#45159 = CARTESIAN_POINT('Ctrl Pts',(-20.6099160380865,-21.5058009332471,
123.298380195676)) ;
#45160 = CARTESIAN_POINT('Ctrl Pts',(-20.9100801364126,-21.3258118528842,
123.270041130568)) ;
#45161 = CARTESIAN_POINT('Ctrl Pts',(-20.5720819647299,-21.5157699784016,
123.092270132128)) ;
#45162 = CARTESIAN_POINT('Ctrl Pts',(-20.8627908877047,-21.3357808980387,
123.01239695694)) ;
#45163 = CARTESIAN_POINT('Ctrl Pts',(-20.499885467458,-21.5256733690351,122.8969600671)) ;
#45164 = CARTESIAN_POINT('Ctrl Pts',(-20.7725483587208,-21.3456842886722,
122.768260657611)) ;
#45165 = CARTESIAN_POINT('Ctrl Pts',(-20.3931639686196,-21.5357311551478,
122.714452129114)) ;
#45166 = CARTESIAN_POINT('Ctrl Pts',(-20.6391462593297,-21.355742074785,122.540122041422)) ;
#45167 = CARTESIAN_POINT('Ctrl Pts',(-20.2592745444822,-21.5455831917976,
122.556386418772)) ;
#45168 = CARTESIAN_POINT('Ctrl Pts',(-20.471796281269,-21.3655941114347,122.342544854426)) ;
#45169 = CARTESIAN_POINT('Ctrl Pts',(-20.0435430288408,-21.5589483159408,
122.376446565359)) ;
#45170 = CARTESIAN_POINT('Ctrl Pts',(-20.202086568455,-21.3789592355779,122.117585029651)) ;
#45171 = CARTESIAN_POINT('Ctrl Pts',(-19.7882330766326,-21.5721743789038,
122.25842779773)) ;
#45172 = CARTESIAN_POINT('Ctrl Pts',(-19.8829746642869,-21.3921852985409,
121.970083356066)) ;
#45173 = CARTESIAN_POINT('Ctrl Pts',(-19.512730849252,-21.5854780271861,122.210256078633)) ;
#45174 = CARTESIAN_POINT('Ctrl Pts',(-19.5386166648269,-21.4054889468232,
121.909867161857)) ;
#45175 = CARTESIAN_POINT('Ctrl Pts',(-19.3026540676817,-21.5954695583491,
122.210450686566)) ;
#45176 = CARTESIAN_POINT('Ctrl Pts',(-19.2760167649195,-21.4154804779862,
121.910107183642)) ;
#45177 = CARTESIAN_POINT('Ctrl Pts',(-19.0948968921359,-21.6055090061484,
122.247567522211)) ;
#45178 = CARTESIAN_POINT('Ctrl Pts',(-19.0163207496462,-21.4255199257855,
121.956500605478)) ;
#45179 = CARTESIAN_POINT('Ctrl Pts',(-18.9004687004283,-21.6153527816622,
122.318496927726)) ;
#45180 = CARTESIAN_POINT('Ctrl Pts',(-18.7732843139319,-21.4353637012994,
122.045159677628)) ;
#45181 = CARTESIAN_POINT('Ctrl Pts',(-18.7185579083454,-21.6253384230499,
122.423213533386)) ;
#45182 = CARTESIAN_POINT('Ctrl Pts',(-18.5458944197202,-21.445349342687,122.176053036341)) ;
#45183 = CARTESIAN_POINT('Ctrl Pts',(-18.5582565476501,-21.6352752074117,
122.557220506057)) ;
#45184 = CARTESIAN_POINT('Ctrl Pts',(-18.3455158402902,-21.4552861270488,
122.343559635745)) ;
#45185 = CARTESIAN_POINT('Ctrl Pts',(-18.4222459587121,-21.645325041879,122.718871713832)) ;
#45186 = CARTESIAN_POINT('Ctrl Pts',(-18.1755004123989,-21.4653359615162,
122.545621877111)) ;
#45187 = CARTESIAN_POINT('Ctrl Pts',(-18.3183162605906,-21.6551754913822,
122.898008987532)) ;
#45188 = CARTESIAN_POINT('Ctrl Pts',(-18.0455857951863,-21.4751864110193,
122.769542152888)) ;
#45189 = CARTESIAN_POINT('Ctrl Pts',(-18.2456911500029,-21.6651475053643,
123.09464249712)) ;
#45190 = CARTESIAN_POINT('Ctrl Pts',(-17.9548017337126,-21.4851584250014,
123.015333175436)) ;
#45191 = CARTESIAN_POINT('Ctrl Pts',(-18.2082412582699,-21.6751426632114,
123.301442369805)) ;
#45192 = CARTESIAN_POINT('Ctrl Pts',(-17.9079865989931,-21.4951535828485,
123.273832595304)) ;
#45193 = CARTESIAN_POINT('Ctrl Pts',(-18.2075185297832,-21.6851765895751,
123.512368066183)) ;
#45194 = CARTESIAN_POINT('Ctrl Pts',(-17.9070803718407,-21.5051875092122,
123.537489745388)) ;
#45195 = CARTESIAN_POINT('Ctrl Pts',(-18.2424799085402,-21.6950322980075,
123.716614333339)) ;
#45196 = CARTESIAN_POINT('Ctrl Pts',(-17.9507793758627,-21.5150432176446,
123.792798278233)) ;
#45197 = CARTESIAN_POINT('Ctrl Pts',(-18.3130824839469,-21.7050304473461,
123.914559389374)) ;
#45198 = CARTESIAN_POINT('Ctrl Pts',(-18.0390300008137,-21.5250413669833,
124.040230621142)) ;
#45199 = CARTESIAN_POINT('Ctrl Pts',(-18.4158251214299,-21.7149298505197,
124.095582065844)) ;
#45200 = CARTESIAN_POINT('Ctrl Pts',(-18.1674560178269,-21.5349407701568,
124.266510551616)) ;
#45201 = CARTESIAN_POINT('Ctrl Pts',(-18.5504028728454,-21.7249810474082,
124.258463624392)) ;
#45202 = CARTESIAN_POINT('Ctrl Pts',(-18.3356760700349,-21.5449919670453,
124.470114254987)) ;
#45203 = CARTESIAN_POINT('Ctrl Pts',(-18.7085246366495,-21.734863371221,124.393249383885)) ;
#45204 = CARTESIAN_POINT('Ctrl Pts',(-18.5333267197165,-21.5548742908582,
124.63859875685)) ;
#45205 = CARTESIAN_POINT('Ctrl Pts',(-18.8894290935753,-21.7448582668776,
124.500128199222)) ;
#45206 = CARTESIAN_POINT('Ctrl Pts',(-18.7594560018533,-21.5648691865148,
124.772199667984)) ;
#45207 = CARTESIAN_POINT('Ctrl Pts',(-19.0867831919036,-21.7548793662602,
124.573882631177)) ;
#45208 = CARTESIAN_POINT('Ctrl Pts',(-19.0061476935566,-21.5748902858973,
124.864395292257)) ;
#45209 = CARTESIAN_POINT('Ctrl Pts',(-19.2915499840716,-21.7647866341222,
124.611973404616)) ;
#45210 = CARTESIAN_POINT('Ctrl Pts',(-19.2621059878606,-21.5847975537594,
124.912011501582)) ;
#45211 = CARTESIAN_POINT('Ctrl Pts',(-19.5004581738309,-21.7747249779475,
124.614356734753)) ;
#45212 = CARTESIAN_POINT('Ctrl Pts',(-19.523241461829,-21.5947358975846,124.914993347183)) ;
#45213 = CARTESIAN_POINT('Ctrl Pts',(-19.7080148034449,-21.784728397248,124.580333186118)) ;
#45214 = CARTESIAN_POINT('Ctrl Pts',(-19.7826877608653,-21.6047393168851,
124.872466522298)) ;
#45215 = CARTESIAN_POINT('Ctrl Pts',(-19.9069801683133,-21.7947629479551,
124.510252770105)) ;
#45216 = CARTESIAN_POINT('Ctrl Pts',(-20.0313953526163,-21.6147738675922,
124.784868563439)) ;
#45217 = CARTESIAN_POINT('Ctrl Pts',(-20.0874764819987,-21.8046078975607,
124.408942640164)) ;
#45218 = CARTESIAN_POINT('Ctrl Pts',(-20.2570175361055,-21.6246188171978,
124.658232944476)) ;
#45219 = CARTESIAN_POINT('Ctrl Pts',(-20.2501460126216,-21.8145937396736,
124.276289518342)) ;
#45220 = CARTESIAN_POINT('Ctrl Pts',(-20.4603562191612,-21.6346046593107,
124.492418457877)) ;
#45221 = CARTESIAN_POINT('Ctrl Pts',(-20.3867706955757,-21.8245285470427,
124.118261781283)) ;
#45222 = CARTESIAN_POINT('Ctrl Pts',(-20.6311392301702,-21.6445394666798,
124.294885221514)) ;
#45223 = CARTESIAN_POINT('Ctrl Pts',(-20.4950064678875,-21.834586088756,123.936658959793)) ;
#45224 = CARTESIAN_POINT('Ctrl Pts',(-20.7664361277187,-21.6545970083931,
124.067883129677)) ;
#45225 = CARTESIAN_POINT('Ctrl Pts',(-20.568620634059,-21.8444076862681,123.743721916865)) ;
#45226 = CARTESIAN_POINT('Ctrl Pts',(-20.8584564948569,-21.6644186059052,
123.826712005177)) ;
#45227 = CARTESIAN_POINT('Ctrl Pts',(-20.6089246273583,-21.8544639457486,
123.53620346997)) ;
#45228 = CARTESIAN_POINT('Ctrl Pts',(-20.9088388978743,-21.6744748653857,
123.567314526484)) ;
#45229 = CARTESIAN_POINT('Ctrl Pts',(-20.6121758192455,-21.864403882049,123.327248711453)) ;
#45230 = CARTESIAN_POINT('Ctrl Pts',(-20.912905442173,-21.6844148016861,123.306120784318)) ;
#45231 = CARTESIAN_POINT('Ctrl Pts',(-20.5798268668381,-21.8743110027934,
123.121499920529)) ;
#45232 = CARTESIAN_POINT('Ctrl Pts',(-20.8724715625939,-21.6943219224305,
123.048933898916)) ;
#45233 = CARTESIAN_POINT('Ctrl Pts',(-20.5112454372603,-21.8843539087187,
122.921820528397)) ;
#45234 = CARTESIAN_POINT('Ctrl Pts',(-20.7867471086995,-21.7043648283558,
122.799333949718)) ;
#45235 = CARTESIAN_POINT('Ctrl Pts',(-20.4104399306398,-21.8942616898179,
122.739536472857)) ;
#45236 = CARTESIAN_POINT('Ctrl Pts',(-20.6607421010669,-21.714272609455,122.571477249608)) ;
#45237 = CARTESIAN_POINT('Ctrl Pts',(-20.2784482766661,-21.9042720588203,
122.57561542797)) ;
#45238 = CARTESIAN_POINT('Ctrl Pts',(-20.4957543255686,-21.7242829784574,
122.366574426333)) ;
#45239 = CARTESIAN_POINT('Ctrl Pts',(-20.1193995034889,-21.9143028973891,
122.437148355259)) ;
#45240 = CARTESIAN_POINT('Ctrl Pts',(-20.2969450012254,-21.7343138170262,
122.19348877084)) ;
#45241 = CARTESIAN_POINT('Ctrl Pts',(-19.9421174960905,-21.9241557370288,
122.33000905002)) ;
#45242 = CARTESIAN_POINT('Ctrl Pts',(-20.0753430040453,-21.7441666566659,
122.059562188914)) ;
#45243 = CARTESIAN_POINT('Ctrl Pts',(-19.7464337621037,-21.9341437381937,
122.253902994198)) ;
#45244 = CARTESIAN_POINT('Ctrl Pts',(-19.8307389892015,-21.7541546578309,
121.964427436421)) ;
#45245 = CARTESIAN_POINT('Ctrl Pts',(-19.5417073868984,-21.9440725571729,
122.213164409012)) ;
#45246 = CARTESIAN_POINT('Ctrl Pts',(-19.5748309877734,-21.76408347681,121.913501885889)) ;
#45247 = CARTESIAN_POINT('Ctrl Pts',(-19.3317819851724,-21.9540602598952,
122.208211065697)) ;
#45248 = CARTESIAN_POINT('Ctrl Pts',(-19.3124241042443,-21.7740711795323,
121.907308024055)) ;
#45249 = CARTESIAN_POINT('Ctrl Pts',(-19.1232546991255,-21.9640962596979,
122.240283219505)) ;
#45250 = CARTESIAN_POINT('Ctrl Pts',(-19.0517647367421,-21.784107179335,121.947395958042)) ;
#45251 = CARTESIAN_POINT('Ctrl Pts',(-18.9269352967466,-21.9739511294993,
122.306534700964)) ;
#45252 = CARTESIAN_POINT('Ctrl Pts',(-18.8063639187183,-21.7939620491364,
122.030208537148)) ;
#45253 = CARTESIAN_POINT('Ctrl Pts',(-18.7423427052336,-21.9839505599228,
122.407048270959)) ;
#45254 = CARTESIAN_POINT('Ctrl Pts',(-18.5756220536227,-21.80396147956,122.155848712853)) ;
#45255 = CARTESIAN_POINT('Ctrl Pts',(-18.5795278154634,-21.9938456773881,
122.536588268655)) ;
#45256 = CARTESIAN_POINT('Ctrl Pts',(-18.3721015982493,-21.8138565970253,
122.317772569663)) ;
#45257 = CARTESIAN_POINT('Ctrl Pts',(-18.4394307306069,-22.0039061709051,
122.695002768727)) ;
#45258 = CARTESIAN_POINT('Ctrl Pts',(-18.1969788650756,-21.8239170905422,
122.515789157084)) ;
#45259 = CARTESIAN_POINT('Ctrl Pts',(-18.3311666833367,-22.0137556511063,
122.871529628342)) ;
#45260 = CARTESIAN_POINT('Ctrl Pts',(-18.0616465449145,-21.8337665707434,
122.736447563643)) ;
#45261 = CARTESIAN_POINT('Ctrl Pts',(-18.253333217475,-22.0237821013701,123.067418185129)) ;
#45262 = CARTESIAN_POINT('Ctrl Pts',(-17.9643529997641,-21.8437930210072,
122.981307539562)) ;
#45263 = CARTESIAN_POINT('Ctrl Pts',(-18.2112421000978,-22.0338133918482,
123.274069161545)) ;
#45264 = CARTESIAN_POINT('Ctrl Pts',(-17.911737129383,-21.8538243114853,123.239620782822)) ;
#45265 = CARTESIAN_POINT('Ctrl Pts',(-18.2053271335064,-22.0436547795,123.480882845049)) ;
#45266 = CARTESIAN_POINT('Ctrl Pts',(-17.9043414975955,-21.8636656991371,
123.498138969836)) ;
#45267 = CARTESIAN_POINT('Ctrl Pts',(-18.235499498762,-22.0536581803912,123.688988918486)) ;
#45268 = CARTESIAN_POINT('Ctrl Pts',(-17.9420552180239,-21.8736691000283,
123.758271923707)) ;
#45269 = CARTESIAN_POINT('Ctrl Pts',(-18.3013232908441,-22.0636425631824,
123.88834285791)) ;
#45270 = CARTESIAN_POINT('Ctrl Pts',(-18.0243333212748,-21.8836534828195,
124.007465107845)) ;
#45271 = CARTESIAN_POINT('Ctrl Pts',(-18.4014559554124,-22.0736816531958,
124.074106712805)) ;
#45272 = CARTESIAN_POINT('Ctrl Pts',(-18.1494974495607,-21.8936925728329,
124.239670692868)) ;
#45273 = CARTESIAN_POINT('Ctrl Pts',(-18.5295972273494,-22.0835274621049,
124.236682169581)) ;
#45274 = CARTESIAN_POINT('Ctrl Pts',(-18.3096733742783,-21.9035383817421,
124.442892027175)) ;
#45275 = CARTESIAN_POINT('Ctrl Pts',(-18.6858761362846,-22.0935118849239,
124.376767470781)) ;
#45276 = CARTESIAN_POINT('Ctrl Pts',(-18.5050211085327,-21.9135228045611,
124.618000034142)) ;
#45277 = CARTESIAN_POINT('Ctrl Pts',(-18.8633080302938,-22.1034515101651,
124.487199990123)) ;
#45278 = CARTESIAN_POINT('Ctrl Pts',(-18.7268105926817,-21.9234624298023,
124.756042327652)) ;
#45279 = CARTESIAN_POINT('Ctrl Pts',(-19.0591476044493,-22.1134911996838,
124.565868443362)) ;
#45280 = CARTESIAN_POINT('Ctrl Pts',(-18.9716093217471,-21.9335021193209,
124.854379340595)) ;
#45281 = CARTESIAN_POINT('Ctrl Pts',(-19.2625612087232,-22.1233793881024,
124.608789289149)) ;
#45282 = CARTESIAN_POINT('Ctrl Pts',(-19.2258769015638,-21.9433903077395,
124.908032136323)) ;
#45283 = CARTESIAN_POINT('Ctrl Pts',(-19.4724346347167,-22.1333689141044,
124.616203338408)) ;
#45284 = CARTESIAN_POINT('Ctrl Pts',(-19.4882188467763,-21.9533798337416,
124.917301153433)) ;
#45285 = CARTESIAN_POINT('Ctrl Pts',(-19.6797404481245,-22.1433274154596,
124.586994703036)) ;
#45286 = CARTESIAN_POINT('Ctrl Pts',(-19.7473517520323,-21.9633383350968,
124.88079179001)) ;
#45287 = CARTESIAN_POINT('Ctrl Pts',(-19.8778238010788,-22.1532270094633,
124.523101680733)) ;
#45288 = CARTESIAN_POINT('Ctrl Pts',(-19.9949571853173,-21.9732379291004,
124.800926502595)) ;
#45289 = CARTESIAN_POINT('Ctrl Pts',(-20.0644952954339,-22.1632748975846,
124.424277452298)) ;
#45290 = CARTESIAN_POINT('Ctrl Pts',(-20.2282969934944,-21.9832858172217,
124.67739751358)) ;
#45291 = CARTESIAN_POINT('Ctrl Pts',(-20.2287857483374,-22.1731703228301,
124.296606248266)) ;
#45292 = CARTESIAN_POINT('Ctrl Pts',(-20.4336615725465,-21.9931812424672,
124.51780896921)) ;
#45293 = CARTESIAN_POINT('Ctrl Pts',(-20.3707381562611,-22.1832317135307,
124.139823950091)) ;
#45294 = CARTESIAN_POINT('Ctrl Pts',(-20.6111028161255,-22.0032426331678,
124.321832200981)) ;
#45295 = CARTESIAN_POINT('Ctrl Pts',(-20.4809482851262,-22.1930772972174,
123.964606584726)) ;
#45296 = CARTESIAN_POINT('Ctrl Pts',(-20.7488672563639,-22.0130882168545,
124.102810049072)) ;
#45297 = CARTESIAN_POINT('Ctrl Pts',(-20.5606363459277,-22.2030402705266,
123.770920839856)) ;
#45298 = CARTESIAN_POINT('Ctrl Pts',(-20.8484784322108,-22.0230511901637,
123.860702848364)) ;
#45299 = CARTESIAN_POINT('Ctrl Pts',(-20.605498138732,-22.2130659373523,123.564965764745)) ;
#45300 = CARTESIAN_POINT('Ctrl Pts',(-20.9045567467684,-22.0330768569895,
123.603259320304)) ;
#45301 = CARTESIAN_POINT('Ctrl Pts',(-20.6139362962588,-22.2229804152186,
123.356710312389)) ;
#45302 = CARTESIAN_POINT('Ctrl Pts',(-20.9151055478435,-22.0429913348558,
123.342939247587)) ;
#45303 = CARTESIAN_POINT('Ctrl Pts',(-20.5862899774463,-22.2329689298936,
123.148530954525)) ;
#45304 = CARTESIAN_POINT('Ctrl Pts',(-20.8805485313156,-22.0529798495308,
123.082714706942)) ;
#45305 = CARTESIAN_POINT('Ctrl Pts',(-20.5221446354155,-22.2430130408091,
122.947370956092)) ;
#45306 = CARTESIAN_POINT('Ctrl Pts',(-20.8003679518013,-22.0630239604462,
122.831264561867)) ;
#45307 = CARTESIAN_POINT('Ctrl Pts',(-20.4265781092213,-22.2528411784036,
122.764149083107)) ;
#45308 = CARTESIAN_POINT('Ctrl Pts',(-20.6809098953037,-22.0728520980408,
122.602235481647)) ;
#45309 = CARTESIAN_POINT('Ctrl Pts',(-20.2975883675018,-22.2629177464626,
122.596160440805)) ;
#45310 = CARTESIAN_POINT('Ctrl Pts',(-20.5196736795458,-22.0829286660997,
122.392249516455)) ;
#45311 = CARTESIAN_POINT('Ctrl Pts',(-20.1448753794696,-22.2727699083667,
122.456169185964)) ;
#45312 = CARTESIAN_POINT('Ctrl Pts',(-20.328782028387,-22.0927808280039,122.217258955797)) ;
#45313 = CARTESIAN_POINT('Ctrl Pts',(-19.9664229552607,-22.2828428703236,
122.342221971823)) ;
#45314 = CARTESIAN_POINT('Ctrl Pts',(-20.1057172725599,-22.1028537899607,
122.074824536988)) ;
#45315 = CARTESIAN_POINT('Ctrl Pts',(-19.7753081970072,-22.2926854323265,
122.26285604015)) ;
#45316 = CARTESIAN_POINT('Ctrl Pts',(-19.8668228113398,-22.1126963519636,
121.975615871429)) ;
#45317 = CARTESIAN_POINT('Ctrl Pts',(-19.5706672880173,-22.3026658688203,
122.216568225967)) ;
#45318 = CARTESIAN_POINT('Ctrl Pts',(-19.6110214816132,-22.1226767884574,
121.917755554155)) ;
#45319 = CARTESIAN_POINT('Ctrl Pts',(-19.3602768856682,-22.3126841741447,
122.206883478724)) ;
#45320 = CARTESIAN_POINT('Ctrl Pts',(-19.3480335183811,-22.1326950937818,
121.905648968687)) ;
#45321 = CARTESIAN_POINT('Ctrl Pts',(-19.1541230507367,-22.3225681380641,
122.233089766057)) ;
#45322 = CARTESIAN_POINT('Ctrl Pts',(-19.090340079734,-22.1425790577013,121.938406487101)) ;
#45323 = CARTESIAN_POINT('Ctrl Pts',(-18.9520588230378,-22.3326340148027,
122.295865398734)) ;
#45324 = CARTESIAN_POINT('Ctrl Pts',(-18.8377600204759,-22.1526449344398,
122.016875429429)) ;
#45325 = CARTESIAN_POINT('Ctrl Pts',(-18.7681011669116,-22.3424731156636,
122.390486931831)) ;
#45326 = CARTESIAN_POINT('Ctrl Pts',(-18.6078114382176,-22.1624840353007,
122.135152615212)) ;
#45327 = CARTESIAN_POINT('Ctrl Pts',(-18.5998200970519,-22.3525061985293,
122.517638100478)) ;
#45328 = CARTESIAN_POINT('Ctrl Pts',(-18.3974600457705,-22.1725171181664,
122.294091316826)) ;
#45329 = CARTESIAN_POINT('Ctrl Pts',(-18.4567024912476,-22.3625278838048,
122.672277268552)) ;
#45330 = CARTESIAN_POINT('Ctrl Pts',(-18.2185627413665,-22.1825388034419,
122.487389938133)) ;
#45331 = CARTESIAN_POINT('Ctrl Pts',(-18.3441099722616,-22.3723945789033,
122.846470293017)) ;
#45332 = CARTESIAN_POINT('Ctrl Pts',(-18.0778211454052,-22.1924054985404,
122.70513209668)) ;
#45333 = CARTESIAN_POINT('Ctrl Pts',(-18.2621912773549,-22.3823544686378,
123.039178686657)) ;
#45334 = CARTESIAN_POINT('Ctrl Pts',(-17.9754225074273,-22.2023653882749,
122.946017980769)) ;
#45335 = CARTESIAN_POINT('Ctrl Pts',(-18.214942034536,-22.3923894564633,123.2447729843)) ;
#45336 = CARTESIAN_POINT('Ctrl Pts',(-17.9163607642041,-22.2124003761004,
123.203010659034)) ;
#45337 = CARTESIAN_POINT('Ctrl Pts',(-18.2039207070877,-22.4022761605376,
123.452359252462)) ;
#45338 = CARTESIAN_POINT('Ctrl Pts',(-17.9025839574836,-22.2222870801747,
123.462494584695)) ;
#45339 = CARTESIAN_POINT('Ctrl Pts',(-18.2296104639163,-22.4123413047705,
123.662360780197)) ;
#45340 = CARTESIAN_POINT('Ctrl Pts',(-17.9346959980839,-22.2323522244076,
123.724996117154)) ;
#45341 = CARTESIAN_POINT('Ctrl Pts',(-18.2898035554938,-22.422180595499,123.860294782693)) ;
#45342 = CARTESIAN_POINT('Ctrl Pts',(-18.0099377691919,-22.2421915151362,
123.972415043862)) ;
#45343 = CARTESIAN_POINT('Ctrl Pts',(-18.3852909858274,-22.4322431529375,
124.049037318576)) ;
#45344 = CARTESIAN_POINT('Ctrl Pts',(-18.1292969690806,-22.2522540725746,
124.208342841471)) ;
#45345 = CARTESIAN_POINT('Ctrl Pts',(-18.5102142780944,-22.4421402041896,
124.215443211625)) ;
#45346 = CARTESIAN_POINT('Ctrl Pts',(-18.2854516849338,-22.2621511238267,
124.416351010826)) ;
#45347 = CARTESIAN_POINT('Ctrl Pts',(-18.6621688535695,-22.4520714109378,
124.358617696287)) ;
#45348 = CARTESIAN_POINT('Ctrl Pts',(-18.4753956190122,-22.272082330575,124.595319409224)) ;
#45349 = CARTESIAN_POINT('Ctrl Pts',(-18.8387544421233,-22.4621135951567,
124.474321570263)) ;
#45350 = CARTESIAN_POINT('Ctrl Pts',(-18.6961275311406,-22.2821245147938,
124.739948983585)) ;
#45351 = CARTESIAN_POINT('Ctrl Pts',(-19.0296939400006,-22.4720002232676,
124.556460841573)) ;
#45352 = CARTESIAN_POINT('Ctrl Pts',(-18.9348029986765,-22.2920111429047,
124.842623278117)) ;
#45353 = CARTESIAN_POINT('Ctrl Pts',(-19.234076559489,-22.4819934958,124.605048925011)) ;
#45354 = CARTESIAN_POINT('Ctrl Pts',(-19.190281558459,-22.3020044154371,124.903358057767)) ;
#45355 = CARTESIAN_POINT('Ctrl Pts',(-19.4427962027987,-22.4919385713414,
124.617281907534)) ;
#45356 = CARTESIAN_POINT('Ctrl Pts',(-19.4511817330596,-22.3119494909786,
124.918648968524)) ;
#45357 = CARTESIAN_POINT('Ctrl Pts',(-19.6506180805942,-22.5018881220697,
124.593481317551)) ;
#45358 = CARTESIAN_POINT('Ctrl Pts',(-19.7109595708651,-22.3218990417068,
124.888897659172)) ;
#45359 = CARTESIAN_POINT('Ctrl Pts',(-19.8528843773795,-22.5119274569177,
124.5332335477)) ;
#45360 = CARTESIAN_POINT('Ctrl Pts',(-19.963792160214,-22.3319383765548,124.813587576149)) ;
#45361 = CARTESIAN_POINT('Ctrl Pts',(-20.0388462005348,-22.5218135958616,
124.440381350932)) ;
#45362 = CARTESIAN_POINT('Ctrl Pts',(-20.196245173065,-22.3418245154987,124.697521392829)) ;
#45363 = CARTESIAN_POINT('Ctrl Pts',(-20.2078788172091,-22.5318117088353,
124.315489125279)) ;
#45364 = CARTESIAN_POINT('Ctrl Pts',(-20.4075357060316,-22.3518226284724,
124.541405526169)) ;
#45365 = CARTESIAN_POINT('Ctrl Pts',(-20.3516487618174,-22.5417314711877,
124.164389810808)) ;
#45366 = CARTESIAN_POINT('Ctrl Pts',(-20.5872481934702,-22.3617423908249,
124.352530361773)) ;
#45367 = CARTESIAN_POINT('Ctrl Pts',(-20.4684258196986,-22.5517708668004,
123.98859191938)) ;
#45368 = CARTESIAN_POINT('Ctrl Pts',(-20.7332188476262,-22.3717817864375,
124.132782767646)) ;
#45369 = CARTESIAN_POINT('Ctrl Pts',(-20.5517552452748,-22.5616800525887,
123.797660250607)) ;
#45370 = CARTESIAN_POINT('Ctrl Pts',(-20.8373803848515,-22.3816909722258,
123.894117096644)) ;
#45371 = CARTESIAN_POINT('Ctrl Pts',(-20.6013649615286,-22.5716152367462,
123.594766848094)) ;
#45372 = CARTESIAN_POINT('Ctrl Pts',(-20.8993918232317,-22.3916261563833,
123.640499494821)) ;
#45373 = CARTESIAN_POINT('Ctrl Pts',(-20.6149297753148,-22.5816562941321,
123.384113634597)) ;
#45374 = CARTESIAN_POINT('Ctrl Pts',(-20.9163470243233,-22.4016672137692,
123.377183112359)) ;
#45375 = CARTESIAN_POINT('Ctrl Pts',(-20.5922146510685,-22.5915434521654,
123.177488411578)) ;
#45376 = CARTESIAN_POINT('Ctrl Pts',(-20.8879521472035,-22.4115543718025,
123.118900643946)) ;
#45377 = CARTESIAN_POINT('Ctrl Pts',(-20.5336910768669,-22.6015357318413,
122.975751109046)) ;
#45378 = CARTESIAN_POINT('Ctrl Pts',(-20.8147966666412,-22.4215466514784,
122.866729097642)) ;
#45379 = CARTESIAN_POINT('Ctrl Pts',(-20.4413703874593,-22.6114842488863,
122.788067427756)) ;
#45380 = CARTESIAN_POINT('Ctrl Pts',(-20.6993946933195,-22.4314951685235,
122.632124438289)) ;
#45381 = CARTESIAN_POINT('Ctrl Pts',(-20.3182652486574,-22.6214210264567,
122.619313417233)) ;
#45382 = CARTESIAN_POINT('Ctrl Pts',(-20.5455120187168,-22.4414319460939,
122.421182047729)) ;
#45383 = CARTESIAN_POINT('Ctrl Pts',(-20.1671801256002,-22.6314040626037,
122.473601909739)) ;
#45384 = CARTESIAN_POINT('Ctrl Pts',(-20.3566546113368,-22.4514149822408,
122.239043334206)) ;
#45385 = CARTESIAN_POINT('Ctrl Pts',(-19.991856607727,-22.6414478141974,122.355972854816)) ;
#45386 = CARTESIAN_POINT('Ctrl Pts',(-20.1374997937318,-22.4614587338345,
122.092007982459)) ;
#45387 = CARTESIAN_POINT('Ctrl Pts',(-19.8030570092897,-22.65127634341,122.271939115384)) ;
#45388 = CARTESIAN_POINT('Ctrl Pts',(-19.9014984819869,-22.4712872630471,
121.986966332369)) ;
#45389 = CARTESIAN_POINT('Ctrl Pts',(-19.5975962709593,-22.6613517043187,
122.220614922131)) ;
#45390 = CARTESIAN_POINT('Ctrl Pts',(-19.644672669795,-22.4813626239558,121.922812414429)) ;
#45391 = CARTESIAN_POINT('Ctrl Pts',(-19.3908522666017,-22.6712083032059,
122.205989042453)) ;
#45392 = CARTESIAN_POINT('Ctrl Pts',(-19.3862413607618,-22.491219222843,121.904531259593)) ;
#45393 = CARTESIAN_POINT('Ctrl Pts',(-19.1804545485629,-22.6812712972238,
122.227705733918)) ;
#45394 = CARTESIAN_POINT('Ctrl Pts',(-19.1232446773172,-22.5012822168609,
121.931678446646)) ;
#45395 = CARTESIAN_POINT('Ctrl Pts',(-18.9806951570671,-22.6911492315132,
122.284594628893)) ;
#45396 = CARTESIAN_POINT('Ctrl Pts',(-18.8735448281778,-22.5111601511503,
122.002791143889)) ;
#45397 = CARTESIAN_POINT('Ctrl Pts',(-18.7914526517928,-22.7011498790713,
122.376106438856)) ;
#45398 = CARTESIAN_POINT('Ctrl Pts',(-18.6369922199882,-22.5211607987084,
122.117182286071)) ;
#45399 = CARTESIAN_POINT('Ctrl Pts',(-18.6222332954635,-22.7110677255094,
122.497984639726)) ;
#45400 = CARTESIAN_POINT('Ctrl Pts',(-18.4254683343915,-22.5310786451465,
122.269531684477)) ;
#45401 = CARTESIAN_POINT('Ctrl Pts',(-18.474883672655,-22.721118842515,122.649391564558)) ;
#45402 = CARTESIAN_POINT('Ctrl Pts',(-18.2412825269459,-22.5411297621521,
122.45879123557)) ;
#45403 = CARTESIAN_POINT('Ctrl Pts',(-18.3579599908217,-22.7309895778256,
122.820875939281)) ;
#45404 = CARTESIAN_POINT('Ctrl Pts',(-18.0951286476762,-22.5510004974627,
122.673148447113)) ;
#45405 = CARTESIAN_POINT('Ctrl Pts',(-18.270849081835,-22.7410602850686,123.013805427642)) ;
#45406 = CARTESIAN_POINT('Ctrl Pts',(-17.986241610246,-22.5610712047057,122.914310640418)) ;
#45407 = CARTESIAN_POINT('Ctrl Pts',(-18.2196899669182,-22.7508932925205,
123.214115396645)) ;
#45408 = CARTESIAN_POINT('Ctrl Pts',(-17.9222939724761,-22.5709042121576,
123.164699747312)) ;
#45409 = CARTESIAN_POINT('Ctrl Pts',(-18.203176745519,-22.7609237848228,123.42433279345)) ;
#45410 = CARTESIAN_POINT('Ctrl Pts',(-17.9016542679233,-22.5809347044599,
123.427471548306)) ;
#45411 = CARTESIAN_POINT('Ctrl Pts',(-18.2240311555207,-22.7709553798962,
123.634206914964)) ;
#45412 = CARTESIAN_POINT('Ctrl Pts',(-17.927723884169,-22.5909662995333,123.689813957202)) ;
#45413 = CARTESIAN_POINT('Ctrl Pts',(-18.2794406669794,-22.7807850790344,
123.83327619676)) ;
#45414 = CARTESIAN_POINT('Ctrl Pts',(-17.9969878123147,-22.6007959986715,
123.93865131243)) ;
#45415 = CARTESIAN_POINT('Ctrl Pts',(-18.3694648397809,-22.790774528916,124.023019043572)) ;
#45416 = CARTESIAN_POINT('Ctrl Pts',(-18.1095198729244,-22.6107854485531,
124.175829191989)) ;
#45417 = CARTESIAN_POINT('Ctrl Pts',(-18.4921611930021,-22.8008183867317,
124.194863216364)) ;
#45418 = CARTESIAN_POINT('Ctrl Pts',(-18.2628916857644,-22.6208293063688,
124.390633246382)) ;
#45419 = CARTESIAN_POINT('Ctrl Pts',(-18.6391999982746,-22.8106400773219,
124.339828342554)) ;
#45420 = CARTESIAN_POINT('Ctrl Pts',(-18.446692434265,-22.630650996959,124.571839161793)) ;
#45421 = CARTESIAN_POINT('Ctrl Pts',(-18.8125751270944,-22.8206751678623,
124.460026469785)) ;
#45422 = CARTESIAN_POINT('Ctrl Pts',(-18.6634124377873,-22.6406860874994,
124.722085054435)) ;
#45423 = CARTESIAN_POINT('Ctrl Pts',(-19.0042354854205,-22.830699686845,124.547700241937)) ;
#45424 = CARTESIAN_POINT('Ctrl Pts',(-18.9029886662497,-22.6507106064821,
124.831675526016)) ;
#45425 = CARTESIAN_POINT('Ctrl Pts',(-19.2047392934395,-22.8405595322552,
124.600226995631)) ;
#45426 = CARTESIAN_POINT('Ctrl Pts',(-19.1536198777574,-22.6605704518923,
124.897332264122)) ;
#45427 = CARTESIAN_POINT('Ctrl Pts',(-19.4133825738018,-22.8505193085708,
124.617890170241)) ;
#45428 = CARTESIAN_POINT('Ctrl Pts',(-19.4144244913002,-22.670530228208,124.919409092967)) ;
#45429 = CARTESIAN_POINT('Ctrl Pts',(-19.6233229031397,-22.8605475058855,
124.598638239538)) ;
#45430 = CARTESIAN_POINT('Ctrl Pts',(-19.6768496651292,-22.6805584255226,
124.895342097645)) ;
#45431 = CARTESIAN_POINT('Ctrl Pts',(-19.8243679055007,-22.8704550481758,
124.544126078897)) ;
#45432 = CARTESIAN_POINT('Ctrl Pts',(-19.9281559636117,-22.6904659678129,
124.827199646983)) ;
#45433 = CARTESIAN_POINT('Ctrl Pts',(-20.0152757096399,-22.8804876987396,
124.454494142613)) ;
#45434 = CARTESIAN_POINT('Ctrl Pts',(-20.1667897461997,-22.7004986183768,
124.715157775083)) ;
#45435 = CARTESIAN_POINT('Ctrl Pts',(-20.1852178949266,-22.8903716551663,
124.33491330894)) ;
#45436 = CARTESIAN_POINT('Ctrl Pts',(-20.3792168210052,-22.7103825748034,
124.56567950925)) ;
#45437 = CARTESIAN_POINT('Ctrl Pts',(-20.3337523313298,-22.9003613565281,
124.186436934306)) ;
#45438 = CARTESIAN_POINT('Ctrl Pts',(-20.5648833309736,-22.7203722761653,
124.380082284069)) ;
#45439 = CARTESIAN_POINT('Ctrl Pts',(-20.4544985548872,-22.9104023518042,
124.013286908638)) ;
#45440 = CARTESIAN_POINT('Ctrl Pts',(-20.7158142403492,-22.7304132714413,
124.163643559951)) ;
#45441 = CARTESIAN_POINT('Ctrl Pts',(-20.5418120177757,-22.9202352410725,
123.825917664307)) ;
#45442 = CARTESIAN_POINT('Ctrl Pts',(-20.8249543879318,-22.7402461607097,
123.929430163563)) ;
#45443 = CARTESIAN_POINT('Ctrl Pts',(-20.5967197719903,-22.93022839944,123.623135595412)) ;
#45444 = CARTESIAN_POINT('Ctrl Pts',(-20.8935867559205,-22.7502393190771,
123.675951817842)) ;
#45445 = CARTESIAN_POINT('Ctrl Pts',(-20.6152207366922,-22.9402604417921,
123.413033506782)) ;
#45446 = CARTESIAN_POINT('Ctrl Pts',(-20.9167106283028,-22.7602713614292,
123.413324039136)) ;
#45447 = CARTESIAN_POINT('Ctrl Pts',(-20.5975204253957,-22.9501256857505,
123.2064025244)) ;
#45448 = CARTESIAN_POINT('Ctrl Pts',(-20.8945827853963,-22.7701366053876,
123.155034786092)) ;
#45449 = CARTESIAN_POINT('Ctrl Pts',(-20.5442580745083,-22.9600875769965,
123.003852214581)) ;
#45450 = CARTESIAN_POINT('Ctrl Pts',(-20.82800234089,-22.7800984966336,122.901847296241)) ;
#45451 = CARTESIAN_POINT('Ctrl Pts',(-20.4556884997879,-22.970122477015,122.812391064617)) ;
#45452 = CARTESIAN_POINT('Ctrl Pts',(-20.7172881603951,-22.7901333966521,
122.662521920387)) ;
#45453 = CARTESIAN_POINT('Ctrl Pts',(-20.3372800803288,-22.9800075574296,
122.641575983214)) ;
#45454 = CARTESIAN_POINT('Ctrl Pts',(-20.5692752424808,-22.8000184770667,
122.449004039222)) ;
#45455 = CARTESIAN_POINT('Ctrl Pts',(-20.1883694042385,-22.9900727295544,
122.491279319789)) ;
#45456 = CARTESIAN_POINT('Ctrl Pts',(-20.3831352080727,-22.8100836491915,
122.261135086256)) ;
#45457 = CARTESIAN_POINT('Ctrl Pts',(-20.0193951599007,-22.9999199642779,
122.37164075247)) ;
#45458 = CARTESIAN_POINT('Ctrl Pts',(-20.1719153765991,-22.819930883915,122.111588554488)) ;
#45459 = CARTESIAN_POINT('Ctrl Pts',(-19.8289685430891,-23.0099507755956,
122.281076764927)) ;
#45460 = CARTESIAN_POINT('Ctrl Pts',(-19.9338810019722,-22.8299616952328,
121.998385955222)) ;
#45461 = CARTESIAN_POINT('Ctrl Pts',(-19.6259877305142,-23.0199603915091,
122.225477205925)) ;
#45462 = CARTESIAN_POINT('Ctrl Pts',(-19.6801542546242,-22.8399713111463,
121.928888950712)) ;
#45463 = CARTESIAN_POINT('Ctrl Pts',(-19.4185677638405,-23.0298711709128,
122.205958909889)) ;
#45464 = CARTESIAN_POINT('Ctrl Pts',(-19.4208786354196,-22.84988209055,121.904493618432)) ;
#45465 = CARTESIAN_POINT('Ctrl Pts',(-19.2104507212989,-23.0398004367019,
122.222263809827)) ;
#45466 = CARTESIAN_POINT('Ctrl Pts',(-19.1607322268354,-22.859811356339,121.924877430898)) ;
#45467 = CARTESIAN_POINT('Ctrl Pts',(-19.0060800631454,-23.0498431300145,
122.275221685096)) ;
#45468 = CARTESIAN_POINT('Ctrl Pts',(-18.9052696006217,-22.8698540496516,
121.991077325652)) ;
#45469 = CARTESIAN_POINT('Ctrl Pts',(-18.816920652705,-23.0597296627092,122.361382751279)) ;
#45470 = CARTESIAN_POINT('Ctrl Pts',(-18.6688210508467,-22.8797405823464,
122.098781259546)) ;
#45471 = CARTESIAN_POINT('Ctrl Pts',(-18.6435653180198,-23.0697228078125,
122.480041622256)) ;
#45472 = CARTESIAN_POINT('Ctrl Pts',(-18.4521283292672,-22.8897337274496,
122.247107144986)) ;
#45473 = CARTESIAN_POINT('Ctrl Pts',(-18.4942067621472,-23.0796684884866,
122.626365687683)) ;
#45474 = CARTESIAN_POINT('Ctrl Pts',(-18.2654318576276,-22.8996794081237,
122.430014319229)) ;
#45475 = CARTESIAN_POINT('Ctrl Pts',(-18.3721507507593,-23.0896157461133,
122.796186530113)) ;
#45476 = CARTESIAN_POINT('Ctrl Pts',(-18.1128639588266,-22.9096266657504,
122.642292140986)) ;
#45477 = CARTESIAN_POINT('Ctrl Pts',(-18.280738860759,-23.0996636482348,122.986614485634)) ;
#45478 = CARTESIAN_POINT('Ctrl Pts',(-17.9986015572507,-22.9196745678719,
122.880328253833)) ;
#45479 = CARTESIAN_POINT('Ctrl Pts',(-18.2247452921894,-23.1095113538565,
123.185929489645)) ;
#45480 = CARTESIAN_POINT('Ctrl Pts',(-17.9286121291567,-22.9295222734936,
123.129473138919)) ;
#45481 = CARTESIAN_POINT('Ctrl Pts',(-18.203315371917,-23.1194728204906,123.394243964455)) ;
#45482 = CARTESIAN_POINT('Ctrl Pts',(-17.9018275042711,-22.9394837401277,
123.389866644002)) ;
#45483 = CARTESIAN_POINT('Ctrl Pts',(-18.2187690231212,-23.1295023737588,
123.604537566451)) ;
#45484 = CARTESIAN_POINT('Ctrl Pts',(-17.9211473399048,-22.9495132933959,
123.652733485376)) ;
#45485 = CARTESIAN_POINT('Ctrl Pts',(-18.2697520445231,-23.1394092657862,
123.806478018759)) ;
#45486 = CARTESIAN_POINT('Ctrl Pts',(-17.9848788717473,-22.9594201854233,
123.905158576402)) ;
#45487 = CARTESIAN_POINT('Ctrl Pts',(-18.3549970966278,-23.1493569098992,
123.997428173794)) ;
#45488 = CARTESIAN_POINT('Ctrl Pts',(-18.0914378078134,-22.9693678295363,
124.143845240036)) ;
#45489 = CARTESIAN_POINT('Ctrl Pts',(-18.4726356234465,-23.1593569529281,
124.171699257656)) ;
#45490 = CARTESIAN_POINT('Ctrl Pts',(-18.2384883382395,-22.9793678725652,
124.361682579422)) ;
#45491 = CARTESIAN_POINT('Ctrl Pts',(-18.6195515746322,-23.1693957189221,
124.323190189224)) ;
#45492 = CARTESIAN_POINT('Ctrl Pts',(-18.4221353271476,-22.9894066385592,
124.551044334108)) ;
#45493 = CARTESIAN_POINT('Ctrl Pts',(-18.7866669271075,-23.1792207809443,
124.444609990743)) ;
#45494 = CARTESIAN_POINT('Ctrl Pts',(-18.6310313255418,-22.9992317005814,
124.702816918751)) ;
#45495 = CARTESIAN_POINT('Ctrl Pts',(-18.9764845901678,-23.1892753282707,
124.537586105056)) ;
#45496 = CARTESIAN_POINT('Ctrl Pts',(-18.8683046803637,-23.0092862479078,
124.81903454041)) ;
#45497 = CARTESIAN_POINT('Ctrl Pts',(-19.1774335204479,-23.1992185717199,
124.595200515695)) ;
#45498 = CARTESIAN_POINT('Ctrl Pts',(-19.1194917233323,-23.019229491357,124.891049871198)) ;
#45499 = CARTESIAN_POINT('Ctrl Pts',(-19.3844025852747,-23.2091207433278,
124.617601381638)) ;
#45500 = CARTESIAN_POINT('Ctrl Pts',(-19.3782034066478,-23.0291316629649,
124.919048155738)) ;
#45501 = CARTESIAN_POINT('Ctrl Pts',(-19.5952575378545,-23.219173578938,124.603384824931)) ;
#45502 = CARTESIAN_POINT('Ctrl Pts',(-19.6417720055539,-23.0391844985751,
124.9012746228)) ;
#45503 = CARTESIAN_POINT('Ctrl Pts',(-19.796808082773,-23.2290466366235,124.553754633832)) ;
#45504 = CARTESIAN_POINT('Ctrl Pts',(-19.8937094829923,-23.0490575562606,
124.839234191459)) ;
#45505 = CARTESIAN_POINT('Ctrl Pts',(-19.9892291256445,-23.2390418981492,
124.469324547835)) ;
#45506 = CARTESIAN_POINT('Ctrl Pts',(-20.1342348698061,-23.0590528177863,
124.733693798384)) ;
#45507 = CARTESIAN_POINT('Ctrl Pts',(-20.1643902735447,-23.2490672675697,
124.352097383469)) ;
#45508 = CARTESIAN_POINT('Ctrl Pts',(-20.3531841875638,-23.0690781872068,
124.587158170132)) ;
#45509 = CARTESIAN_POINT('Ctrl Pts',(-20.3146713289308,-23.2589571000963,
124.208405044587)) ;
#45510 = CARTESIAN_POINT('Ctrl Pts',(-20.5410358788454,-23.0789680197334,
124.407538039965)) ;
#45511 = CARTESIAN_POINT('Ctrl Pts',(-20.4803738058375,-23.2722550709057,
123.98326749613)) ;
#45512 = CARTESIAN_POINT('Ctrl Pts',(-20.74814931711,-23.0922659905428,124.126127329763)) ;
#45513 = CARTESIAN_POINT('Ctrl Pts',(-20.5831671550575,-23.2854534660148,
123.722071678799)) ;
#45514 = CARTESIAN_POINT('Ctrl Pts',(-20.87663678955,-23.105464385652,123.799667857733)) ;
#45515 = CARTESIAN_POINT('Ctrl Pts',(-20.6148571245368,-23.2988489082943,
123.442305301246)) ;
#45516 = CARTESIAN_POINT('Ctrl Pts',(-20.9162580761209,-23.1188598279314,
123.449902418922)) ;
#45517 = CARTESIAN_POINT('Ctrl Pts',(-20.6022321518531,-23.3087247465333,
123.235027259948)) ;
#45518 = CARTESIAN_POINT('Ctrl Pts',(-20.9004717403109,-23.1287356661704,
123.190816756868)) ;
#45519 = CARTESIAN_POINT('Ctrl Pts',(-20.5530100746428,-23.318786149131,123.029348117295)) ;
#45520 = CARTESIAN_POINT('Ctrl Pts',(-20.8389416666321,-23.1387970687681,
122.933714939038)) ;
#45521 = CARTESIAN_POINT('Ctrl Pts',(-20.470495204662,-23.3286512060661,122.839039896976)) ;
#45522 = CARTESIAN_POINT('Ctrl Pts',(-20.7357971607144,-23.1486621257033,
122.69583283738)) ;
#45523 = CARTESIAN_POINT('Ctrl Pts',(-20.3548367842642,-23.3386633020149,
122.663215896037)) ;
#45524 = CARTESIAN_POINT('Ctrl Pts',(-20.5912157870178,-23.1586742216521,
122.476050346887)) ;
#45525 = CARTESIAN_POINT('Ctrl Pts',(-20.1631967914319,-23.3519406111604,
122.460187922931)) ;
#45526 = CARTESIAN_POINT('Ctrl Pts',(-20.3516936594044,-23.1719515307975,
122.222286259416)) ;
#45527 = CARTESIAN_POINT('Ctrl Pts',(-19.8630377268875,-23.3685396366677,
122.274632914981)) ;
#45528 = CARTESIAN_POINT('Ctrl Pts',(-19.9764398067608,-23.1885505563048,
121.990323874655)) ;
#45529 = CARTESIAN_POINT('Ctrl Pts',(-19.517487437228,-23.3851386847007,122.202591928007)) ;
#45530 = CARTESIAN_POINT('Ctrl Pts',(-19.5445846288261,-23.2051496043378,
121.900290049291)) ;
#45531 = CARTESIAN_POINT('Ctrl Pts',(-19.23951312528,-23.3983820967316,122.217815968059)) ;
#45532 = CARTESIAN_POINT('Ctrl Pts',(-19.197050432373,-23.2183930163688,121.919316506906)) ;
#45533 = CARTESIAN_POINT('Ctrl Pts',(-19.0339916765018,-23.4084195244201,
122.265667627133)) ;
#45534 = CARTESIAN_POINT('Ctrl Pts',(-18.9401631491161,-23.2284304440572,
121.979134289703)) ;
#45535 = CARTESIAN_POINT('Ctrl Pts',(-18.8424913044911,-23.4183238263757,
122.347410808801)) ;
#45536 = CARTESIAN_POINT('Ctrl Pts',(-18.7007825062615,-23.2383347460128,
122.08131781826)) ;
#45537 = CARTESIAN_POINT('Ctrl Pts',(-18.6084602838952,-23.4315906663508,
122.499189778994)) ;
#45538 = CARTESIAN_POINT('Ctrl Pts',(-18.4082618728628,-23.251601585988,122.271030307521)) ;
#45539 = CARTESIAN_POINT('Ctrl Pts',(-18.3717345959788,-23.4482168644408,
122.761707590166)) ;
#45540 = CARTESIAN_POINT('Ctrl Pts',(-18.1123399887699,-23.2682277840779,
122.599191193754)) ;
#45541 = CARTESIAN_POINT('Ctrl Pts',(-18.2123565640676,-23.4681359798242,
123.154114455554)) ;
#45542 = CARTESIAN_POINT('Ctrl Pts',(-17.9131297581632,-23.2881468994613,
123.089717711788)) ;
#45543 = CARTESIAN_POINT('Ctrl Pts',(-18.1988208253406,-23.4847424029584,
123.506996953541)) ;
#45544 = CARTESIAN_POINT('Ctrl Pts',(-17.8962057487813,-23.3047533225956,
123.530754190466)) ;
#45545 = CARTESIAN_POINT('Ctrl Pts',(-18.2607588524776,-23.4980386234541,
123.779530753442)) ;
#45546 = CARTESIAN_POINT('Ctrl Pts',(-17.9736383080703,-23.3180495430913,
123.871481315084)) ;
#45547 = CARTESIAN_POINT('Ctrl Pts',(-18.3683238744161,-23.5113074557956,
124.036997547401)) ;
#45548 = CARTESIAN_POINT('Ctrl Pts',(-18.1080876895051,-23.3313183754327,
124.193291225439)) ;
#45549 = CARTESIAN_POINT('Ctrl Pts',(-18.585515956159,-23.5279987038287,124.31755527357)) ;
#45550 = CARTESIAN_POINT('Ctrl Pts',(-18.3795904845808,-23.3480096234658,
124.544002089629)) ;
#45551 = CARTESIAN_POINT('Ctrl Pts',(-18.9413317824027,-23.5478084355015,
124.543077586913)) ;
#45552 = CARTESIAN_POINT('Ctrl Pts',(-18.8243580038784,-23.3678193551386,
124.825895671555)) ;
#45553 = CARTESIAN_POINT('Ctrl Pts',(-19.3559796542478,-23.56778604283,124.635208528437)) ;
#45554 = CARTESIAN_POINT('Ctrl Pts',(-19.3426692477421,-23.3877969624672,
124.941057197669)) ;
#45555 = CARTESIAN_POINT('Ctrl Pts',(-19.7759608022422,-23.5877123518879,
124.579685890579)) ;
#45556 = CARTESIAN_POINT('Ctrl Pts',(-19.8676443126626,-23.407723271525,124.871649885225)) ;
#45557 = CARTESIAN_POINT('Ctrl Pts',(-20.1505472402133,-23.6075292120526,
124.386491448277)) ;
#45558 = CARTESIAN_POINT('Ctrl Pts',(-20.3358743901566,-23.4275401316897,
124.630155280585)) ;
#45559 = CARTESIAN_POINT('Ctrl Pts',(-20.4401428515061,-23.6276290276466,
124.072390207339)) ;
#45560 = CARTESIAN_POINT('Ctrl Pts',(-20.6978674016167,-23.4476399472837,
124.237525821763)) ;
#45561 = CARTESIAN_POINT('Ctrl Pts',(-20.6026657871358,-23.6473859915291,
123.684825873049)) ;
#45562 = CARTESIAN_POINT('Ctrl Pts',(-20.9010174941863,-23.4673969111663,
123.753071870117)) ;
#45563 = CARTESIAN_POINT('Ctrl Pts',(-20.6242876059637,-23.6674229175986,
123.259481688023)) ;
#45564 = CARTESIAN_POINT('Ctrl Pts',(-20.9280426935608,-23.4874338372357,
123.221391133714)) ;
#45565 = CARTESIAN_POINT('Ctrl Pts',(-20.4997957023964,-23.6872924999801,
122.855645078802)) ;
#45566 = CARTESIAN_POINT('Ctrl Pts',(-20.772426096765,-23.5073034196172,122.716597558778)) ;
#45567 = CARTESIAN_POINT('Ctrl Pts',(-20.2454865673464,-23.7071970717333,
122.517448321673)) ;
#45568 = CARTESIAN_POINT('Ctrl Pts',(-20.4545393933605,-23.5272079913704,
122.293853597091)) ;
#45569 = CARTESIAN_POINT('Ctrl Pts',(-19.8900271158853,-23.7271496739318,
122.285727883188)) ;
#45570 = CARTESIAN_POINT('Ctrl Pts',(-20.0102149504557,-23.5471605935689,
122.004204373971)) ;
#45571 = CARTESIAN_POINT('Ctrl Pts',(-19.4778464728188,-23.747059164902,122.189596892363)) ;
#45572 = CARTESIAN_POINT('Ctrl Pts',(-19.4949902616942,-23.5670700845392,
121.884042017214)) ;
#45573 = CARTESIAN_POINT('Ctrl Pts',(-19.0585021845433,-23.7669105336015,
122.238587168872)) ;
#45574 = CARTESIAN_POINT('Ctrl Pts',(-18.9708122647659,-23.5869214532386,
121.94527950064)) ;
#45575 = CARTESIAN_POINT('Ctrl Pts',(-18.6771515985997,-23.7869907297375,
122.43039174872)) ;
#45576 = CARTESIAN_POINT('Ctrl Pts',(-18.4941229340544,-23.6070016493746,
122.185035924344)) ;
#45577 = CARTESIAN_POINT('Ctrl Pts',(-18.3880786328134,-23.8067916733129,
122.736642917923)) ;
#45578 = CARTESIAN_POINT('Ctrl Pts',(-18.1327837985555,-23.62680259295,122.567847534588)) ;
#45579 = CARTESIAN_POINT('Ctrl Pts',(-18.2185138748618,-23.8267756498224,
123.126183556028)) ;
#45580 = CARTESIAN_POINT('Ctrl Pts',(-17.9208269264055,-23.6467865694595,
123.054772698368)) ;
#45581 = CARTESIAN_POINT('Ctrl Pts',(-18.1928000702527,-23.846691612798,123.54886807584)) ;
#45582 = CARTESIAN_POINT('Ctrl Pts',(-17.8886839110732,-23.6667025324351,
123.583127051767)) ;
#45583 = CARTESIAN_POINT('Ctrl Pts',(-18.3114981929088,-23.8665620476199,
123.954437415859)) ;
#45584 = CARTESIAN_POINT('Ctrl Pts',(-18.0370543006657,-23.686572967257,124.090087584522)) ;
#45585 = CARTESIAN_POINT('Ctrl Pts',(-18.5641851710754,-23.886612332853,124.297650548748)) ;
#45586 = CARTESIAN_POINT('Ctrl Pts',(-18.3529120736301,-23.7066232524901,
124.519105466772)) ;
#45587 = CARTESIAN_POINT('Ctrl Pts',(-18.9138459519034,-23.9063863016123,
124.531438448419)) ;
#45588 = CARTESIAN_POINT('Ctrl Pts',(-18.789984541274,-23.7263972212494,124.811340607854)) ;
#45589 = CARTESIAN_POINT('Ctrl Pts',(-19.327728107229,-23.9264427597318,124.633511754983)) ;
#45590 = CARTESIAN_POINT('Ctrl Pts',(-19.3073372095614,-23.746453679369,124.93893490729)) ;
#45591 = CARTESIAN_POINT('Ctrl Pts',(-19.7463440551213,-23.9462376427228,
124.588636490226)) ;
#45592 = CARTESIAN_POINT('Ctrl Pts',(-19.8306051755044,-23.76624856236,124.882843707526)) ;
#45593 = CARTESIAN_POINT('Ctrl Pts',(-20.128134455108,-23.9662042980252,124.403168082798)) ;
#45594 = CARTESIAN_POINT('Ctrl Pts',(-20.3078444224997,-23.7862152176623,
124.651011447722)) ;
#45595 = CARTESIAN_POINT('Ctrl Pts',(-20.4232185491835,-23.9861632681017,
124.098054033906)) ;
#45596 = CARTESIAN_POINT('Ctrl Pts',(-20.6767016461882,-23.8061741877388,
124.269621393362)) ;
#45597 = CARTESIAN_POINT('Ctrl Pts',(-20.5961622014183,-24.0060593556918,
123.711998667547)) ;
#45598 = CARTESIAN_POINT('Ctrl Pts',(-20.892884068729,-23.8260702753289,123.787054530312)) ;
#45599 = CARTESIAN_POINT('Ctrl Pts',(-20.6274889819743,-24.0259575256034,
123.290106766545)) ;
#45600 = CARTESIAN_POINT('Ctrl Pts',(-20.9320464014087,-23.8459684452405,
123.259690813219)) ;
#45601 = CARTESIAN_POINT('Ctrl Pts',(-20.513337763902,-24.0458633609705,122.882506566483)) ;
#45602 = CARTESIAN_POINT('Ctrl Pts',(-20.7893616368976,-23.8658742806076,
122.750190072207)) ;
#45603 = CARTESIAN_POINT('Ctrl Pts',(-20.266431677999,-24.0658132859084,122.537627079781)) ;
#45604 = CARTESIAN_POINT('Ctrl Pts',(-20.4807327588592,-23.8858242055455,
122.319088447684)) ;
#45605 = CARTESIAN_POINT('Ctrl Pts',(-19.9180548383199,-24.0856924758188,
122.298181469176)) ;
#45606 = CARTESIAN_POINT('Ctrl Pts',(-20.0452649316201,-23.9057033954559,
122.019778092239)) ;
#45607 = CARTESIAN_POINT('Ctrl Pts',(-19.5069122512383,-24.1056738000994,
122.191249797151)) ;
#45608 = CARTESIAN_POINT('Ctrl Pts',(-19.5313379424967,-23.9256847197365,
121.886108846057)) ;
#45609 = CARTESIAN_POINT('Ctrl Pts',(-19.0849454561733,-24.1256035843077,
122.231166566416)) ;
#45610 = CARTESIAN_POINT('Ctrl Pts',(-19.0038793190178,-23.9456145039448,
121.936000230857)) ;
#45611 = CARTESIAN_POINT('Ctrl Pts',(-18.7022509031181,-24.1455235736985,
122.412432300618)) ;
#45612 = CARTESIAN_POINT('Ctrl Pts',(-18.5255093850671,-23.9655344933356,
122.162577000674)) ;
#45613 = CARTESIAN_POINT('Ctrl Pts',(-18.4045331289834,-24.1653787690525,
122.711900017558)) ;
#45614 = CARTESIAN_POINT('Ctrl Pts',(-18.1533588423712,-23.9853896886896,
122.536910497568)) ;
#45615 = CARTESIAN_POINT('Ctrl Pts',(-18.2256300026401,-24.1854247707119,
123.098661615411)) ;
#45616 = CARTESIAN_POINT('Ctrl Pts',(-17.9297252155865,-24.005435690349,123.020349675099)) ;
#45617 = CARTESIAN_POINT('Ctrl Pts',(-18.1956840876194,-24.2019245179217,
123.448290706154)) ;
#45618 = CARTESIAN_POINT('Ctrl Pts',(-17.8922881637436,-24.0219354375588,
123.457418896112)) ;
#45619 = CARTESIAN_POINT('Ctrl Pts',(-18.244751099481,-24.2153131223698,123.725437756677)) ;
#45620 = CARTESIAN_POINT('Ctrl Pts',(-17.9536182369137,-24.0353240420069,
123.803823185436)) ;
#45621 = CARTESIAN_POINT('Ctrl Pts',(-18.3158010212771,-24.2251749507047,
123.92021291796)) ;
#45622 = CARTESIAN_POINT('Ctrl Pts',(-18.0424306542549,-24.0451858703418,
124.047300970856)) ;
#45623 = CARTESIAN_POINT('Ctrl Pts',(-18.4201246805275,-24.2351410934622,
124.101932284297)) ;
#45624 = CARTESIAN_POINT('Ctrl Pts',(-18.1728224348044,-24.0551520130994,
124.274441107709)) ;
#45625 = CARTESIAN_POINT('Ctrl Pts',(-18.600479700421,-24.2485028395872,124.317163919076)) ;
#45626 = CARTESIAN_POINT('Ctrl Pts',(-18.398315477012,-24.0685137592243,124.543527593381)) ;
#45627 = CARTESIAN_POINT('Ctrl Pts',(-18.8864879871126,-24.2649571685423,
124.518993893139)) ;
#45628 = CARTESIAN_POINT('Ctrl Pts',(-18.7557534014151,-24.0849680881794,
124.795766078304)) ;
#45629 = CARTESIAN_POINT('Ctrl Pts',(-19.2302450355489,-24.2817244135906,
124.612794594497)) ;
#45630 = CARTESIAN_POINT('Ctrl Pts',(-19.1855079887731,-24.1017353332277,
124.913045707015)) ;
#45631 = CARTESIAN_POINT('Ctrl Pts',(-19.5076006939437,-24.2949109788646,
124.613694249436)) ;
#45632 = CARTESIAN_POINT('Ctrl Pts',(-19.5321625871901,-24.1149218985017,
124.914163508115)) ;
#45633 = CARTESIAN_POINT('Ctrl Pts',(-19.714585996907,-24.3049004376092,124.57853472076)) ;
#45634 = CARTESIAN_POINT('Ctrl Pts',(-19.7909027433267,-24.1249113572463,
124.870218955293)) ;
#45635 = CARTESIAN_POINT('Ctrl Pts',(-19.9117282679633,-24.3148542100903,
124.508226632481)) ;
#45636 = CARTESIAN_POINT('Ctrl Pts',(-20.0373293987813,-24.1348651297274,
124.782335916118)) ;
#45637 = CARTESIAN_POINT('Ctrl Pts',(-20.0952429868065,-24.324902026623,124.40366816945)) ;
#45638 = CARTESIAN_POINT('Ctrl Pts',(-20.2667248444726,-24.1449129462601,
124.651640371251)) ;
#45639 = CARTESIAN_POINT('Ctrl Pts',(-20.2546683283464,-24.3347435597455,
124.271759801232)) ;
#45640 = CARTESIAN_POINT('Ctrl Pts',(-20.4660081191832,-24.1547544793826,
124.486757064472)) ;
#45641 = CARTESIAN_POINT('Ctrl Pts',(-20.3910452829839,-24.3447298019652,
124.112189741865)) ;
#45642 = CARTESIAN_POINT('Ctrl Pts',(-20.6364815530708,-24.1647407216023,
124.287296273843)) ;
#45643 = CARTESIAN_POINT('Ctrl Pts',(-20.4972397987561,-24.3546664253901,
123.932255968931)) ;
#45644 = CARTESIAN_POINT('Ctrl Pts',(-20.7692271456916,-24.1746773450272,
124.062380424929)) ;
#45645 = CARTESIAN_POINT('Ctrl Pts',(-20.5712954604918,-24.3647163027731,
123.73440257886)) ;
#45646 = CARTESIAN_POINT('Ctrl Pts',(-20.8617993883025,-24.1847272224102,
123.815064619583)) ;
#45647 = CARTESIAN_POINT('Ctrl Pts',(-20.6092665986412,-24.3745667415506,
123.530810616257)) ;
#45648 = CARTESIAN_POINT('Ctrl Pts',(-20.9092661000716,-24.1945776611878,
123.560575071859)) ;
#45649 = CARTESIAN_POINT('Ctrl Pts',(-20.6118828892727,-24.3845387555194,
123.321210192378)) ;
#45650 = CARTESIAN_POINT('Ctrl Pts',(-20.9125392723098,-24.2045496751565,
123.298574461719)) ;
#45651 = CARTESIAN_POINT('Ctrl Pts',(-20.5779494879227,-24.3945339241455,
123.113804511949)) ;
#45652 = CARTESIAN_POINT('Ctrl Pts',(-20.8701252717379,-24.2145448437826,
123.039316830709)) ;
#45653 = CARTESIAN_POINT('Ctrl Pts',(-20.5080285322928,-24.4045678074067,
122.914803419106)) ;
#45654 = CARTESIAN_POINT('Ctrl Pts',(-20.7827267210347,-24.2245787270438,
122.790564493814)) ;
#45655 = CARTESIAN_POINT('Ctrl Pts',(-20.4067104297543,-24.41442367747,122.734046050817)) ;
#45656 = CARTESIAN_POINT('Ctrl Pts',(-20.6560814228119,-24.2344345971071,
122.564616215145)) ;
#45657 = CARTESIAN_POINT('Ctrl Pts',(-20.2739437816179,-24.4244212233872,
122.571137981273)) ;
#45658 = CARTESIAN_POINT('Ctrl Pts',(-20.4901252098502,-24.2444321430243,
122.3609792939)) ;
#45659 = CARTESIAN_POINT('Ctrl Pts',(-20.1163503321144,-24.4343293502864,
122.434915065284)) ;
#45660 = CARTESIAN_POINT('Ctrl Pts',(-20.293135035734,-24.2543402699236,122.190698398529)) ;
#45661 = CARTESIAN_POINT('Ctrl Pts',(-19.9358381554827,-24.4443397218086,
122.326707961461)) ;
#45662 = CARTESIAN_POINT('Ctrl Pts',(-20.0674961654377,-24.2643506414457,
122.055437128195)) ;
#45663 = CARTESIAN_POINT('Ctrl Pts',(-19.7387342050816,-24.454370164556,122.251783176735)) ;
#45664 = CARTESIAN_POINT('Ctrl Pts',(-19.8211172047256,-24.2743810841931,
121.961778537735)) ;
#45665 = CARTESIAN_POINT('Ctrl Pts',(-19.5354521664302,-24.4642181171093,
122.212461214448)) ;
#45666 = CARTESIAN_POINT('Ctrl Pts',(-19.5670147878812,-24.2842290367464,
121.912623318456)) ;
#45667 = CARTESIAN_POINT('Ctrl Pts',(-19.3239551652899,-24.4742807861303,
122.208794045191)) ;
#45668 = CARTESIAN_POINT('Ctrl Pts',(-19.3026436245788,-24.2942917057674,
121.908036631008)) ;
#45669 = CARTESIAN_POINT('Ctrl Pts',(-19.1185123192759,-24.4841751615942,
122.241504281932)) ;
#45670 = CARTESIAN_POINT('Ctrl Pts',(-19.0458393133714,-24.3041860812313,
121.948921771872)) ;
#45671 = CARTESIAN_POINT('Ctrl Pts',(-18.9207873898694,-24.4941169599123,
122.309170126325)) ;
#45672 = CARTESIAN_POINT('Ctrl Pts',(-18.7986820358757,-24.3141278795495,
122.033501629842)) ;
#45673 = CARTESIAN_POINT('Ctrl Pts',(-18.7366115575641,-24.5041194536396,
122.410711220208)) ;
#45674 = CARTESIAN_POINT('Ctrl Pts',(-18.5684608876012,-24.3241303732768,
122.160425707919)) ;
#45675 = CARTESIAN_POINT('Ctrl Pts',(-18.5725769314898,-24.5141542521466,
122.543347790697)) ;
#45676 = CARTESIAN_POINT('Ctrl Pts',(-18.3634159135229,-24.3341651717837,
122.326219304177)) ;
#45677 = CARTESIAN_POINT('Ctrl Pts',(-18.4364059179355,-24.5239991361259,
122.699231885075)) ;
#45678 = CARTESIAN_POINT('Ctrl Pts',(-18.1931997744196,-24.3440100557631,
122.521073096174)) ;
#45679 = CARTESIAN_POINT('Ctrl Pts',(-18.3275230682562,-24.533984992944,122.878683232876)) ;
#45680 = CARTESIAN_POINT('Ctrl Pts',(-18.0570939034257,-24.3539959125811,
122.745386068162)) ;
#45681 = CARTESIAN_POINT('Ctrl Pts',(-18.2516769257629,-24.5439198071187,
123.073327761756)) ;
#45682 = CARTESIAN_POINT('Ctrl Pts',(-17.9622837121039,-24.3639307267559,
122.988691099202)) ;
#45683 = CARTESIAN_POINT('Ctrl Pts',(-18.2104726947077,-24.5539773069041,
123.280683690247)) ;
#45684 = CARTESIAN_POINT('Ctrl Pts',(-17.9107758866694,-24.3739882265412,
123.247885388004)) ;
#45685 = CARTESIAN_POINT('Ctrl Pts',(-18.2056888743538,-24.5637990653224,
123.487134857633)) ;
#45686 = CARTESIAN_POINT('Ctrl Pts',(-17.904793545213,-24.3838099849595,123.505950068629)) ;
#45687 = CARTESIAN_POINT('Ctrl Pts',(-18.2371668828863,-24.5738547231064,
123.696162130977)) ;
#45688 = CARTESIAN_POINT('Ctrl Pts',(-17.9441385895894,-24.3938656427435,
123.767234420915)) ;
#45689 = CARTESIAN_POINT('Ctrl Pts',(-18.3040695591823,-24.5837969052864,
123.894192986261)) ;
#45690 = CARTESIAN_POINT('Ctrl Pts',(-18.0277646258523,-24.4038078249235,
124.014774122479)) ;
#45691 = CARTESIAN_POINT('Ctrl Pts',(-18.4034039808886,-24.5937021139811,
124.07720850749)) ;
#45692 = CARTESIAN_POINT('Ctrl Pts',(-18.1519307759585,-24.4137130336182,
124.243545142332)) ;
#45693 = CARTESIAN_POINT('Ctrl Pts',(-18.5348467278453,-24.6037439049435,
124.242401635363)) ;
#45694 = CARTESIAN_POINT('Ctrl Pts',(-18.3162322484998,-24.4237548245807,
124.450038000876)) ;
#45695 = CARTESIAN_POINT('Ctrl Pts',(-18.6908591823526,-24.6136516794158,
124.380420797567)) ;
#45696 = CARTESIAN_POINT('Ctrl Pts',(-18.5112465951366,-24.4336625990529,
124.622564118162)) ;
#45697 = CARTESIAN_POINT('Ctrl Pts',(-18.8701202015806,-24.6236631796434,
124.490724089556)) ;
#45698 = CARTESIAN_POINT('Ctrl Pts',(-18.7353216882572,-24.4436740992805,
124.760445262885)) ;
#45699 = CARTESIAN_POINT('Ctrl Pts',(-19.0663816760572,-24.6336959400361,
124.567979438688)) ;
#45700 = CARTESIAN_POINT('Ctrl Pts',(-18.9806475911732,-24.4537068596732,
124.857016709312)) ;
#45701 = CARTESIAN_POINT('Ctrl Pts',(-19.2692552137906,-24.643546509171,124.609578863151)) ;
#45702 = CARTESIAN_POINT('Ctrl Pts',(-19.2342398512447,-24.4635574288081,
124.909018469813)) ;
#45703 = CARTESIAN_POINT('Ctrl Pts',(-19.4791376987757,-24.6535351187009,
124.615797717259)) ;
#45704 = CARTESIAN_POINT('Ctrl Pts',(-19.496593073052,-24.473546038338,124.916794312844)) ;
#45705 = CARTESIAN_POINT('Ctrl Pts',(-19.6856874087961,-24.663463774725,124.585656540183)) ;
#45706 = CARTESIAN_POINT('Ctrl Pts',(-19.7547810174037,-24.4834746943621,
124.879120015881)) ;
#45707 = CARTESIAN_POINT('Ctrl Pts',(-19.8851618333618,-24.6734515209028,
124.520055763717)) ;
#45708 = CARTESIAN_POINT('Ctrl Pts',(-20.0041249025158,-24.4934624405399,
124.797121058112)) ;
#45709 = CARTESIAN_POINT('Ctrl Pts',(-20.0709240901513,-24.6834875098385,
124.420032910437)) ;
#45710 = CARTESIAN_POINT('Ctrl Pts',(-20.2363287243684,-24.5034984294756,
124.672094532501)) ;
#45711 = CARTESIAN_POINT('Ctrl Pts',(-20.2337420876468,-24.6933423796521,
124.291888982276)) ;
#45712 = CARTESIAN_POINT('Ctrl Pts',(-20.4398532893897,-24.5133532992892,
124.511915768883)) ;
#45713 = CARTESIAN_POINT('Ctrl Pts',(-20.3740410207416,-24.7033418208939,
124.135384425764)) ;
#45714 = CARTESIAN_POINT('Ctrl Pts',(-20.6152286146219,-24.523352740531,124.316286380148)) ;
#45715 = CARTESIAN_POINT('Ctrl Pts',(-20.4841026431737,-24.713236895074,123.958818728685)) ;
#45716 = CARTESIAN_POINT('Ctrl Pts',(-20.7528077611867,-24.5332478147111,
124.095579716367)) ;
#45717 = CARTESIAN_POINT('Ctrl Pts',(-20.5630911584333,-24.7232975509137,
123.762644267269)) ;
#45718 = CARTESIAN_POINT('Ctrl Pts',(-20.8515452176625,-24.5433084705508,
123.850362627596)) ;
#45719 = CARTESIAN_POINT('Ctrl Pts',(-20.6060224074376,-24.7331464251093,
123.560073880987)) ;
#45720 = CARTESIAN_POINT('Ctrl Pts',(-20.90521146566,-24.5531573447464,123.597149046186)) ;
#45721 = CARTESIAN_POINT('Ctrl Pts',(-20.6137892692649,-24.7431751370725,
123.349384846586)) ;
#45722 = CARTESIAN_POINT('Ctrl Pts',(-20.9149218984342,-24.5631860567097,
123.333787858284)) ;
#45723 = CARTESIAN_POINT('Ctrl Pts',(-20.5842846845228,-24.7532045376556,
123.140605694628)) ;
#45724 = CARTESIAN_POINT('Ctrl Pts',(-20.8780431867244,-24.5732154572928,
123.072813707619)) ;
#45725 = CARTESIAN_POINT('Ctrl Pts',(-20.5206480631986,-24.7630447312725,
122.943761957022)) ;
#45726 = CARTESIAN_POINT('Ctrl Pts',(-20.7984988600526,-24.5830556509096,
122.826757371458)) ;
#45727 = CARTESIAN_POINT('Ctrl Pts',(-20.4225485419105,-24.7730481538477,
122.757764156564)) ;
#45728 = CARTESIAN_POINT('Ctrl Pts',(-20.675875973219,-24.5930590734848,122.594259198633)) ;
#45729 = CARTESIAN_POINT('Ctrl Pts',(-20.2937856669965,-24.7830336909408,
122.591919417926)) ;
#45730 = CARTESIAN_POINT('Ctrl Pts',(-20.5149236678703,-24.6030446105779,
122.386952011327)) ;
#45731 = CARTESIAN_POINT('Ctrl Pts',(-20.1372175607481,-24.7930746954276,
122.450362162771)) ;
#45732 = CARTESIAN_POINT('Ctrl Pts',(-20.319214882974,-24.6130856150647,122.210004150072)) ;
#45733 = CARTESIAN_POINT('Ctrl Pts',(-19.9620847517272,-24.8029182343688,
122.340090117792)) ;
#45734 = CARTESIAN_POINT('Ctrl Pts',(-20.100298824301,-24.6229291540059,122.072161974285)) ;
#45735 = CARTESIAN_POINT('Ctrl Pts',(-19.7679204826026,-24.8129032653596,
122.260388804538)) ;
#45736 = CARTESIAN_POINT('Ctrl Pts',(-19.8575938757749,-24.6329141849967,
121.972533729906)) ;
#45737 = CARTESIAN_POINT('Ctrl Pts',(-19.5637613025099,-24.8228427278816,
122.215721170497)) ;
#45738 = CARTESIAN_POINT('Ctrl Pts',(-19.6023947114749,-24.6428536475187,
121.916697509575)) ;
#45739 = CARTESIAN_POINT('Ctrl Pts',(-19.3528855208101,-24.8328824601054,
122.207143938468)) ;
#45740 = CARTESIAN_POINT('Ctrl Pts',(-19.3388001962216,-24.6528933797425,
121.905974359338)) ;
#45741 = CARTESIAN_POINT('Ctrl Pts',(-19.1468393604488,-24.8427706404226,
122.234788301827)) ;
#45742 = CARTESIAN_POINT('Ctrl Pts',(-19.0812413725031,-24.6627815600597,
121.940528367606)) ;
#45743 = CARTESIAN_POINT('Ctrl Pts',(-18.9465910465543,-24.8527601561251,
122.298052941285)) ;
#45744 = CARTESIAN_POINT('Ctrl Pts',(-18.830930339593,-24.6727710757622,122.019607849904)) ;
#45745 = CARTESIAN_POINT('Ctrl Pts',(-18.7610210692701,-24.8627187067798,
122.394969542259)) ;
#45746 = CARTESIAN_POINT('Ctrl Pts',(-18.5989667873706,-24.6827296264169,
122.140752466296)) ;
#45747 = CARTESIAN_POINT('Ctrl Pts',(-18.5957514950734,-24.8726181138848,
122.521477714569)) ;
#45748 = CARTESIAN_POINT('Ctrl Pts',(-18.3923783177254,-24.6926290335219,
122.298887165231)) ;
#45749 = CARTESIAN_POINT('Ctrl Pts',(-18.4529280511965,-24.8826667003011,
122.677100505805)) ;
#45750 = CARTESIAN_POINT('Ctrl Pts',(-18.2138481637525,-24.7026776199382,
122.493414575767)) ;
#45751 = CARTESIAN_POINT('Ctrl Pts',(-18.3408505972411,-24.8925595192655,
122.85234593428)) ;
#45752 = CARTESIAN_POINT('Ctrl Pts',(-18.0737497675781,-24.7125704389027,
122.712471449112)) ;
#45753 = CARTESIAN_POINT('Ctrl Pts',(-18.2595668677293,-24.9026306367953,
123.047801925644)) ;
#45754 = CARTESIAN_POINT('Ctrl Pts',(-17.9721440404555,-24.7226415564325,
122.95679058556)) ;
#45755 = CARTESIAN_POINT('Ctrl Pts',(-18.2143360447103,-24.9124463307614,
123.249180345051)) ;
#45756 = CARTESIAN_POINT('Ctrl Pts',(-17.9156039987701,-24.7324572503985,
123.208514840523)) ;
#45757 = CARTESIAN_POINT('Ctrl Pts',(-18.2042126503118,-24.9225127082587,
123.460520176297)) ;
#45758 = CARTESIAN_POINT('Ctrl Pts',(-17.9029486725744,-24.7425236278958,
123.472689210429)) ;
#45759 = CARTESIAN_POINT('Ctrl Pts',(-18.2305681873623,-24.9324116943406,
123.667004534321)) ;
#45760 = CARTESIAN_POINT('Ctrl Pts',(-17.935892095498,-24.7524226139777,123.730795685717)) ;
#45761 = CARTESIAN_POINT('Ctrl Pts',(-18.2932377700678,-24.9424658743341,
123.868822725467)) ;
#45762 = CARTESIAN_POINT('Ctrl Pts',(-18.0142279454651,-24.7624767939712,
123.983068491379)) ;
#45763 = CARTESIAN_POINT('Ctrl Pts',(-18.3880943306794,-24.9523366872668,
124.053444339054)) ;
#45764 = CARTESIAN_POINT('Ctrl Pts',(-18.1327982653444,-24.7723476069039,
124.213846997016)) ;
#45765 = CARTESIAN_POINT('Ctrl Pts',(-18.5160928318226,-24.9624105881206,
124.222110708763)) ;
#45766 = CARTESIAN_POINT('Ctrl Pts',(-18.2927953165878,-24.7824215077577,
124.424680232047)) ;
#45767 = CARTESIAN_POINT('Ctrl Pts',(-18.6674180149936,-24.9722307435072,
124.362618007818)) ;
#45768 = CARTESIAN_POINT('Ctrl Pts',(-18.4819523062821,-24.7922416631444,
124.600316090913)) ;
#45769 = CARTESIAN_POINT('Ctrl Pts',(-18.8452136411496,-24.9823094504595,
124.477780776126)) ;
#45770 = CARTESIAN_POINT('Ctrl Pts',(-18.7041959809352,-24.8023203700966,
124.744270009316)) ;
#45771 = CARTESIAN_POINT('Ctrl Pts',(-19.0359724593799,-24.9921610389983,
124.558567319872)) ;
#45772 = CARTESIAN_POINT('Ctrl Pts',(-18.9426453970189,-24.8121719586354,
124.845254460228)) ;
#45773 = CARTESIAN_POINT('Ctrl Pts',(-19.2422734738344,-25.0022341555233,
124.606210580914)) ;
#45774 = CARTESIAN_POINT('Ctrl Pts',(-19.200521069137,-24.8222450751604,124.904809172551)) ;
#45775 = CARTESIAN_POINT('Ctrl Pts',(-19.4489294427733,-25.0120766726191,
124.617025230768)) ;
#45776 = CARTESIAN_POINT('Ctrl Pts',(-19.4588424041164,-24.8320875922562,
124.91832832477)) ;
#45777 = CARTESIAN_POINT('Ctrl Pts',(-19.6572595399181,-25.022057134173,124.592142989449)) ;
#45778 = CARTESIAN_POINT('Ctrl Pts',(-19.7192553917927,-24.8420680538102,
124.887225976131)) ;
#45779 = CARTESIAN_POINT('Ctrl Pts',(-19.858754508053,-25.0320753841638,124.530845580541)) ;
#45780 = CARTESIAN_POINT('Ctrl Pts',(-19.9711242826029,-24.8520863038009,
124.810604842072)) ;
#45781 = CARTESIAN_POINT('Ctrl Pts',(-20.0442458404208,-25.0419595443576,
124.437141256552)) ;
#45782 = CARTESIAN_POINT('Ctrl Pts',(-20.2029896410635,-24.8619704639947,
124.693474375189)) ;
#45783 = CARTESIAN_POINT('Ctrl Pts',(-20.2136336533158,-25.0520246913326,
124.310362839137)) ;
#45784 = CARTESIAN_POINT('Ctrl Pts',(-20.4147243951242,-24.8720356109697,
124.535001991824)) ;
#45785 = CARTESIAN_POINT('Ctrl Pts',(-20.3553327642867,-25.0618665149734,
124.159573795063)) ;
#45786 = CARTESIAN_POINT('Ctrl Pts',(-20.5918496186671,-24.8818774346105,
124.346514930548)) ;
#45787 = CARTESIAN_POINT('Ctrl Pts',(-20.4713227735349,-25.0718959874342,
123.98349792825)) ;
#45788 = CARTESIAN_POINT('Ctrl Pts',(-20.7368372685072,-24.8919069070713,
124.126420308641)) ;
#45789 = CARTESIAN_POINT('Ctrl Pts',(-20.5544183696664,-25.0819228426962,
123.789765828092)) ;
#45790 = CARTESIAN_POINT('Ctrl Pts',(-20.8407071584653,-24.9019337623334,
123.884255455993)) ;
#45791 = CARTESIAN_POINT('Ctrl Pts',(-20.6022129333517,-25.0917660928068,
123.58842207058)) ;
#45792 = CARTESIAN_POINT('Ctrl Pts',(-20.9004509562917,-24.9117770124439,
123.632574419147)) ;
#45793 = CARTESIAN_POINT('Ctrl Pts',(-20.6148605428865,-25.1018145323899,
123.377557024283)) ;
#45794 = CARTESIAN_POINT('Ctrl Pts',(-20.916260611242,-24.9218254520271,123.368993380643)) ;
#45795 = CARTESIAN_POINT('Ctrl Pts',(-20.590610957124,-25.1117640266378,123.16979691793)) ;
#45796 = CARTESIAN_POINT('Ctrl Pts',(-20.8859488523691,-24.931774946275,123.109292637768)) ;
#45797 = CARTESIAN_POINT('Ctrl Pts',(-20.5315027514083,-25.1216718823638,
122.970053451003)) ;
#45798 = CARTESIAN_POINT('Ctrl Pts',(-20.812063374515,-24.941682802001,122.85961242254)) ;
#45799 = CARTESIAN_POINT('Ctrl Pts',(-20.4370028959412,-25.1317313590138,
122.780884060618)) ;
#45800 = CARTESIAN_POINT('Ctrl Pts',(-20.6939388264685,-24.9517422786509,
122.623150935641)) ;
#45801 = CARTESIAN_POINT('Ctrl Pts',(-20.3140267459724,-25.1415721684225,
122.614484936629)) ;
#45802 = CARTESIAN_POINT('Ctrl Pts',(-20.5402177796958,-24.9615830880596,
122.415150839327)) ;
#45803 = CARTESIAN_POINT('Ctrl Pts',(-20.1608696779371,-25.1516343187233,
122.46860151475)) ;
#45804 = CARTESIAN_POINT('Ctrl Pts',(-20.3487716521003,-24.9716452383604,
122.232796879525)) ;
#45805 = CARTESIAN_POINT('Ctrl Pts',(-19.9874513742878,-25.1615314798458,
122.353608540262)) ;
#45806 = CARTESIAN_POINT('Ctrl Pts',(-20.1319979378848,-24.981542399483,122.089055106717)) ;
#45807 = CARTESIAN_POINT('Ctrl Pts',(-19.7963375421497,-25.1714626542499,
122.269557911198)) ;
#45808 = CARTESIAN_POINT('Ctrl Pts',(-19.8931048762682,-24.991473573887,121.983991783669)) ;
#45809 = CARTESIAN_POINT('Ctrl Pts',(-19.5912085972719,-25.1815048579749,
122.219637399699)) ;
#45810 = CARTESIAN_POINT('Ctrl Pts',(-19.6366938542377,-25.001515777612,121.921591372385)) ;
#45811 = CARTESIAN_POINT('Ctrl Pts',(-19.3837898601191,-25.1913914404053,
122.206149497569)) ;
#45812 = CARTESIAN_POINT('Ctrl Pts',(-19.3774193320319,-25.0114023600425,
121.904731667752)) ;
#45813 = CARTESIAN_POINT('Ctrl Pts',(-19.174930617181,-25.2013848761537,122.228779671047)) ;
#45814 = CARTESIAN_POINT('Ctrl Pts',(-19.116345118076,-25.0213957957908,121.933019786069)) ;
#45815 = CARTESIAN_POINT('Ctrl Pts',(-18.9741668937736,-25.2113293445118,
122.287109961351)) ;
#45816 = CARTESIAN_POINT('Ctrl Pts',(-18.8653899853733,-25.031340264149,122.0059331557)) ;
#45817 = CARTESIAN_POINT('Ctrl Pts',(-18.7862616744613,-25.2212811607574,
122.379130251146)) ;
#45818 = CARTESIAN_POINT('Ctrl Pts',(-18.6305081904514,-25.0412920803945,
122.120959221121)) ;
#45819 = CARTESIAN_POINT('Ctrl Pts',(-18.6158633692364,-25.2313185968719,
122.503584025425)) ;
#45820 = CARTESIAN_POINT('Ctrl Pts',(-18.4175106984375,-25.051329516509,122.276526693865)) ;
#45821 = CARTESIAN_POINT('Ctrl Pts',(-18.4717187038832,-25.2412035560482,
122.653303494758)) ;
#45822 = CARTESIAN_POINT('Ctrl Pts',(-18.2373294887089,-25.0612144756854,
122.463677159572)) ;
#45823 = CARTESIAN_POINT('Ctrl Pts',(-18.3542495988289,-25.2512016742602,
122.827576694392)) ;
#45824 = CARTESIAN_POINT('Ctrl Pts',(-18.0904935273236,-25.0712125938973,
122.681519130343)) ;
#45825 = CARTESIAN_POINT('Ctrl Pts',(-18.2693324752695,-25.2611226067721,
123.018101116052)) ;
#45826 = CARTESIAN_POINT('Ctrl Pts',(-17.9843474113932,-25.0811335264093,
122.919675638714)) ;
#45827 = CARTESIAN_POINT('Ctrl Pts',(-18.2181276836119,-25.2711639069942,
123.2228864421)) ;
#45828 = CARTESIAN_POINT('Ctrl Pts',(-17.9203421285094,-25.0911748266313,
123.175657289294)) ;
#45829 = CARTESIAN_POINT('Ctrl Pts',(-18.203527625728,-25.2810708253842,123.430650481538)) ;
#45830 = CARTESIAN_POINT('Ctrl Pts',(-17.9020926498255,-25.1010817450213,
123.435363279085)) ;
#45831 = CARTESIAN_POINT('Ctrl Pts',(-18.2246915361504,-25.2910066170932,
123.638458055856)) ;
#45832 = CARTESIAN_POINT('Ctrl Pts',(-17.9285484881312,-25.1110175367304,
123.69512331008)) ;
#45833 = CARTESIAN_POINT('Ctrl Pts',(-18.2824223938012,-25.3010475116711,
123.841496647617)) ;
#45834 = CARTESIAN_POINT('Ctrl Pts',(-18.0007127842541,-25.1210584313083,
123.948921149935)) ;
#45835 = CARTESIAN_POINT('Ctrl Pts',(-18.3729909834067,-25.310934713385,124.028599784085)) ;
#45836 = CARTESIAN_POINT('Ctrl Pts',(-18.1139247515408,-25.1309456330221,
124.18280063066)) ;
#45837 = CARTESIAN_POINT('Ctrl Pts',(-18.4956664931269,-25.3209269811466,
124.19910961797)) ;
#45838 = CARTESIAN_POINT('Ctrl Pts',(-18.2672700656794,-25.1409379007837,
124.395937506852)) ;
#45839 = CARTESIAN_POINT('Ctrl Pts',(-18.6454852083747,-25.3308755021684,
124.345063822644)) ;
#45840 = CARTESIAN_POINT('Ctrl Pts',(-18.4545445264848,-25.1508864218055,
124.578379945049)) ;
#45841 = CARTESIAN_POINT('Ctrl Pts',(-18.8179761803924,-25.3408122757461,
124.462875898515)) ;
#45842 = CARTESIAN_POINT('Ctrl Pts',(-18.6701593794825,-25.1608231953832,
124.72564450551)) ;
#45843 = CARTESIAN_POINT('Ctrl Pts',(-19.0091199998643,-25.3507953238871,
124.549608305468)) ;
#45844 = CARTESIAN_POINT('Ctrl Pts',(-18.9090898746252,-25.1708062435242,
124.834059046402)) ;
#45845 = CARTESIAN_POINT('Ctrl Pts',(-19.2137039022557,-25.3608390314972,
124.601767255972)) ;
#45846 = CARTESIAN_POINT('Ctrl Pts',(-19.1648198261409,-25.1808499511343,
124.899256681723)) ;
#45847 = CARTESIAN_POINT('Ctrl Pts',(-19.4197410435178,-25.3706677246505,
124.617749119944)) ;
#45848 = CARTESIAN_POINT('Ctrl Pts',(-19.4223677819913,-25.1906786442876,
124.919232914373)) ;
#45849 = CARTESIAN_POINT('Ctrl Pts',(-19.6305293861476,-25.3807424737799,
124.597364532467)) ;
#45850 = CARTESIAN_POINT('Ctrl Pts',(-19.6858526790546,-25.200753393417,124.893750955826)) ;
#45851 = CARTESIAN_POINT('Ctrl Pts',(-19.8303729849827,-25.3906077995755,
124.541808861825)) ;
#45852 = CARTESIAN_POINT('Ctrl Pts',(-19.9356579462158,-25.2106187192126,
124.824304856564)) ;
#45853 = CARTESIAN_POINT('Ctrl Pts',(-20.0207155288672,-25.4006299739324,
124.451476082817)) ;
#45854 = CARTESIAN_POINT('Ctrl Pts',(-20.173585469303,-25.2206408935695,124.711387601586)) ;
#45855 = CARTESIAN_POINT('Ctrl Pts',(-20.1922659082655,-25.4106560271393,
124.328983469291)) ;
#45856 = CARTESIAN_POINT('Ctrl Pts',(-20.3880226560733,-25.2306669467765,
124.558270853384)) ;
#45857 = CARTESIAN_POINT('Ctrl Pts',(-20.3376209909237,-25.4205097239856,
124.181407992117)) ;
#45858 = CARTESIAN_POINT('Ctrl Pts',(-20.5697163878782,-25.2405206436227,
124.373799671678)) ;
#45859 = CARTESIAN_POINT('Ctrl Pts',(-20.4569372871272,-25.4304691287386,
124.009344969333)) ;
#45860 = CARTESIAN_POINT('Ctrl Pts',(-20.7188606913848,-25.2504800483757,
124.15871963452)) ;
#45861 = CARTESIAN_POINT('Ctrl Pts',(-20.5449097818086,-25.4405073744435,
123.817532980503)) ;
#45862 = CARTESIAN_POINT('Ctrl Pts',(-20.8288249195141,-25.2605182940806,
123.91895416316)) ;
#45863 = CARTESIAN_POINT('Ctrl Pts',(-20.5977398559491,-25.4503815586055,
123.616753729714)) ;
#45864 = CARTESIAN_POINT('Ctrl Pts',(-20.8948612313139,-25.2703924782426,
123.667978712676)) ;
#45865 = CARTESIAN_POINT('Ctrl Pts',(-20.6152318947396,-25.4604513417434,
123.405808054371)) ;
#45866 = CARTESIAN_POINT('Ctrl Pts',(-20.9167246661195,-25.2804622613806,
123.404296836379)) ;
#45867 = CARTESIAN_POINT('Ctrl Pts',(-20.5963934662247,-25.4702845967642,
123.199925169976)) ;
#45868 = CARTESIAN_POINT('Ctrl Pts',(-20.8931748950452,-25.2902955164013,
123.146942101532)) ;
#45869 = CARTESIAN_POINT('Ctrl Pts',(-20.5415866211297,-25.4803150228959,
122.99630793319)) ;
#45870 = CARTESIAN_POINT('Ctrl Pts',(-20.824664603496,-25.300325942533,122.892421113422)) ;
#45871 = CARTESIAN_POINT('Ctrl Pts',(-20.4516839654255,-25.4903466350829,
122.805521136802)) ;
#45872 = CARTESIAN_POINT('Ctrl Pts',(-20.7122848539056,-25.31035755472,122.653938383803)) ;
#45873 = CARTESIAN_POINT('Ctrl Pts',(-20.3328358727724,-25.5001763319375,
122.636482789407)) ;
#45874 = CARTESIAN_POINT('Ctrl Pts',(-20.5637225648046,-25.3201872515746,
122.442640422475)) ;
#45875 = CARTESIAN_POINT('Ctrl Pts',(-20.1844921702679,-25.51016577384,122.487819824173)) ;
#45876 = CARTESIAN_POINT('Ctrl Pts',(-20.3782914259255,-25.3301766934771,
122.2568129731)) ;
#45877 = CARTESIAN_POINT('Ctrl Pts',(-20.0113511337868,-25.5202096658556,
122.366957918595)) ;
#45878 = CARTESIAN_POINT('Ctrl Pts',(-20.1618642262399,-25.3402205854928,
122.105737145019)) ;
#45879 = CARTESIAN_POINT('Ctrl Pts',(-19.8242733803076,-25.5300312276249,
122.279578448375)) ;
#45880 = CARTESIAN_POINT('Ctrl Pts',(-19.9280150892264,-25.350042147262,121.996514020556)) ;
#45881 = CARTESIAN_POINT('Ctrl Pts',(-19.6206530982633,-25.5400667992491,
122.2243313612)) ;
#45882 = CARTESIAN_POINT('Ctrl Pts',(-19.6734892886853,-25.3600777188862,
121.927457195706)) ;
#45883 = CARTESIAN_POINT('Ctrl Pts',(-19.4106109576734,-25.5500960735309,
122.205921274925)) ;
#45884 = CARTESIAN_POINT('Ctrl Pts',(-19.4109364974854,-25.370106993168,121.904446478748)) ;
#45885 = CARTESIAN_POINT('Ctrl Pts',(-19.2046030647571,-25.5599299106495,
122.22335172287)) ;
#45886 = CARTESIAN_POINT('Ctrl Pts',(-19.153425698316,-25.3799408302867,121.92623667871)) ;
#45887 = CARTESIAN_POINT('Ctrl Pts',(-19.000259823004,-25.5699823067377,122.277212320983)) ;
#45888 = CARTESIAN_POINT('Ctrl Pts',(-18.8979973838901,-25.3899932263748,
121.99356443242)) ;
#45889 = CARTESIAN_POINT('Ctrl Pts',(-18.8106744902198,-25.5799190736882,
122.364971233025)) ;
#45890 = CARTESIAN_POINT('Ctrl Pts',(-18.6610161340933,-25.3999299933253,
122.103265136597)) ;
#45891 = CARTESIAN_POINT('Ctrl Pts',(-18.6389522732557,-25.5898533086675,
122.483834336028)) ;
#45892 = CARTESIAN_POINT('Ctrl Pts',(-18.4463642084405,-25.4098642283046,
122.251846102408)) ;
#45893 = CARTESIAN_POINT('Ctrl Pts',(-18.4892297183612,-25.5998770719943,
122.632124416292)) ;
#45894 = CARTESIAN_POINT('Ctrl Pts',(-18.2592125481551,-25.4198879916314,
122.437210228712)) ;
#45895 = CARTESIAN_POINT('Ctrl Pts',(-18.3690729527359,-25.6097634133789,
122.801712077461)) ;
#45896 = CARTESIAN_POINT('Ctrl Pts',(-18.1090179641426,-25.429774333016,122.649196677396)) ;
#45897 = CARTESIAN_POINT('Ctrl Pts',(-18.2788188736161,-25.6197524621459,
122.991336888981)) ;
#45898 = CARTESIAN_POINT('Ctrl Pts',(-17.9962023976865,-25.439763381783,122.886228834323)) ;
#45899 = CARTESIAN_POINT('Ctrl Pts',(-18.2229938244163,-25.6297936828433,
123.194918820965)) ;
#45900 = CARTESIAN_POINT('Ctrl Pts',(-17.92642324804,-25.4498046024804,123.140706746069)) ;
#45901 = CARTESIAN_POINT('Ctrl Pts',(-18.2034358522084,-25.6396263230212,
123.400700722428)) ;
#45902 = CARTESIAN_POINT('Ctrl Pts',(-17.9019779830715,-25.4596372426583,
123.397935296118)) ;
#45903 = CARTESIAN_POINT('Ctrl Pts',(-18.2195753607672,-25.6496202523291,
123.610182629394)) ;
#45904 = CARTESIAN_POINT('Ctrl Pts',(-17.9221548130397,-25.4696311719663,
123.659787613403)) ;
#45905 = CARTESIAN_POINT('Ctrl Pts',(-18.2724604743426,-25.6596494600097,
123.814289690547)) ;
#45906 = CARTESIAN_POINT('Ctrl Pts',(-17.9882634627547,-25.4796603796468,
123.914920831953)) ;
#45907 = CARTESIAN_POINT('Ctrl Pts',(-18.358339643957,-25.6695252717138,124.003328990778)) ;
#45908 = CARTESIAN_POINT('Ctrl Pts',(-18.095614902813,-25.4895361913509,124.151219574805)) ;
#45909 = CARTESIAN_POINT('Ctrl Pts',(-18.4769919261622,-25.6795244986852,
124.176823257226)) ;
#45910 = CARTESIAN_POINT('Ctrl Pts',(-18.243932354423,-25.4995354183223,124.368086107195)) ;
#45911 = CARTESIAN_POINT('Ctrl Pts',(-18.6225453670208,-25.6894339798409,
124.325912667589)) ;
#45912 = CARTESIAN_POINT('Ctrl Pts',(-18.4258762775159,-25.509444899478,124.554446462771)) ;
#45913 = CARTESIAN_POINT('Ctrl Pts',(-18.7942023877807,-25.6994872101418,
124.449174674582)) ;
#45914 = CARTESIAN_POINT('Ctrl Pts',(-18.6404489287507,-25.5194981297789,
124.708521879958)) ;
#45915 = CARTESIAN_POINT('Ctrl Pts',(-18.9811834854639,-25.7093578266928,
124.539201485248)) ;
#45916 = CARTESIAN_POINT('Ctrl Pts',(-18.8741769469546,-25.52936874633,124.821053391255)) ;
#45917 = CARTESIAN_POINT('Ctrl Pts',(-19.1838697790237,-25.7193794884249,
124.596699644364)) ;
#45918 = CARTESIAN_POINT('Ctrl Pts',(-19.127535526737,-25.539390408062,124.892923586668)) ;
#45919 = CARTESIAN_POINT('Ctrl Pts',(-19.3935471693339,-25.729402301606,124.617654797258)) ;
#45920 = CARTESIAN_POINT('Ctrl Pts',(-19.3896325300281,-25.5494132212431,
124.919115026202)) ;
#45921 = CARTESIAN_POINT('Ctrl Pts',(-19.6004203943415,-25.7392694660659,
124.60247790701)) ;
#45922 = CARTESIAN_POINT('Ctrl Pts',(-19.6482244565105,-25.5592803857031,
124.900141299359)) ;
#45923 = CARTESIAN_POINT('Ctrl Pts',(-19.804222528808,-25.7492629082859,124.551424075459)) ;
#45924 = CARTESIAN_POINT('Ctrl Pts',(-19.902976585568,-25.569273827923,124.83632140457)) ;
#45925 = CARTESIAN_POINT('Ctrl Pts',(-19.9966241110481,-25.7592945818862,
124.465058729289)) ;
#45926 = CARTESIAN_POINT('Ctrl Pts',(-20.1434775002714,-25.5793055015233,
124.728362358273)) ;
#45927 = CARTESIAN_POINT('Ctrl Pts',(-20.1684200868147,-25.7691610169992,
124.348807750651)) ;
#45928 = CARTESIAN_POINT('Ctrl Pts',(-20.3582214202011,-25.5891719366363,
124.583046155646)) ;
#45929 = CARTESIAN_POINT('Ctrl Pts',(-20.3194620562051,-25.7791484675323,
124.202992595232)) ;
#45930 = CARTESIAN_POINT('Ctrl Pts',(-20.5470220993217,-25.5991593871694,
124.400775187836)) ;
#45931 = CARTESIAN_POINT('Ctrl Pts',(-20.4424893830337,-25.7890933973602,
124.033909844264)) ;
#45932 = CARTESIAN_POINT('Ctrl Pts',(-20.7008042109663,-25.6091043169973,
124.189419968421)) ;
#45933 = CARTESIAN_POINT('Ctrl Pts',(-20.5350834451132,-25.7991382924153,
123.844138661879)) ;
#45934 = CARTESIAN_POINT('Ctrl Pts',(-20.8165443609091,-25.6191492120525,
123.952204828847)) ;
#45935 = CARTESIAN_POINT('Ctrl Pts',(-20.5924455699357,-25.8090003541012,
123.64488433114)) ;
#45936 = CARTESIAN_POINT('Ctrl Pts',(-20.8882445301737,-25.6290112737383,
123.70313575114)) ;
#45937 = CARTESIAN_POINT('Ctrl Pts',(-20.6150418051958,-25.818992076888,123.436062409259)) ;
#45938 = CARTESIAN_POINT('Ctrl Pts',(-20.9164870894924,-25.6390029965252,
123.442107956851)) ;
#45939 = CARTESIAN_POINT('Ctrl Pts',(-20.6010425706833,-25.828924291128,123.22772327375)) ;
#45940 = CARTESIAN_POINT('Ctrl Pts',(-20.8989852870473,-25.6489352107651,
123.181683998695)) ;
#45941 = CARTESIAN_POINT('Ctrl Pts',(-20.5515128182878,-25.8388636096937,
123.024716518231)) ;
#45942 = CARTESIAN_POINT('Ctrl Pts',(-20.8370703423436,-25.6588745293309,
122.927926047669)) ;
#45943 = CARTESIAN_POINT('Ctrl Pts',(-20.4664264572267,-25.8489077844696,
122.831461041933)) ;
#45944 = CARTESIAN_POINT('Ctrl Pts',(-20.7307098426691,-25.6689187041067,
122.686357803622)) ;
#45945 = CARTESIAN_POINT('Ctrl Pts',(-20.3511977884892,-25.8587783385346,
122.658884676041)) ;
#45946 = CARTESIAN_POINT('Ctrl Pts',(-20.5866715410215,-25.6787892581717,
122.47063867262)) ;
#45947 = CARTESIAN_POINT('Ctrl Pts',(-20.2068205658345,-25.8687433208888,
122.507083215677)) ;
#45948 = CARTESIAN_POINT('Ctrl Pts',(-20.4061979028758,-25.6887542405259,
122.280888722177)) ;
#45949 = CARTESIAN_POINT('Ctrl Pts',(-20.0369803709032,-25.8787740237786,
122.382099598688)) ;
#45950 = CARTESIAN_POINT('Ctrl Pts',(-20.1938959519348,-25.6987849434157,
122.124661424676)) ;
#45951 = CARTESIAN_POINT('Ctrl Pts',(-19.8507320191725,-25.8886663638038,
122.289510710408)) ;
#45952 = CARTESIAN_POINT('Ctrl Pts',(-19.9610841220414,-25.7086772834409,
122.008927766554)) ;
#45953 = CARTESIAN_POINT('Ctrl Pts',(-19.6480507991876,-25.8987195969637,
122.229703855428)) ;
#45954 = CARTESIAN_POINT('Ctrl Pts',(-19.7077317559287,-25.7187305166009,
121.934171888619)) ;
#45955 = CARTESIAN_POINT('Ctrl Pts',(-19.4416056541742,-25.9086008414405,
122.206269923725)) ;
#45956 = CARTESIAN_POINT('Ctrl Pts',(-19.4496748815431,-25.7286117610776,
121.904882259363)) ;
#45957 = CARTESIAN_POINT('Ctrl Pts',(-19.2311053037005,-25.9186339623115,
122.219073769285)) ;
#45958 = CARTESIAN_POINT('Ctrl Pts',(-19.1865495494831,-25.7386448819486,
121.920889891667)) ;
#45959 = CARTESIAN_POINT('Ctrl Pts',(-19.0290124695695,-25.9285151725866,
122.267326061068)) ;
#45960 = CARTESIAN_POINT('Ctrl Pts',(-18.933934095788,-25.7485260922237,121.981208015015)) ;
#45961 = CARTESIAN_POINT('Ctrl Pts',(-18.8349223161673,-25.9385772483559,
122.351365482574)) ;
#45962 = CARTESIAN_POINT('Ctrl Pts',(-18.6913224502721,-25.758588167993,122.086259918764)) ;
#45963 = CARTESIAN_POINT('Ctrl Pts',(-18.6618773393018,-25.9484343067377,
122.465428901543)) ;
#45964 = CARTESIAN_POINT('Ctrl Pts',(-18.4750177696445,-25.7684452263748,
122.228841554689)) ;
#45965 = CARTESIAN_POINT('Ctrl Pts',(-18.508920686306,-25.9584288620267,122.609440179343)) ;
#45966 = CARTESIAN_POINT('Ctrl Pts',(-18.2838238477272,-25.7784397816638,
122.408857735709)) ;
#45967 = CARTESIAN_POINT('Ctrl Pts',(-18.3840592104564,-25.9683547495622,
122.776670958682)) ;
#45968 = CARTESIAN_POINT('Ctrl Pts',(-18.1277492566093,-25.7883656691993,
122.617897877619)) ;
#45969 = CARTESIAN_POINT('Ctrl Pts',(-18.2891587151755,-25.9783797695574,
122.964835760839)) ;
#45970 = CARTESIAN_POINT('Ctrl Pts',(-18.0091260993972,-25.7983906891946,
122.853105228335)) ;
#45971 = CARTESIAN_POINT('Ctrl Pts',(-18.2290682932492,-25.9882771466611,
123.164050381415)) ;
#45972 = CARTESIAN_POINT('Ctrl Pts',(-17.9340157762588,-25.8082880662982,
123.102124235181)) ;
#45973 = CARTESIAN_POINT('Ctrl Pts',(-18.2037946806714,-25.998267383742,123.3725562714)) ;
#45974 = CARTESIAN_POINT('Ctrl Pts',(-17.9024264992633,-25.8182783033791,
123.362756958186)) ;
#45975 = CARTESIAN_POINT('Ctrl Pts',(-18.2155658880432,-26.0083039965508,
123.583225928318)) ;
#45976 = CARTESIAN_POINT('Ctrl Pts',(-17.9171433202812,-25.8283149161879,
123.62609402293)) ;
#45977 = CARTESIAN_POINT('Ctrl Pts',(-18.2625157876823,-26.0181538799688,
123.784916905059)) ;
#45978 = CARTESIAN_POINT('Ctrl Pts',(-17.9758333009536,-25.8381647996059,
123.878206838358)) ;
#45979 = CARTESIAN_POINT('Ctrl Pts',(-18.3446404620089,-26.0281574968712,
123.978504100519)) ;
#45980 = CARTESIAN_POINT('Ctrl Pts',(-18.0784917995666,-25.8481684165084,
124.120189945079)) ;
#45981 = CARTESIAN_POINT('Ctrl Pts',(-18.4590946254507,-26.0381469086364,
124.154624318019)) ;
#45982 = CARTESIAN_POINT('Ctrl Pts',(-18.2215613397651,-25.8581578282735,
124.340338256903)) ;
#45983 = CARTESIAN_POINT('Ctrl Pts',(-18.6028685076964,-26.0481656699812,
124.308517074879)) ;
#45984 = CARTESIAN_POINT('Ctrl Pts',(-18.4012825635189,-25.8681765896183,
124.532704279284)) ;
#45985 = CARTESIAN_POINT('Ctrl Pts',(-18.8247544491437,-26.0613843453623,
124.475917456974)) ;
#45986 = CARTESIAN_POINT('Ctrl Pts',(-18.6786331146531,-25.8813952649994,
124.7419424)) ;
#45987 = CARTESIAN_POINT('Ctrl Pts',(-19.0869231326057,-26.074694652607,124.582399606467)) ;
#45988 = CARTESIAN_POINT('Ctrl Pts',(-19.0063037436624,-25.8947055722441,
124.875037990649)) ;
#45989 = CARTESIAN_POINT('Ctrl Pts',(-19.363072798974,-26.087932318833,124.616808325891)) ;
#45990 = CARTESIAN_POINT('Ctrl Pts',(-19.3515492793032,-25.9079432384701,
124.918059062423)) ;
#45991 = CARTESIAN_POINT('Ctrl Pts',(-19.5713918157783,-26.0978520142437,
124.606935546831)) ;
#45992 = CARTESIAN_POINT('Ctrl Pts',(-19.6119358669547,-25.9178629338808,
124.905712873478)) ;
#45993 = CARTESIAN_POINT('Ctrl Pts',(-19.7774861802108,-26.1079048812422,
124.560193148227)) ;
#45994 = CARTESIAN_POINT('Ctrl Pts',(-19.8695568706956,-25.9279158008794,
124.847282646854)) ;
#45995 = CARTESIAN_POINT('Ctrl Pts',(-19.9686281474796,-26.1177602895715,
124.480186051397)) ;
#45996 = CARTESIAN_POINT('Ctrl Pts',(-20.1084811470634,-25.9377712092086,
124.747272818571)) ;
#45997 = CARTESIAN_POINT('Ctrl Pts',(-20.14637377885,-26.1277989212481,124.366438520996)) ;
#45998 = CARTESIAN_POINT('Ctrl Pts',(-20.3306652047621,-25.9478098408852,
124.60508116567)) ;
#45999 = CARTESIAN_POINT('Ctrl Pts',(-20.3519626171017,-26.1411011035151,
124.176812384291)) ;
#46000 = CARTESIAN_POINT('Ctrl Pts',(-20.5876341488702,-25.9611120231522,
124.368071353018)) ;
#46001 = CARTESIAN_POINT('Ctrl Pts',(-20.5406207798638,-26.157646116598,123.879908726874)) ;
#46002 = CARTESIAN_POINT('Ctrl Pts',(-20.8234715239028,-25.9776570362351,
123.996893725382)) ;
#46003 = CARTESIAN_POINT('Ctrl Pts',(-20.6172088047157,-26.1742981326742,
123.534214772238)) ;
#46004 = CARTESIAN_POINT('Ctrl Pts',(-20.9191905979447,-25.9943090523113,
123.56485434143)) ;
#46005 = CARTESIAN_POINT('Ctrl Pts',(-20.6051217054238,-26.1875212235794,
123.256506578879)) ;
#46006 = CARTESIAN_POINT('Ctrl Pts',(-20.9040855806235,-26.0075321432166,
123.217655815596)) ;
#46007 = CARTESIAN_POINT('Ctrl Pts',(-20.5603924279369,-26.1974821831388,
123.05192147308)) ;
#46008 = CARTESIAN_POINT('Ctrl Pts',(-20.8481710288913,-26.0174931027759,
122.961938491828)) ;
#46009 = CARTESIAN_POINT('Ctrl Pts',(-20.4800725687243,-26.2075069798899,
122.857083849691)) ;
#46010 = CARTESIAN_POINT('Ctrl Pts',(-20.7477672743641,-26.027517899527,122.718386742879)) ;
#46011 = CARTESIAN_POINT('Ctrl Pts',(-20.3313987181556,-26.2207314272857,
122.62210740137)) ;
#46012 = CARTESIAN_POINT('Ctrl Pts',(-20.561933381812,-26.0407423469228,122.424679164752)) ;
#46013 = CARTESIAN_POINT('Ctrl Pts',(-20.0717140768469,-26.2373652119848,
122.382085717408)) ;
#46014 = CARTESIAN_POINT('Ctrl Pts',(-20.2373134506599,-26.0573761316219,
122.124643357412)) ;
#46015 = CARTESIAN_POINT('Ctrl Pts',(-19.6815099293272,-26.2572678787097,
122.218198924247)) ;
#46016 = CARTESIAN_POINT('Ctrl Pts',(-19.7495611853889,-26.0772787983468,
121.919792632271)) ;
#46017 = CARTESIAN_POINT('Ctrl Pts',(-19.2589510713564,-26.2771681064916,
122.196756051272)) ;
#46018 = CARTESIAN_POINT('Ctrl Pts',(-19.22136228124,-26.0971790261287,121.892991857284)) ;
#46019 = CARTESIAN_POINT('Ctrl Pts',(-18.8539777559444,-26.2970855940231,
122.320631928225)) ;
#46020 = CARTESIAN_POINT('Ctrl Pts',(-18.715147674176,-26.1170965136602,122.047840068895)) ;
#46021 = CARTESIAN_POINT('Ctrl Pts',(-18.5152044782925,-26.31701511984,122.575227475119)) ;
#46022 = CARTESIAN_POINT('Ctrl Pts',(-18.2916834899083,-26.1370260394771,
122.366086543322)) ;
#46023 = CARTESIAN_POINT('Ctrl Pts',(-18.2833320361407,-26.3369773877262,
122.930774152276)) ;
#46024 = CARTESIAN_POINT('Ctrl Pts',(-18.0018457091614,-26.1569883073634,
122.810521281011)) ;
#46025 = CARTESIAN_POINT('Ctrl Pts',(-18.187043146482,-26.3568675826784,123.342528444568)) ;
#46026 = CARTESIAN_POINT('Ctrl Pts',(-17.8814876928622,-26.1768785023156,
123.325213587121)) ;
#46027 = CARTESIAN_POINT('Ctrl Pts',(-18.2360005587426,-26.3767578274247,
123.762699469235)) ;
#46028 = CARTESIAN_POINT('Ctrl Pts',(-17.942686360803,-26.1967687470618,123.850425839036)) ;
#46029 = CARTESIAN_POINT('Ctrl Pts',(-18.4278756911333,-26.3968321999872,
124.143912754518)) ;
#46030 = CARTESIAN_POINT('Ctrl Pts',(-18.182532872639,-26.2168431196243,124.326942241085)) ;
#46031 = CARTESIAN_POINT('Ctrl Pts',(-18.7338400806782,-26.4166175773475,
124.432727082962)) ;
#46032 = CARTESIAN_POINT('Ctrl Pts',(-18.5649877790472,-26.2366284969846,
124.687956672163)) ;
#46033 = CARTESIAN_POINT('Ctrl Pts',(-19.1228257813227,-26.4365794514146,
124.602461953777)) ;
#46034 = CARTESIAN_POINT('Ctrl Pts',(-19.0512197803277,-26.2565903710517,
124.900124064153)) ;
#46035 = CARTESIAN_POINT('Ctrl Pts',(-19.5468805261724,-26.4565594269051,
124.628280549384)) ;
#46036 = CARTESIAN_POINT('Ctrl Pts',(-19.5812880978387,-26.2765703465422,
124.932395779744)) ;
#46037 = CARTESIAN_POINT('Ctrl Pts',(-19.9511224656437,-26.476371856783,124.509636259826)) ;
#46038 = CARTESIAN_POINT('Ctrl Pts',(-20.0865875254388,-26.2963827764202,
124.784090581285)) ;
#46039 = CARTESIAN_POINT('Ctrl Pts',(-20.2937255390238,-26.4963519648733,
124.258562719939)) ;
#46040 = CARTESIAN_POINT('Ctrl Pts',(-20.5148410357087,-26.3163628845105,
124.470248873448)) ;
#46041 = CARTESIAN_POINT('Ctrl Pts',(-20.5290130856317,-26.5162463484706,
123.906914863893)) ;
#46042 = CARTESIAN_POINT('Ctrl Pts',(-20.8089496480924,-26.3362572681077,
124.030690459046)) ;
#46043 = CARTESIAN_POINT('Ctrl Pts',(-20.6306703899268,-26.5361732764478,
123.495687774504)) ;
#46044 = CARTESIAN_POINT('Ctrl Pts',(-20.9360216455939,-26.3561841960849,
123.516657893152)) ;
#46045 = CARTESIAN_POINT('Ctrl Pts',(-20.58650883794,-26.556068133749,123.074882964739)) ;
#46046 = CARTESIAN_POINT('Ctrl Pts',(-20.8808211228342,-26.3760790533862,
122.990653193015)) ;
#46047 = CARTESIAN_POINT('Ctrl Pts',(-20.3997314232741,-26.5761073273527,
122.691961278104)) ;
#46048 = CARTESIAN_POINT('Ctrl Pts',(-20.647350202661,-26.3961182469898,122.512000068605)) ;
#46049 = CARTESIAN_POINT('Ctrl Pts',(-20.0964143874877,-26.5959472952634,
122.39871350997)) ;
#46050 = CARTESIAN_POINT('Ctrl Pts',(-20.2682064549475,-26.4159582149006,
122.145440895336)) ;
#46051 = CARTESIAN_POINT('Ctrl Pts',(-19.7103017728837,-26.6158621122275,
122.224956806707)) ;
#46052 = CARTESIAN_POINT('Ctrl Pts',(-19.7855675978371,-26.4358730318646,
121.928243360252)) ;
#46053 = CARTESIAN_POINT('Ctrl Pts',(-19.2874660199691,-26.6358043576238,
122.193640512695)) ;
#46054 = CARTESIAN_POINT('Ctrl Pts',(-19.2570238059739,-26.4558152772609,
121.889095738746)) ;
#46055 = CARTESIAN_POINT('Ctrl Pts',(-18.8804463278445,-26.6556764057383,
122.30743483587)) ;
#46056 = CARTESIAN_POINT('Ctrl Pts',(-18.748249738879,-26.4756873253754,122.031335489932)) ;
#46057 = CARTESIAN_POINT('Ctrl Pts',(-18.534656096257,-26.6756874706924,122.555130633679)) ;
#46058 = CARTESIAN_POINT('Ctrl Pts',(-18.3160101803626,-26.4956983903295,
122.340952921604)) ;
#46059 = CARTESIAN_POINT('Ctrl Pts',(-18.2958118938891,-26.695498994996,122.902353695436)) ;
#46060 = CARTESIAN_POINT('Ctrl Pts',(-18.0174531568864,-26.5155099146331,
122.774978345867)) ;
#46061 = CARTESIAN_POINT('Ctrl Pts',(-18.1886180442207,-26.7155942069594,
123.315793755655)) ;
#46062 = CARTESIAN_POINT('Ctrl Pts',(-17.883457283048,-26.5356051265965,123.29177843999)) ;
#46063 = CARTESIAN_POINT('Ctrl Pts',(-18.2284182206714,-26.7353749308792,
123.734667026007)) ;
#46064 = CARTESIAN_POINT('Ctrl Pts',(-17.9332038026506,-26.5553858505163,
123.815368387734)) ;
#46065 = CARTESIAN_POINT('Ctrl Pts',(-18.4096610154177,-26.755366006522,124.118979626269)) ;
#46066 = CARTESIAN_POINT('Ctrl Pts',(-18.1597535329976,-26.5753769261591,
124.295760856938)) ;
#46067 = CARTESIAN_POINT('Ctrl Pts',(-18.7099242034501,-26.775247945565,124.416730191879)) ;
#46068 = CARTESIAN_POINT('Ctrl Pts',(-18.5350790245251,-26.5952588652021,
124.667951356014)) ;
#46069 = CARTESIAN_POINT('Ctrl Pts',(-19.0947640893078,-26.7952005500682,
124.595125233846)) ;
#46070 = CARTESIAN_POINT('Ctrl Pts',(-19.0161267182173,-26.6152114697054,
124.89094908574)) ;
#46071 = CARTESIAN_POINT('Ctrl Pts',(-19.5163545803771,-26.8150994187989,
124.631394180349)) ;
#46072 = CARTESIAN_POINT('Ctrl Pts',(-19.5431138580635,-26.635110338436,124.936289536443)) ;
#46073 = CARTESIAN_POINT('Ctrl Pts',(-19.9249223900067,-26.8349928186085,
124.522185577163)) ;
#46074 = CARTESIAN_POINT('Ctrl Pts',(-20.0538241489415,-26.6550037382456,
124.799784245693)) ;
#46075 = CARTESIAN_POINT('Ctrl Pts',(-20.2724780813472,-26.8549019494485,
124.28036241543)) ;
#46076 = CARTESIAN_POINT('Ctrl Pts',(-20.4882718449817,-26.6749128690856,
124.497507103209)) ;
#46077 = CARTESIAN_POINT('Ctrl Pts',(-20.5176077328645,-26.8749340492121,
123.93208451665)) ;
#46078 = CARTESIAN_POINT('Ctrl Pts',(-20.7946862216762,-26.6949449688492,
124.062171882771)) ;
#46079 = CARTESIAN_POINT('Ctrl Pts',(-20.6098098899142,-26.8914661223815,
123.592826429201)) ;
#46080 = CARTESIAN_POINT('Ctrl Pts',(-20.9099487231253,-26.7114770420187,
123.638071483004)) ;
#46081 = CARTESIAN_POINT('Ctrl Pts',(-20.6110911401444,-26.9048014629875,
123.312495899499)) ;
#46082 = CARTESIAN_POINT('Ctrl Pts',(-20.9115489477632,-26.7248123826246,
123.287684923675)) ;
#46083 = CARTESIAN_POINT('Ctrl Pts',(-20.5764556782728,-26.9146440215272,
123.108474267684)) ;
#46084 = CARTESIAN_POINT('Ctrl Pts',(-20.8682561091955,-26.7346549411643,
123.032650001442)) ;
#46085 = CARTESIAN_POINT('Ctrl Pts',(-20.505658826445,-26.9246959283771,122.909381601415)) ;
#46086 = CARTESIAN_POINT('Ctrl Pts',(-20.77977083026,-26.7447068480142,122.78379500435)) ;
#46087 = CARTESIAN_POINT('Ctrl Pts',(-20.3681524800132,-26.937944442768,122.66718118586)) ;
#46088 = CARTESIAN_POINT('Ctrl Pts',(-20.6078481493321,-26.7579553624051,
122.480989791618)) ;
#46089 = CARTESIAN_POINT('Ctrl Pts',(-20.1207621070725,-26.9545436177157,
122.415419343604)) ;
#46090 = CARTESIAN_POINT('Ctrl Pts',(-20.2986718809481,-26.7745545373529,
122.166348506659)) ;
#46091 = CARTESIAN_POINT('Ctrl Pts',(-19.8026232747545,-26.9711324035108,
122.26320952748)) ;
#46092 = CARTESIAN_POINT('Ctrl Pts',(-19.9009478345017,-26.7911433231479,
121.976048097058)) ;
#46093 = CARTESIAN_POINT('Ctrl Pts',(-19.5282752383854,-26.9844082198528,
122.211739570841)) ;
#46094 = CARTESIAN_POINT('Ctrl Pts',(-19.5580496300445,-26.8044191394899,
121.911724128209)) ;
#46095 = CARTESIAN_POINT('Ctrl Pts',(-19.318603845964,-26.9943820706466,122.209154533502)) ;
#46096 = CARTESIAN_POINT('Ctrl Pts',(-19.2959531359205,-26.8143929902837,
121.908486613091)) ;
#46097 = CARTESIAN_POINT('Ctrl Pts',(-19.1105694524777,-27.004411102739,122.243420895193)) ;
#46098 = CARTESIAN_POINT('Ctrl Pts',(-19.0359115386452,-26.8244220223761,
121.951317775132)) ;
#46099 = CARTESIAN_POINT('Ctrl Pts',(-18.9143115037935,-27.0143012282409,
122.3121202507)) ;
#46100 = CARTESIAN_POINT('Ctrl Pts',(-18.7905877643252,-26.834312147878,122.037189062032)) ;
#46101 = CARTESIAN_POINT('Ctrl Pts',(-18.730980558228,-27.0242937065124,122.414640859144)) ;
#46102 = CARTESIAN_POINT('Ctrl Pts',(-18.5614228030226,-26.8443046261495,
122.165337470072)) ;
#46103 = CARTESIAN_POINT('Ctrl Pts',(-18.5687919015397,-27.0342449216098,
122.546836923164)) ;
#46104 = CARTESIAN_POINT('Ctrl Pts',(-18.3586851596353,-26.8542558412469,
122.330580371171)) ;
#46105 = CARTESIAN_POINT('Ctrl Pts',(-18.4308500276103,-27.0442934233648,
122.706804310669)) ;
#46106 = CARTESIAN_POINT('Ctrl Pts',(-18.1862556413636,-26.8643043430019,
122.530537857795)) ;
#46107 = CARTESIAN_POINT('Ctrl Pts',(-18.324778682574,-27.0541347729816,122.884464775646)) ;
#46108 = CARTESIAN_POINT('Ctrl Pts',(-18.0536640724743,-26.8741456926187,
122.752611956706)) ;
#46109 = CARTESIAN_POINT('Ctrl Pts',(-18.2496811215229,-27.0641210640018,
123.080480376407)) ;
#46110 = CARTESIAN_POINT('Ctrl Pts',(-17.9597894559771,-26.8841319836389,
122.997630523713)) ;
#46111 = CARTESIAN_POINT('Ctrl Pts',(-18.2098424384287,-27.0740576757304,
123.285580848838)) ;
#46112 = CARTESIAN_POINT('Ctrl Pts',(-17.9099883261813,-26.8940685953675,
123.254005646133)) ;
#46113 = CARTESIAN_POINT('Ctrl Pts',(-18.206286456587,-27.084107551098,123.496809557806)) ;
#46114 = CARTESIAN_POINT('Ctrl Pts',(-17.9055405282516,-26.9041184707351,
123.518041545854)) ;
#46115 = CARTESIAN_POINT('Ctrl Pts',(-18.2386548673565,-27.0939580096334,
123.701367310787)) ;
#46116 = CARTESIAN_POINT('Ctrl Pts',(-17.9459982769325,-26.9139689292705,
123.7737392886)) ;
#46117 = CARTESIAN_POINT('Ctrl Pts',(-18.3063479731576,-27.1039299465862,
123.899751686817)) ;
#46118 = CARTESIAN_POINT('Ctrl Pts',(-18.0306120394359,-26.9239408662233,
124.021720774531)) ;
#46119 = CARTESIAN_POINT('Ctrl Pts',(-18.4077546179831,-27.1139254035183,
124.083836779179)) ;
#46120 = CARTESIAN_POINT('Ctrl Pts',(-18.1573679303231,-26.9339363231554,
124.251828560722)) ;
#46121 = CARTESIAN_POINT('Ctrl Pts',(-18.5402337139463,-27.1239582105714,
124.247943977524)) ;
#46122 = CARTESIAN_POINT('Ctrl Pts',(-18.3229646348335,-26.9439691302085,
124.456964358552)) ;
#46123 = CARTESIAN_POINT('Ctrl Pts',(-18.696288367492,-27.1338180971613,124.384394875918)) ;
#46124 = CARTESIAN_POINT('Ctrl Pts',(-18.5180312778613,-26.9538290167985,
124.627530238962)) ;
#46125 = CARTESIAN_POINT('Ctrl Pts',(-18.8757602839204,-27.1438071777266,
124.493403942456)) ;
#46126 = CARTESIAN_POINT('Ctrl Pts',(-18.7423698226788,-26.9638180973637,
124.763794005457)) ;
#46127 = CARTESIAN_POINT('Ctrl Pts',(-19.0703285555277,-27.1537386569357,
124.569162296289)) ;
#46128 = CARTESIAN_POINT('Ctrl Pts',(-18.9855793301611,-26.9737495765729,
124.858494603905)) ;
#46129 = CARTESIAN_POINT('Ctrl Pts',(-19.2761569854026,-27.1637245163817,
124.610551053502)) ;
#46130 = CARTESIAN_POINT('Ctrl Pts',(-19.2428644372235,-26.9837354360188,
124.910233267454)) ;
#46131 = CARTESIAN_POINT('Ctrl Pts',(-19.4871247300181,-27.1737626670289,
124.61522608717)) ;
#46132 = CARTESIAN_POINT('Ctrl Pts',(-19.5065740592286,-26.993773586666,124.916079842677)) ;
#46133 = CARTESIAN_POINT('Ctrl Pts',(-19.6918470853474,-27.1836107575333,
124.584217748348)) ;
#46134 = CARTESIAN_POINT('Ctrl Pts',(-19.7624778086568,-27.0036216771704,
124.877322071397)) ;
#46135 = CARTESIAN_POINT('Ctrl Pts',(-19.8923339922519,-27.1936716660512,
124.516888561277)) ;
#46136 = CARTESIAN_POINT('Ctrl Pts',(-20.0130872707028,-27.0136825856884,
124.793163184846)) ;
#46137 = CARTESIAN_POINT('Ctrl Pts',(-20.0749863200746,-27.2035665132092,
124.417294329767)) ;
#46138 = CARTESIAN_POINT('Ctrl Pts',(-20.2414042796906,-27.0235774328464,
124.668672645301)) ;
#46139 = CARTESIAN_POINT('Ctrl Pts',(-20.2386525978464,-27.2135081852543,
124.287347778684)) ;
#46140 = CARTESIAN_POINT('Ctrl Pts',(-20.4459889974729,-27.0335191048914,
124.506241389245)) ;
#46141 = CARTESIAN_POINT('Ctrl Pts',(-20.3782156387396,-27.2235107123797,
124.130014539962)) ;
#46142 = CARTESIAN_POINT('Ctrl Pts',(-20.6204448444618,-27.0435216320169,
124.309576543544)) ;
#46143 = CARTESIAN_POINT('Ctrl Pts',(-20.4883897656227,-27.2335455035672,
123.950121732222)) ;
#46144 = CARTESIAN_POINT('Ctrl Pts',(-20.758164805552,-27.0535564232043,124.084711962413)) ;
#46145 = CARTESIAN_POINT('Ctrl Pts',(-20.5645263195821,-27.2433903834263,
123.757649358259)) ;
#46146 = CARTESIAN_POINT('Ctrl Pts',(-20.8533381771542,-27.0634013030634,
123.8441219504)) ;
#46147 = CARTESIAN_POINT('Ctrl Pts',(-20.6070596189447,-27.2533762640448,
123.552103054265)) ;
#46148 = CARTESIAN_POINT('Ctrl Pts',(-20.9065073830601,-27.0733871836819,
123.587189440378)) ;
#46149 = CARTESIAN_POINT('Ctrl Pts',(-20.6133781384881,-27.263310987138,123.343300034861)) ;
#46150 = CARTESIAN_POINT('Ctrl Pts',(-20.9144081114304,-27.0833219067751,
123.326185418482)) ;
#46151 = CARTESIAN_POINT('Ctrl Pts',(-20.5827915728053,-27.2733688274492,
123.134108713238)) ;
#46152 = CARTESIAN_POINT('Ctrl Pts',(-20.8761775034525,-27.0933797470863,
123.064696003703)) ;
#46153 = CARTESIAN_POINT('Ctrl Pts',(-20.5182131701365,-27.2831893148457,
122.937983170637)) ;
#46154 = CARTESIAN_POINT('Ctrl Pts',(-20.7954566740253,-27.1032002344828,
122.819537535272)) ;
#46155 = CARTESIAN_POINT('Ctrl Pts',(-20.4185100813219,-27.2932497161908,
122.751485493187)) ;
#46156 = CARTESIAN_POINT('Ctrl Pts',(-20.6708300595228,-27.1132606358279,
122.586414372848)) ;
#46157 = CARTESIAN_POINT('Ctrl Pts',(-20.2893670926231,-27.3031806817437,
122.587408843276)) ;
#46158 = CARTESIAN_POINT('Ctrl Pts',(-20.5094030853154,-27.1231916013808,
122.381316698631)) ;
#46159 = CARTESIAN_POINT('Ctrl Pts',(-20.1339171194866,-27.3131195440802,
122.447821260435)) ;
#46160 = CARTESIAN_POINT('Ctrl Pts',(-20.3150919759397,-27.1331304637173,
122.206830149708)) ;
#46161 = CARTESIAN_POINT('Ctrl Pts',(-19.9557909141703,-27.3231052750064,
122.336681000777)) ;
#46162 = CARTESIAN_POINT('Ctrl Pts',(-20.0924353593602,-27.1431161946435,
122.067902692524)) ;
#46163 = CARTESIAN_POINT('Ctrl Pts',(-19.7602720484493,-27.3331296604338,
122.258075382976)) ;
#46164 = CARTESIAN_POINT('Ctrl Pts',(-19.8480377025175,-27.1531405800709,
121.969643385179)) ;
#46165 = CARTESIAN_POINT('Ctrl Pts',(-19.5565899889511,-27.3430329447871,
122.214817299832)) ;
#46166 = CARTESIAN_POINT('Ctrl Pts',(-19.59343508194,-27.1630438644242,121.915568323419)) ;
#46167 = CARTESIAN_POINT('Ctrl Pts',(-19.3452475882926,-27.3530929493651,
122.207539583544)) ;
#46168 = CARTESIAN_POINT('Ctrl Pts',(-19.3292573389903,-27.1731038690022,
121.90646877428)) ;
#46169 = CARTESIAN_POINT('Ctrl Pts',(-19.1402979082901,-27.3629362184342,
122.236294727092)) ;
#46170 = CARTESIAN_POINT('Ctrl Pts',(-19.0730690560541,-27.1829471380713,
121.942410469089)) ;
#46171 = CARTESIAN_POINT('Ctrl Pts',(-18.9404022090521,-27.3729267840419,
122.300676483571)) ;
#46172 = CARTESIAN_POINT('Ctrl Pts',(-18.8231985706705,-27.192937703679,122.02288556215)) ;
#46173 = CARTESIAN_POINT('Ctrl Pts',(-18.7558672982378,-27.3828549158207,
122.398221029593)) ;
#46174 = CARTESIAN_POINT('Ctrl Pts',(-18.5925284415636,-27.2028658354578,
122.144814465017)) ;
#46175 = CARTESIAN_POINT('Ctrl Pts',(-18.5898557423788,-27.3928428029016,
122.526807079815)) ;
#46176 = CARTESIAN_POINT('Ctrl Pts',(-18.3850125185332,-27.2128537225387,
122.305545417301)) ;
#46177 = CARTESIAN_POINT('Ctrl Pts',(-18.4482910581977,-27.4028787524703,
122.68324070113)) ;
#46178 = CARTESIAN_POINT('Ctrl Pts',(-18.2080550368114,-27.2228896721074,
122.501085855653)) ;
#46179 = CARTESIAN_POINT('Ctrl Pts',(-18.3377591304148,-27.4127336388491,
122.858492901612)) ;
#46180 = CARTESIAN_POINT('Ctrl Pts',(-18.0698877945043,-27.2327445584862,
122.720150718132)) ;
#46181 = CARTESIAN_POINT('Ctrl Pts',(-18.2579406650141,-27.422733053197,123.052931220241)) ;
#46182 = CARTESIAN_POINT('Ctrl Pts',(-17.9701127120356,-27.2427439728341,
122.963197940076)) ;
#46183 = CARTESIAN_POINT('Ctrl Pts',(-18.2133303124607,-27.4326282183875,
123.256154680513)) ;
#46184 = CARTESIAN_POINT('Ctrl Pts',(-17.9143476221429,-27.2526391380246,
123.217227543753)) ;
#46185 = CARTESIAN_POINT('Ctrl Pts',(-18.204564058286,-27.4426885370794,123.467444615832)) ;
#46186 = CARTESIAN_POINT('Ctrl Pts',(-17.9033877648429,-27.2626994567166,
123.481339637183)) ;
#46187 = CARTESIAN_POINT('Ctrl Pts',(-18.2319167259409,-27.4525386688555,
123.672729223044)) ;
#46188 = CARTESIAN_POINT('Ctrl Pts',(-17.937576742963,-27.2725495884926,123.737946697359)) ;
#46189 = CARTESIAN_POINT('Ctrl Pts',(-18.2951613085268,-27.4625692393058,
123.87388597203)) ;
#46190 = CARTESIAN_POINT('Ctrl Pts',(-18.0166306722375,-27.2825801589429,
123.989393136718)) ;
#46191 = CARTESIAN_POINT('Ctrl Pts',(-18.392639370384,-27.4725833899786,124.060501742582)) ;
#46192 = CARTESIAN_POINT('Ctrl Pts',(-18.1384764760697,-27.2925943096157,
124.222663794495)) ;
#46193 = CARTESIAN_POINT('Ctrl Pts',(-18.5192133454885,-27.482476323524,124.225536129967)) ;
#46194 = CARTESIAN_POINT('Ctrl Pts',(-18.2966929164752,-27.3024872431611,
124.428958569241)) ;
#46195 = CARTESIAN_POINT('Ctrl Pts',(-18.6738373848897,-27.4924658375142,
124.367619074625)) ;
#46196 = CARTESIAN_POINT('Ctrl Pts',(-18.4899718704159,-27.3124767571514,
124.60656373873)) ;
#46197 = CARTESIAN_POINT('Ctrl Pts',(-18.8501175734663,-27.5024196081667,
124.480434768082)) ;
#46198 = CARTESIAN_POINT('Ctrl Pts',(-18.7103215045909,-27.3224305278038,
124.74758509881)) ;
#46199 = CARTESIAN_POINT('Ctrl Pts',(-19.0451588516024,-27.5124673768272,
124.561494657488)) ;
#46200 = CARTESIAN_POINT('Ctrl Pts',(-18.9541222140896,-27.3324782964644,
124.848911596832)) ;
#46201 = CARTESIAN_POINT('Ctrl Pts',(-19.2470679046849,-27.522309103267,124.606762346263)) ;
#46202 = CARTESIAN_POINT('Ctrl Pts',(-19.2065092981465,-27.3423200229042,
124.905498197986)) ;
#46203 = CARTESIAN_POINT('Ctrl Pts',(-19.4567187804264,-27.5322946200898,
124.616878516761)) ;
#46204 = CARTESIAN_POINT('Ctrl Pts',(-19.4685730601993,-27.3523055397269,
124.918145048951)) ;
#46205 = CARTESIAN_POINT('Ctrl Pts',(-19.6640500637913,-27.5422339517853,
124.590629381917)) ;
#46206 = CARTESIAN_POINT('Ctrl Pts',(-19.727737905255,-27.3622448714225,124.885335148688)) ;
#46207 = CARTESIAN_POINT('Ctrl Pts',(-19.8656328349993,-27.5522737214829,
124.52812532427)) ;
#46208 = CARTESIAN_POINT('Ctrl Pts',(-19.9797167083431,-27.37228464112,124.807206664709)) ;
#46209 = CARTESIAN_POINT('Ctrl Pts',(-20.050539305733,-27.5621618827317,124.433105551511)) ;
#46210 = CARTESIAN_POINT('Ctrl Pts',(-20.210851339288,-27.3821728023688,124.688432935281)) ;
#46211 = CARTESIAN_POINT('Ctrl Pts',(-20.2180592426687,-27.5721514372341,
124.306460221141)) ;
#46212 = CARTESIAN_POINT('Ctrl Pts',(-20.4202523049205,-27.3921623568712,
124.530127299133)) ;
#46213 = CARTESIAN_POINT('Ctrl Pts',(-20.3604835812191,-27.5821098517577,
124.153021019065)) ;
#46214 = CARTESIAN_POINT('Ctrl Pts',(-20.5982841261054,-27.4021207713948,
124.338329003495)) ;
#46215 = CARTESIAN_POINT('Ctrl Pts',(-20.473871725562,-27.5920097645871,123.978479224777)) ;
#46216 = CARTESIAN_POINT('Ctrl Pts',(-20.7400208952278,-27.4120206842242,
124.120151747141)) ;
#46217 = CARTESIAN_POINT('Ctrl Pts',(-20.5563690525815,-27.602056464237,123.784065248068)) ;
#46218 = CARTESIAN_POINT('Ctrl Pts',(-20.8431437130591,-27.4220673838741,
123.877134998684)) ;
#46219 = CARTESIAN_POINT('Ctrl Pts',(-20.6033030576586,-27.6119563245426,
123.581267591945)) ;
#46220 = CARTESIAN_POINT('Ctrl Pts',(-20.9018126855217,-27.4319672441797,
123.623637353348)) ;
#46221 = CARTESIAN_POINT('Ctrl Pts',(-20.6145464495285,-27.622007728748,123.370284273142)) ;
#46222 = CARTESIAN_POINT('Ctrl Pts',(-20.9158681861848,-27.4420186483852,
123.359908517845)) ;
#46223 = CARTESIAN_POINT('Ctrl Pts',(-20.5894865428159,-27.6318887656692,
123.164040601756)) ;
#46224 = CARTESIAN_POINT('Ctrl Pts',(-20.8845444215458,-27.4518996853063,
123.102102763115)) ;
#46225 = CARTESIAN_POINT('Ctrl Pts',(-20.5285619224102,-27.6418885978467,
122.96287053044)) ;
#46226 = CARTESIAN_POINT('Ctrl Pts',(-20.8083897017697,-27.4618995174838,
122.850639705419)) ;
#46227 = CARTESIAN_POINT('Ctrl Pts',(-20.4345314205031,-27.6518066008316,
122.776728506564)) ;
#46228 = CARTESIAN_POINT('Ctrl Pts',(-20.6908521995959,-27.4718175204687,
122.61796100732)) ;
#46229 = CARTESIAN_POINT('Ctrl Pts',(-20.307917816095,-27.6618579067061,122.607595735028)) ;
#46230 = CARTESIAN_POINT('Ctrl Pts',(-20.5325862276468,-27.4818688263432,
122.406544566139)) ;
#46231 = CARTESIAN_POINT('Ctrl Pts',(-20.1567577654715,-27.6717277300977,
122.465387827078)) ;
#46232 = CARTESIAN_POINT('Ctrl Pts',(-20.3436360267876,-27.4917386497348,
122.228783160696)) ;
#46233 = CARTESIAN_POINT('Ctrl Pts',(-19.979678811247,-27.681801896148,122.349293202809)) ;
#46234 = CARTESIAN_POINT('Ctrl Pts',(-20.1222882553386,-27.5018128157851,
122.083664260692)) ;
#46235 = CARTESIAN_POINT('Ctrl Pts',(-19.7900524651862,-27.6916219802896,
122.267545505754)) ;
#46236 = CARTESIAN_POINT('Ctrl Pts',(-19.8852542608473,-27.5116328999267,
121.981478176074)) ;
#46237 = CARTESIAN_POINT('Ctrl Pts',(-19.5839641602467,-27.7017007070255,
122.218539726718)) ;
#46238 = CARTESIAN_POINT('Ctrl Pts',(-19.6276445348726,-27.5217116266626,
121.920220233275)) ;
#46239 = CARTESIAN_POINT('Ctrl Pts',(-19.3771678744328,-27.711552287675,122.206266541028)) ;
#46240 = CARTESIAN_POINT('Ctrl Pts',(-19.3691479103184,-27.5315632073121,
121.904877852358)) ;
#46241 = CARTESIAN_POINT('Ctrl Pts',(-19.1668198410956,-27.7216254159734,
122.230427368706)) ;
#46242 = CARTESIAN_POINT('Ctrl Pts',(-19.1062132173581,-27.5416363356105,
121.935078088023)) ;
#46243 = CARTESIAN_POINT('Ctrl Pts',(-18.9684654062851,-27.7314678938648,
122.289410143151)) ;
#46244 = CARTESIAN_POINT('Ctrl Pts',(-18.8582685980059,-27.5514788135019,
122.008806224884)) ;
#46245 = CARTESIAN_POINT('Ctrl Pts',(-18.7804810737789,-27.7414485004629,
122.382594626151)) ;
#46246 = CARTESIAN_POINT('Ctrl Pts',(-18.6232876861483,-27.5614594201,122.125286522871)) ;
#46247 = CARTESIAN_POINT('Ctrl Pts',(-18.6111314469125,-27.7514662094817,
122.50779197817)) ;
#46248 = CARTESIAN_POINT('Ctrl Pts',(-18.4116002704639,-27.5714771291188,
122.281782687979)) ;
#46249 = CARTESIAN_POINT('Ctrl Pts',(-18.46769289707,-27.7613523885191,122.65822099697)) ;
#46250 = CARTESIAN_POINT('Ctrl Pts',(-18.2323009870814,-27.5813633081562,
122.469819398542)) ;
#46251 = CARTESIAN_POINT('Ctrl Pts',(-18.3505632690495,-27.7714100010914,
122.834235024386)) ;
#46252 = CARTESIAN_POINT('Ctrl Pts',(-18.0858887221731,-27.5914209207286,
122.689836404072)) ;
#46253 = CARTESIAN_POINT('Ctrl Pts',(-18.2672711578626,-27.7812863944636,
123.024442583232)) ;
#46254 = CARTESIAN_POINT('Ctrl Pts',(-17.981772680714,-27.6012973141007,122.927596725681)) ;
#46255 = CARTESIAN_POINT('Ctrl Pts',(-18.2171766731924,-27.791281422614,123.228504736778)) ;
#46256 = CARTESIAN_POINT('Ctrl Pts',(-17.9191542665853,-27.6112923422511,
123.182674524743)) ;
#46257 = CARTESIAN_POINT('Ctrl Pts',(-18.2035981744951,-27.80130216946,123.438743704045)) ;
#46258 = CARTESIAN_POINT('Ctrl Pts',(-17.9021807329972,-27.6213130890971,
123.445473162291)) ;
#46259 = CARTESIAN_POINT('Ctrl Pts',(-18.2262128560997,-27.8112042381264,
123.645681904527)) ;
#46260 = CARTESIAN_POINT('Ctrl Pts',(-17.930448869701,-27.6312151577635,123.704146901839)) ;
#46261 = CARTESIAN_POINT('Ctrl Pts',(-18.284639933744,-27.8211949779461,123.847429809037)) ;
#46262 = CARTESIAN_POINT('Ctrl Pts',(-18.0034825912362,-27.6412058975832,
123.956332064129)) ;
#46263 = CARTESIAN_POINT('Ctrl Pts',(-18.3770881160731,-27.8311581741564,
124.035370273374)) ;
#46264 = CARTESIAN_POINT('Ctrl Pts',(-18.1190427862629,-27.6511690937935,
124.191258163438)) ;
#46265 = CARTESIAN_POINT('Ctrl Pts',(-18.4996327245681,-27.8410623584565,
124.203730145458)) ;
#46266 = CARTESIAN_POINT('Ctrl Pts',(-18.2722240570765,-27.6610732780936,
124.401708795378)) ;
#46267 = CARTESIAN_POINT('Ctrl Pts',(-18.652006072211,-27.8511228188474,124.350375168077)) ;
#46268 = CARTESIAN_POINT('Ctrl Pts',(-18.4626904000373,-27.6711337384845,
124.585014918484)) ;
#46269 = CARTESIAN_POINT('Ctrl Pts',(-18.8235862046144,-27.8609633647182,
124.466005825925)) ;
#46270 = CARTESIAN_POINT('Ctrl Pts',(-18.6771667745688,-27.6809742843553,
124.729554078274)) ;
#46271 = CARTESIAN_POINT('Ctrl Pts',(-19.0167402747536,-27.8710255854299,
124.552208647531)) ;
#46272 = CARTESIAN_POINT('Ctrl Pts',(-18.9186090603338,-27.6910365050671,
124.83730737481)) ;
#46273 = CARTESIAN_POINT('Ctrl Pts',(-19.2186463887635,-27.8809227284465,
124.602519019844)) ;
#46274 = CARTESIAN_POINT('Ctrl Pts',(-19.1709926750529,-27.7009336480836,
124.900195583727)) ;
#46275 = CARTESIAN_POINT('Ctrl Pts',(-19.4268700305496,-27.8908539048637,
124.617749388412)) ;
#46276 = CARTESIAN_POINT('Ctrl Pts',(-19.4312729665485,-27.7108648245008,
124.919233320648)) ;
#46277 = CARTESIAN_POINT('Ctrl Pts',(-19.6368755079311,-27.9008961186423,
124.596126506695)) ;
#46278 = CARTESIAN_POINT('Ctrl Pts',(-19.6937795868889,-27.7209070382794,
124.892204557255)) ;
#46279 = CARTESIAN_POINT('Ctrl Pts',(-19.8368447731837,-27.910782658845,124.539408291931)) ;
#46280 = CARTESIAN_POINT('Ctrl Pts',(-19.9437421483585,-27.7307935784821,
124.821306255689)) ;
#46281 = CARTESIAN_POINT('Ctrl Pts',(-20.026076968928,-27.9207762534504,124.448165743483)) ;
#46282 = CARTESIAN_POINT('Ctrl Pts',(-20.180282407611,-27.7407871730876,124.707252644134)) ;
#46283 = CARTESIAN_POINT('Ctrl Pts',(-20.1957478692997,-27.930720128608,124.326020666064)) ;
#46284 = CARTESIAN_POINT('Ctrl Pts',(-20.3923713220577,-27.7507310482451,
124.554570637425)) ;
#46285 = CARTESIAN_POINT('Ctrl Pts',(-20.3420563337105,-27.9406806647228,
124.176229596615)) ;
#46286 = CARTESIAN_POINT('Ctrl Pts',(-20.5752568933734,-27.7606915843599,
124.367331130021)) ;
#46287 = CARTESIAN_POINT('Ctrl Pts',(-20.4606861174511,-27.9506772680455,
124.002726210929)) ;
#46288 = CARTESIAN_POINT('Ctrl Pts',(-20.7235437790341,-27.7706881876827,
124.150451479886)) ;
#46289 = CARTESIAN_POINT('Ctrl Pts',(-20.5474206151358,-27.960710351,123.810462365008)) ;
#46290 = CARTESIAN_POINT('Ctrl Pts',(-20.8319614750394,-27.7807212706372,
123.910121632712)) ;
#46291 = CARTESIAN_POINT('Ctrl Pts',(-20.5987649896307,-27.9705615197016,
123.609829364369)) ;
#46292 = CARTESIAN_POINT('Ctrl Pts',(-20.8961417940296,-27.7905724393387,
123.65932892789)) ;
#46293 = CARTESIAN_POINT('Ctrl Pts',(-20.6152871156439,-27.9805240104005,
123.401046818215)) ;
#46294 = CARTESIAN_POINT('Ctrl Pts',(-20.9167937428057,-27.8005349300376,
123.398350225034)) ;
#46295 = CARTESIAN_POINT('Ctrl Pts',(-20.5949125271602,-27.9905524388182,
123.191192264674)) ;
#46296 = CARTESIAN_POINT('Ctrl Pts',(-20.8913248727649,-27.8105633584554,
123.136032193867)) ;
#46297 = CARTESIAN_POINT('Ctrl Pts',(-20.53914584983,-28.0004628061828,122.990457378277)) ;
#46298 = CARTESIAN_POINT('Ctrl Pts',(-20.8216156440544,-27.8204737258199,
122.885112920422)) ;
#46299 = CARTESIAN_POINT('Ctrl Pts',(-20.4496374418431,-28.0103976737979,
122.801740219199)) ;
#46300 = CARTESIAN_POINT('Ctrl Pts',(-20.7097290522174,-27.830408593435,122.649216253135)) ;
#46301 = CARTESIAN_POINT('Ctrl Pts',(-20.3272748886815,-28.0204388157769,
122.629733634215)) ;
#46302 = CARTESIAN_POINT('Ctrl Pts',(-20.5567753117552,-27.840449735414,122.434208642636)) ;
#46303 = CARTESIAN_POINT('Ctrl Pts',(-20.1793010965195,-28.0303259519801,
122.483741362788)) ;
#46304 = CARTESIAN_POINT('Ctrl Pts',(-20.371806724897,-27.8503368716172,122.251718186914)) ;
#46305 = CARTESIAN_POINT('Ctrl Pts',(-20.0066274113567,-28.0403182343835,
122.364130675041)) ;
#46306 = CARTESIAN_POINT('Ctrl Pts',(-20.1559638841929,-27.8603291540206,
122.102205529793)) ;
#46307 = CARTESIAN_POINT('Ctrl Pts',(-19.8165954509597,-28.0502667623487,
122.276745364225)) ;
#46308 = CARTESIAN_POINT('Ctrl Pts',(-19.9184230348256,-27.8702776819858,
121.99297454764)) ;
#46309 = CARTESIAN_POINT('Ctrl Pts',(-19.6146202820985,-28.0602034935108,
122.223467272798)) ;
#46310 = CARTESIAN_POINT('Ctrl Pts',(-19.665953180287,-27.8802144131479,121.926377817828)) ;
#46311 = CARTESIAN_POINT('Ctrl Pts',(-19.4054676734705,-28.0701867043708,
122.205721541684)) ;
#46312 = CARTESIAN_POINT('Ctrl Pts',(-19.4045120642448,-27.8901976240079,
121.904196807196)) ;
#46313 = CARTESIAN_POINT('Ctrl Pts',(-19.1952379005433,-28.0802298035207,
122.225046803646)) ;
#46314 = CARTESIAN_POINT('Ctrl Pts',(-19.1417251311674,-27.9002407231578,
121.92835440127)) ;
#46315 = CARTESIAN_POINT('Ctrl Pts',(-18.9956932343111,-28.0900607677956,
122.278974247708)) ;
#46316 = CARTESIAN_POINT('Ctrl Pts',(-18.892293224786,-27.9100716874327,121.995765252508)) ;
#46317 = CARTESIAN_POINT('Ctrl Pts',(-18.8039248705908,-28.1001336201815,
122.368723820022)) ;
#46318 = CARTESIAN_POINT('Ctrl Pts',(-18.6525836805033,-27.9201445398186,
122.107953193368)) ;
#46319 = CARTESIAN_POINT('Ctrl Pts',(-18.6342195703199,-28.1099977478933,
122.487946903188)) ;
#46320 = CARTESIAN_POINT('Ctrl Pts',(-18.4404518362338,-27.9300086675304,
122.256983728471)) ;
#46321 = CARTESIAN_POINT('Ctrl Pts',(-18.4851003678343,-28.1200199500282,
122.636789063921)) ;
#46322 = CARTESIAN_POINT('Ctrl Pts',(-18.2540538810711,-27.9400308696653,
122.44303741669)) ;
#46323 = CARTESIAN_POINT('Ctrl Pts',(-18.3644270649533,-28.1300471429966,
122.809651509413)) ;
#46324 = CARTESIAN_POINT('Ctrl Pts',(-18.1032133230383,-27.9500580626337,
122.659116134907)) ;
#46325 = CARTESIAN_POINT('Ctrl Pts',(-18.2768385867952,-28.1399027369636,
122.997405819395)) ;
#46326 = CARTESIAN_POINT('Ctrl Pts',(-17.9937284543403,-27.9599136566007,
122.893810711294)) ;
#46327 = CARTESIAN_POINT('Ctrl Pts',(-18.2220200004676,-28.1498599088289,
123.199439317662)) ;
#46328 = CARTESIAN_POINT('Ctrl Pts',(-17.9252066477856,-27.969870828466,123.146353412769)) ;
#46329 = CARTESIAN_POINT('Ctrl Pts',(-18.2033226183059,-28.1598987528273,
123.409644983658)) ;
#46330 = CARTESIAN_POINT('Ctrl Pts',(-17.9018363926086,-27.9799096724644,
123.409110487333)) ;
#46331 = CARTESIAN_POINT('Ctrl Pts',(-18.2207487622362,-28.1697727767028,
123.616522805315)) ;
#46332 = CARTESIAN_POINT('Ctrl Pts',(-17.9236207437678,-27.98978369634,123.667708642615)) ;
#46333 = CARTESIAN_POINT('Ctrl Pts',(-18.2748756328717,-28.1798426026932,
123.821155710981)) ;
#46334 = CARTESIAN_POINT('Ctrl Pts',(-17.9912807797275,-27.9998535223304,
123.923499029241)) ;
#46335 = CARTESIAN_POINT('Ctrl Pts',(-18.3615430076775,-28.1896758465905,
124.008855877301)) ;
#46336 = CARTESIAN_POINT('Ctrl Pts',(-18.0996170115864,-28.0096867662276,
124.158124720439)) ;
#46337 = CARTESIAN_POINT('Ctrl Pts',(-18.4813453459947,-28.1997062743635,
124.18238158238)) ;
#46338 = CARTESIAN_POINT('Ctrl Pts',(-18.249371382821,-28.0197171940007,124.375030745284)) ;
#46339 = CARTESIAN_POINT('Ctrl Pts',(-18.6299243812976,-28.2097378911087,
124.332069289836)) ;
#46340 = CARTESIAN_POINT('Ctrl Pts',(-18.4350962680924,-28.0297488107458,
124.562139179243)) ;
#46341 = CARTESIAN_POINT('Ctrl Pts',(-18.7984985629321,-28.2195675680894,
124.451573981328)) ;
#46342 = CARTESIAN_POINT('Ctrl Pts',(-18.6458160519967,-28.0395784877265,
124.711519341739)) ;
#46343 = CARTESIAN_POINT('Ctrl Pts',(-18.9880488787878,-28.2295570849293,
124.542006375535)) ;
#46344 = CARTESIAN_POINT('Ctrl Pts',(-18.8827549500496,-28.0495680045665,
124.824558143869)) ;
#46345 = CARTESIAN_POINT('Ctrl Pts',(-19.1916515256229,-28.2396006970691,
124.597937925507)) ;
#46346 = CARTESIAN_POINT('Ctrl Pts',(-19.1372585887124,-28.0596116167062,
124.894470815532)) ;
#46347 = CARTESIAN_POINT('Ctrl Pts',(-19.3972114936263,-28.2494233034044,
124.617664945189)) ;
#46348 = CARTESIAN_POINT('Ctrl Pts',(-19.3942099817878,-28.0694342230415,
124.91912779169)) ;
#46349 = CARTESIAN_POINT('Ctrl Pts',(-19.6076212256826,-28.2594615333036,
124.601522484725)) ;
#46350 = CARTESIAN_POINT('Ctrl Pts',(-19.6572218646034,-28.0794724529408,
124.898947663021)) ;
#46351 = CARTESIAN_POINT('Ctrl Pts',(-19.8113776911949,-28.2694725680956,
124.548753711217)) ;
#46352 = CARTESIAN_POINT('Ctrl Pts',(-19.9119170104515,-28.0894834877327,
124.832984826371)) ;
#46353 = CARTESIAN_POINT('Ctrl Pts',(-20.0008298539462,-28.2793702990627,
124.462706665286)) ;
#46354 = CARTESIAN_POINT('Ctrl Pts',(-20.1487320477206,-28.0993812186998,
124.725423875281)) ;
#46355 = CARTESIAN_POINT('Ctrl Pts',(-20.1742139857442,-28.2893599269132,
124.344205140818)) ;
#46356 = CARTESIAN_POINT('Ctrl Pts',(-20.3654611748462,-28.1093708465503,
124.5772951408)) ;
#46357 = CARTESIAN_POINT('Ctrl Pts',(-20.3238283363393,-28.2993157173592,
124.19784376409)) ;
#46358 = CARTESIAN_POINT('Ctrl Pts',(-20.5524779416027,-28.1193266369963,
124.394341663434)) ;
#46359 = CARTESIAN_POINT('Ctrl Pts',(-20.4457396566452,-28.3092431159212,
124.028437006786)) ;
#46360 = CARTESIAN_POINT('Ctrl Pts',(-20.7048656204767,-28.1292540355584,
124.182581520283)) ;
#46361 = CARTESIAN_POINT('Ctrl Pts',(-20.5372193180134,-28.3192687110311,
123.838562812821)) ;
#46362 = CARTESIAN_POINT('Ctrl Pts',(-20.8192132351186,-28.1392796306682,
123.945237856592)) ;
#46363 = CARTESIAN_POINT('Ctrl Pts',(-20.5936698159923,-28.3291545617007,
123.638543561245)) ;
#46364 = CARTESIAN_POINT('Ctrl Pts',(-20.8897744387993,-28.1491654813378,
123.695212486568)) ;
#46365 = CARTESIAN_POINT('Ctrl Pts',(-20.6152462524492,-28.3391437415449,
123.429645094941)) ;
#46366 = CARTESIAN_POINT('Ctrl Pts',(-20.9167426862714,-28.159154661182,123.434089007642)) ;
#46367 = CARTESIAN_POINT('Ctrl Pts',(-20.5997049484337,-28.3491849286484,
123.219121094953)) ;
#46368 = CARTESIAN_POINT('Ctrl Pts',(-20.8973138529512,-28.1691958482856,
123.170934263122)) ;
#46369 = CARTESIAN_POINT('Ctrl Pts',(-20.5492532199071,-28.3590175721244,
123.018663279547)) ;
#46370 = CARTESIAN_POINT('Ctrl Pts',(-20.8342467261708,-28.1790284917615,
122.920361624849)) ;
#46371 = CARTESIAN_POINT('Ctrl Pts',(-20.4639239618416,-28.3690115218339,
122.826668029978)) ;
#46372 = CARTESIAN_POINT('Ctrl Pts',(-20.7275828726051,-28.189022441471,122.680368443651)) ;
#46373 = CARTESIAN_POINT('Ctrl Pts',(-20.3457702484628,-28.3790406446104,
122.652037807507)) ;
#46374 = CARTESIAN_POINT('Ctrl Pts',(-20.5798888066981,-28.1990515642475,
122.462081994114)) ;
#46375 = CARTESIAN_POINT('Ctrl Pts',(-20.2015610995993,-28.3889167755291,
122.502648999928)) ;
#46376 = CARTESIAN_POINT('Ctrl Pts',(-20.3996251641318,-28.2089276951662,
122.275347174546)) ;
#46377 = CARTESIAN_POINT('Ctrl Pts',(-20.0317039479304,-28.3989148105461,
122.37888357769)) ;
#46378 = CARTESIAN_POINT('Ctrl Pts',(-20.1873021799441,-28.2189257301832,
122.120642324747)) ;
#46379 = CARTESIAN_POINT('Ctrl Pts',(-19.8445504166726,-28.4088287403048,
122.287101606991)) ;
#46380 = CARTESIAN_POINT('Ctrl Pts',(-19.9533587455655,-28.2288396599419,
122.005916898594)) ;
#46381 = CARTESIAN_POINT('Ctrl Pts',(-19.6417453548372,-28.4188719280426,
122.228424618647)) ;
#46382 = CARTESIAN_POINT('Ctrl Pts',(-19.6998517913933,-28.2388828476797,
121.932573093305)) ;
#46383 = CARTESIAN_POINT('Ctrl Pts',(-19.4348032819945,-28.428771770183,122.206158950053)) ;
#46384 = CARTESIAN_POINT('Ctrl Pts',(-19.4411734358199,-28.2487826898201,
121.904743447238)) ;
#46385 = CARTESIAN_POINT('Ctrl Pts',(-19.225199951328,-28.438763036991,122.219845479332)) ;
#46386 = CARTESIAN_POINT('Ctrl Pts',(-19.1791693222562,-28.2587739566281,
121.921854204058)) ;
#46387 = CARTESIAN_POINT('Ctrl Pts',(-19.0204087974407,-28.4487951391229,
122.270276783567)) ;
#46388 = CARTESIAN_POINT('Ctrl Pts',(-18.923180998322,-28.2688060587601,121.984895781452)) ;
#46389 = CARTESIAN_POINT('Ctrl Pts',(-18.8305583447142,-28.4586620200777,
122.353843034253)) ;
#46390 = CARTESIAN_POINT('Ctrl Pts',(-18.6858684267657,-28.2786729397148,
122.08935619064)) ;
#46391 = CARTESIAN_POINT('Ctrl Pts',(-18.6556330787561,-28.4686538113658,
122.470151417965)) ;
#46392 = CARTESIAN_POINT('Ctrl Pts',(-18.4672132264588,-28.288664731003,122.234743944374)) ;
#46393 = CARTESIAN_POINT('Ctrl Pts',(-18.5032314430184,-28.4786859272774,
122.61594277691)) ;
#46394 = CARTESIAN_POINT('Ctrl Pts',(-18.276712974157,-28.2986968469145,122.416985014583)) ;
#46395 = CARTESIAN_POINT('Ctrl Pts',(-18.380260915545,-28.4885522440774,122.782991829368)) ;
#46396 = CARTESIAN_POINT('Ctrl Pts',(-18.1230016340979,-28.3085631637145,
122.625798315029)) ;
#46397 = CARTESIAN_POINT('Ctrl Pts',(-18.286740408124,-28.498539725551,122.970954331532)) ;
#46398 = CARTESIAN_POINT('Ctrl Pts',(-18.0061033569078,-28.3185506451881,
122.86075275285)) ;
#46399 = CARTESIAN_POINT('Ctrl Pts',(-18.2274077058308,-28.5084846499299,
123.171464369965)) ;
#46400 = CARTESIAN_POINT('Ctrl Pts',(-17.931940003922,-28.328495569567,123.111391293711)) ;
#46401 = CARTESIAN_POINT('Ctrl Pts',(-18.2036772806348,-28.5185295358406,
123.381282408305)) ;
#46402 = CARTESIAN_POINT('Ctrl Pts',(-17.902279648867,-28.3385404554777,123.373664123611)) ;
#46403 = CARTESIAN_POINT('Ctrl Pts',(-18.2163217636226,-28.5283916395532,
123.588243745579)) ;
#46404 = CARTESIAN_POINT('Ctrl Pts',(-17.9180879856087,-28.3484025591903,
123.632366059909)) ;
#46405 = CARTESIAN_POINT('Ctrl Pts',(-18.2649253863527,-28.5383832033776,
123.792581695052)) ;
#46406 = CARTESIAN_POINT('Ctrl Pts',(-17.978845222314,-28.3583941230148,123.887787950721)) ;
#46407 = CARTESIAN_POINT('Ctrl Pts',(-18.3478659471332,-28.5483160114405,
123.984221813374)) ;
#46408 = CARTESIAN_POINT('Ctrl Pts',(-18.0825235360191,-28.3683269310777,
124.127337211337)) ;
#46409 = CARTESIAN_POINT('Ctrl Pts',(-18.4624497179601,-28.5582531136769,
124.158918671784)) ;
#46410 = CARTESIAN_POINT('Ctrl Pts',(-18.2257556811439,-28.378264033314,124.345706898237)) ;
#46411 = CARTESIAN_POINT('Ctrl Pts',(-18.6074717807451,-28.5683055599473,
124.312619227432)) ;
#46412 = CARTESIAN_POINT('Ctrl Pts',(-18.4070352870554,-28.3883164795844,
124.537830699298)) ;
#46413 = CARTESIAN_POINT('Ctrl Pts',(-18.7733489453358,-28.5781516755289,
124.436472624767)) ;
#46414 = CARTESIAN_POINT('Ctrl Pts',(-18.6143836431893,-28.398162595166,124.692645379455)) ;
#46415 = CARTESIAN_POINT('Ctrl Pts',(-18.9618249797804,-28.5881996952438,
124.531831590146)) ;
#46416 = CARTESIAN_POINT('Ctrl Pts',(-18.8499799673712,-28.4082106148809,
124.811841582492)) ;
#46417 = CARTESIAN_POINT('Ctrl Pts',(-19.1619711895627,-28.5981416468727,
124.592099396301)) ;
#46418 = CARTESIAN_POINT('Ctrl Pts',(-19.1001636769322,-28.4181525665098,
124.887173703346)) ;
#46419 = CARTESIAN_POINT('Ctrl Pts',(-19.36940458292,-28.6080804278718,124.617204452178)) ;
#46420 = CARTESIAN_POINT('Ctrl Pts',(-19.3594558684256,-28.4280913475089,
124.91855224253)) ;
#46421 = CARTESIAN_POINT('Ctrl Pts',(-19.5798534901081,-28.6181064765979,
124.605652962537)) ;
#46422 = CARTESIAN_POINT('Ctrl Pts',(-19.6225169288426,-28.438117396235,124.904110048364)) ;
#46423 = CARTESIAN_POINT('Ctrl Pts',(-19.7823487906233,-28.6279933370061,
124.558649540917)) ;
#46424 = CARTESIAN_POINT('Ctrl Pts',(-19.8756354818284,-28.4480042566432,
124.845353062354)) ;
#46425 = CARTESIAN_POINT('Ctrl Pts',(-19.9763812601013,-28.6380246121379,
124.476122124052)) ;
#46426 = CARTESIAN_POINT('Ctrl Pts',(-20.1181752200281,-28.458035531775,124.742190925089)) ;
#46427 = CARTESIAN_POINT('Ctrl Pts',(-20.1507052106711,-28.6479075894383,
124.362992233123)) ;
#46428 = CARTESIAN_POINT('Ctrl Pts',(-20.3360779496977,-28.4679185090754,
124.600777052286)) ;
#46429 = CARTESIAN_POINT('Ctrl Pts',(-20.3053443200726,-28.6579644428455,
124.218890410107)) ;
#46430 = CARTESIAN_POINT('Ctrl Pts',(-20.5293776948737,-28.4779753624826,
124.420644314917)) ;
#46431 = CARTESIAN_POINT('Ctrl Pts',(-20.4724604666755,-28.6711326839214,
123.998058155589)) ;
#46432 = CARTESIAN_POINT('Ctrl Pts',(-20.7382563360483,-28.4911436035585,
124.144618303968)) ;
#46433 = CARTESIAN_POINT('Ctrl Pts',(-20.5799131365806,-28.6845337131479,
123.73425819107)) ;
#46434 = CARTESIAN_POINT('Ctrl Pts',(-20.8725696183407,-28.504544632785,123.814898572995)) ;
#46435 = CARTESIAN_POINT('Ctrl Pts',(-20.6142236375671,-28.6977466298788,
123.458567013862)) ;
#46436 = CARTESIAN_POINT('Ctrl Pts',(-20.9154664864313,-28.5177575495159,
123.470229804426)) ;
#46437 = CARTESIAN_POINT('Ctrl Pts',(-20.604352967794,-28.707675024332,123.250109379369)) ;
#46438 = CARTESIAN_POINT('Ctrl Pts',(-20.9031228604222,-28.5276859439691,
123.209668872578)) ;
#46439 = CARTESIAN_POINT('Ctrl Pts',(-20.5583282587321,-28.7176565244601,
123.045346923892)) ;
#46440 = CARTESIAN_POINT('Ctrl Pts',(-20.8455899283561,-28.5376674440972,
122.953713451803)) ;
#46441 = CARTESIAN_POINT('Ctrl Pts',(-20.4767166915395,-28.7276970677302,
122.850689815527)) ;
#46442 = CARTESIAN_POINT('Ctrl Pts',(-20.7435726949857,-28.5477079873673,
122.710393832338)) ;
#46443 = CARTESIAN_POINT('Ctrl Pts',(-20.3649428036905,-28.7375463995133,
122.676381992891)) ;
#46444 = CARTESIAN_POINT('Ctrl Pts',(-20.6038530329981,-28.5575573191504,
122.492510433972)) ;
#46445 = CARTESIAN_POINT('Ctrl Pts',(-20.2229203006753,-28.747541803985,122.521509294334)) ;
#46446 = CARTESIAN_POINT('Ctrl Pts',(-20.4263234254277,-28.5675527236221,
122.298921849287)) ;
#46447 = CARTESIAN_POINT('Ctrl Pts',(-20.0555849748291,-28.7575581314336,
122.393679057562)) ;
#46448 = CARTESIAN_POINT('Ctrl Pts',(-20.2171504397288,-28.5775690510707,
122.139134607576)) ;
#46449 = CARTESIAN_POINT('Ctrl Pts',(-19.8088912325934,-28.7707817886001,
122.265428926498)) ;
#46450 = CARTESIAN_POINT('Ctrl Pts',(-19.9087920777924,-28.5907927082372,
121.978832990271)) ;
#46451 = CARTESIAN_POINT('Ctrl Pts',(-19.5330216381452,-28.7840760799895,
122.203967929054)) ;
#46452 = CARTESIAN_POINT('Ctrl Pts',(-19.5639959876032,-28.6040869996266,
121.90200706357)) ;
#46453 = CARTESIAN_POINT('Ctrl Pts',(-19.2539859157199,-28.797360430921,122.215868648645)) ;
#46454 = CARTESIAN_POINT('Ctrl Pts',(-19.2151418343695,-28.6173713505581,
121.916882629654)) ;
#46455 = CARTESIAN_POINT('Ctrl Pts',(-19.0492445151565,-28.8073328119828,
122.260874137876)) ;
#46456 = CARTESIAN_POINT('Ctrl Pts',(-18.9592277477311,-28.6273437316199,
121.973142750752)) ;
#46457 = CARTESIAN_POINT('Ctrl Pts',(-18.8564919194603,-28.8172411916084,
122.339917001314)) ;
#46458 = CARTESIAN_POINT('Ctrl Pts',(-18.7182849243588,-28.6372521112455,
122.071948770313)) ;
#46459 = CARTESIAN_POINT('Ctrl Pts',(-18.6778931742279,-28.8272951903564,
122.452918665696)) ;
#46460 = CARTESIAN_POINT('Ctrl Pts',(-18.4950390577731,-28.6473061099936,
122.213201780035)) ;
#46461 = CARTESIAN_POINT('Ctrl Pts',(-18.524471696003,-28.8371573874727,122.592405825859)) ;
#46462 = CARTESIAN_POINT('Ctrl Pts',(-18.3032620688519,-28.6571683071099,
122.38756772639)) ;
#46463 = CARTESIAN_POINT('Ctrl Pts',(-18.3524307607685,-28.8505045138469,
122.814082154856)) ;
#46464 = CARTESIAN_POINT('Ctrl Pts',(-18.0882237967221,-28.670515433484,122.664637872146)) ;
#46465 = CARTESIAN_POINT('Ctrl Pts',(-18.2159876348167,-28.8670414794883,
123.138150036716)) ;
#46466 = CARTESIAN_POINT('Ctrl Pts',(-17.9176634712148,-28.6870523991254,
123.069772556873)) ;
#46467 = CARTESIAN_POINT('Ctrl Pts',(-18.1976653162901,-28.8836760836622,
123.491362438096)) ;
#46468 = CARTESIAN_POINT('Ctrl Pts',(-17.8947632869084,-28.7036870032994,
123.511208297081)) ;
#46469 = CARTESIAN_POINT('Ctrl Pts',(-18.2560525173173,-28.8969658769049,
123.764590199396)) ;
#46470 = CARTESIAN_POINT('Ctrl Pts',(-17.9677541226804,-28.716976796542,123.852806493769)) ;
#46471 = CARTESIAN_POINT('Ctrl Pts',(-18.3343741631932,-28.9069185081643,
123.958600107731)) ;
#46472 = CARTESIAN_POINT('Ctrl Pts',(-18.0656567609654,-28.7269294278014,
124.095304375433)) ;
#46473 = CARTESIAN_POINT('Ctrl Pts',(-18.4449965967694,-28.916870475469,124.136207394979)) ;
#46474 = CARTESIAN_POINT('Ctrl Pts',(-18.2039394803118,-28.7368813951061,
124.317317362258)) ;
#46475 = CARTESIAN_POINT('Ctrl Pts',(-18.6328431511708,-28.9302377339328,
124.345197379133)) ;
#46476 = CARTESIAN_POINT('Ctrl Pts',(-18.4387363200913,-28.7502486535699,
124.578542730155)) ;
#46477 = CARTESIAN_POINT('Ctrl Pts',(-18.9269841780433,-28.9467545458819,
124.537227554656)) ;
#46478 = CARTESIAN_POINT('Ctrl Pts',(-18.8064292376097,-28.7667654655191,
124.818587725884)) ;
#46479 = CARTESIAN_POINT('Ctrl Pts',(-19.3414615997305,-28.9667804408883,
124.634301072555)) ;
#46480 = CARTESIAN_POINT('Ctrl Pts',(-19.3245222155934,-28.7867913605254,
124.939922033055)) ;
#46481 = CARTESIAN_POINT('Ctrl Pts',(-19.759850235118,-28.9865911710184,124.584749330712)) ;
#46482 = CARTESIAN_POINT('Ctrl Pts',(-19.8475073460439,-28.8066020906556,
124.877979440127)) ;
#46483 = CARTESIAN_POINT('Ctrl Pts',(-20.1396804889429,-29.0065683871483,
124.394678367115)) ;
#46484 = CARTESIAN_POINT('Ctrl Pts',(-20.3222930272887,-28.8265793067854,
124.640387404646)) ;
#46485 = CARTESIAN_POINT('Ctrl Pts',(-20.4305598017003,-29.0264952625436,
124.086638339135)) ;
#46486 = CARTESIAN_POINT('Ctrl Pts',(-20.6858890813368,-28.8465061821807,
124.255335344324)) ;
#46487 = CARTESIAN_POINT('Ctrl Pts',(-20.5992504484349,-29.0463167240198,
123.700349376274)) ;
#46488 = CARTESIAN_POINT('Ctrl Pts',(-20.896748937638,-28.866327643657,123.772474684031)) ;
#46489 = CARTESIAN_POINT('Ctrl Pts',(-20.626046085885,-29.0663910418292,123.274422117827)) ;
#46490 = CARTESIAN_POINT('Ctrl Pts',(-20.930240651337,-28.8864019614663,123.240064582413)) ;
#46491 = CARTESIAN_POINT('Ctrl Pts',(-20.506795066352,-29.0862390108371,122.869477985307)) ;
#46492 = CARTESIAN_POINT('Ctrl Pts',(-20.7811745275789,-28.9062499304742,
122.733886817119)) ;
#46493 = CARTESIAN_POINT('Ctrl Pts',(-20.2560944539261,-29.1061860449003,
122.527490551716)) ;
#46494 = CARTESIAN_POINT('Ctrl Pts',(-20.4677973260097,-28.9261969645374,
122.306404432572)) ;
#46495 = CARTESIAN_POINT('Ctrl Pts',(-19.9044790885967,-29.1260819958724,
122.292205363375)) ;
#46496 = CARTESIAN_POINT('Ctrl Pts',(-20.0282780332881,-28.9460929155096,
122.012300463532)) ;
#46497 = CARTESIAN_POINT('Ctrl Pts',(-19.493912747964,-29.1459774754907,122.190368785616)) ;
#46498 = CARTESIAN_POINT('Ctrl Pts',(-19.5150711784553,-28.9659883951278,
121.885006525189)) ;
#46499 = CARTESIAN_POINT('Ctrl Pts',(-19.0718902420119,-29.1659335864555,
122.234795537404)) ;
#46500 = CARTESIAN_POINT('Ctrl Pts',(-18.987543756163,-28.9859445060926,121.940541079356)) ;
#46501 = CARTESIAN_POINT('Ctrl Pts',(-18.6914823643913,-29.1858381344955,
122.420160422829)) ;
#46502 = CARTESIAN_POINT('Ctrl Pts',(-18.5120357100849,-29.0058490541326,
122.172247469475)) ;
#46503 = CARTESIAN_POINT('Ctrl Pts',(-18.3967545767849,-29.2057122588146,
122.723103992137)) ;
#46504 = CARTESIAN_POINT('Ctrl Pts',(-18.1436273509991,-29.0257231784517,
122.550925494824)) ;
#46505 = CARTESIAN_POINT('Ctrl Pts',(-18.2221384336728,-29.2257667888136,
123.11205184558)) ;
#46506 = CARTESIAN_POINT('Ctrl Pts',(-17.9253569901024,-29.0457777084507,
123.037111210492)) ;
#46507 = CARTESIAN_POINT('Ctrl Pts',(-18.190981362348,-29.2455743025736,123.532149795036)) ;
#46508 = CARTESIAN_POINT('Ctrl Pts',(-17.8864107136343,-29.0655852222107,
123.562230606204)) ;
#46509 = CARTESIAN_POINT('Ctrl Pts',(-18.3051612613185,-29.2655576583413,
123.941359506721)) ;
#46510 = CARTESIAN_POINT('Ctrl Pts',(-18.0291344865639,-29.0855685779784,
124.073742812752)) ;
#46511 = CARTESIAN_POINT('Ctrl Pts',(-18.5518768276411,-29.2854759609252,
124.285589142629)) ;
#46512 = CARTESIAN_POINT('Ctrl Pts',(-18.3375275327191,-29.1054868805624,
124.504029337498)) ;
#46513 = CARTESIAN_POINT('Ctrl Pts',(-18.8998033234493,-29.305344176371,124.525350894694)) ;
#46514 = CARTESIAN_POINT('Ctrl Pts',(-18.7724331767996,-29.1253550960081,
124.803732067651)) ;
#46515 = CARTESIAN_POINT('Ctrl Pts',(-19.3123749934706,-29.3253944931673,
124.632263603809)) ;
#46516 = CARTESIAN_POINT('Ctrl Pts',(-19.2881479519155,-29.1454054128044,
124.937374691163)) ;
#46517 = CARTESIAN_POINT('Ctrl Pts',(-19.7312061051285,-29.3451705550497,
124.593056434788)) ;
#46518 = CARTESIAN_POINT('Ctrl Pts',(-19.8116842876558,-29.1651814746869,
124.888368150055)) ;
#46519 = CARTESIAN_POINT('Ctrl Pts',(-20.1166949902579,-29.3652251607422,
124.411179447447)) ;
#46520 = CARTESIAN_POINT('Ctrl Pts',(-20.2935470559368,-29.1852360803793,
124.661024000669)) ;
#46521 = CARTESIAN_POINT('Ctrl Pts',(-20.413193850282,-29.3850188498981,124.112306030586)) ;
#46522 = CARTESIAN_POINT('Ctrl Pts',(-20.6641709204212,-29.2050297695352,
124.287435707295)) ;
#46523 = CARTESIAN_POINT('Ctrl Pts',(-20.5924104104792,-29.4049855414925,
123.727541429383)) ;
#46524 = CARTESIAN_POINT('Ctrl Pts',(-20.8881946382118,-29.2249964611296,
123.806481690324)) ;
#46525 = CARTESIAN_POINT('Ctrl Pts',(-20.6289121024175,-29.4249455872434,
123.304630992729)) ;
#46526 = CARTESIAN_POINT('Ctrl Pts',(-20.9338249693073,-29.2449565068806,
123.277844260743)) ;
#46527 = CARTESIAN_POINT('Ctrl Pts',(-20.5195428798539,-29.4448438473937,
122.895946670909)) ;
#46528 = CARTESIAN_POINT('Ctrl Pts',(-20.7971171356574,-29.2648547670308,
122.766988876807)) ;
#46529 = CARTESIAN_POINT('Ctrl Pts',(-20.2777340208433,-29.4647387629429,
122.548875500711)) ;
#46530 = CARTESIAN_POINT('Ctrl Pts',(-20.4948597929885,-29.28474968258,122.33314837501)) ;
#46531 = CARTESIAN_POINT('Ctrl Pts',(-19.9319526108886,-29.4846489433565,
122.30463596634)) ;
#46532 = CARTESIAN_POINT('Ctrl Pts',(-20.0626359964947,-29.3046598629936,
122.027845909722)) ;
#46533 = CARTESIAN_POINT('Ctrl Pts',(-19.5230900240382,-29.5045847424707,
122.192721165908)) ;
#46534 = CARTESIAN_POINT('Ctrl Pts',(-19.5515593327172,-29.3245956621079,
121.887948224382)) ;
#46535 = CARTESIAN_POINT('Ctrl Pts',(-19.1005503152697,-29.5245226041249,
122.227022561574)) ;
#46536 = CARTESIAN_POINT('Ctrl Pts',(-19.0233846938744,-29.344533523762,121.930820617086)) ;
#46537 = CARTESIAN_POINT('Ctrl Pts',(-18.7153085805982,-29.5444416507625,
122.403062773862)) ;
#46538 = CARTESIAN_POINT('Ctrl Pts',(-18.5418309889796,-29.3644525703997,
122.150865733304)) ;
#46539 = CARTESIAN_POINT('Ctrl Pts',(-18.4127914875677,-29.5643905488167,
122.700380117268)) ;
#46540 = CARTESIAN_POINT('Ctrl Pts',(-18.1636813294162,-29.3844014684538,
122.522511403366)) ;
#46541 = CARTESIAN_POINT('Ctrl Pts',(-18.2301756318706,-29.5842963762597,
123.082237752554)) ;
#46542 = CARTESIAN_POINT('Ctrl Pts',(-17.9354075384507,-29.4043072958969,
122.999821271264)) ;
#46543 = CARTESIAN_POINT('Ctrl Pts',(-18.1953684956847,-29.600879071625,123.433028159498)) ;
#46544 = CARTESIAN_POINT('Ctrl Pts',(-17.8918934979895,-29.4208899912622,
123.438338526591)) ;
#46545 = CARTESIAN_POINT('Ctrl Pts',(-18.24027601235,-29.6141532853487,123.708522208439)) ;
#46546 = CARTESIAN_POINT('Ctrl Pts',(-17.9480247352152,-29.4341642049858,
123.782679410161)) ;
#46547 = CARTESIAN_POINT('Ctrl Pts',(-18.3100397706379,-29.624200004548,123.907851703837)) ;
#46548 = CARTESIAN_POINT('Ctrl Pts',(-18.0352295821613,-29.4442109241851,
124.031850013628)) ;
#46549 = CARTESIAN_POINT('Ctrl Pts',(-18.4110966673818,-29.6340440391937,
124.088481382499)) ;
#46550 = CARTESIAN_POINT('Ctrl Pts',(-18.1615379687603,-29.4540549588308,
124.257627504343)) ;
#46551 = CARTESIAN_POINT('Ctrl Pts',(-18.5878370635189,-29.6473784240982,
124.305998065082)) ;
#46552 = CARTESIAN_POINT('Ctrl Pts',(-18.3825117400926,-29.4673893437353,
124.529570908532)) ;
#46553 = CARTESIAN_POINT('Ctrl Pts',(-18.8736671997377,-29.663965641398,124.512799362027)) ;
#46554 = CARTESIAN_POINT('Ctrl Pts',(-18.7397290349317,-29.4839765610351,
124.788022651488)) ;
#46555 = CARTESIAN_POINT('Ctrl Pts',(-19.2135861785788,-29.6805988534359,
124.610126724355)) ;
#46556 = CARTESIAN_POINT('Ctrl Pts',(-19.1646822605817,-29.500609773073,124.90971077457)) ;
#46557 = CARTESIAN_POINT('Ctrl Pts',(-19.4928463617671,-29.6938812957081,
124.61484124617)) ;
#46558 = CARTESIAN_POINT('Ctrl Pts',(-19.5137203885275,-29.5138922153452,
124.915596996125)) ;
#46559 = CARTESIAN_POINT('Ctrl Pts',(-19.6985621110543,-29.7037871836223,
124.582563757789)) ;
#46560 = CARTESIAN_POINT('Ctrl Pts',(-19.7708729287446,-29.5237981032594,
124.875254844356)) ;
#46561 = CARTESIAN_POINT('Ctrl Pts',(-19.8973061665422,-29.7137756017274,
124.514736011145)) ;
#46562 = CARTESIAN_POINT('Ctrl Pts',(-20.0193014854552,-29.5337865213645,
124.790472867222)) ;
#46563 = CARTESIAN_POINT('Ctrl Pts',(-20.0817838352029,-29.7237990289661,
124.412880710944)) ;
#46564 = CARTESIAN_POINT('Ctrl Pts',(-20.2499022751864,-29.5438099486033,
124.663153811252)) ;
#46565 = CARTESIAN_POINT('Ctrl Pts',(-20.2438922250525,-29.7337034600831,
124.282207760991)) ;
#46566 = CARTESIAN_POINT('Ctrl Pts',(-20.4525327560064,-29.5537143797203,
124.499823981593)) ;
#46567 = CARTESIAN_POINT('Ctrl Pts',(-20.4278473297483,-29.7469666126936,
124.072677307792)) ;
#46568 = CARTESIAN_POINT('Ctrl Pts',(-20.6825120254526,-29.5669775323307,
124.237867726831)) ;
#46569 = CARTESIAN_POINT('Ctrl Pts',(-20.5532267657517,-29.7602915105975,
123.81863575924)) ;
#46570 = CARTESIAN_POINT('Ctrl Pts',(-20.8392151516731,-29.5803024302346,
123.9203381995)) ;
#46571 = CARTESIAN_POINT('Ctrl Pts',(-20.607805933461,-29.7735472542131,123.545295424663)) ;
#46572 = CARTESIAN_POINT('Ctrl Pts',(-20.9074394904579,-29.5935581738502,
123.578684401647)) ;
#46573 = CARTESIAN_POINT('Ctrl Pts',(-20.6128379852353,-29.7835066276604,
123.336009205538)) ;
#46574 = CARTESIAN_POINT('Ctrl Pts',(-20.9137330388378,-29.6035175472975,
123.317072430943)) ;
#46575 = CARTESIAN_POINT('Ctrl Pts',(-20.5817572009049,-29.7934504515873,
123.129255120168)) ;
#46576 = CARTESIAN_POINT('Ctrl Pts',(-20.8748846541773,-29.6134613712245,
123.058630457453)) ;
#46577 = CARTESIAN_POINT('Ctrl Pts',(-20.5143943920179,-29.8034983957346,
122.929061237664)) ;
#46578 = CARTESIAN_POINT('Ctrl Pts',(-20.7906838438031,-29.6235093153718,
122.808386846984)) ;
#46579 = CARTESIAN_POINT('Ctrl Pts',(-20.4154235821622,-29.8133493669528,
122.747128077914)) ;
#46580 = CARTESIAN_POINT('Ctrl Pts',(-20.666972739531,-29.6333602865899,122.580969032646)) ;
#46581 = CARTESIAN_POINT('Ctrl Pts',(-20.2852290763675,-29.8233211843949,
122.582848316609)) ;
#46582 = CARTESIAN_POINT('Ctrl Pts',(-20.504231739043,-29.643332104032,122.37561747521)) ;
#46583 = CARTESIAN_POINT('Ctrl Pts',(-20.128053971246,-29.833316606687,122.443331037292)) ;
#46584 = CARTESIAN_POINT('Ctrl Pts',(-20.3077646577954,-29.6533275263241,
122.20121873475)) ;
#46585 = CARTESIAN_POINT('Ctrl Pts',(-19.9482825221474,-29.8433496718107,
122.333015974272)) ;
#46586 = CARTESIAN_POINT('Ctrl Pts',(-20.0830517816903,-29.6633605914478,
122.063322483088)) ;
#46587 = CARTESIAN_POINT('Ctrl Pts',(-19.7554396738521,-29.8532150044759,
122.25669701737)) ;
#46588 = CARTESIAN_POINT('Ctrl Pts',(-19.8419990547799,-29.673225924113,121.967921099706)) ;
#46589 = CARTESIAN_POINT('Ctrl Pts',(-19.5504291193949,-29.8631755470735,
122.214013364722)) ;
#46590 = CARTESIAN_POINT('Ctrl Pts',(-19.5857362753535,-29.6831864667106,
121.914563791572)) ;
#46591 = CARTESIAN_POINT('Ctrl Pts',(-19.3395885460387,-29.8732092325752,
122.207884141582)) ;
#46592 = CARTESIAN_POINT('Ctrl Pts',(-19.3221856204255,-29.6932201522123,
121.906899471747)) ;
#46593 = CARTESIAN_POINT('Ctrl Pts',(-19.1338922316553,-29.8830940645654,
122.237651972592)) ;
#46594 = CARTESIAN_POINT('Ctrl Pts',(-19.0650645565921,-29.7031049842026,
121.944106565339)) ;
#46595 = CARTESIAN_POINT('Ctrl Pts',(-18.93291875455,-29.8931614913253,122.303910124113)) ;
#46596 = CARTESIAN_POINT('Ctrl Pts',(-18.8138468784926,-29.7131724109624,
122.026926609439)) ;
#46597 = CARTESIAN_POINT('Ctrl Pts',(-18.7505843551157,-29.9029999804841,
122.40163291113)) ;
#46598 = CARTESIAN_POINT('Ctrl Pts',(-18.5859272208204,-29.7230109001213,
122.149077864787)) ;
#46599 = CARTESIAN_POINT('Ctrl Pts',(-18.5841468216196,-29.9130634616742,
122.532193860216)) ;
#46600 = CARTESIAN_POINT('Ctrl Pts',(-18.3778786570836,-29.7330743813114,
122.312276880641)) ;
#46601 = CARTESIAN_POINT('Ctrl Pts',(-18.445382712112,-29.9229576194894,122.687180679488)) ;
#46602 = CARTESIAN_POINT('Ctrl Pts',(-18.2044212593036,-29.7429685391265,
122.506008820073)) ;
#46603 = CARTESIAN_POINT('Ctrl Pts',(-18.3346512088788,-29.9328994762337,
122.864415832755)) ;
#46604 = CARTESIAN_POINT('Ctrl Pts',(-18.0660044708574,-29.7529103958708,
122.727551566468)) ;
#46605 = CARTESIAN_POINT('Ctrl Pts',(-18.2558045501675,-29.9429019539051,
123.059389134583)) ;
#46606 = CARTESIAN_POINT('Ctrl Pts',(-17.9674436496093,-29.7629128735422,
122.971267274101)) ;
#46607 = CARTESIAN_POINT('Ctrl Pts',(-18.2122015809126,-29.9529367582094,
123.265783338575)) ;
#46608 = CARTESIAN_POINT('Ctrl Pts',(-17.9129372902024,-29.7729476778465,
123.229259453664)) ;
#46609 = CARTESIAN_POINT('Ctrl Pts',(-18.204883750954,-29.962781635055,123.472638058067)) ;
#46610 = CARTESIAN_POINT('Ctrl Pts',(-17.9037873257415,-29.7827925546922,
123.487828320676)) ;
#46611 = CARTESIAN_POINT('Ctrl Pts',(-18.2336070809338,-29.9727675146106,
123.680563989553)) ;
#46612 = CARTESIAN_POINT('Ctrl Pts',(-17.9396889314393,-29.7927784342477,
123.747736250522)) ;
#46613 = CARTESIAN_POINT('Ctrl Pts',(-18.2975455094374,-29.9827022449691,
123.879438238451)) ;
#46614 = CARTESIAN_POINT('Ctrl Pts',(-18.0196096204046,-29.8027131646062,
123.996330158484)) ;
#46615 = CARTESIAN_POINT('Ctrl Pts',(-18.3963927749203,-29.992760057282,124.066318685816)) ;
#46616 = CARTESIAN_POINT('Ctrl Pts',(-18.1431663387283,-29.8127709769191,
124.229931834435)) ;
#46617 = CARTESIAN_POINT('Ctrl Pts',(-18.5228873624992,-30.0025806494063,
124.229532798022)) ;
#46618 = CARTESIAN_POINT('Ctrl Pts',(-18.3012830487912,-29.8225915690435,
124.433951656902)) ;
#46619 = CARTESIAN_POINT('Ctrl Pts',(-18.6793976240298,-30.0126472350161,
124.371920994788)) ;
#46620 = CARTESIAN_POINT('Ctrl Pts',(-18.4969190824133,-29.8326581546532,
124.611938648179)) ;
#46621 = CARTESIAN_POINT('Ctrl Pts',(-18.8553834505121,-30.0225468155979,
124.483111642296)) ;
#46622 = CARTESIAN_POINT('Ctrl Pts',(-18.7169004533599,-29.8425577352351,
124.750929340355)) ;
#46623 = CARTESIAN_POINT('Ctrl Pts',(-19.0508479412311,-30.0325984152762,
124.563308795256)) ;
#46624 = CARTESIAN_POINT('Ctrl Pts',(-18.9612300162177,-29.8526093349133,
124.851178041536)) ;
#46625 = CARTESIAN_POINT('Ctrl Pts',(-19.2536676439756,-30.0424726016932,
124.607724013289)) ;
#46626 = CARTESIAN_POINT('Ctrl Pts',(-19.2147547487882,-29.8624835213303,
124.90669960071)) ;
#46627 = CARTESIAN_POINT('Ctrl Pts',(-19.4648637458808,-30.0525290775741,
124.616538418553)) ;
#46628 = CARTESIAN_POINT('Ctrl Pts',(-19.4787496446823,-29.8725399972112,
124.917720031893)) ;
#46629 = CARTESIAN_POINT('Ctrl Pts',(-19.6710664677573,-30.0624220088767,
124.589069886953)) ;
#46630 = CARTESIAN_POINT('Ctrl Pts',(-19.7365039466463,-29.8824329285138,
124.883386677831)) ;
#46631 = CARTESIAN_POINT('Ctrl Pts',(-19.8727094603673,-30.0724847875893,
124.525198764561)) ;
#46632 = CARTESIAN_POINT('Ctrl Pts',(-19.9885582400929,-29.8924957072264,
124.803550123632)) ;
#46633 = CARTESIAN_POINT('Ctrl Pts',(-20.0561959945725,-30.0823273131705,
124.429495466673)) ;
#46634 = CARTESIAN_POINT('Ctrl Pts',(-20.2179182729383,-29.9023382328076,
124.683922711731)) ;
#46635 = CARTESIAN_POINT('Ctrl Pts',(-20.2230137933602,-30.0923180785953,
124.301917210482)) ;
#46636 = CARTESIAN_POINT('Ctrl Pts',(-20.4264420362186,-29.9123289982325,
124.524451584241)) ;
#46637 = CARTESIAN_POINT('Ctrl Pts',(-20.364251196426,-30.1022461545934,124.148229737283)) ;
#46638 = CARTESIAN_POINT('Ctrl Pts',(-20.6029907905239,-29.9222570742305,
124.332343420825)) ;
#46639 = CARTESIAN_POINT('Ctrl Pts',(-20.4776444590878,-30.1122340649804,
123.971491927839)) ;
#46640 = CARTESIAN_POINT('Ctrl Pts',(-20.7447343008597,-29.9322449846175,
124.11142218186)) ;
#46641 = CARTESIAN_POINT('Ctrl Pts',(-20.5586797306925,-30.1222699771053,
123.776696813867)) ;
#46642 = CARTESIAN_POINT('Ctrl Pts',(-20.8460304545597,-29.9422808967425,
123.867929241378)) ;
#46643 = CARTESIAN_POINT('Ctrl Pts',(-20.6041716223551,-30.132124989953,123.57455346389)) ;
#46644 = CARTESIAN_POINT('Ctrl Pts',(-20.9028976475888,-29.9521359095901,
123.61524963978)) ;
#46645 = CARTESIAN_POINT('Ctrl Pts',(-20.6143059846248,-30.1421239358693,
123.364622415793)) ;
#46646 = CARTESIAN_POINT('Ctrl Pts',(-20.9155677101948,-29.9621348555064,
123.352835793816)) ;
#46647 = CARTESIAN_POINT('Ctrl Pts',(-20.5882986886202,-30.1520208483173,
123.158157718472)) ;
#46648 = CARTESIAN_POINT('Ctrl Pts',(-20.8830605294398,-29.9720317679544,
123.094753953415)) ;
#46649 = CARTESIAN_POINT('Ctrl Pts',(-20.5259041849406,-30.1620746464108,
122.956241447257)) ;
#46650 = CARTESIAN_POINT('Ctrl Pts',(-20.805069403928,-29.9820855660479,122.84235819033)) ;
#46651 = CARTESIAN_POINT('Ctrl Pts',(-20.4310894011429,-30.1719555672375,
122.771388410386)) ;
#46652 = CARTESIAN_POINT('Ctrl Pts',(-20.6865523391872,-29.9919664868746,
122.611290225832)) ;
#46653 = CARTESIAN_POINT('Ctrl Pts',(-20.3043799559765,-30.1819600932352,
122.603543945781)) ;
#46654 = CARTESIAN_POINT('Ctrl Pts',(-20.5281670015566,-30.0019710128723,
122.40148341337)) ;
#46655 = CARTESIAN_POINT('Ctrl Pts',(-20.1506815547945,-30.1919440568527,
122.460549966187)) ;
#46656 = CARTESIAN_POINT('Ctrl Pts',(-20.3360451640396,-30.0119549764898,
122.222739387201)) ;
#46657 = CARTESIAN_POINT('Ctrl Pts',(-19.9734411230241,-30.201983697404,122.345973899521)) ;
#46658 = CARTESIAN_POINT('Ctrl Pts',(-20.1144958155581,-30.0219946170411,
122.079517699187)) ;
#46659 = CARTESIAN_POINT('Ctrl Pts',(-19.782871813628,-30.2118277230187,122.26527172513)) ;
#46660 = CARTESIAN_POINT('Ctrl Pts',(-19.8762838854574,-30.0318386426558,
121.978637774701)) ;
#46661 = CARTESIAN_POINT('Ctrl Pts',(-19.5783094050863,-30.221818728836,122.217602614152)) ;
#46662 = CARTESIAN_POINT('Ctrl Pts',(-19.6205810796489,-30.0418296484732,
121.919049659348)) ;
#46663 = CARTESIAN_POINT('Ctrl Pts',(-19.3675704704491,-30.2318565203682,
122.206603916104)) ;
#46664 = CARTESIAN_POINT('Ctrl Pts',(-19.3571576412147,-30.0518674400053,
121.905299416152)) ;
#46665 = CARTESIAN_POINT('Ctrl Pts',(-19.1621069099491,-30.2417009201566,
122.231506538147)) ;
#46666 = CARTESIAN_POINT('Ctrl Pts',(-19.1003268169004,-30.0617118397937,
121.936426083733)) ;
#46667 = CARTESIAN_POINT('Ctrl Pts',(-18.9611771135097,-30.2516857207133,
122.292157840187)) ;
#46668 = CARTESIAN_POINT('Ctrl Pts',(-18.8491638611297,-30.0716966403505,
122.012238721689)) ;
#46669 = CARTESIAN_POINT('Ctrl Pts',(-18.7745889266096,-30.2616252441245,
122.386291238736)) ;
#46670 = CARTESIAN_POINT('Ctrl Pts',(-18.6159274223169,-30.0816361637616,
122.129904287764)) ;
#46671 = CARTESIAN_POINT('Ctrl Pts',(-18.6055578608464,-30.2716649632255,
122.512666339246)) ;
#46672 = CARTESIAN_POINT('Ctrl Pts',(-18.4046377386934,-30.0916758828626,
122.287871780247)) ;
#46673 = CARTESIAN_POINT('Ctrl Pts',(-18.4631237680064,-30.2815531351448,
122.664098676228)) ;
#46674 = CARTESIAN_POINT('Ctrl Pts',(-18.2265933390173,-30.1015640547819,
122.477161788335)) ;
#46675 = CARTESIAN_POINT('Ctrl Pts',(-18.3476602750316,-30.2915426975618,
122.839512639782)) ;
#46676 = CARTESIAN_POINT('Ctrl Pts',(-18.0822626446461,-30.1115536171989,
122.696428624441)) ;
#46677 = CARTESIAN_POINT('Ctrl Pts',(-18.264811021222,-30.3015010697565,123.031774138297)) ;
#46678 = CARTESIAN_POINT('Ctrl Pts',(-17.9786995241896,-30.1215119893936,
122.936755300708)) ;
#46679 = CARTESIAN_POINT('Ctrl Pts',(-18.2163954880168,-30.3114011439872,
123.234202863219)) ;
#46680 = CARTESIAN_POINT('Ctrl Pts',(-17.9181786121953,-30.1314120636243,
123.189791746356)) ;
#46681 = CARTESIAN_POINT('Ctrl Pts',(-18.2037078203567,-30.3214472403608,
123.445012427325)) ;
#46682 = CARTESIAN_POINT('Ctrl Pts',(-17.9023177046355,-30.1414581599979,
123.453303427384)) ;
#46683 = CARTESIAN_POINT('Ctrl Pts',(-18.2274762171961,-30.3313558243579,
123.651971116123)) ;
#46684 = CARTESIAN_POINT('Ctrl Pts',(-17.9320269697077,-30.151366743995,123.712002752069)) ;
#46685 = CARTESIAN_POINT('Ctrl Pts',(-18.2870541787712,-30.3413664029488,
123.853819127414)) ;
#46686 = CARTESIAN_POINT('Ctrl Pts',(-18.0064982865296,-30.1613773225859,
123.964313150607)) ;
#46687 = CARTESIAN_POINT('Ctrl Pts',(-18.3813325232713,-30.3513955610616,
124.042419862782)) ;
#46688 = CARTESIAN_POINT('Ctrl Pts',(-18.1243449648106,-30.1714064806987,
124.200064581345)) ;
#46689 = CARTESIAN_POINT('Ctrl Pts',(-18.5044666604839,-30.3612484428997,
124.20896945013)) ;
#46690 = CARTESIAN_POINT('Ctrl Pts',(-18.2782623863857,-30.1812593625368,
124.408253321648)) ;
#46691 = CARTESIAN_POINT('Ctrl Pts',(-18.6558439163059,-30.3712080040507,
124.353634907533)) ;
#46692 = CARTESIAN_POINT('Ctrl Pts',(-18.4674836005063,-30.1912189236878,
124.589086196399)) ;
#46693 = CARTESIAN_POINT('Ctrl Pts',(-18.8316171646393,-30.3812464386398,
124.470406891884)) ;
#46694 = CARTESIAN_POINT('Ctrl Pts',(-18.687199388826,-30.2012573582769,124.735052040734)) ;
#46695 = CARTESIAN_POINT('Ctrl Pts',(-19.0216991726386,-30.3911197108669,
124.553872844899)) ;
#46696 = CARTESIAN_POINT('Ctrl Pts',(-18.9248025261078,-30.211130630504,124.839385850343)) ;
#46697 = CARTESIAN_POINT('Ctrl Pts',(-19.2274128061745,-30.4011929528604,
124.603980425918)) ;
#46698 = CARTESIAN_POINT('Ctrl Pts',(-19.1819439103011,-30.2212038724976,
124.902021223868)) ;
#46699 = CARTESIAN_POINT('Ctrl Pts',(-19.4334667110816,-30.4110132843935,
124.617542684811)) ;
#46700 = CARTESIAN_POINT('Ctrl Pts',(-19.4395127810917,-30.2310242040306,
124.918975069592)) ;
#46701 = CARTESIAN_POINT('Ctrl Pts',(-19.64406951049,-30.4210919456203,124.594736003978)) ;
#46702 = CARTESIAN_POINT('Ctrl Pts',(-19.7027659038404,-30.2411028652574,
124.890467615748)) ;
#46703 = CARTESIAN_POINT('Ctrl Pts',(-19.8430448442677,-30.4309435409145,
124.537080259069)) ;
#46704 = CARTESIAN_POINT('Ctrl Pts',(-19.9514865660436,-30.2509544605516,
124.818398357271)) ;
#46705 = CARTESIAN_POINT('Ctrl Pts',(-20.0331712259711,-30.4410166761433,
124.443902678436)) ;
#46706 = CARTESIAN_POINT('Ctrl Pts',(-20.1891444820223,-30.2610275957804,
124.701927251076)) ;
#46707 = CARTESIAN_POINT('Ctrl Pts',(-20.200339647076,-30.4508591116683,124.32192778539)) ;
#46708 = CARTESIAN_POINT('Ctrl Pts',(-20.398106604193,-30.2708700313055,124.549458419366)) ;
#46709 = CARTESIAN_POINT('Ctrl Pts',(-20.3462888347876,-30.4608398808017,
124.171191115801)) ;
#46710 = CARTESIAN_POINT('Ctrl Pts',(-20.5805436587888,-30.2808508004389,
124.361037704408)) ;
#46711 = CARTESIAN_POINT('Ctrl Pts',(-20.4639585613339,-30.4708569820456,
123.996541687798)) ;
#46712 = CARTESIAN_POINT('Ctrl Pts',(-20.7276313527105,-30.2908679016827,
124.142726286126)) ;
#46713 = CARTESIAN_POINT('Ctrl Pts',(-20.5487810389583,-30.4807454296474,
123.806730562509)) ;
#46714 = CARTESIAN_POINT('Ctrl Pts',(-20.8336603363903,-30.3007563492846,
123.905461600815)) ;
#46715 = CARTESIAN_POINT('Ctrl Pts',(-20.6002259549947,-30.4908011438283,
123.601702375123)) ;
#46716 = CARTESIAN_POINT('Ctrl Pts',(-20.897966874934,-30.3108120634654,123.649176787978)) ;
#46717 = CARTESIAN_POINT('Ctrl Pts',(-20.615052892875,-30.5006763502421,123.394610916813)) ;
#46718 = CARTESIAN_POINT('Ctrl Pts',(-20.916501105489,-30.3206872698793,123.390311340077)) ;
#46719 = CARTESIAN_POINT('Ctrl Pts',(-20.5939426510148,-30.5106714027149,
123.185552599972)) ;
#46720 = CARTESIAN_POINT('Ctrl Pts',(-20.8901135577961,-30.330682322352,123.128988240062)) ;
#46721 = CARTESIAN_POINT('Ctrl Pts',(-20.536367759922,-30.520693286677,122.982872051517)) ;
#46722 = CARTESIAN_POINT('Ctrl Pts',(-20.8181453544106,-30.3407042063141,
122.87563748445)) ;
#46723 = CARTESIAN_POINT('Ctrl Pts',(-20.4457706611139,-30.5305972592063,
122.795404854875)) ;
#46724 = CARTESIAN_POINT('Ctrl Pts',(-20.7048988527743,-30.3506081788434,
122.641302484579)) ;
#46725 = CARTESIAN_POINT('Ctrl Pts',(-20.3232033140456,-30.5405857558672,
122.624895059131)) ;
#46726 = CARTESIAN_POINT('Ctrl Pts',(-20.5516896929561,-30.3605966755043,
122.428164932682)) ;
#46727 = CARTESIAN_POINT('Ctrl Pts',(-20.1731729387286,-30.5505495531152,
122.478730184432)) ;
#46728 = CARTESIAN_POINT('Ctrl Pts',(-20.3641515811051,-30.3705604727523,
122.245458339291)) ;
#46729 = CARTESIAN_POINT('Ctrl Pts',(-20.0013435844137,-30.5604535764232,
122.361105057577)) ;
#46730 = CARTESIAN_POINT('Ctrl Pts',(-20.1493641423966,-30.3804644960603,
122.098426355358)) ;
#46731 = CARTESIAN_POINT('Ctrl Pts',(-19.8086729775666,-30.5705140797448,
122.27392287476)) ;
#46732 = CARTESIAN_POINT('Ctrl Pts',(-19.9085262576648,-30.3905249993819,
121.989448658708)) ;
#46733 = CARTESIAN_POINT('Ctrl Pts',(-19.6082855481598,-30.5803546148847,
122.222396123201)) ;
#46734 = CARTESIAN_POINT('Ctrl Pts',(-19.6580405512922,-30.4003655345218,
121.925039834791)) ;
#46735 = CARTESIAN_POINT('Ctrl Pts',(-19.3974190538605,-30.5904168355893,
122.20582075455)) ;
#46736 = CARTESIAN_POINT('Ctrl Pts',(-19.3944577950573,-30.4104277552264,
121.904320740095)) ;
#46737 = CARTESIAN_POINT('Ctrl Pts',(-19.1903195961826,-30.6003139893655,
122.225997239462)) ;
#46738 = CARTESIAN_POINT('Ctrl Pts',(-19.1355824753204,-30.4203249090026,
121.929541442186)) ;
#46739 = CARTESIAN_POINT('Ctrl Pts',(-18.9890100939322,-30.610245122751,122.281343791059)) ;
#46740 = CARTESIAN_POINT('Ctrl Pts',(-18.8839449757999,-30.4302560423881,
121.998725090014)) ;
#46741 = CARTESIAN_POINT('Ctrl Pts',(-18.7983550338524,-30.6202874978967,
122.372017641209)) ;
#46742 = CARTESIAN_POINT('Ctrl Pts',(-18.6456264180008,-30.4402984175338,
122.112067478881)) ;
#46743 = CARTESIAN_POINT('Ctrl Pts',(-18.6289139729558,-30.6301734356628,
122.492389628347)) ;
#46744 = CARTESIAN_POINT('Ctrl Pts',(-18.4338243469554,-30.4501843553,122.26253329312)) ;
#46745 = CARTESIAN_POINT('Ctrl Pts',(-18.4811125942436,-30.6401692786477,
122.641749676501)) ;
#46746 = CARTESIAN_POINT('Ctrl Pts',(-18.2490727524169,-30.4601801982848,
122.449233759781)) ;
#46747 = CARTESIAN_POINT('Ctrl Pts',(-18.3621388083306,-30.6501112565263,
122.813609855738)) ;
#46748 = CARTESIAN_POINT('Ctrl Pts',(-18.1003554686225,-30.4701221761634,
122.664059702261)) ;
#46749 = CARTESIAN_POINT('Ctrl Pts',(-18.2744107318474,-30.6600706310073,
123.003708981063)) ;
#46750 = CARTESIAN_POINT('Ctrl Pts',(-17.9906956060769,-30.4800815506444,
122.901684237793)) ;
#46751 = CARTESIAN_POINT('Ctrl Pts',(-18.2207100016037,-30.6700672468411,
123.206915248933)) ;
#46752 = CARTESIAN_POINT('Ctrl Pts',(-17.9235701573867,-30.4900781664782,
123.15569235127)) ;
#46753 = CARTESIAN_POINT('Ctrl Pts',(-18.2033237827632,-30.6801014654146,
123.4171423923)) ;
#46754 = CARTESIAN_POINT('Ctrl Pts',(-17.9018377987369,-30.5001123850517,
123.418476175523)) ;
#46755 = CARTESIAN_POINT('Ctrl Pts',(-18.2221037500632,-30.6899545326252,
123.623428518409)) ;
#46756 = CARTESIAN_POINT('Ctrl Pts',(-17.9253133851979,-30.5099654522623,
123.676335153502)) ;
#46757 = CARTESIAN_POINT('Ctrl Pts',(-18.2764164848045,-30.6999147905028,
123.825650685452)) ;
#46758 = CARTESIAN_POINT('Ctrl Pts',(-17.9932051454583,-30.5199257101399,
123.929113114964)) ;
#46759 = CARTESIAN_POINT('Ctrl Pts',(-18.3658619188668,-30.7099438172084,
124.016591993771)) ;
#46760 = CARTESIAN_POINT('Ctrl Pts',(-18.1050124820995,-30.5299547368455,
124.167789386581)) ;
#46761 = CARTESIAN_POINT('Ctrl Pts',(-18.4856036512729,-30.7198540242428,
124.187076921124)) ;
#46762 = CARTESIAN_POINT('Ctrl Pts',(-18.2546907015098,-30.5398649438799,
124.380895877564)) ;
#46763 = CARTESIAN_POINT('Ctrl Pts',(-18.6331183540979,-30.7297889348904,
124.334947217682)) ;
#46764 = CARTESIAN_POINT('Ctrl Pts',(-18.4390851726062,-30.5497998545275,
124.565733591977)) ;
#46765 = CARTESIAN_POINT('Ctrl Pts',(-18.805998293057,-30.7398300650696,124.456072455855)) ;
#46766 = CARTESIAN_POINT('Ctrl Pts',(-18.6551854058701,-30.5598409847068,
124.71713937099)) ;
#46767 = CARTESIAN_POINT('Ctrl Pts',(-18.9943042437929,-30.7497172054396,
124.544111417618)) ;
#46768 = CARTESIAN_POINT('Ctrl Pts',(-18.8905691522215,-30.5697281250767,
124.827187732175)) ;
#46769 = CARTESIAN_POINT('Ctrl Pts',(-19.1970545158081,-30.7597094829755,
124.599022917554)) ;
#46770 = CARTESIAN_POINT('Ctrl Pts',(-19.1440074490238,-30.5797204026127,
124.895826199179)) ;
#46771 = CARTESIAN_POINT('Ctrl Pts',(-19.4053746987768,-30.7696580262439,
124.617756988556)) ;
#46772 = CARTESIAN_POINT('Ctrl Pts',(-19.4044083048242,-30.589668945881,124.919242868932)) ;
#46773 = CARTESIAN_POINT('Ctrl Pts',(-19.6135329763721,-30.7795947010611,
124.60035612135)) ;
#46774 = CARTESIAN_POINT('Ctrl Pts',(-19.6646066985077,-30.5996056206982,
124.897490650973)) ;
#46775 = CARTESIAN_POINT('Ctrl Pts',(-19.8165585167842,-30.7895781219974,
124.5470606735)) ;
#46776 = CARTESIAN_POINT('Ctrl Pts',(-19.9183885696594,-30.6095890416346,
124.830870140857)) ;
#46777 = CARTESIAN_POINT('Ctrl Pts',(-20.0081989085124,-30.7996204371867,
124.458507416817)) ;
#46778 = CARTESIAN_POINT('Ctrl Pts',(-20.1579384638186,-30.6196313568238,
124.720177686834)) ;
#46779 = CARTESIAN_POINT('Ctrl Pts',(-20.1782668651698,-30.8094607546259,
124.340716223305)) ;
#46780 = CARTESIAN_POINT('Ctrl Pts',(-20.3705238609549,-30.629471674263,124.572936951925)) ;
#46781 = CARTESIAN_POINT('Ctrl Pts',(-20.328476682033,-30.8194904586834,124.192735300873)) ;
#46782 = CARTESIAN_POINT('Ctrl Pts',(-20.5582851075911,-30.6395013783205,
124.387959911787)) ;
#46783 = CARTESIAN_POINT('Ctrl Pts',(-20.4501392005903,-30.8295114154059,
124.020744611247)) ;
#46784 = CARTESIAN_POINT('Ctrl Pts',(-20.7103623023063,-30.649522335043,124.172970910553)) ;
#46785 = CARTESIAN_POINT('Ctrl Pts',(-20.5391909200879,-30.8393779577095,
123.833391228608)) ;
#46786 = CARTESIAN_POINT('Ctrl Pts',(-20.8216762306296,-30.6593888773466,
123.938777584491)) ;
#46787 = CARTESIAN_POINT('Ctrl Pts',(-20.595495855653,-30.8494490576546,123.629308992589)) ;
#46788 = CARTESIAN_POINT('Ctrl Pts',(-20.8920560097773,-30.6694599772918,
123.683674797178)) ;
#46789 = CARTESIAN_POINT('Ctrl Pts',(-20.6150525003595,-30.8592911318322,
123.423316450362)) ;
#46790 = CARTESIAN_POINT('Ctrl Pts',(-20.9165006065021,-30.6793020514693,
123.426182698946)) ;
#46791 = CARTESIAN_POINT('Ctrl Pts',(-20.5991170580468,-30.8692519264192,
123.214521188728)) ;
#46792 = CARTESIAN_POINT('Ctrl Pts',(-20.8965796706122,-30.6892628460564,
123.165188338066)) ;
#46793 = CARTESIAN_POINT('Ctrl Pts',(-20.546363865341,-30.8792897993201,123.010200870518)) ;
#46794 = CARTESIAN_POINT('Ctrl Pts',(-20.8306367978976,-30.6993007189572,
122.909788435439)) ;
#46795 = CARTESIAN_POINT('Ctrl Pts',(-20.4606968836195,-30.8891640848642,
122.821085418058)) ;
#46796 = CARTESIAN_POINT('Ctrl Pts',(-20.7235512011237,-30.7091750045013,
122.673393853135)) ;
#46797 = CARTESIAN_POINT('Ctrl Pts',(-20.3411946934181,-30.8992338352781,
122.646376318982)) ;
#46798 = CARTESIAN_POINT('Ctrl Pts',(-20.5741723489282,-30.7192447549152,
122.45500866596)) ;
#46799 = CARTESIAN_POINT('Ctrl Pts',(-20.19669738145,-30.9090671198127,122.498514065535)) ;
#46800 = CARTESIAN_POINT('Ctrl Pts',(-20.3935486500737,-30.7290780394499,
122.270181067719)) ;
#46801 = CARTESIAN_POINT('Ctrl Pts',(-20.025723038719,-30.9190974606128,122.375099669013)) ;
#46802 = CARTESIAN_POINT('Ctrl Pts',(-20.1798297267143,-30.7391083802499,
122.115914599699)) ;
#46803 = CARTESIAN_POINT('Ctrl Pts',(-19.8356036746159,-30.9291293846124,
122.283783083488)) ;
#46804 = CARTESIAN_POINT('Ctrl Pts',(-19.9421798972545,-30.7491403042495,
122.001770363478)) ;
#46805 = CARTESIAN_POINT('Ctrl Pts',(-19.6367747487569,-30.9389579195483,
122.227591752257)) ;
#46806 = CARTESIAN_POINT('Ctrl Pts',(-19.6936420289257,-30.7589688391854,
121.931532551847)) ;
#46807 = CARTESIAN_POINT('Ctrl Pts',(-19.4278031799893,-30.948951697313,122.205853025162)) ;
#46808 = CARTESIAN_POINT('Ctrl Pts',(-19.4324272173847,-30.7689626169501,
121.904361062443)) ;
#46809 = CARTESIAN_POINT('Ctrl Pts',(-19.2175414225101,-30.9589794077985,
122.221194257031)) ;
#46810 = CARTESIAN_POINT('Ctrl Pts',(-19.1696001927807,-30.7789903274356,
121.923539411999)) ;
#46811 = CARTESIAN_POINT('Ctrl Pts',(-19.0159184250757,-30.9688678186325,
122.271841404524)) ;
#46812 = CARTESIAN_POINT('Ctrl Pts',(-18.9175710994844,-30.7888787382696,
121.986850390428)) ;
#46813 = CARTESIAN_POINT('Ctrl Pts',(-18.8243211742747,-30.978844669168,122.357145110244)) ;
#46814 = CARTESIAN_POINT('Ctrl Pts',(-18.6780751168425,-30.7988555888051,
122.09348195838)) ;
#46815 = CARTESIAN_POINT('Ctrl Pts',(-18.6501372622533,-30.9888364657185,
122.474607486696)) ;
#46816 = CARTESIAN_POINT('Ctrl Pts',(-18.4603462228554,-30.8088473853556,
122.240311680779)) ;
#46817 = CARTESIAN_POINT('Ctrl Pts',(-18.4985386548746,-30.9988724718122,
122.621327863081)) ;
#46818 = CARTESIAN_POINT('Ctrl Pts',(-18.2708493730239,-30.8188833914493,
122.42371347671)) ;
#46819 = CARTESIAN_POINT('Ctrl Pts',(-18.3767267027261,-31.008723206075,122.788826198165)) ;
#46820 = CARTESIAN_POINT('Ctrl Pts',(-18.1185854663055,-30.8287341257121,
122.633088418445)) ;
#46821 = CARTESIAN_POINT('Ctrl Pts',(-18.2842463817907,-31.0187144646032,
122.977386152329)) ;
#46822 = CARTESIAN_POINT('Ctrl Pts',(-18.0029869058182,-30.8387253842403,
122.868789450594)) ;
#46823 = CARTESIAN_POINT('Ctrl Pts',(-18.2262044455862,-31.0286323595064,
123.177677702795)) ;
#46824 = CARTESIAN_POINT('Ctrl Pts',(-17.9304364001845,-30.8486432791435,
123.119155041273)) ;
#46825 = CARTESIAN_POINT('Ctrl Pts',(-18.2035238002497,-31.0386605011694,
123.387260137324)) ;
#46826 = CARTESIAN_POINT('Ctrl Pts',(-17.9020877614499,-30.8586714208065,
123.3811332833)) ;
#46827 = CARTESIAN_POINT('Ctrl Pts',(-18.2172919464805,-31.0485456692853,
123.594625950143)) ;
#46828 = CARTESIAN_POINT('Ctrl Pts',(-17.9193001864898,-30.8685565889224,
123.640341140622)) ;
#46829 = CARTESIAN_POINT('Ctrl Pts',(-18.2668826506638,-31.0585350327913,
123.79869899324)) ;
#46830 = CARTESIAN_POINT('Ctrl Pts',(-17.9812908655851,-30.8785459524284,
123.895432047551)) ;
#46831 = CARTESIAN_POINT('Ctrl Pts',(-18.3519971283237,-31.0685761678013,
123.991875632271)) ;
#46832 = CARTESIAN_POINT('Ctrl Pts',(-18.0876859531419,-30.8885870874385,
124.136901868337)) ;
#46833 = CARTESIAN_POINT('Ctrl Pts',(-18.4666381472819,-31.0784088359894,
124.163882158032)) ;
#46834 = CARTESIAN_POINT('Ctrl Pts',(-18.2309896742768,-30.8984197556265,
124.35190954771)) ;
#46835 = CARTESIAN_POINT('Ctrl Pts',(-18.6113111204173,-31.0884027389439,
124.31623927594)) ;
#46836 = CARTESIAN_POINT('Ctrl Pts',(-18.4118327452605,-30.908413658581,124.542354351649)) ;
#46837 = CARTESIAN_POINT('Ctrl Pts',(-18.7811066172618,-31.0984320240284,
124.441246279883)) ;
#46838 = CARTESIAN_POINT('Ctrl Pts',(-18.6240784848063,-30.9184429436655,
124.698611210536)) ;
#46839 = CARTESIAN_POINT('Ctrl Pts',(-18.9669894085724,-31.1083075524703,
124.533744474352)) ;
#46840 = CARTESIAN_POINT('Ctrl Pts',(-18.856433654806,-30.9283184721074,124.814232093926)) ;
#46841 = CARTESIAN_POINT('Ctrl Pts',(-19.1685234135853,-31.1183078350863,
124.593519235339)) ;
#46842 = CARTESIAN_POINT('Ctrl Pts',(-19.1083519713591,-30.9383187547235,
124.888948210804)) ;
#46843 = CARTESIAN_POINT('Ctrl Pts',(-19.3755624886653,-31.1282198511434,
124.617355261767)) ;
#46844 = CARTESIAN_POINT('Ctrl Pts',(-19.3671515658204,-30.9482307707805,
124.918740815708)) ;
#46845 = CARTESIAN_POINT('Ctrl Pts',(-19.5862881147713,-31.1382619264824,
124.604773299215)) ;
#46846 = CARTESIAN_POINT('Ctrl Pts',(-19.6305583756846,-30.9582728461195,
124.903010863025)) ;
#46847 = CARTESIAN_POINT('Ctrl Pts',(-19.7887432035316,-31.1481617591385,
124.556475850266)) ;
#46848 = CARTESIAN_POINT('Ctrl Pts',(-19.8836271403426,-30.9681726787756,
124.842636496997)) ;
#46849 = CARTESIAN_POINT('Ctrl Pts',(-19.9816984118981,-31.1581541597165,
124.473418066137)) ;
#46850 = CARTESIAN_POINT('Ctrl Pts',(-20.1248202353029,-30.9781650793536,
124.738811837685)) ;
#46851 = CARTESIAN_POINT('Ctrl Pts',(-20.1578289058847,-31.1681881814759,
124.357322944161)) ;
#46852 = CARTESIAN_POINT('Ctrl Pts',(-20.3449819506173,-30.988199101113,124.593690835872)) ;
#46853 = CARTESIAN_POINT('Ctrl Pts',(-20.3087153180884,-31.1780527923171,
124.215054802295)) ;
#46854 = CARTESIAN_POINT('Ctrl Pts',(-20.5335886314549,-30.9980637119542,
124.415853378407)) ;
#46855 = CARTESIAN_POINT('Ctrl Pts',(-20.4346283251563,-31.1880451917782,
124.046895705598)) ;
#46856 = CARTESIAN_POINT('Ctrl Pts',(-20.6909778265813,-31.0080561114154,
124.205652827145)) ;
#46857 = CARTESIAN_POINT('Ctrl Pts',(-20.5294345452315,-31.1980771451111,
123.858502766262)) ;
#46858 = CARTESIAN_POINT('Ctrl Pts',(-20.8094832862645,-31.0180880647483,
123.970160489407)) ;
#46859 = CARTESIAN_POINT('Ctrl Pts',(-20.5893954841832,-31.2079435040528,
123.659927548445)) ;
#46860 = CARTESIAN_POINT('Ctrl Pts',(-20.8844320812118,-31.0279544236899,
123.721940205726)) ;
#46861 = CARTESIAN_POINT('Ctrl Pts',(-20.6146037556417,-31.2179309795386,
123.451503773627)) ;
#46862 = CARTESIAN_POINT('Ctrl Pts',(-20.9159397608911,-31.0379418991757,
123.461410041658)) ;
#46863 = CARTESIAN_POINT('Ctrl Pts',(-20.6033971471085,-31.2278758857271,
123.24270000188)) ;
#46864 = CARTESIAN_POINT('Ctrl Pts',(-20.9019287886433,-31.0478868053642,
123.200405236579)) ;
#46865 = CARTESIAN_POINT('Ctrl Pts',(-20.5555242405054,-31.2379208503873,
123.037041915201)) ;
#46866 = CARTESIAN_POINT('Ctrl Pts',(-20.8420850390457,-31.0579317700244,
122.943333258433)) ;
#46867 = CARTESIAN_POINT('Ctrl Pts',(-20.4743386324737,-31.2477826572922,
122.846253520561)) ;
#46868 = CARTESIAN_POINT('Ctrl Pts',(-20.7406003647243,-31.0677935769293,
122.704848430439)) ;
#46869 = CARTESIAN_POINT('Ctrl Pts',(-20.360117950421,-31.2577753295979,122.669966551316)) ;
#46870 = CARTESIAN_POINT('Ctrl Pts',(-20.597822144092,-31.0777862492351,122.484491140274)) ;
#46871 = CARTESIAN_POINT('Ctrl Pts',(-20.2178975470522,-31.2677040005433,
122.51716583229)) ;
#46872 = CARTESIAN_POINT('Ctrl Pts',(-20.4200444703197,-31.0877149201804,
122.293491951008)) ;
#46873 = CARTESIAN_POINT('Ctrl Pts',(-20.0511349253016,-31.2776565427686,
122.390821276081)) ;
#46874 = CARTESIAN_POINT('Ctrl Pts',(-20.2115893827837,-31.0976674624057,
122.135563380117)) ;
#46875 = CARTESIAN_POINT('Ctrl Pts',(-19.8640731557152,-31.2876578987645,
122.294767252677)) ;
#46876 = CARTESIAN_POINT('Ctrl Pts',(-19.9777608298293,-31.1076688184016,
122.015498299379)) ;
#46877 = CARTESIAN_POINT('Ctrl Pts',(-19.6625721454269,-31.2976865110392,
122.232767913839)) ;
#46878 = CARTESIAN_POINT('Ctrl Pts',(-19.7258837090503,-31.1176974306763,
121.93800176093)) ;
#46879 = CARTESIAN_POINT('Ctrl Pts',(-19.4568083883109,-31.3075508455887,
122.20682000382)) ;
#46880 = CARTESIAN_POINT('Ctrl Pts',(-19.468678402315,-31.1275617652258,121.905569609794)) ;
#46881 = CARTESIAN_POINT('Ctrl Pts',(-19.2470034323369,-31.3175431696653,
122.216797567056)) ;
#46882 = CARTESIAN_POINT('Ctrl Pts',(-19.2064222623212,-31.1375540893024,
121.918044378445)) ;
#46883 = CARTESIAN_POINT('Ctrl Pts',(-19.0433631987087,-31.3274706620311,
122.26264289437)) ;
#46884 = CARTESIAN_POINT('Ctrl Pts',(-18.9518724580088,-31.1474815816683,
121.975353810798)) ;
#46885 = CARTESIAN_POINT('Ctrl Pts',(-18.8488944828603,-31.337498020582,122.343946304587)) ;
#46886 = CARTESIAN_POINT('Ctrl Pts',(-18.7087875925179,-31.1575089402191,
122.076985697164)) ;
#46887 = CARTESIAN_POINT('Ctrl Pts',(-18.6738227975292,-31.3473844386331,
122.456025056537)) ;
#46888 = CARTESIAN_POINT('Ctrl Pts',(-18.4899494031481,-31.1673953582702,
122.217086576)) ;
#46889 = CARTESIAN_POINT('Ctrl Pts',(-18.5185992416469,-31.3574161733685,
122.598745584505)) ;
#46890 = CARTESIAN_POINT('Ctrl Pts',(-18.2959218218459,-31.1774270930056,
122.395489361766)) ;
#46891 = CARTESIAN_POINT('Ctrl Pts',(-18.3922256515261,-31.3672977546117,
122.76367605931)) ;
#46892 = CARTESIAN_POINT('Ctrl Pts',(-18.1379570317836,-31.1873086742489,
122.601654224087)) ;
#46893 = CARTESIAN_POINT('Ctrl Pts',(-18.2946472022262,-31.3773597326441,
122.951323265286)) ;
#46894 = CARTESIAN_POINT('Ctrl Pts',(-18.0159864387997,-31.1973706522812,
122.836214609579)) ;
#46895 = CARTESIAN_POINT('Ctrl Pts',(-18.2323356671991,-31.3872168110058,
123.148990652215)) ;
#46896 = CARTESIAN_POINT('Ctrl Pts',(-17.9380997062694,-31.2072277306429,
123.083299705092)) ;
#46897 = CARTESIAN_POINT('Ctrl Pts',(-18.2045044604485,-31.3972113841118,
123.357222538529)) ;
#46898 = CARTESIAN_POINT('Ctrl Pts',(-17.9033134792368,-31.2172223037489,
123.343589981846)) ;
#46899 = CARTESIAN_POINT('Ctrl Pts',(-18.2131184967394,-31.4071371803994,
123.565745265259)) ;
#46900 = CARTESIAN_POINT('Ctrl Pts',(-17.9140838363557,-31.2271481000365,
123.604243273479)) ;
#46901 = CARTESIAN_POINT('Ctrl Pts',(-18.2581923238068,-31.4171625475691,
123.771616644239)) ;
#46902 = CARTESIAN_POINT('Ctrl Pts',(-17.9704288396952,-31.2371734672062,
123.861581949243)) ;
#46903 = CARTESIAN_POINT('Ctrl Pts',(-18.3372215849961,-31.427058627223,123.964077719536)) ;
#46904 = CARTESIAN_POINT('Ctrl Pts',(-18.0692181290173,-31.2470695468601,
124.102157307068)) ;
#46905 = CARTESIAN_POINT('Ctrl Pts',(-18.4492191595014,-31.4370537069285,
124.141874347234)) ;
#46906 = CARTESIAN_POINT('Ctrl Pts',(-18.2092168773112,-31.2570646265657,
124.324401074987)) ;
#46907 = CARTESIAN_POINT('Ctrl Pts',(-18.5910734083571,-31.4470787947444,
124.297744881585)) ;
#46908 = CARTESIAN_POINT('Ctrl Pts',(-18.3865390046239,-31.2670897143815,
124.519239586884)) ;
#46909 = CARTESIAN_POINT('Ctrl Pts',(-18.8100884239902,-31.4602626171116,
124.467625344121)) ;
#46910 = CARTESIAN_POINT('Ctrl Pts',(-18.6602990640863,-31.2802735367488,
124.731576473087)) ;
#46911 = CARTESIAN_POINT('Ctrl Pts',(-19.0709153029651,-31.4735847352576,
124.578138378408)) ;
#46912 = CARTESIAN_POINT('Ctrl Pts',(-18.9862948594309,-31.2935956548947,
124.869711357312)) ;
#46913 = CARTESIAN_POINT('Ctrl Pts',(-19.3495941389619,-31.4869639448852,
124.6162385658)) ;
#46914 = CARTESIAN_POINT('Ctrl Pts',(-19.3347015527575,-31.3069748645223,
124.917347223178)) ;
#46915 = CARTESIAN_POINT('Ctrl Pts',(-19.5563094575702,-31.4968021821294,
124.608810856145)) ;
#46916 = CARTESIAN_POINT('Ctrl Pts',(-19.5930836021212,-31.3168131017665,
124.908057132309)) ;
#46917 = CARTESIAN_POINT('Ctrl Pts',(-19.763395166937,-31.5068751053881,124.564668379505)) ;
#46918 = CARTESIAN_POINT('Ctrl Pts',(-19.8519437779237,-31.3268860250252,
124.852876717695)) ;
#46919 = CARTESIAN_POINT('Ctrl Pts',(-19.9554908372654,-31.5167317468432,
124.486904342967)) ;
#46920 = CARTESIAN_POINT('Ctrl Pts',(-20.0920602272961,-31.3367426664803,
124.755670606679)) ;
#46921 = CARTESIAN_POINT('Ctrl Pts',(-20.1337307856986,-31.5267171223493,
124.376027908366)) ;
#46922 = CARTESIAN_POINT('Ctrl Pts',(-20.3148623984286,-31.3467280419864,
124.617067390045)) ;
#46923 = CARTESIAN_POINT('Ctrl Pts',(-20.3414635779869,-31.5400011538097,
124.189405170033)) ;
#46924 = CARTESIAN_POINT('Ctrl Pts',(-20.5745088879433,-31.3600120734468,
124.383813942974)) ;
#46925 = CARTESIAN_POINT('Ctrl Pts',(-20.5342357011611,-31.55651994568,123.895695798079)) ;
#46926 = CARTESIAN_POINT('Ctrl Pts',(-20.8154916492515,-31.3765308653172,
124.016626072661)) ;
#46927 = CARTESIAN_POINT('Ctrl Pts',(-20.615702601322,-31.5733056626867,123.5482462708)) ;
#46928 = CARTESIAN_POINT('Ctrl Pts',(-20.9173070492714,-31.3933165823238,
123.582394229583)) ;
#46929 = CARTESIAN_POINT('Ctrl Pts',(-20.607065235222,-31.5864188111957,123.272686183113)) ;
#46930 = CARTESIAN_POINT('Ctrl Pts',(-20.906515294897,-31.4064297308328,123.237879258058)) ;
#46931 = CARTESIAN_POINT('Ctrl Pts',(-20.5647775941507,-31.5964543602758,
123.066008473396)) ;
#46932 = CARTESIAN_POINT('Ctrl Pts',(-20.8536524123544,-31.416465279913,122.97954630541)) ;
#46933 = CARTESIAN_POINT('Ctrl Pts',(-20.4868139035535,-31.6064704164553,
122.870382663184)) ;
#46934 = CARTESIAN_POINT('Ctrl Pts',(-20.7561932613821,-31.4264813360924,
122.73500867879)) ;
#46935 = CARTESIAN_POINT('Ctrl Pts',(-20.3416392377526,-31.6196484523213,
122.634448176635)) ;
#46936 = CARTESIAN_POINT('Ctrl Pts',(-20.5747356330736,-31.4396593719584,
122.440107128178)) ;
#46937 = CARTESIAN_POINT('Ctrl Pts',(-20.0859156395753,-31.6362503295084,
122.3910420022)) ;
#46938 = CARTESIAN_POINT('Ctrl Pts',(-20.2550642401252,-31.4562612491455,
122.135837120638)) ;
#46939 = CARTESIAN_POINT('Ctrl Pts',(-19.6946086357507,-31.6563134741243,
122.221176683087)) ;
#46940 = CARTESIAN_POINT('Ctrl Pts',(-19.7659328719897,-31.4763243937614,
121.923514400748)) ;
#46941 = CARTESIAN_POINT('Ctrl Pts',(-19.2743459249407,-31.676114364208,122.195122229128)) ;
#46942 = CARTESIAN_POINT('Ctrl Pts',(-19.2406043647874,-31.4961252838451,
121.89094955361)) ;
#46943 = CARTESIAN_POINT('Ctrl Pts',(-18.8673343999719,-31.6960574894867,
122.313844662609)) ;
#46944 = CARTESIAN_POINT('Ctrl Pts',(-18.731841866447,-31.5160684091238,122.039356586224)) ;
#46945 = CARTESIAN_POINT('Ctrl Pts',(-18.5261587627728,-31.7159555346063,
122.564031122159)) ;
#46946 = CARTESIAN_POINT('Ctrl Pts',(-18.3053752399663,-31.5359664542434,
122.352092202936)) ;
#46947 = CARTESIAN_POINT('Ctrl Pts',(-18.2900690142787,-31.735841294233,122.914876518788)) ;
#46948 = CARTESIAN_POINT('Ctrl Pts',(-18.0102664114479,-31.5558522138702,
122.790649876929)) ;
#46949 = CARTESIAN_POINT('Ctrl Pts',(-18.1876243917938,-31.7559064694129,
123.328998046209)) ;
#46950 = CARTESIAN_POINT('Ctrl Pts',(-17.8822137797069,-31.57591738905,123.30830329177)) ;
#46951 = CARTESIAN_POINT('Ctrl Pts',(-18.2322702694616,-31.7757331125157,
123.748268184179)) ;
#46952 = CARTESIAN_POINT('Ctrl Pts',(-17.9380242803409,-31.5957440321528,
123.832388879101)) ;
#46953 = CARTESIAN_POINT('Ctrl Pts',(-18.4169480013837,-31.7956418219641,
124.129048330367)) ;
#46954 = CARTESIAN_POINT('Ctrl Pts',(-18.1688732800194,-31.6156527416012,
124.308361931682)) ;
#46955 = CARTESIAN_POINT('Ctrl Pts',(-18.7212311690732,-31.8155936589959,
124.424824302643)) ;
#46956 = CARTESIAN_POINT('Ctrl Pts',(-18.5492284834963,-31.635604578633,124.678079899656)) ;
#46957 = CARTESIAN_POINT('Ctrl Pts',(-19.109410695338,-31.835602133699,124.59881362796)) ;
#46958 = CARTESIAN_POINT('Ctrl Pts',(-19.0344540490019,-31.6556130533361,
124.895564294001)) ;
#46959 = CARTESIAN_POINT('Ctrl Pts',(-19.5292929940374,-31.8554035924605,
124.630074904832)) ;
#46960 = CARTESIAN_POINT('Ctrl Pts',(-19.5593044714881,-31.6754145120976,
124.934638681105)) ;
#46961 = CARTESIAN_POINT('Ctrl Pts',(-19.9381051953959,-31.8753604806964,
124.516346944635)) ;
#46962 = CARTESIAN_POINT('Ctrl Pts',(-20.0703188207212,-31.6953714003336,
124.792477849082)) ;
#46963 = CARTESIAN_POINT('Ctrl Pts',(-20.2834627517452,-31.8953443181105,
124.268832628097)) ;
#46964 = CARTESIAN_POINT('Ctrl Pts',(-20.502014723073,-31.7153552377477,124.483083841928)) ;
#46965 = CARTESIAN_POINT('Ctrl Pts',(-20.5222631166498,-31.9151527573315,
123.921823635472)) ;
#46966 = CARTESIAN_POINT('Ctrl Pts',(-20.8005129693209,-31.7351636769686,
124.049324638335)) ;
#46967 = CARTESIAN_POINT('Ctrl Pts',(-20.6296391609579,-31.9351384667117,
123.510794184968)) ;
#46968 = CARTESIAN_POINT('Ctrl Pts',(-20.9347328465596,-31.7551493863488,
123.535538119656)) ;
#46969 = CARTESIAN_POINT('Ctrl Pts',(-20.5906472244068,-31.955007989727,123.089943615466)) ;
#46970 = CARTESIAN_POINT('Ctrl Pts',(-20.8859933951321,-31.7750189093641,
123.009476827453)) ;
#46971 = CARTESIAN_POINT('Ctrl Pts',(-20.4089954990554,-31.9750287288442,
122.705129085206)) ;
#46972 = CARTESIAN_POINT('Ctrl Pts',(-20.6589290212962,-31.7950396484813,
122.528458277174)) ;
#46973 = CARTESIAN_POINT('Ctrl Pts',(-20.1103555337929,-31.9948327938211,
122.408035535206)) ;
#46974 = CARTESIAN_POINT('Ctrl Pts',(-20.2856318116993,-31.8148437134583,
122.157092625036)) ;
#46975 = CARTESIAN_POINT('Ctrl Pts',(-19.7236013982933,-32.0148947575519,
122.228362978264)) ;
#46976 = CARTESIAN_POINT('Ctrl Pts',(-19.8021889396994,-31.834905677189,121.932500294498)) ;
#46977 = CARTESIAN_POINT('Ctrl Pts',(-19.3033421555285,-32.0347279378404,
122.192269701717)) ;
#46978 = CARTESIAN_POINT('Ctrl Pts',(-19.2768672597706,-31.8547388574775,
121.88738259078)) ;
#46979 = CARTESIAN_POINT('Ctrl Pts',(-18.8940840487304,-32.0546471351664,
122.301037263848)) ;
#46980 = CARTESIAN_POINT('Ctrl Pts',(-18.7652950498868,-31.8746580548036,
122.02333953517)) ;
#46981 = CARTESIAN_POINT('Ctrl Pts',(-18.5462767706842,-32.0745851602798,
122.543427443625)) ;
#46982 = CARTESIAN_POINT('Ctrl Pts',(-18.3305352276764,-31.8945960799169,
122.32632493169)) ;
#46983 = CARTESIAN_POINT('Ctrl Pts',(-18.3022836708014,-32.0944632063358,
122.888601365163)) ;
#46984 = CARTESIAN_POINT('Ctrl Pts',(-18.0255423060835,-31.914474125973,122.757789608184)) ;
#46985 = CARTESIAN_POINT('Ctrl Pts',(-18.1901182041216,-32.1144479406239,
123.298403225457)) ;
#46986 = CARTESIAN_POINT('Ctrl Pts',(-17.8853325731395,-31.934458860261,123.270040998411)) ;
#46987 = CARTESIAN_POINT('Ctrl Pts',(-18.2243400099676,-32.1343587573024,
123.720498462101)) ;
#46988 = CARTESIAN_POINT('Ctrl Pts',(-17.928106557493,-31.9543696769395,123.797659471924)) ;
#46989 = CARTESIAN_POINT('Ctrl Pts',(-18.4014838664741,-32.1543577328211,
124.106965037813)) ;
#46990 = CARTESIAN_POINT('Ctrl Pts',(-18.1495333782431,-31.9743686524582,
124.280744001209)) ;
#46991 = CARTESIAN_POINT('Ctrl Pts',(-18.6967305235978,-32.1741626534663,
124.40735164037)) ;
#46992 = CARTESIAN_POINT('Ctrl Pts',(-18.5185878611027,-31.9941735731034,
124.656228575391)) ;
#46993 = CARTESIAN_POINT('Ctrl Pts',(-19.0797563575211,-32.1941466137575,
124.59108153163)) ;
#46994 = CARTESIAN_POINT('Ctrl Pts',(-18.9973682960231,-32.0141575333947,
124.885894562646)) ;
#46995 = CARTESIAN_POINT('Ctrl Pts',(-19.500620909332,-32.2140328174815,124.632705731497)) ;
#46996 = CARTESIAN_POINT('Ctrl Pts',(-19.5234477413584,-32.0340437371186,
124.937928873616)) ;
#46997 = CARTESIAN_POINT('Ctrl Pts',(-19.91172625123,-32.2339819958047,124.528376651481)) ;
#46998 = CARTESIAN_POINT('Ctrl Pts',(-20.0373301585634,-32.0539929154418,
124.807521706156)) ;
#46999 = CARTESIAN_POINT('Ctrl Pts',(-20.2616847114276,-32.2538837950442,
124.290492641391)) ;
#47000 = CARTESIAN_POINT('Ctrl Pts',(-20.4747803851015,-32.0738947146813,
124.510171457429)) ;
#47001 = CARTESIAN_POINT('Ctrl Pts',(-20.5099132977842,-32.2737624000966,
123.948363389314)) ;
#47002 = CARTESIAN_POINT('Ctrl Pts',(-20.7850691732621,-32.0937733197337,
124.082510674293)) ;
#47003 = CARTESIAN_POINT('Ctrl Pts',(-20.627203071623,-32.2937947598223,123.538857802633)) ;
#47004 = CARTESIAN_POINT('Ctrl Pts',(-20.9316880819048,-32.1138056794594,
123.570639458984)) ;
#47005 = CARTESIAN_POINT('Ctrl Pts',(-20.6022414190364,-32.3103764857783,
123.187181314506)) ;
#47006 = CARTESIAN_POINT('Ctrl Pts',(-20.9004840928426,-32.1303874054155,
123.13101387148)) ;
#47007 = CARTESIAN_POINT('Ctrl Pts',(-20.5124528604533,-32.3235706560763,
122.924720422985)) ;
#47008 = CARTESIAN_POINT('Ctrl Pts',(-20.7882628387208,-32.1435815757134,
122.802971043195)) ;
#47009 = CARTESIAN_POINT('Ctrl Pts',(-20.3776944343899,-32.3368828341695,
122.679500006612)) ;
#47010 = CARTESIAN_POINT('Ctrl Pts',(-20.6197762199004,-32.1568937538066,
122.496386987847)) ;
#47011 = CARTESIAN_POINT('Ctrl Pts',(-20.1339928139378,-32.3534490137628,
122.425047262597)) ;
#47012 = CARTESIAN_POINT('Ctrl Pts',(-20.3152084467147,-32.1734599333999,
122.178383590941)) ;
#47013 = CARTESIAN_POINT('Ctrl Pts',(-19.8172190621121,-32.370077208623,122.268225534679)) ;
#47014 = CARTESIAN_POINT('Ctrl Pts',(-19.9191951145893,-32.1900881282601,
121.982318684066)) ;
#47015 = CARTESIAN_POINT('Ctrl Pts',(-19.5432299461013,-32.3833657903327,
122.213296215293)) ;
#47016 = CARTESIAN_POINT('Ctrl Pts',(-19.5767420543761,-32.2033767099699,
121.913670003331)) ;
#47017 = CARTESIAN_POINT('Ctrl Pts',(-19.3337508719107,-32.3933340384363,
122.208232309393)) ;
#47018 = CARTESIAN_POINT('Ctrl Pts',(-19.3148866166845,-32.2133449580735,
121.907334290486)) ;
#47019 = CARTESIAN_POINT('Ctrl Pts',(-19.1276189549108,-32.4032487946925,
122.239193486121)) ;
#47020 = CARTESIAN_POINT('Ctrl Pts',(-19.0572238635977,-32.2232597143296,
121.946033185605)) ;
#47021 = CARTESIAN_POINT('Ctrl Pts',(-18.9279557063151,-32.4132619453437,
122.305913698926)) ;
#47022 = CARTESIAN_POINT('Ctrl Pts',(-18.8076409322538,-32.2332728649808,
122.029433371392)) ;
#47023 = CARTESIAN_POINT('Ctrl Pts',(-18.7430842089401,-32.4232746525457,
122.406578399065)) ;
#47024 = CARTESIAN_POINT('Ctrl Pts',(-18.5765593857256,-32.2432855721828,
122.155251712162)) ;
#47025 = CARTESIAN_POINT('Ctrl Pts',(-18.5254677572598,-32.436493941237,122.579410532713)) ;
#47026 = CARTESIAN_POINT('Ctrl Pts',(-18.3044914721772,-32.2565048608741,
122.371339808174)) ;
#47027 = CARTESIAN_POINT('Ctrl Pts',(-18.3148360496128,-32.453112622235,122.863088731423)) ;
#47028 = CARTESIAN_POINT('Ctrl Pts',(-18.0412520385267,-32.2731235418722,
122.725865756024)) ;
#47029 = CARTESIAN_POINT('Ctrl Pts',(-18.2135427727924,-32.4696775300085,
123.200444286709)) ;
#47030 = CARTESIAN_POINT('Ctrl Pts',(-17.9146049570504,-32.2896884496456,
123.147620680735)) ;
#47031 = CARTESIAN_POINT('Ctrl Pts',(-18.2053428109417,-32.4830760016193,
123.482028619465)) ;
#47032 = CARTESIAN_POINT('Ctrl Pts',(-17.904363104532,-32.3030869212564,123.499558748901)) ;
#47033 = CARTESIAN_POINT('Ctrl Pts',(-18.2351263930126,-32.4929172571063,
123.686778633759)) ;
#47034 = CARTESIAN_POINT('Ctrl Pts',(-17.9415874189062,-32.3129281767434,
123.755505137551)) ;
#47035 = CARTESIAN_POINT('Ctrl Pts',(-18.3005104295691,-32.5029035726945,
123.886247272274)) ;
#47036 = CARTESIAN_POINT('Ctrl Pts',(-18.0233154440135,-32.3229144923316,
124.004839610842)) ;
#47037 = CARTESIAN_POINT('Ctrl Pts',(-18.3989864711992,-32.5128401802809,
124.070517770327)) ;
#47038 = CARTESIAN_POINT('Ctrl Pts',(-18.1464078763225,-32.332851099918,124.2351797327)) ;
#47039 = CARTESIAN_POINT('Ctrl Pts',(-18.5294794836623,-32.5228900476492,
124.236655331214)) ;
#47040 = CARTESIAN_POINT('Ctrl Pts',(-18.3095220075479,-32.3429009672863,
124.44285330986)) ;
#47041 = CARTESIAN_POINT('Ctrl Pts',(-18.6836393496476,-32.532740542324,124.374955006091)) ;
#47042 = CARTESIAN_POINT('Ctrl Pts',(-18.5022200305885,-32.3527514619611,
124.615730119443)) ;
#47043 = CARTESIAN_POINT('Ctrl Pts',(-18.8613101056891,-32.5427123427185,
124.486175930194)) ;
#47044 = CARTESIAN_POINT('Ctrl Pts',(-18.7243070867326,-32.3627232623556,
124.754758703636)) ;
#47045 = CARTESIAN_POINT('Ctrl Pts',(-19.0561314475104,-32.5527083097443,
124.565050529732)) ;
#47046 = CARTESIAN_POINT('Ctrl Pts',(-18.9678327868554,-32.3727192293814,
124.853354582418)) ;
#47047 = CARTESIAN_POINT('Ctrl Pts',(-19.2625472172633,-32.5627457691255,
124.608788649609)) ;
#47048 = CARTESIAN_POINT('Ctrl Pts',(-19.225851948996,-32.3827566887626,124.90802999486)) ;
#47049 = CARTESIAN_POINT('Ctrl Pts',(-19.4693094256783,-32.5725864700262,
124.616272691469)) ;
#47050 = CARTESIAN_POINT('Ctrl Pts',(-19.4843048557896,-32.3925973896634,
124.917387851395)) ;
#47051 = CARTESIAN_POINT('Ctrl Pts',(-19.6785662287874,-32.5826344912936,
124.587453910695)) ;
#47052 = CARTESIAN_POINT('Ctrl Pts',(-19.7458762676805,-32.4026454109307,
124.881367125265)) ;
#47053 = CARTESIAN_POINT('Ctrl Pts',(-19.8775350367199,-32.5925818843763,
124.523064897387)) ;
#47054 = CARTESIAN_POINT('Ctrl Pts',(-19.9945882738061,-32.4125928040134,
124.800883482138)) ;
#47055 = CARTESIAN_POINT('Ctrl Pts',(-20.0619149648412,-32.6024920304227,
124.426032573854)) ;
#47056 = CARTESIAN_POINT('Ctrl Pts',(-20.2250646863654,-32.4225029500598,
124.679595400653)) ;
#47057 = CARTESIAN_POINT('Ctrl Pts',(-20.2289464125442,-32.6125509442723,
124.296375819046)) ;
#47058 = CARTESIAN_POINT('Ctrl Pts',(-20.4338556734805,-32.4325618639094,
124.517526668951)) ;
#47059 = CARTESIAN_POINT('Ctrl Pts',(-20.3680971425257,-32.6223917145616,
124.143243416164)) ;
#47060 = CARTESIAN_POINT('Ctrl Pts',(-20.6077963923764,-32.4424026341987,
124.326112710777)) ;
#47061 = CARTESIAN_POINT('Ctrl Pts',(-20.4812183694655,-32.6324545841402,
123.964505832737)) ;
#47062 = CARTESIAN_POINT('Ctrl Pts',(-20.749200205045,-32.4524655037773,124.102692225348)) ;
#47063 = CARTESIAN_POINT('Ctrl Pts',(-20.5601018658738,-32.6423489072707,
123.772009901321)) ;
#47064 = CARTESIAN_POINT('Ctrl Pts',(-20.8478072363101,-32.4623598269078,
123.862073047581)) ;
#47065 = CARTESIAN_POINT('Ctrl Pts',(-20.6051186285884,-32.6522907143652,
123.567933795961)) ;
#47066 = CARTESIAN_POINT('Ctrl Pts',(-20.9040808602051,-32.4723016340023,
123.606978235594)) ;
#47067 = CARTESIAN_POINT('Ctrl Pts',(-20.6141529517269,-32.6622932253205,
123.357815073032)) ;
#47068 = CARTESIAN_POINT('Ctrl Pts',(-20.9153764258059,-32.4823041449576,
123.34432986247)) ;
#47069 = CARTESIAN_POINT('Ctrl Pts',(-20.5861553370163,-32.6723279461389,
123.148732523265)) ;
#47070 = CARTESIAN_POINT('Ctrl Pts',(-20.8803820948059,-32.492338865776,123.082976331004)) ;
#47071 = CARTESIAN_POINT('Ctrl Pts',(-20.5238045844199,-32.6821731236446,
122.95135818224)) ;
#47072 = CARTESIAN_POINT('Ctrl Pts',(-20.8024460213099,-32.5021840432817,
122.836257068615)) ;
#47073 = CARTESIAN_POINT('Ctrl Pts',(-20.4271596502256,-32.6921578840457,
122.76505202383)) ;
#47074 = CARTESIAN_POINT('Ctrl Pts',(-20.6816420858177,-32.5121688036828,
122.603373026614)) ;
#47075 = CARTESIAN_POINT('Ctrl Pts',(-20.3002621335287,-32.7020967903621,
122.599012732577)) ;
#47076 = CARTESIAN_POINT('Ctrl Pts',(-20.523022050828,-32.5221077099992,122.395822102444)) ;
#47077 = CARTESIAN_POINT('Ctrl Pts',(-20.1448530384785,-32.7121390179978,
122.456148065448)) ;
#47078 = CARTESIAN_POINT('Ctrl Pts',(-20.3287624729339,-32.5321499376349,
122.217239391601)) ;
#47079 = CARTESIAN_POINT('Ctrl Pts',(-19.9698227420243,-32.7220242295822,
122.344065587158)) ;
#47080 = CARTESIAN_POINT('Ctrl Pts',(-20.1099755420916,-32.5420351492193,
122.077133850417)) ;
#47081 = CARTESIAN_POINT('Ctrl Pts',(-19.7759374579204,-32.7320231597841,
122.262927443023)) ;
#47082 = CARTESIAN_POINT('Ctrl Pts',(-19.8676198087422,-32.5520340794212,
121.975708802829)) ;
#47083 = CARTESIAN_POINT('Ctrl Pts',(-19.5725517032629,-32.7419405826945,
122.216894103156)) ;
#47084 = CARTESIAN_POINT('Ctrl Pts',(-19.6133877400118,-32.5619515023317,
121.918164610241)) ;
#47085 = CARTESIAN_POINT('Ctrl Pts',(-19.3615855045364,-32.7519885147733,
122.206786949472)) ;
#47086 = CARTESIAN_POINT('Ctrl Pts',(-19.3496802081964,-32.5719994344104,
121.905528177764)) ;
#47087 = CARTESIAN_POINT('Ctrl Pts',(-19.1555344402761,-32.7618658905827,
122.232817208028)) ;
#47088 = CARTESIAN_POINT('Ctrl Pts',(-19.0921154350541,-32.5818768102198,
121.938063647421)) ;
#47089 = CARTESIAN_POINT('Ctrl Pts',(-18.9536242961126,-32.7719197837506,
122.29520263043)) ;
#47090 = CARTESIAN_POINT('Ctrl Pts',(-18.8397271603765,-32.5919307033877,
122.016043063102)) ;
#47091 = CARTESIAN_POINT('Ctrl Pts',(-18.7684970290784,-32.7818134070039,
122.390109939971)) ;
#47092 = CARTESIAN_POINT('Ctrl Pts',(-18.6083164557563,-32.601824326641,122.134675324029)) ;
#47093 = CARTESIAN_POINT('Ctrl Pts',(-18.5998696574853,-32.7918760006269,
122.517792698711)) ;
#47094 = CARTESIAN_POINT('Ctrl Pts',(-18.3975309341739,-32.611886920264,122.29427674415)) ;
#47095 = CARTESIAN_POINT('Ctrl Pts',(-18.4590017312758,-32.8017185746159,
122.669394023076)) ;
#47096 = CARTESIAN_POINT('Ctrl Pts',(-18.221443696393,-32.6217294942531,122.483777412127)) ;
#47097 = CARTESIAN_POINT('Ctrl Pts',(-18.3445119360111,-32.8117093314989,
122.845452008546)) ;
#47098 = CARTESIAN_POINT('Ctrl Pts',(-18.0783294582589,-32.631720251136,122.703848805901)) ;
#47099 = CARTESIAN_POINT('Ctrl Pts',(-18.2628657738663,-32.8216373932568,
123.037550195113)) ;
#47100 = CARTESIAN_POINT('Ctrl Pts',(-17.9762694762357,-32.6416483128939,
122.943971098664)) ;
#47101 = CARTESIAN_POINT('Ctrl Pts',(-18.2151746216112,-32.831625369146,123.242049850644)) ;
#47102 = CARTESIAN_POINT('Ctrl Pts',(-17.9166533727178,-32.6516362887831,
123.19959535074)) ;
#47103 = CARTESIAN_POINT('Ctrl Pts',(-18.2040142138472,-32.8416610335024,
123.452729593888)) ;
#47104 = CARTESIAN_POINT('Ctrl Pts',(-17.9027006002209,-32.6616719531395,
123.462944824449)) ;
#47105 = CARTESIAN_POINT('Ctrl Pts',(-18.2288249971323,-32.8515169719221,
123.658452238389)) ;
#47106 = CARTESIAN_POINT('Ctrl Pts',(-17.9337120201421,-32.6715278915592,
123.720099296854)) ;
#47107 = CARTESIAN_POINT('Ctrl Pts',(-18.2894914318515,-32.861512463319,123.859618101424)) ;
#47108 = CARTESIAN_POINT('Ctrl Pts',(-18.0095431011939,-32.6815233829561,
123.971557376319)) ;
#47109 = CARTESIAN_POINT('Ctrl Pts',(-18.3833118947942,-32.8714222682724,
124.045643520541)) ;
#47110 = CARTESIAN_POINT('Ctrl Pts',(-18.1268171255641,-32.6914331879096,
124.20409067232)) ;
#47111 = CARTESIAN_POINT('Ctrl Pts',(-18.509018904418,-32.8814344905392,124.214478322823)) ;
#47112 = CARTESIAN_POINT('Ctrl Pts',(-18.2839493311189,-32.7014454101763,
124.41513539528)) ;
#47113 = CARTESIAN_POINT('Ctrl Pts',(-18.6626514296269,-32.891462371232,124.358845529882)) ;
#47114 = CARTESIAN_POINT('Ctrl Pts',(-18.4759885042275,-32.7114732908691,
124.595595889866)) ;
#47115 = CARTESIAN_POINT('Ctrl Pts',(-18.8358044204708,-32.9013187672146,
124.472662632877)) ;
#47116 = CARTESIAN_POINT('Ctrl Pts',(-18.6924294796709,-32.7213296868517,
124.737869480862)) ;
#47117 = CARTESIAN_POINT('Ctrl Pts',(-19.0291703242302,-32.9113435643946,
124.556493615886)) ;
#47118 = CARTESIAN_POINT('Ctrl Pts',(-18.9341360919731,-32.7313544840317,
124.842659911602)) ;
#47119 = CARTESIAN_POINT('Ctrl Pts',(-19.2344039020975,-32.9213744943784,
124.605003116564)) ;
#47120 = CARTESIAN_POINT('Ctrl Pts',(-19.1906775296738,-32.7413854140155,
124.903298738838)) ;
#47121 = CARTESIAN_POINT('Ctrl Pts',(-19.4409936637498,-32.931219096887,124.617286306071)) ;
#47122 = CARTESIAN_POINT('Ctrl Pts',(-19.4489157332629,-32.7512300165242,
124.918654695543)) ;
#47123 = CARTESIAN_POINT('Ctrl Pts',(-19.6497118954831,-32.9412099481111,
124.593725011282)) ;
#47124 = CARTESIAN_POINT('Ctrl Pts',(-19.7098139114528,-32.7612208677483,
124.889204775659)) ;
#47125 = CARTESIAN_POINT('Ctrl Pts',(-19.8519756476524,-32.9512477811224,
124.533550068226)) ;
#47126 = CARTESIAN_POINT('Ctrl Pts',(-19.962644010255,-32.7712587007595,124.813987935703)) ;
#47127 = CARTESIAN_POINT('Ctrl Pts',(-20.0372510161014,-32.9610921695878,
124.441308298038)) ;
#47128 = CARTESIAN_POINT('Ctrl Pts',(-20.1942400544308,-32.7811030892249,
124.698686780465)) ;
#47129 = CARTESIAN_POINT('Ctrl Pts',(-20.206287933549,-32.9710769739574,124.316898276306)) ;
#47130 = CARTESIAN_POINT('Ctrl Pts',(-20.4055373690367,-32.7910878935945,
124.543175419173)) ;
#47131 = CARTESIAN_POINT('Ctrl Pts',(-20.3506030576117,-32.9810164934402,
124.165738129342)) ;
#47132 = CARTESIAN_POINT('Ctrl Pts',(-20.5859328054878,-32.8010274130773,
124.354225945988)) ;
#47133 = CARTESIAN_POINT('Ctrl Pts',(-20.4675814605525,-32.9910562244416,
123.990072866531)) ;
#47134 = CARTESIAN_POINT('Ctrl Pts',(-20.7321570744506,-32.8110671440787,
124.134645385839)) ;
#47135 = CARTESIAN_POINT('Ctrl Pts',(-20.5511100440207,-33.0009443526879,
123.799699797302)) ;
#47136 = CARTESIAN_POINT('Ctrl Pts',(-20.8365696228075,-32.820955272325,123.896678841576)) ;
#47137 = CARTESIAN_POINT('Ctrl Pts',(-20.6011952592599,-33.0109340778964,
123.595752254043)) ;
#47138 = CARTESIAN_POINT('Ctrl Pts',(-20.8991776003898,-32.8309449975335,
123.641744550588)) ;
#47139 = CARTESIAN_POINT('Ctrl Pts',(-20.6149126949009,-33.0208918425979,
123.386861704438)) ;
#47140 = CARTESIAN_POINT('Ctrl Pts',(-20.9163259243604,-32.840902762235,123.380631029218)) ;
#47141 = CARTESIAN_POINT('Ctrl Pts',(-20.5927628252155,-33.0307941840099,
123.179858179155)) ;
#47142 = CARTESIAN_POINT('Ctrl Pts',(-20.8886398161754,-32.850805103647,123.121875613575)) ;
#47143 = CARTESIAN_POINT('Ctrl Pts',(-20.5341646522333,-33.0408383797163,
122.977001703688)) ;
#47144 = CARTESIAN_POINT('Ctrl Pts',(-20.8153934381563,-32.8608492993534,
122.868304834852)) ;
#47145 = CARTESIAN_POINT('Ctrl Pts',(-20.4425109806158,-33.0507457804755,
122.789954482795)) ;
#47146 = CARTESIAN_POINT('Ctrl Pts',(-20.7008271858602,-32.8707567001127,
122.634494488512)) ;
#47147 = CARTESIAN_POINT('Ctrl Pts',(-20.3187974646894,-33.0607563803499,
122.619697924543)) ;
#47148 = CARTESIAN_POINT('Ctrl Pts',(-20.5461862319884,-32.880767299987,122.421673048565)) ;
#47149 = CARTESIAN_POINT('Ctrl Pts',(-20.1668178861132,-33.0707866762621,
122.473511957559)) ;
#47150 = CARTESIAN_POINT('Ctrl Pts',(-20.356212767659,-32.8907975958992,122.238939688487)) ;
#47151 = CARTESIAN_POINT('Ctrl Pts',(-19.9950035419231,-33.0806414559118,
122.357764747843)) ;
#47152 = CARTESIAN_POINT('Ctrl Pts',(-20.1414444851523,-32.9006523755489,
122.094253937587)) ;
#47153 = CARTESIAN_POINT('Ctrl Pts',(-19.8039737443084,-33.0905987841293,
122.272141541311)) ;
#47154 = CARTESIAN_POINT('Ctrl Pts',(-19.9026572208542,-32.9106097037664,
121.987223818498)) ;
#47155 = CARTESIAN_POINT('Ctrl Pts',(-19.5992424579009,-33.1006378170362,
122.220935616222)) ;
#47156 = CARTESIAN_POINT('Ctrl Pts',(-19.6467435512146,-32.9206487366733,
121.923215339529)) ;
#47157 = CARTESIAN_POINT('Ctrl Pts',(-19.3921897280463,-33.1105109289255,
122.205912912299)) ;
#47158 = CARTESIAN_POINT('Ctrl Pts',(-19.3879265897767,-32.9305218485626,
121.90443588022)) ;
#47159 = CARTESIAN_POINT('Ctrl Pts',(-19.1815696557166,-33.1205842139526,
122.227554268862)) ;
#47160 = CARTESIAN_POINT('Ctrl Pts',(-19.1246518188088,-32.9405951335897,
121.93148651026)) ;
#47161 = CARTESIAN_POINT('Ctrl Pts',(-18.9828627675349,-33.1304045336893,
122.283747306268)) ;
#47162 = CARTESIAN_POINT('Ctrl Pts',(-18.8762664627294,-32.9504154533265,
122.001727342518)) ;
#47163 = CARTESIAN_POINT('Ctrl Pts',(-18.7920430269983,-33.1404831990678,
122.37573379343)) ;
#47164 = CARTESIAN_POINT('Ctrl Pts',(-18.6377418415184,-32.9604941187049,
122.116709479966)) ;
#47165 = CARTESIAN_POINT('Ctrl Pts',(-18.6238449944928,-33.1503347895516,
122.496666905546)) ;
#47166 = CARTESIAN_POINT('Ctrl Pts',(-18.4274927507125,-32.9703457091887,
122.267875972372)) ;
#47167 = CARTESIAN_POINT('Ctrl Pts',(-18.4758763515475,-33.1604079398705,
122.648110975471)) ;
#47168 = CARTESIAN_POINT('Ctrl Pts',(-18.2425317134073,-32.9804188595076,
122.457180219424)) ;
#47169 = CARTESIAN_POINT('Ctrl Pts',(-18.3591783280429,-33.1702503198455,
122.8190052862)) ;
#47170 = CARTESIAN_POINT('Ctrl Pts',(-18.0966577530102,-32.9902612394826,
122.670798846665)) ;
#47171 = CARTESIAN_POINT('Ctrl Pts',(-18.2721117533038,-33.1802312960886,
123.009903540524)) ;
#47172 = CARTESIAN_POINT('Ctrl Pts',(-17.987823954365,-33.0002422157257,122.90942173405)) ;
#47173 = CARTESIAN_POINT('Ctrl Pts',(-18.2196648188066,-33.1902476244439,
123.213853808958)) ;
#47174 = CARTESIAN_POINT('Ctrl Pts',(-17.9222646672302,-33.010258544081,123.164359426917)) ;
#47175 = CARTESIAN_POINT('Ctrl Pts',(-18.2033572918697,-33.200145421435,123.421288579882)) ;
#47176 = CARTESIAN_POINT('Ctrl Pts',(-17.9018796513175,-33.0201563410721,
123.423653833823)) ;
#47177 = CARTESIAN_POINT('Ctrl Pts',(-18.223190034098,-33.2101579781671,123.630863236516)) ;
#47178 = CARTESIAN_POINT('Ctrl Pts',(-17.9266701886612,-33.0301688978042,
123.685622214838)) ;
#47179 = CARTESIAN_POINT('Ctrl Pts',(-18.2796939241535,-33.2201900130135,
123.834047999503)) ;
#47180 = CARTESIAN_POINT('Ctrl Pts',(-17.9972994489001,-33.0402009326507,
123.939603199681)) ;
#47181 = CARTESIAN_POINT('Ctrl Pts',(-18.3684191094839,-33.230029413829,124.020926505679)) ;
#47182 = CARTESIAN_POINT('Ctrl Pts',(-18.1082062116321,-33.0500403334661,
124.173202825564)) ;
#47183 = CARTESIAN_POINT('Ctrl Pts',(-18.4908474188606,-33.2400951994806,
124.193500366468)) ;
#47184 = CARTESIAN_POINT('Ctrl Pts',(-18.2612411137015,-33.0601061191177,
124.388920029464)) ;
#47185 = CARTESIAN_POINT('Ctrl Pts',(-18.6388594412923,-33.2499856545952,
124.339567692069)) ;
#47186 = CARTESIAN_POINT('Ctrl Pts',(-18.4462566311347,-33.0699965742323,
124.571505176903)) ;
#47187 = CARTESIAN_POINT('Ctrl Pts',(-18.8114608537052,-33.2599777732309,
124.459283778179)) ;
#47188 = CARTESIAN_POINT('Ctrl Pts',(-18.6620084681289,-33.0799886928681,
124.721150558715)) ;
#47189 = CARTESIAN_POINT('Ctrl Pts',(-19.0017546265229,-33.269940599994,124.546778303222)) ;
#47190 = CARTESIAN_POINT('Ctrl Pts',(-18.8998759883332,-33.0899515196311,
124.830519144683)) ;
#47191 = CARTESIAN_POINT('Ctrl Pts',(-19.2030467259017,-33.2798448832669,
124.600106280176)) ;
#47192 = CARTESIAN_POINT('Ctrl Pts',(-19.1514920073142,-33.099855802904,124.897179406725)) ;
#47193 = CARTESIAN_POINT('Ctrl Pts',(-19.4137849185456,-33.289905317214,124.617764888055)) ;
#47194 = CARTESIAN_POINT('Ctrl Pts',(-19.4149143853563,-33.1099162368511,
124.919252762117)) ;
#47195 = CARTESIAN_POINT('Ctrl Pts',(-19.6198604520968,-33.2997458698872,
124.599243558957)) ;
#47196 = CARTESIAN_POINT('Ctrl Pts',(-19.6725102686655,-33.1197567895243,
124.896100987741)) ;
#47197 = CARTESIAN_POINT('Ctrl Pts',(-19.8241111476887,-33.3098080898329,
124.544278855776)) ;
#47198 = CARTESIAN_POINT('Ctrl Pts',(-19.9278232585217,-33.12981900947,124.827395120368)) ;
#47199 = CARTESIAN_POINT('Ctrl Pts',(-20.0125096552998,-33.3197052291114,
124.455943774085)) ;
#47200 = CARTESIAN_POINT('Ctrl Pts',(-20.1633223010035,-33.1397161487486,
124.716975844118)) ;
#47201 = CARTESIAN_POINT('Ctrl Pts',(-20.1836814999991,-33.3296364212465,
124.336404331942)) ;
#47202 = CARTESIAN_POINT('Ctrl Pts',(-20.377287539303,-33.1496473408836,124.567550900585)) ;
#47203 = CARTESIAN_POINT('Ctrl Pts',(-20.3329814659399,-33.3396785758916,
124.187146312258)) ;
#47204 = CARTESIAN_POINT('Ctrl Pts',(-20.5639122193513,-33.1596894955287,
124.380978396875)) ;
#47205 = CARTESIAN_POINT('Ctrl Pts',(-20.4523759830474,-33.3495653369109,
124.016987842125)) ;
#47206 = CARTESIAN_POINT('Ctrl Pts',(-20.7131557897439,-33.169576256548,124.168279265478)) ;
#47207 = CARTESIAN_POINT('Ctrl Pts',(-20.5416382969896,-33.3595646386281,
123.826694295305)) ;
#47208 = CARTESIAN_POINT('Ctrl Pts',(-20.8247334245669,-33.1795755582652,
123.930412036511)) ;
#47209 = CARTESIAN_POINT('Ctrl Pts',(-20.596223942968,-33.3694854367949,123.625368027277)) ;
#47210 = CARTESIAN_POINT('Ctrl Pts',(-20.8929652906654,-33.189496356432,123.678753341723)) ;
#47211 = CARTESIAN_POINT('Ctrl Pts',(-20.615255722677,-33.3795194903916,123.415304326235)) ;
#47212 = CARTESIAN_POINT('Ctrl Pts',(-20.9167545830113,-33.1995304100287,
123.416173818305)) ;
#47213 = CARTESIAN_POINT('Ctrl Pts',(-20.5978416091603,-33.389442607958,123.207385396435)) ;
#47214 = CARTESIAN_POINT('Ctrl Pts',(-20.894986412613,-33.2094535275951,123.156274431571)) ;
#47215 = CARTESIAN_POINT('Ctrl Pts',(-20.5438456870571,-33.3994987314571,
123.003007585044)) ;
#47216 = CARTESIAN_POINT('Ctrl Pts',(-20.8274911534907,-33.2195096510942,
122.900802570426)) ;
#47217 = CARTESIAN_POINT('Ctrl Pts',(-20.4571105200585,-33.4093441731119,
122.81506612472)) ;
#47218 = CARTESIAN_POINT('Ctrl Pts',(-20.7190711618733,-33.2293550927491,
122.665874666496)) ;
#47219 = CARTESIAN_POINT('Ctrl Pts',(-20.3382374891591,-33.4193064742361,
122.642647202006)) ;
#47220 = CARTESIAN_POINT('Ctrl Pts',(-20.5704789953411,-33.2393173938732,
122.450351068691)) ;
#47221 = CARTESIAN_POINT('Ctrl Pts',(-20.1900385777374,-33.4293349535112,
122.492672258745)) ;
#47222 = CARTESIAN_POINT('Ctrl Pts',(-20.3852299651721,-33.2493458731483,
122.262882911342)) ;
#47223 = CARTESIAN_POINT('Ctrl Pts',(-20.0201373732377,-33.4392453070209,
122.372100343306)) ;
#47224 = CARTESIAN_POINT('Ctrl Pts',(-20.172852355375,-33.259256226658,122.112168058019)) ;
#47225 = CARTESIAN_POINT('Ctrl Pts',(-19.8316354394708,-33.4491801791981,
122.282138877027)) ;
#47226 = CARTESIAN_POINT('Ctrl Pts',(-19.9372239609423,-33.2691910988352,
121.999716737927)) ;
#47227 = CARTESIAN_POINT('Ctrl Pts',(-19.628183907834,-33.4592213167838,122.225869096708)) ;
#47228 = CARTESIAN_POINT('Ctrl Pts',(-19.6829095119979,-33.2792322364209,
121.92938034057)) ;
#47229 = CARTESIAN_POINT('Ctrl Pts',(-19.4212710659109,-33.4691084659983,
122.205941031249)) ;
#47230 = CARTESIAN_POINT('Ctrl Pts',(-19.4242673412634,-33.2891193856355,
121.904471017884)) ;
#47231 = CARTESIAN_POINT('Ctrl Pts',(-19.2118367929156,-33.4791007007494,
122.222063506245)) ;
#47232 = CARTESIAN_POINT('Ctrl Pts',(-19.1624743734912,-33.2991116203865,
121.924625120071)) ;
#47233 = CARTESIAN_POINT('Ctrl Pts',(-19.0092605385172,-33.4890494063124,
122.274143933396)) ;
#47234 = CARTESIAN_POINT('Ctrl Pts',(-18.9092537722081,-33.3090603259495,
121.989726729914)) ;
#47235 = CARTESIAN_POINT('Ctrl Pts',(-18.8189440039273,-33.4989854747361,
122.360209294255)) ;
#47236 = CARTESIAN_POINT('Ctrl Pts',(-18.6713579683458,-33.3189963943732,
122.097309682469)) ;
#47237 = CARTESIAN_POINT('Ctrl Pts',(-18.6454357357952,-33.5089711589519,
122.478422695815)) ;
#47238 = CARTESIAN_POINT('Ctrl Pts',(-18.454473086345,-33.328982078589,122.245077547478)) ;
#47239 = CARTESIAN_POINT('Ctrl Pts',(-18.4945213063124,-33.5190115855205,
122.625987981149)) ;
#47240 = CARTESIAN_POINT('Ctrl Pts',(-18.2658309062383,-33.3390225051576,
122.429534786724)) ;
#47241 = CARTESIAN_POINT('Ctrl Pts',(-18.3736983247787,-33.5288506989843,
122.793886133219)) ;
#47242 = CARTESIAN_POINT('Ctrl Pts',(-18.1148023371037,-33.3488616186214,
122.639409270607)) ;
#47243 = CARTESIAN_POINT('Ctrl Pts',(-18.28169524401,-33.5388804331601,122.983614959474)) ;
#47244 = CARTESIAN_POINT('Ctrl Pts',(-17.9997997485683,-33.3588913527972,
122.876570796198)) ;
#47245 = CARTESIAN_POINT('Ctrl Pts',(-18.2246058172832,-33.548902532666,123.186427396069)) ;
#47246 = CARTESIAN_POINT('Ctrl Pts',(-17.9284390777351,-33.3689134523031,
123.130086625313)) ;
#47247 = CARTESIAN_POINT('Ctrl Pts',(-18.2034007562052,-33.5587709725594,
123.392821859869)) ;
#47248 = CARTESIAN_POINT('Ctrl Pts',(-17.9019339658882,-33.3787818921965,
123.388080969439)) ;
#47249 = CARTESIAN_POINT('Ctrl Pts',(-18.218661353348,-33.568839837245,123.603931402573)) ;
#47250 = CARTESIAN_POINT('Ctrl Pts',(-17.9210110195692,-33.3888507568821,
123.651967424913)) ;
#47251 = CARTESIAN_POINT('Ctrl Pts',(-18.2691838785988,-33.5786825103436,
123.804599750498)) ;
#47252 = CARTESIAN_POINT('Ctrl Pts',(-17.9841657910811,-33.3986934299808,
123.902803793652)) ;
#47253 = CARTESIAN_POINT('Ctrl Pts',(-18.3540908209291,-33.5886431445061,
123.996012857149)) ;
#47254 = CARTESIAN_POINT('Ctrl Pts',(-18.0903011027806,-33.4086540641432,
124.142069897794)) ;
#47255 = CARTESIAN_POINT('Ctrl Pts',(-18.472193287036,-33.5986810601842,124.170889366581)) ;
#47256 = CARTESIAN_POINT('Ctrl Pts',(-18.237930321801,-33.4186919798213,124.360664605472)) ;
#47257 = CARTESIAN_POINT('Ctrl Pts',(-18.6162214398664,-33.6085553350436,
124.320419679324)) ;
#47258 = CARTESIAN_POINT('Ctrl Pts',(-18.4179673638906,-33.4285662546808,
124.547577121921)) ;
#47259 = CARTESIAN_POINT('Ctrl Pts',(-18.787310591261,-33.6186250854188,124.445049310116)) ;
#47260 = CARTESIAN_POINT('Ctrl Pts',(-18.6318294560732,-33.4386360050559,
124.703362669157)) ;
#47261 = CARTESIAN_POINT('Ctrl Pts',(-18.9729667813463,-33.6284583807933,
124.536013927551)) ;
#47262 = CARTESIAN_POINT('Ctrl Pts',(-18.8639015606415,-33.4484693004304,
124.817067545813)) ;
#47263 = CARTESIAN_POINT('Ctrl Pts',(-19.1753880863516,-33.6384886782729,
124.595078783209)) ;
#47264 = CARTESIAN_POINT('Ctrl Pts',(-19.116928618104,-33.45849959791,124.890896842844)) ;
#47265 = CARTESIAN_POINT('Ctrl Pts',(-19.385109828368,-33.6485207647143,124.61748724909)) ;
#47266 = CARTESIAN_POINT('Ctrl Pts',(-19.3790808832761,-33.4685316843515,
124.918905806779)) ;
#47267 = CARTESIAN_POINT('Ctrl Pts',(-19.5912662914409,-33.6583486932033,
124.603887833734)) ;
#47268 = CARTESIAN_POINT('Ctrl Pts',(-19.6367776217658,-33.4783596128404,
124.901904690569)) ;
#47269 = CARTESIAN_POINT('Ctrl Pts',(-19.7955034306806,-33.668344734314,124.554404004129)) ;
#47270 = CARTESIAN_POINT('Ctrl Pts',(-19.8920737335198,-33.4883556539512,
124.840047977085)) ;
#47271 = CARTESIAN_POINT('Ctrl Pts',(-19.9884633521273,-33.6783705464153,
124.469582265232)) ;
#47272 = CARTESIAN_POINT('Ctrl Pts',(-20.133272867296,-33.4983814660524,124.734019156174)) ;
#47273 = CARTESIAN_POINT('Ctrl Pts',(-20.1614882739156,-33.6882577813101,
124.354388322665)) ;
#47274 = CARTESIAN_POINT('Ctrl Pts',(-20.3495536621585,-33.5082687009472,
124.590024685913)) ;
#47275 = CARTESIAN_POINT('Ctrl Pts',(-20.3134732484457,-33.6982346475211,
124.209865201567)) ;
#47276 = CARTESIAN_POINT('Ctrl Pts',(-20.5395336848334,-33.5182455671582,
124.409369154937)) ;
#47277 = CARTESIAN_POINT('Ctrl Pts',(-20.4383121739259,-33.7082275913929,
124.040861571576)) ;
#47278 = CARTESIAN_POINT('Ctrl Pts',(-20.6955808166486,-33.52823851103,124.198113299847)) ;
#47279 = CARTESIAN_POINT('Ctrl Pts',(-20.5320713712117,-33.7182655140643,
123.851823217952)) ;
#47280 = CARTESIAN_POINT('Ctrl Pts',(-20.8127780411408,-33.5382764337014,
123.961814580438)) ;
#47281 = CARTESIAN_POINT('Ctrl Pts',(-20.5907682106731,-33.728113978326,123.653255911294)) ;
#47282 = CARTESIAN_POINT('Ctrl Pts',(-20.8861474399005,-33.5481248979631,
123.713603887042)) ;
#47283 = CARTESIAN_POINT('Ctrl Pts',(-20.6148023086895,-33.73810584507,123.444605714219)) ;
#47284 = CARTESIAN_POINT('Ctrl Pts',(-20.9161879631416,-33.5581167647071,
123.452790730188)) ;
#47285 = CARTESIAN_POINT('Ctrl Pts',(-20.6024505201895,-33.7480235771112,
123.236442898067)) ;
#47286 = CARTESIAN_POINT('Ctrl Pts',(-20.9007460375611,-33.5680344967483,
123.192586764787)) ;
#47287 = CARTESIAN_POINT('Ctrl Pts',(-20.5536692961249,-33.7580517620064,
123.031357793843)) ;
#47288 = CARTESIAN_POINT('Ctrl Pts',(-20.8397673980302,-33.5780626816436,
122.936230922789)) ;
#47289 = CARTESIAN_POINT('Ctrl Pts',(-20.4712833025613,-33.7679369200553,
122.840563071159)) ;
#47290 = CARTESIAN_POINT('Ctrl Pts',(-20.7367825952507,-33.5879478396924,
122.697737712798)) ;
#47291 = CARTESIAN_POINT('Ctrl Pts',(-20.3562437198245,-33.777926280597,122.664861804041)) ;
#47292 = CARTESIAN_POINT('Ctrl Pts',(-20.5929810834346,-33.5979372002341,
122.478112272451)) ;
#47293 = CARTESIAN_POINT('Ctrl Pts',(-20.2113763674384,-33.7879674375313,
122.511319512586)) ;
#47294 = CARTESIAN_POINT('Ctrl Pts',(-20.4118953447041,-33.6079783571685,
122.28618599598)) ;
#47295 = CARTESIAN_POINT('Ctrl Pts',(-20.0457742353741,-33.7978000209865,
122.38760905629)) ;
#47296 = CARTESIAN_POINT('Ctrl Pts',(-20.2048905331621,-33.6178109406236,
122.131549195167)) ;
#47297 = CARTESIAN_POINT('Ctrl Pts',(-19.8584418259696,-33.8077942409485,
122.29246902554)) ;
#47298 = CARTESIAN_POINT('Ctrl Pts',(-19.9707238077735,-33.6278051605856,
122.012626278824)) ;
#47299 = CARTESIAN_POINT('Ctrl Pts',(-19.6566211003262,-33.8178223427358,
122.23150371137)) ;
#47300 = CARTESIAN_POINT('Ctrl Pts',(-19.718447243707,-33.6378332623729,121.936421881646)) ;
#47301 = CARTESIAN_POINT('Ctrl Pts',(-19.4504107987317,-33.8277022873588,
122.206582828826)) ;
#47302 = CARTESIAN_POINT('Ctrl Pts',(-19.4606834132683,-33.647713206996,121.905273090565)) ;
#47303 = CARTESIAN_POINT('Ctrl Pts',(-19.2406868639278,-33.8376926139159,
122.21764677824)) ;
#47304 = CARTESIAN_POINT('Ctrl Pts',(-19.1985284829144,-33.657703533553,121.919105510909)) ;
#47305 = CARTESIAN_POINT('Ctrl Pts',(-19.0370644043963,-33.8476335455702,
122.264726339862)) ;
#47306 = CARTESIAN_POINT('Ctrl Pts',(-18.9440006247662,-33.6676444652073,
121.977957452937)) ;
#47307 = CARTESIAN_POINT('Ctrl Pts',(-18.8436891463967,-33.8576206640731,
122.346553932478)) ;
#47308 = CARTESIAN_POINT('Ctrl Pts',(-18.7022824096691,-33.6776315837102,
122.080244334494)) ;
#47309 = CARTESIAN_POINT('Ctrl Pts',(-18.6668496652182,-33.8676539969703,
122.461506020677)) ;
#47310 = CARTESIAN_POINT('Ctrl Pts',(-18.481234424871,-33.6876649166074,122.223936502288)) ;
#47311 = CARTESIAN_POINT('Ctrl Pts',(-18.5149208707951,-33.877520101415,122.602747192623)) ;
#47312 = CARTESIAN_POINT('Ctrl Pts',(-18.2913247035046,-33.6975310210521,
122.400490262853)) ;
#47313 = CARTESIAN_POINT('Ctrl Pts',(-18.3872775083727,-33.8875862152953,
122.77150901783)) ;
#47314 = CARTESIAN_POINT('Ctrl Pts',(-18.1317726324715,-33.7075971349325,
122.611443969021)) ;
#47315 = CARTESIAN_POINT('Ctrl Pts',(-18.2928599718456,-33.8974422270637,
122.955967537504)) ;
#47316 = CARTESIAN_POINT('Ctrl Pts',(-18.0137527035476,-33.7174531467009,
122.84201884311)) ;
#47317 = CARTESIAN_POINT('Ctrl Pts',(-18.2304603251342,-33.9074369306951,
123.156602452202)) ;
#47318 = CARTESIAN_POINT('Ctrl Pts',(-17.9357556600526,-33.7274478503322,
123.0928133731)) ;
#47319 = CARTESIAN_POINT('Ctrl Pts',(-18.2041945369859,-33.9174682664199,
123.365854471469)) ;
#47320 = CARTESIAN_POINT('Ctrl Pts',(-17.9029259941155,-33.7374791860571,
123.354378720209)) ;
#47321 = CARTESIAN_POINT('Ctrl Pts',(-18.2141592542206,-33.9273347916236,
123.573047505969)) ;
#47322 = CARTESIAN_POINT('Ctrl Pts',(-17.9153845549704,-33.7473457112607,
123.613370405302)) ;
#47323 = CARTESIAN_POINT('Ctrl Pts',(-18.2601719129641,-33.9373222196694,
123.777885455416)) ;
#47324 = CARTESIAN_POINT('Ctrl Pts',(-17.9729030336068,-33.7573331393065,
123.869417371802)) ;
#47325 = CARTESIAN_POINT('Ctrl Pts',(-18.3406253597855,-33.9472671493558,
123.970893068674)) ;
#47326 = CARTESIAN_POINT('Ctrl Pts',(-18.0734724275908,-33.767278068993,124.110676065872)) ;
#47327 = CARTESIAN_POINT('Ctrl Pts',(-18.4545761365393,-33.9573120674643,
124.148662539094)) ;
#47328 = CARTESIAN_POINT('Ctrl Pts',(-18.2159131529908,-33.7773229871015,
124.332886434286)) ;
#47329 = CARTESIAN_POINT('Ctrl Pts',(-18.5949446142755,-33.9671740370782,
124.301270643735)) ;
#47330 = CARTESIAN_POINT('Ctrl Pts',(-18.3913760380472,-33.7871849567154,
124.523645046325)) ;
#47331 = CARTESIAN_POINT('Ctrl Pts',(-18.7615730312214,-33.9771661050995,
124.42915104515)) ;
#47332 = CARTESIAN_POINT('Ctrl Pts',(-18.5996633149286,-33.7971770247366,
124.683493416082)) ;
#47333 = CARTESIAN_POINT('Ctrl Pts',(-18.946781772386,-33.987097030474,124.525545967815)) ;
#47334 = CARTESIAN_POINT('Ctrl Pts',(-18.8311757134717,-33.8071079501112,
124.803984732102)) ;
#47335 = CARTESIAN_POINT('Ctrl Pts',(-19.1461772309718,-33.9970476586975,
124.588768735179)) ;
#47336 = CARTESIAN_POINT('Ctrl Pts',(-19.0804210325099,-33.8170585783346,
124.883010582507)) ;
#47337 = CARTESIAN_POINT('Ctrl Pts',(-19.3545768509614,-34.0070478977566,
124.616672563708)) ;
#47338 = CARTESIAN_POINT('Ctrl Pts',(-19.3409209971923,-33.8270588173937,
124.917887617961)) ;
#47339 = CARTESIAN_POINT('Ctrl Pts',(-19.5652047456883,-34.0170763531258,
124.607640135001)) ;
#47340 = CARTESIAN_POINT('Ctrl Pts',(-19.6042058083092,-33.8370872727629,
124.906594290871)) ;
#47341 = CARTESIAN_POINT('Ctrl Pts',(-19.7678153879952,-34.026942387709,124.563211304919)) ;
#47342 = CARTESIAN_POINT('Ctrl Pts',(-19.8574687091397,-33.8469533073462,
124.851055548244)) ;
#47343 = CARTESIAN_POINT('Ctrl Pts',(-19.9621929863248,-34.0369347094565,
124.483598324612)) ;
#47344 = CARTESIAN_POINT('Ctrl Pts',(-20.1004399415462,-33.8569456290936,
124.751536396934)) ;
#47345 = CARTESIAN_POINT('Ctrl Pts',(-20.1387770996676,-34.0468669991335,
124.372126827251)) ;
#47346 = CARTESIAN_POINT('Ctrl Pts',(-20.3211678423663,-33.8668779187706,
124.612195664073)) ;
#47347 = CARTESIAN_POINT('Ctrl Pts',(-20.2945220917022,-34.0568686441042,
124.230877087231)) ;
#47348 = CARTESIAN_POINT('Ctrl Pts',(-20.5158504184365,-33.8768795637414,
124.435627299884)) ;
#47349 = CARTESIAN_POINT('Ctrl Pts',(-20.4659642035819,-34.0701812775203,
124.009619570015)) ;
#47350 = CARTESIAN_POINT('Ctrl Pts',(-20.730134344151,-33.8901921971574,124.159073181011)) ;
#47351 = CARTESIAN_POINT('Ctrl Pts',(-20.575254365758,-34.0834130269018,123.750361749611)) ;
#47352 = CARTESIAN_POINT('Ctrl Pts',(-20.8667466130496,-33.903423946539,123.835025634149)) ;
#47353 = CARTESIAN_POINT('Ctrl Pts',(-20.6136526413231,-34.0967362917189,
123.472950552117)) ;
#47354 = CARTESIAN_POINT('Ctrl Pts',(-20.9147529608524,-33.916747211356,123.488209575824)) ;
#47355 = CARTESIAN_POINT('Ctrl Pts',(-20.6062950710004,-34.1066119979366,
123.265445897535)) ;
#47356 = CARTESIAN_POINT('Ctrl Pts',(-20.9055507233818,-33.9266229175737,
123.228839180932)) ;
#47357 = CARTESIAN_POINT('Ctrl Pts',(-20.5627942065194,-34.1166015890366,
123.060012974967)) ;
#47358 = CARTESIAN_POINT('Ctrl Pts',(-20.8511725357474,-33.9366125086737,
122.972045792766)) ;
#47359 = CARTESIAN_POINT('Ctrl Pts',(-20.4848858375353,-34.126528685492,122.866373888595)) ;
#47360 = CARTESIAN_POINT('Ctrl Pts',(-20.7537843023225,-33.9465396051291,
122.72999873487)) ;
#47361 = CARTESIAN_POINT('Ctrl Pts',(-20.3734933893588,-34.1365538339966,
122.687478257524)) ;
#47362 = CARTESIAN_POINT('Ctrl Pts',(-20.6145413556846,-33.9565647536337,
122.506380398598)) ;
#47363 = CARTESIAN_POINT('Ctrl Pts',(-20.2346205228606,-34.1464494881433,
122.532553580072)) ;
#47364 = CARTESIAN_POINT('Ctrl Pts',(-20.4409482369391,-33.9664604077804,
122.312726536766)) ;
#47365 = CARTESIAN_POINT('Ctrl Pts',(-20.0693873756585,-34.1564530225215,
122.402484078199)) ;
#47366 = CARTESIAN_POINT('Ctrl Pts',(-20.234405044289,-33.9764639421586,122.150141791109)) ;
#47367 = CARTESIAN_POINT('Ctrl Pts',(-19.8843645713023,-34.1664381609615,
122.303256991677)) ;
#47368 = CARTESIAN_POINT('Ctrl Pts',(-20.0031251936759,-33.9864490805987,
122.026110363717)) ;
#47369 = CARTESIAN_POINT('Ctrl Pts',(-19.6838837822579,-34.1764740855569,
122.237544345005)) ;
#47370 = CARTESIAN_POINT('Ctrl Pts',(-19.7525232072214,-33.996485005194,121.943972168262)) ;
#47371 = CARTESIAN_POINT('Ctrl Pts',(-19.4789063239412,-34.1863253609846,
122.207945323593)) ;
#47372 = CARTESIAN_POINT('Ctrl Pts',(-19.4963012262117,-34.0063362806217,
121.906976170342)) ;
#47373 = CARTESIAN_POINT('Ctrl Pts',(-19.2689143031909,-34.1963176221459,
122.213879430628)) ;
#47374 = CARTESIAN_POINT('Ctrl Pts',(-19.2338112579742,-34.0163285417831,
121.914396519971)) ;
#47375 = CARTESIAN_POINT('Ctrl Pts',(-19.0622877357805,-34.2063575061635,
122.256906073786)) ;
#47376 = CARTESIAN_POINT('Ctrl Pts',(-18.9755284714672,-34.0263684258007,
121.968182550343)) ;
#47377 = CARTESIAN_POINT('Ctrl Pts',(-18.8700474354873,-34.216192280666,122.33308360955)) ;
#47378 = CARTESIAN_POINT('Ctrl Pts',(-18.7352293588995,-34.0362032003031,
122.063406918151)) ;
#47379 = CARTESIAN_POINT('Ctrl Pts',(-18.6896382083871,-34.2262686616863,
122.444048971715)) ;
#47380 = CARTESIAN_POINT('Ctrl Pts',(-18.5097194264488,-34.0462795813234,
122.202115742426)) ;
#47381 = CARTESIAN_POINT('Ctrl Pts',(-18.5347718576947,-34.2361149348369,
122.581438980249)) ;
#47382 = CARTESIAN_POINT('Ctrl Pts',(-18.3161370097982,-34.056125854474,122.37385617066)) ;
#47383 = CARTESIAN_POINT('Ctrl Pts',(-18.3597451156534,-34.2494794561221,
122.801234068625)) ;
#47384 = CARTESIAN_POINT('Ctrl Pts',(-18.0973641720853,-34.0694903757593,
122.648596301571)) ;
#47385 = CARTESIAN_POINT('Ctrl Pts',(-18.2477846712695,-34.2626857005566,
123.058779918869)) ;
#47386 = CARTESIAN_POINT('Ctrl Pts',(-17.9574233667404,-34.0826966201937,
122.97048578706)) ;
#47387 = CARTESIAN_POINT('Ctrl Pts',(-18.205709003732,-34.2759506552338,123.334400391849)) ;
#47388 = CARTESIAN_POINT('Ctrl Pts',(-17.9048166903989,-34.0959615748709,
123.315069758424)) ;
#47389 = CARTESIAN_POINT('Ctrl Pts',(-18.2106566690873,-34.2859829357855,
123.545267006591)) ;
#47390 = CARTESIAN_POINT('Ctrl Pts',(-17.9110068532374,-34.1059938554226,
123.57864144408)) ;
#47391 = CARTESIAN_POINT('Ctrl Pts',(-18.2516149367393,-34.2958916693034,
123.749507046798)) ;
#47392 = CARTESIAN_POINT('Ctrl Pts',(-17.9622064695877,-34.1159025889405,
123.833943902984)) ;
#47393 = CARTESIAN_POINT('Ctrl Pts',(-18.3271317964583,-34.3058292201709,
123.944308961896)) ;
#47394 = CARTESIAN_POINT('Ctrl Pts',(-18.0566040745096,-34.125840139808,124.077443630493)) ;
#47395 = CARTESIAN_POINT('Ctrl Pts',(-18.4364641233543,-34.3158590677648,
124.124581975054)) ;
#47396 = CARTESIAN_POINT('Ctrl Pts',(-18.1932746081133,-34.1358699874019,
124.302786499422)) ;
#47397 = CARTESIAN_POINT('Ctrl Pts',(-18.6196354097619,-34.3290942076852,
124.334139196948)) ;
#47398 = CARTESIAN_POINT('Ctrl Pts',(-18.4222258929034,-34.1491051273224,
124.564718290271)) ;
#47399 = CARTESIAN_POINT('Ctrl Pts',(-18.9138855860305,-34.3457626720564,
124.531468794228)) ;
#47400 = CARTESIAN_POINT('Ctrl Pts',(-18.7900532730984,-34.1657735916935,
124.811391878838)) ;
#47401 = CARTESIAN_POINT('Ctrl Pts',(-19.3240781905893,-34.3656336839303,
124.633306467972)) ;
#47402 = CARTESIAN_POINT('Ctrl Pts',(-19.3028100031656,-34.1856446035674,
124.938674734945)) ;
#47403 = CARTESIAN_POINT('Ctrl Pts',(-19.6773043637108,-34.3823407683133,
124.596000454904)) ;
#47404 = CARTESIAN_POINT('Ctrl Pts',(-19.7442781237528,-34.2023516879504,
124.8920557054)) ;
#47405 = CARTESIAN_POINT('Ctrl Pts',(-19.9358882444672,-34.3955180496239,
124.496604146033)) ;
#47406 = CARTESIAN_POINT('Ctrl Pts',(-20.0675644892654,-34.215528969261,124.767792583565)) ;
#47407 = CARTESIAN_POINT('Ctrl Pts',(-20.1754272741693,-34.408785510138,124.353698894968)) ;
#47408 = CARTESIAN_POINT('Ctrl Pts',(-20.3669683527793,-34.2287964297751,
124.589169379259)) ;
#47409 = CARTESIAN_POINT('Ctrl Pts',(-20.4216795722527,-34.4253994008252,
124.10043464984)) ;
#47410 = CARTESIAN_POINT('Ctrl Pts',(-20.6747925423891,-34.2454103204623,
124.272577564532)) ;
#47411 = CARTESIAN_POINT('Ctrl Pts',(-20.5958914665089,-34.4453482002526,
123.713647161789)) ;
#47412 = CARTESIAN_POINT('Ctrl Pts',(-20.8925501699724,-34.2653591198897,
123.789095141607)) ;
#47413 = CARTESIAN_POINT('Ctrl Pts',(-20.6275282466341,-34.4652693117834,
123.291312891227)) ;
#47414 = CARTESIAN_POINT('Ctrl Pts',(-20.9320934628038,-34.2852802314206,
123.26117694893)) ;
#47415 = CARTESIAN_POINT('Ctrl Pts',(-20.5142733747202,-34.4851357599563,
122.884295294386)) ;
#47416 = CARTESIAN_POINT('Ctrl Pts',(-20.7905220573564,-34.3051466795934,
122.752407298956)) ;
#47417 = CARTESIAN_POINT('Ctrl Pts',(-20.2668055992271,-34.5051621065734,
122.537830920578)) ;
#47418 = CARTESIAN_POINT('Ctrl Pts',(-20.4811847888518,-34.3251730262106,
122.319328242786)) ;
#47419 = CARTESIAN_POINT('Ctrl Pts',(-19.9186956223332,-34.525024150963,122.298589670166)) ;
#47420 = CARTESIAN_POINT('Ctrl Pts',(-20.0460469289995,-34.3450350706001,
122.020279911706)) ;
#47421 = CARTESIAN_POINT('Ctrl Pts',(-19.5084246289227,-34.5449694536441,
122.191442824304)) ;
#47422 = CARTESIAN_POINT('Ctrl Pts',(-19.5332082975654,-34.3649803732812,
121.886348768634)) ;
#47423 = CARTESIAN_POINT('Ctrl Pts',(-19.0872125174688,-34.564864760703,122.230706330331)) ;
#47424 = CARTESIAN_POINT('Ctrl Pts',(-19.0066946739163,-34.3848756803401,
121.93543015809)) ;
#47425 = CARTESIAN_POINT('Ctrl Pts',(-18.7043989473763,-34.5847580308706,
122.410642685401)) ;
#47426 = CARTESIAN_POINT('Ctrl Pts',(-18.528179666335,-34.4047689505077,122.160351280735)) ;
#47427 = CARTESIAN_POINT('Ctrl Pts',(-18.4049696018283,-34.604723623551,122.711540803692)) ;
#47428 = CARTESIAN_POINT('Ctrl Pts',(-18.1538942485171,-34.4247345431882,
122.53647446393)) ;
#47429 = CARTESIAN_POINT('Ctrl Pts',(-18.2267125295678,-34.6245989472359,
123.094736417654)) ;
#47430 = CARTESIAN_POINT('Ctrl Pts',(-17.9310744457826,-34.444609866873,123.015467619857)) ;
#47431 = CARTESIAN_POINT('Ctrl Pts',(-18.1893069394518,-34.6445740098108,
123.517829036567)) ;
#47432 = CARTESIAN_POINT('Ctrl Pts',(-17.8843177630335,-34.464584929448,123.544333074597)) ;
#47433 = CARTESIAN_POINT('Ctrl Pts',(-18.299019392422,-34.6645264194419,123.927638801905)) ;
#47434 = CARTESIAN_POINT('Ctrl Pts',(-18.0214586110986,-34.4845373390791,
124.056594429955)) ;
#47435 = CARTESIAN_POINT('Ctrl Pts',(-18.5399052285237,-34.684362473678,124.273849716243)) ;
#47436 = CARTESIAN_POINT('Ctrl Pts',(-18.3225640751946,-34.5043733933152,
124.489356119812)) ;
#47437 = CARTESIAN_POINT('Ctrl Pts',(-18.8866675177332,-34.7043403850956,
124.51920099619)) ;
#47438 = CARTESIAN_POINT('Ctrl Pts',(-18.7560161142767,-34.5243513047327,
124.796045846229)) ;
#47439 = CARTESIAN_POINT('Ctrl Pts',(-19.2952182234732,-34.7242584345991,
124.630665769838)) ;
#47440 = CARTESIAN_POINT('Ctrl Pts',(-19.2667030759239,-34.5442693542362,
124.935377333597)) ;
#47441 = CARTESIAN_POINT('Ctrl Pts',(-19.7164297540769,-34.7441265783672,
124.597207733981)) ;
#47442 = CARTESIAN_POINT('Ctrl Pts',(-19.7932159078448,-34.5641374980043,
124.893556756045)) ;
#47443 = CARTESIAN_POINT('Ctrl Pts',(-20.1040277686893,-34.7641774349545,
124.419895888455)) ;
#47444 = CARTESIAN_POINT('Ctrl Pts',(-20.2777146690572,-34.5841883545916,
124.671918199537)) ;
#47445 = CARTESIAN_POINT('Ctrl Pts',(-20.404229106633,-34.7839578714104,124.125155942307)) ;
#47446 = CARTESIAN_POINT('Ctrl Pts',(-20.6529658815064,-34.6039687910475,
124.303496686845)) ;
#47447 = CARTESIAN_POINT('Ctrl Pts',(-20.5886433658768,-34.8039879270882,
123.741366661607)) ;
#47448 = CARTESIAN_POINT('Ctrl Pts',(-20.8834863290637,-34.6239988467253,
123.823760909331)) ;
#47449 = CARTESIAN_POINT('Ctrl Pts',(-20.630003600706,-34.823869032263,123.320595871531)) ;
#47450 = CARTESIAN_POINT('Ctrl Pts',(-20.9351889705778,-34.6438799519001,
123.297798988631)) ;
#47451 = CARTESIAN_POINT('Ctrl Pts',(-20.5264818869687,-34.8437494946307,
122.91079906104)) ;
#47452 = CARTESIAN_POINT('Ctrl Pts',(-20.805790334357,-34.6637604142679,122.785553366895)) ;
#47453 = CARTESIAN_POINT('Ctrl Pts',(-20.2879555038815,-34.8637346417751,
122.55910414027)) ;
#47454 = CARTESIAN_POINT('Ctrl Pts',(-20.5076352220214,-34.6837455614122,
122.345932910046)) ;
#47455 = CARTESIAN_POINT('Ctrl Pts',(-19.9453039790159,-34.8836252203115,
122.311181550038)) ;
#47456 = CARTESIAN_POINT('Ctrl Pts',(-20.0793236955457,-34.7036361399486,
122.036027427117)) ;
#47457 = CARTESIAN_POINT('Ctrl Pts',(-19.5387683050646,-34.9035192401859,
122.194334979435)) ;
#47458 = CARTESIAN_POINT('Ctrl Pts',(-19.5711560383436,-34.723530159823,121.889965636303)) ;
#47459 = CARTESIAN_POINT('Ctrl Pts',(-19.1162346707492,-34.9234406849123,
122.223156044862)) ;
#47460 = CARTESIAN_POINT('Ctrl Pts',(-19.0429893283783,-34.7434516045494,
121.925987779891)) ;
#47461 = CARTESIAN_POINT('Ctrl Pts',(-18.7288788831415,-34.9433388229677,
122.393621819122)) ;
#47462 = CARTESIAN_POINT('Ctrl Pts',(-18.5587933443279,-34.7633497426048,
122.139065599401)) ;
#47463 = CARTESIAN_POINT('Ctrl Pts',(-18.4209986101695,-34.9634095781838,
122.68903279055)) ;
#47464 = CARTESIAN_POINT('Ctrl Pts',(-18.1739396124289,-34.7834204978209,
122.508326536902)) ;
#47465 = CARTESIAN_POINT('Ctrl Pts',(-18.2348330469421,-34.983195128235,123.066398593346)) ;
#47466 = CARTESIAN_POINT('Ctrl Pts',(-17.9412291317738,-34.8032060478722,
122.980030562384)) ;
#47467 = CARTESIAN_POINT('Ctrl Pts',(-18.1871490528402,-35.0031782031124,
123.488530219856)) ;
#47468 = CARTESIAN_POINT('Ctrl Pts',(-17.8816194222905,-34.8231891227495,
123.507694573191)) ;
#47469 = CARTESIAN_POINT('Ctrl Pts',(-18.2866725644005,-35.0230872857583,
123.899991070555)) ;
#47470 = CARTESIAN_POINT('Ctrl Pts',(-18.0060182323476,-34.8430982053954,
124.022021160858)) ;
#47471 = CARTESIAN_POINT('Ctrl Pts',(-18.5190486689243,-35.0429458448811,
124.252608438494)) ;
#47472 = CARTESIAN_POINT('Ctrl Pts',(-18.2964865246401,-34.8629567645182,
124.462795926968)) ;
#47473 = CARTESIAN_POINT('Ctrl Pts',(-18.8611531383577,-35.0629892887198,
124.506625814478)) ;
#47474 = CARTESIAN_POINT('Ctrl Pts',(-18.7241036774144,-34.8830002083569,
124.780319588221)) ;
#47475 = CARTESIAN_POINT('Ctrl Pts',(-19.1973105599933,-35.079489353449,124.60730897235)) ;
#47476 = CARTESIAN_POINT('Ctrl Pts',(-19.1443314362236,-34.8995002730861,
124.906184977463)) ;
#47477 = CARTESIAN_POINT('Ctrl Pts',(-19.4786570547526,-35.0928790932979,
124.615810466112)) ;
#47478 = CARTESIAN_POINT('Ctrl Pts',(-19.4959856145689,-34.912890012935,124.916808895163)) ;
#47479 = CARTESIAN_POINT('Ctrl Pts',(-19.6837596141147,-35.1027359945063,
124.58607447705)) ;
#47480 = CARTESIAN_POINT('Ctrl Pts',(-19.7523697501484,-34.9227469141434,
124.879642738554)) ;
#47481 = CARTESIAN_POINT('Ctrl Pts',(-19.8833526181919,-35.1127275203528,
124.520719105362)) ;
#47482 = CARTESIAN_POINT('Ctrl Pts',(-20.0018598351797,-34.9327384399899,
124.79795143579)) ;
#47483 = CARTESIAN_POINT('Ctrl Pts',(-20.0674176518561,-35.1226522008037,
124.422401605199)) ;
#47484 = CARTESIAN_POINT('Ctrl Pts',(-20.2319445660988,-34.9426631204409,
124.675054574799)) ;
#47485 = CARTESIAN_POINT('Ctrl Pts',(-20.2330436349176,-35.1326627908481,
124.292596619006)) ;
#47486 = CARTESIAN_POINT('Ctrl Pts',(-20.438971803788,-34.9526737104853,124.512809926613)) ;
#47487 = CARTESIAN_POINT('Ctrl Pts',(-20.4195165261857,-35.1459220515518,
124.085363429725)) ;
#47488 = CARTESIAN_POINT('Ctrl Pts',(-20.6720998991134,-34.9659329711889,
124.253723717875)) ;
#47489 = CARTESIAN_POINT('Ctrl Pts',(-20.5482036535186,-35.1592731267021,
123.832398852526)) ;
#47490 = CARTESIAN_POINT('Ctrl Pts',(-20.8329350805989,-34.9792840463392,
123.937545082256)) ;
#47491 = CARTESIAN_POINT('Ctrl Pts',(-20.6059607274363,-35.1724794359369,
123.560762637728)) ;
#47492 = CARTESIAN_POINT('Ctrl Pts',(-20.9051329385635,-34.992490355574,123.598017654249)) ;
#47493 = CARTESIAN_POINT('Ctrl Pts',(-20.6137261119894,-35.1824662695272,
123.350990307265)) ;
#47494 = CARTESIAN_POINT('Ctrl Pts',(-20.914842890768,-35.0024771891643,123.335798885094)) ;
#47495 = CARTESIAN_POINT('Ctrl Pts',(-20.5851416406984,-35.1924189970233,
123.143676946331)) ;
#47496 = CARTESIAN_POINT('Ctrl Pts',(-20.8791149640092,-35.0124299166604,
123.076657694403)) ;
#47497 = CARTESIAN_POINT('Ctrl Pts',(-20.5202297895318,-35.2024670938648,
122.942679277039)) ;
#47498 = CARTESIAN_POINT('Ctrl Pts',(-20.7979778136165,-35.022478013502,122.825409407708)) ;
#47499 = CARTESIAN_POINT('Ctrl Pts',(-20.4236321858874,-35.2123085507367,
122.75969231486)) ;
#47500 = CARTESIAN_POINT('Ctrl Pts',(-20.6772333062096,-35.0323194703738,
122.596674503416)) ;
#47501 = CARTESIAN_POINT('Ctrl Pts',(-20.2952501726806,-35.2222948176502,
122.593621170823)) ;
#47502 = CARTESIAN_POINT('Ctrl Pts',(-20.5167579761239,-35.0423057372873,
122.389083764502)) ;
#47503 = CARTESIAN_POINT('Ctrl Pts',(-20.1407744583381,-35.2322314185506,
122.45294261696)) ;
#47504 = CARTESIAN_POINT('Ctrl Pts',(-20.3236651757576,-35.0522423381877,
122.213233449278)) ;
#47505 = CARTESIAN_POINT('Ctrl Pts',(-19.9621957115618,-35.2422813613376,
122.340068651411)) ;
#47506 = CARTESIAN_POINT('Ctrl Pts',(-20.1004431975683,-35.0622922809748,
122.072138574706)) ;
#47507 = CARTESIAN_POINT('Ctrl Pts',(-19.77064229135,-35.2521315610234,122.261352205955)) ;
#47508 = CARTESIAN_POINT('Ctrl Pts',(-19.861002389051,-35.0721424806605,121.973740369883)) ;
#47509 = CARTESIAN_POINT('Ctrl Pts',(-19.5659662743928,-35.2621044659555,
122.216007869496)) ;
#47510 = CARTESIAN_POINT('Ctrl Pts',(-19.6051578614204,-35.0821153855926,
121.917057183094)) ;
#47511 = CARTESIAN_POINT('Ctrl Pts',(-19.3559388586588,-35.2721028404351,
122.20693299255)) ;
#47512 = CARTESIAN_POINT('Ctrl Pts',(-19.3426236375317,-35.0921137600722,
121.905710783946)) ;
#47513 = CARTESIAN_POINT('Ctrl Pts',(-19.1471235458461,-35.2821230143051,
122.234669898377)) ;
#47514 = CARTESIAN_POINT('Ctrl Pts',(-19.0816040718578,-35.1021339339422,
121.940379135869)) ;
#47515 = CARTESIAN_POINT('Ctrl Pts',(-18.9486182041443,-35.2920240582471,
122.297318677213)) ;
#47516 = CARTESIAN_POINT('Ctrl Pts',(-18.8334713868321,-35.1120349778842,
122.018687487834)) ;
#47517 = CARTESIAN_POINT('Ctrl Pts',(-18.7622230203345,-35.3020128619714,
122.394038689284)) ;
#47518 = CARTESIAN_POINT('Ctrl Pts',(-18.600476033389,-35.1220237816085,122.139585076272)) ;
#47519 = CARTESIAN_POINT('Ctrl Pts',(-18.5959401033665,-35.3119783288032,
122.521468994438)) ;
#47520 = CARTESIAN_POINT('Ctrl Pts',(-18.3926205883172,-35.1319892484403,
122.298870811014)) ;
#47521 = CARTESIAN_POINT('Ctrl Pts',(-18.4547977142894,-35.3218818910762,
122.674558023421)) ;
#47522 = CARTESIAN_POINT('Ctrl Pts',(-18.2161904041538,-35.1418928107133,
122.490230413735)) ;
#47523 = CARTESIAN_POINT('Ctrl Pts',(-18.3407694318747,-35.3319425689542,
122.852663128969)) ;
#47524 = CARTESIAN_POINT('Ctrl Pts',(-18.0736527312663,-35.1519534885913,
122.712860272288)) ;
#47525 = CARTESIAN_POINT('Ctrl Pts',(-18.2609128534862,-35.3417828669036,
123.043535459525)) ;
#47526 = CARTESIAN_POINT('Ctrl Pts',(-17.9738293172813,-35.1617937865408,
122.951450001417)) ;
#47527 = CARTESIAN_POINT('Ctrl Pts',(-18.2141440011338,-35.3518458618131,
123.24982878148)) ;
#47528 = CARTESIAN_POINT('Ctrl Pts',(-17.9153656043643,-35.1718567814502,
123.209316008984)) ;
#47529 = CARTESIAN_POINT('Ctrl Pts',(-18.2042462712093,-35.3617401559602,
123.457624789983)) ;
#47530 = CARTESIAN_POINT('Ctrl Pts',(-17.9029906881241,-35.1817510755973,
123.469061216247)) ;
#47531 = CARTESIAN_POINT('Ctrl Pts',(-18.2301365974252,-35.3716819536571,
123.66499700929)) ;
#47532 = CARTESIAN_POINT('Ctrl Pts',(-17.9353509724904,-35.1916928732942,
123.728277083016)) ;
#47533 = CARTESIAN_POINT('Ctrl Pts',(-18.2919583226803,-35.3816845311862,
123.866019002124)) ;
#47534 = CARTESIAN_POINT('Ctrl Pts',(-18.0126256104855,-35.2016954508233,
123.979555436209)) ;
#47535 = CARTESIAN_POINT('Ctrl Pts',(-18.38832214789,-35.3917189951073,124.053667683726)) ;
#47536 = CARTESIAN_POINT('Ctrl Pts',(-18.1330779756745,-35.2117299147444,
124.214117512253)) ;
#47537 = CARTESIAN_POINT('Ctrl Pts',(-18.5131632869251,-35.4015651336283,
124.218788839764)) ;
#47538 = CARTESIAN_POINT('Ctrl Pts',(-18.2891276130123,-35.2215760532655,
124.420521008391)) ;
#47539 = CARTESIAN_POINT('Ctrl Pts',(-18.6665221671683,-35.4115463068653,
124.361984621255)) ;
#47540 = CARTESIAN_POINT('Ctrl Pts',(-18.4808245709193,-35.2315572265025,
124.59951775017)) ;
#47541 = CARTESIAN_POINT('Ctrl Pts',(-18.8419525073359,-35.4214986008226,
124.476017082833)) ;
#47542 = CARTESIAN_POINT('Ctrl Pts',(-18.7001113066703,-35.2415095204597,
124.742060651056)) ;
#47543 = CARTESIAN_POINT('Ctrl Pts',(-19.0353199148675,-35.4314973959572,
124.558494549662)) ;
#47544 = CARTESIAN_POINT('Ctrl Pts',(-18.9418196622479,-35.2515083155943,
124.845159871712)) ;
#47545 = CARTESIAN_POINT('Ctrl Pts',(-19.2409602408548,-35.441536504218,124.605934758552)) ;
#47546 = CARTESIAN_POINT('Ctrl Pts',(-19.1988694220206,-35.2615474238551,
124.904462676824)) ;
#47547 = CARTESIAN_POINT('Ctrl Pts',(-19.4472187958602,-35.4513614456571,
124.617157941758)) ;
#47548 = CARTESIAN_POINT('Ctrl Pts',(-19.4566932433114,-35.2713723652943,
124.918494235156)) ;
#47549 = CARTESIAN_POINT('Ctrl Pts',(-19.6571046505334,-35.4614161327315,
124.59216665789)) ;
#47550 = CARTESIAN_POINT('Ctrl Pts',(-19.7190507496054,-35.2814270523687,
124.887257605285)) ;
#47551 = CARTESIAN_POINT('Ctrl Pts',(-19.8571259179256,-35.4713589376717,
124.531443581548)) ;
#47552 = CARTESIAN_POINT('Ctrl Pts',(-19.9690783925131,-35.2913698573088,
124.811356103697)) ;
#47553 = CARTESIAN_POINT('Ctrl Pts',(-20.0431203480413,-35.4812627236682,
124.437854636446)) ;
#47554 = CARTESIAN_POINT('Ctrl Pts',(-20.2015729912878,-35.3012736433053,
124.694371844272)) ;
#47555 = CARTESIAN_POINT('Ctrl Pts',(-20.2123551288087,-35.491309540233,124.31150595345)) ;
#47556 = CARTESIAN_POINT('Ctrl Pts',(-20.4131178490129,-35.3113204598701,
124.536438012286)) ;
#47557 = CARTESIAN_POINT('Ctrl Pts',(-20.355073515676,-35.5012050597117,124.160099178899)) ;
#47558 = CARTESIAN_POINT('Ctrl Pts',(-20.5915179796175,-35.3212159793488,
124.347180770753)) ;
#47559 = CARTESIAN_POINT('Ctrl Pts',(-20.471223424041,-35.5112671450361,123.983338753384)) ;
#47560 = CARTESIAN_POINT('Ctrl Pts',(-20.7367072779153,-35.3312780646732,
124.126231712253)) ;
#47561 = CARTESIAN_POINT('Ctrl Pts',(-20.5532221554608,-35.521109855994,123.793329340615)) ;
#47562 = CARTESIAN_POINT('Ctrl Pts',(-20.8392082177454,-35.3411207756312,
123.888720096976)) ;
#47563 = CARTESIAN_POINT('Ctrl Pts',(-20.6021745079103,-35.5311005733001,
123.589104323875)) ;
#47564 = CARTESIAN_POINT('Ctrl Pts',(-20.9004009016988,-35.3511114929372,
123.633439183849)) ;
#47565 = CARTESIAN_POINT('Ctrl Pts',(-20.6148094254628,-35.5410286563966,
123.380757851225)) ;
#47566 = CARTESIAN_POINT('Ctrl Pts',(-20.9161968438839,-35.3610395760338,
123.373005745111)) ;
#47567 = CARTESIAN_POINT('Ctrl Pts',(-20.5912974926631,-35.5510165865084,
123.172091972982)) ;
#47568 = CARTESIAN_POINT('Ctrl Pts',(-20.8868090725257,-35.3710275061455,
123.112172972253)) ;
#47569 = CARTESIAN_POINT('Ctrl Pts',(-20.5312904374153,-35.5610524126357,
122.969827521401)) ;
#47570 = CARTESIAN_POINT('Ctrl Pts',(-20.8118024544747,-35.3810633322728,
122.859341843818)) ;
#47571 = CARTESIAN_POINT('Ctrl Pts',(-20.4390581243751,-35.5709077497493,
122.78428606231)) ;
#47572 = CARTESIAN_POINT('Ctrl Pts',(-20.6965136129544,-35.3909186693864,
122.627413231324)) ;
#47573 = CARTESIAN_POINT('Ctrl Pts',(-20.3145205708958,-35.5809054845995,
122.614998952204)) ;
#47574 = CARTESIAN_POINT('Ctrl Pts',(-20.5408432692029,-35.4009164042366,
122.415802979033)) ;
#47575 = CARTESIAN_POINT('Ctrl Pts',(-20.1638726572033,-35.5908133885839,
122.471137864884)) ;
#47576 = CARTESIAN_POINT('Ctrl Pts',(-20.3525343320192,-35.4108243082211,
122.235974665639)) ;
#47577 = CARTESIAN_POINT('Ctrl Pts',(-19.9889273945464,-35.6008244631324,
122.354124867634)) ;
#47578 = CARTESIAN_POINT('Ctrl Pts',(-20.1338538119606,-35.4208353827695,
122.089706748638)) ;
#47579 = CARTESIAN_POINT('Ctrl Pts',(-19.7958300056756,-35.610852318668,122.269519731036)) ;
#47580 = CARTESIAN_POINT('Ctrl Pts',(-19.8924829761476,-35.4308632383051,
121.983948431218)) ;
#47581 = CARTESIAN_POINT('Ctrl Pts',(-19.5945466869052,-35.6207099125732,
122.220212795873)) ;
#47582 = CARTESIAN_POINT('Ctrl Pts',(-19.6408783355081,-35.4407208322104,
121.922312589415)) ;
#47583 = CARTESIAN_POINT('Ctrl Pts',(-19.3842341645356,-35.6307365994113,
122.205941341897)) ;
#47584 = CARTESIAN_POINT('Ctrl Pts',(-19.3779878358377,-35.4507475190485,
121.904471410872)) ;
#47585 = CARTESIAN_POINT('Ctrl Pts',(-19.1746497432009,-35.6407652685651,
122.228931469731)) ;
#47586 = CARTESIAN_POINT('Ctrl Pts',(-19.116007159778,-35.4607761882022,121.933207053321)) ;
#47587 = CARTESIAN_POINT('Ctrl Pts',(-18.9758531060999,-35.6506104768465,
122.286508207348)) ;
#47588 = CARTESIAN_POINT('Ctrl Pts',(-18.8675097602884,-35.4706213964836,
122.005176454278)) ;
#47589 = CARTESIAN_POINT('Ctrl Pts',(-18.78706524933,-35.6606011658096,122.378575193346)) ;
#47590 = CARTESIAN_POINT('Ctrl Pts',(-18.6315240046396,-35.4806120854467,
122.120258716243)) ;
#47591 = CARTESIAN_POINT('Ctrl Pts',(-18.6166109529874,-35.6706390420919,
122.502982907208)) ;
#47592 = CARTESIAN_POINT('Ctrl Pts',(-18.4184551336644,-35.490649961729,122.275766762544)) ;
#47593 = CARTESIAN_POINT('Ctrl Pts',(-18.4728999980008,-35.6804834197341,
122.651921164381)) ;
#47594 = CARTESIAN_POINT('Ctrl Pts',(-18.2388143581137,-35.5004943393712,
122.461939201288)) ;
#47595 = CARTESIAN_POINT('Ctrl Pts',(-18.3552581448824,-35.6904682241255,
122.825736375078)) ;
#47596 = CARTESIAN_POINT('Ctrl Pts',(-18.0917605510307,-35.5104791437627,
122.679207506938)) ;
#47597 = CARTESIAN_POINT('Ctrl Pts',(-18.2698663052676,-35.7004077543441,
123.016483700906)) ;
#47598 = CARTESIAN_POINT('Ctrl Pts',(-17.9850190706446,-35.5204186739812,
122.917641507292)) ;
#47599 = CARTESIAN_POINT('Ctrl Pts',(-18.218436347525,-35.710447442381,123.221171010836)) ;
#47600 = CARTESIAN_POINT('Ctrl Pts',(-17.9207300902949,-35.5304583620181,
123.173500108613)) ;
#47601 = CARTESIAN_POINT('Ctrl Pts',(-18.2034516389984,-35.7203357317493,
123.428524856059)) ;
#47602 = CARTESIAN_POINT('Ctrl Pts',(-17.9019975600655,-35.5403466513864,
123.43269321979)) ;
#47603 = CARTESIAN_POINT('Ctrl Pts',(-18.2245179381264,-35.7303248554341,
123.637461026191)) ;
#47604 = CARTESIAN_POINT('Ctrl Pts',(-17.928329013415,-35.5503357750712,123.693863790479)) ;
#47605 = CARTESIAN_POINT('Ctrl Pts',(-18.281534545644,-35.7402848651087,123.838935805631)) ;
#47606 = CARTESIAN_POINT('Ctrl Pts',(-17.9995984433313,-35.5602957847458,
123.945708092075)) ;
#47607 = CARTESIAN_POINT('Ctrl Pts',(-18.3716800461657,-35.7501852948129,
124.026546743199)) ;
#47608 = CARTESIAN_POINT('Ctrl Pts',(-18.1122794989603,-35.57019621445,124.180223126085)) ;
#47609 = CARTESIAN_POINT('Ctrl Pts',(-18.4947794817171,-35.7602283762197,
124.198074355247)) ;
#47610 = CARTESIAN_POINT('Ctrl Pts',(-18.2661525939819,-35.5802392958568,
124.394633262475)) ;
#47611 = CARTESIAN_POINT('Ctrl Pts',(-18.6437627494517,-35.7701357701273,
124.343645611898)) ;
#47612 = CARTESIAN_POINT('Ctrl Pts',(-18.4523813317248,-35.5901466897644,
124.576598857662)) ;
#47613 = CARTESIAN_POINT('Ctrl Pts',(-18.8173428519059,-35.7801475011165,
124.462690565596)) ;
#47614 = CARTESIAN_POINT('Ctrl Pts',(-18.6693558214365,-35.6001584207536,
124.725406064343)) ;
#47615 = CARTESIAN_POINT('Ctrl Pts',(-19.0095259153143,-35.7901797188313,
124.549587699707)) ;
#47616 = CARTESIAN_POINT('Ctrl Pts',(-18.9095840015776,-35.6101906384684,
124.834028669225)) ;
#47617 = CARTESIAN_POINT('Ctrl Pts',(-19.2101294613733,-35.8000322280774,
124.601126477445)) ;
#47618 = CARTESIAN_POINT('Ctrl Pts',(-19.1603393482666,-35.6200431477146,
124.898453661677)) ;
#47619 = CARTESIAN_POINT('Ctrl Pts',(-19.4188119264436,-35.8099901646204,
124.617871878663)) ;
#47620 = CARTESIAN_POINT('Ctrl Pts',(-19.4211928177086,-35.6300010842576,
124.919386454323)) ;
#47621 = CARTESIAN_POINT('Ctrl Pts',(-19.6288700822666,-35.8200290346287,
124.59759241421)) ;
#47622 = CARTESIAN_POINT('Ctrl Pts',(-19.6837654584528,-35.6400399542659,
124.894038281209)) ;
#47623 = CARTESIAN_POINT('Ctrl Pts',(-19.8290080686716,-35.829902189787,124.542441752005)) ;
#47624 = CARTESIAN_POINT('Ctrl Pts',(-19.9339392913664,-35.6499131094241,
124.825100619419)) ;
#47625 = CARTESIAN_POINT('Ctrl Pts',(-20.0202339068438,-35.8399754646367,
124.45154743179)) ;
#47626 = CARTESIAN_POINT('Ctrl Pts',(-20.1729716447795,-35.6599863842738,
124.711483830272)) ;
#47627 = CARTESIAN_POINT('Ctrl Pts',(-20.1886685597443,-35.8497957818141,
124.332082596939)) ;
#47628 = CARTESIAN_POINT('Ctrl Pts',(-20.3835167615202,-35.6698067014512,
124.562152640001)) ;
#47629 = CARTESIAN_POINT('Ctrl Pts',(-20.3376896490082,-35.8598744676076,
124.181528608811)) ;
#47630 = CARTESIAN_POINT('Ctrl Pts',(-20.5697933970036,-35.6798853872447,
124.373961088606)) ;
#47631 = CARTESIAN_POINT('Ctrl Pts',(-20.455705088691,-35.8697259789907,124.011272096574)) ;
#47632 = CARTESIAN_POINT('Ctrl Pts',(-20.7173141230226,-35.6897368986278,
124.161139832778)) ;
#47633 = CARTESIAN_POINT('Ctrl Pts',(-20.5444435166218,-35.8797994252973,
123.81902845343)) ;
#47634 = CARTESIAN_POINT('Ctrl Pts',(-20.8282376597634,-35.6998103449344,
123.920835993557)) ;
#47635 = CARTESIAN_POINT('Ctrl Pts',(-20.5972105460148,-35.889640700422,123.618952464279)) ;
#47636 = CARTESIAN_POINT('Ctrl Pts',(-20.8941975462152,-35.7096516200591,
123.670739828049)) ;
#47637 = CARTESIAN_POINT('Ctrl Pts',(-20.6153373392273,-35.8996258000788,
123.409838328814)) ;
#47638 = CARTESIAN_POINT('Ctrl Pts',(-20.9168565666188,-35.7196367197159,
123.409346913405)) ;
#47639 = CARTESIAN_POINT('Ctrl Pts',(-20.5965431076934,-35.9096332762131,
123.200274922463)) ;
#47640 = CARTESIAN_POINT('Ctrl Pts',(-20.8933643885283,-35.7296441958502,
123.147392528966)) ;
#47641 = CARTESIAN_POINT('Ctrl Pts',(-20.5423042520483,-35.919555863922,122.998856521941)) ;
#47642 = CARTESIAN_POINT('Ctrl Pts',(-20.8255661487373,-35.7395667835592,
122.89561863727)) ;
#47643 = CARTESIAN_POINT('Ctrl Pts',(-20.453642398187,-35.9295424681954,122.808524797024)) ;
#47644 = CARTESIAN_POINT('Ctrl Pts',(-20.7147391058567,-35.7495533878325,
122.657703592569)) ;
#47645 = CARTESIAN_POINT('Ctrl Pts',(-20.3323311287311,-35.9395825965295,
122.635813523666)) ;
#47646 = CARTESIAN_POINT('Ctrl Pts',(-20.5631005957844,-35.7595935161666,
122.44181432373)) ;
#47647 = CARTESIAN_POINT('Ctrl Pts',(-20.1861543358301,-35.9494220310629,
122.48942292078)) ;
#47648 = CARTESIAN_POINT('Ctrl Pts',(-20.380378834698,-35.7694329507,122.258824742576)) ;
#47649 = CARTESIAN_POINT('Ctrl Pts',(-20.0130523083208,-35.9594860855539,
122.367808286558)) ;
#47650 = CARTESIAN_POINT('Ctrl Pts',(-20.1640017994239,-35.779497005191,122.106806406757)) ;
#47651 = CARTESIAN_POINT('Ctrl Pts',(-19.8246772259409,-35.969377004791,122.279705165194)) ;
#47652 = CARTESIAN_POINT('Ctrl Pts',(-19.9285321533398,-35.7893879244282,
121.996676734452)) ;
#47653 = CARTESIAN_POINT('Ctrl Pts',(-19.6219619525249,-35.9793689980971,
122.224671937856)) ;
#47654 = CARTESIAN_POINT('Ctrl Pts',(-19.67513790255,-35.7993799177342,121.927884966154)) ;
#47655 = CARTESIAN_POINT('Ctrl Pts',(-19.4133577856184,-35.9893318620564,
122.205921690186)) ;
#47656 = CARTESIAN_POINT('Ctrl Pts',(-19.4143822634357,-35.8093427816935,
121.904446853395)) ;
#47657 = CARTESIAN_POINT('Ctrl Pts',(-19.2058271684787,-35.9992361218741,
122.223048719964)) ;
#47658 = CARTESIAN_POINT('Ctrl Pts',(-19.1549680514992,-35.8192470415113,
121.925855666197)) ;
#47659 = CARTESIAN_POINT('Ctrl Pts',(-19.0013346182317,-36.0092966124456,
122.276950648324)) ;
#47660 = CARTESIAN_POINT('Ctrl Pts',(-18.8993526736226,-35.8293075320827,
121.993232864711)) ;
#47661 = CARTESIAN_POINT('Ctrl Pts',(-18.8133472495276,-36.0191369620766,
122.363379425987)) ;
#47662 = CARTESIAN_POINT('Ctrl Pts',(-18.6643671184913,-35.8391478817137,
122.101269435871)) ;
#47663 = CARTESIAN_POINT('Ctrl Pts',(-18.639274963066,-36.0291999375666,122.483558189516)) ;
#47664 = CARTESIAN_POINT('Ctrl Pts',(-18.4467771153745,-35.8492108572037,
122.251492745729)) ;
#47665 = CARTESIAN_POINT('Ctrl Pts',(-18.4913225975558,-36.03909425771,122.629802380059)) ;
#47666 = CARTESIAN_POINT('Ctrl Pts',(-18.2618359407232,-35.8591051773471,
122.434298711921)) ;
#47667 = CARTESIAN_POINT('Ctrl Pts',(-18.3700032350797,-36.0490359708416,
122.799959594122)) ;
#47668 = CARTESIAN_POINT('Ctrl Pts',(-18.1101865601334,-35.8690468904787,
122.646995887001)) ;
#47669 = CARTESIAN_POINT('Ctrl Pts',(-18.2794097534421,-36.0590388606357,
122.98977331008)) ;
#47670 = CARTESIAN_POINT('Ctrl Pts',(-17.9969449047293,-35.8790497802728,
122.884263259516)) ;
#47671 = CARTESIAN_POINT('Ctrl Pts',(-18.2233291545152,-36.0690787177962,
123.193235333935)) ;
#47672 = CARTESIAN_POINT('Ctrl Pts',(-17.9268443214871,-35.8890896374333,
123.138590645404)) ;
#47673 = CARTESIAN_POINT('Ctrl Pts',(-18.2033834024276,-36.0789028986338,
123.39882135021)) ;
#47674 = CARTESIAN_POINT('Ctrl Pts',(-17.9019122829128,-35.8989138182709,
123.395574782342)) ;
#47675 = CARTESIAN_POINT('Ctrl Pts',(-18.2195239600936,-36.088959872137,123.609616533739)) ;
#47676 = CARTESIAN_POINT('Ctrl Pts',(-17.9220883778628,-35.9089707917741,
123.659068393619)) ;
#47677 = CARTESIAN_POINT('Ctrl Pts',(-18.271611751821,-36.0988879963241,123.811744957845)) ;
#47678 = CARTESIAN_POINT('Ctrl Pts',(-17.9871986049093,-35.9188989159612,
123.911729558089)) ;
#47679 = CARTESIAN_POINT('Ctrl Pts',(-18.3577130799816,-36.1088416913975,
124.002470019801)) ;
#47680 = CARTESIAN_POINT('Ctrl Pts',(-18.0948259751119,-35.9288526110346,
124.150136156797)) ;
#47681 = CARTESIAN_POINT('Ctrl Pts',(-18.4769655018994,-36.1188878849728,
124.176781923495)) ;
#47682 = CARTESIAN_POINT('Ctrl Pts',(-18.2438917115577,-35.9388988046099,
124.368025599995)) ;
#47683 = CARTESIAN_POINT('Ctrl Pts',(-18.6216180385642,-36.1287359873327,
124.324902759185)) ;
#47684 = CARTESIAN_POINT('Ctrl Pts',(-18.4247087145349,-35.9487469069698,
124.553177298368)) ;
#47685 = CARTESIAN_POINT('Ctrl Pts',(-18.7913448950173,-36.1386975755603,
124.447570338406)) ;
#47686 = CARTESIAN_POINT('Ctrl Pts',(-18.6368680943373,-35.9587084951974,
124.706511430656)) ;
#47687 = CARTESIAN_POINT('Ctrl Pts',(-18.9811968842923,-36.1487262457165,
124.539290730649)) ;
#47688 = CARTESIAN_POINT('Ctrl Pts',(-18.8741832744797,-35.9687371653537,
124.821161297278)) ;
#47689 = CARTESIAN_POINT('Ctrl Pts',(-19.181656131435,-36.1586365485983,124.596034870755)) ;
#47690 = CARTESIAN_POINT('Ctrl Pts',(-19.1247583602108,-35.9786474682354,
124.892091064519)) ;
#47691 = CARTESIAN_POINT('Ctrl Pts',(-19.3893970231701,-36.1685714324062,
124.617709477038)) ;
#47692 = CARTESIAN_POINT('Ctrl Pts',(-19.3844352240823,-35.9885823520433,
124.919183512007)) ;
#47693 = CARTESIAN_POINT('Ctrl Pts',(-19.5999475350248,-36.1786125740968,
124.602631344921)) ;
#47694 = CARTESIAN_POINT('Ctrl Pts',(-19.6476231191508,-35.9986234937339,
124.900335055066)) ;
#47695 = CARTESIAN_POINT('Ctrl Pts',(-19.801594360988,-36.1884996952608,124.552149971975)) ;
#47696 = CARTESIAN_POINT('Ctrl Pts',(-19.8996824512963,-36.0085106148979,
124.837232249301)) ;
#47697 = CARTESIAN_POINT('Ctrl Pts',(-19.9935521891846,-36.1984920381093,
124.466851568675)) ;
#47698 = CARTESIAN_POINT('Ctrl Pts',(-20.1396295182809,-36.0185029577464,
124.730608252142)) ;
#47699 = CARTESIAN_POINT('Ctrl Pts',(-20.1670027855748,-36.2084403393333,
124.34997292154)) ;
#47700 = CARTESIAN_POINT('Ctrl Pts',(-20.3564426703236,-36.0284512589704,
124.584508836111)) ;
#47701 = CARTESIAN_POINT('Ctrl Pts',(-20.317556983034,-36.2183779170154,124.205144373366)) ;
#47702 = CARTESIAN_POINT('Ctrl Pts',(-20.5446351269655,-36.0383888366525,
124.403471920414)) ;
#47703 = CARTESIAN_POINT('Ctrl Pts',(-20.4414732897196,-36.228364491466,124.035646668692)) ;
#47704 = CARTESIAN_POINT('Ctrl Pts',(-20.6995297067376,-36.0483754111031,
124.191598913458)) ;
#47705 = CARTESIAN_POINT('Ctrl Pts',(-20.5342434755889,-36.2383933013744,
123.846317983117)) ;
#47706 = CARTESIAN_POINT('Ctrl Pts',(-20.8154914356218,-36.0584042210115,
123.954937669147)) ;
#47707 = CARTESIAN_POINT('Ctrl Pts',(-20.5920471788539,-36.2482716226812,
123.646853844354)) ;
#47708 = CARTESIAN_POINT('Ctrl Pts',(-20.887745257479,-36.0682825423183,123.705606150759)) ;
#47709 = CARTESIAN_POINT('Ctrl Pts',(-20.6150868311933,-36.2582632700286,
123.438058171806)) ;
#47710 = CARTESIAN_POINT('Ctrl Pts',(-20.9165435264159,-36.0782741896657,
123.444611225449)) ;
#47711 = CARTESIAN_POINT('Ctrl Pts',(-20.6010348993728,-36.2682977934664,
123.22757890962)) ;
#47712 = CARTESIAN_POINT('Ctrl Pts',(-20.8989774525734,-36.0883087131035,
123.181512331536)) ;
#47713 = CARTESIAN_POINT('Ctrl Pts',(-20.5519217356949,-36.278161150345,123.026098209884)) ;
#47714 = CARTESIAN_POINT('Ctrl Pts',(-20.8375844347476,-36.0981720699821,
122.929660650926)) ;
#47715 = CARTESIAN_POINT('Ctrl Pts',(-20.4668785726101,-36.2882313770253,
122.832246771308)) ;
#47716 = CARTESIAN_POINT('Ctrl Pts',(-20.7312794061574,-36.1082422966624,
122.687347241547)) ;
#47717 = CARTESIAN_POINT('Ctrl Pts',(-20.3520998438178,-36.2980736851599,
122.660073371831)) ;
#47718 = CARTESIAN_POINT('Ctrl Pts',(-20.5878041611143,-36.1180846047971,
122.472130151302)) ;
#47719 = CARTESIAN_POINT('Ctrl Pts',(-20.2080189864902,-36.3080344171834,
122.508121261806)) ;
#47720 = CARTESIAN_POINT('Ctrl Pts',(-20.4077016432791,-36.1280453368205,
122.282190824122)) ;
#47721 = CARTESIAN_POINT('Ctrl Pts',(-20.038192664759,-36.3180723063815,122.382865970972)) ;
#47722 = CARTESIAN_POINT('Ctrl Pts',(-20.1954179813049,-36.1380832260186,
122.125622966376)) ;
#47723 = CARTESIAN_POINT('Ctrl Pts',(-19.8524204650629,-36.3279465893003,
122.290172252973)) ;
#47724 = CARTESIAN_POINT('Ctrl Pts',(-19.9632011127719,-36.1479575089374,
122.009756791366)) ;
#47725 = CARTESIAN_POINT('Ctrl Pts',(-19.6494833161937,-36.3380163339178,
122.23000096421)) ;
#47726 = CARTESIAN_POINT('Ctrl Pts',(-19.7095295605332,-36.1580272535549,
121.93454430428)) ;
#47727 = CARTESIAN_POINT('Ctrl Pts',(-19.4440883718789,-36.3478496442634,
122.206429346095)) ;
#47728 = CARTESIAN_POINT('Ctrl Pts',(-19.4527844206973,-36.1678605639005,
121.90508124975)) ;
#47729 = CARTESIAN_POINT('Ctrl Pts',(-19.2335726861195,-36.3578798876161,
122.218526616125)) ;
#47730 = CARTESIAN_POINT('Ctrl Pts',(-19.1896400044963,-36.1778908072532,
121.920204651437)) ;
#47731 = CARTESIAN_POINT('Ctrl Pts',(-19.0284500534322,-36.3679121755945,
122.267618772406)) ;
#47732 = CARTESIAN_POINT('Ctrl Pts',(-18.9332371754208,-36.1879230952316,
121.981571396722)) ;
#47733 = CARTESIAN_POINT('Ctrl Pts',(-18.838731464373,-36.3777393520626,122.349413172309)) ;
#47734 = CARTESIAN_POINT('Ctrl Pts',(-18.6960884547325,-36.1977502716997,
122.083816541885)) ;
#47735 = CARTESIAN_POINT('Ctrl Pts',(-18.66275010468,-36.3877447349294,122.464585531392)) ;
#47736 = CARTESIAN_POINT('Ctrl Pts',(-18.4761127317123,-36.2077556545666,
122.22778364051)) ;
#47737 = CARTESIAN_POINT('Ctrl Pts',(-18.5097875290952,-36.3977273739222,
122.608332945589)) ;
#47738 = CARTESIAN_POINT('Ctrl Pts',(-18.2849106465945,-36.2177382935593,
122.407469430057)) ;
#47739 = CARTESIAN_POINT('Ctrl Pts',(-18.3835787051131,-36.4077714410588,
122.777596314135)) ;
#47740 = CARTESIAN_POINT('Ctrl Pts',(-18.127151161634,-36.2277823606959,122.619049599079)) ;
#47741 = CARTESIAN_POINT('Ctrl Pts',(-18.2904495023674,-36.4175926598628,
122.961880766302)) ;
#47742 = CARTESIAN_POINT('Ctrl Pts',(-18.0107408057579,-36.2376035794999,
122.849407145954)) ;
#47743 = CARTESIAN_POINT('Ctrl Pts',(-18.2289081179151,-36.4276294988008,
123.163709417083)) ;
#47744 = CARTESIAN_POINT('Ctrl Pts',(-17.9338160941293,-36.247640418438,123.101693464145)) ;
#47745 = CARTESIAN_POINT('Ctrl Pts',(-18.2039726595456,-36.4376539108986,
123.372981004564)) ;
#47746 = CARTESIAN_POINT('Ctrl Pts',(-17.902648663204,-36.2576648305357,123.363283148383)) ;
#47747 = CARTESIAN_POINT('Ctrl Pts',(-18.215091683057,-36.4475059953039,123.579807254946)) ;
#47748 = CARTESIAN_POINT('Ctrl Pts',(-17.9165495303506,-36.267516914941,123.621816862721)) ;
#47749 = CARTESIAN_POINT('Ctrl Pts',(-18.2622958006013,-36.457496892047,123.784448454171)) ;
#47750 = CARTESIAN_POINT('Ctrl Pts',(-17.9755567901383,-36.2775078116842,
123.877618050233)) ;
#47751 = CARTESIAN_POINT('Ctrl Pts',(-18.3436111264905,-36.467414883948,123.976473263927)) ;
#47752 = CARTESIAN_POINT('Ctrl Pts',(-18.0772031608818,-36.2874258035851,
124.117648747743)) ;
#47753 = CARTESIAN_POINT('Ctrl Pts',(-18.4582275633681,-36.477442999405,124.153397817123)) ;
#47754 = CARTESIAN_POINT('Ctrl Pts',(-18.2204755143682,-36.2974539190421,
124.338803226218)) ;
#47755 = CARTESIAN_POINT('Ctrl Pts',(-18.5997258463659,-36.4873281753471,
124.305609353233)) ;
#47756 = CARTESIAN_POINT('Ctrl Pts',(-18.3973504809565,-36.3073390949842,
124.529066690562)) ;
#47757 = CARTESIAN_POINT('Ctrl Pts',(-18.7669421447371,-36.497317533754,124.432667569944)) ;
#47758 = CARTESIAN_POINT('Ctrl Pts',(-18.6063723872479,-36.3173284533911,
124.687887703223)) ;
#47759 = CARTESIAN_POINT('Ctrl Pts',(-18.9548477278309,-36.5073586813343,
124.528860622711)) ;
#47760 = CARTESIAN_POINT('Ctrl Pts',(-18.8412552934419,-36.3273696009714,
124.808127004772)) ;
#47761 = CARTESIAN_POINT('Ctrl Pts',(-19.1523079783713,-36.5171913043407,
124.590003139352)) ;
#47762 = CARTESIAN_POINT('Ctrl Pts',(-19.088082204701,-36.3372022239778,124.884553235414)) ;
#47763 = CARTESIAN_POINT('Ctrl Pts',(-19.3606753506828,-36.5271853754515,
124.616945728491)) ;
#47764 = CARTESIAN_POINT('Ctrl Pts',(-19.3485418518654,-36.3471962950886,
124.918229067231)) ;
#47765 = CARTESIAN_POINT('Ctrl Pts',(-19.5712789350383,-36.5372140330923,
124.606849592832)) ;
#47766 = CARTESIAN_POINT('Ctrl Pts',(-19.6117962054243,-36.3572249527295,
124.905606556835)) ;
#47767 = CARTESIAN_POINT('Ctrl Pts',(-19.7740000727098,-36.5470983592851,
124.561235915968)) ;
#47768 = CARTESIAN_POINT('Ctrl Pts',(-19.8651977309864,-36.3671092789223,
124.848586979554)) ;
#47769 = CARTESIAN_POINT('Ctrl Pts',(-19.9675160561407,-36.5570641027758,
124.48092624152)) ;
#47770 = CARTESIAN_POINT('Ctrl Pts',(-20.1070919688669,-36.3770750224129,
124.748197481995)) ;
#47771 = CARTESIAN_POINT('Ctrl Pts',(-20.1450804636381,-36.567092481907,124.36727939808)) ;
#47772 = CARTESIAN_POINT('Ctrl Pts',(-20.3290461476334,-36.3871034015441,
124.606136879299)) ;
#47773 = CARTESIAN_POINT('Ctrl Pts',(-20.2984821281396,-36.5769933281139,
124.226551618622)) ;
#47774 = CARTESIAN_POINT('Ctrl Pts',(-20.5207969131445,-36.397004247751,124.430224963369)) ;
#47775 = CARTESIAN_POINT('Ctrl Pts',(-20.4270554223315,-36.587051985531,124.058705204649)) ;
#47776 = CARTESIAN_POINT('Ctrl Pts',(-20.6815114754316,-36.4070629051681,
124.220415524595)) ;
#47777 = CARTESIAN_POINT('Ctrl Pts',(-20.5228088976676,-36.5969095483129,
123.874874545121)) ;
#47778 = CARTESIAN_POINT('Ctrl Pts',(-20.8012013743605,-36.41692046795,123.990625446808)) ;
#47779 = CARTESIAN_POINT('Ctrl Pts',(-20.5866346710282,-36.6069779508661,
123.673090041248)) ;
#47780 = CARTESIAN_POINT('Ctrl Pts',(-20.8809810994181,-36.4269888705032,
123.738394192383)) ;
#47781 = CARTESIAN_POINT('Ctrl Pts',(-20.6138518765132,-36.6168333496057,
123.46767623189)) ;
#47782 = CARTESIAN_POINT('Ctrl Pts',(-20.9150001537344,-36.4368442692428,
123.481625971228)) ;
#47783 = CARTESIAN_POINT('Ctrl Pts',(-20.6054955842666,-36.6268282166796,
123.257725834414)) ;
#47784 = CARTESIAN_POINT('Ctrl Pts',(-20.9045521214138,-36.4468391363167,
123.219187981031)) ;
#47785 = CARTESIAN_POINT('Ctrl Pts',(-20.5602021180779,-36.636859511663,123.051753465069)) ;
#47786 = CARTESIAN_POINT('Ctrl Pts',(-20.8479327596291,-36.4568704313002,
122.961723074886)) ;
#47787 = CARTESIAN_POINT('Ctrl Pts',(-20.4814585623447,-36.6467260363896,
122.859848018416)) ;
#47788 = CARTESIAN_POINT('Ctrl Pts',(-20.7495006730971,-36.4667369560267,
122.721841789066)) ;
#47789 = CARTESIAN_POINT('Ctrl Pts',(-20.3695334272533,-36.6567135070853,
122.682228468216)) ;
#47790 = CARTESIAN_POINT('Ctrl Pts',(-20.609591909687,-36.4767244267224,122.499818683266)) ;
#47791 = CARTESIAN_POINT('Ctrl Pts',(-20.2291188401914,-36.6666582666492,
122.527284926112)) ;
#47792 = CARTESIAN_POINT('Ctrl Pts',(-20.4340715146542,-36.4866691862863,
122.306140896146)) ;
#47793 = CARTESIAN_POINT('Ctrl Pts',(-20.0622231051933,-36.676703822598,122.397914061097)) ;
#47794 = CARTESIAN_POINT('Ctrl Pts',(-20.2254502142119,-36.4967147422351,
122.144429454285)) ;
#47795 = CARTESIAN_POINT('Ctrl Pts',(-19.8789187763763,-36.6865634109731,
122.301092451122)) ;
#47796 = CARTESIAN_POINT('Ctrl Pts',(-19.9963181527322,-36.5065743306102,
122.023404639029)) ;
#47797 = CARTESIAN_POINT('Ctrl Pts',(-19.6789119610615,-36.6965643661092,
122.23637511333)) ;
#47798 = CARTESIAN_POINT('Ctrl Pts',(-19.7463087037596,-36.5165752857463,
121.942510562632)) ;
#47799 = CARTESIAN_POINT('Ctrl Pts',(-19.4726764661033,-36.7064685933867,
122.207479051172)) ;
#47800 = CARTESIAN_POINT('Ctrl Pts',(-19.4885136890261,-36.5264795130239,
121.906393185174)) ;
#47801 = CARTESIAN_POINT('Ctrl Pts',(-19.2617182497028,-36.7165106702819,
122.214872705184)) ;
#47802 = CARTESIAN_POINT('Ctrl Pts',(-19.2248160077214,-36.536521589919,121.915638023373)) ;
#47803 = CARTESIAN_POINT('Ctrl Pts',(-19.057927154021,-36.726418282968,122.2581086562)) ;
#47804 = CARTESIAN_POINT('Ctrl Pts',(-18.9700774883834,-36.5464292026052,
121.969685726458)) ;
#47805 = CARTESIAN_POINT('Ctrl Pts',(-18.8619321432003,-36.7364728135838,
122.337188886544)) ;
#47806 = CARTESIAN_POINT('Ctrl Pts',(-18.7250847627801,-36.5564837332209,
122.068538595468)) ;
#47807 = CARTESIAN_POINT('Ctrl Pts',(-18.6859875564324,-36.7463336001326,
122.446869658722)) ;
#47808 = CARTESIAN_POINT('Ctrl Pts',(-18.5051552713082,-36.5663445197698,
122.205642071035)) ;
#47809 = CARTESIAN_POINT('Ctrl Pts',(-18.5294655824155,-36.7563273552037,
122.586972488339)) ;
#47810 = CARTESIAN_POINT('Ctrl Pts',(-18.309504624998,-36.5763382748409,122.380772756738)) ;
#47811 = CARTESIAN_POINT('Ctrl Pts',(-18.4004150751371,-36.7662527154437,
122.750983302961)) ;
#47812 = CARTESIAN_POINT('Ctrl Pts',(-18.1481936177485,-36.5862636350808,
122.585788118924)) ;
#47813 = CARTESIAN_POINT('Ctrl Pts',(-18.3008055717462,-36.776280644839,122.936753966816)) ;
#47814 = CARTESIAN_POINT('Ctrl Pts',(-18.0236841922653,-36.5962915644761,
122.818002834881)) ;
#47815 = CARTESIAN_POINT('Ctrl Pts',(-18.2356726374387,-36.7861669116383,
123.134158053417)) ;
#47816 = CARTESIAN_POINT('Ctrl Pts',(-17.9422706636189,-36.6061778312754,
123.064758942346)) ;
#47817 = CARTESIAN_POINT('Ctrl Pts',(-18.2052669474954,-36.7961986805365,
123.342818627154)) ;
#47818 = CARTESIAN_POINT('Ctrl Pts',(-17.9042663342486,-36.6162096001737,
123.325585129761)) ;
#47819 = CARTESIAN_POINT('Ctrl Pts',(-18.2112586660847,-36.8060802763801,
123.550511838692)) ;
#47820 = CARTESIAN_POINT('Ctrl Pts',(-17.9117588182437,-36.6260911960173,
123.585201643652)) ;
#47821 = CARTESIAN_POINT('Ctrl Pts',(-18.2539211094933,-36.8161421618481,
123.757665242363)) ;
#47822 = CARTESIAN_POINT('Ctrl Pts',(-17.9650896020763,-36.6361530814852,
123.844142860244)) ;
#47823 = CARTESIAN_POINT('Ctrl Pts',(-18.3302768913769,-36.825999595867,123.950348541592)) ;
#47824 = CARTESIAN_POINT('Ctrl Pts',(-18.0605371633806,-36.6460105155041,
124.084996144572)) ;
#47825 = CARTESIAN_POINT('Ctrl Pts',(-18.4400202960657,-36.8359928389089,
124.129465514795)) ;
#47826 = CARTESIAN_POINT('Ctrl Pts',(-18.1977180729179,-36.6560037585461,
124.308890236601)) ;
#47827 = CARTESIAN_POINT('Ctrl Pts',(-18.5783392874067,-36.8459235997953,
124.285860530243)) ;
#47828 = CARTESIAN_POINT('Ctrl Pts',(-18.3706217888367,-36.6659345194324,
124.504384734692)) ;
#47829 = CARTESIAN_POINT('Ctrl Pts',(-18.7977945098984,-36.8592725919925,
124.460845444457)) ;
#47830 = CARTESIAN_POINT('Ctrl Pts',(-18.6449288885869,-36.6792835116296,
124.7231001116)) ;
#47831 = CARTESIAN_POINT('Ctrl Pts',(-19.0564575910086,-36.8725409648089,
124.573487171901)) ;
#47832 = CARTESIAN_POINT('Ctrl Pts',(-18.9682246085567,-36.692551884446,124.863897618014)) ;
#47833 = CARTESIAN_POINT('Ctrl Pts',(-19.332518152077,-36.8858239061933,124.615432948066)) ;
#47834 = CARTESIAN_POINT('Ctrl Pts',(-19.3133563776516,-36.7058348258304,
124.916340475203)) ;
#47835 = CARTESIAN_POINT('Ctrl Pts',(-19.5435804177348,-36.8958666920355,
124.610274690913)) ;
#47836 = CARTESIAN_POINT('Ctrl Pts',(-19.5771730601609,-36.7158776116726,
124.9098870958)) ;
#47837 = CARTESIAN_POINT('Ctrl Pts',(-19.7466220723449,-36.9057166345876,
124.569566521813)) ;
#47838 = CARTESIAN_POINT('Ctrl Pts',(-19.8309776235917,-36.7257275542247,
124.858999538569)) ;
#47839 = CARTESIAN_POINT('Ctrl Pts',(-19.9425753325179,-36.9157138675065,
124.493590570334)) ;
#47840 = CARTESIAN_POINT('Ctrl Pts',(-20.0759163398289,-36.7357247871437,
124.764028514352)) ;
#47841 = CARTESIAN_POINT('Ctrl Pts',(-20.1225212109622,-36.9257287628411,
124.384267908977)) ;
#47842 = CARTESIAN_POINT('Ctrl Pts',(-20.3008516831836,-36.7457396824782,
124.627366616209)) ;
#47843 = CARTESIAN_POINT('Ctrl Pts',(-20.3318880894533,-36.9389684394793,
124.200821795761)) ;
#47844 = CARTESIAN_POINT('Ctrl Pts',(-20.5625371625823,-36.7589793591164,
124.398087289449)) ;
#47845 = CARTESIAN_POINT('Ctrl Pts',(-20.528163224449,-36.9555156638846,123.9088995619)) ;
#47846 = CARTESIAN_POINT('Ctrl Pts',(-20.8079029753691,-36.7755265835217,
124.033128787356)) ;
#47847 = CARTESIAN_POINT('Ctrl Pts',(-20.6137528393046,-36.9721631010157,
123.56536786537)) ;
#47848 = CARTESIAN_POINT('Ctrl Pts',(-20.9148689308505,-36.7921740206528,
123.60379676647)) ;
#47849 = CARTESIAN_POINT('Ctrl Pts',(-20.6085683059766,-36.9854525984939,
123.286061986322)) ;
#47850 = CARTESIAN_POINT('Ctrl Pts',(-20.9083945687103,-36.805463518131,123.254597757722)) ;
#47851 = CARTESIAN_POINT('Ctrl Pts',(-20.5693560188396,-36.9953260063163,
123.082217819628)) ;
#47852 = CARTESIAN_POINT('Ctrl Pts',(-20.8593749513475,-36.8153369259534,
122.99980702422)) ;
#47853 = CARTESIAN_POINT('Ctrl Pts',(-20.4940428412356,-37.005378383909,122.884773388024)) ;
#47854 = CARTESIAN_POINT('Ctrl Pts',(-20.7652312032613,-36.8253893035461,
122.752998369539)) ;
#47855 = CARTESIAN_POINT('Ctrl Pts',(-20.3871047058436,-37.0152820374499,
122.706108282335)) ;
#47856 = CARTESIAN_POINT('Ctrl Pts',(-20.6315577727922,-36.835292957087,122.529670136184)) ;
#47857 = CARTESIAN_POINT('Ctrl Pts',(-20.2506236096731,-37.0252263064452,
122.547784485508)) ;
#47858 = CARTESIAN_POINT('Ctrl Pts',(-20.4609498467479,-36.8452372260823,
122.331765024518)) ;
#47859 = CARTESIAN_POINT('Ctrl Pts',(-20.0335787700198,-37.0385573147779,
122.37035520076)) ;
#47860 = CARTESIAN_POINT('Ctrl Pts',(-20.1896663855523,-36.858568234415,122.109990345323)) ;
#47861 = CARTESIAN_POINT('Ctrl Pts',(-19.7113303634737,-37.0551788953021,
122.225449965275)) ;
#47862 = CARTESIAN_POINT('Ctrl Pts',(-19.7868089891935,-36.8751898149393,
121.928852787723)) ;
#47863 = CARTESIAN_POINT('Ctrl Pts',(-19.3605381967804,-37.0717215660005,
122.198625173765)) ;
#47864 = CARTESIAN_POINT('Ctrl Pts',(-19.3483970122196,-36.8917324856377,
121.895325330693)) ;
#47865 = CARTESIAN_POINT('Ctrl Pts',(-19.084756283337,-37.0850707255635,122.250326858334)) ;
#47866 = CARTESIAN_POINT('Ctrl Pts',(-19.0036058959069,-36.9050816452006,
121.959959179237)) ;
#47867 = CARTESIAN_POINT('Ctrl Pts',(-18.8243006026364,-37.098298875723,122.34794994263)) ;
#47868 = CARTESIAN_POINT('Ctrl Pts',(-18.678061892058,-36.9183097953601,122.081981867065)) ;
#47869 = CARTESIAN_POINT('Ctrl Pts',(-18.5364100435384,-37.1149295528605,
122.553165444984)) ;
#47870 = CARTESIAN_POINT('Ctrl Pts',(-18.3181836591371,-36.9349404724976,
122.338513488551)) ;
#47871 = CARTESIAN_POINT('Ctrl Pts',(-18.2963005996991,-37.1348324921486,
122.901714167161)) ;
#47872 = CARTESIAN_POINT('Ctrl Pts',(-18.0180562107992,-36.9548434117857,
122.774198058464)) ;
#47873 = CARTESIAN_POINT('Ctrl Pts',(-18.1891582578052,-37.1547353587518,
123.311031502207)) ;
#47874 = CARTESIAN_POINT('Ctrl Pts',(-17.884130698863,-36.974746278389,123.285845641894)) ;
#47875 = CARTESIAN_POINT('Ctrl Pts',(-18.2275156867731,-37.1746485238567,
123.732793359214)) ;
#47876 = CARTESIAN_POINT('Ctrl Pts',(-17.9320811341198,-36.9946594434938,
123.813046654327)) ;
#47877 = CARTESIAN_POINT('Ctrl Pts',(-18.409140585469,-37.194684352998,124.118086353196)) ;
#47878 = CARTESIAN_POINT('Ctrl Pts',(-18.159115508631,-37.0146952726351,124.294661831118)) ;
#47879 = CARTESIAN_POINT('Ctrl Pts',(-18.7080016710259,-37.2145029278761,
124.41531311931)) ;
#47880 = CARTESIAN_POINT('Ctrl Pts',(-18.5326928560836,-37.0345138475132,
124.666191700449)) ;
#47881 = CARTESIAN_POINT('Ctrl Pts',(-19.0927718739483,-37.2344732289181,
124.594578380774)) ;
#47882 = CARTESIAN_POINT('Ctrl Pts',(-19.0136563927245,-37.0544841485552,
124.890270639901)) ;
#47883 = CARTESIAN_POINT('Ctrl Pts',(-19.5142339391822,-37.2543647612826,
124.631795562197)) ;
#47884 = CARTESIAN_POINT('Ctrl Pts',(-19.5404829664515,-37.0743756809197,
124.936789595179)) ;
#47885 = CARTESIAN_POINT('Ctrl Pts',(-19.9254766838517,-37.2743878590991,
124.521993821233)) ;
#47886 = CARTESIAN_POINT('Ctrl Pts',(-20.0545360586126,-37.0943987787363,
124.799534983068)) ;
#47887 = CARTESIAN_POINT('Ctrl Pts',(-20.2709110278147,-37.2941846120191,
124.281362408259)) ;
#47888 = CARTESIAN_POINT('Ctrl Pts',(-20.4863256454403,-37.1141955316562,
124.498745537816)) ;
#47889 = CARTESIAN_POINT('Ctrl Pts',(-20.5163858033962,-37.3141457005079,
123.935170853578)) ;
#47890 = CARTESIAN_POINT('Ctrl Pts',(-20.7931678599209,-37.134156620145,124.066005974626)) ;
#47891 = CARTESIAN_POINT('Ctrl Pts',(-20.6282493094601,-37.33412396944,123.52533621411)) ;
#47892 = CARTESIAN_POINT('Ctrl Pts',(-20.9329957734479,-37.1541348890772,
123.553712501942)) ;
#47893 = CARTESIAN_POINT('Ctrl Pts',(-20.5944348756213,-37.353943984231,123.105306555051)) ;
#47894 = CARTESIAN_POINT('Ctrl Pts',(-20.8907271345775,-37.1739549038682,
123.028678283237)) ;
#47895 = CARTESIAN_POINT('Ctrl Pts',(-20.419241626978,-37.3738823934829,122.719230553153)) ;
#47896 = CARTESIAN_POINT('Ctrl Pts',(-20.6717362479,-37.19389331312,122.546084069936)) ;
#47897 = CARTESIAN_POINT('Ctrl Pts',(-20.1204934119422,-37.3939295108753,
122.415110115247)) ;
#47898 = CARTESIAN_POINT('Ctrl Pts',(-20.298300215747,-37.2139404305124,122.165933042875)) ;
#47899 = CARTESIAN_POINT('Ctrl Pts',(-19.7397550775313,-37.4137757567091,
122.233254243053)) ;
#47900 = CARTESIAN_POINT('Ctrl Pts',(-19.8223796112928,-37.2337866763463,
121.938614397227)) ;
#47901 = CARTESIAN_POINT('Ctrl Pts',(-19.3198536517042,-37.4336247252212,
122.19057464082)) ;
#47902 = CARTESIAN_POINT('Ctrl Pts',(-19.2975051439848,-37.2536356448583,
121.885263707638)) ;
#47903 = CARTESIAN_POINT('Ctrl Pts',(-18.9066386247496,-37.4536750275325,
122.295305344993)) ;
#47904 = CARTESIAN_POINT('Ctrl Pts',(-18.7809853427193,-37.2736859471696,
122.01617607887)) ;
#47905 = CARTESIAN_POINT('Ctrl Pts',(-18.5576843444494,-37.4735099499637,
122.53234187102)) ;
#47906 = CARTESIAN_POINT('Ctrl Pts',(-18.3447935795883,-37.2935208696008,
122.312469305322)) ;
#47907 = CARTESIAN_POINT('Ctrl Pts',(-18.3088629623989,-37.4934403511896,
122.87517401801)) ;
#47908 = CARTESIAN_POINT('Ctrl Pts',(-18.0337656489116,-37.3134512708267,
122.741007439741)) ;
#47909 = CARTESIAN_POINT('Ctrl Pts',(-18.191627159294,-37.5133252965484,123.281572566289)) ;
#47910 = CARTESIAN_POINT('Ctrl Pts',(-17.8872187178112,-37.3333362161856,
123.249003693809)) ;
#47911 = CARTESIAN_POINT('Ctrl Pts',(-18.2210576117943,-37.5333979046998,
123.707273120117)) ;
#47912 = CARTESIAN_POINT('Ctrl Pts',(-17.9240043991043,-37.353408824337,123.781130410511)) ;
#47913 = CARTESIAN_POINT('Ctrl Pts',(-18.3915612941918,-37.5531892210279,
124.092070927854)) ;
#47914 = CARTESIAN_POINT('Ctrl Pts',(-18.1371306277917,-37.3732001406651,
124.262126611238)) ;
#47915 = CARTESIAN_POINT('Ctrl Pts',(-18.6846818237289,-37.5731540107952,
124.399080855856)) ;
#47916 = CARTESIAN_POINT('Ctrl Pts',(-18.5035285318798,-37.3931649304323,
124.645891221234)) ;
#47917 = CARTESIAN_POINT('Ctrl Pts',(-19.0658286606464,-37.5931369665455,
124.5868719561)) ;
#47918 = CARTESIAN_POINT('Ctrl Pts',(-18.979960539183,-37.4131478861826,124.8806328502)) ;
#47919 = CARTESIAN_POINT('Ctrl Pts',(-19.4844281526955,-37.6129454885216,
124.633785399383)) ;
#47920 = CARTESIAN_POINT('Ctrl Pts',(-19.5032077670167,-37.4329564081588,
124.93927814081)) ;
#47921 = CARTESIAN_POINT('Ctrl Pts',(-19.8975569980139,-37.6329310632575,
124.534652953361)) ;
#47922 = CARTESIAN_POINT('Ctrl Pts',(-20.0196196742879,-37.4529419828946,
124.815366561225)) ;
#47923 = CARTESIAN_POINT('Ctrl Pts',(-20.2503434108889,-37.6528137033259,
124.301519197252)) ;
#47924 = CARTESIAN_POINT('Ctrl Pts',(-20.4606042546842,-37.472824622963,124.523953283866)) ;
#47925 = CARTESIAN_POINT('Ctrl Pts',(-20.503477443757,-37.6727690154578,123.96110057976)) ;
#47926 = CARTESIAN_POINT('Ctrl Pts',(-20.7770251297192,-37.4927799350949,
124.098432867934)) ;
#47927 = CARTESIAN_POINT('Ctrl Pts',(-20.6250594607957,-37.6926433720656,
123.556310778876)) ;
#47928 = CARTESIAN_POINT('Ctrl Pts',(-20.9290068708027,-37.5126542917027,
123.592447664143)) ;
#47929 = CARTESIAN_POINT('Ctrl Pts',(-20.60136228044,-37.7126255789266,123.132144136794)) ;
#47930 = CARTESIAN_POINT('Ctrl Pts',(-20.8993899561854,-37.5326364985638,
123.062239130214)) ;
#47931 = CARTESIAN_POINT('Ctrl Pts',(-20.4345064783654,-37.7325566568766,
122.742488170039)) ;
#47932 = CARTESIAN_POINT('Ctrl Pts',(-20.690825481049,-37.5525675765137,122.575167631245)) ;
#47933 = CARTESIAN_POINT('Ctrl Pts',(-20.1449218342173,-37.7524836317316,
122.433312486334)) ;
#47934 = CARTESIAN_POINT('Ctrl Pts',(-20.3288457045334,-37.5724945513687,
122.188694790906)) ;
#47935 = CARTESIAN_POINT('Ctrl Pts',(-19.769249258697,-37.7723160906805,122.241620195832)) ;
#47936 = CARTESIAN_POINT('Ctrl Pts',(-19.8592684233419,-37.5923270103176,
121.94907564169)) ;
#47937 = CARTESIAN_POINT('Ctrl Pts',(-19.417912839103,-37.7889737748557,122.197692406398)) ;
#47938 = CARTESIAN_POINT('Ctrl Pts',(-19.4200658004663,-37.6089846944928,
121.894159881209)) ;
#47939 = CARTESIAN_POINT('Ctrl Pts',(-19.1419000183344,-37.8022229987628,
122.235811998342)) ;
#47940 = CARTESIAN_POINT('Ctrl Pts',(-19.0750788995633,-37.6222339183999,
121.941806794377)) ;
#47941 = CARTESIAN_POINT('Ctrl Pts',(-18.9408249504578,-37.812272020214,122.300516733024)) ;
#47942 = CARTESIAN_POINT('Ctrl Pts',(-18.8237258577179,-37.6322829398511,
122.022687580734)) ;
#47943 = CARTESIAN_POINT('Ctrl Pts',(-18.75748940626,-37.8221320284445,122.39727315745)) ;
#47944 = CARTESIAN_POINT('Ctrl Pts',(-18.5945663208798,-37.6421429480816,
122.143620577139)) ;
#47945 = CARTESIAN_POINT('Ctrl Pts',(-18.5363454819024,-37.8354155416691,
122.567770253279)) ;
#47946 = CARTESIAN_POINT('Ctrl Pts',(-18.318087679396,-37.6554264613062,122.356789242169)) ;
#47947 = CARTESIAN_POINT('Ctrl Pts',(-18.3218393831635,-37.8520614606699,
122.849331128677)) ;
#47948 = CARTESIAN_POINT('Ctrl Pts',(-18.0500066419728,-37.672072380307,122.708670183428)) ;
#47949 = CARTESIAN_POINT('Ctrl Pts',(-18.2164325706239,-37.868615438486,123.185138476082)) ;
#47950 = CARTESIAN_POINT('Ctrl Pts',(-17.9182173116251,-37.6886263581231,
123.1284860917)) ;
#47951 = CARTESIAN_POINT('Ctrl Pts',(-18.2044905733032,-37.8819751674576,
123.465776368873)) ;
#47952 = CARTESIAN_POINT('Ctrl Pts',(-17.9032980831102,-37.7019860870947,
123.479244069035)) ;
#47953 = CARTESIAN_POINT('Ctrl Pts',(-18.2317111895261,-37.8918682192543,
123.671978883509)) ;
#47954 = CARTESIAN_POINT('Ctrl Pts',(-17.9373186787806,-37.7118791388914,
123.737005381468)) ;
#47955 = CARTESIAN_POINT('Ctrl Pts',(-18.294652658177,-37.9018581845353,123.87232240774)) ;
#47956 = CARTESIAN_POINT('Ctrl Pts',(-18.0159935017335,-37.7218691041725,
123.987433562175)) ;
#47957 = CARTESIAN_POINT('Ctrl Pts',(-18.3909713233348,-37.9118100653962,
124.058088930702)) ;
#47958 = CARTESIAN_POINT('Ctrl Pts',(-18.1363891804887,-37.7318209850333,
124.219643590471)) ;
#47959 = CARTESIAN_POINT('Ctrl Pts',(-18.5194225453027,-37.921858417088,124.225768775159)) ;
#47960 = CARTESIAN_POINT('Ctrl Pts',(-18.2969510924967,-37.7418693367251,
124.42924502608)) ;
#47961 = CARTESIAN_POINT('Ctrl Pts',(-18.671696215703,-37.9316997011942,124.365864629888)) ;
#47962 = CARTESIAN_POINT('Ctrl Pts',(-18.4872912316246,-37.7517106208313,
124.60436691775)) ;
#47963 = CARTESIAN_POINT('Ctrl Pts',(-18.8482704727161,-37.9416864043198,
124.479380726251)) ;
#47964 = CARTESIAN_POINT('Ctrl Pts',(-18.7080075972399,-37.761697323957,124.746264446467)) ;
#47965 = CARTESIAN_POINT('Ctrl Pts',(-19.0408922738897,-37.9516214331373,
124.560242685434)) ;
#47966 = CARTESIAN_POINT('Ctrl Pts',(-18.9487838243805,-37.7716323527744,
124.847344520004)) ;
#47967 = CARTESIAN_POINT('Ctrl Pts',(-19.2470723983466,-37.9616772280442,
124.606804319472)) ;
#47968 = CARTESIAN_POINT('Ctrl Pts',(-19.2065084133453,-37.7816881476813,
124.905549326523)) ;
#47969 = CARTESIAN_POINT('Ctrl Pts',(-19.4534751390395,-37.9715055913335,
124.616954335681)) ;
#47970 = CARTESIAN_POINT('Ctrl Pts',(-19.4645118314012,-37.7915165109706,
124.918239663582)) ;
#47971 = CARTESIAN_POINT('Ctrl Pts',(-19.6633369830596,-37.9815665612314,
124.590805337205)) ;
#47972 = CARTESIAN_POINT('Ctrl Pts',(-19.7268395348764,-37.8015774808685,
124.885556198697)) ;
#47973 = CARTESIAN_POINT('Ctrl Pts',(-19.8625213753835,-37.9914808401212,
124.529341700821)) ;
#47974 = CARTESIAN_POINT('Ctrl Pts',(-19.975820977289,-37.8114917597583,124.808729302256)) ;
#47975 = CARTESIAN_POINT('Ctrl Pts',(-20.0499508132267,-38.0014898345894,
124.433695820454)) ;
#47976 = CARTESIAN_POINT('Ctrl Pts',(-20.2101091148539,-37.8215007542265,
124.689174409311)) ;
#47977 = CARTESIAN_POINT('Ctrl Pts',(-20.2180109913369,-38.0115196691532,
124.306354445413)) ;
#47978 = CARTESIAN_POINT('Ctrl Pts',(-20.4201860704738,-37.8315305887903,
124.529999912084)) ;
#47979 = CARTESIAN_POINT('Ctrl Pts',(-20.3592543198836,-38.0213778992254,
124.154667140303)) ;
#47980 = CARTESIAN_POINT('Ctrl Pts',(-20.596742436033,-37.8413888188625,124.340392518913)) ;
#47981 = CARTESIAN_POINT('Ctrl Pts',(-20.4738072405077,-38.0313766049678,
123.978459990424)) ;
#47982 = CARTESIAN_POINT('Ctrl Pts',(-20.7399359738029,-37.8513875246049,
124.120135025723)) ;
#47983 = CARTESIAN_POINT('Ctrl Pts',(-20.5554252299828,-38.0412712608866,
123.787082603069)) ;
#47984 = CARTESIAN_POINT('Ctrl Pts',(-20.8419611023496,-37.8612821805237,
123.880914135963)) ;
#47985 = CARTESIAN_POINT('Ctrl Pts',(-20.6032952967785,-38.0513343252705,
123.581049295425)) ;
#47986 = CARTESIAN_POINT('Ctrl Pts',(-20.9018013798977,-37.8713452449077,
123.62337316206)) ;
#47987 = CARTESIAN_POINT('Ctrl Pts',(-20.6146442268699,-38.0611739835504,
123.374466194036)) ;
#47988 = CARTESIAN_POINT('Ctrl Pts',(-20.9159903077687,-37.8811849031876,
123.365144028715)) ;
#47989 = CARTESIAN_POINT('Ctrl Pts',(-20.5896648476914,-38.0712371506323,
123.164415788226)) ;
#47990 = CARTESIAN_POINT('Ctrl Pts',(-20.8847687942713,-37.8912480702694,
123.102580743054)) ;
#47991 = CARTESIAN_POINT('Ctrl Pts',(-20.5294350178213,-38.0811313957594,
122.965294396189)) ;
#47992 = CARTESIAN_POINT('Ctrl Pts',(-20.809484036126,-37.9011423153965,122.853677895888)) ;
#47993 = CARTESIAN_POINT('Ctrl Pts',(-20.4356240821456,-38.091073217364,122.778550856413)) ;
#47994 = CARTESIAN_POINT('Ctrl Pts',(-20.6922226402162,-37.9110841370011,
122.620247034589)) ;
#47995 = CARTESIAN_POINT('Ctrl Pts',(-20.3100810134852,-38.1010757482821,
122.609819097008)) ;
#47996 = CARTESIAN_POINT('Ctrl Pts',(-20.5352958890887,-37.9210866679192,
122.40933067988)) ;
#47997 = CARTESIAN_POINT('Ctrl Pts',(-20.1564607952852,-38.1111103747396,
122.465250449914)) ;
#47998 = CARTESIAN_POINT('Ctrl Pts',(-20.3432724835516,-37.9311212943767,
122.228617908719)) ;
#47999 = CARTESIAN_POINT('Ctrl Pts',(-19.9835623722376,-38.120955909726,122.351445881566)) ;
#48000 = CARTESIAN_POINT('Ctrl Pts',(-20.1271504515569,-37.9409668293631,
122.086359667686)) ;
#48001 = CARTESIAN_POINT('Ctrl Pts',(-19.7910718790852,-38.130939334565,122.267833463766)) ;
#48002 = CARTESIAN_POINT('Ctrl Pts',(-19.8865382083941,-37.9509502542022,
121.981841696408)) ;
#48003 = CARTESIAN_POINT('Ctrl Pts',(-19.5876306579575,-38.1408897249301,
122.219111287809)) ;
#48004 = CARTESIAN_POINT('Ctrl Pts',(-19.6322370248592,-37.9609006445672,
121.920936388949)) ;
#48005 = CARTESIAN_POINT('Ctrl Pts',(-19.377833549305,-38.1508873652272,122.206109169437)) ;
#48006 = CARTESIAN_POINT('Ctrl Pts',(-19.3699906918077,-37.9708982848643,
121.904681189327)) ;
#48007 = CARTESIAN_POINT('Ctrl Pts',(-19.1681777198956,-38.1609264457904,
122.230248686122)) ;
#48008 = CARTESIAN_POINT('Ctrl Pts',(-19.1079206636273,-37.9809373654275,
121.934852971173)) ;
#48009 = CARTESIAN_POINT('Ctrl Pts',(-18.9700348987054,-38.1707525965595,
122.288711476729)) ;
#48010 = CARTESIAN_POINT('Ctrl Pts',(-18.860240682653,-37.9907635161966,122.007929238581)) ;
#48011 = CARTESIAN_POINT('Ctrl Pts',(-18.7805861370791,-38.1808091714886,
122.382535043644)) ;
#48012 = CARTESIAN_POINT('Ctrl Pts',(-18.6234287247367,-38.0008200911257,
122.125206427547)) ;
#48013 = CARTESIAN_POINT('Ctrl Pts',(-18.6124721251259,-38.1907497108689,
122.506687338433)) ;
#48014 = CARTESIAN_POINT('Ctrl Pts',(-18.4132844279037,-38.010760630506,122.280394942276)) ;
#48015 = CARTESIAN_POINT('Ctrl Pts',(-18.4685228176919,-38.2006541038453,
122.657141441856)) ;
#48016 = CARTESIAN_POINT('Ctrl Pts',(-18.2333456791287,-38.0206650234824,
122.468461282899)) ;
#48017 = CARTESIAN_POINT('Ctrl Pts',(-18.3513466171436,-38.2107007580502,
122.832848241972)) ;
#48018 = CARTESIAN_POINT('Ctrl Pts',(-18.0868734496572,-38.0307116776873,
122.68809334047)) ;
#48019 = CARTESIAN_POINT('Ctrl Pts',(-18.2675409912502,-38.2205963199886,
123.023293670157)) ;
#48020 = CARTESIAN_POINT('Ctrl Pts',(-17.9821139835232,-38.0406072396257,
122.926149688474)) ;
#48021 = CARTESIAN_POINT('Ctrl Pts',(-18.2172590198728,-38.2306583978341,
123.228736388666)) ;
#48022 = CARTESIAN_POINT('Ctrl Pts',(-17.9192592235961,-38.0506693174713,
123.182952338498)) ;
#48023 = CARTESIAN_POINT('Ctrl Pts',(-18.203592355486,-38.2405010962479,123.435232302293)) ;
#48024 = CARTESIAN_POINT('Ctrl Pts',(-17.9021734628791,-38.060512015885,123.441072933946)) ;
#48025 = CARTESIAN_POINT('Ctrl Pts',(-18.2258256609928,-38.2504918712094,
123.644062640654)) ;
#48026 = CARTESIAN_POINT('Ctrl Pts',(-17.9299628607559,-38.0705027908465,
123.702111270586)) ;
#48027 = CARTESIAN_POINT('Ctrl Pts',(-18.2836555871143,-38.2604197362285,
123.844617912795)) ;
#48028 = CARTESIAN_POINT('Ctrl Pts',(-18.0022482230094,-38.0804306558656,
123.952806457239)) ;
#48029 = CARTESIAN_POINT('Ctrl Pts',(-18.3756740561465,-38.2704084809947,
124.033382785649)) ;
#48030 = CARTESIAN_POINT('Ctrl Pts',(-18.1172694269985,-38.0904194006318,
124.188763665487)) ;
#48031 = CARTESIAN_POINT('Ctrl Pts',(-18.4998651142318,-38.2804412665816,
124.203869104548)) ;
#48032 = CARTESIAN_POINT('Ctrl Pts',(-18.2725063779841,-38.1004521862187,
124.401872836885)) ;
#48033 = CARTESIAN_POINT('Ctrl Pts',(-18.649102754769,-38.2903079512023,124.347923475099)) ;
#48034 = CARTESIAN_POINT('Ctrl Pts',(-18.4590525160662,-38.1103188708394,
124.581942987114)) ;
#48035 = CARTESIAN_POINT('Ctrl Pts',(-18.8224168744023,-38.3002698433654,
124.465501995061)) ;
#48036 = CARTESIAN_POINT('Ctrl Pts',(-18.6756943059788,-38.1202807630025,
124.728918023254)) ;
#48037 = CARTESIAN_POINT('Ctrl Pts',(-19.0150124373623,-38.310303320278,124.551507630539)) ;
#48038 = CARTESIAN_POINT('Ctrl Pts',(-18.9164378070942,-38.1303142399151,
124.836426983259)) ;
#48039 = CARTESIAN_POINT('Ctrl Pts',(-19.2165276853303,-38.3201876615263,
124.602331746933)) ;
#48040 = CARTESIAN_POINT('Ctrl Pts',(-19.1683321359747,-38.1401985811634,
124.899959302381)) ;
#48041 = CARTESIAN_POINT('Ctrl Pts',(-19.4274995678866,-38.3302506036474,
124.617665373522)) ;
#48042 = CARTESIAN_POINT('Ctrl Pts',(-19.4320465863447,-38.1502615232845,
124.919128358715)) ;
#48043 = CARTESIAN_POINT('Ctrl Pts',(-19.6335365424027,-38.340101005267,124.596684953135)) ;
#48044 = CARTESIAN_POINT('Ctrl Pts',(-19.6895940464433,-38.1601119249041,
124.892904733968)) ;
#48045 = CARTESIAN_POINT('Ctrl Pts',(-19.8364952866382,-38.3501278940566,
124.539756466439)) ;
#48046 = CARTESIAN_POINT('Ctrl Pts',(-19.9432929414163,-38.1701388136938,
124.821745925476)) ;
#48047 = CARTESIAN_POINT('Ctrl Pts',(-20.0262936192823,-38.3601565090128,
124.447932183891)) ;
#48048 = CARTESIAN_POINT('Ctrl Pts',(-20.1805416769707,-38.18016742865,124.706967424635)) ;
#48049 = CARTESIAN_POINT('Ctrl Pts',(-20.1943496803359,-38.3700017321329,
124.327134832878)) ;
#48050 = CARTESIAN_POINT('Ctrl Pts',(-20.3906137720793,-38.19001265177,124.555971632204)) ;
#48051 = CARTESIAN_POINT('Ctrl Pts',(-20.3414292534082,-38.3799924159389,
124.17718516851)) ;
#48052 = CARTESIAN_POINT('Ctrl Pts',(-20.574464611682,-38.200003335576,124.368535624673)) ;
#48053 = CARTESIAN_POINT('Ctrl Pts',(-20.4604073331127,-38.3900302980113,
124.002897673385)) ;
#48054 = CARTESIAN_POINT('Ctrl Pts',(-20.7231886883335,-38.2100412176484,
124.1506774248)) ;
#48055 = CARTESIAN_POINT('Ctrl Pts',(-20.5459739903831,-38.3998746576501,
123.814446734929)) ;
#48056 = CARTESIAN_POINT('Ctrl Pts',(-20.8301490996899,-38.2198855772873,
123.915113415464)) ;
#48057 = CARTESIAN_POINT('Ctrl Pts',(-20.5986469705977,-38.4098595282649,
123.611278948678)) ;
#48058 = CARTESIAN_POINT('Ctrl Pts',(-20.8959919668574,-38.229870447902,123.661153850813)) ;
#48059 = CARTESIAN_POINT('Ctrl Pts',(-20.6152674854277,-38.4197988115935,
123.402955218507)) ;
#48060 = CARTESIAN_POINT('Ctrl Pts',(-20.9167692456538,-38.2398097312307,
123.400748772405)) ;
#48061 = CARTESIAN_POINT('Ctrl Pts',(-20.5952009161257,-38.4298394209667,
123.192847662507)) ;
#48062 = CARTESIAN_POINT('Ctrl Pts',(-20.8916876625912,-38.2498503406038,
123.138114322854)) ;
#48063 = CARTESIAN_POINT('Ctrl Pts',(-20.5399668125986,-38.4397242718799,
122.992486933)) ;
#48064 = CARTESIAN_POINT('Ctrl Pts',(-20.8226462971584,-38.259735191517,122.887662089246)) ;
#48065 = CARTESIAN_POINT('Ctrl Pts',(-20.4499783459561,-38.4497262280487,
122.802478082637)) ;
#48066 = CARTESIAN_POINT('Ctrl Pts',(-20.710161993773,-38.2697371476858,122.650150261944)) ;
#48067 = CARTESIAN_POINT('Ctrl Pts',(-20.3294778320045,-38.4596448247692,
122.632260562364)) ;
#48068 = CARTESIAN_POINT('Ctrl Pts',(-20.5595370994859,-38.2796557444063,
122.437376954978)) ;
#48069 = CARTESIAN_POINT('Ctrl Pts',(-20.1793517400514,-38.469691646845,122.483728376265)) ;
#48070 = CARTESIAN_POINT('Ctrl Pts',(-20.3718806509748,-38.2897025664821,
122.251710845181)) ;
#48071 = CARTESIAN_POINT('Ctrl Pts',(-20.0087562410276,-38.4795659279577,
122.365386621562)) ;
#48072 = CARTESIAN_POINT('Ctrl Pts',(-20.1586361996875,-38.2995768475948,
122.103781930093)) ;
#48073 = CARTESIAN_POINT('Ctrl Pts',(-19.8168874460983,-38.4896201280023,
122.27679388918)) ;
#48074 = CARTESIAN_POINT('Ctrl Pts',(-19.9188009996355,-38.3096310476394,
121.993039914093)) ;
#48075 = CARTESIAN_POINT('Ctrl Pts',(-19.6157267682506,-38.4995155576375,
122.223611335087)) ;
#48076 = CARTESIAN_POINT('Ctrl Pts',(-19.6673495935004,-38.3195264772746,
121.926560229075)) ;
#48077 = CARTESIAN_POINT('Ctrl Pts',(-19.4049744065646,-38.5095771859549,
122.2058271605)) ;
#48078 = CARTESIAN_POINT('Ctrl Pts',(-19.403909575533,-38.329588105592,121.904328761475)) ;
#48079 = CARTESIAN_POINT('Ctrl Pts',(-19.198843636696,-38.5194218147848,122.224471407226)) ;
#48080 = CARTESIAN_POINT('Ctrl Pts',(-19.1462446840125,-38.3394327344219,
121.927632920062)) ;
#48081 = CARTESIAN_POINT('Ctrl Pts',(-18.9965533130945,-38.5293818623904,
122.278528162173)) ;
#48082 = CARTESIAN_POINT('Ctrl Pts',(-18.8933810810859,-38.3493927820275,
121.99520301882)) ;
#48083 = CARTESIAN_POINT('Ctrl Pts',(-18.8054118271966,-38.5394201685644,
122.367955384898)) ;
#48084 = CARTESIAN_POINT('Ctrl Pts',(-18.6544538829586,-38.3594310882016,
122.106985936773)) ;
#48085 = CARTESIAN_POINT('Ctrl Pts',(-18.63527681131,-38.5492934679971,122.48691582821)) ;
#48086 = CARTESIAN_POINT('Ctrl Pts',(-18.4417836193016,-38.3693043876342,
122.255686315727)) ;
#48087 = CARTESIAN_POINT('Ctrl Pts',(-18.4855083632064,-38.5593667295834,
122.636576989724)) ;
#48088 = CARTESIAN_POINT('Ctrl Pts',(-18.254572634365,-38.3793776492205,122.442761738888)) ;
#48089 = CARTESIAN_POINT('Ctrl Pts',(-18.3667777956026,-38.5691869555401,
122.805528697943)) ;
#48090 = CARTESIAN_POINT('Ctrl Pts',(-18.1061577776451,-38.3891978751772,
122.653952116024)) ;
#48091 = CARTESIAN_POINT('Ctrl Pts',(-18.2767515118799,-38.5792660194796,
122.997287213327)) ;
#48092 = CARTESIAN_POINT('Ctrl Pts',(-17.9936243510384,-38.3992769391167,
122.893649468812)) ;
#48093 = CARTESIAN_POINT('Ctrl Pts',(-18.2225229813274,-38.5891161094994,
123.197198324746)) ;
#48094 = CARTESIAN_POINT('Ctrl Pts',(-17.9258375544917,-38.4091270291365,
123.143539427592)) ;
#48095 = CARTESIAN_POINT('Ctrl Pts',(-18.2032956686347,-38.5991948631132,
123.408157950958)) ;
#48096 = CARTESIAN_POINT('Ctrl Pts',(-17.9018026838566,-38.4192057827503,
123.40723841002)) ;
#48097 = CARTESIAN_POINT('Ctrl Pts',(-18.2203875577578,-38.6090163303726,
123.613973329019)) ;
#48098 = CARTESIAN_POINT('Ctrl Pts',(-17.923166969544,-38.4290272500098,123.664509279081)) ;
#48099 = CARTESIAN_POINT('Ctrl Pts',(-18.2739238887591,-38.6190819287303,
123.818650277656)) ;
#48100 = CARTESIAN_POINT('Ctrl Pts',(-17.9900867207186,-38.4390928483674,
123.920355248471)) ;
#48101 = CARTESIAN_POINT('Ctrl Pts',(-18.3608489444241,-38.628984584505,124.007876019705)) ;
#48102 = CARTESIAN_POINT('Ctrl Pts',(-18.0987428644432,-38.4489955041421,
124.156888509072)) ;
#48103 = CARTESIAN_POINT('Ctrl Pts',(-18.4809742235416,-38.6390354103346,
124.181656276088)) ;
#48104 = CARTESIAN_POINT('Ctrl Pts',(-18.2488988281451,-38.4590463299717,
124.374113939604)) ;
#48105 = CARTESIAN_POINT('Ctrl Pts',(-18.6267574232004,-38.6489096146735,
124.329501799845)) ;
#48106 = CARTESIAN_POINT('Ctrl Pts',(-18.4311282813033,-38.4689205343106,
124.558922029202)) ;
#48107 = CARTESIAN_POINT('Ctrl Pts',(-18.7993133903288,-38.6589820647126,
124.452162400167)) ;
#48108 = CARTESIAN_POINT('Ctrl Pts',(-18.6468226000741,-38.4789929843497,
124.712247945028)) ;
#48109 = CARTESIAN_POINT('Ctrl Pts',(-18.9859137942603,-38.6688110814861,
124.541017706794)) ;
#48110 = CARTESIAN_POINT('Ctrl Pts',(-18.8800743167778,-38.4888220011232,
124.823318123614)) ;
#48111 = CARTESIAN_POINT('Ctrl Pts',(-19.1897774494704,-38.6788779274009,
124.597717051206)) ;
#48112 = CARTESIAN_POINT('Ctrl Pts',(-19.1349034186575,-38.498888847038,124.894192497804)) ;
#48113 = CARTESIAN_POINT('Ctrl Pts',(-19.3967662896624,-38.6887680987027,
124.617671141115)) ;
#48114 = CARTESIAN_POINT('Ctrl Pts',(-19.3936404772055,-38.5087790183398,
124.919135574597)) ;
#48115 = CARTESIAN_POINT('Ctrl Pts',(-19.6062117856198,-38.6987602923265,
124.601677520649)) ;
#48116 = CARTESIAN_POINT('Ctrl Pts',(-19.6554475745632,-38.5187712119636,
124.899143715405)) ;
#48117 = CARTESIAN_POINT('Ctrl Pts',(-19.8090578521169,-38.7087231029499,
124.549518835879)) ;
#48118 = CARTESIAN_POINT('Ctrl Pts',(-19.9090056650285,-38.5287340225871,
124.833945501294)) ;
#48119 = CARTESIAN_POINT('Ctrl Pts',(-19.9988839578665,-38.7186273757934,
124.463912950195)) ;
#48120 = CARTESIAN_POINT('Ctrl Pts',(-20.1462891748571,-38.5386382954305,
124.726937805208)) ;
#48121 = CARTESIAN_POINT('Ctrl Pts',(-20.1735373576463,-38.728687867598,124.344670095455)) ;
#48122 = CARTESIAN_POINT('Ctrl Pts',(-20.3646057034677,-38.5486987872351,
124.577884540204)) ;
#48123 = CARTESIAN_POINT('Ctrl Pts',(-20.3217496628908,-38.7385281992703,
124.200302181168)) ;
#48124 = CARTESIAN_POINT('Ctrl Pts',(-20.549872151261,-38.5585391189074,124.397423633048)) ;
#48125 = CARTESIAN_POINT('Ctrl Pts',(-20.4455536404309,-38.7485912453621,
124.028786981094)) ;
#48126 = CARTESIAN_POINT('Ctrl Pts',(-20.7046268368384,-38.5686021649992,
124.183029887266)) ;
#48127 = CARTESIAN_POINT('Ctrl Pts',(-20.5360148595755,-38.7584853010572,
123.841460701052)) ;
#48128 = CARTESIAN_POINT('Ctrl Pts',(-20.8177037943771,-38.5784962206943,
123.948871113631)) ;
#48129 = CARTESIAN_POINT('Ctrl Pts',(-20.5933924658413,-38.7684280013801,
123.640487605806)) ;
#48130 = CARTESIAN_POINT('Ctrl Pts',(-20.889425745872,-38.5884389210173,123.697654055537)) ;
#48131 = CARTESIAN_POINT('Ctrl Pts',(-20.6151860212168,-38.7784337423077,
123.431245299403)) ;
#48132 = CARTESIAN_POINT('Ctrl Pts',(-20.9166674415414,-38.5984446619449,
123.436101061356)) ;
#48133 = CARTESIAN_POINT('Ctrl Pts',(-20.6000592508299,-38.7884546528233,
123.221122882198)) ;
#48134 = CARTESIAN_POINT('Ctrl Pts',(-20.8977588227754,-38.6084655724604,
123.173448091062)) ;
#48135 = CARTESIAN_POINT('Ctrl Pts',(-20.5495758365941,-38.7983453882732,
123.0194036364)) ;
#48136 = CARTESIAN_POINT('Ctrl Pts',(-20.8346540510326,-38.6183563079104,
122.921298084122)) ;
#48137 = CARTESIAN_POINT('Ctrl Pts',(-20.4642602817029,-38.8083369290021,
122.827465431094)) ;
#48138 = CARTESIAN_POINT('Ctrl Pts',(-20.7280091756525,-38.6283478486392,
122.68137528438)) ;
#48139 = CARTESIAN_POINT('Ctrl Pts',(-20.3473737278901,-38.8182847894237,
122.654045824063)) ;
#48140 = CARTESIAN_POINT('Ctrl Pts',(-20.5819003598894,-38.6382957090609,
122.46460048107)) ;
#48141 = CARTESIAN_POINT('Ctrl Pts',(-20.202456742999,-38.8282314586101,122.503277801019)) ;
#48142 = CARTESIAN_POINT('Ctrl Pts',(-20.400753356158,-38.6482423782472,122.276140396852)) ;
#48143 = CARTESIAN_POINT('Ctrl Pts',(-20.0317199746376,-38.8382795347457,
122.378903058221)) ;
#48144 = CARTESIAN_POINT('Ctrl Pts',(-20.1873323482229,-38.6582904543828,
122.12067245961)) ;
#48145 = CARTESIAN_POINT('Ctrl Pts',(-19.8458354362141,-38.8481271327513,
122.287756233757)) ;
#48146 = CARTESIAN_POINT('Ctrl Pts',(-19.9549752001431,-38.6681380523884,
122.006738756206)) ;
#48147 = CARTESIAN_POINT('Ctrl Pts',(-19.6448376579705,-38.8580888558358,
122.228975330459)) ;
#48148 = CARTESIAN_POINT('Ctrl Pts',(-19.703727329421,-38.6780997754729,121.933263220706)) ;
#48149 = CARTESIAN_POINT('Ctrl Pts',(-19.4352361415482,-38.8681174909188,
122.206096194231)) ;
#48150 = CARTESIAN_POINT('Ctrl Pts',(-19.4417254602095,-38.6881284105559,
121.904664952716)) ;
#48151 = CARTESIAN_POINT('Ctrl Pts',(-19.2273465752442,-38.8780277992368,
122.219725256983)) ;
#48152 = CARTESIAN_POINT('Ctrl Pts',(-19.181862671313,-38.6980387188739,121.921702009282)) ;
#48153 = CARTESIAN_POINT('Ctrl Pts',(-19.0243342885466,-38.8879626963727,
122.26883883605)) ;
#48154 = CARTESIAN_POINT('Ctrl Pts',(-18.9280968782032,-38.7079736160098,
121.98309499747)) ;
#48155 = CARTESIAN_POINT('Ctrl Pts',(-18.8309772013695,-38.8980037793153,
122.353523961238)) ;
#48156 = CARTESIAN_POINT('Ctrl Pts',(-18.6864010149185,-38.7180146989524,
122.088952068271)) ;
#48157 = CARTESIAN_POINT('Ctrl Pts',(-18.6578590680997,-38.9078911221435,
122.468595150492)) ;
#48158 = CARTESIAN_POINT('Ctrl Pts',(-18.4700029594323,-38.7279020417806,
122.232792348805)) ;
#48159 = CARTESIAN_POINT('Ctrl Pts',(-18.5055317513843,-38.9178826370828,
122.613211351364)) ;
#48160 = CARTESIAN_POINT('Ctrl Pts',(-18.2795943518185,-38.73789355672,122.413563464237)) ;
#48161 = CARTESIAN_POINT('Ctrl Pts',(-18.3811911630624,-38.9278340282793,
122.781466926608)) ;
#48162 = CARTESIAN_POINT('Ctrl Pts',(-18.1241690742749,-38.7478449479164,
122.623883939098)) ;
#48163 = CARTESIAN_POINT('Ctrl Pts',(-18.2878097045155,-38.9377665616119,
122.968234846333)) ;
#48164 = CARTESIAN_POINT('Ctrl Pts',(-18.0074429397806,-38.7577774812491,
122.857344924824)) ;
#48165 = CARTESIAN_POINT('Ctrl Pts',(-18.2278106534503,-38.9477637195114,
123.1696520482)) ;
#48166 = CARTESIAN_POINT('Ctrl Pts',(-17.9324451631841,-38.7677746391485,
123.109116894518)) ;
#48167 = CARTESIAN_POINT('Ctrl Pts',(-18.2036416355779,-38.9577487296749,
123.378205341425)) ;
#48168 = CARTESIAN_POINT('Ctrl Pts',(-17.9022350151,-38.777759649312,123.369808873099)) ;
#48169 = CARTESIAN_POINT('Ctrl Pts',(-18.2164291819651,-38.9677915562447,
123.588920968376)) ;
#48170 = CARTESIAN_POINT('Ctrl Pts',(-17.918220476194,-38.7878024758818,123.633203162121)) ;
#48171 = CARTESIAN_POINT('Ctrl Pts',(-18.2641206916243,-38.9776217905496,
123.790038485593)) ;
#48172 = CARTESIAN_POINT('Ctrl Pts',(-17.9778363800637,-38.7976327101868,
123.884601181613)) ;
#48173 = CARTESIAN_POINT('Ctrl Pts',(-18.3479385843405,-38.9876978157843,
123.984532944223)) ;
#48174 = CARTESIAN_POINT('Ctrl Pts',(-18.0826097273411,-38.8077087354214,
124.127718361036)) ;
#48175 = CARTESIAN_POINT('Ctrl Pts',(-18.4616277736015,-38.9975500522752,
124.157720560445)) ;
#48176 = CARTESIAN_POINT('Ctrl Pts',(-18.22472296995,-38.8175609719123,124.344203206639)) ;
#48177 = CARTESIAN_POINT('Ctrl Pts',(-18.6066621317061,-39.0076232587093,
124.31198450881)) ;
#48178 = CARTESIAN_POINT('Ctrl Pts',(-18.4060166292549,-38.8276341783464,
124.537031920896)) ;
#48179 = CARTESIAN_POINT('Ctrl Pts',(-18.7724492303032,-39.0174647682165,
124.435789163625)) ;
#48180 = CARTESIAN_POINT('Ctrl Pts',(-18.6132523458117,-38.8374756878536,
124.691787453132)) ;
#48181 = CARTESIAN_POINT('Ctrl Pts',(-18.9590824114606,-39.0274257149963,
124.530751648875)) ;
#48182 = CARTESIAN_POINT('Ctrl Pts',(-18.8465449135048,-38.8474366346334,
124.810489310294)) ;
#48183 = CARTESIAN_POINT('Ctrl Pts',(-19.1610387527157,-39.0374635437963,
124.591933966622)) ;
#48184 = CARTESIAN_POINT('Ctrl Pts',(-19.0989906357663,-38.8574744634334,
124.886965770252)) ;
#48185 = CARTESIAN_POINT('Ctrl Pts',(-19.3671221533313,-39.0473378535508,
124.617096782991)) ;
#48186 = CARTESIAN_POINT('Ctrl Pts',(-19.3565960865171,-38.8673487731879,
124.918417832295)) ;
#48187 = CARTESIAN_POINT('Ctrl Pts',(-19.5784931233021,-39.0574075512239,
124.605867995762)) ;
#48188 = CARTESIAN_POINT('Ctrl Pts',(-19.620809364879,-38.8774184708611,124.90438027923)) ;
#48189 = CARTESIAN_POINT('Ctrl Pts',(-19.7799321898415,-39.0672410225113,
124.55932535313)) ;
#48190 = CARTESIAN_POINT('Ctrl Pts',(-19.8726090818737,-38.8872519421485,
124.846200103951)) ;
#48191 = CARTESIAN_POINT('Ctrl Pts',(-19.9742453524244,-39.0772706690413,
124.477468158144)) ;
#48192 = CARTESIAN_POINT('Ctrl Pts',(-20.1154997478902,-38.8972815886784,
124.743876964785)) ;
#48193 = CARTESIAN_POINT('Ctrl Pts',(-20.1511369807371,-39.0873051833686,
124.36251502401)) ;
#48194 = CARTESIAN_POINT('Ctrl Pts',(-20.336613329244,-38.9073161030058,124.600184240686)) ;
#48195 = CARTESIAN_POINT('Ctrl Pts',(-20.3025021754356,-39.0971304688395,
124.221961302064)) ;
#48196 = CARTESIAN_POINT('Ctrl Pts',(-20.525819561072,-38.9171413884767,124.424489904963)) ;
#48197 = CARTESIAN_POINT('Ctrl Pts',(-20.4297743163725,-39.1071347103881,
124.05455039433)) ;
#48198 = CARTESIAN_POINT('Ctrl Pts',(-20.684908264894,-38.9271456300252,124.215225042705)) ;
#48199 = CARTESIAN_POINT('Ctrl Pts',(-20.5257881932866,-39.1171173554672,
123.867889590297)) ;
#48200 = CARTESIAN_POINT('Ctrl Pts',(-20.8049240326916,-38.9371282751043,
123.981897983475)) ;
#48201 = CARTESIAN_POINT('Ctrl Pts',(-20.588074926157,-39.1271625525587,123.666125982417)) ;
#48202 = CARTESIAN_POINT('Ctrl Pts',(-20.8827806719574,-38.9471734721958,
123.729693087427)) ;
#48203 = CARTESIAN_POINT('Ctrl Pts',(-20.6141505417572,-39.1369856683188,
123.461258677549)) ;
#48204 = CARTESIAN_POINT('Ctrl Pts',(-20.915373446422,-38.9569965879559,123.473607472964)) ;
#48205 = CARTESIAN_POINT('Ctrl Pts',(-20.60457754197,-39.1470202801191,123.250519610856)) ;
#48206 = CARTESIAN_POINT('Ctrl Pts',(-20.9034051256726,-38.9670311997562,
123.210183840102)) ;
#48207 = CARTESIAN_POINT('Ctrl Pts',(-20.5580262468952,-39.1570452888922,
123.044960994217)) ;
#48208 = CARTESIAN_POINT('Ctrl Pts',(-20.8452141569218,-38.9770562085294,
122.953236014192)) ;
#48209 = CARTESIAN_POINT('Ctrl Pts',(-20.478316885892,-39.1668972137338,122.853791086259)) ;
#48210 = CARTESIAN_POINT('Ctrl Pts',(-20.7455751866615,-38.9869081333709,
122.714273478739)) ;
#48211 = CARTESIAN_POINT('Ctrl Pts',(-20.3653360181163,-39.1768881520565,
122.676754747224)) ;
#48212 = CARTESIAN_POINT('Ctrl Pts',(-20.6043472152323,-38.9968990716936,
122.492979055733)) ;
#48213 = CARTESIAN_POINT('Ctrl Pts',(-20.2244345622947,-39.186806137203,122.523026316099)) ;
#48214 = CARTESIAN_POINT('Ctrl Pts',(-20.4282184151075,-39.0068170568401,
122.300819554238)) ;
#48215 = CARTESIAN_POINT('Ctrl Pts',(-20.0572079878956,-39.1968342380985,
122.394673439318)) ;
#48216 = CARTESIAN_POINT('Ctrl Pts',(-20.2191838999621,-39.0168451577356,
122.140380206335)) ;
#48217 = CARTESIAN_POINT('Ctrl Pts',(-19.8729210552735,-39.2067194790411,
122.298607224345)) ;
#48218 = CARTESIAN_POINT('Ctrl Pts',(-19.988823563365,-39.0267303986782,122.020299045368)) ;
#48219 = CARTESIAN_POINT('Ctrl Pts',(-19.6728247514948,-39.2167085920077,
122.234848345753)) ;
#48220 = CARTESIAN_POINT('Ctrl Pts',(-19.7387023265392,-39.0367195116448,
121.940602617723)) ;
#48221 = CARTESIAN_POINT('Ctrl Pts',(-19.4635439074029,-39.2267506563485,
122.207112896328)) ;
#48222 = CARTESIAN_POINT('Ctrl Pts',(-19.477101074724,-39.0467615759856,121.905935512538)) ;
#48223 = CARTESIAN_POINT('Ctrl Pts',(-19.2570678726038,-39.236579857753,122.215554269047)) ;
#48224 = CARTESIAN_POINT('Ctrl Pts',(-19.2190051557775,-39.0565907773901,
121.91648957557)) ;
#48225 = CARTESIAN_POINT('Ctrl Pts',(-19.0514789396674,-39.2465866985112,
122.260060325551)) ;
#48226 = CARTESIAN_POINT('Ctrl Pts',(-18.96201942726,-39.0665976181483,121.972124528539)) ;
#48227 = CARTESIAN_POINT('Ctrl Pts',(-18.857109213024,-39.2565742227031,122.33957226792)) ;
#48228 = CARTESIAN_POINT('Ctrl Pts',(-18.7190580246925,-39.0765851423402,
122.071516726106)) ;
#48229 = CARTESIAN_POINT('Ctrl Pts',(-18.6788723961599,-39.2666038685117,
122.452193066981)) ;
#48230 = CARTESIAN_POINT('Ctrl Pts',(-18.4962632862226,-39.0866147881488,
122.21229469891)) ;
#48231 = CARTESIAN_POINT('Ctrl Pts',(-18.5251202819395,-39.2764778992504,
122.591691852542)) ;
#48232 = CARTESIAN_POINT('Ctrl Pts',(-18.3040742602747,-39.0964888188876,
122.386670421096)) ;
#48233 = CARTESIAN_POINT('Ctrl Pts',(-18.3961396998256,-39.2864772221145,
122.757647081456)) ;
#48234 = CARTESIAN_POINT('Ctrl Pts',(-18.142850412755,-39.1064881417517,122.594116058602)) ;
#48235 = CARTESIAN_POINT('Ctrl Pts',(-18.2985886975645,-39.2963880576901,
122.941797700532)) ;
#48236 = CARTESIAN_POINT('Ctrl Pts',(-18.0209136491181,-39.1163989773273,
122.824305926561)) ;
#48237 = CARTESIAN_POINT('Ctrl Pts',(-18.2336609868071,-39.3064423056642,
123.142915425112)) ;
#48238 = CARTESIAN_POINT('Ctrl Pts',(-17.939756418586,-39.1264532253013,123.075703741562)) ;
#48239 = CARTESIAN_POINT('Ctrl Pts',(-18.2049530968866,-39.3163010499269,
123.348215710506)) ;
#48240 = CARTESIAN_POINT('Ctrl Pts',(-17.9038739773889,-39.136311969564,123.332330097261)) ;
#48241 = CARTESIAN_POINT('Ctrl Pts',(-18.2123561541688,-39.3263691359999,
123.559718460866)) ;
#48242 = CARTESIAN_POINT('Ctrl Pts',(-17.9131303556298,-39.146380055637,123.596708290308)) ;
#48243 = CARTESIAN_POINT('Ctrl Pts',(-18.2554666856692,-39.3362246191794,
123.762394729141)) ;
#48244 = CARTESIAN_POINT('Ctrl Pts',(-17.9670211523186,-39.1562355388165,
123.850053708663)) ;
#48245 = CARTESIAN_POINT('Ctrl Pts',(-18.333618279946,-39.3462194649736,123.957436253623)) ;
#48246 = CARTESIAN_POINT('Ctrl Pts',(-18.0647131560755,-39.1662303846107,
124.093854715308)) ;
#48247 = CARTESIAN_POINT('Ctrl Pts',(-18.4452442598356,-39.3562507606361,
124.136365747188)) ;
#48248 = CARTESIAN_POINT('Ctrl Pts',(-18.2042478281487,-39.1762616802733,
124.31751521221)) ;
#48249 = CARTESIAN_POINT('Ctrl Pts',(-18.5836826690354,-39.366117303926,124.290842760862)) ;
#48250 = CARTESIAN_POINT('Ctrl Pts',(-18.3772981542013,-39.1861282235631,
124.510610102635)) ;
#48251 = CARTESIAN_POINT('Ctrl Pts',(-18.748604585584,-39.3761046996894,124.420751361441)) ;
#48252 = CARTESIAN_POINT('Ctrl Pts',(-18.5834523133935,-39.1961156193265,
124.672993813445)) ;
#48253 = CARTESIAN_POINT('Ctrl Pts',(-18.9327894876098,-39.3860497404194,
124.519754705833)) ;
#48254 = CARTESIAN_POINT('Ctrl Pts',(-18.8136849281219,-39.2060606600565,
124.796745724654)) ;
#48255 = CARTESIAN_POINT('Ctrl Pts',(-19.1333404381493,-39.3960942466361,
124.585800268565)) ;
#48256 = CARTESIAN_POINT('Ctrl Pts',(-19.0643744385041,-39.2161051662732,
124.879300115833)) ;
#48257 = CARTESIAN_POINT('Ctrl Pts',(-19.3385607919778,-39.4059577527734,
124.615667658985)) ;
#48258 = CARTESIAN_POINT('Ctrl Pts',(-19.3209006976939,-39.2259686724105,
124.916631731165)) ;
#48259 = CARTESIAN_POINT('Ctrl Pts',(-19.5485278972259,-39.4159506136095,
124.609740631774)) ;
#48260 = CARTESIAN_POINT('Ctrl Pts',(-19.5833595972504,-39.2359615332466,
124.909220187151)) ;
#48261 = CARTESIAN_POINT('Ctrl Pts',(-19.7529825851974,-39.4258768073284,
124.567812438431)) ;
#48262 = CARTESIAN_POINT('Ctrl Pts',(-19.838927622203,-39.2458877269655,124.856807196961)) ;
#48263 = CARTESIAN_POINT('Ctrl Pts',(-19.9488284655848,-39.435895733361,124.490360997072)) ;
#48264 = CARTESIAN_POINT('Ctrl Pts',(-20.0837340012441,-39.2559066529981,
124.759990302351)) ;
#48265 = CARTESIAN_POINT('Ctrl Pts',(-20.126540851108,-39.4458107327286,124.381363000925)) ;
#48266 = CARTESIAN_POINT('Ctrl Pts',(-20.3058732169499,-39.2658216523657,
124.623740322462)) ;
#48267 = CARTESIAN_POINT('Ctrl Pts',(-20.2847556242028,-39.4558655042859,
124.241221421377)) ;
#48268 = CARTESIAN_POINT('Ctrl Pts',(-20.5036398438425,-39.275876423923,124.448561261991)) ;
#48269 = CARTESIAN_POINT('Ctrl Pts',(-20.4138101110339,-39.4657244665834,
124.079002697982)) ;
#48270 = CARTESIAN_POINT('Ctrl Pts',(-20.6649559413948,-39.2857353862206,
124.245785908657)) ;
#48271 = CARTESIAN_POINT('Ctrl Pts',(-20.514413173183,-39.4757187104213,123.894581207319)) ;
#48272 = CARTESIAN_POINT('Ctrl Pts',(-20.7907073337683,-39.2957296300584,
124.015257630016)) ;
#48273 = CARTESIAN_POINT('Ctrl Pts',(-20.5811176261202,-39.4856439398455,
123.69683639536)) ;
#48274 = CARTESIAN_POINT('Ctrl Pts',(-20.8740852786362,-39.3056548594826,
123.76807558954)) ;
#48275 = CARTESIAN_POINT('Ctrl Pts',(-20.6127981685667,-39.495671903737,123.488439172828)) ;
#48276 = CARTESIAN_POINT('Ctrl Pts',(-20.9136831801555,-39.3156828233741,
123.507578576389)) ;
#48277 = CARTESIAN_POINT('Ctrl Pts',(-20.6080961840771,-39.5055581633674,
123.280620724186)) ;
#48278 = CARTESIAN_POINT('Ctrl Pts',(-20.9078028794062,-39.3255690830045,
123.247805458002)) ;
#48279 = CARTESIAN_POINT('Ctrl Pts',(-20.5669027528603,-39.5155899264452,
123.073819312021)) ;
#48280 = CARTESIAN_POINT('Ctrl Pts',(-20.8563083055305,-39.3356008460823,
122.989304179214)) ;
#48281 = CARTESIAN_POINT('Ctrl Pts',(-20.4917344516677,-39.5254715527393,
122.880112689592)) ;
#48282 = CARTESIAN_POINT('Ctrl Pts',(-20.7623452754649,-39.3454824723765,
122.747171858518)) ;
#48283 = CARTESIAN_POINT('Ctrl Pts',(-20.3821947597893,-39.5355333222255,
122.69919029706)) ;
#48284 = CARTESIAN_POINT('Ctrl Pts',(-20.6254181998426,-39.3555442418626,
122.521020260046)) ;
#48285 = CARTESIAN_POINT('Ctrl Pts',(-20.2457369593962,-39.545391189721,122.543178844289)) ;
#48286 = CARTESIAN_POINT('Ctrl Pts',(-20.4548438165245,-39.3654021093581,
122.326007790114)) ;
#48287 = CARTESIAN_POINT('Ctrl Pts',(-20.0824035138093,-39.5553828148383,
122.411136991431)) ;
#48288 = CARTESIAN_POINT('Ctrl Pts',(-20.2506752048756,-39.3753937344755,
122.160957633342)) ;
#48289 = CARTESIAN_POINT('Ctrl Pts',(-19.8995811867269,-39.5653196139466,
122.310034299086)) ;
#48290 = CARTESIAN_POINT('Ctrl Pts',(-20.0221459359135,-39.3853305335837,
122.034581725534)) ;
#48291 = CARTESIAN_POINT('Ctrl Pts',(-19.7010155069493,-39.5753104435039,
122.241558693215)) ;
#48292 = CARTESIAN_POINT('Ctrl Pts',(-19.7739378812529,-39.3953213631411,
121.948989845805)) ;
#48293 = CARTESIAN_POINT('Ctrl Pts',(-19.492862253122,-39.5853336792171,122.208735174446)) ;
#48294 = CARTESIAN_POINT('Ctrl Pts',(-19.5137457792809,-39.4053445988542,
121.90796320333)) ;
#48295 = CARTESIAN_POINT('Ctrl Pts',(-19.2848447608836,-39.5952300272463,
122.212328557573)) ;
#48296 = CARTESIAN_POINT('Ctrl Pts',(-19.2537240353539,-39.4152409468834,
121.912457737756)) ;
#48297 = CARTESIAN_POINT('Ctrl Pts',(-19.0785873856562,-39.6052195897488,
122.251922424187)) ;
#48298 = CARTESIAN_POINT('Ctrl Pts',(-18.9959028450578,-39.4252305093859,
121.961952758598)) ;
#48299 = CARTESIAN_POINT('Ctrl Pts',(-18.8815126411,-39.6152598974333,122.327498065648)) ;
#48300 = CARTESIAN_POINT('Ctrl Pts',(-18.7495601440801,-39.4352708170704,
122.056425100597)) ;
#48301 = CARTESIAN_POINT('Ctrl Pts',(-18.7038945149076,-39.6251022007805,
122.433676485987)) ;
#48302 = CARTESIAN_POINT('Ctrl Pts',(-18.5275396488835,-39.4451131204176,
122.189149904879)) ;
#48303 = CARTESIAN_POINT('Ctrl Pts',(-18.5443823308829,-39.6351259090596,
122.571330211097)) ;
#48304 = CARTESIAN_POINT('Ctrl Pts',(-18.3281491908963,-39.4551368286967,
122.361220908179)) ;
#48305 = CARTESIAN_POINT('Ctrl Pts',(-18.3685442000014,-39.6483480865273,
122.786691141863)) ;
#48306 = CARTESIAN_POINT('Ctrl Pts',(-18.1083641388758,-39.4683590061644,
122.630415698339)) ;
#48307 = CARTESIAN_POINT('Ctrl Pts',(-18.2520900531708,-39.6616406715866,
123.044166683935)) ;
#48308 = CARTESIAN_POINT('Ctrl Pts',(-17.9628051141578,-39.4816515912237,
122.952220149241)) ;
#48309 = CARTESIAN_POINT('Ctrl Pts',(-18.2067947635487,-39.6749255275082,
123.319772585123)) ;
#48310 = CARTESIAN_POINT('Ctrl Pts',(-17.9061735340481,-39.4949364471453,
123.296785705772)) ;
#48311 = CARTESIAN_POINT('Ctrl Pts',(-18.2090712913271,-39.684897754681,123.529386284599)) ;
#48312 = CARTESIAN_POINT('Ctrl Pts',(-17.9090249687646,-39.5049086743181,
123.558791097656)) ;
#48313 = CARTESIAN_POINT('Ctrl Pts',(-18.2471189349561,-39.69480637112,123.734216590928)) ;
#48314 = CARTESIAN_POINT('Ctrl Pts',(-17.956586488933,-39.5148172907571,123.814831513861)) ;
#48315 = CARTESIAN_POINT('Ctrl Pts',(-18.3212835409877,-39.7048595765037,
123.932106036806)) ;
#48316 = CARTESIAN_POINT('Ctrl Pts',(-18.0492936761947,-39.5248704961408,
124.062190998726)) ;
#48317 = CARTESIAN_POINT('Ctrl Pts',(-18.4265731448462,-39.714724710264,124.110805164923)) ;
#48318 = CARTESIAN_POINT('Ctrl Pts',(-18.1809125138042,-39.5347356299011,
124.285566478985)) ;
#48319 = CARTESIAN_POINT('Ctrl Pts',(-18.6083337458461,-39.7280637678903,
124.324363825404)) ;
#48320 = CARTESIAN_POINT('Ctrl Pts',(-18.4080910892468,-39.5480746875274,
124.552496993327)) ;
#48321 = CARTESIAN_POINT('Ctrl Pts',(-18.8983167375147,-39.7446329552234,
124.524458458027)) ;
#48322 = CARTESIAN_POINT('Ctrl Pts',(-18.7706176279161,-39.5646438748606,
124.802631868927)) ;
#48323 = CARTESIAN_POINT('Ctrl Pts',(-19.2406669716427,-39.7612780950745,
124.61423815662)) ;
#48324 = CARTESIAN_POINT('Ctrl Pts',(-19.1984775012585,-39.5812890147116,
124.914837427631)) ;
#48325 = CARTESIAN_POINT('Ctrl Pts',(-19.5196867167119,-39.7745503975479,
124.61271922313)) ;
#48326 = CARTESIAN_POINT('Ctrl Pts',(-19.5473160626107,-39.594561317185,124.912945050677)) ;
#48327 = CARTESIAN_POINT('Ctrl Pts',(-19.7261653450185,-39.7845313609955,
124.575425604287)) ;
#48328 = CARTESIAN_POINT('Ctrl Pts',(-19.8054003621908,-39.6045422806326,
124.866324423649)) ;
#48329 = CARTESIAN_POINT('Ctrl Pts',(-19.9223292162796,-39.7944731930648,
124.503237795506)) ;
#48330 = CARTESIAN_POINT('Ctrl Pts',(-20.0506098849888,-39.6144841127019,
124.776085831053)) ;
#48331 = CARTESIAN_POINT('Ctrl Pts',(-20.1643724086472,-39.8077927622802,
124.362474521717)) ;
#48332 = CARTESIAN_POINT('Ctrl Pts',(-20.3531494019142,-39.6278036819174,
124.600140541929)) ;
#48333 = CARTESIAN_POINT('Ctrl Pts',(-20.412637735221,-39.824322917213,124.113575614291)) ;
#48334 = CARTESIAN_POINT('Ctrl Pts',(-20.6634916788334,-39.6443338368501,
124.289002055755)) ;
#48335 = CARTESIAN_POINT('Ctrl Pts',(-20.5921614259415,-39.8443446427051,
123.727677934125)) ;
#48336 = CARTESIAN_POINT('Ctrl Pts',(-20.8878880488286,-39.6643555623422,
123.80663214029)) ;
#48337 = CARTESIAN_POINT('Ctrl Pts',(-20.62909002806,-39.8641560393119,123.307952932077)) ;
#48338 = CARTESIAN_POINT('Ctrl Pts',(-20.9340458411,-39.684166958949,123.281975948021)) ;
#48339 = CARTESIAN_POINT('Ctrl Pts',(-20.5203568846511,-39.8841412880207,
122.897261125277)) ;
#48340 = CARTESIAN_POINT('Ctrl Pts',(-20.7981256340549,-39.7041522076579,
122.768612564933)) ;
#48341 = CARTESIAN_POINT('Ctrl Pts',(-20.2787761694729,-39.9040353506567,
122.549947579521)) ;
#48342 = CARTESIAN_POINT('Ctrl Pts',(-20.4961474222789,-39.7240462702938,
122.334473379802)) ;
#48343 = CARTESIAN_POINT('Ctrl Pts',(-19.9329494436863,-39.9239670298303,
122.304988298998)) ;
#48344 = CARTESIAN_POINT('Ctrl Pts',(-20.0638627446628,-39.7439779494674,
122.028277249774)) ;
#48345 = CARTESIAN_POINT('Ctrl Pts',(-19.5235438881534,-39.9439310843023,
122.192828842814)) ;
#48346 = CARTESIAN_POINT('Ctrl Pts',(-19.552105313075,-39.7639420039394,121.888081012904)) ;
#48347 = CARTESIAN_POINT('Ctrl Pts',(-19.1021579397527,-39.9638119860652,
122.226651373111)) ;
#48348 = CARTESIAN_POINT('Ctrl Pts',(-19.0253744540023,-39.7838229057023,
121.930361827111)) ;
#48349 = CARTESIAN_POINT('Ctrl Pts',(-18.7163649280739,-39.9837506476736,
122.402373200005)) ;
#48350 = CARTESIAN_POINT('Ctrl Pts',(-18.5431348409718,-39.8037615673107,
122.150015941344)) ;
#48351 = CARTESIAN_POINT('Ctrl Pts',(-18.4142773535418,-40.0036471729289,
122.698534548937)) ;
#48352 = CARTESIAN_POINT('Ctrl Pts',(-18.1655278033416,-39.823658092566,122.520218221338)) ;
#48353 = CARTESIAN_POINT('Ctrl Pts',(-18.2307652703842,-40.0235422113832,
123.07969577924)) ;
#48354 = CARTESIAN_POINT('Ctrl Pts',(-17.9361396477719,-39.8435531310203,
122.99666905445)) ;
#48355 = CARTESIAN_POINT('Ctrl Pts',(-18.1882574040753,-40.0435060346893,
123.502015421763)) ;
#48356 = CARTESIAN_POINT('Ctrl Pts',(-17.883006132507,-39.8635169543264,123.524568225147)) ;
#48357 = CARTESIAN_POINT('Ctrl Pts',(-18.29165985598,-40.0633801588183,123.911779372075)) ;
#48358 = CARTESIAN_POINT('Ctrl Pts',(-18.0122595317287,-39.8833910784555,
124.036771136618)) ;
#48359 = CARTESIAN_POINT('Ctrl Pts',(-18.5295568784576,-40.0833552345456,
124.263648018593)) ;
#48360 = CARTESIAN_POINT('Ctrl Pts',(-18.3096308451413,-39.9033661541827,
124.476606505038)) ;
#48361 = CARTESIAN_POINT('Ctrl Pts',(-18.873213806286,-40.1033088039022,124.512438604021)) ;
#48362 = CARTESIAN_POINT('Ctrl Pts',(-18.7392016865621,-39.9233197235393,
124.787593898478)) ;
#48363 = CARTESIAN_POINT('Ctrl Pts',(-19.2785655362842,-40.12314671409,124.629117591118)) ;
#48364 = CARTESIAN_POINT('Ctrl Pts',(-19.245888696071,-39.9431576337272,124.933442271979)) ;
#48365 = CARTESIAN_POINT('Ctrl Pts',(-19.7023551259677,-40.143122542661,124.600718350869)) ;
#48366 = CARTESIAN_POINT('Ctrl Pts',(-19.7756254405552,-39.9631334622981,
124.897944226643)) ;
#48367 = CARTESIAN_POINT('Ctrl Pts',(-20.0896769698093,-40.1630405873712,
124.429488132005)) ;
#48368 = CARTESIAN_POINT('Ctrl Pts',(-20.259776971264,-39.9830515070084,124.68390775287)) ;
#48369 = CARTESIAN_POINT('Ctrl Pts',(-20.3954104326446,-40.1829108331589,
124.137764071626)) ;
#48370 = CARTESIAN_POINT('Ctrl Pts',(-20.6419438140887,-40.002921752796,124.319255201488)) ;
#48371 = CARTESIAN_POINT('Ctrl Pts',(-20.5842765338552,-40.2029598362585,
123.755710496064)) ;
#48372 = CARTESIAN_POINT('Ctrl Pts',(-20.8780281936789,-40.0229707558956,
123.841688417852)) ;
#48373 = CARTESIAN_POINT('Ctrl Pts',(-20.6312875915322,-40.2227390774993,
123.337660256565)) ;
#48374 = CARTESIAN_POINT('Ctrl Pts',(-20.9367938161444,-40.0427499971364,
123.319128562746)) ;
#48375 = CARTESIAN_POINT('Ctrl Pts',(-20.532247620092,-40.2427691412082,122.923541794563)) ;
#48376 = CARTESIAN_POINT('Ctrl Pts',(-20.8129964068986,-40.0627800608453,
122.801479468829)) ;
#48377 = CARTESIAN_POINT('Ctrl Pts',(-20.2989045718909,-40.2626514261102,
122.570943457578)) ;
#48378 = CARTESIAN_POINT('Ctrl Pts',(-20.5213204071413,-40.0826623457473,
122.360731282124)) ;
#48379 = CARTESIAN_POINT('Ctrl Pts',(-19.9600279754679,-40.2825337270031,
122.318257760773)) ;
#48380 = CARTESIAN_POINT('Ctrl Pts',(-20.0977276287473,-40.1025446466403,
122.044872252735)) ;
#48381 = CARTESIAN_POINT('Ctrl Pts',(-19.5531288014987,-40.3025168366215,
122.195882017085)) ;
#48382 = CARTESIAN_POINT('Ctrl Pts',(-19.5891047472004,-40.1225277562586,
121.891899364651)) ;
#48383 = CARTESIAN_POINT('Ctrl Pts',(-19.1308454732642,-40.3224072319994,
122.219647803408)) ;
#48384 = CARTESIAN_POINT('Ctrl Pts',(-19.0612514000338,-40.1424181516365,
121.921603035673)) ;
#48385 = CARTESIAN_POINT('Ctrl Pts',(-18.7417231158238,-40.3423040220336,
122.38552655651)) ;
#48386 = CARTESIAN_POINT('Ctrl Pts',(-18.5748477163413,-40.1623149416708,
122.128947492388)) ;
#48387 = CARTESIAN_POINT('Ctrl Pts',(-18.4318742792953,-40.3622210759752,
122.674244241734)) ;
#48388 = CARTESIAN_POINT('Ctrl Pts',(-18.1875342172556,-40.1822319956124,
122.489841093225)) ;
#48389 = CARTESIAN_POINT('Ctrl Pts',(-18.2384227273083,-40.3822246241788,
123.053097596815)) ;
#48390 = CARTESIAN_POINT('Ctrl Pts',(-17.9457158456868,-40.2022355438159,
122.963405930333)) ;
#48391 = CARTESIAN_POINT('Ctrl Pts',(-18.1866699600762,-40.4021629178314,
123.473848629645)) ;
#48392 = CARTESIAN_POINT('Ctrl Pts',(-17.8810209349113,-40.2221738374685,
123.489343815251)) ;
#48393 = CARTESIAN_POINT('Ctrl Pts',(-18.280049631561,-40.4219844052643,123.884838555175)) ;
#48394 = CARTESIAN_POINT('Ctrl Pts',(-17.9977400537545,-40.2419953249014,
124.003081008329)) ;
#48395 = CARTESIAN_POINT('Ctrl Pts',(-18.5094838644823,-40.4419627982552,
124.242285334387)) ;
#48396 = CARTESIAN_POINT('Ctrl Pts',(-18.2845312148424,-40.2619737178923,
124.449892679348)) ;
#48397 = CARTESIAN_POINT('Ctrl Pts',(-18.8460247213349,-40.4618611798689,
124.498817471921)) ;
#48398 = CARTESIAN_POINT('Ctrl Pts',(-18.7051945465058,-40.281872099506,124.770559205405)) ;
#48399 = CARTESIAN_POINT('Ctrl Pts',(-19.1823032913064,-40.4784441105988,
124.604500943763)) ;
#48400 = CARTESIAN_POINT('Ctrl Pts',(-19.1255703487818,-40.2984550302359,
124.902674539461)) ;
#48401 = CARTESIAN_POINT('Ctrl Pts',(-19.4611720898915,-40.4917183461876,
124.616752614585)) ;
#48402 = CARTESIAN_POINT('Ctrl Pts',(-19.4741295857763,-40.3117292658247,
124.917986772684)) ;
#48403 = CARTESIAN_POINT('Ctrl Pts',(-19.6705355947193,-40.5017647636438,
124.589137634991)) ;
#48404 = CARTESIAN_POINT('Ctrl Pts',(-19.7358425463294,-40.3217756832809,
124.883469686194)) ;
#48405 = CARTESIAN_POINT('Ctrl Pts',(-19.8680131387049,-40.5116099888631,
124.527058907304)) ;
#48406 = CARTESIAN_POINT('Ctrl Pts',(-19.9826774778135,-40.3316209085002,
124.805881778584)) ;
#48407 = CARTESIAN_POINT('Ctrl Pts',(-20.1170123821962,-40.5249449599025,
124.398409715662)) ;
#48408 = CARTESIAN_POINT('Ctrl Pts',(-20.293982933582,-40.3449558795396,124.645032731908)) ;
#48409 = CARTESIAN_POINT('Ctrl Pts',(-20.3777873292751,-40.5415278166951,
124.160882668887)) ;
#48410 = CARTESIAN_POINT('Ctrl Pts',(-20.6198884114383,-40.3615387363322,
124.348182656226)) ;
#48411 = CARTESIAN_POINT('Ctrl Pts',(-20.5424028350229,-40.5581708190445,
123.847768971427)) ;
#48412 = CARTESIAN_POINT('Ctrl Pts',(-20.8256972515988,-40.3781817386816,
123.956743051151)) ;
#48413 = CARTESIAN_POINT('Ctrl Pts',(-20.6040438140094,-40.5714145500762,
123.576158500164)) ;
#48414 = CARTESIAN_POINT('Ctrl Pts',(-20.9027340822747,-40.3914254697133,
123.617264907875)) ;
#48415 = CARTESIAN_POINT('Ctrl Pts',(-20.6143139077877,-40.5814689447508,
123.36507953087)) ;
#48416 = CARTESIAN_POINT('Ctrl Pts',(-20.9155780417739,-40.4014798643879,
123.353409333891)) ;
#48417 = CARTESIAN_POINT('Ctrl Pts',(-20.5885990189638,-40.5913100061393,
123.159754071886)) ;
#48418 = CARTESIAN_POINT('Ctrl Pts',(-20.8834362366564,-40.4113209257765,
123.096754250363)) ;
#48419 = CARTESIAN_POINT('Ctrl Pts',(-20.5264471958815,-40.6013762304958,
122.957500488943)) ;
#48420 = CARTESIAN_POINT('Ctrl Pts',(-20.805749324976,-40.421387150133,122.843935791926)) ;
#48421 = CARTESIAN_POINT('Ctrl Pts',(-20.4318111963384,-40.6112568434155,
122.772550933144)) ;
#48422 = CARTESIAN_POINT('Ctrl Pts',(-20.6874567828035,-40.4312677630526,
122.61274782886)) ;
#48423 = CARTESIAN_POINT('Ctrl Pts',(-20.3054294573994,-40.6212501365751,
122.604767036362)) ;
#48424 = CARTESIAN_POINT('Ctrl Pts',(-20.5294818312083,-40.4412610562122,
122.403016184153)) ;
#48425 = CARTESIAN_POINT('Ctrl Pts',(-20.1524873681173,-40.6312011447987,
122.461975515907)) ;
#48426 = CARTESIAN_POINT('Ctrl Pts',(-20.3383061144584,-40.4512120644359,
122.224524733115)) ;
#48427 = CARTESIAN_POINT('Ctrl Pts',(-19.9753190448652,-40.6412496591607,
122.346959912909)) ;
#48428 = CARTESIAN_POINT('Ctrl Pts',(-20.116847152072,-40.4612605787978,122.080752823443)) ;
#48429 = CARTESIAN_POINT('Ctrl Pts',(-19.7849296325353,-40.6510911652234,
122.265920115438)) ;
#48430 = CARTESIAN_POINT('Ctrl Pts',(-19.8788615309096,-40.4711020848605,
121.979450513905)) ;
#48431 = CARTESIAN_POINT('Ctrl Pts',(-19.5805644894003,-40.6610768178531,
122.218048516374)) ;
#48432 = CARTESIAN_POINT('Ctrl Pts',(-19.623405666514,-40.4810877374902,121.919608247054)) ;
#48433 = CARTESIAN_POINT('Ctrl Pts',(-19.3719102404823,-40.671015826698,122.206359844049)) ;
#48434 = CARTESIAN_POINT('Ctrl Pts',(-19.3625879444289,-40.4910267463351,
121.904994593026)) ;
#48435 = CARTESIAN_POINT('Ctrl Pts',(-19.1623259439942,-40.681056751991,122.231380193141)) ;
#48436 = CARTESIAN_POINT('Ctrl Pts',(-19.1006071741867,-40.5010676716281,
121.936267236992)) ;
#48437 = CARTESIAN_POINT('Ctrl Pts',(-18.9632287027856,-40.6909470737459,
122.291388692216)) ;
#48438 = CARTESIAN_POINT('Ctrl Pts',(-18.8517347176778,-40.510957993383,122.011275192603)) ;
#48439 = CARTESIAN_POINT('Ctrl Pts',(-18.7754842627344,-40.7009430470793,
122.385762996334)) ;
#48440 = CARTESIAN_POINT('Ctrl Pts',(-18.6170528304471,-40.5209539667164,
122.129240595666)) ;
#48441 = CARTESIAN_POINT('Ctrl Pts',(-18.6080361030909,-40.7108744466613,
122.51049410798)) ;
#48442 = CARTESIAN_POINT('Ctrl Pts',(-18.4077408551288,-40.5308853662985,
122.285152304524)) ;
#48443 = CARTESIAN_POINT('Ctrl Pts',(-18.4635012584254,-40.7208799871384,
122.663335115609)) ;
#48444 = CARTESIAN_POINT('Ctrl Pts',(-18.2270702114119,-40.5408909067755,
122.476201697503)) ;
#48445 = CARTESIAN_POINT('Ctrl Pts',(-18.3477150281808,-40.7309129710697,
122.839629729903)) ;
#48446 = CARTESIAN_POINT('Ctrl Pts',(-18.0823350470843,-40.5509238907068,
122.696568451517)) ;
#48447 = CARTESIAN_POINT('Ctrl Pts',(-18.2654267208358,-40.7407686018965,
123.029802709535)) ;
#48448 = CARTESIAN_POINT('Ctrl Pts',(-17.9794720037659,-40.5607795215337,
122.934283776559)) ;
#48449 = CARTESIAN_POINT('Ctrl Pts',(-18.2164553752564,-40.7507680040897,
123.234201010115)) ;
#48450 = CARTESIAN_POINT('Ctrl Pts',(-17.9182550889907,-40.5707789237268,
123.189781090327)) ;
#48451 = CARTESIAN_POINT('Ctrl Pts',(-18.2036080978333,-40.7606624734508,
123.441855570182)) ;
#48452 = CARTESIAN_POINT('Ctrl Pts',(-17.9021932202681,-40.5806733930879,
123.44934937898)) ;
#48453 = CARTESIAN_POINT('Ctrl Pts',(-18.2274647702079,-40.770725587615,123.652027977728)) ;
#48454 = CARTESIAN_POINT('Ctrl Pts',(-17.932011300945,-40.5907365072521,123.712065167649)) ;
#48455 = CARTESIAN_POINT('Ctrl Pts',(-18.2859206509781,-40.7805652333314,
123.85049263691)) ;
#48456 = CARTESIAN_POINT('Ctrl Pts',(-18.0050786320666,-40.6005761529685,
123.960147159055)) ;
#48457 = CARTESIAN_POINT('Ctrl Pts',(-18.3797695061755,-40.7906284008871,
124.040064614096)) ;
#48458 = CARTESIAN_POINT('Ctrl Pts',(-18.122387240134,-40.6106393205242,124.197113300157)) ;
#48459 = CARTESIAN_POINT('Ctrl Pts',(-18.5031774126307,-40.800522656682,124.207538533751)) ;
#48460 = CARTESIAN_POINT('Ctrl Pts',(-18.2766451104993,-40.6205335763191,
124.406457589584)) ;
#48461 = CARTESIAN_POINT('Ctrl Pts',(-18.654084810904,-40.8104644351417,124.352107908462)) ;
#48462 = CARTESIAN_POINT('Ctrl Pts',(-18.4652776966857,-40.6304753547788,
124.587171422744)) ;
#48463 = CARTESIAN_POINT('Ctrl Pts',(-18.828869034011,-40.8204671279719,124.469083088964)) ;
#48464 = CARTESIAN_POINT('Ctrl Pts',(-18.6837565652639,-40.640478047609,124.733392656185)) ;
#48465 = CARTESIAN_POINT('Ctrl Pts',(-19.0220064357381,-40.8305011499257,
124.553889575478)) ;
#48466 = CARTESIAN_POINT('Ctrl Pts',(-18.9251772147638,-40.6505120695628,
124.839403238279)) ;
#48467 = CARTESIAN_POINT('Ctrl Pts',(-19.223072436617,-40.8403489410147,124.603257935098)) ;
#48468 = CARTESIAN_POINT('Ctrl Pts',(-19.176509623626,-40.6603598606518,124.901116406676)) ;
#48469 = CARTESIAN_POINT('Ctrl Pts',(-19.4324060765276,-40.8503304655638,
124.617611036992)) ;
#48470 = CARTESIAN_POINT('Ctrl Pts',(-19.4381766703649,-40.6703413852009,
124.919060383607)) ;
#48471 = CARTESIAN_POINT('Ctrl Pts',(-19.6403984022838,-40.8602796890547,
124.595436731621)) ;
#48472 = CARTESIAN_POINT('Ctrl Pts',(-19.6981676204706,-40.6802906086918,
124.891345054652)) ;
#48473 = CARTESIAN_POINT('Ctrl Pts',(-19.842443083507,-40.8702773452713,124.537454340177)) ;
#48474 = CARTESIAN_POINT('Ctrl Pts',(-19.9507242764533,-40.6902882649084,
124.818869487459)) ;
#48475 = CARTESIAN_POINT('Ctrl Pts',(-20.0319489132289,-40.8803175583263,
124.444528163005)) ;
#48476 = CARTESIAN_POINT('Ctrl Pts',(-20.1876076661773,-40.7003284779634,
124.702714148648)) ;
#48477 = CARTESIAN_POINT('Ctrl Pts',(-20.1991246682804,-40.8901456056026,
124.323088911922)) ;
#48478 = CARTESIAN_POINT('Ctrl Pts',(-20.39657947432,-40.7101565252397,124.550916691026)) ;
#48479 = CARTESIAN_POINT('Ctrl Pts',(-20.346201088897,-40.9001999526349,124.171290921794)) ;
#48480 = CARTESIAN_POINT('Ctrl Pts',(-20.5804267072164,-40.7202108722721,
124.361171005036)) ;
#48481 = CARTESIAN_POINT('Ctrl Pts',(-20.4630696212735,-40.9101410889635,
123.998019997422)) ;
#48482 = CARTESIAN_POINT('Ctrl Pts',(-20.7265146724235,-40.7301520086006,
124.144583500037)) ;
#48483 = CARTESIAN_POINT('Ctrl Pts',(-20.5483504789561,-40.9200453220432,
123.808062649806)) ;
#48484 = CARTESIAN_POINT('Ctrl Pts',(-20.833118168353,-40.7400562416803,123.907137322024)) ;
#48485 = CARTESIAN_POINT('Ctrl Pts',(-20.5999532572044,-40.9300920188868,
123.60326863494)) ;
#48486 = CARTESIAN_POINT('Ctrl Pts',(-20.8976239886845,-40.7501029385239,
123.651145500443)) ;
#48487 = CARTESIAN_POINT('Ctrl Pts',(-20.6151760608575,-40.9399875701671,
123.395757075014)) ;
#48488 = CARTESIAN_POINT('Ctrl Pts',(-20.9166549329738,-40.7599984898042,
123.391755647878)) ;
#48489 = CARTESIAN_POINT('Ctrl Pts',(-20.5937893271631,-40.9500496480066,
123.185334655096)) ;
#48490 = CARTESIAN_POINT('Ctrl Pts',(-20.8899239295474,-40.7700605676437,
123.128727559493)) ;
#48491 = CARTESIAN_POINT('Ctrl Pts',(-20.5375466139094,-40.9598923571026,
122.986176025129)) ;
#48492 = CARTESIAN_POINT('Ctrl Pts',(-20.8196225925667,-40.7799032767398,
122.879777795718)) ;
#48493 = CARTESIAN_POINT('Ctrl Pts',(-20.4466945331734,-40.9698830893411,
122.796834964654)) ;
#48494 = CARTESIAN_POINT('Ctrl Pts',(-20.7060594583057,-40.7898940089782,
122.643100332516)) ;
#48495 = CARTESIAN_POINT('Ctrl Pts',(-20.32506530426,-40.9798111145698,122.627205149371)) ;
#48496 = CARTESIAN_POINT('Ctrl Pts',(-20.554024482547,-40.799822034207,122.43106134549)) ;
#48497 = CARTESIAN_POINT('Ctrl Pts',(-20.1751809243749,-40.9897992612204,
122.480136248305)) ;
#48498 = CARTESIAN_POINT('Ctrl Pts',(-20.3666704074435,-40.8098101808575,
122.247223536498)) ;
#48499 = CARTESIAN_POINT('Ctrl Pts',(-20.0010440003547,-40.9998342790604,
122.361035774299)) ;
#48500 = CARTESIAN_POINT('Ctrl Pts',(-20.1490005900659,-40.8198451986975,
122.098346117619)) ;
#48501 = CARTESIAN_POINT('Ctrl Pts',(-19.8122322682539,-41.0096990761655,
122.275263236687)) ;
#48502 = CARTESIAN_POINT('Ctrl Pts',(-19.9129860527782,-40.8297099958027,
121.991128079681)) ;
#48503 = CARTESIAN_POINT('Ctrl Pts',(-19.6095835568502,-41.0196598085217,
122.222477105135)) ;
#48504 = CARTESIAN_POINT('Ctrl Pts',(-19.6596753422036,-40.8396707281588,
121.925143350382)) ;
#48505 = CARTESIAN_POINT('Ctrl Pts',(-19.3993089283046,-41.0296932709187,
122.205909546878)) ;
#48506 = CARTESIAN_POINT('Ctrl Pts',(-19.3968323127543,-40.8497041905558,
121.904431778563)) ;
#48507 = CARTESIAN_POINT('Ctrl Pts',(-19.1923814571992,-41.0395788051301,
122.225463175371)) ;
#48508 = CARTESIAN_POINT('Ctrl Pts',(-19.1381719931737,-40.8595897247672,
121.928871855677)) ;
#48509 = CARTESIAN_POINT('Ctrl Pts',(-18.9884081997025,-41.0496436458101,
122.281644422525)) ;
#48510 = CARTESIAN_POINT('Ctrl Pts',(-18.8832051234913,-40.8696545654472,
121.999096373019)) ;
#48511 = CARTESIAN_POINT('Ctrl Pts',(-18.8013257411855,-41.0594917775389,
122.370368828685)) ;
#48512 = CARTESIAN_POINT('Ctrl Pts',(-18.6493502439054,-40.8795026971761,
122.110000505807)) ;
#48513 = CARTESIAN_POINT('Ctrl Pts',(-18.6291184084903,-41.0695192745291,
122.491953508965)) ;
#48514 = CARTESIAN_POINT('Ctrl Pts',(-18.4340900376583,-40.8895301941662,
122.261979815528)) ;
#48515 = CARTESIAN_POINT('Ctrl Pts',(-18.4810087173521,-41.0795477265741,
122.642011387807)) ;
#48516 = CARTESIAN_POINT('Ctrl Pts',(-18.2489515312442,-40.8995586462113,
122.449550693022)) ;
#48517 = CARTESIAN_POINT('Ctrl Pts',(-18.3630810655382,-41.0893929931382,
122.812094313911)) ;
#48518 = CARTESIAN_POINT('Ctrl Pts',(-18.1015397641077,-40.9094039127754,
122.662154181766)) ;
#48519 = CARTESIAN_POINT('Ctrl Pts',(-18.2746791888148,-41.0993836660792,
123.00262605961)) ;
#48520 = CARTESIAN_POINT('Ctrl Pts',(-17.9910357650172,-40.9193945857163,
122.900318312532)) ;
#48521 = CARTESIAN_POINT('Ctrl Pts',(-18.2209040134384,-41.1094215481676,
123.206685229747)) ;
#48522 = CARTESIAN_POINT('Ctrl Pts',(-17.9238150126673,-40.9294324678048,
123.155391668012)) ;
#48523 = CARTESIAN_POINT('Ctrl Pts',(-18.2033541254263,-41.1192659186073,
123.412907134102)) ;
#48524 = CARTESIAN_POINT('Ctrl Pts',(-17.9018757959936,-40.9392768382444,
123.413170064838)) ;
#48525 = CARTESIAN_POINT('Ctrl Pts',(-18.2217257491831,-41.1292507460027,
123.621985540264)) ;
#48526 = CARTESIAN_POINT('Ctrl Pts',(-17.9248387222201,-40.9492616656398,
123.674518463669)) ;
#48527 = CARTESIAN_POINT('Ctrl Pts',(-18.2757990112521,-41.139190191408,123.82385763404)) ;
#48528 = CARTESIAN_POINT('Ctrl Pts',(-17.9924288980122,-40.9592011110451,
123.926859519996)) ;
#48529 = CARTESIAN_POINT('Ctrl Pts',(-18.3650287174585,-41.1492301956939,
124.01511881118)) ;
#48530 = CARTESIAN_POINT('Ctrl Pts',(-18.1039644977268,-40.969241115331,124.165936540769)) ;
#48531 = CARTESIAN_POINT('Ctrl Pts',(-18.4841771963513,-41.1591173048795,
124.18546666406)) ;
#48532 = CARTESIAN_POINT('Ctrl Pts',(-18.2528993475112,-40.9791282245166,
124.378873025714)) ;
#48533 = CARTESIAN_POINT('Ctrl Pts',(-18.6325483512414,-41.169117364782,124.334363428523)) ;
#48534 = CARTESIAN_POINT('Ctrl Pts',(-18.4383623409919,-40.9891282844191,
124.564995129704)) ;
#48535 = CARTESIAN_POINT('Ctrl Pts',(-18.8030499054225,-41.1790347806967,
124.45442108235)) ;
#48536 = CARTESIAN_POINT('Ctrl Pts',(-18.6514890497464,-40.9990457003338,
124.715068772833)) ;
#48537 = CARTESIAN_POINT('Ctrl Pts',(-18.9942377867766,-41.1890815954375,
124.544124964319)) ;
#48538 = CARTESIAN_POINT('Ctrl Pts',(-18.8904730960395,-41.0090925150746,
124.827199842309)) ;
#48539 = CARTESIAN_POINT('Ctrl Pts',(-19.194625243992,-41.1989570726341,124.59855210773)) ;
#48540 = CARTESIAN_POINT('Ctrl Pts',(-19.1409580665125,-41.0189679922713,
124.895235368087)) ;
#48541 = CARTESIAN_POINT('Ctrl Pts',(-19.4051209957553,-41.2090131683554,
124.617812738333)) ;
#48542 = CARTESIAN_POINT('Ctrl Pts',(-19.4040773768789,-41.0290240879925,
124.919312459321)) ;
#48543 = CARTESIAN_POINT('Ctrl Pts',(-19.612431639119,-41.2189063303704,124.600588284095)) ;
#48544 = CARTESIAN_POINT('Ctrl Pts',(-19.6632167072632,-41.0389172500076,
124.897783110469)) ;
#48545 = CARTESIAN_POINT('Ctrl Pts',(-19.8169921171162,-41.228968566393,124.546802146257)) ;
#48546 = CARTESIAN_POINT('Ctrl Pts',(-19.918917313857,-41.0489794860302,124.830551760871)) ;
#48547 = CARTESIAN_POINT('Ctrl Pts',(-20.0049876675589,-41.238813032022,124.460234593198)) ;
#48548 = CARTESIAN_POINT('Ctrl Pts',(-20.1539134835327,-41.0588239516591,
124.722342924619)) ;
#48549 = CARTESIAN_POINT('Ctrl Pts',(-20.1775149384373,-41.2487731247261,
124.341583226709)) ;
#48550 = CARTESIAN_POINT('Ctrl Pts',(-20.3695735130956,-41.0687840443633,
124.574029278927)) ;
#48551 = CARTESIAN_POINT('Ctrl Pts',(-20.3276957983037,-41.2588114137072,
124.193333688779)) ;
#48552 = CARTESIAN_POINT('Ctrl Pts',(-20.5573002807056,-41.0788223333443,
124.388718288801)) ;
#48553 = CARTESIAN_POINT('Ctrl Pts',(-20.4481963084003,-41.2686847368134,
124.024285690543)) ;
#48554 = CARTESIAN_POINT('Ctrl Pts',(-20.7079273846869,-41.0886956564505,
124.177407956231)) ;
#48555 = CARTESIAN_POINT('Ctrl Pts',(-20.5392295552627,-41.2787579208985,
123.833127087447)) ;
#48556 = CARTESIAN_POINT('Ctrl Pts',(-20.8217196875643,-41.0987688405356,
123.938460528923)) ;
#48557 = CARTESIAN_POINT('Ctrl Pts',(-20.5945544507421,-41.2885784331864,
123.634173535179)) ;
#48558 = CARTESIAN_POINT('Ctrl Pts',(-20.8908771120928,-41.1085893528235,
123.689767340494)) ;
#48559 = CARTESIAN_POINT('Ctrl Pts',(-20.6152109322945,-41.2986564293022,
123.4233616068)) ;
#48560 = CARTESIAN_POINT('Ctrl Pts',(-20.9166985130199,-41.1186673489393,
123.426252975594)) ;
#48561 = CARTESIAN_POINT('Ctrl Pts',(-20.5993528249516,-41.3085105042855,
123.216758416183)) ;
#48562 = CARTESIAN_POINT('Ctrl Pts',(-20.8968766070843,-41.1285214239226,
123.167997632845)) ;
#48563 = CARTESIAN_POINT('Ctrl Pts',(-20.5470119355056,-41.3185743858692,
123.011801977239)) ;
#48564 = CARTESIAN_POINT('Ctrl Pts',(-20.8314512990001,-41.1385853055063,
122.911802236426)) ;
#48565 = CARTESIAN_POINT('Ctrl Pts',(-20.4613754347014,-41.3284578118429,
122.822450585418)) ;
#48566 = CARTESIAN_POINT('Ctrl Pts',(-20.7244059189189,-41.14846873148,122.675111707094)) ;
#48567 = CARTESIAN_POINT('Ctrl Pts',(-20.3430903346169,-41.338458415764,122.648681232655)) ;
#48568 = CARTESIAN_POINT('Ctrl Pts',(-20.5765499860383,-41.1584693354011,
122.457899543958)) ;
#48569 = CARTESIAN_POINT('Ctrl Pts',(-20.1976579653882,-41.3483782001018,
122.49916106268)) ;
#48570 = CARTESIAN_POINT('Ctrl Pts',(-20.3947593959915,-41.168389119739,122.270998373932)) ;
#48571 = CARTESIAN_POINT('Ctrl Pts',(-20.0263274877781,-41.3584255504587,
122.375678234952)) ;
#48572 = CARTESIAN_POINT('Ctrl Pts',(-20.1805968421938,-41.1784364700958,
122.116644490037)) ;
#48573 = CARTESIAN_POINT('Ctrl Pts',(-19.8394159318229,-41.368302892693,122.285119868391)) ;
#48574 = CARTESIAN_POINT('Ctrl Pts',(-19.9469565780985,-41.1883138123301,
122.003445575771)) ;
#48575 = CARTESIAN_POINT('Ctrl Pts',(-19.6358016808575,-41.3783727737676,
122.227321629888)) ;
#48576 = CARTESIAN_POINT('Ctrl Pts',(-19.6924393110652,-41.1983836934047,
121.931197405337)) ;
#48577 = CARTESIAN_POINT('Ctrl Pts',(-19.4302105986271,-41.3882024789693,
122.206046078144)) ;
#48578 = CARTESIAN_POINT('Ctrl Pts',(-19.4354489668085,-41.2082133986064,
121.904602386854)) ;
#48579 = CARTESIAN_POINT('Ctrl Pts',(-19.2191313622272,-41.3982691401357,
122.220859081126)) ;
#48580 = CARTESIAN_POINT('Ctrl Pts',(-19.1716002965813,-41.2182800597728,
121.923118301563)) ;
#48581 = CARTESIAN_POINT('Ctrl Pts',(-19.0174028500584,-41.408159362003,122.271341345919)) ;
#48582 = CARTESIAN_POINT('Ctrl Pts',(-18.9194385507973,-41.2281702816401,
121.986221032481)) ;
#48583 = CARTESIAN_POINT('Ctrl Pts',(-18.8253933440022,-41.4181515381132,
122.356520476582)) ;
#48584 = CARTESIAN_POINT('Ctrl Pts',(-18.6794263982386,-41.2381624577503,
122.092694865169)) ;
#48585 = CARTESIAN_POINT('Ctrl Pts',(-18.6517079385557,-41.4281143682258,
122.473569637497)) ;
#48586 = CARTESIAN_POINT('Ctrl Pts',(-18.462319115849,-41.2481252878629,122.239006352315)) ;
#48587 = CARTESIAN_POINT('Ctrl Pts',(-18.5014870756419,-41.4380185806261,
122.61777683837)) ;
#48588 = CARTESIAN_POINT('Ctrl Pts',(-18.2745423237503,-41.2580295002633,
122.419265967195)) ;
#48589 = CARTESIAN_POINT('Ctrl Pts',(-18.3768239906411,-41.448079294714,122.788607618059)) ;
#48590 = CARTESIAN_POINT('Ctrl Pts',(-18.1187135739592,-41.2680902143511,
122.632804079682)) ;
#48591 = CARTESIAN_POINT('Ctrl Pts',(-18.2854831726733,-41.4579187976968,
122.974241715456)) ;
#48592 = CARTESIAN_POINT('Ctrl Pts',(-18.0045368875343,-41.2779297173339,
122.864848022296)) ;
#48593 = CARTESIAN_POINT('Ctrl Pts',(-18.2262434983332,-41.4679849362632,
123.177367766874)) ;
#48594 = CARTESIAN_POINT('Ctrl Pts',(-17.9304874746578,-41.2879958559003,
123.11875522056)) ;
#48595 = CARTESIAN_POINT('Ctrl Pts',(-18.2036641637308,-41.4778674507492,
123.383929826508)) ;
#48596 = CARTESIAN_POINT('Ctrl Pts',(-17.902263224335,-41.2978783703863,123.376958924445)) ;
#48597 = CARTESIAN_POINT('Ctrl Pts',(-18.217028771755,-41.4878597501047,123.593541694944)) ;
#48598 = CARTESIAN_POINT('Ctrl Pts',(-17.9189692034043,-41.3078706697419,
123.638973965491)) ;
#48599 = CARTESIAN_POINT('Ctrl Pts',(-18.266354986361,-41.4978128170581,123.796921608966)) ;
#48600 = CARTESIAN_POINT('Ctrl Pts',(-17.9806273077311,-41.3178237366953,
123.893199304568)) ;
#48601 = CARTESIAN_POINT('Ctrl Pts',(-18.3509953062756,-41.5078475252634,
123.990141633652)) ;
#48602 = CARTESIAN_POINT('Ctrl Pts',(-18.0864278200169,-41.3278584449005,
124.134724121174)) ;
#48603 = CARTESIAN_POINT('Ctrl Pts',(-18.4660813786671,-41.5177357461675,
124.16327447273)) ;
#48604 = CARTESIAN_POINT('Ctrl Pts',(-18.2302862077972,-41.3377466658047,
124.351140926558)) ;
#48605 = CARTESIAN_POINT('Ctrl Pts',(-18.6107545882689,-41.527730169198,124.315632016027)) ;
#48606 = CARTESIAN_POINT('Ctrl Pts',(-18.411128140004,-41.3477410888351,124.541587743708)) ;
#48607 = CARTESIAN_POINT('Ctrl Pts',(-18.7789136987431,-41.5376755086441,
124.439882085286)) ;
#48608 = CARTESIAN_POINT('Ctrl Pts',(-18.6213277144287,-41.3576864282813,
124.696900401289)) ;
#48609 = CARTESIAN_POINT('Ctrl Pts',(-18.9659468148119,-41.5476228532555,
124.533455179256)) ;
#48610 = CARTESIAN_POINT('Ctrl Pts',(-18.8551198560532,-41.3676337728926,
124.813866561764)) ;
#48611 = CARTESIAN_POINT('Ctrl Pts',(-19.1684641307119,-41.5576707486665,
124.593501263556)) ;
#48612 = CARTESIAN_POINT('Ctrl Pts',(-19.1082663812488,-41.3776816683036,
124.888923688486)) ;
#48613 = CARTESIAN_POINT('Ctrl Pts',(-19.3741360186057,-41.5675183941458,
124.617169452633)) ;
#48614 = CARTESIAN_POINT('Ctrl Pts',(-19.3653576889217,-41.387529313783,124.918508593892)) ;
#48615 = CARTESIAN_POINT('Ctrl Pts',(-19.5832145971549,-41.5774801080598,
124.605278842965)) ;
#48616 = CARTESIAN_POINT('Ctrl Pts',(-19.6267063239456,-41.397491027697,124.903644555584)) ;
#48617 = CARTESIAN_POINT('Ctrl Pts',(-19.788383314369,-41.5875087323508,124.556678207782)) ;
#48618 = CARTESIAN_POINT('Ctrl Pts',(-19.8831669773239,-41.4075196519879,
124.842893155659)) ;
#48619 = CARTESIAN_POINT('Ctrl Pts',(-19.979718451431,-41.5974190930075,124.47424697805)) ;
#48620 = CARTESIAN_POINT('Ctrl Pts',(-20.1223364379903,-41.4174300126446,
124.739853154527)) ;
#48621 = CARTESIAN_POINT('Ctrl Pts',(-20.1545793968166,-41.6073537915808,
124.360016047797)) ;
#48622 = CARTESIAN_POINT('Ctrl Pts',(-20.3409126898904,-41.4273647112179,
124.597063389142)) ;
#48623 = CARTESIAN_POINT('Ctrl Pts',(-20.3084369890171,-41.617395616435,124.215477929178)) ;
#48624 = CARTESIAN_POINT('Ctrl Pts',(-20.5332339905114,-41.4374065360721,
124.416390285309)) ;
#48625 = CARTESIAN_POINT('Ctrl Pts',(-20.4330452256544,-41.6272801901794,
124.04915416565)) ;
#48626 = CARTESIAN_POINT('Ctrl Pts',(-20.6889942202741,-41.4472911098165,
124.208484214558)) ;
#48627 = CARTESIAN_POINT('Ctrl Pts',(-20.5281974762761,-41.6372820395426,
123.861676921121)) ;
#48628 = CARTESIAN_POINT('Ctrl Pts',(-20.8079337346372,-41.4572929591797,
123.974137087454)) ;
#48629 = CARTESIAN_POINT('Ctrl Pts',(-20.5890105169507,-41.6472013411166,
123.662177464747)) ;
#48630 = CARTESIAN_POINT('Ctrl Pts',(-20.8839492756787,-41.4672122607537,
123.724761737193)) ;
#48631 = CARTESIAN_POINT('Ctrl Pts',(-20.6145770333962,-41.6572454494619,
123.452589429869)) ;
#48632 = CARTESIAN_POINT('Ctrl Pts',(-20.9159063783837,-41.477256369099,123.462776779803)) ;
#48633 = CARTESIAN_POINT('Ctrl Pts',(-20.6036034057865,-41.6671298729041,
123.245068543956)) ;
#48634 = CARTESIAN_POINT('Ctrl Pts',(-20.9021882404978,-41.4871407925413,
123.203374700093)) ;
#48635 = CARTESIAN_POINT('Ctrl Pts',(-20.5565952979151,-41.6771462348136,
123.039799079144)) ;
#48636 = CARTESIAN_POINT('Ctrl Pts',(-20.8434269167983,-41.4971571544507,
122.946788139686)) ;
#48637 = CARTESIAN_POINT('Ctrl Pts',(-20.4739898693975,-41.687182890319,122.845651147378)) ;
#48638 = CARTESIAN_POINT('Ctrl Pts',(-20.740169246239,-41.5071938099561,122.704103736706)) ;
#48639 = CARTESIAN_POINT('Ctrl Pts',(-20.3617495143391,-41.6970130205083,
122.672097956593)) ;
#48640 = CARTESIAN_POINT('Ctrl Pts',(-20.5998669968465,-41.5170239401454,
122.487161714525)) ;
#48641 = CARTESIAN_POINT('Ctrl Pts',(-20.2176578236803,-41.7070890735982,
122.516880089597)) ;
#48642 = CARTESIAN_POINT('Ctrl Pts',(-20.4197517580595,-41.5270999932353,
122.293140547087)) ;
#48643 = CARTESIAN_POINT('Ctrl Pts',(-20.0525570282774,-41.716941302784,122.391738375316)) ;
#48644 = CARTESIAN_POINT('Ctrl Pts',(-20.2133740001492,-41.5369522224211,
122.136713686681)) ;
#48645 = CARTESIAN_POINT('Ctrl Pts',(-19.864251762106,-41.7270145105833,122.294921019345)) ;
#48646 = CARTESIAN_POINT('Ctrl Pts',(-19.9779921555952,-41.5470254302204,
122.015693380369)) ;
#48647 = CARTESIAN_POINT('Ctrl Pts',(-19.666587072999,-41.7368560219347,122.233752490588)) ;
#48648 = CARTESIAN_POINT('Ctrl Pts',(-19.7309096530658,-41.5568669415718,
121.939233606283)) ;
#48649 = CARTESIAN_POINT('Ctrl Pts',(-19.458933216277,-41.7468169599722,122.206739976442)) ;
#48650 = CARTESIAN_POINT('Ctrl Pts',(-19.4713417220652,-41.5668278796093,
121.905469506213)) ;
#48651 = CARTESIAN_POINT('Ctrl Pts',(-19.2481470392033,-41.7568548218972,
122.21668888155)) ;
#48652 = CARTESIAN_POINT('Ctrl Pts',(-19.2078592032353,-41.5768657415343,
121.917907090772)) ;
#48653 = CARTESIAN_POINT('Ctrl Pts',(-19.0455303660746,-41.7667290078943,
122.261958044375)) ;
#48654 = CARTESIAN_POINT('Ctrl Pts',(-18.9545877190135,-41.5867399275314,
121.974495320736)) ;
#48655 = CARTESIAN_POINT('Ctrl Pts',(-18.8501065214671,-41.7767991674721,
122.343300097971)) ;
#48656 = CARTESIAN_POINT('Ctrl Pts',(-18.7103088483806,-41.5968100871093,
122.076174219164)) ;
#48657 = CARTESIAN_POINT('Ctrl Pts',(-18.675884913286,-41.786630914898,122.454554501871)) ;
#48658 = CARTESIAN_POINT('Ctrl Pts',(-18.4925316287136,-41.6066418345351,
122.215244290512)) ;
#48659 = CARTESIAN_POINT('Ctrl Pts',(-18.5201147053539,-41.7966669949693,
122.596849719958)) ;
#48660 = CARTESIAN_POINT('Ctrl Pts',(-18.2978201733905,-41.6166779146064,
122.393114575387)) ;
#48661 = CARTESIAN_POINT('Ctrl Pts',(-18.3920704361308,-41.8066840418218,
122.764054383414)) ;
#48662 = CARTESIAN_POINT('Ctrl Pts',(-18.1377661291796,-41.6266949614589,
122.602121409424)) ;
#48663 = CARTESIAN_POINT('Ctrl Pts',(-18.2959657375201,-41.8165662999884,
122.948249336601)) ;
#48664 = CARTESIAN_POINT('Ctrl Pts',(-18.0176363964437,-41.6365772196255,
122.832366722384)) ;
#48665 = CARTESIAN_POINT('Ctrl Pts',(-18.2324121268901,-41.8265539827847,
123.148349956058)) ;
#48666 = CARTESIAN_POINT('Ctrl Pts',(-17.9381960769655,-41.6465649024218,
123.082493245792)) ;
#48667 = CARTESIAN_POINT('Ctrl Pts',(-18.2045073332423,-41.8365006395015,
123.355622216733)) ;
#48668 = CARTESIAN_POINT('Ctrl Pts',(-17.9033168942799,-41.6565115591386,
123.341584277109)) ;
#48669 = CARTESIAN_POINT('Ctrl Pts',(-18.2133253026657,-41.8465576975816,
123.566846105413)) ;
#48670 = CARTESIAN_POINT('Ctrl Pts',(-17.9143411683041,-41.6665686172188,
123.605613842751)) ;
#48671 = CARTESIAN_POINT('Ctrl Pts',(-18.2573346938639,-41.8563758771311,
123.768519750159)) ;
#48672 = CARTESIAN_POINT('Ctrl Pts',(-17.969355045573,-41.6763867967682,123.857706729659)) ;
#48673 = CARTESIAN_POINT('Ctrl Pts',(-18.3368951497359,-41.86641181157,123.963925455045)) ;
#48674 = CARTESIAN_POINT('Ctrl Pts',(-18.0688075005491,-41.6864227312072,
124.101962973962)) ;
#48675 = CARTESIAN_POINT('Ctrl Pts',(-18.449568449613,-41.876436465999,124.142036436665)) ;
#48676 = CARTESIAN_POINT('Ctrl Pts',(-18.2096507194806,-41.6964473856362,
124.324600663781)) ;
#48677 = CARTESIAN_POINT('Ctrl Pts',(-18.5886702041934,-41.8862884855786,
124.295499146271)) ;
#48678 = CARTESIAN_POINT('Ctrl Pts',(-18.3835301012507,-41.7062994052157,
124.51642843277)) ;
#48679 = CARTESIAN_POINT('Ctrl Pts',(-18.7543933359487,-41.8962793992935,
124.424504024787)) ;
#48680 = CARTESIAN_POINT('Ctrl Pts',(-18.5906854588075,-41.7162903189306,
124.677682956406)) ;
#48681 = CARTESIAN_POINT('Ctrl Pts',(-18.9386244083252,-41.9061973881331,
124.522200361594)) ;
#48682 = CARTESIAN_POINT('Ctrl Pts',(-18.8209758181354,-41.7262083077702,
124.799801736939)) ;
#48683 = CARTESIAN_POINT('Ctrl Pts',(-19.1391682617768,-41.9162254988639,
124.587172771734)) ;
#48684 = CARTESIAN_POINT('Ctrl Pts',(-19.0716562721303,-41.736236418501,124.88101516819)) ;
#48685 = CARTESIAN_POINT('Ctrl Pts',(-19.3449799514909,-41.9261106967723,
124.616011040742)) ;
#48686 = CARTESIAN_POINT('Ctrl Pts',(-19.3289219205496,-41.7461216164094,
124.917060930178)) ;
#48687 = CARTESIAN_POINT('Ctrl Pts',(-19.554878431118,-41.9360999720403,124.609111482474)) ;
#48688 = CARTESIAN_POINT('Ctrl Pts',(-19.5912951011556,-41.7561108916774,
124.908434150028)) ;
#48689 = CARTESIAN_POINT('Ctrl Pts',(-19.7613596240019,-41.9461414302098,
124.565200707997)) ;
#48690 = CARTESIAN_POINT('Ctrl Pts',(-19.8493960390687,-41.7661523498469,
124.853543536914)) ;
#48691 = CARTESIAN_POINT('Ctrl Pts',(-19.9531398235918,-41.9559728939981,
124.48810716658)) ;
#48692 = CARTESIAN_POINT('Ctrl Pts',(-20.089121327571,-41.7759838136352,124.757174104887)) ;
#48693 = CARTESIAN_POINT('Ctrl Pts',(-20.1319364909177,-41.965977826302,124.377372382878)) ;
#48694 = CARTESIAN_POINT('Ctrl Pts',(-20.3126159520966,-41.7859887459391,
124.618753527264)) ;
#48695 = CARTESIAN_POINT('Ctrl Pts',(-20.2884681065489,-41.9759641901967,
124.237408278261)) ;
#48696 = CARTESIAN_POINT('Ctrl Pts',(-20.5082790000552,-41.7959751098338,
124.44379651089)) ;
#48697 = CARTESIAN_POINT('Ctrl Pts',(-20.4187181316533,-41.9859938190826,
124.071617468983)) ;
#48698 = CARTESIAN_POINT('Ctrl Pts',(-20.6710896620277,-41.8060047387197,
124.236556568521)) ;
#48699 = CARTESIAN_POINT('Ctrl Pts',(-20.5169261211042,-41.995869041191,123.888684071241)) ;
#48700 = CARTESIAN_POINT('Ctrl Pts',(-20.7938478463196,-41.8158799608281,
124.007888084102)) ;
#48701 = CARTESIAN_POINT('Ctrl Pts',(-20.5829278692201,-42.0058702535881,
123.689089793923)) ;
#48702 = CARTESIAN_POINT('Ctrl Pts',(-20.8763477233689,-41.8258811732252,
123.758394357555)) ;
#48703 = CARTESIAN_POINT('Ctrl Pts',(-20.6131956145041,-42.0157788328236,
123.482954015089)) ;
#48704 = CARTESIAN_POINT('Ctrl Pts',(-20.9141799974451,-41.8357897524607,
123.500723797923)) ;
#48705 = CARTESIAN_POINT('Ctrl Pts',(-20.6070613238518,-42.0258336853796,
123.271692586383)) ;
#48706 = CARTESIAN_POINT('Ctrl Pts',(-20.9065096443018,-41.8458446050167,
123.236647196744)) ;
#48707 = CARTESIAN_POINT('Ctrl Pts',(-20.5653915462767,-42.0356922676544,
123.068629174948)) ;
#48708 = CARTESIAN_POINT('Ctrl Pts',(-20.8544198064542,-41.8557031872915,
122.982817801589)) ;
#48709 = CARTESIAN_POINT('Ctrl Pts',(-20.4876191246396,-42.0457603970971,
122.871804464288)) ;
#48710 = CARTESIAN_POINT('Ctrl Pts',(-20.7572019522211,-41.8657713167342,
122.736787999825)) ;
#48711 = CARTESIAN_POINT('Ctrl Pts',(-20.3791532075603,-42.0556158687862,
122.695250592433)) ;
#48712 = CARTESIAN_POINT('Ctrl Pts',(-20.6216170476226,-41.8756267884233,
122.516096462903)) ;
#48713 = CARTESIAN_POINT('Ctrl Pts',(-20.2402233414134,-42.0656107171724,
122.53762013048)) ;
#48714 = CARTESIAN_POINT('Ctrl Pts',(-20.4479526497867,-41.8856216368096,
122.319060073039)) ;
#48715 = CARTESIAN_POINT('Ctrl Pts',(-20.0751431990478,-42.0756420139569,
122.406377183477)) ;
#48716 = CARTESIAN_POINT('Ctrl Pts',(-20.2416008599543,-41.895652933594,122.155008415797)) ;
#48717 = CARTESIAN_POINT('Ctrl Pts',(-19.8929827389423,-42.085508550167,122.307151426831)) ;
#48718 = CARTESIAN_POINT('Ctrl Pts',(-20.0138985646584,-41.9055194698041,
122.030978291943)) ;
#48719 = CARTESIAN_POINT('Ctrl Pts',(-19.6940889865307,-42.0954959731278,
122.239940435497)) ;
#48720 = CARTESIAN_POINT('Ctrl Pts',(-19.7652803949844,-41.9155068927649,
121.946967065513)) ;
#48721 = CARTESIAN_POINT('Ctrl Pts',(-19.4873935007549,-42.1054409121476,
122.208304514953)) ;
#48722 = CARTESIAN_POINT('Ctrl Pts',(-19.5069103967345,-41.9254518317847,
121.907424800281)) ;
#48723 = CARTESIAN_POINT('Ctrl Pts',(-19.2762891943971,-42.1154857980076,
122.213185852874)) ;
#48724 = CARTESIAN_POINT('Ctrl Pts',(-19.2430300937842,-41.9354967176447,
121.913529165086)) ;
#48725 = CARTESIAN_POINT('Ctrl Pts',(-19.0728324499465,-42.1253543330938,
122.253813361827)) ;
#48726 = CARTESIAN_POINT('Ctrl Pts',(-18.9887092821943,-41.9453652527309,
121.964316287629)) ;
#48727 = CARTESIAN_POINT('Ctrl Pts',(-18.877416228865,-42.1353202011005,122.329344157201)) ;
#48728 = CARTESIAN_POINT('Ctrl Pts',(-18.7444398718667,-41.9553311207376,
122.058732418128)) ;
#48729 = CARTESIAN_POINT('Ctrl Pts',(-18.697163938135,-42.145342848553,122.438490697059)) ;
#48730 = CARTESIAN_POINT('Ctrl Pts',(-18.5191258960405,-41.9653537681901,
122.195167959833)) ;
#48731 = CARTESIAN_POINT('Ctrl Pts',(-18.5401483686295,-42.1552664875606,
122.575845813976)) ;
#48732 = CARTESIAN_POINT('Ctrl Pts',(-18.322858065799,-41.9752774071977,122.366864085304)) ;
#48733 = CARTESIAN_POINT('Ctrl Pts',(-18.408710854997,-42.1652092125663,122.738393134439)) ;
#48734 = CARTESIAN_POINT('Ctrl Pts',(-18.1585632397569,-41.9852201322034,
122.570050124167)) ;
#48735 = CARTESIAN_POINT('Ctrl Pts',(-18.3066794566052,-42.1752548186182,
122.92328748586)) ;
#48736 = CARTESIAN_POINT('Ctrl Pts',(-18.0310264117004,-41.9952657382553,
122.80116942064)) ;
#48737 = CARTESIAN_POINT('Ctrl Pts',(-18.2393302313391,-42.1851162411393,
123.119379879712)) ;
#48738 = CARTESIAN_POINT('Ctrl Pts',(-17.9468424318338,-42.0051271607764,
123.046286075553)) ;
#48739 = CARTESIAN_POINT('Ctrl Pts',(-18.2062726029867,-42.1951098095885,
123.32682877589)) ;
#48740 = CARTESIAN_POINT('Ctrl Pts',(-17.9055231594074,-42.0151207292256,
123.305597710692)) ;
#48741 = CARTESIAN_POINT('Ctrl Pts',(-18.2096058519718,-42.2050352803438,
123.53549760296)) ;
#48742 = CARTESIAN_POINT('Ctrl Pts',(-17.9096925519482,-42.0250461999809,
123.56643384868)) ;
#48743 = CARTESIAN_POINT('Ctrl Pts',(-18.2495067475796,-42.2150629542996,
123.742474063571)) ;
#48744 = CARTESIAN_POINT('Ctrl Pts',(-17.9595713839581,-42.0350738739368,
123.825153894762)) ;
#48745 = CARTESIAN_POINT('Ctrl Pts',(-18.3235158516873,-42.2249501323413,
123.936741246355)) ;
#48746 = CARTESIAN_POINT('Ctrl Pts',(-18.0520856877186,-42.0449610519785,
124.067987197481)) ;
#48747 = CARTESIAN_POINT('Ctrl Pts',(-18.4314996605536,-42.2349785117095,
124.117783872996)) ;
#48748 = CARTESIAN_POINT('Ctrl Pts',(-18.187066988808,-42.0549894313466,124.294288291678)) ;
#48749 = CARTESIAN_POINT('Ctrl Pts',(-18.5673819663472,-42.244872754431,124.27530549087)) ;
#48750 = CARTESIAN_POINT('Ctrl Pts',(-18.3569254897191,-42.0648836740681,
124.491191503969)) ;
#48751 = CARTESIAN_POINT('Ctrl Pts',(-18.784709731541,-42.2582256710819,124.452982254129)) ;
#48752 = CARTESIAN_POINT('Ctrl Pts',(-18.6285705558117,-42.078236590719,124.71326978042)) ;
#48753 = CARTESIAN_POINT('Ctrl Pts',(-19.0405785225545,-42.2714281888286,
124.568605528917)) ;
#48754 = CARTESIAN_POINT('Ctrl Pts',(-18.948377526286,-42.0914391084657,124.857795814166)) ;
#48755 = CARTESIAN_POINT('Ctrl Pts',(-19.3175485571435,-42.2847840941096,
124.614299554858)) ;
#48756 = CARTESIAN_POINT('Ctrl Pts',(-19.2946442505059,-42.1047950137467,
124.914924015773)) ;
#48757 = CARTESIAN_POINT('Ctrl Pts',(-19.5256323724528,-42.2946807427474,
124.612199384341)) ;
#48758 = CARTESIAN_POINT('Ctrl Pts',(-19.5547381910601,-42.1146916623845,
124.912293117139)) ;
#48759 = CARTESIAN_POINT('Ctrl Pts',(-19.7332792605488,-42.3047288807999,
124.573491321626)) ;
#48760 = CARTESIAN_POINT('Ctrl Pts',(-19.8142993016192,-42.124739800437,124.86390602345)) ;
#48761 = CARTESIAN_POINT('Ctrl Pts',(-19.9279820672216,-42.3146198409776,
124.500461827482)) ;
#48762 = CARTESIAN_POINT('Ctrl Pts',(-20.0576759368903,-42.1346307606148,
124.772616402038)) ;
#48763 = CARTESIAN_POINT('Ctrl Pts',(-20.1091567639837,-42.3246126768544,
124.394101946924)) ;
#48764 = CARTESIAN_POINT('Ctrl Pts',(-20.2841432703349,-42.1446235964915,
124.639664036342)) ;
#48765 = CARTESIAN_POINT('Ctrl Pts',(-20.2695244297562,-42.334651771856,124.256910080624)) ;
#48766 = CARTESIAN_POINT('Ctrl Pts',(-20.4846006078538,-42.1546626914931,
124.468172605259)) ;
#48767 = CARTESIAN_POINT('Ctrl Pts',(-20.4013315978798,-42.3444891277071,
124.097515807606)) ;
#48768 = CARTESIAN_POINT('Ctrl Pts',(-20.6493590677972,-42.1645000473443,
124.268925825602)) ;
#48769 = CARTESIAN_POINT('Ctrl Pts',(-20.5404892382136,-42.3578820756379,
123.852779647777)) ;
#48770 = CARTESIAN_POINT('Ctrl Pts',(-20.8232941424064,-42.177892995275,123.963015567167)) ;
#48771 = CARTESIAN_POINT('Ctrl Pts',(-20.6114090444013,-42.3710487520648,
123.581847669317)) ;
#48772 = CARTESIAN_POINT('Ctrl Pts',(-20.9119427186459,-42.1910596717019,
123.624389608226)) ;
#48773 = CARTESIAN_POINT('Ctrl Pts',(-20.6101088531211,-42.3844335334716,
123.300551825487)) ;
#48774 = CARTESIAN_POINT('Ctrl Pts',(-20.9103198254801,-42.2044444531087,
123.272710611957)) ;
#48775 = CARTESIAN_POINT('Ctrl Pts',(-20.5732425145346,-42.3942953161154,
123.096486655904)) ;
#48776 = CARTESIAN_POINT('Ctrl Pts',(-20.8642332429121,-42.2143062357526,
123.017641919768)) ;
#48777 = CARTESIAN_POINT('Ctrl Pts',(-20.5008532734841,-42.4042944640685,
122.899177214063)) ;
#48778 = CARTESIAN_POINT('Ctrl Pts',(-20.7737441303443,-42.2243053837056,
122.771002649473)) ;
#48779 = CARTESIAN_POINT('Ctrl Pts',(-20.3964434183661,-42.4141972566856,
122.719010769963)) ;
#48780 = CARTESIAN_POINT('Ctrl Pts',(-20.6432311626779,-42.2342081763227,
122.545797674276)) ;
#48781 = CARTESIAN_POINT('Ctrl Pts',(-20.2603721575889,-42.4242468365765,
122.5574632317)) ;
#48782 = CARTESIAN_POINT('Ctrl Pts',(-20.4731343577102,-42.2442577562136,
122.343862138749)) ;
#48783 = CARTESIAN_POINT('Ctrl Pts',(-20.0479239998599,-42.437433910386,122.379158143776)) ;
#48784 = CARTESIAN_POINT('Ctrl Pts',(-20.2076003346992,-42.2574448300231,
122.12099560958)) ;
#48785 = CARTESIAN_POINT('Ctrl Pts',(-19.7251865030468,-42.4541867003572,
122.228834167967)) ;
#48786 = CARTESIAN_POINT('Ctrl Pts',(-19.8041265873875,-42.2741976199943,
121.933081385993)) ;
#48787 = CARTESIAN_POINT('Ctrl Pts',(-19.3757249735959,-42.4706753524519,
122.198219597745)) ;
#48788 = CARTESIAN_POINT('Ctrl Pts',(-19.3673812946828,-42.290686272089,121.894819463525)) ;
#48789 = CARTESIAN_POINT('Ctrl Pts',(-19.0992014727295,-42.4840321786353,
122.246369143376)) ;
#48790 = CARTESIAN_POINT('Ctrl Pts',(-19.0216618585074,-42.3040430982724,
121.955010874022)) ;
#48791 = CARTESIAN_POINT('Ctrl Pts',(-18.9034559148771,-42.4939285635132,
122.317028660144)) ;
#48792 = CARTESIAN_POINT('Ctrl Pts',(-18.7769948829387,-42.3139394831503,
122.043336388622)) ;
#48793 = CARTESIAN_POINT('Ctrl Pts',(-18.7209921103284,-42.5039350780337,
122.42160568978)) ;
#48794 = CARTESIAN_POINT('Ctrl Pts',(-18.5489107993243,-42.3239459976708,
122.174062497428)) ;
#48795 = CARTESIAN_POINT('Ctrl Pts',(-18.5074778701341,-42.5171252015501,
122.598716946262)) ;
#48796 = CARTESIAN_POINT('Ctrl Pts',(-18.2820313956166,-42.3371361211872,
122.395439854909)) ;
#48797 = CARTESIAN_POINT('Ctrl Pts',(-18.3017330813565,-42.5338917626996,
122.889684627251)) ;
#48798 = CARTESIAN_POINT('Ctrl Pts',(-18.0248416307128,-42.3539026823368,
122.759167368776)) ;
#48799 = CARTESIAN_POINT('Ctrl Pts',(-18.1906918477385,-42.5536762514077,
123.295564658477)) ;
#48800 = CARTESIAN_POINT('Ctrl Pts',(-17.886048515107,-42.3736871710448,123.266512292216)) ;
#48801 = CARTESIAN_POINT('Ctrl Pts',(-18.2237744744841,-42.5736216990041,
123.718259239701)) ;
#48802 = CARTESIAN_POINT('Ctrl Pts',(-17.9274046621304,-42.3936326186413,
123.794881011967)) ;
#48803 = CARTESIAN_POINT('Ctrl Pts',(-18.3992319347338,-42.5935333611601,
124.103576998798)) ;
#48804 = CARTESIAN_POINT('Ctrl Pts',(-18.1467300052869,-42.4135442807972,
124.276525572974)) ;
#48805 = CARTESIAN_POINT('Ctrl Pts',(-18.6947270079494,-42.6134255531789,
124.406289323311)) ;
#48806 = CARTESIAN_POINT('Ctrl Pts',(-18.5161004763561,-42.4334364728161,
124.654913018434)) ;
#48807 = CARTESIAN_POINT('Ctrl Pts',(-19.078800891227,-42.6334666837336,124.590739441501)) ;
#48808 = CARTESIAN_POINT('Ctrl Pts',(-18.9961947812989,-42.4534776033707,
124.885472692553)) ;
#48809 = CARTESIAN_POINT('Ctrl Pts',(-19.4981893983463,-42.6532850183492,
124.632822667758)) ;
#48810 = CARTESIAN_POINT('Ctrl Pts',(-19.5204288936076,-42.4732959379863,
124.938073341943)) ;
#48811 = CARTESIAN_POINT('Ctrl Pts',(-19.9098714360872,-42.6732575835688,
124.529182144137)) ;
#48812 = CARTESIAN_POINT('Ctrl Pts',(-20.0350303911064,-42.4932685032059,
124.808520139639)) ;
#48813 = CARTESIAN_POINT('Ctrl Pts',(-20.2603190889311,-42.6931467997404,
124.292190471673)) ;
#48814 = CARTESIAN_POINT('Ctrl Pts',(-20.473087584271,-42.5131577193775,124.512279231662)) ;
#48815 = CARTESIAN_POINT('Ctrl Pts',(-20.5101445680897,-42.7131703740631,
123.947568704461)) ;
#48816 = CARTESIAN_POINT('Ctrl Pts',(-20.7853676285003,-42.5331812937002,
124.081500341418)) ;
#48817 = CARTESIAN_POINT('Ctrl Pts',(-20.6263908959112,-42.7329675371513,
123.542918161152)) ;
#48818 = CARTESIAN_POINT('Ctrl Pts',(-20.9306728526506,-42.5529784567885,
123.575689148436)) ;
#48819 = CARTESIAN_POINT('Ctrl Pts',(-20.5983617331869,-42.7529330309751,
123.119413546413)) ;
#48820 = CARTESIAN_POINT('Ctrl Pts',(-20.8956352696577,-42.5729439506122,
123.046309019479)) ;
#48821 = CARTESIAN_POINT('Ctrl Pts',(-20.4270355343715,-42.7728867387165,
122.731150195956)) ;
#48822 = CARTESIAN_POINT('Ctrl Pts',(-20.6814765719901,-42.5928976583536,
122.560980844406)) ;
#48823 = CARTESIAN_POINT('Ctrl Pts',(-20.1343395660946,-42.7927941154431,
122.425505425646)) ;
#48824 = CARTESIAN_POINT('Ctrl Pts',(-20.3156068294175,-42.6128050350802,
122.178926648595)) ;
#48825 = CARTESIAN_POINT('Ctrl Pts',(-19.7563159918193,-42.8126463269917,
122.237523332506)) ;
#48826 = CARTESIAN_POINT('Ctrl Pts',(-19.8430795028509,-42.6326572466288,
121.943950043858)) ;
#48827 = CARTESIAN_POINT('Ctrl Pts',(-19.3322246512801,-42.8327187139374,
122.189721479614)) ;
#48828 = CARTESIAN_POINT('Ctrl Pts',(-19.3129641321421,-42.6527296335745,
121.884197616228)) ;
#48829 = CARTESIAN_POINT('Ctrl Pts',(-18.9222367590498,-42.8525565835777,
122.288891061449)) ;
#48830 = CARTESIAN_POINT('Ctrl Pts',(-18.8004818960636,-42.6725675032148,
122.008159120081)) ;
#48831 = CARTESIAN_POINT('Ctrl Pts',(-18.5694696067115,-42.8724072381308,
122.520633431099)) ;
#48832 = CARTESIAN_POINT('Ctrl Pts',(-18.3595239816206,-42.6924181577679,
122.297834685126)) ;
#48833 = CARTESIAN_POINT('Ctrl Pts',(-18.314918147968,-42.8924591724712,122.862621733189)) ;
#48834 = CARTESIAN_POINT('Ctrl Pts',(-18.0413332378271,-42.7124700921084,
122.725319925752)) ;
#48835 = CARTESIAN_POINT('Ctrl Pts',(-18.1937042551041,-42.9122923600373,
123.266633949038)) ;
#48836 = CARTESIAN_POINT('Ctrl Pts',(-17.8898151802692,-42.7323032796744,
123.230332622468)) ;
#48837 = CARTESIAN_POINT('Ctrl Pts',(-18.2168953535135,-42.932221572268,123.689590915752)) ;
#48838 = CARTESIAN_POINT('Ctrl Pts',(-17.9188018275413,-42.7522324919051,
123.759028000003)) ;
#48839 = CARTESIAN_POINT('Ctrl Pts',(-18.382321733306,-42.9521065374824,124.078869953119)) ;
#48840 = CARTESIAN_POINT('Ctrl Pts',(-18.1255818945999,-42.7721174571195,
124.245626671825)) ;
#48841 = CARTESIAN_POINT('Ctrl Pts',(-18.6737062137308,-42.972180278627,124.390635608847)) ;
#48842 = CARTESIAN_POINT('Ctrl Pts',(-18.4898112910282,-42.7921911982641,
124.635336040243)) ;
#48843 = CARTESIAN_POINT('Ctrl Pts',(-19.0487871348763,-42.9919734604074,
124.581662444527)) ;
#48844 = CARTESIAN_POINT('Ctrl Pts',(-18.9586591560268,-42.8119843800445,
124.874120892103)) ;
#48845 = CARTESIAN_POINT('Ctrl Pts',(-19.4698565957341,-43.0119361684101,
124.634936091618)) ;
#48846 = CARTESIAN_POINT('Ctrl Pts',(-19.4849952307029,-42.8319470880472,
124.940716397595)) ;
#48847 = CARTESIAN_POINT('Ctrl Pts',(-19.88406254428,-43.0319191201525,124.540216705959)) ;
#48848 = CARTESIAN_POINT('Ctrl Pts',(-20.0027532085215,-42.8519300397896,
124.822320272742)) ;
#48849 = CARTESIAN_POINT('Ctrl Pts',(-20.2384793849242,-43.0517297399247,
124.312505833384)) ;
#48850 = CARTESIAN_POINT('Ctrl Pts',(-20.4457748038711,-42.8717406595618,
124.537685736192)) ;
#48851 = CARTESIAN_POINT('Ctrl Pts',(-20.4964670998854,-43.0717134559576,
123.975002267441)) ;
#48852 = CARTESIAN_POINT('Ctrl Pts',(-20.7682626054881,-42.8917243755947,
124.115808826861)) ;
#48853 = CARTESIAN_POINT('Ctrl Pts',(-20.6231390461281,-43.0915949198549,
123.571582193787)) ;
#48854 = CARTESIAN_POINT('Ctrl Pts',(-20.9266062652679,-42.911605839492,123.611535793601)) ;
#48855 = CARTESIAN_POINT('Ctrl Pts',(-20.6047789342682,-43.1115502496993,
123.147760811554)) ;
#48856 = CARTESIAN_POINT('Ctrl Pts',(-20.9036603572419,-42.9315611693364,
123.081759157368)) ;
#48857 = CARTESIAN_POINT('Ctrl Pts',(-20.4437676887391,-43.1314257105047,
122.756956257546)) ;
#48858 = CARTESIAN_POINT('Ctrl Pts',(-20.7024014511106,-42.9514366301419,
122.593252469761)) ;
#48859 = CARTESIAN_POINT('Ctrl Pts',(-20.1577658156796,-43.1514100305563,
122.442758918448)) ;
#48860 = CARTESIAN_POINT('Ctrl Pts',(-20.3449003201343,-42.9714209501934,
122.200502446689)) ;
#48861 = CARTESIAN_POINT('Ctrl Pts',(-19.7825309062967,-43.1713380633459,
122.245718411537)) ;
#48862 = CARTESIAN_POINT('Ctrl Pts',(-19.8758679528504,-42.991348982983,121.954198379585)) ;
#48863 = CARTESIAN_POINT('Ctrl Pts',(-19.4327161765644,-43.1879468252857,
122.19803250865)) ;
#48864 = CARTESIAN_POINT('Ctrl Pts',(-19.438573167792,-43.0079577449228,121.894584975642)) ;
#48865 = CARTESIAN_POINT('Ctrl Pts',(-19.1575751517247,-43.2011344639758,
122.232458878335)) ;
#48866 = CARTESIAN_POINT('Ctrl Pts',(-19.0946716817039,-43.0211453836129,
121.937615803098)) ;
#48867 = CARTESIAN_POINT('Ctrl Pts',(-18.9568164762122,-43.2111208983359,
122.29383159449)) ;
#48868 = CARTESIAN_POINT('Ctrl Pts',(-18.8437153066299,-43.031131817973,122.014331380066)) ;
#48869 = CARTESIAN_POINT('Ctrl Pts',(-18.7693989059073,-43.2211302722953,
122.389560213479)) ;
#48870 = CARTESIAN_POINT('Ctrl Pts',(-18.6094527009105,-43.0411411919324,
122.133980200505)) ;
#48871 = CARTESIAN_POINT('Ctrl Pts',(-18.5463444276645,-43.2344203058605,
122.557741103274)) ;
#48872 = CARTESIAN_POINT('Ctrl Pts',(-18.3305857336724,-43.0544312254977,
122.344252306569)) ;
#48873 = CARTESIAN_POINT('Ctrl Pts',(-18.3288675857434,-43.251014293523,122.835683924907)) ;
#48874 = CARTESIAN_POINT('Ctrl Pts',(-18.0587919012148,-43.0710252131601,
122.691613440136)) ;
#48875 = CARTESIAN_POINT('Ctrl Pts',(-18.2190954075611,-43.2676465487985,
123.171796668551)) ;
#48876 = CARTESIAN_POINT('Ctrl Pts',(-17.9215463024505,-43.0876574684357,
123.111805424013)) ;
#48877 = CARTESIAN_POINT('Ctrl Pts',(-18.2039836097742,-43.2808889324664,
123.449819348037)) ;
#48878 = CARTESIAN_POINT('Ctrl Pts',(-17.9026645543824,-43.1008998521035,
123.459298795023)) ;
#48879 = CARTESIAN_POINT('Ctrl Pts',(-18.2283482509571,-43.2908031406938,
123.656820558235)) ;
#48880 = CARTESIAN_POINT('Ctrl Pts',(-17.9331154384697,-43.1108140603309,
123.718057560274)) ;
#48881 = CARTESIAN_POINT('Ctrl Pts',(-18.289369033941,-43.3008597799655,123.85923089601)) ;
#48882 = CARTESIAN_POINT('Ctrl Pts',(-18.0093888248284,-43.1208706996026,
123.971069080689)) ;
#48883 = CARTESIAN_POINT('Ctrl Pts',(-18.382402147398,-43.3107055863856,124.044152684337)) ;
#48884 = CARTESIAN_POINT('Ctrl Pts',(-18.1256799001394,-43.1307165060227,
124.202224696424)) ;
#48885 = CARTESIAN_POINT('Ctrl Pts',(-18.5083351564249,-43.3207505860188,
124.213670912525)) ;
#48886 = CARTESIAN_POINT('Ctrl Pts',(-18.2830849970775,-43.1407615056559,
124.414117164475)) ;
#48887 = CARTESIAN_POINT('Ctrl Pts',(-18.7114677451612,-43.3340316083915,
124.405150502509)) ;
#48888 = CARTESIAN_POINT('Ctrl Pts',(-18.537043251934,-43.1540425280286,124.65350405423)) ;
#48889 = CARTESIAN_POINT('Ctrl Pts',(-18.9580635205512,-43.3472290549162,
124.539134994554)) ;
#48890 = CARTESIAN_POINT('Ctrl Pts',(-18.8452649773422,-43.1672399745533,
124.820961905211)) ;
#48891 = CARTESIAN_POINT('Ctrl Pts',(-19.232360254932,-43.3606433527231,124.60475396977)) ;
#48892 = CARTESIAN_POINT('Ctrl Pts',(-19.1881152200042,-43.1806542723603,
124.902985565981)) ;
#48893 = CARTESIAN_POINT('Ctrl Pts',(-19.4388332017117,-43.3704824181259,
124.617341847239)) ;
#48894 = CARTESIAN_POINT('Ctrl Pts',(-19.4462101896744,-43.190493337763,124.918723959337)) ;
#48895 = CARTESIAN_POINT('Ctrl Pts',(-19.6473989067929,-43.3804656244036,
124.594097451494)) ;
#48896 = CARTESIAN_POINT('Ctrl Pts',(-19.7069166424415,-43.2004765440407,
124.889671060815)) ;
#48897 = CARTESIAN_POINT('Ctrl Pts',(-19.8481271767385,-43.3904168593164,
124.535103924099)) ;
#48898 = CARTESIAN_POINT('Ctrl Pts',(-19.9578281238234,-43.2104277789535,
124.815931888651)) ;
#48899 = CARTESIAN_POINT('Ctrl Pts',(-20.0366117400743,-43.400417859018,124.441917217521)) ;
#48900 = CARTESIAN_POINT('Ctrl Pts',(-20.1934350689946,-43.2204287786551,
124.699450981921)) ;
#48901 = CARTESIAN_POINT('Ctrl Pts',(-20.2063611151425,-43.4104492048053,
124.316781602561)) ;
#48902 = CARTESIAN_POINT('Ctrl Pts',(-20.4056235278496,-43.2304601244425,
124.543033701341)) ;
#48903 = CARTESIAN_POINT('Ctrl Pts',(-20.3494415293354,-43.4203029695104,
124.166967548006)) ;
#48904 = CARTESIAN_POINT('Ctrl Pts',(-20.5844761556059,-43.2403138891475,
124.355767995576)) ;
#48905 = CARTESIAN_POINT('Ctrl Pts',(-20.4660990695742,-43.4302736231787,
123.992841247419)) ;
#48906 = CARTESIAN_POINT('Ctrl Pts',(-20.7303004788071,-43.2502845428158,
124.138111587072)) ;
#48907 = CARTESIAN_POINT('Ctrl Pts',(-20.550990914283,-43.4402708668359,123.800540309338)) ;
#48908 = CARTESIAN_POINT('Ctrl Pts',(-20.836417878929,-43.260281786473,123.897736472941)) ;
#48909 = CARTESIAN_POINT('Ctrl Pts',(-20.6011102529221,-43.4503043227801,
123.595664099876)) ;
#48910 = CARTESIAN_POINT('Ctrl Pts',(-20.8990697974022,-43.2703152424172,
123.641641842364)) ;
#48911 = CARTESIAN_POINT('Ctrl Pts',(-20.614988288072,-43.4601598270805,123.388915446738)) ;
#48912 = CARTESIAN_POINT('Ctrl Pts',(-20.9164201484356,-43.2801707467176,
123.383205983392)) ;
#48913 = CARTESIAN_POINT('Ctrl Pts',(-20.5927177301591,-43.4701592633666,
123.179916340754)) ;
#48914 = CARTESIAN_POINT('Ctrl Pts',(-20.8885847142338,-43.2901701830037,
123.121956715712)) ;
#48915 = CARTESIAN_POINT('Ctrl Pts',(-20.5353148533199,-43.4800537228825,
122.979940150803)) ;
#48916 = CARTESIAN_POINT('Ctrl Pts',(-20.8168337005953,-43.3000646425196,
122.871985466953)) ;
#48917 = CARTESIAN_POINT('Ctrl Pts',(-20.4424830563002,-43.4901168423341,
122.789877503651)) ;
#48918 = CARTESIAN_POINT('Ctrl Pts',(-20.7007964614407,-43.3101277619712,
122.634405971093)) ;
#48919 = CARTESIAN_POINT('Ctrl Pts',(-20.3209670354075,-43.4999564767461,
122.622428572666)) ;
#48920 = CARTESIAN_POINT('Ctrl Pts',(-20.5489034190072,-43.3199673963832,
122.425092863815)) ;
#48921 = CARTESIAN_POINT('Ctrl Pts',(-20.1690754221766,-43.5100196842319,
122.475206765639)) ;
#48922 = CARTESIAN_POINT('Ctrl Pts',(-20.3590408300149,-43.330030603869,122.2410636791)) ;
#48923 = CARTESIAN_POINT('Ctrl Pts',(-19.9967306491501,-43.5199137916111,
122.358701622462)) ;
#48924 = CARTESIAN_POINT('Ctrl Pts',(-20.1436111274021,-43.3399247112482,
122.095429795694)) ;
#48925 = CARTESIAN_POINT('Ctrl Pts',(-19.8061253691053,-43.5298561238035,
122.272988374327)) ;
#48926 = CARTESIAN_POINT('Ctrl Pts',(-19.9053553865041,-43.3498670434406,
121.988285686092)) ;
#48927 = CARTESIAN_POINT('Ctrl Pts',(-19.6023104751595,-43.5398567501185,
122.221256111772)) ;
#48928 = CARTESIAN_POINT('Ctrl Pts',(-19.6505873376339,-43.3598676697556,
121.923617759925)) ;
#48929 = CARTESIAN_POINT('Ctrl Pts',(-19.3917705372051,-43.5498984844004,
122.206031467105)) ;
#48930 = CARTESIAN_POINT('Ctrl Pts',(-19.3874126433953,-43.3699094040375,
121.904584247529)) ;
#48931 = CARTESIAN_POINT('Ctrl Pts',(-19.1862281430007,-43.5597239103495,
122.226676883472)) ;
#48932 = CARTESIAN_POINT('Ctrl Pts',(-19.1304837624484,-43.3797348299866,
121.930388446646)) ;
#48933 = CARTESIAN_POINT('Ctrl Pts',(-18.9826551708029,-43.5697807368771,
122.283706162221)) ;
#48934 = CARTESIAN_POINT('Ctrl Pts',(-18.876016923458,-43.3897916565143,122.001672516022)) ;
#48935 = CARTESIAN_POINT('Ctrl Pts',(-18.7946320656292,-43.5797081699987,
122.374314662117)) ;
#48936 = CARTESIAN_POINT('Ctrl Pts',(-18.6409865992809,-43.3997190896358,
122.114930897131)) ;
#48937 = CARTESIAN_POINT('Ctrl Pts',(-18.6244661109234,-43.5896581624049,
122.495982615423)) ;
#48938 = CARTESIAN_POINT('Ctrl Pts',(-18.428277440835,-43.4096690820421,122.267013929381)) ;
#48939 = CARTESIAN_POINT('Ctrl Pts',(-18.4767445700098,-43.5997133634789,
122.647173613548)) ;
#48940 = CARTESIAN_POINT('Ctrl Pts',(-18.2436237169547,-43.4197242831161,
122.456000772691)) ;
#48941 = CARTESIAN_POINT('Ctrl Pts',(-18.3599557995264,-43.6095356375312,
122.817488686517)) ;
#48942 = CARTESIAN_POINT('Ctrl Pts',(-18.0976352137637,-43.4295465571684,
122.668893815947)) ;
#48943 = CARTESIAN_POINT('Ctrl Pts',(-18.2721502560574,-43.6195915314905,
123.009781982913)) ;
#48944 = CARTESIAN_POINT('Ctrl Pts',(-17.987876075402,-43.4396024511276,122.909259308021)) ;
#48945 = CARTESIAN_POINT('Ctrl Pts',(-18.2200294874752,-43.6295322533356,
123.212171534823)) ;
#48946 = CARTESIAN_POINT('Ctrl Pts',(-17.9227225617815,-43.4495431729727,
123.162245934171)) ;
#48947 = CARTESIAN_POINT('Ctrl Pts',(-18.2032511636616,-43.6394365974222,
123.419718607872)) ;
#48948 = CARTESIAN_POINT('Ctrl Pts',(-17.9017472036595,-43.4594475170593,
123.421680109374)) ;
#48949 = CARTESIAN_POINT('Ctrl Pts',(-18.2231767398449,-43.6494832647217,
123.629971456285)) ;
#48950 = CARTESIAN_POINT('Ctrl Pts',(-17.926651728431,-43.4694941843588,123.684496298927)) ;
#48951 = CARTESIAN_POINT('Ctrl Pts',(-18.2782926714603,-43.6593788231716,
123.830608023793)) ;
#48952 = CARTESIAN_POINT('Ctrl Pts',(-17.9955444787495,-43.4793897428087,
123.935293204385)) ;
#48953 = CARTESIAN_POINT('Ctrl Pts',(-18.368880857869,-43.6694409018763,124.021733140042)) ;
#48954 = CARTESIAN_POINT('Ctrl Pts',(-18.1087774586024,-43.4894518215134,
124.174200467457)) ;
#48955 = CARTESIAN_POINT('Ctrl Pts',(-18.4885436290757,-43.6792836003421,
124.19057641474)) ;
#48956 = CARTESIAN_POINT('Ctrl Pts',(-18.258354480537,-43.4992945199792,124.38525663974)) ;
#48957 = CARTESIAN_POINT('Ctrl Pts',(-18.637534073092,-43.6892743742365,124.338585277532)) ;
#48958 = CARTESIAN_POINT('Ctrl Pts',(-18.4445910638163,-43.5092852938737,
124.570269448432)) ;
#48959 = CARTESIAN_POINT('Ctrl Pts',(-18.8089243606345,-43.6992022434715,
124.457711598807)) ;
#48960 = CARTESIAN_POINT('Ctrl Pts',(-18.6588280253988,-43.5192131631086,
124.719179491474)) ;
#48961 = CARTESIAN_POINT('Ctrl Pts',(-18.9994025238417,-43.7091909724413,
124.546144010481)) ;
#48962 = CARTESIAN_POINT('Ctrl Pts',(-18.8969249830435,-43.5292018920784,
124.829722059016)) ;
#48963 = CARTESIAN_POINT('Ctrl Pts',(-19.2034513375471,-43.7192303744251,
124.600051021114)) ;
#48964 = CARTESIAN_POINT('Ctrl Pts',(-19.1519853155007,-43.5392412940622,
124.897107996918)) ;
#48965 = CARTESIAN_POINT('Ctrl Pts',(-19.4095740593302,-43.7290705421618,
124.617767680818)) ;
#48966 = CARTESIAN_POINT('Ctrl Pts',(-19.4096395220042,-43.549081461799,124.91925607013)) ;
#48967 = CARTESIAN_POINT('Ctrl Pts',(-19.6200056310843,-43.7391187525363,
124.599348020896)) ;
#48968 = CARTESIAN_POINT('Ctrl Pts',(-19.6726790143965,-43.5591296721735,
124.896233588286)) ;
#48969 = CARTESIAN_POINT('Ctrl Pts',(-19.8219167217474,-43.7490659228241,
124.544896993531)) ;
#48970 = CARTESIAN_POINT('Ctrl Pts',(-19.9250688422305,-43.5690768424612,
124.828171804027)) ;
#48971 = CARTESIAN_POINT('Ctrl Pts',(-20.0108816230602,-43.7589767710792,
124.457103125973)) ;
#48972 = CARTESIAN_POINT('Ctrl Pts',(-20.1612764162791,-43.5789876907163,
124.718431010593)) ;
#48973 = CARTESIAN_POINT('Ctrl Pts',(-20.1841105037693,-43.7690330987569,
124.335929383685)) ;
#48974 = CARTESIAN_POINT('Ctrl Pts',(-20.3778135163567,-43.5890440183941,
124.566965650242)) ;
#48975 = CARTESIAN_POINT('Ctrl Pts',(-20.3307480730598,-43.7788835115255,
124.189689219311)) ;
#48976 = CARTESIAN_POINT('Ctrl Pts',(-20.561112631005,-43.5988944311626,124.384166137477)) ;
#48977 = CARTESIAN_POINT('Ctrl Pts',(-20.4523107242859,-43.7889103973592,
124.017478146335)) ;
#48978 = CARTESIAN_POINT('Ctrl Pts',(-20.7130674436225,-43.6089213169963,
124.168903399289)) ;
#48979 = CARTESIAN_POINT('Ctrl Pts',(-20.5416506384017,-43.79893901299,123.826498737951)) ;
#48980 = CARTESIAN_POINT('Ctrl Pts',(-20.8247441401648,-43.6189499326271,
123.930180059024)) ;
#48981 = CARTESIAN_POINT('Ctrl Pts',(-20.5958423754753,-43.8087842363675,
123.626753384018)) ;
#48982 = CARTESIAN_POINT('Ctrl Pts',(-20.8924859435401,-43.6287951560046,
123.680497788512)) ;
#48983 = CARTESIAN_POINT('Ctrl Pts',(-20.6153678869501,-43.8187749184691,
123.417621815396)) ;
#48984 = CARTESIAN_POINT('Ctrl Pts',(-20.9168945752152,-43.6387858381062,
123.419083293922)) ;
#48985 = CARTESIAN_POINT('Ctrl Pts',(-20.5977356287722,-43.8288128071015,
123.207333737344)) ;
#48986 = CARTESIAN_POINT('Ctrl Pts',(-20.8948561360059,-43.6488237267386,
123.156223171646)) ;
#48987 = CARTESIAN_POINT('Ctrl Pts',(-20.5452446975445,-43.8386571422047,
123.007134061094)) ;
#48988 = CARTESIAN_POINT('Ctrl Pts',(-20.8292438813552,-43.6586680618418,
122.905971997117)) ;
#48989 = CARTESIAN_POINT('Ctrl Pts',(-20.4579454357753,-43.8486421044022,
122.816264363838)) ;
#48990 = CARTESIAN_POINT('Ctrl Pts',(-20.7201211840109,-43.6686530240393,
122.667383970185)) ;
#48991 = CARTESIAN_POINT('Ctrl Pts',(-20.3394267685731,-43.8585810459356,
122.644144630097)) ;
#48992 = CARTESIAN_POINT('Ctrl Pts',(-20.5719738572654,-43.6785919655727,
122.452232949088)) ;
#48993 = CARTESIAN_POINT('Ctrl Pts',(-20.1912921885784,-43.868622930907,122.493758530072)) ;
#48994 = CARTESIAN_POINT('Ctrl Pts',(-20.3868068904669,-43.6886338505441,
122.264249292356)) ;
#48995 = CARTESIAN_POINT('Ctrl Pts',(-20.0220013238299,-43.8785094788153,
122.373139062939)) ;
#48996 = CARTESIAN_POINT('Ctrl Pts',(-20.1751934660884,-43.6985203984524,
122.113473137318)) ;
#48997 = CARTESIAN_POINT('Ctrl Pts',(-19.8324762444945,-43.8885034043153,
122.282516116147)) ;
#48998 = CARTESIAN_POINT('Ctrl Pts',(-19.9382875919748,-43.7085143239524,
122.000193047115)) ;
#48999 = CARTESIAN_POINT('Ctrl Pts',(-19.6312362520306,-43.8984394954417,
122.226393147008)) ;
#49000 = CARTESIAN_POINT('Ctrl Pts',(-19.6867374287566,-43.7184504150789,
121.930037797555)) ;
#49001 = CARTESIAN_POINT('Ctrl Pts',(-19.4214139020312,-43.9084687644217,
122.205920422731)) ;
#49002 = CARTESIAN_POINT('Ctrl Pts',(-19.4244597082895,-43.7284796840588,
121.904445450491)) ;
#49003 = CARTESIAN_POINT('Ctrl Pts',(-19.2142240963958,-43.918351146981,122.221693374748)) ;
#49004 = CARTESIAN_POINT('Ctrl Pts',(-19.1654713412245,-43.7383620666181,
121.924160359803)) ;
#49005 = CARTESIAN_POINT('Ctrl Pts',(-19.009498669417,-43.9284036640689,122.274004896839)) ;
#49006 = CARTESIAN_POINT('Ctrl Pts',(-18.909564469388,-43.748414583706,121.989548406113)) ;
#49007 = CARTESIAN_POINT('Ctrl Pts',(-18.819892626088,-43.9382977848928,122.359628820028)) ;
#49008 = CARTESIAN_POINT('Ctrl Pts',(-18.672555542748,-43.7583087045299,122.096577505371)) ;
#49009 = CARTESIAN_POINT('Ctrl Pts',(-18.6451418431221,-43.9483597643132,
122.478785235648)) ;
#49010 = CARTESIAN_POINT('Ctrl Pts',(-18.4541166120411,-43.7683706839503,
122.245521781435)) ;
#49011 = CARTESIAN_POINT('Ctrl Pts',(-18.4969665742692,-43.9582042975421,
122.623287056138)) ;
#49012 = CARTESIAN_POINT('Ctrl Pts',(-18.2688956918944,-43.7782152171792,
122.426149066543)) ;
#49013 = CARTESIAN_POINT('Ctrl Pts',(-18.3741086579576,-43.9681643764484,
122.792844278905)) ;
#49014 = CARTESIAN_POINT('Ctrl Pts',(-18.1153222214896,-43.7881752960855,
122.63809537997)) ;
#49015 = CARTESIAN_POINT('Ctrl Pts',(-18.2822146957173,-43.978202653021,122.982811873734)) ;
#49016 = CARTESIAN_POINT('Ctrl Pts',(-18.0004538039104,-43.7982135726581,
122.875554226971)) ;
#49017 = CARTESIAN_POINT('Ctrl Pts',(-18.2252522008148,-43.9880760395588,
123.182444364765)) ;
#49018 = CARTESIAN_POINT('Ctrl Pts',(-17.9292494152414,-43.8080869591959,
123.125095646778)) ;
#49019 = CARTESIAN_POINT('Ctrl Pts',(-18.2034535742499,-43.9981489823259,
123.393043925117)) ;
#49020 = CARTESIAN_POINT('Ctrl Pts',(-17.902000155212,-43.818159901963,123.388344568531)) ;
#49021 = CARTESIAN_POINT('Ctrl Pts',(-18.2179298683599,-44.0079703964542,
123.599052536948)) ;
#49022 = CARTESIAN_POINT('Ctrl Pts',(-17.9200947062017,-43.8279813160913,
123.645856942376)) ;
#49023 = CARTESIAN_POINT('Ctrl Pts',(-18.2689797272042,-44.0180450265265,
123.804569296683)) ;
#49024 = CARTESIAN_POINT('Ctrl Pts',(-17.9839061111706,-43.8380559461636,
123.902752660032)) ;
#49025 = CARTESIAN_POINT('Ctrl Pts',(-18.3532690236661,-44.0279116638434,
123.994127168066)) ;
#49026 = CARTESIAN_POINT('Ctrl Pts',(-18.0892674357171,-43.8479225834805,
124.139701464723)) ;
#49027 = CARTESIAN_POINT('Ctrl Pts',(-18.4705660574724,-44.0379352092152,
124.169178578053)) ;
#49028 = CARTESIAN_POINT('Ctrl Pts',(-18.2358881550822,-43.8579461288523,
124.358516056916)) ;
#49029 = CARTESIAN_POINT('Ctrl Pts',(-18.6168901850746,-44.0479609607324,
124.320901604425)) ;
#49030 = CARTESIAN_POINT('Ctrl Pts',(-18.4187926357899,-43.8679718803695,
124.54817037461)) ;
#49031 = CARTESIAN_POINT('Ctrl Pts',(-18.7841854234927,-44.0578145477417,
124.443049390508)) ;
#49032 = CARTESIAN_POINT('Ctrl Pts',(-18.6279123309116,-43.8778254673789,
124.700856473428)) ;
#49033 = CARTESIAN_POINT('Ctrl Pts',(-18.9722447032616,-44.0677915079697,
124.535943542531)) ;
#49034 = CARTESIAN_POINT('Ctrl Pts',(-18.8629865023443,-43.8878024276068,
124.816974766263)) ;
#49035 = CARTESIAN_POINT('Ctrl Pts',(-19.1745538584046,-44.0778126509981,
124.594687633836)) ;
#49036 = CARTESIAN_POINT('Ctrl Pts',(-19.1158727506149,-43.8978235706353,
124.890405499117)) ;
#49037 = CARTESIAN_POINT('Ctrl Pts',(-19.3810867415163,-44.0876952570181,
124.617517604128)) ;
#49038 = CARTESIAN_POINT('Ctrl Pts',(-19.3740398930884,-43.9077061766552,
124.918943559724)) ;
#49039 = CARTESIAN_POINT('Ctrl Pts',(-19.5922777528914,-44.0977637276508,
124.603809178215)) ;
#49040 = CARTESIAN_POINT('Ctrl Pts',(-19.6380282810842,-43.9177746472879,
124.901808568913)) ;
#49041 = CARTESIAN_POINT('Ctrl Pts',(-19.7931371162424,-44.1075938108345,
124.555043900469)) ;
#49042 = CARTESIAN_POINT('Ctrl Pts',(-19.889104080618,-43.9276047304716,124.840852015822)) ;
#49043 = CARTESIAN_POINT('Ctrl Pts',(-19.9870797834277,-44.1176603705148,
124.470429298828)) ;
#49044 = CARTESIAN_POINT('Ctrl Pts',(-20.1315321754818,-43.937671290152,124.735084209406)) ;
#49045 = CARTESIAN_POINT('Ctrl Pts',(-20.1602737104804,-44.1275506203441,
124.355334521144)) ;
#49046 = CARTESIAN_POINT('Ctrl Pts',(-20.3480256593167,-43.9475615399812,
124.591215461382)) ;
#49047 = CARTESIAN_POINT('Ctrl Pts',(-20.3126945664649,-44.1375427860929,
124.210797364723)) ;
#49048 = CARTESIAN_POINT('Ctrl Pts',(-20.5385520107773,-43.95755370573,124.41054400151)) ;
#49049 = CARTESIAN_POINT('Ctrl Pts',(-20.4371805511039,-44.147505629689,124.042362117162)) ;
#49050 = CARTESIAN_POINT('Ctrl Pts',(-20.6941599747678,-43.9675165493261,
124.199999732193)) ;
#49051 = CARTESIAN_POINT('Ctrl Pts',(-20.5304651406943,-44.1574097985167,
123.856190907026)) ;
#49052 = CARTESIAN_POINT('Ctrl Pts',(-20.8107661786076,-43.9774207181539,
123.967284902334)) ;
#49053 = CARTESIAN_POINT('Ctrl Pts',(-20.5907535668492,-44.1674706734111,
123.653482764697)) ;
#49054 = CARTESIAN_POINT('Ctrl Pts',(-20.8861267321908,-43.9874815930482,
123.713900101275)) ;
#49055 = CARTESIAN_POINT('Ctrl Pts',(-20.6146904777119,-44.1773095767404,
123.447994903833)) ;
#49056 = CARTESIAN_POINT('Ctrl Pts',(-20.9160480543138,-43.9973204963776,
123.457038808334)) ;
#49057 = CARTESIAN_POINT('Ctrl Pts',(-20.6025093175598,-44.1873779531143,
123.236711105022)) ;
#49058 = CARTESIAN_POINT('Ctrl Pts',(-20.9008215569112,-44.0073888727515,
123.192934464757)) ;
#49059 = CARTESIAN_POINT('Ctrl Pts',(-20.5546520539257,-44.197258569747,123.034546463508)) ;
#49060 = CARTESIAN_POINT('Ctrl Pts',(-20.8409996767229,-44.0172694893841,
122.940227571329)) ;
#49061 = CARTESIAN_POINT('Ctrl Pts',(-20.4719127587511,-44.207249729976,122.841516718461)) ;
#49062 = CARTESIAN_POINT('Ctrl Pts',(-20.7375752826336,-44.0272606496131,
122.698940269794)) ;
#49063 = CARTESIAN_POINT('Ctrl Pts',(-20.3573466961592,-44.2172028034081,
122.666384942682)) ;
#49064 = CARTESIAN_POINT('Ctrl Pts',(-20.5943672382838,-44.0372137230452,
122.480025241818)) ;
#49065 = CARTESIAN_POINT('Ctrl Pts',(-20.2129041498641,-44.2272386390207,
122.512619796291)) ;
#49066 = CARTESIAN_POINT('Ctrl Pts',(-20.413814021043,-44.0472495586578,122.28781904818)) ;
#49067 = CARTESIAN_POINT('Ctrl Pts',(-20.0464710387891,-44.2371287657509,
122.387973352536)) ;
#49068 = CARTESIAN_POINT('Ctrl Pts',(-20.2057716275745,-44.057139685388,122.132010547474)) ;
#49069 = CARTESIAN_POINT('Ctrl Pts',(-19.8591825427843,-44.2471209475202,
122.292859773078)) ;
#49070 = CARTESIAN_POINT('Ctrl Pts',(-19.9716606492844,-44.0671318671573,
122.013118819397)) ;
#49071 = CARTESIAN_POINT('Ctrl Pts',(-19.6591233355574,-44.2570668874946,
122.232057906524)) ;
#49072 = CARTESIAN_POINT('Ctrl Pts',(-19.721585969689,-44.0770778071318,121.93711664901)) ;
#49073 = CARTESIAN_POINT('Ctrl Pts',(-19.4515603480813,-44.2670140712541,
122.206490694919)) ;
#49074 = CARTESIAN_POINT('Ctrl Pts',(-19.4621316011703,-44.0870249908912,
121.905158079447)) ;
#49075 = CARTESIAN_POINT('Ctrl Pts',(-19.2406254966303,-44.2770620095444,
122.217696911722)) ;
#49076 = CARTESIAN_POINT('Ctrl Pts',(-19.1984633098486,-44.0970729291816,
121.91916626143)) ;
#49077 = CARTESIAN_POINT('Ctrl Pts',(-19.0388958129296,-44.286909644358,122.264239155619)) ;
#49078 = CARTESIAN_POINT('Ctrl Pts',(-18.9462999517132,-44.1069205639951,
121.977344862777)) ;
#49079 = CARTESIAN_POINT('Ctrl Pts',(-18.8458583821311,-44.296871358056,122.345428988857)) ;
#49080 = CARTESIAN_POINT('Ctrl Pts',(-18.7050030349617,-44.1168822776931,
122.078833023626)) ;
#49081 = CARTESIAN_POINT('Ctrl Pts',(-18.6687933154075,-44.3068999938771,
122.459902791905)) ;
#49082 = CARTESIAN_POINT('Ctrl Pts',(-18.4836721334991,-44.1269109135143,
122.221925767037)) ;
#49083 = CARTESIAN_POINT('Ctrl Pts',(-18.5160880962946,-44.3168103086289,
122.601623849684)) ;
#49084 = CARTESIAN_POINT('Ctrl Pts',(-18.2927904240574,-44.136821228266,122.39907817817)) ;
#49085 = CARTESIAN_POINT('Ctrl Pts',(-18.3895506603922,-44.3267451792916,
122.767800295044)) ;
#49086 = CARTESIAN_POINT('Ctrl Pts',(-18.1346189321038,-44.1467560989287,
122.60679979726)) ;
#49087 = CARTESIAN_POINT('Ctrl Pts',(-18.2929514113174,-44.3367863616933,
122.955488189601)) ;
#49088 = CARTESIAN_POINT('Ctrl Pts',(-18.0138706731733,-44.1567972813305,
122.841409864127)) ;
#49089 = CARTESIAN_POINT('Ctrl Pts',(-18.2312003577601,-44.3466733331581,
123.153977478668)) ;
#49090 = CARTESIAN_POINT('Ctrl Pts',(-17.9366823755265,-44.1666842527952,
123.089522740013)) ;
#49091 = CARTESIAN_POINT('Ctrl Pts',(-18.2042924362549,-44.3566727654207,
123.362440492209)) ;
#49092 = CARTESIAN_POINT('Ctrl Pts',(-17.903048419426,-44.1766836850578,123.350101781409)) ;
#49093 = CARTESIAN_POINT('Ctrl Pts',(-18.2137740339436,-44.3665928306773,
123.5708007757)) ;
#49094 = CARTESIAN_POINT('Ctrl Pts',(-17.9149014701427,-44.1866037503144,
123.610552838708)) ;
#49095 = CARTESIAN_POINT('Ctrl Pts',(-18.2597764971867,-44.3766296832615,
123.776719598034)) ;
#49096 = CARTESIAN_POINT('Ctrl Pts',(-17.9724055290717,-44.1966406028986,
123.867950986159)) ;
#49097 = CARTESIAN_POINT('Ctrl Pts',(-18.3398426561002,-44.3865423426014,
123.969124187214)) ;
#49098 = CARTESIAN_POINT('Ctrl Pts',(-18.072489495965,-44.2065532622386,124.10845708331)) ;
#49099 = CARTESIAN_POINT('Ctrl Pts',(-18.4526095787518,-44.3965335545164,
124.146348677994)) ;
#49100 = CARTESIAN_POINT('Ctrl Pts',(-18.2134492761814,-44.2165444741535,
124.329987229818)) ;
#49101 = CARTESIAN_POINT('Ctrl Pts',(-18.5954817229628,-44.4065751959195,
124.301740665686)) ;
#49102 = CARTESIAN_POINT('Ctrl Pts',(-18.3920400927921,-44.2265861155566,
124.524226386298)) ;
#49103 = CARTESIAN_POINT('Ctrl Pts',(-18.7593291885529,-44.4164039901265,
124.427686436395)) ;
#49104 = CARTESIAN_POINT('Ctrl Pts',(-18.5968513118657,-44.2364149097636,
124.681658511536)) ;
#49105 = CARTESIAN_POINT('Ctrl Pts',(-18.9470682784548,-44.4264804012478,
124.525725017682)) ;
#49106 = CARTESIAN_POINT('Ctrl Pts',(-18.8315253713429,-44.2464913208849,
124.804205426187)) ;
#49107 = CARTESIAN_POINT('Ctrl Pts',(-19.1445330347221,-44.4363325342902,
124.588381426749)) ;
#49108 = CARTESIAN_POINT('Ctrl Pts',(-19.0783578845555,-44.2563434539274,
124.882525081973)) ;
#49109 = CARTESIAN_POINT('Ctrl Pts',(-19.3543837050247,-44.4464057686315,
124.616582421442)) ;
#49110 = CARTESIAN_POINT('Ctrl Pts',(-19.3406710042076,-44.2664166882687,
124.917774928891)) ;
#49111 = CARTESIAN_POINT('Ctrl Pts',(-19.561120757118,-44.4562472699582,124.608057607434)) ;
#49112 = CARTESIAN_POINT('Ctrl Pts',(-19.5990935689742,-44.2762581895953,
124.907117526406)) ;
#49113 = CARTESIAN_POINT('Ctrl Pts',(-19.7658378555304,-44.466208221553,124.564003318983)) ;
#49114 = CARTESIAN_POINT('Ctrl Pts',(-19.8549900005199,-44.2862191411901,
124.852048007979)) ;
#49115 = CARTESIAN_POINT('Ctrl Pts',(-19.9611338445933,-44.4762460392736,
124.484072288273)) ;
#49116 = CARTESIAN_POINT('Ctrl Pts',(-20.0991093096047,-44.2962569589108,
124.752132918042)) ;
#49117 = CARTESIAN_POINT('Ctrl Pts',(-20.1369108495217,-44.4861203885307,
124.373589262142)) ;
#49118 = CARTESIAN_POINT('Ctrl Pts',(-20.3188305768388,-44.3061313081678,
124.61402724624)) ;
#49119 = CARTESIAN_POINT('Ctrl Pts',(-20.2938275249447,-44.4961899392729,
124.231536291723)) ;
#49120 = CARTESIAN_POINT('Ctrl Pts',(-20.5149750943613,-44.31620085891,124.436460091646)) ;
#49121 = CARTESIAN_POINT('Ctrl Pts',(-20.4207811078669,-44.5060239587815,
124.068339987398)) ;
#49122 = CARTESIAN_POINT('Ctrl Pts',(-20.6736665782886,-44.3260348784186,
124.232462693714)) ;
#49123 = CARTESIAN_POINT('Ctrl Pts',(-20.5199150721139,-44.516058113361,123.882148162082)) ;
#49124 = CARTESIAN_POINT('Ctrl Pts',(-20.7975823820433,-44.3360690329981,
123.999722159393)) ;
#49125 = CARTESIAN_POINT('Ctrl Pts',(-20.5846066652837,-44.5260740391835,
123.68175257298)) ;
#49126 = CARTESIAN_POINT('Ctrl Pts',(-20.8784453196383,-44.3460849588206,
123.749227159064)) ;
#49127 = CARTESIAN_POINT('Ctrl Pts',(-20.6135027473333,-44.5359562943777,
123.476012739199)) ;
#49128 = CARTESIAN_POINT('Ctrl Pts',(-20.914563804666,-44.3559672140149,123.492051220715)) ;
#49129 = CARTESIAN_POINT('Ctrl Pts',(-20.6064192234333,-44.5459451008887,
123.266159254011)) ;
#49130 = CARTESIAN_POINT('Ctrl Pts',(-20.9057075528016,-44.3659560205258,
123.229734225039)) ;
#49131 = CARTESIAN_POINT('Ctrl Pts',(-20.5633248096925,-44.5558936681514,
123.061463359673)) ;
#49132 = CARTESIAN_POINT('Ctrl Pts',(-20.8518375941005,-44.3759045877885,
122.973864298052)) ;
#49133 = CARTESIAN_POINT('Ctrl Pts',(-20.4843220668197,-44.5659484734534,
122.865422401674)) ;
#49134 = CARTESIAN_POINT('Ctrl Pts',(-20.7530825570645,-44.3859593930905,
122.728813985344)) ;
#49135 = CARTESIAN_POINT('Ctrl Pts',(-20.3753421768984,-44.575767256717,122.69010150794)) ;
#49136 = CARTESIAN_POINT('Ctrl Pts',(-20.616855401469,-44.3957781763541,122.509662800884)) ;
#49137 = CARTESIAN_POINT('Ctrl Pts',(-20.2349634944572,-44.5858030290775,
122.532602841201)) ;
#49138 = CARTESIAN_POINT('Ctrl Pts',(-20.4413805689007,-44.4058139487147,
122.312790934125)) ;
#49139 = CARTESIAN_POINT('Ctrl Pts',(-20.0691703030276,-44.5958277281062,
122.402480939027)) ;
#49140 = CARTESIAN_POINT('Ctrl Pts',(-20.2341379246685,-44.4158386477433,
122.150140067367)) ;
#49141 = CARTESIAN_POINT('Ctrl Pts',(-19.8867241174746,-44.6056797313652,
122.304432926397)) ;
#49142 = CARTESIAN_POINT('Ctrl Pts',(-20.0060783372853,-44.4256906510024,
122.027581366541)) ;
#49143 = CARTESIAN_POINT('Ctrl Pts',(-19.6873786654677,-44.6156706657625,
122.238342902669)) ;
#49144 = CARTESIAN_POINT('Ctrl Pts',(-19.7568956897588,-44.4356815853996,
121.944970803461)) ;
#49145 = CARTESIAN_POINT('Ctrl Pts',(-19.481074169139,-44.6255885881936,122.207949395056)) ;
#49146 = CARTESIAN_POINT('Ctrl Pts',(-19.4990141869541,-44.4455995078307,
121.906980973465)) ;
#49147 = CARTESIAN_POINT('Ctrl Pts',(-19.2703469798628,-44.6356169438759,
122.213857027712)) ;
#49148 = CARTESIAN_POINT('Ctrl Pts',(-19.2356052976764,-44.455627863513,121.914367687928)) ;
#49149 = CARTESIAN_POINT('Ctrl Pts',(-19.0667685393293,-44.6455012283865,
122.255560649441)) ;
#49150 = CARTESIAN_POINT('Ctrl Pts',(-18.9811319610234,-44.4655121480236,
121.966499520298)) ;
#49151 = CARTESIAN_POINT('Ctrl Pts',(-18.8712365177251,-44.6554939122944,
122.332371985697)) ;
#49152 = CARTESIAN_POINT('Ctrl Pts',(-18.7367176525546,-44.4755048319315,
122.06251590164)) ;
#49153 = CARTESIAN_POINT('Ctrl Pts',(-18.6915565635913,-44.6655226493021,
122.442678617086)) ;
#49154 = CARTESIAN_POINT('Ctrl Pts',(-18.5121188960608,-44.4855335689392,
122.20040107881)) ;
#49155 = CARTESIAN_POINT('Ctrl Pts',(-18.5358279806812,-44.675408045931,122.580307301666)) ;
#49156 = CARTESIAN_POINT('Ctrl Pts',(-18.3174591681186,-44.4954189655681,
122.372439116343)) ;
#49157 = CARTESIAN_POINT('Ctrl Pts',(-18.4048030817091,-44.6853959313449,
122.74436173368)) ;
#49158 = CARTESIAN_POINT('Ctrl Pts',(-18.1536797930773,-44.505406850982,122.577508760622)) ;
#49159 = CARTESIAN_POINT('Ctrl Pts',(-18.3045194431609,-44.6953466340055,
122.927987236834)) ;
#49160 = CARTESIAN_POINT('Ctrl Pts',(-18.0283271818904,-44.5153575536426,
122.807042074314)) ;
#49161 = CARTESIAN_POINT('Ctrl Pts',(-18.2371653977238,-44.7053869521029,
123.128009185341)) ;
#49162 = CARTESIAN_POINT('Ctrl Pts',(-17.9441368874462,-44.52539787174,123.057070192369)) ;
#49163 = CARTESIAN_POINT('Ctrl Pts',(-18.2058765293099,-44.7152615174361,
123.333255667552)) ;
#49164 = CARTESIAN_POINT('Ctrl Pts',(-17.9050280766287,-44.5352724370732,
123.313629339727)) ;
#49165 = CARTESIAN_POINT('Ctrl Pts',(-18.2104928246588,-44.7252611774972,
123.543394996734)) ;
#49166 = CARTESIAN_POINT('Ctrl Pts',(-17.9108009163294,-44.5452720971343,
123.576303554644)) ;
#49167 = CARTESIAN_POINT('Ctrl Pts',(-18.2509713151308,-44.7351701726649,
123.747780176754)) ;
#49168 = CARTESIAN_POINT('Ctrl Pts',(-17.9614015776546,-44.555181092302,123.831785012484)) ;
#49169 = CARTESIAN_POINT('Ctrl Pts',(-18.3274676749511,-44.7452249138281,
123.944798878115)) ;
#49170 = CARTESIAN_POINT('Ctrl Pts',(-18.0570243118767,-44.5652358334653,
124.078057381489)) ;
#49171 = CARTESIAN_POINT('Ctrl Pts',(-18.4347054519244,-44.7550835257419,
124.122200708846)) ;
#49172 = CARTESIAN_POINT('Ctrl Pts',(-18.1910740418543,-44.5750944453791,
124.299808917657)) ;
#49173 = CARTESIAN_POINT('Ctrl Pts',(-18.5738749657264,-44.7651516480213,
124.281638187706)) ;
#49174 = CARTESIAN_POINT('Ctrl Pts',(-18.3650377633451,-44.5851625676584,
124.499103963352)) ;
#49175 = CARTESIAN_POINT('Ctrl Pts',(-18.7351819980848,-44.7750071187245,
124.411700343814)) ;
#49176 = CARTESIAN_POINT('Ctrl Pts',(-18.5666736485935,-44.5950180383616,
124.661680062319)) ;
#49177 = CARTESIAN_POINT('Ctrl Pts',(-18.9188616429352,-44.7850019782178,
124.513733292732)) ;
#49178 = CARTESIAN_POINT('Ctrl Pts',(-18.7962745857909,-44.605012897855,124.789218966965)) ;
#49179 = CARTESIAN_POINT('Ctrl Pts',(-19.1183492113281,-44.7950332315598,
124.58214803004)) ;
#49180 = CARTESIAN_POINT('Ctrl Pts',(-19.0456348868395,-44.6150441511969,
124.874734939455)) ;
#49181 = CARTESIAN_POINT('Ctrl Pts',(-19.323218690417,-44.8048999304329,124.61467366931)) ;
#49182 = CARTESIAN_POINT('Ctrl Pts',(-19.3017226630708,-44.62491085007,124.915389460278)) ;
#49183 = CARTESIAN_POINT('Ctrl Pts',(-19.5331246188192,-44.8148867461841,
124.61143594484)) ;
#49184 = CARTESIAN_POINT('Ctrl Pts',(-19.5641051552104,-44.6348976658212,
124.911339609303)) ;
#49185 = CARTESIAN_POINT('Ctrl Pts',(-19.7385308241501,-44.8248339513795,
124.572042427275)) ;
#49186 = CARTESIAN_POINT('Ctrl Pts',(-19.8208626335505,-44.6448448710167,
124.862095013778)) ;
#49187 = CARTESIAN_POINT('Ctrl Pts',(-19.9357852330403,-44.8348769395058,
124.496793289442)) ;
#49188 = CARTESIAN_POINT('Ctrl Pts',(-20.0674296681808,-44.6548878591429,
124.76803108169)) ;
#49189 = CARTESIAN_POINT('Ctrl Pts',(-20.1138908734245,-44.8447442941273,
124.39042646345)) ;
#49190 = CARTESIAN_POINT('Ctrl Pts',(-20.2900606909374,-44.6647552137644,
124.635070010698)) ;
#49191 = CARTESIAN_POINT('Ctrl Pts',(-20.2727462782933,-44.8547101874254,
124.25383373658)) ;
#49192 = CARTESIAN_POINT('Ctrl Pts',(-20.4886282483647,-44.6747211070625,
124.464326907893)) ;
#49193 = CARTESIAN_POINT('Ctrl Pts',(-20.4060875110616,-44.8647339648015,
124.090636353554)) ;
#49194 = CARTESIAN_POINT('Ctrl Pts',(-20.6553026894128,-44.6847448844386,
124.260328412907)) ;
#49195 = CARTESIAN_POINT('Ctrl Pts',(-20.5080877736395,-44.8746595127332,
123.908610854612)) ;
#49196 = CARTESIAN_POINT('Ctrl Pts',(-20.7828007334005,-44.6946704323703,
124.032794984382)) ;
#49197 = CARTESIAN_POINT('Ctrl Pts',(-20.5775102693516,-44.8845999891542,
123.711485460031)) ;
#49198 = CARTESIAN_POINT('Ctrl Pts',(-20.8695762747895,-44.7046109087913,
123.786387153745)) ;
#49199 = CARTESIAN_POINT('Ctrl Pts',(-20.6117719571326,-44.8946461988171,
123.503092758623)) ;
#49200 = CARTESIAN_POINT('Ctrl Pts',(-20.912400649323,-44.7146571184542,123.525895807852)) ;
#49201 = CARTESIAN_POINT('Ctrl Pts',(-20.6095960962421,-44.9045074554789,
123.295771336016)) ;
#49202 = CARTESIAN_POINT('Ctrl Pts',(-20.9096780311405,-44.724518375116,123.26674378884)) ;
#49203 = CARTESIAN_POINT('Ctrl Pts',(-20.5713071076348,-44.9145010837542,
123.08922311595)) ;
#49204 = CARTESIAN_POINT('Ctrl Pts',(-20.8618140135343,-44.7345120033913,
123.008558951118)) ;
#49205 = CARTESIAN_POINT('Ctrl Pts',(-20.4983191373996,-44.9244264810644,
122.893708018613)) ;
#49206 = CARTESIAN_POINT('Ctrl Pts',(-20.7705763697433,-44.7444374007015,
122.764165937578)) ;
#49207 = CARTESIAN_POINT('Ctrl Pts',(-20.391433863342,-44.9344543889746,122.712025942917)) ;
#49208 = CARTESIAN_POINT('Ctrl Pts',(-20.6369673169243,-44.7544653086117,
122.537064718162)) ;
#49209 = CARTESIAN_POINT('Ctrl Pts',(-20.2566836205498,-44.9443407046438,
122.55374389634)) ;
#49210 = CARTESIAN_POINT('Ctrl Pts',(-20.4685272889073,-44.7643516242809,
122.33921389434)) ;
#49211 = CARTESIAN_POINT('Ctrl Pts',(-20.0942650307571,-44.9543722995476,
122.419270807689)) ;
#49212 = CARTESIAN_POINT('Ctrl Pts',(-20.2655021977993,-44.7743832191847,
122.171124667766)) ;
#49213 = CARTESIAN_POINT('Ctrl Pts',(-19.9137299172441,-44.9642545424993,
122.316394133528)) ;
#49214 = CARTESIAN_POINT('Ctrl Pts',(-20.0398318506451,-44.7842654621364,
122.042531241798)) ;
#49215 = CARTESIAN_POINT('Ctrl Pts',(-19.7146500331995,-44.9743140135291,
122.24510774136)) ;
#49216 = CARTESIAN_POINT('Ctrl Pts',(-19.790980965489,-44.7943249331663,121.953425884434)) ;
#49217 = CARTESIAN_POINT('Ctrl Pts',(-19.5101771870513,-44.9841804581923,
122.210176444507)) ;
#49218 = CARTESIAN_POINT('Ctrl Pts',(-19.5353894138272,-44.8041913778294,
121.909764540214)) ;
#49219 = CARTESIAN_POINT('Ctrl Pts',(-19.3006636334398,-44.994146582641,122.210628861832)) ;
#49220 = CARTESIAN_POINT('Ctrl Pts',(-19.2734974473692,-44.8141575022781,
121.910332881293)) ;
#49221 = CARTESIAN_POINT('Ctrl Pts',(-19.0931406754314,-45.0041768260321,
122.248023638702)) ;
#49222 = CARTESIAN_POINT('Ctrl Pts',(-19.0140941942044,-44.8241877456692,
121.957079096099)) ;
#49223 = CARTESIAN_POINT('Ctrl Pts',(-18.8978469326455,-45.0140698609852,
122.319615465346)) ;
#49224 = CARTESIAN_POINT('Ctrl Pts',(-18.7699778546539,-44.8340807806223,
122.04657166839)) ;
#49225 = CARTESIAN_POINT('Ctrl Pts',(-18.7150830259635,-45.024120775222,122.425627543441)) ;
#49226 = CARTESIAN_POINT('Ctrl Pts',(-18.5415249218624,-44.8441316948591,
122.179088598224)) ;
#49227 = CARTESIAN_POINT('Ctrl Pts',(-18.5560590605076,-45.0340106014466,
122.559577916951)) ;
#49228 = CARTESIAN_POINT('Ctrl Pts',(-18.3427444001931,-44.8540215210837,
122.346531093265)) ;
#49229 = CARTESIAN_POINT('Ctrl Pts',(-18.3758084791143,-45.0473454164935,
122.774344433157)) ;
#49230 = CARTESIAN_POINT('Ctrl Pts',(-18.1174461021876,-44.8673563361306,
122.614979487024)) ;
#49231 = CARTESIAN_POINT('Ctrl Pts',(-18.2567530669862,-45.060622507665,123.03030649385)) ;
#49232 = CARTESIAN_POINT('Ctrl Pts',(-17.9686335760902,-44.8806334273021,
122.934896659141)) ;
#49233 = CARTESIAN_POINT('Ctrl Pts',(-18.2079946984886,-45.0738707962633,
123.304511382558)) ;
#49234 = CARTESIAN_POINT('Ctrl Pts',(-17.9076731562678,-44.8938817159004,
123.277709414345)) ;
#49235 = CARTESIAN_POINT('Ctrl Pts',(-18.2078213156215,-45.0839256377574,
123.515872423413)) ;
#49236 = CARTESIAN_POINT('Ctrl Pts',(-17.9074623164892,-44.9039365573945,
123.541899571283)) ;
#49237 = CARTESIAN_POINT('Ctrl Pts',(-18.2432033461838,-45.0937566270649,
123.719534287493)) ;
#49238 = CARTESIAN_POINT('Ctrl Pts',(-17.9516919899064,-44.913767546702,123.796479325853)) ;
#49239 = CARTESIAN_POINT('Ctrl Pts',(-18.3149935437228,-45.1038331913881,
123.918803697903)) ;
#49240 = CARTESIAN_POINT('Ctrl Pts',(-18.0414310833544,-44.9238441110252,
124.045563596302)) ;
#49241 = CARTESIAN_POINT('Ctrl Pts',(-18.4179463690853,-45.1136825165221,
124.098479005577)) ;
#49242 = CARTESIAN_POINT('Ctrl Pts',(-18.1701298255741,-44.9336934361592,
124.270160085588)) ;
#49243 = CARTESIAN_POINT('Ctrl Pts',(-18.5971230912793,-45.1270305161593,
124.314496308919)) ;
#49244 = CARTESIAN_POINT('Ctrl Pts',(-18.3940753258795,-44.9470414357965,
124.540160290177)) ;
#49245 = CARTESIAN_POINT('Ctrl Pts',(-18.8849989168967,-45.1436152756959,
124.518050402463)) ;
#49246 = CARTESIAN_POINT('Ctrl Pts',(-18.7539725180923,-44.963626195333,124.794623795617)) ;
#49247 = CARTESIAN_POINT('Ctrl Pts',(-19.224601952066,-45.160183827044,124.611932790248)) ;
#49248 = CARTESIAN_POINT('Ctrl Pts',(-19.1783954643001,-44.9801947466811,
124.911954796591)) ;
#49249 = CARTESIAN_POINT('Ctrl Pts',(-19.5054327742707,-45.173543651863,124.613960046694)) ;
#49250 = CARTESIAN_POINT('Ctrl Pts',(-19.5295000394639,-44.9935545715001,
124.914496420765)) ;
#49251 = CARTESIAN_POINT('Ctrl Pts',(-19.7108114161679,-45.1834490606937,
124.579447586727)) ;
#49252 = CARTESIAN_POINT('Ctrl Pts',(-19.7862085515421,-45.0034599803308,
124.87135192276)) ;
#49253 = CARTESIAN_POINT('Ctrl Pts',(-19.9082218453753,-45.1934090872777,
124.509714834404)) ;
#49254 = CARTESIAN_POINT('Ctrl Pts',(-20.0329770475992,-45.0134200069148,
124.784181635824)) ;
#49255 = CARTESIAN_POINT('Ctrl Pts',(-20.1511287525541,-45.206666671463,124.372952742759)) ;
#49256 = CARTESIAN_POINT('Ctrl Pts',(-20.3365929403509,-45.0266775911001,
124.613239797289)) ;
#49257 = CARTESIAN_POINT('Ctrl Pts',(-20.4042739888879,-45.2233178829577,
124.12545280733)) ;
#49258 = CARTESIAN_POINT('Ctrl Pts',(-20.6530388478672,-45.0433288025948,
124.303846929761)) ;
#49259 = CARTESIAN_POINT('Ctrl Pts',(-20.5876289534092,-45.243236097068,123.743705041852)) ;
#49260 = CARTESIAN_POINT('Ctrl Pts',(-20.8822225928719,-45.0632470167051,
123.826665489803)) ;
#49261 = CARTESIAN_POINT('Ctrl Pts',(-20.630530145128,-45.2631138602888,123.323172796485)) ;
#49262 = CARTESIAN_POINT('Ctrl Pts',(-20.9358462100671,-45.0831247799259,
123.300999284693)) ;
#49263 = CARTESIAN_POINT('Ctrl Pts',(-20.5263138562725,-45.283126528076,122.910688719133)) ;
#49264 = CARTESIAN_POINT('Ctrl Pts',(-20.8055712371326,-45.1031374477131,
122.785395465323)) ;
#49265 = CARTESIAN_POINT('Ctrl Pts',(-20.2902208181443,-45.3029390507426,
122.561698389052)) ;
#49266 = CARTESIAN_POINT('Ctrl Pts',(-20.5104525719544,-45.1229499703797,
122.349160972193)) ;
#49267 = CARTESIAN_POINT('Ctrl Pts',(-19.9467946863038,-45.3229223507425,
122.31164395972)) ;
#49268 = CARTESIAN_POINT('Ctrl Pts',(-20.081167872577,-45.1429332703796,122.036595982268)) ;
#49269 = CARTESIAN_POINT('Ctrl Pts',(-19.5402451083145,-45.3428166278438,
122.194572866398)) ;
#49270 = CARTESIAN_POINT('Ctrl Pts',(-19.5729808270998,-45.1628275474809,
121.890260817414)) ;
#49271 = CARTESIAN_POINT('Ctrl Pts',(-19.1173631256665,-45.3627493896015,
122.222652545081)) ;
#49272 = CARTESIAN_POINT('Ctrl Pts',(-19.0443792388159,-45.1827603092387,
121.925363493254)) ;
#49273 = CARTESIAN_POINT('Ctrl Pts',(-18.7289083515365,-45.3827153953663,
122.393915397857)) ;
#49274 = CARTESIAN_POINT('Ctrl Pts',(-18.5588123388653,-45.2027263150034,
122.139444767471)) ;
#49275 = CARTESIAN_POINT('Ctrl Pts',(-18.4233281728612,-45.4025939275311,
122.685968903404)) ;
#49276 = CARTESIAN_POINT('Ctrl Pts',(-18.1768400075753,-45.2226048471683,
122.504512707876)) ;
#49277 = CARTESIAN_POINT('Ctrl Pts',(-18.2348448265652,-45.4225335941915,
123.065690568163)) ;
#49278 = CARTESIAN_POINT('Ctrl Pts',(-17.9412382746725,-45.2425445138286,
122.979165174917)) ;
#49279 = CARTESIAN_POINT('Ctrl Pts',(-18.1872285477888,-45.4424284688368,
123.486065831409)) ;
#49280 = CARTESIAN_POINT('Ctrl Pts',(-17.8817201357155,-45.262439388474,123.504633155352)) ;
#49281 = CARTESIAN_POINT('Ctrl Pts',(-18.2855438839301,-45.4623356081302,
123.897669851793)) ;
#49282 = CARTESIAN_POINT('Ctrl Pts',(-18.0046155637013,-45.2823465277673,
124.019136501102)) ;
#49283 = CARTESIAN_POINT('Ctrl Pts',(-18.5179787925655,-45.4822461562087,
124.251671884329)) ;
#49284 = CARTESIAN_POINT('Ctrl Pts',(-18.2951592685282,-45.3022570758458,
124.461637555377)) ;
#49285 = CARTESIAN_POINT('Ctrl Pts',(-18.8603532025877,-45.5023147415659,
124.506196821107)) ;
#49286 = CARTESIAN_POINT('Ctrl Pts',(-18.7231289192442,-45.322325661203,124.779793280886)) ;
#49287 = CARTESIAN_POINT('Ctrl Pts',(-19.2632916538043,-45.5220965388806,
124.627332831793)) ;
#49288 = CARTESIAN_POINT('Ctrl Pts',(-19.2267990765381,-45.3421074585177,
124.931211593154)) ;
#49289 = CARTESIAN_POINT('Ctrl Pts',(-19.6879024854321,-45.5421040858251,
124.604065554752)) ;
#49290 = CARTESIAN_POINT('Ctrl Pts',(-19.7575625515052,-45.3621150054623,
124.902127405188)) ;
#49291 = CARTESIAN_POINT('Ctrl Pts',(-20.0757175915424,-45.561925824128,124.438753736194)) ;
#49292 = CARTESIAN_POINT('Ctrl Pts',(-20.2423289587424,-45.3819367437651,
124.695488931146)) ;
#49293 = CARTESIAN_POINT('Ctrl Pts',(-20.3866991980944,-45.5819058440321,
124.149413523319)) ;
#49294 = CARTESIAN_POINT('Ctrl Pts',(-20.6310564599377,-45.4019167636693,
124.333814619466)) ;
#49295 = CARTESIAN_POINT('Ctrl Pts',(-20.579213898747,-45.6018232952944,123.772183038511)) ;
#49296 = CARTESIAN_POINT('Ctrl Pts',(-20.8717000555941,-45.4218342149315,
123.862278018821)) ;
#49297 = CARTESIAN_POINT('Ctrl Pts',(-20.6323140250136,-45.6216982164671,
123.35290988801)) ;
#49298 = CARTESIAN_POINT('Ctrl Pts',(-20.9380767680918,-45.4417091361042,
123.338188475184)) ;
#49299 = CARTESIAN_POINT('Ctrl Pts',(-20.5381944095279,-45.6417225850179,
122.937699622663)) ;
#49300 = CARTESIAN_POINT('Ctrl Pts',(-20.8204289201312,-45.461733504655,122.819174893006)) ;
#49301 = CARTESIAN_POINT('Ctrl Pts',(-20.3096913478822,-45.6615892693914,
122.582336964708)) ;
#49302 = CARTESIAN_POINT('Ctrl Pts',(-20.5348026192168,-45.4816001890285,
122.374971928378)) ;
#49303 = CARTESIAN_POINT('Ctrl Pts',(-19.9728378596493,-45.6815330912376,
122.324818392206)) ;
#49304 = CARTESIAN_POINT('Ctrl Pts',(-20.113737828752,-45.5015440108747,122.053072103722)) ;
#49305 = CARTESIAN_POINT('Ctrl Pts',(-19.5689770807575,-45.7014404604891,
122.198058930962)) ;
#49306 = CARTESIAN_POINT('Ctrl Pts',(-19.6089136734289,-45.5214513801262,
121.894620584429)) ;
#49307 = CARTESIAN_POINT('Ctrl Pts',(-19.1467685091688,-45.7213151582358,
122.215906390113)) ;
#49308 = CARTESIAN_POINT('Ctrl Pts',(-19.0811541092211,-45.5413260778729,
121.916926618997)) ;
#49309 = CARTESIAN_POINT('Ctrl Pts',(-18.7538192203983,-45.7412971007575,
122.377543259028)) ;
#49310 = CARTESIAN_POINT('Ctrl Pts',(-18.5899663032709,-45.5613080203947,
122.11896949238)) ;
#49311 = CARTESIAN_POINT('Ctrl Pts',(-18.4411535486972,-45.7611997676684,
122.662651717635)) ;
#49312 = CARTESIAN_POINT('Ctrl Pts',(-18.1991325996576,-45.5812106873055,
122.475351878754)) ;
#49313 = CARTESIAN_POINT('Ctrl Pts',(-18.2438603449424,-45.7810551252071,
123.035964325074)) ;
#49314 = CARTESIAN_POINT('Ctrl Pts',(-17.9525130136247,-45.6010660448442,
122.94198968938)) ;
#49315 = CARTESIAN_POINT('Ctrl Pts',(-18.1856815046609,-45.8011191639231,
123.458527247341)) ;
#49316 = CARTESIAN_POINT('Ctrl Pts',(-17.8797853306708,-45.6211300835602,
123.470193368152)) ;
#49317 = CARTESIAN_POINT('Ctrl Pts',(-18.2744755391468,-45.8209743436481,
123.871419259032)) ;
#49318 = CARTESIAN_POINT('Ctrl Pts',(-17.9907738386166,-45.6409852632853,
123.986308188026)) ;
#49319 = CARTESIAN_POINT('Ctrl Pts',(-18.4997930018078,-45.8409544483126,
124.231383616986)) ;
#49320 = CARTESIAN_POINT('Ctrl Pts',(-18.2724161799833,-45.6609653679497,
124.436265927067)) ;
#49321 = CARTESIAN_POINT('Ctrl Pts',(-18.8314673108359,-45.8607635534824,
124.49118909027)) ;
#49322 = CARTESIAN_POINT('Ctrl Pts',(-18.6870078952182,-45.6807744731195,
124.761025281335)) ;
#49323 = CARTESIAN_POINT('Ctrl Pts',(-19.2352299421936,-45.8807561738231,
124.623756846675)) ;
#49324 = CARTESIAN_POINT('Ctrl Pts',(-19.1916999501427,-45.7007670934602,
124.926741074859)) ;
#49325 = CARTESIAN_POINT('Ctrl Pts',(-19.586815630739,-45.8972956563272,124.612921446625)) ;
#49326 = CARTESIAN_POINT('Ctrl Pts',(-19.6312118173371,-45.7173065759643,
124.913196409966)) ;
#49327 = CARTESIAN_POINT('Ctrl Pts',(-19.8558718361537,-45.9106599743914,
124.532044526927)) ;
#49328 = CARTESIAN_POINT('Ctrl Pts',(-19.9674993568783,-45.7306708940285,
124.812112387644)) ;
#49329 = CARTESIAN_POINT('Ctrl Pts',(-20.1042094269978,-45.9238775768929,
124.407362624785)) ;
#49330 = CARTESIAN_POINT('Ctrl Pts',(-20.2779790594621,-45.74388849653,124.656227492421)) ;
#49331 = CARTESIAN_POINT('Ctrl Pts',(-20.368961477355,-45.9405351711707,124.172135837994)) ;
#49332 = CARTESIAN_POINT('Ctrl Pts',(-20.6088613725694,-45.7605460908078,
124.362235325753)) ;
#49333 = CARTESIAN_POINT('Ctrl Pts',(-20.5701552804557,-45.9604008732124,
123.800652640584)) ;
#49334 = CARTESIAN_POINT('Ctrl Pts',(-20.8603771681575,-45.7804117928495,
123.897882285973)) ;
#49335 = CARTESIAN_POINT('Ctrl Pts',(-20.6228240088762,-45.9770305999024,
123.451100482239)) ;
#49336 = CARTESIAN_POINT('Ctrl Pts',(-20.9262145451772,-45.7970415195396,
123.460911151536)) ;
#49337 = CARTESIAN_POINT('Ctrl Pts',(-20.5914361189551,-45.9903197150403,
123.173415800151)) ;
#49338 = CARTESIAN_POINT('Ctrl Pts',(-20.8869828199733,-45.8103306346774,
123.113835882224)) ;
#49339 = CARTESIAN_POINT('Ctrl Pts',(-20.5323594467668,-46.0002840620174,
122.972457040269)) ;
#49340 = CARTESIAN_POINT('Ctrl Pts',(-20.813137221631,-45.8202949816545,122.862628158048)) ;
#49341 = CARTESIAN_POINT('Ctrl Pts',(-20.4397374973719,-46.0102124300189,
122.785404683368)) ;
#49342 = CARTESIAN_POINT('Ctrl Pts',(-20.6973720958994,-45.830223349656,122.628822672111)) ;
#49343 = CARTESIAN_POINT('Ctrl Pts',(-20.2747057487913,-46.0234958631076,
122.560148912213)) ;
#49344 = CARTESIAN_POINT('Ctrl Pts',(-20.491036246019,-45.8435067827447,122.347203200446)) ;
#49345 = CARTESIAN_POINT('Ctrl Pts',(-19.9984819879349,-46.0401479408479,
122.338567938627)) ;
#49346 = CARTESIAN_POINT('Ctrl Pts',(-20.145826084982,-45.8601588604851,122.070280119537)) ;
#49347 = CARTESIAN_POINT('Ctrl Pts',(-19.6654083029669,-46.0566993101488,
122.225111293764)) ;
#49348 = CARTESIAN_POINT('Ctrl Pts',(-19.7294257177558,-45.8767102297859,
121.928426697341)) ;
#49349 = CARTESIAN_POINT('Ctrl Pts',(-19.3866709636188,-46.0699867382977,
122.205956450198)) ;
#49350 = CARTESIAN_POINT('Ctrl Pts',(-19.3810452958569,-45.8899976579349,
121.904492705596)) ;
#49351 = CARTESIAN_POINT('Ctrl Pts',(-19.1767289526485,-46.0800312779978,
122.228493274204)) ;
#49352 = CARTESIAN_POINT('Ctrl Pts',(-19.1186091401649,-45.900042197635,121.932658291026)) ;
#49353 = CARTESIAN_POINT('Ctrl Pts',(-18.9778591393557,-46.0898741198217,
122.285724273761)) ;
#49354 = CARTESIAN_POINT('Ctrl Pts',(-18.8700233535146,-45.9098850394588,
122.00419504513)) ;
#49355 = CARTESIAN_POINT('Ctrl Pts',(-18.7890949169887,-46.0998584040686,
122.37747258679)) ;
#49356 = CARTESIAN_POINT('Ctrl Pts',(-18.6340661750229,-45.9198693237057,
122.118877741184)) ;
#49357 = CARTESIAN_POINT('Ctrl Pts',(-18.6197187705816,-46.1098080494678,
122.500228764062)) ;
#49358 = CARTESIAN_POINT('Ctrl Pts',(-18.4223444457942,-45.9298189691049,
122.272320772615)) ;
#49359 = CARTESIAN_POINT('Ctrl Pts',(-18.4733104190095,-46.1198078111562,
122.651108437036)) ;
#49360 = CARTESIAN_POINT('Ctrl Pts',(-18.2393318883207,-45.9398187307933,
122.460918444187)) ;
#49361 = CARTESIAN_POINT('Ctrl Pts',(-18.3552472327061,-46.1298391571151,
122.825850445849)) ;
#49362 = CARTESIAN_POINT('Ctrl Pts',(-18.0917505487203,-45.9498500767522,
122.679344429148)) ;
#49363 = CARTESIAN_POINT('Ctrl Pts',(-18.2705494607926,-46.1396941115922,
123.014933391385)) ;
#49364 = CARTESIAN_POINT('Ctrl Pts',(-17.9858757132729,-45.9597050312293,
122.915697062005)) ;
#49365 = CARTESIAN_POINT('Ctrl Pts',(-18.2188977661992,-46.1496666495927,
123.218103084829)) ;
#49366 = CARTESIAN_POINT('Ctrl Pts',(-17.9213083460971,-45.9696775692299,
123.1696585988)) ;
#49367 = CARTESIAN_POINT('Ctrl Pts',(-18.2032838337834,-46.1596616433277,
123.427680803576)) ;
#49368 = CARTESIAN_POINT('Ctrl Pts',(-17.9017881316978,-45.9796725629648,
123.43163061832)) ;
#49369 = CARTESIAN_POINT('Ctrl Pts',(-18.2246312081846,-46.1696957021218,
123.637527281541)) ;
#49370 = CARTESIAN_POINT('Ctrl Pts',(-17.9284695515831,-45.9897066217589,
123.693939039804)) ;
#49371 = CARTESIAN_POINT('Ctrl Pts',(-18.2807599390842,-46.1795510449448,
123.836991427032)) ;
#49372 = CARTESIAN_POINT('Ctrl Pts',(-17.9986278342862,-45.9995619645819,
123.943270201395)) ;
#49373 = CARTESIAN_POINT('Ctrl Pts',(-18.3717042160913,-46.1895505242904,
124.026480311802)) ;
#49374 = CARTESIAN_POINT('Ctrl Pts',(-18.1123057056934,-46.0095614439275,
124.180132595263)) ;
#49375 = CARTESIAN_POINT('Ctrl Pts',(-18.4927341945723,-46.1994449730457,
124.195705746537)) ;
#49376 = CARTESIAN_POINT('Ctrl Pts',(-18.2635910838762,-46.0194558926828,
124.391666206078)) ;
#49377 = CARTESIAN_POINT('Ctrl Pts',(-18.6438307854289,-46.2095080924802,
124.343730651591)) ;
#49378 = CARTESIAN_POINT('Ctrl Pts',(-18.4524598572534,-46.0295190121173,
124.576699295059)) ;
#49379 = CARTESIAN_POINT('Ctrl Pts',(-18.8143876956358,-46.2193477377214,
124.460844662452)) ;
#49380 = CARTESIAN_POINT('Ctrl Pts',(-18.6656547763294,-46.0393586573585,
124.723094304069)) ;
#49381 = CARTESIAN_POINT('Ctrl Pts',(-19.0067961425218,-46.2294109019075,
124.548731031768)) ;
#49382 = CARTESIAN_POINT('Ctrl Pts',(-18.9061641632514,-46.0494218215446,
124.832954725746)) ;
#49383 = CARTESIAN_POINT('Ctrl Pts',(-19.2082002254343,-46.2393051716563,
124.60082520619)) ;
#49384 = CARTESIAN_POINT('Ctrl Pts',(-19.1579188977088,-46.0593160912934,
124.898075179652)) ;
#49385 = CARTESIAN_POINT('Ctrl Pts',(-19.4164887508991,-46.2492468976701,
124.617795648775)) ;
#49386 = CARTESIAN_POINT('Ctrl Pts',(-19.4182795982721,-46.0692578173072,
124.919290922679)) ;
#49387 = CARTESIAN_POINT('Ctrl Pts',(-19.625908760725,-46.2592497863295,124.598307790084)) ;
#49388 = CARTESIAN_POINT('Ctrl Pts',(-19.6800549445947,-46.0792607059666,
124.894933738321)) ;
#49389 = CARTESIAN_POINT('Ctrl Pts',(-19.8293605211461,-46.2692896351235,
124.542189850238)) ;
#49390 = CARTESIAN_POINT('Ctrl Pts',(-19.9343703358343,-46.0893005547606,
124.824788939864)) ;
#49391 = CARTESIAN_POINT('Ctrl Pts',(-20.0161177451334,-46.2791138505843,
124.453953136808)) ;
#49392 = CARTESIAN_POINT('Ctrl Pts',(-20.1678185633982,-46.0991247702215,
124.714495173511)) ;
#49393 = CARTESIAN_POINT('Ctrl Pts',(-20.1888529807882,-46.2891706940779,
124.332063949481)) ;
#49394 = CARTESIAN_POINT('Ctrl Pts',(-20.3837390423242,-46.109181613715,124.562135863679)) ;
#49395 = CARTESIAN_POINT('Ctrl Pts',(-20.3357237419567,-46.2990993034739,
124.183735609964)) ;
#49396 = CARTESIAN_POINT('Ctrl Pts',(-20.5673296043918,-46.119110223111,124.376727071012)) ;
#49397 = CARTESIAN_POINT('Ctrl Pts',(-20.4553698807106,-46.3090511875118,
124.012092768846)) ;
#49398 = CARTESIAN_POINT('Ctrl Pts',(-20.7168895335636,-46.1290621071489,
124.162174744986)) ;
#49399 = CARTESIAN_POINT('Ctrl Pts',(-20.5439344328811,-46.3191041403194,
123.820215375579)) ;
#49400 = CARTESIAN_POINT('Ctrl Pts',(-20.8275975547341,-46.1391150599565,
123.922329195858)) ;
#49401 = CARTESIAN_POINT('Ctrl Pts',(-20.5969834126444,-46.3289270167856,
123.620621819729)) ;
#49402 = CARTESIAN_POINT('Ctrl Pts',(-20.8939114402365,-46.1489379364227,
123.672837152796)) ;
#49403 = CARTESIAN_POINT('Ctrl Pts',(-20.6153551246027,-46.3389827493557,
123.41003275426)) ;
#49404 = CARTESIAN_POINT('Ctrl Pts',(-20.9168785394599,-46.1589936689928,
123.409601144836)) ;
#49405 = CARTESIAN_POINT('Ctrl Pts',(-20.5967235165246,-46.3489235143433,
123.201871132053)) ;
#49406 = CARTESIAN_POINT('Ctrl Pts',(-20.893591540016,-46.1689344339805,123.149398558187)) ;
#49407 = CARTESIAN_POINT('Ctrl Pts',(-20.5430611916777,-46.358827847249,123.000680696278)) ;
#49408 = CARTESIAN_POINT('Ctrl Pts',(-20.8265158340173,-46.1788387668861,
122.89790937762)) ;
#49409 = CARTESIAN_POINT('Ctrl Pts',(-20.4539067996073,-46.3688745161297,
122.809226303737)) ;
#49410 = CARTESIAN_POINT('Ctrl Pts',(-20.7150751051334,-46.1888854357668,
122.658590446776)) ;
#49411 = CARTESIAN_POINT('Ctrl Pts',(-20.3348107304018,-46.3787700794355,
122.638612779929)) ;
#49412 = CARTESIAN_POINT('Ctrl Pts',(-20.5662066575866,-46.1987809990726,
122.445321690522)) ;
#49413 = CARTESIAN_POINT('Ctrl Pts',(-20.1854730789962,-46.3888321371358,
122.48883600952)) ;
#49414 = CARTESIAN_POINT('Ctrl Pts',(-20.379536426161,-46.2088430567729,122.258099155572)) ;
#49415 = CARTESIAN_POINT('Ctrl Pts',(-20.0161942508695,-46.3986749147633,
122.369786755293)) ;
#49416 = CARTESIAN_POINT('Ctrl Pts',(-20.1679385535702,-46.2186858344004,
122.109285146216)) ;
#49417 = CARTESIAN_POINT('Ctrl Pts',(-19.8262618796166,-46.4086653930151,
122.28019126902)) ;
#49418 = CARTESIAN_POINT('Ctrl Pts',(-19.9305238988353,-46.2286763126523,
121.997288664891)) ;
#49419 = CARTESIAN_POINT('Ctrl Pts',(-19.6248584878059,-46.4185943656587,
122.225294019457)) ;
#49420 = CARTESIAN_POINT('Ctrl Pts',(-19.6787697821799,-46.2386052852958,
121.928664786175)) ;
#49421 = CARTESIAN_POINT('Ctrl Pts',(-19.4157226032529,-46.4285855025382,
122.205756739938)) ;
#49422 = CARTESIAN_POINT('Ctrl Pts',(-19.4173499655239,-46.2485964221754,
121.904240994676)) ;
#49423 = CARTESIAN_POINT('Ctrl Pts',(-19.2057405057304,-46.4386076200272,
122.223135749663)) ;
#49424 = CARTESIAN_POINT('Ctrl Pts',(-19.1548721753511,-46.2586185396643,
121.92596250925)) ;
#49425 = CARTESIAN_POINT('Ctrl Pts',(-19.0043894905299,-46.4485081304294,
122.275869896389)) ;
#49426 = CARTESIAN_POINT('Ctrl Pts',(-18.9031822162054,-46.2685190500665,
121.991878228814)) ;
#49427 = CARTESIAN_POINT('Ctrl Pts',(-18.813429020907,-46.4584971231755,122.363241063598)) ;
#49428 = CARTESIAN_POINT('Ctrl Pts',(-18.6644805817943,-46.2785080428126,
122.101090338779)) ;
#49429 = CARTESIAN_POINT('Ctrl Pts',(-18.6410397094411,-46.4684623672261,
122.482274292673)) ;
#49430 = CARTESIAN_POINT('Ctrl Pts',(-18.4489924497402,-46.2884732868632,
122.249880282488)) ;
#49431 = CARTESIAN_POINT('Ctrl Pts',(-18.4924874516743,-46.4783666317393,
122.62819862701)) ;
#49432 = CARTESIAN_POINT('Ctrl Pts',(-18.2633002251361,-46.2983775513764,
122.43228474134)) ;
#49433 = CARTESIAN_POINT('Ctrl Pts',(-18.3697789016585,-46.4884247234375,
122.800382922365)) ;
#49434 = CARTESIAN_POINT('Ctrl Pts',(-18.1099129937586,-46.3084356430746,
122.64751373004)) ;
#49435 = CARTESIAN_POINT('Ctrl Pts',(-18.2805605389299,-46.4982746638659,
122.987267125253)) ;
#49436 = CARTESIAN_POINT('Ctrl Pts',(-17.9983877780156,-46.318285583503,122.881119052211)) ;
#49437 = CARTESIAN_POINT('Ctrl Pts',(-18.2236525306218,-46.5083016750394,
123.190235923869)) ;
#49438 = CARTESIAN_POINT('Ctrl Pts',(-17.9272509867176,-46.3283125946766,
123.13482951254)) ;
#49439 = CARTESIAN_POINT('Ctrl Pts',(-18.2033939632025,-46.5183302616515,
123.400103024954)) ;
#49440 = CARTESIAN_POINT('Ctrl Pts',(-17.901925769436,-46.3383411812886,123.397163125626)) ;
#49441 = CARTESIAN_POINT('Ctrl Pts',(-18.2191889497681,-46.5281754757642,
123.606465447685)) ;
#49442 = CARTESIAN_POINT('Ctrl Pts',(-17.9216676872438,-46.3481863954013,
123.655117412453)) ;
#49443 = CARTESIAN_POINT('Ctrl Pts',(-18.2707942324504,-46.5381662239437,
123.810069040328)) ;
#49444 = CARTESIAN_POINT('Ctrl Pts',(-17.9861726596863,-46.3581771435809,
123.909622518266)) ;
#49445 = CARTESIAN_POINT('Ctrl Pts',(-18.357794261464,-46.5482038575292,124.002323055344)) ;
#49446 = CARTESIAN_POINT('Ctrl Pts',(-18.0949209308514,-46.3682147771664,
124.149940691054)) ;
#49447 = CARTESIAN_POINT('Ctrl Pts',(-18.4742897524447,-46.5580491467421,
124.173407953581)) ;
#49448 = CARTESIAN_POINT('Ctrl Pts',(-18.2405394895734,-46.3780600663792,
124.363798772761)) ;
#49449 = CARTESIAN_POINT('Ctrl Pts',(-18.620370895161,-46.568030547548,124.324028601828)) ;
#49450 = CARTESIAN_POINT('Ctrl Pts',(-18.4231399414147,-46.3880414671851,
124.552075901713)) ;
#49451 = CARTESIAN_POINT('Ctrl Pts',(-18.7899363735675,-46.5779827805379,
124.44660926478)) ;
#49452 = CARTESIAN_POINT('Ctrl Pts',(-18.6350962163679,-46.397993700175,124.705303329863)) ;
#49453 = CARTESIAN_POINT('Ctrl Pts',(-18.9789812034734,-46.5879815919945,
124.538563788364)) ;
#49454 = CARTESIAN_POINT('Ctrl Pts',(-18.8714017008727,-46.4079925116317,
124.820247929086)) ;
#49455 = CARTESIAN_POINT('Ctrl Pts',(-19.1820191632644,-46.5980206959252,
124.596131546056)) ;
#49456 = CARTESIAN_POINT('Ctrl Pts',(-19.1251985398827,-46.4180316155623,
124.892209201477)) ;
#49457 = CARTESIAN_POINT('Ctrl Pts',(-19.3874680290362,-46.6078456383445,
124.617557565118)) ;
#49458 = CARTESIAN_POINT('Ctrl Pts',(-19.3820108279109,-46.4278565579816,
124.918993385592)) ;
#49459 = CARTESIAN_POINT('Ctrl Pts',(-19.5983341246022,-46.6179003258204,
124.602993200605)) ;
#49460 = CARTESIAN_POINT('Ctrl Pts',(-19.64559328927,-46.4379112454576,124.900789356719)) ;
#49461 = CARTESIAN_POINT('Ctrl Pts',(-19.8011174374927,-46.6278431281773,
124.552252454525)) ;
#49462 = CARTESIAN_POINT('Ctrl Pts',(-19.8990733415374,-46.4478540478144,
124.837364781521)) ;
#49463 = CARTESIAN_POINT('Ctrl Pts',(-19.9915187465345,-46.637746924117,124.467991218211)) ;
#49464 = CARTESIAN_POINT('Ctrl Pts',(-20.1370762828401,-46.4577578437542,
124.732039090923)) ;
#49465 = CARTESIAN_POINT('Ctrl Pts',(-20.166805154378,-46.6477937034921,124.350181343917)) ;
#49466 = CARTESIAN_POINT('Ctrl Pts',(-20.3561848751386,-46.4678046231292,
124.584777991393)) ;
#49467 = CARTESIAN_POINT('Ctrl Pts',(-20.3168442450622,-46.6576893617867,
124.20602634747)) ;
#49468 = CARTESIAN_POINT('Ctrl Pts',(-20.5437352889847,-46.4777002814238,
124.40458454613)) ;
#49469 = CARTESIAN_POINT('Ctrl Pts',(-20.4416202810829,-46.6677509290373,
124.035249876144)) ;
#49470 = CARTESIAN_POINT('Ctrl Pts',(-20.6997061794261,-46.4877618486744,
124.191114977027)) ;
#49471 = CARTESIAN_POINT('Ctrl Pts',(-20.5328807367812,-46.6775955734746,
123.849484643393)) ;
#49472 = CARTESIAN_POINT('Ctrl Pts',(-20.8137834732747,-46.4976064931117,
123.958907813317)) ;
#49473 = CARTESIAN_POINT('Ctrl Pts',(-20.5918946295246,-46.6875556197173,
123.64858424823)) ;
#49474 = CARTESIAN_POINT('Ctrl Pts',(-20.8875519244176,-46.5075665393544,
123.707782162122)) ;
#49475 = CARTESIAN_POINT('Ctrl Pts',(-20.6148993357899,-46.6975939157357,
123.43881520395)) ;
#49476 = CARTESIAN_POINT('Ctrl Pts',(-20.9163089327259,-46.5176048353728,
123.445571143073)) ;
#49477 = CARTESIAN_POINT('Ctrl Pts',(-20.6017530846061,-46.707467257154,123.231632331)) ;
#49478 = CARTESIAN_POINT('Ctrl Pts',(-20.8998770457403,-46.5274781767911,
123.186591367245)) ;
#49479 = CARTESIAN_POINT('Ctrl Pts',(-20.5517975292825,-46.7175403609533,
123.025882379625)) ;
#49480 = CARTESIAN_POINT('Ctrl Pts',(-20.8374336990215,-46.5375512805904,
122.92940409922)) ;
#49481 = CARTESIAN_POINT('Ctrl Pts',(-20.4692073505912,-46.7273611760722,
122.836612568494)) ;
#49482 = CARTESIAN_POINT('Ctrl Pts',(-20.7341962066025,-46.5473720957093,
122.692815045796)) ;
#49483 = CARTESIAN_POINT('Ctrl Pts',(-20.3522770027166,-46.7374380411502,
122.660005076197)) ;
#49484 = CARTESIAN_POINT('Ctrl Pts',(-20.5880342149854,-46.5574489607873,
122.472055591262)) ;
#49485 = CARTESIAN_POINT('Ctrl Pts',(-20.2094265317654,-46.7473027808054,
122.509626266143)) ;
#49486 = CARTESIAN_POINT('Ctrl Pts',(-20.4094709146945,-46.5673137004426,
122.28408059887)) ;
#49487 = CARTESIAN_POINT('Ctrl Pts',(-20.0403249054971,-46.7573251840468,
122.383941295046)) ;
#49488 = CARTESIAN_POINT('Ctrl Pts',(-20.1980943113753,-46.5773361036839,
122.126973882739)) ;
#49489 = CARTESIAN_POINT('Ctrl Pts',(-19.8516517065092,-46.7673509083353,
122.28995820191)) ;
#49490 = CARTESIAN_POINT('Ctrl Pts',(-19.962253273062,-46.5873618279724,122.009494285123)) ;
#49491 = CARTESIAN_POINT('Ctrl Pts',(-19.6531005041751,-46.7772056913566,
122.23083936213)) ;
#49492 = CARTESIAN_POINT('Ctrl Pts',(-19.7140632034375,-46.5972166109937,
121.935594664619)) ;
#49493 = CARTESIAN_POINT('Ctrl Pts',(-19.4447550366577,-46.7871845350798,
122.206249292003)) ;
#49494 = CARTESIAN_POINT('Ctrl Pts',(-19.453631099447,-46.607195454717,121.904856532763)) ;
#49495 = CARTESIAN_POINT('Ctrl Pts',(-19.2345000747721,-46.7972034273165,
122.218618665142)) ;
#49496 = CARTESIAN_POINT('Ctrl Pts',(-19.1908123744642,-46.6172143469536,
121.920317600805)) ;
#49497 = CARTESIAN_POINT('Ctrl Pts',(-19.0322268033516,-46.8070866363575,
122.266237363921)) ;
#49498 = CARTESIAN_POINT('Ctrl Pts',(-18.9379696064049,-46.6270975559946,
121.979840758629)) ;
#49499 = CARTESIAN_POINT('Ctrl Pts',(-18.8378107169686,-46.8171549456977,
122.349847749281)) ;
#49500 = CARTESIAN_POINT('Ctrl Pts',(-18.6949496716682,-46.6371658653348,
122.084353104064)) ;
#49501 = CARTESIAN_POINT('Ctrl Pts',(-18.6648606133521,-46.8269850710304,
122.463033827998)) ;
#49502 = CARTESIAN_POINT('Ctrl Pts',(-18.4787605240765,-46.6469959906675,
122.225836194928)) ;
#49503 = CARTESIAN_POINT('Ctrl Pts',(-18.5104293304733,-46.8370516234074,
122.607686193805)) ;
#49504 = CARTESIAN_POINT('Ctrl Pts',(-18.2857214966169,-46.6570625430445,
122.406651152196)) ;
#49505 = CARTESIAN_POINT('Ctrl Pts',(-18.3857520045829,-46.8469418603011,
122.774114785356)) ;
#49506 = CARTESIAN_POINT('Ctrl Pts',(-18.1298739186722,-46.6669527799382,
122.614687511568)) ;
#49507 = CARTESIAN_POINT('Ctrl Pts',(-18.2905056904675,-46.8569340850951,
122.961335246674)) ;
#49508 = CARTESIAN_POINT('Ctrl Pts',(-18.0108157653476,-46.6769450047322,
122.848713195629)) ;
#49509 = CARTESIAN_POINT('Ctrl Pts',(-18.2295789136963,-46.866896705446,123.161719579238)) ;
#49510 = CARTESIAN_POINT('Ctrl Pts',(-17.9346569102099,-46.6869076250832,
123.099193972045)) ;
#49511 = CARTESIAN_POINT('Ctrl Pts',(-18.2040027326687,-46.8768017082092,
123.368391035254)) ;
#49512 = CARTESIAN_POINT('Ctrl Pts',(-17.9026865142012,-46.6968126278463,
123.35753421386)) ;
#49513 = CARTESIAN_POINT('Ctrl Pts',(-18.2150087934461,-46.8868594706073,
123.579531972586)) ;
#49514 = CARTESIAN_POINT('Ctrl Pts',(-17.9164439568202,-46.7068703902444,
123.621460054285)) ;
#49515 = CARTESIAN_POINT('Ctrl Pts',(-18.261371220002,-46.8967099899861,123.781380377064)) ;
#49516 = CARTESIAN_POINT('Ctrl Pts',(-17.9743972615009,-46.7167209096232,
123.873771940566)) ;
#49517 = CARTESIAN_POINT('Ctrl Pts',(-18.3431220571985,-46.9067415669843,
123.975771653837)) ;
#49518 = CARTESIAN_POINT('Ctrl Pts',(-18.076585890768,-46.7267524866214,124.116760874155)) ;
#49519 = CARTESIAN_POINT('Ctrl Pts',(-18.4574955443547,-46.9167513020892,
124.152440425366)) ;
#49520 = CARTESIAN_POINT('Ctrl Pts',(-18.2195527491891,-46.7367622217263,
124.337596888945)) ;
#49521 = CARTESIAN_POINT('Ctrl Pts',(-18.5992104285265,-46.9266608787155,
124.305119300968)) ;
#49522 = CARTESIAN_POINT('Ctrl Pts',(-18.3966970018907,-46.7466717983526,
124.528446109055)) ;
#49523 = CARTESIAN_POINT('Ctrl Pts',(-18.765279645767,-46.9365882645721,124.431541302977)) ;
#49524 = CARTESIAN_POINT('Ctrl Pts',(-18.6042842738298,-46.7565991842093,
124.686473857333)) ;
#49525 = CARTESIAN_POINT('Ctrl Pts',(-18.9530362774689,-46.9466331990624,
124.528179929632)) ;
#49526 = CARTESIAN_POINT('Ctrl Pts',(-18.8389799600762,-46.7666441186995,
124.807271873775)) ;
#49527 = CARTESIAN_POINT('Ctrl Pts',(-19.151511474355,-46.9565191312504,124.589883618221)) ;
#49528 = CARTESIAN_POINT('Ctrl Pts',(-19.0870750670697,-46.7765300508875,
124.884401576548)) ;
#49529 = CARTESIAN_POINT('Ctrl Pts',(-19.3598549427328,-46.9665124372034,
124.616830207834)) ;
#49530 = CARTESIAN_POINT('Ctrl Pts',(-19.3475046537344,-46.7865233568405,
124.918084459445)) ;
#49531 = CARTESIAN_POINT('Ctrl Pts',(-19.5687199932944,-46.9764580749853,
124.607155449397)) ;
#49532 = CARTESIAN_POINT('Ctrl Pts',(-19.6085865453895,-46.7964689946224,
124.905990634094)) ;
#49533 = CARTESIAN_POINT('Ctrl Pts',(-19.7728690713917,-46.9864053433312,
124.561770557663)) ;
#49534 = CARTESIAN_POINT('Ctrl Pts',(-19.8637733413823,-46.8064162629683,
124.84925888775)) ;
#49535 = CARTESIAN_POINT('Ctrl Pts',(-19.9678843674529,-46.9964532454683,
124.480604259967)) ;
#49536 = CARTESIAN_POINT('Ctrl Pts',(-20.1075420667063,-46.8164641651054,
124.747800719658)) ;
#49537 = CARTESIAN_POINT('Ctrl Pts',(-20.1423977281203,-47.0063009403085,
124.369220465197)) ;
#49538 = CARTESIAN_POINT('Ctrl Pts',(-20.3256846821778,-46.8263118599456,
124.608569806517)) ;
#49539 = CARTESIAN_POINT('Ctrl Pts',(-20.2971232610949,-47.0162624500529,
124.228102585513)) ;
#49540 = CARTESIAN_POINT('Ctrl Pts',(-20.5190914280319,-46.83627336969,124.432171593144)) ;
#49541 = CARTESIAN_POINT('Ctrl Pts',(-20.4256537019022,-47.0262918416617,
124.060947461949)) ;
#49542 = CARTESIAN_POINT('Ctrl Pts',(-20.6797539090321,-46.8463027612989,
124.223227378211)) ;
#49543 = CARTESIAN_POINT('Ctrl Pts',(-20.5221200134929,-47.0361993372165,
123.876344757324)) ;
#49544 = CARTESIAN_POINT('Ctrl Pts',(-20.8003366055072,-46.8562102568536,
123.992472885729)) ;
#49545 = CARTESIAN_POINT('Ctrl Pts',(-20.585700963853,-47.0461447288795,123.677180951145)) ;
#49546 = CARTESIAN_POINT('Ctrl Pts',(-20.8798121649612,-46.8661556485166,
123.743517315993)) ;
#49547 = CARTESIAN_POINT('Ctrl Pts',(-20.6140236281274,-47.0561466464769,
123.468796635054)) ;
#49548 = CARTESIAN_POINT('Ctrl Pts',(-20.915214625767,-46.876157566114,123.48303667498)) ;
#49549 = CARTESIAN_POINT('Ctrl Pts',(-20.6053144754768,-47.0661867140291,
123.257921725322)) ;
#49550 = CARTESIAN_POINT('Ctrl Pts',(-20.9043274469187,-46.8861976336662,
123.219443241607)) ;
#49551 = CARTESIAN_POINT('Ctrl Pts',(-20.5615451992037,-47.0760110254689,
123.056057517403)) ;
#49552 = CARTESIAN_POINT('Ctrl Pts',(-20.8496146260734,-46.896021945106,122.967111685229)) ;
#49553 = CARTESIAN_POINT('Ctrl Pts',(-20.48182941958,-47.086067266625,122.860270767228)) ;
#49554 = CARTESIAN_POINT('Ctrl Pts',(-20.7499690603553,-46.9060781862621,
122.722378928017)) ;
#49555 = CARTESIAN_POINT('Ctrl Pts',(-20.3705003700426,-47.0959981883606,
122.683623151021)) ;
#49556 = CARTESIAN_POINT('Ctrl Pts',(-20.6108065948018,-46.9160091079977,
122.501569334543)) ;
#49557 = CARTESIAN_POINT('Ctrl Pts',(-20.2303667268952,-47.1059414244368,
122.528548074826)) ;
#49558 = CARTESIAN_POINT('Ctrl Pts',(-20.4356383205666,-46.925952344074,122.307725777461)) ;
#49559 = CARTESIAN_POINT('Ctrl Pts',(-20.0648823735269,-47.1159227084493,
122.399473602791)) ;
#49560 = CARTESIAN_POINT('Ctrl Pts',(-20.2287819479061,-46.9359336280864,
122.146383450111)) ;
#49561 = CARTESIAN_POINT('Ctrl Pts',(-19.878210560702,-47.125967010075,122.300821311272)) ;
#49562 = CARTESIAN_POINT('Ctrl Pts',(-19.9954418662365,-46.9459779297121,
122.023069093696)) ;
#49563 = CARTESIAN_POINT('Ctrl Pts',(-19.6816640223288,-47.1357950912944,
122.236998796321)) ;
#49564 = CARTESIAN_POINT('Ctrl Pts',(-19.7497569427276,-46.9558060109315,
121.943291660823)) ;
#49565 = CARTESIAN_POINT('Ctrl Pts',(-19.4719363919362,-47.1458716941436,
122.207454533547)) ;
#49566 = CARTESIAN_POINT('Ctrl Pts',(-19.4875976586509,-46.9658826137807,
121.90636263565)) ;
#49567 = CARTESIAN_POINT('Ctrl Pts',(-19.2648901369236,-47.1557237732621,
122.214511172754)) ;
#49568 = CARTESIAN_POINT('Ctrl Pts',(-19.228788648694,-46.9757346928992,121.915184765414)) ;
#49569 = CARTESIAN_POINT('Ctrl Pts',(-19.0577050674081,-47.165797031571,122.258180662651)) ;
#49570 = CARTESIAN_POINT('Ctrl Pts',(-18.9698079849325,-46.9858079512082,
121.969772870616)) ;
#49571 = CARTESIAN_POINT('Ctrl Pts',(-18.8657477434276,-47.1756384909513,
122.335414466867)) ;
#49572 = CARTESIAN_POINT('Ctrl Pts',(-18.7298606158885,-46.9956494105884,
122.066316849577)) ;
#49573 = CARTESIAN_POINT('Ctrl Pts',(-18.6875856486329,-47.1855995863637,
122.445455661587)) ;
#49574 = CARTESIAN_POINT('Ctrl Pts',(-18.507158497528,-47.0056105060008,122.203869923558)) ;
#49575 = CARTESIAN_POINT('Ctrl Pts',(-18.5303140250955,-47.1956368707604,
122.586136597021)) ;
#49576 = CARTESIAN_POINT('Ctrl Pts',(-18.3105700406655,-47.0156477903975,
122.379722097263)) ;
#49577 = CARTESIAN_POINT('Ctrl Pts',(-18.4016481952308,-47.2055132094957,
122.749125228209)) ;
#49578 = CARTESIAN_POINT('Ctrl Pts',(-18.1497383800558,-47.0255241291328,
122.583459652795)) ;
#49579 = CARTESIAN_POINT('Ctrl Pts',(-18.3013741603539,-47.2155753356489,
122.935356273905)) ;
#49580 = CARTESIAN_POINT('Ctrl Pts',(-18.0243973839348,-47.0355862552861,
122.816248967698)) ;
#49581 = CARTESIAN_POINT('Ctrl Pts',(-18.2361754948208,-47.2254435096255,
123.132331116174)) ;
#49582 = CARTESIAN_POINT('Ctrl Pts',(-17.942900261197,-47.0454544292626,123.062469015826)) ;
#49583 = CARTESIAN_POINT('Ctrl Pts',(-18.205338043931,-47.2354490581293,123.340378376433)) ;
#49584 = CARTESIAN_POINT('Ctrl Pts',(-17.9043551712799,-47.0554599777664,
123.322528432364)) ;
#49585 = CARTESIAN_POINT('Ctrl Pts',(-18.2111535129992,-47.2454316900249,
123.550202526117)) ;
#49586 = CARTESIAN_POINT('Ctrl Pts',(-17.911626244223,-47.065442609662,123.58480879542)) ;
#49587 = CARTESIAN_POINT('Ctrl Pts',(-18.2537758997071,-47.2554756324466,
123.756993471745)) ;
#49588 = CARTESIAN_POINT('Ctrl Pts',(-17.964905818864,-47.0754865520838,123.843296984547)) ;
#49589 = CARTESIAN_POINT('Ctrl Pts',(-18.3297319147639,-47.2653037804738,
123.94914374406)) ;
#49590 = CARTESIAN_POINT('Ctrl Pts',(-18.0598529385593,-47.0853147001109,
124.083485382796)) ;
#49591 = CARTESIAN_POINT('Ctrl Pts',(-18.4391033103602,-47.2752936478482,
124.128436677712)) ;
#49592 = CARTESIAN_POINT('Ctrl Pts',(-18.1965689479448,-47.0953045674853,
124.307600675723)) ;
#49593 = CARTESIAN_POINT('Ctrl Pts',(-18.5791042370888,-47.2853373868037,
124.286501486607)) ;
#49594 = CARTESIAN_POINT('Ctrl Pts',(-18.3715713484641,-47.1053483064408,
124.505180389695)) ;
#49595 = CARTESIAN_POINT('Ctrl Pts',(-18.7405005083197,-47.2951591353416,
124.415289290748)) ;
#49596 = CARTESIAN_POINT('Ctrl Pts',(-18.5733188648744,-47.1151700549788,
124.666164420579)) ;
#49597 = CARTESIAN_POINT('Ctrl Pts',(-18.9254963348016,-47.3051941129514,
124.516697212118)) ;
#49598 = CARTESIAN_POINT('Ctrl Pts',(-18.8045645528301,-47.1252050325885,
124.792922450378)) ;
#49599 = CARTESIAN_POINT('Ctrl Pts',(-19.1252827024843,-47.3152190257091,
124.583820831396)) ;
#49600 = CARTESIAN_POINT('Ctrl Pts',(-19.0542980945525,-47.1352299453462,
124.876825162639)) ;
#49601 = CARTESIAN_POINT('Ctrl Pts',(-19.3300236054208,-47.3250709688029,
124.615141144271)) ;
#49602 = CARTESIAN_POINT('Ctrl Pts',(-19.3102255315884,-47.14508188844,124.915973693937)) ;
#49603 = CARTESIAN_POINT('Ctrl Pts',(-19.5399921824132,-47.335061930132,124.61069150491)) ;
#49604 = CARTESIAN_POINT('Ctrl Pts',(-19.5726863790115,-47.1550728497691,
124.910409512825)) ;
#49605 = CARTESIAN_POINT('Ctrl Pts',(-19.7445687503477,-47.3449798050004,
124.570275657887)) ;
#49606 = CARTESIAN_POINT('Ctrl Pts',(-19.8284072327233,-47.1649907246376,
124.859887472714)) ;
#49607 = CARTESIAN_POINT('Ctrl Pts',(-19.9411645038063,-47.3550083240017,
124.494169080804)) ;
#49608 = CARTESIAN_POINT('Ctrl Pts',(-20.074151105226,-47.1750192436388,124.764752235649)) ;
#49609 = CARTESIAN_POINT('Ctrl Pts',(-20.1190316044298,-47.3648920027995,
124.386736912704)) ;
#49610 = CARTESIAN_POINT('Ctrl Pts',(-20.2964844789698,-47.1849029224366,
124.630459757665)) ;
#49611 = CARTESIAN_POINT('Ctrl Pts',(-20.2776029483936,-47.3748869462393,
124.248868784575)) ;
#49612 = CARTESIAN_POINT('Ctrl Pts',(-20.4946972413566,-47.1948978658764,
124.458122754185)) ;
#49613 = CARTESIAN_POINT('Ctrl Pts',(-20.4099687757007,-47.3849138000617,
124.084811617486)) ;
#49614 = CARTESIAN_POINT('Ctrl Pts',(-20.6601527760735,-47.2049247196988,
124.253049913782)) ;
#49615 = CARTESIAN_POINT('Ctrl Pts',(-20.510642437193,-47.3947979644006,123.90302150782)) ;
#49616 = CARTESIAN_POINT('Ctrl Pts',(-20.7859931800233,-47.2148088840377,
124.025810555363)) ;
#49617 = CARTESIAN_POINT('Ctrl Pts',(-20.5791870198789,-47.404786062443,123.704564661141)) ;
#49618 = CARTESIAN_POINT('Ctrl Pts',(-20.8716717234267,-47.2247969820801,
123.777738571855)) ;
#49619 = CARTESIAN_POINT('Ctrl Pts',(-20.6122318337484,-47.4147371689001,
123.497960882242)) ;
#49620 = CARTESIAN_POINT('Ctrl Pts',(-20.912975435298,-47.2347480885372,123.519483140428)) ;
#49621 = CARTESIAN_POINT('Ctrl Pts',(-20.6087528151844,-47.4247822200682,
123.286823087064)) ;
#49622 = CARTESIAN_POINT('Ctrl Pts',(-20.908624300372,-47.2447931397053,123.255561025828)) ;
#49623 = CARTESIAN_POINT('Ctrl Pts',(-20.5695080656403,-47.4346439804265,
123.083245164977)) ;
#49624 = CARTESIAN_POINT('Ctrl Pts',(-20.8595658745191,-47.2546549000636,
123.001088343712)) ;
#49625 = CARTESIAN_POINT('Ctrl Pts',(-20.495357370561,-47.4446067972569,122.88735923458)) ;
#49626 = CARTESIAN_POINT('Ctrl Pts',(-20.7668750532524,-47.264617716894,122.756231591829)) ;
#49627 = CARTESIAN_POINT('Ctrl Pts',(-20.3872427945494,-47.4546414785377,
122.706219208448)) ;
#49628 = CARTESIAN_POINT('Ctrl Pts',(-20.6317297453688,-47.2746523981748,
122.529807845383)) ;
#49629 = CARTESIAN_POINT('Ctrl Pts',(-20.2516200642963,-47.4645265083184,
122.548722650758)) ;
#49630 = CARTESIAN_POINT('Ctrl Pts',(-20.4621990513068,-47.2845374279556,
122.332938364002)) ;
#49631 = CARTESIAN_POINT('Ctrl Pts',(-20.0877899814674,-47.4745921017164,
122.414841028809)) ;
#49632 = CARTESIAN_POINT('Ctrl Pts',(-20.2574099722437,-47.2946030213536,
122.16558837992)) ;
#49633 = CARTESIAN_POINT('Ctrl Pts',(-19.9073992267312,-47.4844312700779,
122.313551418133)) ;
#49634 = CARTESIAN_POINT('Ctrl Pts',(-20.0319196599626,-47.3044421897151,
122.038978242884)) ;
#49635 = CARTESIAN_POINT('Ctrl Pts',(-19.7078787306478,-47.4944938678194,
122.243312824082)) ;
#49636 = CARTESIAN_POINT('Ctrl Pts',(-19.7825183008089,-47.3145047874566,
121.95118250225)) ;
#49637 = CARTESIAN_POINT('Ctrl Pts',(-19.5025547915718,-47.5043908802264,
122.209566875106)) ;
#49638 = CARTESIAN_POINT('Ctrl Pts',(-19.5258624977633,-47.3244017998635,
121.909002521009)) ;
#49639 = CARTESIAN_POINT('Ctrl Pts',(-19.2937789957374,-47.514322202052,122.211297493397)) ;
#49640 = CARTESIAN_POINT('Ctrl Pts',(-19.2648924723534,-47.3343331216891,
121.911168475374)) ;
#49641 = CARTESIAN_POINT('Ctrl Pts',(-19.0862316655902,-47.5243639648065,
122.249899659143)) ;
#49642 = CARTESIAN_POINT('Ctrl Pts',(-19.0054588236434,-47.3443748844436,
121.959423773206)) ;
#49643 = CARTESIAN_POINT('Ctrl Pts',(-18.8914968548924,-47.5342521636972,
122.322686181889)) ;
#49644 = CARTESIAN_POINT('Ctrl Pts',(-18.7620408415515,-47.3542630833343,
122.050409572673)) ;
#49645 = CARTESIAN_POINT('Ctrl Pts',(-18.7102985265331,-47.544246102297,122.429005812639)) ;
#49646 = CARTESIAN_POINT('Ctrl Pts',(-18.5355442147587,-47.3642570219342,
122.18331150089)) ;
#49647 = CARTESIAN_POINT('Ctrl Pts',(-18.5511494828585,-47.5541869233339,
122.564478677246)) ;
#49648 = CARTESIAN_POINT('Ctrl Pts',(-18.3366094811848,-47.374197842971,122.352654796007)) ;
#49649 = CARTESIAN_POINT('Ctrl Pts',(-18.4175024086679,-47.5641463056221,
122.725638878256)) ;
#49650 = CARTESIAN_POINT('Ctrl Pts',(-18.1695526330089,-47.3841572252593,
122.554106932035)) ;
#49651 = CARTESIAN_POINT('Ctrl Pts',(-18.3133427089413,-47.5741440652745,
122.90822294444)) ;
#49652 = CARTESIAN_POINT('Ctrl Pts',(-18.0393553532008,-47.3941549849116,
122.782338451518)) ;
#49653 = CARTESIAN_POINT('Ctrl Pts',(-18.2424783139921,-47.5841802014768,
123.106952131826)) ;
#49654 = CARTESIAN_POINT('Ctrl Pts',(-17.9507774145601,-47.4041911211139,
123.03075086766)) ;
#49655 = CARTESIAN_POINT('Ctrl Pts',(-18.2076066802903,-47.5940309989677,
123.311088085714)) ;
#49656 = CARTESIAN_POINT('Ctrl Pts',(-17.9071905133116,-47.4140419186048,
123.285921661673)) ;
#49657 = CARTESIAN_POINT('Ctrl Pts',(-18.2080983621174,-47.603991864044,123.520488926134)) ;
#49658 = CARTESIAN_POINT('Ctrl Pts',(-17.9078079177087,-47.4240027836811,
123.547672833049)) ;
#49659 = CARTESIAN_POINT('Ctrl Pts',(-18.2454476002955,-47.6140207316744,
123.728004942344)) ;
#49660 = CARTESIAN_POINT('Ctrl Pts',(-17.9544972057267,-47.4340316513115,
123.807067402969)) ;
#49661 = CARTESIAN_POINT('Ctrl Pts',(-18.3173323666115,-47.6239309678108,
123.92354610878)) ;
#49662 = CARTESIAN_POINT('Ctrl Pts',(-18.0443558522348,-47.4439418874479,
124.051493099895)) ;
#49663 = CARTESIAN_POINT('Ctrl Pts',(-18.4218727530156,-47.6338659211253,
124.10437188864)) ;
#49664 = CARTESIAN_POINT('Ctrl Pts',(-18.1750338402729,-47.4538768407624,
124.27752403088)) ;
#49665 = CARTESIAN_POINT('Ctrl Pts',(-18.5577961313791,-47.6439068515349,
124.265872819916)) ;
#49666 = CARTESIAN_POINT('Ctrl Pts',(-18.3449402389459,-47.463917771172,124.479398422713)) ;
#49667 = CARTESIAN_POINT('Ctrl Pts',(-18.7171539318421,-47.6537947483165,
124.399365872321)) ;
#49668 = CARTESIAN_POINT('Ctrl Pts',(-18.5441394208993,-47.4738056679536,
124.646262687843)) ;
#49669 = CARTESIAN_POINT('Ctrl Pts',(-18.8989130954372,-47.6637841999752,
124.504559353168)) ;
#49670 = CARTESIAN_POINT('Ctrl Pts',(-18.7713398491585,-47.4837951196123,
124.777752129253)) ;
#49671 = CARTESIAN_POINT('Ctrl Pts',(-19.0956328686204,-47.6737432903405,
124.57621883154)) ;
#49672 = CARTESIAN_POINT('Ctrl Pts',(-19.0172406224052,-47.4937542099777,
124.867323859579)) ;
#49673 = CARTESIAN_POINT('Ctrl Pts',(-19.3004544560536,-47.6836406026468,
124.612933945687)) ;
#49674 = CARTESIAN_POINT('Ctrl Pts',(-19.2732681589925,-47.503651522284,124.913214982479)) ;
#49675 = CARTESIAN_POINT('Ctrl Pts',(-19.5118542835427,-47.6936970285471,
124.613436471454)) ;
#49676 = CARTESIAN_POINT('Ctrl Pts',(-19.5375180334294,-47.5137079481842,
124.913840318976)) ;
#49677 = CARTESIAN_POINT('Ctrl Pts',(-19.7163232652421,-47.7035670311368,
124.577994785846)) ;
#49678 = CARTESIAN_POINT('Ctrl Pts',(-19.7931038035126,-47.523577950774,124.86953541503)) ;
#49679 = CARTESIAN_POINT('Ctrl Pts',(-19.9142840722972,-47.7135709643141,
124.507042269719)) ;
#49680 = CARTESIAN_POINT('Ctrl Pts',(-20.0405538778607,-47.5335818839512,
124.780842159389)) ;
#49681 = CARTESIAN_POINT('Ctrl Pts',(-20.0966064940378,-47.723558224778,124.402844984413)) ;
#49682 = CARTESIAN_POINT('Ctrl Pts',(-20.2684557085201,-47.5435691444151,
124.650592871632)) ;
#49683 = CARTESIAN_POINT('Ctrl Pts',(-20.2585947292332,-47.7335852763637,
124.267974135904)) ;
#49684 = CARTESIAN_POINT('Ctrl Pts',(-20.470938720581,-47.5535961960008,124.482002870623)) ;
#49685 = CARTESIAN_POINT('Ctrl Pts',(-20.393034986563,-47.7434763661898,124.109317573844)) ;
#49686 = CARTESIAN_POINT('Ctrl Pts',(-20.6389889194383,-47.5634872858269,
124.283677447582)) ;
#49687 = CARTESIAN_POINT('Ctrl Pts',(-20.5342723905065,-47.7567741209708,
123.868088225556)) ;
#49688 = CARTESIAN_POINT('Ctrl Pts',(-20.8155222736475,-47.576785040608,123.982153459967)) ;
#49689 = CARTESIAN_POINT('Ctrl Pts',(-20.6091851589647,-47.769972180579,123.597577696433)) ;
#49690 = CARTESIAN_POINT('Ctrl Pts',(-20.9091627271371,-47.5899831002161,
123.644050843664)) ;
#49691 = CARTESIAN_POINT('Ctrl Pts',(-20.6114219199646,-47.7833689211482,
123.316008276815)) ;
#49692 = CARTESIAN_POINT('Ctrl Pts',(-20.911961468793,-47.6033798407853,123.29203099922)) ;
#49693 = CARTESIAN_POINT('Ctrl Pts',(-20.5772346324987,-47.7932398332216,
123.111276079564)) ;
#49694 = CARTESIAN_POINT('Ctrl Pts',(-20.8692234169841,-47.6132507528587,
123.036128094905)) ;
#49695 = CARTESIAN_POINT('Ctrl Pts',(-20.506620197884,-47.8033133949897,122.911669655053)) ;
#49696 = CARTESIAN_POINT('Ctrl Pts',(-20.7809529679,-47.6233243146269,122.78661751852)) ;
#49697 = CARTESIAN_POINT('Ctrl Pts',(-20.4051985250744,-47.8131348075781,
122.731761328968)) ;
#49698 = CARTESIAN_POINT('Ctrl Pts',(-20.6541739490141,-47.6331457272152,
122.561735103917)) ;
#49699 = CARTESIAN_POINT('Ctrl Pts',(-20.2709276734717,-47.8232088248091,
122.568046641826)) ;
#49700 = CARTESIAN_POINT('Ctrl Pts',(-20.4863320285724,-47.6432197444462,
122.357091382162)) ;
#49701 = CARTESIAN_POINT('Ctrl Pts',(-20.0611060975047,-47.8363676117737,
122.387657282842)) ;
#49702 = CARTESIAN_POINT('Ctrl Pts',(-20.2240587467137,-47.6563785314108,
122.131615915309)) ;
#49703 = CARTESIAN_POINT('Ctrl Pts',(-19.805342502725,-47.8497337148678,122.263873713802)) ;
#49704 = CARTESIAN_POINT('Ctrl Pts',(-19.904396611808,-47.669744634505,121.976897634996)) ;
#49705 = CARTESIAN_POINT('Ctrl Pts',(-19.5302562535324,-47.8630476497569,
122.211981763288)) ;
#49706 = CARTESIAN_POINT('Ctrl Pts',(-19.5604802159987,-47.683058569394,121.912018372431)) ;
#49707 = CARTESIAN_POINT('Ctrl Pts',(-19.3221676696211,-47.8729476892044,
122.209028722341)) ;
#49708 = CARTESIAN_POINT('Ctrl Pts',(-19.3003815270742,-47.6929586088415,
121.908333183184)) ;
#49709 = CARTESIAN_POINT('Ctrl Pts',(-19.115305104631,-47.8829120923389,122.242126287116)) ;
#49710 = CARTESIAN_POINT('Ctrl Pts',(-19.0418005240808,-47.702923011976,121.949706846036)) ;
#49711 = CARTESIAN_POINT('Ctrl Pts',(-18.9160968655024,-47.89294205946,122.311266661747)) ;
#49712 = CARTESIAN_POINT('Ctrl Pts',(-18.7927924422109,-47.7129529790972,
122.036134213176)) ;
#49713 = CARTESIAN_POINT('Ctrl Pts',(-18.7342345587612,-47.9028443360691,
122.412551802451)) ;
#49714 = CARTESIAN_POINT('Ctrl Pts',(-18.5654632174081,-47.7228552557062,
122.162745640329)) ;
#49715 = CARTESIAN_POINT('Ctrl Pts',(-18.5173604794192,-47.9161102652382,
122.58797464885)) ;
#49716 = CARTESIAN_POINT('Ctrl Pts',(-18.2943866086344,-47.7361211848754,
122.382011147429)) ;
#49717 = CARTESIAN_POINT('Ctrl Pts',(-18.309565842614,-47.9327317963447,122.873754193906)) ;
#49718 = CARTESIAN_POINT('Ctrl Pts',(-18.0346303797176,-47.7527427159818,
122.739250673809)) ;
#49719 = CARTESIAN_POINT('Ctrl Pts',(-18.1920101676508,-47.9526066249893,
123.279717316389)) ;
#49720 = CARTESIAN_POINT('Ctrl Pts',(-17.8876997701404,-47.7726175446265,
123.246720784385)) ;
#49721 = CARTESIAN_POINT('Ctrl Pts',(-18.2154597866439,-47.9692798330912,
123.633471891769)) ;
#49722 = CARTESIAN_POINT('Ctrl Pts',(-17.917000592734,-47.7892907527283,123.68884871812)) ;
#49723 = CARTESIAN_POINT('Ctrl Pts',(-18.3053614681726,-47.9825309580725,
123.897116716914)) ;
#49724 = CARTESIAN_POINT('Ctrl Pts',(-18.0293936752082,-47.8025418777096,
124.018462677686)) ;
#49725 = CARTESIAN_POINT('Ctrl Pts',(-18.4387378594094,-47.9957732768933,
124.141560057195)) ;
#49726 = CARTESIAN_POINT('Ctrl Pts',(-18.1961054880451,-47.8157841965304,
124.323995100748)) ;
#49727 = CARTESIAN_POINT('Ctrl Pts',(-18.6845127413368,-48.0125065172328,
124.39871352638)) ;
#49728 = CARTESIAN_POINT('Ctrl Pts',(-18.5033373266895,-47.8325174368699,
124.645448284564)) ;
#49729 = CARTESIAN_POINT('Ctrl Pts',(-19.0624327367419,-48.0323356654207,
124.585830606366)) ;
#49730 = CARTESIAN_POINT('Ctrl Pts',(-18.9757346113331,-47.8523465850579,
124.879336049279)) ;
#49731 = CARTESIAN_POINT('Ctrl Pts',(-19.4832475920745,-48.0522603605214,
124.633977070229)) ;
#49732 = CARTESIAN_POINT('Ctrl Pts',(-19.5017537468954,-47.8722712801585,
124.939516678205)) ;
#49733 = CARTESIAN_POINT('Ctrl Pts',(-19.8953466515693,-48.0721835891048,
124.53556105767)) ;
#49734 = CARTESIAN_POINT('Ctrl Pts',(-20.016875861944,-47.8921945087419,124.816493222092)) ;
#49735 = CARTESIAN_POINT('Ctrl Pts',(-20.2491680892978,-48.0921107282309,
124.302550900816)) ;
#49736 = CARTESIAN_POINT('Ctrl Pts',(-20.4591503180632,-47.912121647868,124.525228376918)) ;
#49737 = CARTESIAN_POINT('Ctrl Pts',(-20.5020771655509,-48.1119871908466,
123.963916176458)) ;
#49738 = CARTESIAN_POINT('Ctrl Pts',(-20.7752836476955,-47.9319981104837,
124.101934449769)) ;
#49739 = CARTESIAN_POINT('Ctrl Pts',(-20.6250718690425,-48.1319644194519,
123.557348462164)) ;
#49740 = CARTESIAN_POINT('Ctrl Pts',(-20.9290246638759,-47.951975339089,123.593724361099)) ;
#49741 = CARTESIAN_POINT('Ctrl Pts',(-20.6016537275589,-48.1518992774256,
123.134089906052)) ;
#49742 = CARTESIAN_POINT('Ctrl Pts',(-20.899749641412,-47.9719101970627,123.064652071563)) ;
#49743 = CARTESIAN_POINT('Ctrl Pts',(-20.4359503230159,-48.1717957263564,
122.744874511836)) ;
#49744 = CARTESIAN_POINT('Ctrl Pts',(-20.6926191392148,-47.9918066459935,
122.578134849579)) ;
#49745 = CARTESIAN_POINT('Ctrl Pts',(-20.1473267208655,-48.191717010423,122.434822386439)) ;
#49746 = CARTESIAN_POINT('Ctrl Pts',(-20.3318393279067,-48.0117279300601,
122.190571444876)) ;
#49747 = CARTESIAN_POINT('Ctrl Pts',(-19.7694900246731,-48.2116736600939,
122.241648838417)) ;
#49748 = CARTESIAN_POINT('Ctrl Pts',(-19.859543379667,-48.0316845797311,121.949105900427)) ;
#49749 = CARTESIAN_POINT('Ctrl Pts',(-19.3501801167776,-48.2315509532055,
122.189092571805)) ;
#49750 = CARTESIAN_POINT('Ctrl Pts',(-19.3354077539481,-48.0515618728427,
121.883411775971)) ;
#49751 = CARTESIAN_POINT('Ctrl Pts',(-18.9375691670233,-48.251437425434,122.281750555441)) ;
#49752 = CARTESIAN_POINT('Ctrl Pts',(-18.8196458602332,-48.0714483450711,
121.999233714919)) ;
#49753 = CARTESIAN_POINT('Ctrl Pts',(-18.5785832798502,-48.271498991358,122.512179757162)) ;
#49754 = CARTESIAN_POINT('Ctrl Pts',(-18.3709126385938,-48.0915099109951,
122.287270877205)) ;
#49755 = CARTESIAN_POINT('Ctrl Pts',(-18.3229725036018,-48.2913393988987,
122.847760478558)) ;
#49756 = CARTESIAN_POINT('Ctrl Pts',(-18.0514008754144,-48.1113503185359,
122.706744756814)) ;
#49757 = CARTESIAN_POINT('Ctrl Pts',(-18.1954566816947,-48.3111907228717,
123.250147542051)) ;
#49758 = CARTESIAN_POINT('Ctrl Pts',(-17.8920053839532,-48.1312016425088,
123.209726070964)) ;
#49759 = CARTESIAN_POINT('Ctrl Pts',(-18.2137292660296,-48.3312439928231,
123.676086435332)) ;
#49760 = CARTESIAN_POINT('Ctrl Pts',(-17.9148449517258,-48.1512549124602,
123.742150506195)) ;
#49761 = CARTESIAN_POINT('Ctrl Pts',(-18.3743522701606,-48.3510646502064,
124.065843827562)) ;
#49762 = CARTESIAN_POINT('Ctrl Pts',(-18.1156214422887,-48.1710755698436,
124.229345578872)) ;
#49763 = CARTESIAN_POINT('Ctrl Pts',(-18.6598163322656,-48.3710360715369,
124.380035479297)) ;
#49764 = CARTESIAN_POINT('Ctrl Pts',(-18.4724496628158,-48.1910469911741,
124.622086302263)) ;
#49765 = CARTESIAN_POINT('Ctrl Pts',(-19.0341051163834,-48.3909295639006,
124.577408934611)) ;
#49766 = CARTESIAN_POINT('Ctrl Pts',(-18.9403084788893,-48.2109404835378,
124.86880464151)) ;
#49767 = CARTESIAN_POINT('Ctrl Pts',(-19.4558297886332,-48.4109536501417,
124.635272002044)) ;
#49768 = CARTESIAN_POINT('Ctrl Pts',(-19.4674642242549,-48.2309645697788,
124.941135895711)) ;
#49769 = CARTESIAN_POINT('Ctrl Pts',(-19.8676091497869,-48.4307585292546,
124.54692460703)) ;
#49770 = CARTESIAN_POINT('Ctrl Pts',(-19.982186864098,-48.2507694488917,124.830704772301)) ;
#49771 = CARTESIAN_POINT('Ctrl Pts',(-20.2278594836264,-48.4507175449524,
124.322628489146)) ;
#49772 = CARTESIAN_POINT('Ctrl Pts',(-20.4325013285474,-48.2707284645896,
124.550337764469)) ;
#49773 = CARTESIAN_POINT('Ctrl Pts',(-20.4895249553124,-48.4707035685815,
123.987793204805)) ;
#49774 = CARTESIAN_POINT('Ctrl Pts',(-20.7595855617661,-48.2907144882186,
124.131795730191)) ;
#49775 = CARTESIAN_POINT('Ctrl Pts',(-20.620851700236,-48.490512064342,123.587567929602)) ;
#49776 = CARTESIAN_POINT('Ctrl Pts',(-20.9237469669242,-48.3105229839791,
123.631516939085)) ;
#49777 = CARTESIAN_POINT('Ctrl Pts',(-20.6081359744809,-48.5104947034476,
123.162963885691)) ;
#49778 = CARTESIAN_POINT('Ctrl Pts',(-20.9078563777569,-48.3305056230847,
123.100761863428)) ;
#49779 = CARTESIAN_POINT('Ctrl Pts',(-20.4519095426807,-48.5303761512416,
122.770042814153)) ;
#49780 = CARTESIAN_POINT('Ctrl Pts',(-20.7125774921877,-48.3503870708787,
122.609609792286)) ;
#49781 = CARTESIAN_POINT('Ctrl Pts',(-20.1703007545969,-48.5503326179791,
122.452751245619)) ;
#49782 = CARTESIAN_POINT('Ctrl Pts',(-20.3605699834758,-48.3703435376163,
122.212992650453)) ;
#49783 = CARTESIAN_POINT('Ctrl Pts',(-19.7987956805758,-48.5702100149347,
122.251075325285)) ;
#49784 = CARTESIAN_POINT('Ctrl Pts',(-19.8961915070511,-48.3902209345718,
121.960894036844)) ;
#49785 = CARTESIAN_POINT('Ctrl Pts',(-19.3787174367408,-48.59019196111,122.187732374788)) ;
#49786 = CARTESIAN_POINT('Ctrl Pts',(-19.3710944052881,-48.4102028807471,
121.881710834972)) ;
#49787 = CARTESIAN_POINT('Ctrl Pts',(-18.9632548947561,-48.6101210601467,
122.271556210172)) ;
#49788 = CARTESIAN_POINT('Ctrl Pts',(-18.8517658005324,-48.4301319797839,
121.986485155074)) ;
#49789 = CARTESIAN_POINT('Ctrl Pts',(-18.6014532782387,-48.6300496833594,
122.491970120177)) ;
#49790 = CARTESIAN_POINT('Ctrl Pts',(-18.3995108077568,-48.4500606029965,
122.262000851826)) ;
#49791 = CARTESIAN_POINT('Ctrl Pts',(-18.3371474305036,-48.6498840074658,
122.820662580448)) ;
#49792 = CARTESIAN_POINT('Ctrl Pts',(-18.0691275875861,-48.4698949271029,
122.672852581631)) ;
#49793 = CARTESIAN_POINT('Ctrl Pts',(-18.2224259879656,-48.6665362948492,
123.155533978461)) ;
#49794 = CARTESIAN_POINT('Ctrl Pts',(-17.9257131670204,-48.4865472144863,
123.091471777967)) ;
#49795 = CARTESIAN_POINT('Ctrl Pts',(-18.2035092636524,-48.6797967958714,
123.433741752069)) ;
#49796 = CARTESIAN_POINT('Ctrl Pts',(-17.9020712050957,-48.4998077155085,
123.439203218313)) ;
#49797 = CARTESIAN_POINT('Ctrl Pts',(-18.2254971301078,-48.6897982730727,
123.64284321915)) ;
#49798 = CARTESIAN_POINT('Ctrl Pts',(-17.9295520562288,-48.5098091927098,
123.700586123899)) ;
#49799 = CARTESIAN_POINT('Ctrl Pts',(-18.2839780007626,-48.6998302939322,
123.845485351349)) ;
#49800 = CARTESIAN_POINT('Ctrl Pts',(-18.002650404669,-48.5198412135693,123.953887639431)) ;
#49801 = CARTESIAN_POINT('Ctrl Pts',(-18.3749627895114,-48.7096938376577,
124.03181215673)) ;
#49802 = CARTESIAN_POINT('Ctrl Pts',(-18.116381192127,-48.5297047572949,124.186799307421)) ;
#49803 = CARTESIAN_POINT('Ctrl Pts',(-18.4977838557843,-48.7196625513279,
124.201640045108)) ;
#49804 = CARTESIAN_POINT('Ctrl Pts',(-18.2698960730485,-48.539673470965,124.399078392856)) ;
#49805 = CARTESIAN_POINT('Ctrl Pts',(-18.6994061492759,-48.7330082987316,
124.396656788491)) ;
#49806 = CARTESIAN_POINT('Ctrl Pts',(-18.5219675225796,-48.5530192183687,
124.642888173834)) ;
#49807 = CARTESIAN_POINT('Ctrl Pts',(-18.9435543299916,-48.7461588538042,
124.533062447628)) ;
#49808 = CARTESIAN_POINT('Ctrl Pts',(-18.8271260677206,-48.5661697734414,
124.813370160914)) ;
#49809 = CARTESIAN_POINT('Ctrl Pts',(-19.2163009315313,-48.7595442343541,
124.602291897744)) ;
#49810 = CARTESIAN_POINT('Ctrl Pts',(-19.1680417733709,-48.5795551539912,
124.899907926004)) ;
#49811 = CARTESIAN_POINT('Ctrl Pts',(-19.4236287954365,-48.7694321703469,
124.617669125966)) ;
#49812 = CARTESIAN_POINT('Ctrl Pts',(-19.4272046606678,-48.5894430899841,
124.919132760716)) ;
#49813 = CARTESIAN_POINT('Ctrl Pts',(-19.6326234694383,-48.7794233601596,
124.59695356156)) ;
#49814 = CARTESIAN_POINT('Ctrl Pts',(-19.6884474342547,-48.5994342797967,
124.893240945766)) ;
#49815 = CARTESIAN_POINT('Ctrl Pts',(-19.8341362224527,-48.7893754586979,
124.54055689342)) ;
#49816 = CARTESIAN_POINT('Ctrl Pts',(-19.9403393905158,-48.609386378335,124.822747843543)) ;
#49817 = CARTESIAN_POINT('Ctrl Pts',(-20.0244791000905,-48.7994217151483,
124.449067132527)) ;
#49818 = CARTESIAN_POINT('Ctrl Pts',(-20.1782692262088,-48.6194326347855,
124.708388111913)) ;
#49819 = CARTESIAN_POINT('Ctrl Pts',(-20.1927872751713,-48.8092711625425,
124.328441823876)) ;
#49820 = CARTESIAN_POINT('Ctrl Pts',(-20.3886560573569,-48.6292820821796,
124.557608789877)) ;
#49821 = CARTESIAN_POINT('Ctrl Pts',(-20.3397216534064,-48.8192338150376,
124.179192839321)) ;
#49822 = CARTESIAN_POINT('Ctrl Pts',(-20.572326095922,-48.6392447346748,124.371049479693)) ;
#49823 = CARTESIAN_POINT('Ctrl Pts',(-20.4590010872859,-48.8292569006798,
124.005486486065)) ;
#49824 = CARTESIAN_POINT('Ctrl Pts',(-20.7214277473186,-48.6492678203169,
124.153918077393)) ;
#49825 = CARTESIAN_POINT('Ctrl Pts',(-20.5456810010499,-48.8391820164367,
123.815659921871)) ;
#49826 = CARTESIAN_POINT('Ctrl Pts',(-20.8297802315917,-48.6591929360738,
123.916635975645)) ;
#49827 = CARTESIAN_POINT('Ctrl Pts',(-20.5986636057936,-48.8492344948365,
123.611094978186)) ;
#49828 = CARTESIAN_POINT('Ctrl Pts',(-20.8960112318138,-48.6692454144736,
123.660930444406)) ;
#49829 = CARTESIAN_POINT('Ctrl Pts',(-20.6151308206564,-48.8590859935392,
123.4046256451)) ;
#49830 = CARTESIAN_POINT('Ctrl Pts',(-20.9165980681484,-48.6790969131764,
123.402843889694)) ;
#49831 = CARTESIAN_POINT('Ctrl Pts',(-20.5958067267319,-48.8690577327418,
123.19590749213)) ;
#49832 = CARTESIAN_POINT('Ctrl Pts',(-20.8924457354999,-48.6890686523789,
123.141945824781)) ;
#49833 = CARTESIAN_POINT('Ctrl Pts',(-20.5403646088462,-48.8790529405074,
122.993187529069)) ;
#49834 = CARTESIAN_POINT('Ctrl Pts',(-20.8231457686488,-48.6990638601446,
122.888545055584)) ;
#49835 = CARTESIAN_POINT('Ctrl Pts',(-20.4500071936649,-48.8890869419765,
122.802593518848)) ;
#49836 = CARTESIAN_POINT('Ctrl Pts',(-20.71020152793,-48.7090978616136,122.650301300846)) ;
#49837 = CARTESIAN_POINT('Ctrl Pts',(-20.3303491214858,-48.8989423000689,
122.633423450339)) ;
#49838 = CARTESIAN_POINT('Ctrl Pts',(-20.5606310889083,-48.718953219706,122.438836911348)) ;
#49839 = CARTESIAN_POINT('Ctrl Pts',(-20.1812231910538,-48.9089417756622,
122.485307584382)) ;
#49840 = CARTESIAN_POINT('Ctrl Pts',(-20.3742255768515,-48.7289526952993,
122.253690036881)) ;
#49841 = CARTESIAN_POINT('Ctrl Pts',(-20.0105298951127,-48.9188362241573,
122.366356746529)) ;
#49842 = CARTESIAN_POINT('Ctrl Pts',(-20.1608603226581,-48.7388471437944,
122.104999075767)) ;
#49843 = CARTESIAN_POINT('Ctrl Pts',(-19.8186007680799,-48.928899348385,122.277447738823)) ;
#49844 = CARTESIAN_POINT('Ctrl Pts',(-19.9209501103882,-48.7489102680221,
121.993860313604)) ;
#49845 = CARTESIAN_POINT('Ctrl Pts',(-19.6186814141664,-48.9387389747136,
122.224180471466)) ;
#49846 = CARTESIAN_POINT('Ctrl Pts',(-19.6710512311322,-48.7587498943507,
121.927273469944)) ;
#49847 = CARTESIAN_POINT('Ctrl Pts',(-19.4079521083204,-48.9488022097566,
122.205769170469)) ;
#49848 = CARTESIAN_POINT('Ctrl Pts',(-19.4076398792598,-48.7688131293937,
121.904256633562)) ;
#49849 = CARTESIAN_POINT('Ctrl Pts',(-19.2007357621224,-48.9586962149906,
122.224096611744)) ;
#49850 = CARTESIAN_POINT('Ctrl Pts',(-19.1486188793919,-48.7787071346277,
121.927163232832)) ;
#49851 = CARTESIAN_POINT('Ctrl Pts',(-18.9987560013201,-48.9686389282064,
122.277825494424)) ;
#49852 = CARTESIAN_POINT('Ctrl Pts',(-18.8961432339119,-48.7886498478435,
121.99432181877)) ;
#49853 = CARTESIAN_POINT('Ctrl Pts',(-18.8079128243991,-48.9786446680046,
122.36634819626)) ;
#49854 = CARTESIAN_POINT('Ctrl Pts',(-18.6575880747036,-48.7986555876417,
122.104972809918)) ;
#49855 = CARTESIAN_POINT('Ctrl Pts',(-18.6352354087058,-48.988665570151,122.48702462515)) ;
#49856 = CARTESIAN_POINT('Ctrl Pts',(-18.4417397385889,-48.8086764897881,
122.255816146101)) ;
#49857 = CARTESIAN_POINT('Ctrl Pts',(-18.4878939976367,-48.9985563401998,
122.633756235366)) ;
#49858 = CARTESIAN_POINT('Ctrl Pts',(-18.2575608011542,-48.818567259837,122.439229061463)) ;
#49859 = CARTESIAN_POINT('Ctrl Pts',(-18.366802071252,-49.0085477509796,122.805381393975)) ;
#49860 = CARTESIAN_POINT('Ctrl Pts',(-18.106193675921,-48.8285586706167,122.653759103654)) ;
#49861 = CARTESIAN_POINT('Ctrl Pts',(-18.2777961208184,-49.0184960966441,
122.994637884771)) ;
#49862 = CARTESIAN_POINT('Ctrl Pts',(-17.9949337392161,-48.8385070162812,
122.890328842219)) ;
#49863 = CARTESIAN_POINT('Ctrl Pts',(-18.2225909158697,-49.0284409547052,
123.196309162691)) ;
#49864 = CARTESIAN_POINT('Ctrl Pts',(-17.9259246879504,-48.8484518743424,
123.142417551886)) ;
#49865 = CARTESIAN_POINT('Ctrl Pts',(-18.2033401476526,-49.0384957900982,
123.40679518885)) ;
#49866 = CARTESIAN_POINT('Ctrl Pts',(-17.9018586345267,-48.8585067097353,
123.405524737978)) ;
#49867 = CARTESIAN_POINT('Ctrl Pts',(-18.2201677805228,-49.0483181621996,
123.612623482533)) ;
#49868 = CARTESIAN_POINT('Ctrl Pts',(-17.9228907005279,-48.8683290818368,
123.662811089171)) ;
#49869 = CARTESIAN_POINT('Ctrl Pts',(-18.2733451038834,-49.0583740296434,
123.817216281984)) ;
#49870 = CARTESIAN_POINT('Ctrl Pts',(-17.9893599290882,-48.8783849492805,
123.918552606262)) ;
#49871 = CARTESIAN_POINT('Ctrl Pts',(-18.3605807016632,-49.0683147595013,
124.007132559612)) ;
#49872 = CARTESIAN_POINT('Ctrl Pts',(-18.0984022475195,-48.8883256791384,
124.155949320405)) ;
#49873 = CARTESIAN_POINT('Ctrl Pts',(-18.478492080276,-49.0782190980524,124.178754700712)) ;
#49874 = CARTESIAN_POINT('Ctrl Pts',(-18.2457897778608,-48.8982300176895,
124.370478803514)) ;
#49875 = CARTESIAN_POINT('Ctrl Pts',(-18.6265896771452,-49.0882657794809,
124.329321820747)) ;
#49876 = CARTESIAN_POINT('Ctrl Pts',(-18.4309099578703,-48.908276699118,124.558689346407)) ;
#49877 = CARTESIAN_POINT('Ctrl Pts',(-18.7959241485075,-49.0981612869501,
124.450228240295)) ;
#49878 = CARTESIAN_POINT('Ctrl Pts',(-18.6425771224679,-48.9181722065873,
124.709824664085)) ;
#49879 = CARTESIAN_POINT('Ctrl Pts',(-18.9867862815912,-49.1082235554488,
124.541375926304)) ;
#49880 = CARTESIAN_POINT('Ctrl Pts',(-18.8811535876977,-48.9282344750859,
124.823761366572)) ;
#49881 = CARTESIAN_POINT('Ctrl Pts',(-19.1861338900622,-49.1180655457194,
124.596897992535)) ;
#49882 = CARTESIAN_POINT('Ctrl Pts',(-19.1303382919628,-48.9380764653565,
124.893166471091)) ;
#49883 = CARTESIAN_POINT('Ctrl Pts',(-19.3951586958825,-49.1280589626003,
124.617736026602)) ;
#49884 = CARTESIAN_POINT('Ctrl Pts',(-19.3916192445913,-48.9480698822375,
124.919216288475)) ;
#49885 = CARTESIAN_POINT('Ctrl Pts',(-19.6032371853687,-49.1379834504525,
124.602087040925)) ;
#49886 = CARTESIAN_POINT('Ctrl Pts',(-19.6517180268275,-48.9579943700896,
124.899657271309)) ;
#49887 = CARTESIAN_POINT('Ctrl Pts',(-19.8069854701028,-49.147983084361,124.550380447897)) ;
#49888 = CARTESIAN_POINT('Ctrl Pts',(-19.9064040385048,-48.9679940039981,
124.835026142014)) ;
#49889 = CARTESIAN_POINT('Ctrl Pts',(-19.9984490408071,-49.1579691946177,
124.464185024781)) ;
#49890 = CARTESIAN_POINT('Ctrl Pts',(-20.145734566015,-48.9779801142549,124.72728379971)) ;
#49891 = CARTESIAN_POINT('Ctrl Pts',(-20.1727370286862,-49.1680051458049,
124.345311201538)) ;
#49892 = CARTESIAN_POINT('Ctrl Pts',(-20.363595758635,-48.988016065442,124.578693439179)) ;
#49893 = CARTESIAN_POINT('Ctrl Pts',(-20.3212855419175,-49.1778617841397,
124.200809116619)) ;
#49894 = CARTESIAN_POINT('Ctrl Pts',(-20.5492835774246,-48.9978727037768,
124.398066759077)) ;
#49895 = CARTESIAN_POINT('Ctrl Pts',(-20.4444358570333,-49.1878607442177,
124.030495135267)) ;
#49896 = CARTESIAN_POINT('Ctrl Pts',(-20.7032232576622,-49.0078716638548,
124.185175408038)) ;
#49897 = CARTESIAN_POINT('Ctrl Pts',(-20.5354258116152,-49.1977559745315,
123.843382253148)) ;
#49898 = CARTESIAN_POINT('Ctrl Pts',(-20.8169628556699,-49.0177668941686,
123.951284538968)) ;
#49899 = CARTESIAN_POINT('Ctrl Pts',(-20.5934596272314,-49.2078164870001,
123.640024401084)) ;
#49900 = CARTESIAN_POINT('Ctrl Pts',(-20.8895070310717,-49.0278274066372,
123.697088016909)) ;
#49901 = CARTESIAN_POINT('Ctrl Pts',(-20.614964621342,-49.2176657785463,123.434065207261)) ;
#49902 = CARTESIAN_POINT('Ctrl Pts',(-20.9163903855367,-49.0376766981834,
123.439638200355)) ;
#49903 = CARTESIAN_POINT('Ctrl Pts',(-20.6006524939482,-49.2276929644785,
123.223753772235)) ;
#49904 = CARTESIAN_POINT('Ctrl Pts',(-20.8985020837487,-49.0477038841156,
123.176748817994)) ;
#49905 = CARTESIAN_POINT('Ctrl Pts',(-20.5494925233518,-49.2377215009378,
123.019212625671)) ;
#49906 = CARTESIAN_POINT('Ctrl Pts',(-20.8345541010092,-49.0577324205749,
122.921071960557)) ;
#49907 = CARTESIAN_POINT('Ctrl Pts',(-20.4655325528851,-49.2475667409028,
122.830041408162)) ;
#49908 = CARTESIAN_POINT('Ctrl Pts',(-20.7296054273253,-49.0675776605399,
122.68460614522)) ;
#49909 = CARTESIAN_POINT('Ctrl Pts',(-20.3487525475356,-49.257557435826,122.655457201128)) ;
#49910 = CARTESIAN_POINT('Ctrl Pts',(-20.5836317515741,-49.0775683554631,
122.466374760989)) ;
#49911 = CARTESIAN_POINT('Ctrl Pts',(-20.2024139642059,-49.2675952565846,
122.503414527449)) ;
#49912 = CARTESIAN_POINT('Ctrl Pts',(-20.4007099669352,-49.0876061762217,
122.276320211683)) ;
#49913 = CARTESIAN_POINT('Ctrl Pts',(-20.0353851635832,-49.2774398503615,
122.381196686235)) ;
#49914 = CARTESIAN_POINT('Ctrl Pts',(-20.1919240683842,-49.0974507699987,
122.123545795109)) ;
#49915 = CARTESIAN_POINT('Ctrl Pts',(-19.8472610421014,-49.2874238457376,
122.288151641728)) ;
#49916 = CARTESIAN_POINT('Ctrl Pts',(-19.9567693977097,-49.1074347653747,
122.00723791885)) ;
#49917 = CARTESIAN_POINT('Ctrl Pts',(-19.6465098945046,-49.297372894299,122.229404619294)) ;
#49918 = CARTESIAN_POINT('Ctrl Pts',(-19.705830459049,-49.1173838139361,121.933802445044)) ;
#49919 = CARTESIAN_POINT('Ctrl Pts',(-19.4375191683223,-49.3073753332735,
122.206058321571)) ;
#49920 = CARTESIAN_POINT('Ctrl Pts',(-19.4445921214419,-49.1273862529106,
121.904618015651)) ;
#49921 = CARTESIAN_POINT('Ctrl Pts',(-19.2272793153479,-49.3173965745699,
122.219664475617)) ;
#49922 = CARTESIAN_POINT('Ctrl Pts',(-19.1817922313132,-49.137407494207,121.921624060379)) ;
#49923 = CARTESIAN_POINT('Ctrl Pts',(-19.0251633000382,-49.3272892530094,
122.268684611015)) ;
#49924 = CARTESIAN_POINT('Ctrl Pts',(-18.9291459751133,-49.1473001726465,
121.982897915693)) ;
#49925 = CARTESIAN_POINT('Ctrl Pts',(-18.8326207757844,-49.337279306957,122.352565184891)) ;
#49926 = CARTESIAN_POINT('Ctrl Pts',(-18.6884670363836,-49.1572902265941,
122.087747388181)) ;
#49927 = CARTESIAN_POINT('Ctrl Pts',(-18.65820968593,-49.3472376681055,122.468356623585)) ;
#49928 = CARTESIAN_POINT('Ctrl Pts',(-18.4704519830292,-49.1672485877426,
122.232485671817)) ;
#49929 = CARTESIAN_POINT('Ctrl Pts',(-18.5070800115735,-49.3571372949903,
122.611463780261)) ;
#49930 = CARTESIAN_POINT('Ctrl Pts',(-18.2815383415692,-49.1771482146274,
122.411369259889)) ;
#49931 = CARTESIAN_POINT('Ctrl Pts',(-18.3813177298446,-49.3671851917937,
122.781158712775)) ;
#49932 = CARTESIAN_POINT('Ctrl Pts',(-18.1243345330828,-49.1871961114308,
122.623486945981)) ;
#49933 = CARTESIAN_POINT('Ctrl Pts',(-18.2881930918701,-49.3770805494297,
122.96721883373)) ;
#49934 = CARTESIAN_POINT('Ctrl Pts',(-18.0079271717103,-49.1970914690668,
122.856062333984)) ;
#49935 = CARTESIAN_POINT('Ctrl Pts',(-18.2277777790016,-49.3871422018863,
123.169910866014)) ;
#49936 = CARTESIAN_POINT('Ctrl Pts',(-17.9324068931307,-49.2071531215235,
123.109426695893)) ;
#49937 = CARTESIAN_POINT('Ctrl Pts',(-18.2039634409259,-49.3969868061583,
123.375507420365)) ;
#49938 = CARTESIAN_POINT('Ctrl Pts',(-17.9026375541845,-49.2169977257954,
123.366423552934)) ;
#49939 = CARTESIAN_POINT('Ctrl Pts',(-18.21560282813,-49.4069469278563,123.584573029196)) ;
#49940 = CARTESIAN_POINT('Ctrl Pts',(-17.9171858178237,-49.2269578474934,
123.62775607521)) ;
#49941 = CARTESIAN_POINT('Ctrl Pts',(-18.2641366558949,-49.4169849622188,
123.789939361942)) ;
#49942 = CARTESIAN_POINT('Ctrl Pts',(-17.9778519477484,-49.2369958818559,
123.884464098742)) ;
#49943 = CARTESIAN_POINT('Ctrl Pts',(-18.3458936811806,-49.4268592748053,
123.980778500139)) ;
#49944 = CARTESIAN_POINT('Ctrl Pts',(-18.0800477463435,-49.2468701944424,
124.123014445666)) ;
#49945 = CARTESIAN_POINT('Ctrl Pts',(-18.4617697259283,-49.436928755588,124.1579063665)) ;
#49946 = CARTESIAN_POINT('Ctrl Pts',(-18.2248917333607,-49.2569396752251,
124.344424493672)) ;
#49947 = CARTESIAN_POINT('Ctrl Pts',(-18.6032069971224,-49.4467630916051,
124.308729317286)) ;
#49948 = CARTESIAN_POINT('Ctrl Pts',(-18.4016886197062,-49.2667740112422,
124.532954912051)) ;
#49949 = CARTESIAN_POINT('Ctrl Pts',(-18.7716598122527,-49.4567960493333,
124.435654755595)) ;
#49950 = CARTESIAN_POINT('Ctrl Pts',(-18.612254092902,-49.2768069689704,124.691612235755)) ;
#49951 = CARTESIAN_POINT('Ctrl Pts',(-18.9596285266735,-49.4668164479085,
124.530768810622)) ;
#49952 = CARTESIAN_POINT('Ctrl Pts',(-18.8472145112584,-49.2868273675456,
124.810505656813)) ;
#49953 = CARTESIAN_POINT('Ctrl Pts',(-19.1580012266402,-49.4766820216797,
124.591362825177)) ;
#49954 = CARTESIAN_POINT('Ctrl Pts',(-19.0951813191321,-49.2966929413168,
124.886249263445)) ;
#49955 = CARTESIAN_POINT('Ctrl Pts',(-19.3680870984409,-49.4867508963358,
124.617111323159)) ;
#49956 = CARTESIAN_POINT('Ctrl Pts',(-19.3577881565911,-49.3067618159729,
124.918435602837)) ;
#49957 = CARTESIAN_POINT('Ctrl Pts',(-19.5747954024805,-49.4965963272413,
124.606267618942)) ;
#49958 = CARTESIAN_POINT('Ctrl Pts',(-19.6161749842658,-49.3166072468784,
124.904881658473)) ;
#49959 = CARTESIAN_POINT('Ctrl Pts',(-19.7793647307938,-49.506575952112,124.559725510975)) ;
#49960 = CARTESIAN_POINT('Ctrl Pts',(-19.8718870581051,-49.3265868717491,
124.846704436863)) ;
#49961 = CARTESIAN_POINT('Ctrl Pts',(-19.9733472943274,-49.5165946350261,
124.477683630801)) ;
#49962 = CARTESIAN_POINT('Ctrl Pts',(-20.1143655069739,-49.3366055546632,
124.74415269252)) ;
#49963 = CARTESIAN_POINT('Ctrl Pts',(-20.1480134440682,-49.5264779002099,
124.365106465105)) ;
#49964 = CARTESIAN_POINT('Ctrl Pts',(-20.3326993754849,-49.346488819847,124.603431043373)) ;
#49965 = CARTESIAN_POINT('Ctrl Pts',(-20.3032270535751,-49.5365461943013,
124.221241519737)) ;
#49966 = CARTESIAN_POINT('Ctrl Pts',(-20.5267164375359,-49.3565571139384,
124.423600519391)) ;
#49967 = CARTESIAN_POINT('Ctrl Pts',(-20.4283133218922,-49.5463763244866,
124.056692970203)) ;
#49968 = CARTESIAN_POINT('Ctrl Pts',(-20.6830755384687,-49.3663872441237,
124.217913860219)) ;
#49969 = CARTESIAN_POINT('Ctrl Pts',(-20.5254162570907,-49.5564428727018,
123.868692053615)) ;
#49970 = CARTESIAN_POINT('Ctrl Pts',(-20.8044543031149,-49.3764537923389,
123.982913211132)) ;
#49971 = CARTESIAN_POINT('Ctrl Pts',(-20.5871922984484,-49.5663331213904,
123.67013049004)) ;
#49972 = CARTESIAN_POINT('Ctrl Pts',(-20.881675014768,-49.3863440410275,123.734710364339)) ;
#49973 = CARTESIAN_POINT('Ctrl Pts',(-20.6142760100577,-49.5763253031664,
123.461828924434)) ;
#49974 = CARTESIAN_POINT('Ctrl Pts',(-20.9155298639726,-49.3963362228035,
123.474333218862)) ;
#49975 = CARTESIAN_POINT('Ctrl Pts',(-20.6046113032203,-49.5862880837942,
123.252607087574)) ;
#49976 = CARTESIAN_POINT('Ctrl Pts',(-20.9034492216854,-49.4062990034313,
123.212805454271)) ;
#49977 = CARTESIAN_POINT('Ctrl Pts',(-20.5595393091731,-49.5961924884679,
123.049307305498)) ;
#49978 = CARTESIAN_POINT('Ctrl Pts',(-20.847109080545,-49.4162034081051,122.958679801309)) ;
#49979 = CARTESIAN_POINT('Ctrl Pts',(-20.478467374034,-49.606252482947,122.853990633004)) ;
#49980 = CARTESIAN_POINT('Ctrl Pts',(-20.7457693980106,-49.4262634025841,
122.714534227944)) ;
#49981 = CARTESIAN_POINT('Ctrl Pts',(-20.3672356635817,-49.6161011049168,
122.679339657836)) ;
#49982 = CARTESIAN_POINT('Ctrl Pts',(-20.6067290420419,-49.4361120245539,
122.496219298933)) ;
#49983 = CARTESIAN_POINT('Ctrl Pts',(-20.2251544951592,-49.6261315443286,
122.523536505665)) ;
#49984 = CARTESIAN_POINT('Ctrl Pts',(-20.4291275579387,-49.4461424639657,
122.301465539573)) ;
#49985 = CARTESIAN_POINT('Ctrl Pts',(-20.0582370192232,-49.6361412599634,
122.395350931652)) ;
#49986 = CARTESIAN_POINT('Ctrl Pts',(-20.2204806965298,-49.4561521796005,
122.141233524308)) ;
#49987 = CARTESIAN_POINT('Ctrl Pts',(-19.8735746846781,-49.646052012656,122.298896339654)) ;
#49988 = CARTESIAN_POINT('Ctrl Pts',(-19.9896519589518,-49.4660629322931,
122.020664911616)) ;
#49989 = CARTESIAN_POINT('Ctrl Pts',(-19.6747293616063,-49.6559812856024,
122.23534414131)) ;
#49990 = CARTESIAN_POINT('Ctrl Pts',(-19.7410945155268,-49.4759922052395,
121.941224683221)) ;
#49991 = CARTESIAN_POINT('Ctrl Pts',(-19.4655008779412,-49.666023976995,122.207142648671)) ;
#49992 = CARTESIAN_POINT('Ctrl Pts',(-19.4795590978915,-49.4860348966322,
121.90597303431)) ;
#49993 = CARTESIAN_POINT('Ctrl Pts',(-19.2578087514022,-49.6759105102126,
122.215430584698)) ;
#49994 = CARTESIAN_POINT('Ctrl Pts',(-19.219942862055,-49.4959214298497,121.916333239462)) ;
#49995 = CARTESIAN_POINT('Ctrl Pts',(-19.0524672632715,-49.6859036551446,
122.259778671092)) ;
#49996 = CARTESIAN_POINT('Ctrl Pts',(-18.9632658837388,-49.5059145747817,
121.971768765229)) ;
#49997 = CARTESIAN_POINT('Ctrl Pts',(-18.8588885046853,-49.6958493359811,
122.3388088344)) ;
#49998 = CARTESIAN_POINT('Ctrl Pts',(-18.7212920167133,-49.5158602556182,
122.070557018529)) ;
#49999 = CARTESIAN_POINT('Ctrl Pts',(-18.6817080873745,-49.7057965931296,
122.449910909112)) ;
#50000 = CARTESIAN_POINT('Ctrl Pts',(-18.499816284014,-49.5258075127667,122.209435357243)) ;
#50001 = CARTESIAN_POINT('Ctrl Pts',(-18.5251114478869,-49.7158444970016,
122.591672777569)) ;
#50002 = CARTESIAN_POINT('Ctrl Pts',(-18.3040709556974,-49.5358554166387,
122.386637839566)) ;
#50003 = CARTESIAN_POINT('Ctrl Pts',(-18.3979488536748,-49.7256921960996,
122.755046538999)) ;
#50004 = CARTESIAN_POINT('Ctrl Pts',(-18.1451172426182,-49.5457031157367,
122.590856449756)) ;
#50005 = CARTESIAN_POINT('Ctrl Pts',(-18.2993856740285,-49.7356536870782,
122.939814886333)) ;
#50006 = CARTESIAN_POINT('Ctrl Pts',(-18.0219137176075,-49.5556646067154,
122.821817640682)) ;
#50007 = CARTESIAN_POINT('Ctrl Pts',(-18.2342214042971,-49.7456831494922,
123.140352456418)) ;
#50008 = CARTESIAN_POINT('Ctrl Pts',(-17.940459021946,-49.5656940691293,123.072489705636)) ;
#50009 = CARTESIAN_POINT('Ctrl Pts',(-18.2051140091869,-49.7555903805921,
123.346589615801)) ;
#50010 = CARTESIAN_POINT('Ctrl Pts',(-17.9040753303837,-49.5756013002292,
123.330287135663)) ;
#50011 = CARTESIAN_POINT('Ctrl Pts',(-18.211860951267,-49.7655367592695,123.555572269236)) ;
#50012 = CARTESIAN_POINT('Ctrl Pts',(-17.9125098782815,-49.5855476789066,
123.591516015328)) ;
#50013 = CARTESIAN_POINT('Ctrl Pts',(-18.2549768342654,-49.7755415280784,
123.761455951672)) ;
#50014 = CARTESIAN_POINT('Ctrl Pts',(-17.9664056109614,-49.5955524477155,
123.848870528812)) ;
#50015 = CARTESIAN_POINT('Ctrl Pts',(-18.3335291933488,-49.7855626490986,
123.956934913202)) ;
#50016 = CARTESIAN_POINT('Ctrl Pts',(-18.0645967713653,-49.6055735687357,
124.09321890463)) ;
#50017 = CARTESIAN_POINT('Ctrl Pts',(-18.4431860931502,-49.7954535149512,
124.133615577516)) ;
#50018 = CARTESIAN_POINT('Ctrl Pts',(-18.201669169235,-49.6154644345883,124.314070124033)) ;
#50019 = CARTESIAN_POINT('Ctrl Pts',(-18.5830122161219,-49.8054443237105,
124.290330824793)) ;
#50020 = CARTESIAN_POINT('Ctrl Pts',(-18.3764527037186,-49.6254552433476,
124.509963682935)) ;
#50021 = CARTESIAN_POINT('Ctrl Pts',(-18.747304518671,-49.8153949818908,124.419846948591)) ;
#50022 = CARTESIAN_POINT('Ctrl Pts',(-18.5818191091062,-49.6354059015279,
124.671858407225)) ;
#50023 = CARTESIAN_POINT('Ctrl Pts',(-18.9311656323854,-49.8253311915329,
124.518959631838)) ;
#50024 = CARTESIAN_POINT('Ctrl Pts',(-18.8116465771157,-49.64534211117,124.795748611683)) ;
#50025 = CARTESIAN_POINT('Ctrl Pts',(-19.1303351595038,-49.8353143582578,
124.585224682126)) ;
#50026 = CARTESIAN_POINT('Ctrl Pts',(-19.0606091019556,-49.6553252778949,
124.878578886078)) ;
#50027 = CARTESIAN_POINT('Ctrl Pts',(-19.3392535954594,-49.8453581554681,
124.615693199531)) ;
#50028 = CARTESIAN_POINT('Ctrl Pts',(-19.3217571085356,-49.6653690751052,
124.916663479526)) ;
#50029 = CARTESIAN_POINT('Ctrl Pts',(-19.5458273359172,-49.8551863716364,
124.610045735336)) ;
#50030 = CARTESIAN_POINT('Ctrl Pts',(-19.5799756953038,-49.6751972912734,
124.909602892924)) ;
#50031 = CARTESIAN_POINT('Ctrl Pts',(-19.7533454043374,-49.8652629391056,
124.567682590718)) ;
#50032 = CARTESIAN_POINT('Ctrl Pts',(-19.8393726054235,-49.6852738587427,
124.85664781919)) ;
#50033 = CARTESIAN_POINT('Ctrl Pts',(-19.9460859117418,-49.875115024795,124.491728264813)) ;
#50034 = CARTESIAN_POINT('Ctrl Pts',(-20.0802989166778,-49.6951259444321,
124.761703259049)) ;
#50035 = CARTESIAN_POINT('Ctrl Pts',(-20.126701616753,-49.8851882922004,124.381226191815)) ;
#50036 = CARTESIAN_POINT('Ctrl Pts',(-20.3060674976311,-49.7051992118375,
124.623574721995)) ;
#50037 = CARTESIAN_POINT('Ctrl Pts',(-20.2817328321541,-49.895029708624,124.244194431429)) ;
#50038 = CARTESIAN_POINT('Ctrl Pts',(-20.4998566127892,-49.7150406282611,
124.452283158232)) ;
#50039 = CARTESIAN_POINT('Ctrl Pts',(-20.4127836030217,-49.9049909667667,
124.080861209861)) ;
#50040 = CARTESIAN_POINT('Ctrl Pts',(-20.6636690759953,-49.7250018864038,
124.248115309277)) ;
#50041 = CARTESIAN_POINT('Ctrl Pts',(-20.5138903858792,-49.9150276431986,
123.895664527938)) ;
#50042 = CARTESIAN_POINT('Ctrl Pts',(-20.7900512077694,-49.7350385628358,
124.016618869433)) ;
#50043 = CARTESIAN_POINT('Ctrl Pts',(-20.5805838627807,-49.9249062510625,
123.698962304801)) ;
#50044 = CARTESIAN_POINT('Ctrl Pts',(-20.8734168716423,-49.7449171706996,
123.770739635616)) ;
#50045 = CARTESIAN_POINT('Ctrl Pts',(-20.6127292545574,-49.9349664797013,
123.489949368876)) ;
#50046 = CARTESIAN_POINT('Ctrl Pts',(-20.9135969834897,-49.7549773993384,
123.509473505377)) ;
#50047 = CARTESIAN_POINT('Ctrl Pts',(-20.6082434967595,-49.9448334638621,
123.282536648227)) ;
#50048 = CARTESIAN_POINT('Ctrl Pts',(-20.9079881465136,-49.7648443834992,
123.250206599961)) ;
#50049 = CARTESIAN_POINT('Ctrl Pts',(-20.5676533220387,-49.9548390301148,
123.076169983753)) ;
#50050 = CARTESIAN_POINT('Ctrl Pts',(-20.8572486896229,-49.7748499497519,
122.992248525013)) ;
#50051 = CARTESIAN_POINT('Ctrl Pts',(-20.4919395617635,-49.9648228185294,
122.880371545976)) ;
#50052 = CARTESIAN_POINT('Ctrl Pts',(-20.762604793769,-49.7848337381665,122.747500893272)) ;
#50053 = CARTESIAN_POINT('Ctrl Pts',(-20.3825347856944,-49.974868675332,122.699741996269)) ;
#50054 = CARTESIAN_POINT('Ctrl Pts',(-20.6258474889343,-49.7948795949691,
122.521714953431)) ;
#50055 = CARTESIAN_POINT('Ctrl Pts',(-20.246666531369,-49.984694552548,122.544142027715)) ;
#50056 = CARTESIAN_POINT('Ctrl Pts',(-20.4560100049214,-49.8047054721851,
122.327215170071)) ;
#50057 = CARTESIAN_POINT('Ctrl Pts',(-20.0835826601991,-49.9946850283893,
122.411791016735)) ;
#50058 = CARTESIAN_POINT('Ctrl Pts',(-20.2521537953988,-49.8146959480264,
122.161777820883)) ;
#50059 = CARTESIAN_POINT('Ctrl Pts',(-19.8987503711464,-50.0047286042881,
122.309710132215)) ;
#50060 = CARTESIAN_POINT('Ctrl Pts',(-20.0211126978458,-49.8247395239252,
122.03417835331)) ;
#50061 = CARTESIAN_POINT('Ctrl Pts',(-19.7035546402409,-50.0145503965861,
122.242375343609)) ;
#50062 = CARTESIAN_POINT('Ctrl Pts',(-19.7771162248852,-49.8345613162232,
121.950011278901)) ;
#50063 = CARTESIAN_POINT('Ctrl Pts',(-19.495286249998,-50.024585362212,122.208741496858)) ;
#50064 = CARTESIAN_POINT('Ctrl Pts',(-19.5167805110166,-49.8445962818491,
121.907971037279)) ;
#50065 = CARTESIAN_POINT('Ctrl Pts',(-19.2845564519754,-50.034610279145,122.21236484356)) ;
#50066 = CARTESIAN_POINT('Ctrl Pts',(-19.25336832143,-49.8546211987822,121.912502122807)) ;
#50067 = CARTESIAN_POINT('Ctrl Pts',(-19.0811423574655,-50.0444622175212,
122.251384498715)) ;
#50068 = CARTESIAN_POINT('Ctrl Pts',(-18.9991000929311,-49.8644731371583,
121.961278882292)) ;
#50069 = CARTESIAN_POINT('Ctrl Pts',(-18.8847759421629,-50.0544531935459,
122.325861032936)) ;
#50070 = CARTESIAN_POINT('Ctrl Pts',(-18.7536426685323,-49.8744641131831,
122.054376600934)) ;
#50071 = CARTESIAN_POINT('Ctrl Pts',(-18.7055278261908,-50.0643710143496,
122.432422183055)) ;
#50072 = CARTESIAN_POINT('Ctrl Pts',(-18.5295831349131,-49.8843819339867,
122.187580190448)) ;
#50073 = CARTESIAN_POINT('Ctrl Pts',(-18.5457533128135,-50.0743997349142,
122.569951039098)) ;
#50074 = CARTESIAN_POINT('Ctrl Pts',(-18.3298664401693,-49.8944106545513,
122.359492881508)) ;
#50075 = CARTESIAN_POINT('Ctrl Pts',(-18.4140890328722,-50.0842826615234,
122.730702151589)) ;
#50076 = CARTESIAN_POINT('Ctrl Pts',(-18.1652873217021,-49.9042935811605,
122.56043375668)) ;
#50077 = CARTESIAN_POINT('Ctrl Pts',(-18.3108162869546,-50.0942869466428,
122.913895712092)) ;
#50078 = CARTESIAN_POINT('Ctrl Pts',(-18.0361983461571,-49.91429786628,122.789426912467)) ;
#50079 = CARTESIAN_POINT('Ctrl Pts',(-18.2410673724431,-50.1042706278507,
123.111893587272)) ;
#50080 = CARTESIAN_POINT('Ctrl Pts',(-17.949014297203,-49.9242815474878,123.036925185848)) ;
#50081 = CARTESIAN_POINT('Ctrl Pts',(-18.20680742649,-50.1143116265806,123.320172550146)) ;
#50082 = CARTESIAN_POINT('Ctrl Pts',(-17.9061915789435,-49.9343225462177,
123.297274155865)) ;
#50083 = CARTESIAN_POINT('Ctrl Pts',(-18.2088904962245,-50.1241440714477,
123.52687311072)) ;
#50084 = CARTESIAN_POINT('Ctrl Pts',(-17.9087977233851,-49.9441549910849,
123.555650792521)) ;
#50085 = CARTESIAN_POINT('Ctrl Pts',(-18.2468487955305,-50.1341390698781,
123.733536628154)) ;
#50086 = CARTESIAN_POINT('Ctrl Pts',(-17.9562480238635,-49.9541499895152,
123.81397987155)) ;
#50087 = CARTESIAN_POINT('Ctrl Pts',(-18.3208110885934,-50.1441706186277,
123.931048389592)) ;
#50088 = CARTESIAN_POINT('Ctrl Pts',(-18.0487030674048,-49.9641815382648,
124.060868717992)) ;
#50089 = CARTESIAN_POINT('Ctrl Pts',(-18.4259334331203,-50.1540359969332,
124.109821606205)) ;
#50090 = CARTESIAN_POINT('Ctrl Pts',(-18.1801084382992,-49.9740469165703,
124.284334653721)) ;
#50091 = CARTESIAN_POINT('Ctrl Pts',(-18.5613765662075,-50.1639978443934,
124.26956672375)) ;
#50092 = CARTESIAN_POINT('Ctrl Pts',(-18.3494144439518,-49.9840087640306,
124.484014610873)) ;
#50093 = CARTESIAN_POINT('Ctrl Pts',(-18.7238875342035,-50.1740327852077,
124.404073431431)) ;
#50094 = CARTESIAN_POINT('Ctrl Pts',(-18.5525546909306,-49.9940437048448,
124.652146083478)) ;
#50095 = CARTESIAN_POINT('Ctrl Pts',(-18.9044058295045,-50.1839177462248,
124.507085840432)) ;
#50096 = CARTESIAN_POINT('Ctrl Pts',(-18.7782043027359,-50.003928665862,124.780909685819)) ;
#50097 = CARTESIAN_POINT('Ctrl Pts',(-19.103599497382,-50.1939833551437,124.578405574943)) ;
#50098 = CARTESIAN_POINT('Ctrl Pts',(-19.0271970940224,-50.0139942747808,
124.870056934491)) ;
#50099 = CARTESIAN_POINT('Ctrl Pts',(-19.3074891707686,-50.2038225301854,
124.613469337633)) ;
#50100 = CARTESIAN_POINT('Ctrl Pts',(-19.2820603187455,-50.0238334498225,
124.913884244235)) ;
#50101 = CARTESIAN_POINT('Ctrl Pts',(-19.5190104294486,-50.2138850856853,
124.612870871899)) ;
#50102 = CARTESIAN_POINT('Ctrl Pts',(-19.5464617510403,-50.0338960053224,
124.913133557086)) ;
#50103 = CARTESIAN_POINT('Ctrl Pts',(-19.7237883029565,-50.2237822603782,
124.575939416995)) ;
#50104 = CARTESIAN_POINT('Ctrl Pts',(-19.8024340996347,-50.0437931800154,
124.866966630769)) ;
#50105 = CARTESIAN_POINT('Ctrl Pts',(-19.9199318195631,-50.2337129753016,
124.504433105692)) ;
#50106 = CARTESIAN_POINT('Ctrl Pts',(-20.0476128622874,-50.0537238949387,
124.777581121014)) ;
#50107 = CARTESIAN_POINT('Ctrl Pts',(-20.1026202548277,-50.2437570033792,
124.398553787405)) ;
#50108 = CARTESIAN_POINT('Ctrl Pts',(-20.2759720546877,-50.0637679230163,
124.645229703549)) ;
#50109 = CARTESIAN_POINT('Ctrl Pts',(-20.2617301651388,-50.2536432052325,
124.264811495273)) ;
#50110 = CARTESIAN_POINT('Ctrl Pts',(-20.4748580560086,-50.0736541248696,
124.478049522978)) ;
#50111 = CARTESIAN_POINT('Ctrl Pts',(-20.3968653014659,-50.2636363716993,
124.103982279919)) ;
#50112 = CARTESIAN_POINT('Ctrl Pts',(-20.6437749690615,-50.0836472913365,
124.277011182732)) ;
#50113 = CARTESIAN_POINT('Ctrl Pts',(-20.5015352977048,-50.2735758426865,
123.923098316065)) ;
#50114 = CARTESIAN_POINT('Ctrl Pts',(-20.7746102355523,-50.0935867623236,
124.050904663364)) ;
#50115 = CARTESIAN_POINT('Ctrl Pts',(-20.5737859343558,-50.2835923570407,
123.725325502378)) ;
#50116 = CARTESIAN_POINT('Ctrl Pts',(-20.8649209945911,-50.1036032766778,
123.803687664981)) ;
#50117 = CARTESIAN_POINT('Ctrl Pts',(-20.6104642438826,-50.2935223835175,
123.519782917965)) ;
#50118 = CARTESIAN_POINT('Ctrl Pts',(-20.9107662307901,-50.1135333031546,
123.546758707773)) ;
#50119 = CARTESIAN_POINT('Ctrl Pts',(-20.6108086522076,-50.303574919027,123.308465111307)) ;
#50120 = CARTESIAN_POINT('Ctrl Pts',(-20.9111940114087,-50.1235858386641,
123.282611468914)) ;
#50121 = CARTESIAN_POINT('Ctrl Pts',(-20.5753140283502,-50.3134213222466,
123.104521388382)) ;
#50122 = CARTESIAN_POINT('Ctrl Pts',(-20.8668229607071,-50.1334322418838,
123.02768188537)) ;
#50123 = CARTESIAN_POINT('Ctrl Pts',(-20.5047639569835,-50.3233833651007,
122.907340910753)) ;
#50124 = CARTESIAN_POINT('Ctrl Pts',(-20.7786326898469,-50.1433942847378,
122.781207115451)) ;
#50125 = CARTESIAN_POINT('Ctrl Pts',(-20.4001053609626,-50.3334119158914,
122.724304136021)) ;
#50126 = CARTESIAN_POINT('Ctrl Pts',(-20.6478070135381,-50.1534228355285,
122.552412487854)) ;
#50127 = CARTESIAN_POINT('Ctrl Pts',(-20.2669138933572,-50.343322241609,122.564103535408)) ;
#50128 = CARTESIAN_POINT('Ctrl Pts',(-20.4813154002532,-50.1633331612461,
122.352163354463)) ;
#50129 = CARTESIAN_POINT('Ctrl Pts',(-20.1078761445415,-50.3532571534386,
122.428702223204)) ;
#50130 = CARTESIAN_POINT('Ctrl Pts',(-20.2825162867384,-50.1732680730757,
122.182913771946)) ;
#50131 = CARTESIAN_POINT('Ctrl Pts',(-19.9257330097845,-50.3632981602067,
122.32201626754)) ;
#50132 = CARTESIAN_POINT('Ctrl Pts',(-20.0548359115821,-50.1833090798438,
122.049558725394)) ;
#50133 = CARTESIAN_POINT('Ctrl Pts',(-19.7308882493759,-50.3731857930389,
122.249563232581)) ;
#50134 = CARTESIAN_POINT('Ctrl Pts',(-19.8112788264307,-50.193196712676,121.958995011386)) ;
#50135 = CARTESIAN_POINT('Ctrl Pts',(-19.5243853029293,-50.3831762241369,
122.211289416377)) ;
#50136 = CARTESIAN_POINT('Ctrl Pts',(-19.5531495649687,-50.203187143774,121.911155500967)) ;
#50137 = CARTESIAN_POINT('Ctrl Pts',(-19.3150912519442,-50.3931316606941,
122.209571649096)) ;
#50138 = CARTESIAN_POINT('Ctrl Pts',(-19.2915318676096,-50.2131425803313,
121.909011127631)) ;
#50139 = CARTESIAN_POINT('Ctrl Pts',(-19.1095552736864,-50.4030426087935,
122.243685794913)) ;
#50140 = CARTESIAN_POINT('Ctrl Pts',(-19.0346123538421,-50.2230535284306,
121.951656547324)) ;
#50141 = CARTESIAN_POINT('Ctrl Pts',(-18.9109486179919,-50.4130546848912,
122.313456614259)) ;
#50142 = CARTESIAN_POINT('Ctrl Pts',(-18.7863546985664,-50.2330656045283,
122.038872975967)) ;
#50143 = CARTESIAN_POINT('Ctrl Pts',(-18.727435602444,-50.4230820069661,122.417161220471)) ;
#50144 = CARTESIAN_POINT('Ctrl Pts',(-18.5569655230889,-50.2430929266033,
122.168505406507)) ;
#50145 = CARTESIAN_POINT('Ctrl Pts',(-18.5670779315736,-50.4329407819203,
122.548532884562)) ;
#50146 = CARTESIAN_POINT('Ctrl Pts',(-18.3565173091822,-50.2529517015574,
122.332725267675)) ;
#50147 = CARTESIAN_POINT('Ctrl Pts',(-18.3833334191599,-50.4463669747327,
122.762717425023)) ;
#50148 = CARTESIAN_POINT('Ctrl Pts',(-18.126853897068,-50.2663778943698,122.600443072369)) ;
#50149 = CARTESIAN_POINT('Ctrl Pts',(-18.2623681721055,-50.4594509905141,
123.013391436687)) ;
#50150 = CARTESIAN_POINT('Ctrl Pts',(-17.975652168747,-50.2794619101513,122.913754436189)) ;
#50151 = CARTESIAN_POINT('Ctrl Pts',(-18.2092179613212,-50.4729244392694,
123.29151187479)) ;
#50152 = CARTESIAN_POINT('Ctrl Pts',(-17.909201931477,-50.2929353589065,123.261460162963)) ;
#50153 = CARTESIAN_POINT('Ctrl Pts',(-18.2065405992436,-50.4827573970752,
123.498250206426)) ;
#50154 = CARTESIAN_POINT('Ctrl Pts',(-17.9058612706939,-50.3027683167123,
123.519872041659)) ;
#50155 = CARTESIAN_POINT('Ctrl Pts',(-18.2393587707171,-50.4927206705259,
123.705106522157)) ;
#50156 = CARTESIAN_POINT('Ctrl Pts',(-17.9468858271895,-50.312731590163,123.778444889116)) ;
#50157 = CARTESIAN_POINT('Ctrl Pts',(-18.3085355723821,-50.5027577443438,
123.904453594488)) ;
#50158 = CARTESIAN_POINT('Ctrl Pts',(-18.0333597051189,-50.322768663981,124.027627149675)) ;
#50159 = CARTESIAN_POINT('Ctrl Pts',(-18.409286084184,-50.5126327473555,124.085999426355)) ;
#50160 = CARTESIAN_POINT('Ctrl Pts',(-18.1593001786209,-50.3326436669926,
124.254558222492)) ;
#50161 = CARTESIAN_POINT('Ctrl Pts',(-18.5425517962584,-50.5227004269817,
124.250393752023)) ;
#50162 = CARTESIAN_POINT('Ctrl Pts',(-18.3258841681713,-50.3427113466188,
124.460049111905)) ;
#50163 = CARTESIAN_POINT('Ctrl Pts',(-18.6986982462725,-50.5325412771994,
124.386149557232)) ;
#50164 = CARTESIAN_POINT('Ctrl Pts',(-18.5210703743217,-50.3525521968365,
124.629743114865)) ;
#50165 = CARTESIAN_POINT('Ctrl Pts',(-18.9386955742681,-50.5458774756753,
124.531065619422)) ;
#50166 = CARTESIAN_POINT('Ctrl Pts',(-18.8210606852671,-50.3658883953125,
124.810877501075)) ;
#50167 = CARTESIAN_POINT('Ctrl Pts',(-19.2087059356425,-50.5590949994898,
124.609228100724)) ;
#50168 = CARTESIAN_POINT('Ctrl Pts',(-19.1585310682997,-50.3791059191269,
124.908576997203)) ;
#50169 = CARTESIAN_POINT('Ctrl Pts',(-19.488920896454,-50.572429925981,124.615199991677)) ;
#50170 = CARTESIAN_POINT('Ctrl Pts',(-19.5088595130066,-50.3924408456182,
124.916046147867)) ;
#50171 = CARTESIAN_POINT('Ctrl Pts',(-19.6963926036681,-50.5824130265756,
124.583239687426)) ;
#50172 = CARTESIAN_POINT('Ctrl Pts',(-19.7681867122454,-50.4024239462128,
124.876091752188)) ;
#50173 = CARTESIAN_POINT('Ctrl Pts',(-19.8962274127877,-50.5924578024753,
124.515046658216)) ;
#50174 = CARTESIAN_POINT('Ctrl Pts',(-20.0179829922131,-50.4124687221124,
124.790847910221)) ;
#50175 = CARTESIAN_POINT('Ctrl Pts',(-20.0772393222898,-50.6022757256612,
124.415835187125)) ;
#50176 = CARTESIAN_POINT('Ctrl Pts',(-20.2442444733831,-50.4222866452983,
124.666833014598)) ;
#50177 = CARTESIAN_POINT('Ctrl Pts',(-20.2423226616433,-50.6123250396165,
124.284011355845)) ;
#50178 = CARTESIAN_POINT('Ctrl Pts',(-20.4505999318951,-50.4323359592536,
124.502045800867)) ;
#50179 = CARTESIAN_POINT('Ctrl Pts',(-20.4268261999454,-50.6256287802391,
124.073810716125)) ;
#50180 = CARTESIAN_POINT('Ctrl Pts',(-20.6812147142531,-50.4456396998762,
124.239319481561)) ;
#50181 = CARTESIAN_POINT('Ctrl Pts',(-20.5831565120962,-50.6421189757157,
123.759929328214)) ;
#50182 = CARTESIAN_POINT('Ctrl Pts',(-20.8766371020504,-50.4621298953529,
123.846918741757)) ;
#50183 = CARTESIAN_POINT('Ctrl Pts',(-20.6233943821416,-50.6588381406404,
123.40675844073)) ;
#50184 = CARTESIAN_POINT('Ctrl Pts',(-20.9269267933237,-50.4788490602775,
123.405534034858)) ;
#50185 = CARTESIAN_POINT('Ctrl Pts',(-20.5824794471599,-50.6719991343105,
123.133106842893)) ;
#50186 = CARTESIAN_POINT('Ctrl Pts',(-20.8757804021482,-50.4920100539476,
123.063406602128)) ;
#50187 = CARTESIAN_POINT('Ctrl Pts',(-20.516519250953,-50.6819953564158,122.933581400906)) ;
#50188 = CARTESIAN_POINT('Ctrl Pts',(-20.7933286314175,-50.5020062760529,
122.814013822185)) ;
#50189 = CARTESIAN_POINT('Ctrl Pts',(-20.4162173833348,-50.6920191959495,
122.748251975362)) ;
#50190 = CARTESIAN_POINT('Ctrl Pts',(-20.66794702487,-50.5120301155866,122.58234791319)) ;
#50191 = CARTESIAN_POINT('Ctrl Pts',(-20.2443086428061,-50.7052125179428,
122.530542353315)) ;
#50192 = CARTESIAN_POINT('Ctrl Pts',(-20.4530703195707,-50.5252234375799,
122.310222407941)) ;
#50193 = CARTESIAN_POINT('Ctrl Pts',(-19.9606322188696,-50.7218716897201,
122.318490004045)) ;
#50194 = CARTESIAN_POINT('Ctrl Pts',(-20.0984605249334,-50.5418826093572,
122.04515035663)) ;
#50195 = CARTESIAN_POINT('Ctrl Pts',(-19.5552783088555,-50.7417818652058,
122.196329453374)) ;
#50196 = CARTESIAN_POINT('Ctrl Pts',(-19.5917715291836,-50.5617927848429,
121.89245685484)) ;
#50197 = CARTESIAN_POINT('Ctrl Pts',(-19.1329219062142,-50.7616718530502,
122.218924903769)) ;
#50198 = CARTESIAN_POINT('Ctrl Pts',(-19.0638261203489,-50.5816827726873,
121.920703930916)) ;
#50199 = CARTESIAN_POINT('Ctrl Pts',(-18.7416302883475,-50.781677301065,122.385558421519)) ;
#50200 = CARTESIAN_POINT('Ctrl Pts',(-18.5747132438789,-50.6016882207021,
122.12899945876)) ;
#50201 = CARTESIAN_POINT('Ctrl Pts',(-18.4328824089552,-50.8015136950923,
122.673074672253)) ;
#50202 = CARTESIAN_POINT('Ctrl Pts',(-18.1887817456848,-50.6215246147294,
122.488396023025)) ;
#50203 = CARTESIAN_POINT('Ctrl Pts',(-18.2390777335758,-50.821521488989,123.051656272595)) ;
#50204 = CARTESIAN_POINT('Ctrl Pts',(-17.9465286197536,-50.6415324086261,
122.961624501261)) ;
#50205 = CARTESIAN_POINT('Ctrl Pts',(-18.1864063154851,-50.8413481252829,
123.469998542685)) ;
#50206 = CARTESIAN_POINT('Ctrl Pts',(-17.880692353325,-50.66135904492,123.484550765059)) ;
#50207 = CARTESIAN_POINT('Ctrl Pts',(-18.279598430072,-50.8613270682368,123.884440335655)) ;
#50208 = CARTESIAN_POINT('Ctrl Pts',(-17.9971845806245,-50.6813379878739,
124.002602226816)) ;
#50209 = CARTESIAN_POINT('Ctrl Pts',(-18.5086965529277,-50.8812588701058,
124.240917370752)) ;
#50210 = CARTESIAN_POINT('Ctrl Pts',(-18.2835587250181,-50.701269789743,124.448196582327)) ;
#50211 = CARTESIAN_POINT('Ctrl Pts',(-18.8431584214289,-50.9010831706034,
124.497674618011)) ;
#50212 = CARTESIAN_POINT('Ctrl Pts',(-18.7016353948024,-50.7210940902405,
124.769140330186)) ;
#50213 = CARTESIAN_POINT('Ctrl Pts',(-19.2506039421692,-50.9211791719433,
124.62581638792)) ;
#50214 = CARTESIAN_POINT('Ctrl Pts',(-19.2109425558882,-50.7411900915803,
124.929317666213)) ;
#50215 = CARTESIAN_POINT('Ctrl Pts',(-19.6705888408136,-50.9409375880472,
124.607973358778)) ;
#50216 = CARTESIAN_POINT('Ctrl Pts',(-19.7359254653028,-50.7609485076843,
124.90700825648)) ;
#50217 = CARTESIAN_POINT('Ctrl Pts',(-20.0654721859542,-50.9610312809313,
124.445475299511)) ;
#50218 = CARTESIAN_POINT('Ctrl Pts',(-20.2295077365795,-50.7810422005684,
124.703903011743)) ;
#50219 = CARTESIAN_POINT('Ctrl Pts',(-20.2716279154534,-50.9741422468379,
124.257625275152)) ;
#50220 = CARTESIAN_POINT('Ctrl Pts',(-20.4872438678407,-50.7941531664751,
124.469055541275)) ;
#50221 = CARTESIAN_POINT('Ctrl Pts',(-20.357892637621,-50.9808556216258,124.146615798218)) ;
#50222 = CARTESIAN_POINT('Ctrl Pts',(-20.5950497967257,-50.8008665412629,
124.330315451401)) ;
#50223 = CARTESIAN_POINT('',(-20.8451118641281,-12.0000000003486,123.237406291927)) ;
#50224 = CARTESIAN_POINT('Ctrl Pts',(-20.6521254138848,-12.1170415160268,
123.278341315447)) ;
#50225 = CARTESIAN_POINT('Ctrl Pts',(-20.6736893170551,-12.104042490247,123.276781066563)) ;
#50226 = CARTESIAN_POINT('Ctrl Pts',(-20.6956426458393,-12.0907896304746,
123.274049785805)) ;
#50227 = CARTESIAN_POINT('Ctrl Pts',(-20.7176046968127,-12.0775058642284,
123.270287525093)) ;
#50228 = CARTESIAN_POINT('Ctrl Pts',(-20.7393375909741,-12.0643607036855,
123.266564520626)) ;
#50229 = CARTESIAN_POINT('Ctrl Pts',(-20.7610782944406,-12.0511852792471,
123.261830892347)) ;
#50230 = CARTESIAN_POINT('Ctrl Pts',(-20.782453340365,-12.0381956240751,123.256276579118)) ;
#50231 = CARTESIAN_POINT('Ctrl Pts',(-20.8022914638292,-12.0261399595413,
123.251121635732)) ;
#50232 = CARTESIAN_POINT('Ctrl Pts',(-20.8218141748009,-12.0142443106129,
123.245260029577)) ;
#50233 = CARTESIAN_POINT('Ctrl Pts',(-20.8407272069771,-12.0026813802067,
123.238894624384)) ;
#50234 = CARTESIAN_POINT('Ctrl Pts',(-20.8421924596759,-12.0017855632469,
123.238401476217)) ;
#50235 = CARTESIAN_POINT('Ctrl Pts',(-20.8436540570881,-12.0008917432925,
123.237905329914)) ;
#50236 = CARTESIAN_POINT('Ctrl Pts',(-20.8451118646125,-12.0000000006492,
123.237406292805)) ;
#50237 = CARTESIAN_POINT('Ctrl Pts',(-20.8451118656667,-12.0000000000044,
123.237406292444)) ;
#50238 = CARTESIAN_POINT('Ctrl Pts',(-20.847700442803,-12.0000000000052,123.284550346716)) ;
#50239 = CARTESIAN_POINT('Ctrl Pts',(-20.8479707594182,-12.,123.331561909933)) ;
#50240 = CARTESIAN_POINT('Ctrl Pts',(-20.8459837280419,-12.,123.37822134492)) ;
#50241 = CARTESIAN_POINT('Ctrl Pts',(-20.8424452760623,-12.,123.461311210567)) ;
#50242 = CARTESIAN_POINT('Ctrl Pts',(-20.8317433199247,-12.,123.543372575294)) ;
#50243 = CARTESIAN_POINT('Ctrl Pts',(-20.8138854213481,-12.,123.624030867736)) ;
#50244 = CARTESIAN_POINT('Ctrl Pts',(-20.8018655450891,-12.,123.678320721061)) ;
#50245 = CARTESIAN_POINT('Ctrl Pts',(-20.7866123388131,-11.9999999780286,
123.73193986445)) ;
#50246 = CARTESIAN_POINT('Ctrl Pts',(-20.7684896206078,-11.9999999870879,
123.784085115621)) ;
#50247 = CARTESIAN_POINT('Ctrl Pts',(-20.759636032663,-11.9999999915136,123.809559912609)) ;
#50248 = CARTESIAN_POINT('Ctrl Pts',(-20.7500973712125,-12.,123.834683706848)) ;
#50249 = CARTESIAN_POINT('Ctrl Pts',(-20.7399146692478,-12.,123.859367148951)) ;
#50250 = CARTESIAN_POINT('Ctrl Pts',(-20.7147385522311,-12.,123.92039547217)) ;
#50251 = CARTESIAN_POINT('Ctrl Pts',(-20.6856174547214,-12.0000000184731,
123.97875125416)) ;
#50252 = CARTESIAN_POINT('Ctrl Pts',(-20.6525030990685,-12.0000000058446,
124.034758195809)) ;
#50253 = CARTESIAN_POINT('Ctrl Pts',(-20.644710021447,-12.0000000028726,124.047938776708)) ;
#50254 = CARTESIAN_POINT('Ctrl Pts',(-20.6366958712216,-12.,124.060989060861)) ;
#50255 = CARTESIAN_POINT('Ctrl Pts',(-20.6284602057521,-12.,124.073912891062)) ;
#50256 = CARTESIAN_POINT('Ctrl Pts',(-20.5990742768858,-12.,124.120026803335)) ;
#50257 = CARTESIAN_POINT('Ctrl Pts',(-20.5668676415575,-11.9999999840944,
124.164531604601)) ;
#50258 = CARTESIAN_POINT('Ctrl Pts',(-20.5324147688095,-11.9999999908829,
124.206739731105)) ;
#50259 = CARTESIAN_POINT('Ctrl Pts',(-20.5160790288264,-11.9999999941016,
124.226752604482)) ;
#50260 = CARTESIAN_POINT('Ctrl Pts',(-20.4992378958615,-12.,124.246249796365)) ;
#50261 = CARTESIAN_POINT('Ctrl Pts',(-20.4819503101481,-12.,124.26516140249)) ;
#50262 = CARTESIAN_POINT('Ctrl Pts',(-20.4318371386434,-12.,124.319982276665)) ;
#50263 = CARTESIAN_POINT('Ctrl Pts',(-20.3779831633315,-12.0000000080437,
124.369871658523)) ;
#50264 = CARTESIAN_POINT('Ctrl Pts',(-20.3205125767886,-12.000000000871,124.415059804215)) ;
#50265 = CARTESIAN_POINT('Ctrl Pts',(-20.3162101513788,-12.0000000003341,
124.418442728211)) ;
#50266 = CARTESIAN_POINT('Ctrl Pts',(-20.3118874716527,-12.,124.421799285237)) ;
#50267 = CARTESIAN_POINT('Ctrl Pts',(-20.3075445973449,-12.,124.425129563068)) ;
#50268 = CARTESIAN_POINT('Ctrl Pts',(-20.260709657936,-12.,124.461044339641)) ;
#50269 = CARTESIAN_POINT('Ctrl Pts',(-20.2115143902064,-11.9999999923458,
124.493911559955)) ;
#50270 = CARTESIAN_POINT('Ctrl Pts',(-20.1607019561465,-11.9999999967179,
124.523266658752)) ;
#50271 = CARTESIAN_POINT('Ctrl Pts',(-20.1437230877502,-11.9999999981788,
124.53307560352)) ;
#50272 = CARTESIAN_POINT('Ctrl Pts',(-20.1265633242237,-12.,124.542492681273)) ;
#50273 = CARTESIAN_POINT('Ctrl Pts',(-20.1092493826613,-12.,124.551501370856)) ;
#50274 = CARTESIAN_POINT('Ctrl Pts',(-20.0504925213261,-12.,124.582073399919)) ;
#50275 = CARTESIAN_POINT('Ctrl Pts',(-19.9900187394448,-11.9999999984792,
124.607913308289)) ;
#50276 = CARTESIAN_POINT('Ctrl Pts',(-19.9286682933254,-11.9999999996238,
124.62902433523)) ;
#50277 = CARTESIAN_POINT('Ctrl Pts',(-19.9176392817622,-11.9999999998296,
124.632819478949)) ;
#50278 = CARTESIAN_POINT('Ctrl Pts',(-19.9065818042026,-12.,124.636461817088)) ;
#50279 = CARTESIAN_POINT('Ctrl Pts',(-19.8955005664695,-12.,124.639951394143)) ;
#50280 = CARTESIAN_POINT('Ctrl Pts',(-19.8225767572884,-12.,124.66291572876)) ;
#50281 = CARTESIAN_POINT('Ctrl Pts',(-19.7485397875236,-12.,124.679290222045)) ;
#50282 = CARTESIAN_POINT('Ctrl Pts',(-19.6735413567767,-12.,124.68913473109)) ;
#50283 = CARTESIAN_POINT('Ctrl Pts',(-19.6163274050979,-12.,124.696644798423)) ;
#50284 = CARTESIAN_POINT('Ctrl Pts',(-19.5585508018213,-11.9999999945779,
124.70035487014)) ;
#50285 = CARTESIAN_POINT('Ctrl Pts',(-19.501082391029,-11.9999999978038,124.700220064632)) ;
#50286 = CARTESIAN_POINT('Ctrl Pts',(-19.4831056672055,-11.9999999988129,
124.70017789605)) ;
#50287 = CARTESIAN_POINT('Ctrl Pts',(-19.4651587236123,-12.,124.699759581626)) ;
#50288 = CARTESIAN_POINT('Ctrl Pts',(-19.4472671863275,-12.,124.698963935301)) ;
#50289 = CARTESIAN_POINT('Ctrl Pts',(-19.3889308676436,-12.,124.696369687707)) ;
#50290 = CARTESIAN_POINT('Ctrl Pts',(-19.3312538085245,-11.9999999905181,
124.689768246184)) ;
#50291 = CARTESIAN_POINT('Ctrl Pts',(-19.2749239756733,-11.9999999963922,
124.679509940194)) ;
#50292 = CARTESIAN_POINT('Ctrl Pts',(-19.2585509511539,-11.9999999980996,
124.676528225409)) ;
#50293 = CARTESIAN_POINT('Ctrl Pts',(-19.2422914255352,-12.,124.673237459633)) ;
#50294 = CARTESIAN_POINT('Ctrl Pts',(-19.226161509904,-12.,124.669645992527)) ;
#50295 = CARTESIAN_POINT('Ctrl Pts',(-19.1608299156492,-12.,124.655099340383)) ;
#50296 = CARTESIAN_POINT('Ctrl Pts',(-19.0975570030699,-12.0000000087182,
124.63560435259)) ;
#50297 = CARTESIAN_POINT('Ctrl Pts',(-19.0361906764906,-12.0000000012434,
124.611239898637)) ;
#50298 = CARTESIAN_POINT('Ctrl Pts',(-19.0300689734446,-12.0000000004977,
124.608809380789)) ;
#50299 = CARTESIAN_POINT('Ctrl Pts',(-19.0239662846671,-12.,124.606330417063)) ;
#50300 = CARTESIAN_POINT('Ctrl Pts',(-19.0178824861837,-12.,124.603803095076)) ;
#50301 = CARTESIAN_POINT('Ctrl Pts',(-18.9993535486714,-12.,124.596105833028)) ;
#50302 = CARTESIAN_POINT('Ctrl Pts',(-18.9809968021315,-11.9999999988781,
124.58795874914)) ;
#50303 = CARTESIAN_POINT('Ctrl Pts',(-18.9628485324419,-11.9999999980959,
124.579378422602)) ;
#50304 = CARTESIAN_POINT('Ctrl Pts',(-18.2740109056134,-10.1799890803629,
123.800437437226)) ;
#50305 = CARTESIAN_POINT('Ctrl Pts',(-17.9901976315307,-9.9999999998824,123.897592500224)) ;
#50306 = CARTESIAN_POINT('Ctrl Pts',(-18.3189528014318,-10.186615931181,123.93177221557)) ;
#50307 = CARTESIAN_POINT('Ctrl Pts',(-18.0463587733103,-10.0066268507005,
124.061733136893)) ;
#50308 = CARTESIAN_POINT('Ctrl Pts',(-18.4544999825326,-10.199846557662,124.178242251159)) ;
#50309 = CARTESIAN_POINT('Ctrl Pts',(-18.2158202081591,-10.0198574771815,
124.369865791322)) ;
#50310 = CARTESIAN_POINT('Ctrl Pts',(-18.7737258963307,-10.2198221789206,
124.458448669119)) ;
#50311 = CARTESIAN_POINT('Ctrl Pts',(-18.6148367044047,-10.0398330984402,
124.720100586921)) ;
#50312 = CARTESIAN_POINT('Ctrl Pts',(-19.1683517049307,-10.2397395138226,
124.612076715426)) ;
#50313 = CARTESIAN_POINT('Ctrl Pts',(-19.1081207669815,-10.0597504333421,
124.91214190006)) ;
#50314 = CARTESIAN_POINT('Ctrl Pts',(-19.5908221387894,-10.2596127905386,
124.622761896565)) ;
#50315 = CARTESIAN_POINT('Ctrl Pts',(-19.6362061149637,-10.0796237100581,
124.925498515678)) ;
#50316 = CARTESIAN_POINT('Ctrl Pts',(-19.9944586595383,-10.2796372807025,
124.487357143018)) ;
#50317 = CARTESIAN_POINT('Ctrl Pts',(-20.1407529321144,-10.0996482002221,
124.756244590511)) ;
#50318 = CARTESIAN_POINT('Ctrl Pts',(-20.3250726893908,-10.2995051218533,
124.224284503461)) ;
#50319 = CARTESIAN_POINT('Ctrl Pts',(-20.5540202997451,-10.1195160413728,
124.427406225565)) ;
#50320 = CARTESIAN_POINT('Ctrl Pts',(-20.5474404603406,-10.3194507727328,
123.863209826147)) ;
#50321 = CARTESIAN_POINT('Ctrl Pts',(-20.8319818409441,-10.1394616922523,
123.976064807505)) ;
#50322 = CARTESIAN_POINT('Ctrl Pts',(-20.6329204930996,-10.3393561733498,
123.448689022605)) ;
#50323 = CARTESIAN_POINT('Ctrl Pts',(-20.9388342402948,-10.1593670928693,
123.457915382841)) ;
#50324 = CARTESIAN_POINT('Ctrl Pts',(-20.5727382583942,-10.3592304011661,
123.030414178423)) ;
#50325 = CARTESIAN_POINT('Ctrl Pts',(-20.8636098404201,-10.1792413206857,
122.935072644665)) ;
#50326 = CARTESIAN_POINT('Ctrl Pts',(-20.3723372035374,-10.3792161920437,
122.655670923463)) ;
#50327 = CARTESIAN_POINT('Ctrl Pts',(-20.6131115835654,-10.1992271115633,
122.466642059104)) ;
#50328 = CARTESIAN_POINT('Ctrl Pts',(-20.0574028124706,-10.3991104347035,
122.373313004285)) ;
#50329 = CARTESIAN_POINT('Ctrl Pts',(-20.2194466572948,-10.219121354223,122.11369274918)) ;
#50330 = CARTESIAN_POINT('Ctrl Pts',(-19.6656681691958,-10.4189891507756,
122.214436559376)) ;
#50331 = CARTESIAN_POINT('Ctrl Pts',(-19.7297807740349,-10.2390000702951,
121.915093775182)) ;
#50332 = CARTESIAN_POINT('Ctrl Pts',(-19.2398981074651,-10.4390286006202,
122.199163423108)) ;
#50333 = CARTESIAN_POINT('Ctrl Pts',(-19.1975679684493,-10.2590395201397,
121.895998337618)) ;
#50334 = CARTESIAN_POINT('Ctrl Pts',(-18.8378689724914,-10.458891762158,122.328984896592)) ;
#50335 = CARTESIAN_POINT('Ctrl Pts',(-18.6950312338989,-10.2789026816776,
122.058270950061)) ;
#50336 = CARTESIAN_POINT('Ctrl Pts',(-18.5023795521869,-10.4788711301723,
122.589370841986)) ;
#50337 = CARTESIAN_POINT('Ctrl Pts',(-18.2756669290296,-10.2988820496918,
122.383749835429)) ;
#50338 = CARTESIAN_POINT('Ctrl Pts',(-18.2772917542457,-10.4986817106951,
122.945518138246)) ;
#50339 = CARTESIAN_POINT('Ctrl Pts',(-17.9943038603936,-10.3186926302146,
122.828930487485)) ;
#50340 = CARTESIAN_POINT('Ctrl Pts',(-18.1858955375249,-10.5186626389807,
123.360335745372)) ;
#50341 = CARTESIAN_POINT('Ctrl Pts',(-17.88005400599,-10.3386735585002,123.347451469635)) ;
#50342 = CARTESIAN_POINT('Ctrl Pts',(-18.2415877544767,-10.5385553108501,
123.779674054783)) ;
#50343 = CARTESIAN_POINT('Ctrl Pts',(-17.9496636134843,-10.3585662303696,
123.871624239583)) ;
#50344 = CARTESIAN_POINT('Ctrl Pts',(-18.4366892236376,-10.5584816411372,
124.155765874511)) ;
#50345 = CARTESIAN_POINT('Ctrl Pts',(-18.1935384903263,-10.3784925606567,
124.341742095362)) ;
#50346 = CARTESIAN_POINT('Ctrl Pts',(-18.7493758900079,-10.5784521952295,
124.443056780365)) ;
#50347 = CARTESIAN_POINT('Ctrl Pts',(-18.5843830564956,-10.398463114749,124.700856014448)) ;
#50348 = CARTESIAN_POINT('Ctrl Pts',(-19.0736750036282,-10.5949840343171,
124.578605622473)) ;
#50349 = CARTESIAN_POINT('Ctrl Pts',(-18.9897866675444,-10.4149949538366,
124.87030674853)) ;
#50350 = CARTESIAN_POINT('Ctrl Pts',(-19.3515822133367,-10.6083237731447,
124.616534422033)) ;
#50351 = CARTESIAN_POINT('Ctrl Pts',(-19.3371420473512,-10.4283346926642,
124.917711789974)) ;
#50352 = CARTESIAN_POINT('Ctrl Pts',(-19.5623087353055,-10.6183560153633,
124.608012512987)) ;
#50353 = CARTESIAN_POINT('Ctrl Pts',(-19.6005562667581,-10.4383669348828,
124.907063768978)) ;
#50354 = CARTESIAN_POINT('Ctrl Pts',(-19.7648570829155,-10.6282137160067,
124.564122231623)) ;
#50355 = CARTESIAN_POINT('Ctrl Pts',(-19.8537397871316,-10.4482246355263,
124.852203726934)) ;
#50356 = CARTESIAN_POINT('Ctrl Pts',(-19.9594412369529,-10.638205580646,124.485025335786)) ;
#50357 = CARTESIAN_POINT('Ctrl Pts',(-20.0969735540684,-10.4582165001655,
124.753332920259)) ;
#50358 = CARTESIAN_POINT('Ctrl Pts',(-20.1360906792147,-10.6481281304061,
124.374071893985)) ;
#50359 = CARTESIAN_POINT('Ctrl Pts',(-20.3177787347582,-10.4681390499256,
124.614652183523)) ;
#50360 = CARTESIAN_POINT('Ctrl Pts',(-20.3435921685771,-10.6614059038996,
124.187345412144)) ;
#50361 = CARTESIAN_POINT('Ctrl Pts',(-20.5771970982889,-10.4814168234191,
124.381203459018)) ;
#50362 = CARTESIAN_POINT('Ctrl Pts',(-20.4979359412099,-10.6747532428402,
123.949230531229)) ;
#50363 = CARTESIAN_POINT('Ctrl Pts',(-20.7701003709952,-10.4947641623597,
124.083584310545)) ;
#50364 = CARTESIAN_POINT('Ctrl Pts',(-20.5838202221108,-10.6879604746334,
123.685128933396)) ;
#50365 = CARTESIAN_POINT('Ctrl Pts',(-20.8774553695642,-10.5079713941529,
123.753475217099)) ;
#50366 = CARTESIAN_POINT('Ctrl Pts',(-20.6134756841563,-10.6979475907231,
123.477310674119)) ;
#50367 = CARTESIAN_POINT('Ctrl Pts',(-20.9145282393183,-10.5179585102426,
123.493699384286)) ;
#50368 = CARTESIAN_POINT('Ctrl Pts',(-20.6067552821165,-10.7078984963028,
123.26817900999)) ;
#50369 = CARTESIAN_POINT('Ctrl Pts',(-20.9061303771679,-10.5279094158224,
123.232285620244)) ;
#50370 = CARTESIAN_POINT('Ctrl Pts',(-20.5631517199141,-10.7179535983103,
123.061365279476)) ;
#50371 = CARTESIAN_POINT('Ctrl Pts',(-20.8516285274051,-10.5379645178298,
122.97376743029)) ;
#50372 = CARTESIAN_POINT('Ctrl Pts',(-20.4864480135789,-10.7277752716314,
122.869632358223)) ;
#50373 = CARTESIAN_POINT('Ctrl Pts',(-20.7557521456489,-10.5477861911509,
122.734100762243)) ;
#50374 = CARTESIAN_POINT('Ctrl Pts',(-20.3753148949047,-10.7378337427063,
122.689756073264)) ;
#50375 = CARTESIAN_POINT('Ctrl Pts',(-20.6168357132107,-10.5578446622258,
122.509252277596)) ;
#50376 = CARTESIAN_POINT('Ctrl Pts',(-20.2362698429268,-10.7477583538828,
122.534165638144)) ;
#50377 = CARTESIAN_POINT('Ctrl Pts',(-20.4430403515289,-10.5677692734023,
122.314768071312)) ;
#50378 = CARTESIAN_POINT('Ctrl Pts',(-20.0174236370264,-10.7610356927832,
122.360928612314)) ;
#50379 = CARTESIAN_POINT('Ctrl Pts',(-20.1694406713987,-10.5810466123027,
122.098190251733)) ;
#50380 = CARTESIAN_POINT('Ctrl Pts',(-19.7578453903065,-10.7743345720208,
122.248851511266)) ;
#50381 = CARTESIAN_POINT('Ctrl Pts',(-19.8449850135388,-10.5943454915403,
121.958111265145)) ;
#50382 = CARTESIAN_POINT('Ctrl Pts',(-19.4824813143237,-10.7875734441915,
122.208088439905)) ;
#50383 = CARTESIAN_POINT('Ctrl Pts',(-19.5008057716461,-10.607584363711,121.907157355451)) ;
#50384 = CARTESIAN_POINT('Ctrl Pts',(-19.2721785775522,-10.7975800623281,
122.213521358078)) ;
#50385 = CARTESIAN_POINT('Ctrl Pts',(-19.2379220825648,-10.6175909818476,
121.913944971208)) ;
#50386 = CARTESIAN_POINT('Ctrl Pts',(-19.0656000898289,-10.8076110073896,
122.255887753777)) ;
#50387 = CARTESIAN_POINT('Ctrl Pts',(-18.9796997396923,-10.6276219269091,
121.966900411235)) ;
#50388 = CARTESIAN_POINT('Ctrl Pts',(-18.8727746571245,-10.8174671807414,
122.33177975615)) ;
#50389 = CARTESIAN_POINT('Ctrl Pts',(-18.7386663422547,-10.6374781002609,
122.061762842425)) ;
#50390 = CARTESIAN_POINT('Ctrl Pts',(-18.6933942950045,-10.8274664517043,
122.441317819794)) ;
#50391 = CARTESIAN_POINT('Ctrl Pts',(-18.5144394577593,-10.6474773712238,
122.198683103259)) ;
#50392 = CARTESIAN_POINT('Ctrl Pts',(-18.5371942685893,-10.8373609034616,
122.578747643145)) ;
#50393 = CARTESIAN_POINT('Ctrl Pts',(-18.3191873795342,-10.6573718229811,
122.370468477296)) ;
#50394 = CARTESIAN_POINT('Ctrl Pts',(-18.4051122896899,-10.847424219271,122.743966469464)) ;
#50395 = CARTESIAN_POINT('Ctrl Pts',(-18.1540827675879,-10.6674351387905,
122.576990252157)) ;
#50396 = CARTESIAN_POINT('Ctrl Pts',(-18.3057391169289,-10.8572630760106,
122.925417587621)) ;
#50397 = CARTESIAN_POINT('Ctrl Pts',(-18.0298636945232,-10.6772739955301,
122.80380319054)) ;
#50398 = CARTESIAN_POINT('Ctrl Pts',(-18.2376490708675,-10.8673291978282,
123.125750203822)) ;
#50399 = CARTESIAN_POINT('Ctrl Pts',(-17.9447485716292,-10.6873401173477,
123.054218033055)) ;
#50400 = CARTESIAN_POINT('Ctrl Pts',(-18.2060503452321,-10.8772124255524,
123.331137906529)) ;
#50401 = CARTESIAN_POINT('Ctrl Pts',(-17.9052474069522,-10.697223345072,123.310952604454)) ;
#50402 = CARTESIAN_POINT('Ctrl Pts',(-18.2101816179164,-10.8872018868312,
123.541086163132)) ;
#50403 = CARTESIAN_POINT('Ctrl Pts',(-17.9104088181944,-10.7072128063507,
123.573388107833)) ;
#50404 = CARTESIAN_POINT('Ctrl Pts',(-18.2506800550467,-10.8971655972577,
123.746612755988)) ;
#50405 = CARTESIAN_POINT('Ctrl Pts',(-17.9610292608973,-10.7171765167772,
123.830297050036)) ;
#50406 = CARTESIAN_POINT('Ctrl Pts',(-18.3262823417106,-10.9071605999886,
123.942684202324)) ;
#50407 = CARTESIAN_POINT('Ctrl Pts',(-18.0555296750301,-10.7271715195081,
124.075387412866)) ;
#50408 = CARTESIAN_POINT('Ctrl Pts',(-18.4354992661144,-10.9171969309989,
124.123200848044)) ;
#50409 = CARTESIAN_POINT('Ctrl Pts',(-18.1920485021804,-10.7372078505184,
124.301034604056)) ;
#50410 = CARTESIAN_POINT('Ctrl Pts',(-18.5715282260324,-10.9270431603412,
124.279245467908)) ;
#50411 = CARTESIAN_POINT('Ctrl Pts',(-18.3620830672947,-10.7470540798607,
124.496092551368)) ;
#50412 = CARTESIAN_POINT('Ctrl Pts',(-18.734581283145,-10.9370286586164,124.411415680481)) ;
#50413 = CARTESIAN_POINT('Ctrl Pts',(-18.5658978744819,-10.7570395781359,
124.661307440099)) ;
#50414 = CARTESIAN_POINT('Ctrl Pts',(-18.9171658090595,-10.9469635615994,
124.512917995207)) ;
#50415 = CARTESIAN_POINT('Ctrl Pts',(-18.7941275673887,-10.7669744811189,
124.788187738408)) ;
#50416 = CARTESIAN_POINT('Ctrl Pts',(-19.1170341754858,-10.9570210646946,
124.581816159323)) ;
#50417 = CARTESIAN_POINT('Ctrl Pts',(-19.0439620659481,-10.7770319842141,
124.87431287259)) ;
#50418 = CARTESIAN_POINT('Ctrl Pts',(-19.3209344460454,-10.9668427210651,
124.614507954261)) ;
#50419 = CARTESIAN_POINT('Ctrl Pts',(-19.2988377714655,-10.7868536405847,
124.915180256384)) ;
#50420 = CARTESIAN_POINT('Ctrl Pts',(-19.5323077477126,-10.9768987837303,
124.611618015789)) ;
#50421 = CARTESIAN_POINT('Ctrl Pts',(-19.5630543230825,-10.7969097032498,
124.911570311967)) ;
#50422 = CARTESIAN_POINT('Ctrl Pts',(-19.7375399994228,-10.9868394484335,
124.572149859508)) ;
#50423 = CARTESIAN_POINT('Ctrl Pts',(-19.8195954463956,-10.806850367953,124.862237558484)) ;
#50424 = CARTESIAN_POINT('Ctrl Pts',(-19.932315810984,-10.996743852382,124.498530010297)) ;
#50425 = CARTESIAN_POINT('Ctrl Pts',(-20.0630665621227,-10.8167547719015,
124.770214821818)) ;
#50426 = CARTESIAN_POINT('Ctrl Pts',(-20.1138352643569,-11.0067903373756,
124.39058103883)) ;
#50427 = CARTESIAN_POINT('Ctrl Pts',(-20.2899670416995,-10.8268012568951,
124.635280761928)) ;
#50428 = CARTESIAN_POINT('Ctrl Pts',(-20.271611629066,-11.0166865651873,124.254920335698)) ;
#50429 = CARTESIAN_POINT('Ctrl Pts',(-20.4871895042753,-10.8366974847068,
124.465706330345)) ;
#50430 = CARTESIAN_POINT('Ctrl Pts',(-20.4056065237285,-11.0267461487508,
124.09133118011)) ;
#50431 = CARTESIAN_POINT('Ctrl Pts',(-20.6546848717609,-10.8467570682703,
124.261221540637)) ;
#50432 = CARTESIAN_POINT('Ctrl Pts',(-20.5070605056192,-11.0365981584196,
123.910749358251)) ;
#50433 = CARTESIAN_POINT('Ctrl Pts',(-20.7815048416838,-10.8566090779391,
124.035494716895)) ;
#50434 = CARTESIAN_POINT('Ctrl Pts',(-20.5770451368418,-11.0465606898592,
123.713354618847)) ;
#50435 = CARTESIAN_POINT('Ctrl Pts',(-20.8689878384845,-10.8665716093787,
123.788751735745)) ;
#50436 = CARTESIAN_POINT('Ctrl Pts',(-20.6116136924991,-11.0565922380985,
123.505305288482)) ;
#50437 = CARTESIAN_POINT('Ctrl Pts',(-20.9122007991014,-10.8766031576181,
123.528690516746)) ;
#50438 = CARTESIAN_POINT('Ctrl Pts',(-20.6097611314172,-11.0664836493116,
123.297365165469)) ;
#50439 = CARTESIAN_POINT('Ctrl Pts',(-20.9098873497408,-10.8864945688311,
123.268764662023)) ;
#50440 = CARTESIAN_POINT('Ctrl Pts',(-20.5717257520097,-11.0764999030196,
123.090247708174)) ;
#50441 = CARTESIAN_POINT('Ctrl Pts',(-20.862345248179,-10.8965108225391,123.009867420348)) ;
#50442 = CARTESIAN_POINT('Ctrl Pts',(-20.4977797269794,-11.0865300058643,
122.892777790247)) ;
#50443 = CARTESIAN_POINT('Ctrl Pts',(-20.7699148715379,-10.9065409253838,
122.763029266248)) ;
#50444 = CARTESIAN_POINT('Ctrl Pts',(-20.3928580773295,-11.096386454818,122.714076335493)) ;
#50445 = CARTESIAN_POINT('Ctrl Pts',(-20.6387642263058,-10.9163973743375,
122.53965056498)) ;
#50446 = CARTESIAN_POINT('Ctrl Pts',(-20.2567901765193,-11.1063854655903,
122.553889016232)) ;
#50447 = CARTESIAN_POINT('Ctrl Pts',(-20.4686808695235,-10.9263963851098,
122.339414946257)) ;
#50448 = CARTESIAN_POINT('Ctrl Pts',(-20.0967506938251,-11.1162806825083,
122.420933108959)) ;
#50449 = CARTESIAN_POINT('Ctrl Pts',(-20.2686322563454,-10.9362916020278,
122.173218025888)) ;
#50450 = CARTESIAN_POINT('Ctrl Pts',(-19.9130792390864,-11.1263411978656,
122.316112855486)) ;
#50451 = CARTESIAN_POINT('Ctrl Pts',(-20.0390441622467,-10.9463521173851,
122.042191046808)) ;
#50452 = CARTESIAN_POINT('Ctrl Pts',(-19.7181773873714,-11.1361904912527,
122.246149401792)) ;
#50453 = CARTESIAN_POINT('Ctrl Pts',(-19.7954165502643,-10.9562014107722,
121.954734482314)) ;
#50454 = CARTESIAN_POINT('Ctrl Pts',(-19.5105138121636,-11.1462176669327,
122.209933979005)) ;
#50455 = CARTESIAN_POINT('Ctrl Pts',(-19.5358374377871,-10.9662285864522,
121.9094633788)) ;
#50456 = CARTESIAN_POINT('Ctrl Pts',(-19.2996733625681,-11.1562462425598,
122.210880868471)) ;
#50457 = CARTESIAN_POINT('Ctrl Pts',(-19.2722869357614,-10.9762571620794,
121.910644965915)) ;
#50458 = CARTESIAN_POINT('Ctrl Pts',(-19.0959460919219,-11.1660913361057,
122.247342057068)) ;
#50459 = CARTESIAN_POINT('Ctrl Pts',(-19.017626412583,-10.9861022556252,121.956219772702)) ;
#50460 = CARTESIAN_POINT('Ctrl Pts',(-18.8985578247058,-11.1760825775375,
122.319166361709)) ;
#50461 = CARTESIAN_POINT('Ctrl Pts',(-18.7708903037758,-10.996093497057,122.045998590294)) ;
#50462 = CARTESIAN_POINT('Ctrl Pts',(-18.7160448813455,-11.1861183586808,
122.425022343304)) ;
#50463 = CARTESIAN_POINT('Ctrl Pts',(-18.5427482921645,-11.0061292782003,
122.178316885851)) ;
#50464 = CARTESIAN_POINT('Ctrl Pts',(-18.5574679836989,-11.1959705644105,
122.558254372856)) ;
#50465 = CARTESIAN_POINT('Ctrl Pts',(-18.344525155852,-11.01598148393,122.344856285485)) ;
#50466 = CARTESIAN_POINT('Ctrl Pts',(-18.4224794756724,-11.2059326585275,
122.718377576205)) ;
#50467 = CARTESIAN_POINT('Ctrl Pts',(-18.1757880511084,-11.025943578047,122.545009574719)) ;
#50468 = CARTESIAN_POINT('Ctrl Pts',(-18.3169268323872,-11.2159552193546,
122.900738727932)) ;
#50469 = CARTESIAN_POINT('Ctrl Pts',(-18.0438458204898,-11.0359661388741,
122.772960142216)) ;
#50470 = CARTESIAN_POINT('Ctrl Pts',(-18.2451248266948,-11.2258829910061,
123.096732722796)) ;
#50471 = CARTESIAN_POINT('Ctrl Pts',(-17.9540915964206,-11.0458939105257,
123.017952668875)) ;
#50472 = CARTESIAN_POINT('Ctrl Pts',(-18.2080492813558,-11.235925375131,123.304558510364)) ;
#50473 = CARTESIAN_POINT('Ctrl Pts',(-17.9077456058753,-11.0559362946505,
123.277734456011)) ;
#50474 = CARTESIAN_POINT('Ctrl Pts',(-18.2075431826477,-11.2458145992016,
123.512472427979)) ;
#50475 = CARTESIAN_POINT('Ctrl Pts',(-17.9071113954451,-11.0658255187211,
123.537627775353)) ;
#50476 = CARTESIAN_POINT('Ctrl Pts',(-18.2431137932323,-11.2558038473689,
123.719436413788)) ;
#50477 = CARTESIAN_POINT('Ctrl Pts',(-17.9515732676146,-11.0758147668884,
123.796333212602)) ;
#50478 = CARTESIAN_POINT('Ctrl Pts',(-18.3140127800185,-11.2657624244109,
123.916420734498)) ;
#50479 = CARTESIAN_POINT('Ctrl Pts',(-18.0401957305614,-11.0857733439304,
124.042564530928)) ;
#50480 = CARTESIAN_POINT('Ctrl Pts',(-18.4169840173117,-11.2756619935022,
124.097296523522)) ;
#50481 = CARTESIAN_POINT('Ctrl Pts',(-18.1689090610639,-11.0956729130217,
124.268660685229)) ;
#50482 = CARTESIAN_POINT('Ctrl Pts',(-18.5518230953768,-11.2857099055862,
124.259873078024)) ;
#50483 = CARTESIAN_POINT('Ctrl Pts',(-18.3374567293609,-11.1057208251057,
124.471882073921)) ;
#50484 = CARTESIAN_POINT('Ctrl Pts',(-18.7103328750192,-11.2956052598934,
124.394651304533)) ;
#50485 = CARTESIAN_POINT('Ctrl Pts',(-18.53559381129,-11.1156161794129,124.640356432315)) ;
#50486 = CARTESIAN_POINT('Ctrl Pts',(-18.8927897807584,-11.3056669103846,
124.50162581541)) ;
#50487 = CARTESIAN_POINT('Ctrl Pts',(-18.7636640135305,-11.1256778299041,
124.774075514003)) ;
#50488 = CARTESIAN_POINT('Ctrl Pts',(-19.0867894285585,-11.315511525847,124.573745609378)) ;
#50489 = CARTESIAN_POINT('Ctrl Pts',(-19.0061643663833,-11.1355224453666,
124.864226909417)) ;
#50490 = CARTESIAN_POINT('Ctrl Pts',(-19.2926054693123,-11.3254716047484,
124.612260164776)) ;
#50491 = CARTESIAN_POINT('Ctrl Pts',(-19.263434682634,-11.145482524268,124.912371167907)) ;
#50492 = CARTESIAN_POINT('Ctrl Pts',(-19.5036241030656,-11.3355097991068,
124.6140594671)) ;
#50493 = CARTESIAN_POINT('Ctrl Pts',(-19.5272078042134,-11.1555207186263,
124.914621442972)) ;
#50494 = CARTESIAN_POINT('Ctrl Pts',(-19.7084368116268,-11.3453835145064,
124.580138707835)) ;
#50495 = CARTESIAN_POINT('Ctrl Pts',(-19.7832249579071,-11.1653944340259,
124.872221302339)) ;
#50496 = CARTESIAN_POINT('Ctrl Pts',(-19.9081154986966,-11.3554552240407,
124.509785415039)) ;
#50497 = CARTESIAN_POINT('Ctrl Pts',(-20.0328232712861,-11.1754661435602,
124.784280775746)) ;
#50498 = CARTESIAN_POINT('Ctrl Pts',(-20.0882613339957,-11.3652876644932,
124.408381333972)) ;
#50499 = CARTESIAN_POINT('Ctrl Pts',(-20.2580073161576,-11.1852985840127,
124.657525797751)) ;
#50500 = CARTESIAN_POINT('Ctrl Pts',(-20.251660229155,-11.3753194854186,124.275048143701)) ;
#50501 = CARTESIAN_POINT('Ctrl Pts',(-20.4622563155218,-11.1953304049381,
124.490859965189)) ;
#50502 = CARTESIAN_POINT('Ctrl Pts',(-20.388818370831,-11.3853398553042,124.115153399644)) ;
#50503 = CARTESIAN_POINT('Ctrl Pts',(-20.6337047074071,-11.2053507748237,
124.290992198971)) ;
#50504 = CARTESIAN_POINT('Ctrl Pts',(-20.4949578126602,-11.3952066264379,
123.936918605361)) ;
#50505 = CARTESIAN_POINT('Ctrl Pts',(-20.7663802890228,-11.2152175459574,
124.068198059802)) ;
#50506 = CARTESIAN_POINT('Ctrl Pts',(-20.5700397801666,-11.4052773976273,
123.738981962488)) ;
#50507 = CARTESIAN_POINT('Ctrl Pts',(-20.8602333251997,-11.2252883171468,
123.820777914761)) ;
#50508 = CARTESIAN_POINT('Ctrl Pts',(-20.608748085118,-11.4151205581489,123.535688979496)) ;
#50509 = CARTESIAN_POINT('Ctrl Pts',(-20.9086197173424,-11.2351314776684,
123.566660443412)) ;
#50510 = CARTESIAN_POINT('Ctrl Pts',(-20.6122979783934,-11.4251007913353,
123.32590993056)) ;
#50511 = CARTESIAN_POINT('Ctrl Pts',(-20.9130575839416,-11.2451117108548,
123.304436329193)) ;
#50512 = CARTESIAN_POINT('Ctrl Pts',(-20.5788422571338,-11.4351193113705,
123.117968685033)) ;
#50513 = CARTESIAN_POINT('Ctrl Pts',(-20.8712385790231,-11.25513023089,123.044509679207)) ;
#50514 = CARTESIAN_POINT('Ctrl Pts',(-20.5111294875309,-11.4450026197542,
122.921507091262)) ;
#50515 = CARTESIAN_POINT('Ctrl Pts',(-20.7865977120134,-11.2650135392737,
122.798931493899)) ;
#50516 = CARTESIAN_POINT('Ctrl Pts',(-20.4083944122188,-11.455070903925,122.736483235784)) ;
#50517 = CARTESIAN_POINT('Ctrl Pts',(-20.6581795185986,-11.2750818234445,
122.567651782526)) ;
#50518 = CARTESIAN_POINT('Ctrl Pts',(-20.278392781555,-11.4649010305926,122.575789839308)) ;
#50519 = CARTESIAN_POINT('Ctrl Pts',(-20.4956768375376,-11.2849119501121,
122.366783576156)) ;
#50520 = CARTESIAN_POINT('Ctrl Pts',(-20.1189455476198,-11.4749676027992,
122.43668549405)) ;
#50521 = CARTESIAN_POINT('Ctrl Pts',(-20.2963683003265,-11.2949785223187,
122.19290316997)) ;
#50522 = CARTESIAN_POINT('Ctrl Pts',(-19.9408261904973,-11.4848577590399,
122.329373206102)) ;
#50523 = CARTESIAN_POINT('Ctrl Pts',(-20.07371839416,-11.3048686785594,122.058761956605)) ;
#50524 = CARTESIAN_POINT('Ctrl Pts',(-19.7449718071379,-11.4948502866163,
122.253435565076)) ;
#50525 = CARTESIAN_POINT('Ctrl Pts',(-19.8289002832583,-11.3148612061358,
121.963839656132)) ;
#50526 = CARTESIAN_POINT('Ctrl Pts',(-19.5394995838217,-11.5048117764906,
122.212958774971)) ;
#50527 = CARTESIAN_POINT('Ctrl Pts',(-19.572059601315,-11.3248226960101,121.913243324839)) ;
#50528 = CARTESIAN_POINT('Ctrl Pts',(-19.3312195995513,-11.5147209983778,
122.208316709471)) ;
#50529 = CARTESIAN_POINT('Ctrl Pts',(-19.3117087063637,-11.3347319178973,
121.907440658184)) ;
#50530 = CARTESIAN_POINT('Ctrl Pts',(-19.1224333832175,-11.5247695781881,
122.240425699493)) ;
#50531 = CARTESIAN_POINT('Ctrl Pts',(-19.0507261790371,-11.3447804977076,
121.947576761734)) ;
#50532 = CARTESIAN_POINT('Ctrl Pts',(-18.9256450998965,-11.5346525526582,
122.307117491957)) ;
#50533 = CARTESIAN_POINT('Ctrl Pts',(-18.8047397505395,-11.3546634721777,
122.030941792002)) ;
#50534 = CARTESIAN_POINT('Ctrl Pts',(-18.7411595782649,-11.5446474638009,
122.407688727702)) ;
#50535 = CARTESIAN_POINT('Ctrl Pts',(-18.5741327463721,-11.3646583833204,
122.156656021912)) ;
#50536 = CARTESIAN_POINT('Ctrl Pts',(-18.5766849466755,-11.5546678503745,
122.539338975724)) ;
#50537 = CARTESIAN_POINT('Ctrl Pts',(-18.3685394794627,-11.374678769894,122.321218804719)) ;
#50538 = CARTESIAN_POINT('Ctrl Pts',(-18.4390281447,-11.5645779542315,122.69570721258)) ;
#50539 = CARTESIAN_POINT('Ctrl Pts',(-18.1964679001567,-11.3845888737511,
122.51667981643)) ;
#50540 = CARTESIAN_POINT('Ctrl Pts',(-18.3299418694843,-11.5745056664414,
122.873650877876)) ;
#50541 = CARTESIAN_POINT('Ctrl Pts',(-18.0601098922916,-11.394516585961,122.739110167139)) ;
#50542 = CARTESIAN_POINT('Ctrl Pts',(-18.2526908814426,-11.5845487762087,
123.070140221989)) ;
#50543 = CARTESIAN_POINT('Ctrl Pts',(-17.9635464109793,-11.4045596957282,
122.984721718086)) ;
#50544 = CARTESIAN_POINT('Ctrl Pts',(-18.2112504293198,-11.5944351966642,
123.273822369061)) ;
#50545 = CARTESIAN_POINT('Ctrl Pts',(-17.9117458663191,-11.4144461161838,
123.239325516345)) ;
#50546 = CARTESIAN_POINT('Ctrl Pts',(-18.2053899399513,-11.6044283742699,
123.48381708741)) ;
#50547 = CARTESIAN_POINT('Ctrl Pts',(-17.9044206320669,-11.4244392937894,
123.501819128661)) ;
#50548 = CARTESIAN_POINT('Ctrl Pts',(-18.2360155974427,-11.6143740371738,
123.690651541286)) ;
#50549 = CARTESIAN_POINT('Ctrl Pts',(-17.9427031376008,-11.4343849566933,
123.760362733626)) ;
#50550 = CARTESIAN_POINT('Ctrl Pts',(-18.3016977196334,-11.624321333379,123.889202740392)) ;
#50551 = CARTESIAN_POINT('Ctrl Pts',(-18.0248064635829,-11.4443322528985,
124.00855211509)) ;
#50552 = CARTESIAN_POINT('Ctrl Pts',(-18.4020577550734,-11.6343690989569,
124.075068550386)) ;
#50553 = CARTESIAN_POINT('Ctrl Pts',(-18.1502567638643,-11.4543800184764,
124.240883955251)) ;
#50554 = CARTESIAN_POINT('Ctrl Pts',(-18.53043452236,-11.6442173121745,124.237499635771)) ;
#50555 = CARTESIAN_POINT('Ctrl Pts',(-18.3107289742964,-11.464228231694,124.443923603848)) ;
#50556 = CARTESIAN_POINT('Ctrl Pts',(-18.6863539195395,-11.6541768849686,
124.377247513015)) ;
#50557 = CARTESIAN_POINT('Ctrl Pts',(-18.50562907952,-11.4741878044881,124.618608196157)) ;
#50558 = CARTESIAN_POINT('Ctrl Pts',(-18.8657358234262,-11.6642135060011,
124.488337618152)) ;
#50559 = CARTESIAN_POINT('Ctrl Pts',(-18.7298566495651,-11.4842244255206,
124.757470221492)) ;
#50560 = CARTESIAN_POINT('Ctrl Pts',(-19.0585401018813,-11.6740940208114,
124.565687771704)) ;
#50561 = CARTESIAN_POINT('Ctrl Pts',(-18.9708633136044,-11.494104940331,124.85415763862)) ;
#50562 = CARTESIAN_POINT('Ctrl Pts',(-19.2653207495063,-11.6841466721185,
124.609197173488)) ;
#50563 = CARTESIAN_POINT('Ctrl Pts',(-19.2293390121218,-11.504157591638,124.908543575185)) ;
#50564 = CARTESIAN_POINT('Ctrl Pts',(-19.4732739400485,-11.6940420703985,
124.616120019601)) ;
#50565 = CARTESIAN_POINT('Ctrl Pts',(-19.4892814881059,-11.514052989918,124.917196362711)) ;
#50566 = CARTESIAN_POINT('Ctrl Pts',(-19.6824421140478,-11.7040921921046,
124.586475455409)) ;
#50567 = CARTESIAN_POINT('Ctrl Pts',(-19.7507413265629,-11.5241031116241,
124.88013986058)) ;
#50568 = CARTESIAN_POINT('Ctrl Pts',(-19.8800272774462,-11.7139764716465,
124.522061203542)) ;
#50569 = CARTESIAN_POINT('Ctrl Pts',(-19.9977235239475,-11.533987391166,124.799620909496)) ;
#50570 = CARTESIAN_POINT('Ctrl Pts',(-20.0656260604384,-11.7239712529384,
124.423592328542)) ;
#50571 = CARTESIAN_POINT('Ctrl Pts',(-20.2297217102498,-11.5439821724579,
124.6765338389)) ;
#50572 = CARTESIAN_POINT('Ctrl Pts',(-20.2305069833902,-11.7339190981252,
124.294916040327)) ;
#50573 = CARTESIAN_POINT('Ctrl Pts',(-20.4358226951657,-11.5539300176447,
124.515687379196)) ;
#50574 = CARTESIAN_POINT('Ctrl Pts',(-20.3705912261117,-11.7438560615126,
124.139963124901)) ;
#50575 = CARTESIAN_POINT('Ctrl Pts',(-20.6109276228693,-11.5638669810321,
124.321995035013)) ;
#50576 = CARTESIAN_POINT('Ctrl Pts',(-20.482403685854,-11.7538390262498,123.962322659801)) ;
#50577 = CARTESIAN_POINT('Ctrl Pts',(-20.7506923361084,-11.5738499457693,
124.099943608009)) ;
#50578 = CARTESIAN_POINT('Ctrl Pts',(-20.5617787036582,-11.7638828776654,
123.766682247549)) ;
#50579 = CARTESIAN_POINT('Ctrl Pts',(-20.8499100761848,-11.583893797185,123.855392878915)) ;
#50580 = CARTESIAN_POINT('Ctrl Pts',(-20.6055180822358,-11.7737110790002,
123.564713422646)) ;
#50581 = CARTESIAN_POINT('Ctrl Pts',(-20.9045834155349,-11.5937219985197,
123.602930177834)) ;
#50582 = CARTESIAN_POINT('Ctrl Pts',(-20.6138247387092,-11.7837876515982,
123.353078389392)) ;
#50583 = CARTESIAN_POINT('Ctrl Pts',(-20.9149654651719,-11.6037985711178,
123.338386769827)) ;
#50584 = CARTESIAN_POINT('Ctrl Pts',(-20.5859865681062,-11.7936397316058,
123.147790724545)) ;
#50585 = CARTESIAN_POINT('Ctrl Pts',(-20.880166307973,-11.6136506511253,123.081776137389)) ;
#50586 = CARTESIAN_POINT('Ctrl Pts',(-20.5217060175956,-11.8037130166099,
122.94604661898)) ;
#50587 = CARTESIAN_POINT('Ctrl Pts',(-20.7998144514066,-11.6237239361294,
122.82959680013)) ;
#50588 = CARTESIAN_POINT('Ctrl Pts',(-20.4255657745516,-11.8135543683204,
122.7628267317)) ;
#50589 = CARTESIAN_POINT('Ctrl Pts',(-20.6796373592565,-11.6335652878399,
122.600571403664)) ;
#50590 = CARTESIAN_POINT('Ctrl Pts',(-20.2981587765571,-11.8235158677169,
122.596634860964)) ;
#50591 = CARTESIAN_POINT('Ctrl Pts',(-20.5203770953298,-11.6435267872364,
122.392832222476)) ;
#50592 = CARTESIAN_POINT('Ctrl Pts',(-20.1424149976007,-11.8335516438469,
122.454293214028)) ;
#50593 = CARTESIAN_POINT('Ctrl Pts',(-20.3256964582165,-11.6535625633664,
122.214906329133)) ;
#50594 = CARTESIAN_POINT('Ctrl Pts',(-19.9670619376452,-11.8434400704844,
122.342638696447)) ;
#50595 = CARTESIAN_POINT('Ctrl Pts',(-20.1065035193812,-11.663450990004,122.075338994146)) ;
#50596 = CARTESIAN_POINT('Ctrl Pts',(-19.7726633460982,-11.8534553925594,
122.261733680716)) ;
#50597 = CARTESIAN_POINT('Ctrl Pts',(-19.8635046296482,-11.6734663120789,
121.974209274792)) ;
#50598 = CARTESIAN_POINT('Ctrl Pts',(-19.5667618955136,-11.8634857414596,
122.216223716099)) ;
#50599 = CARTESIAN_POINT('Ctrl Pts',(-19.6061275734969,-11.6834966609791,
121.917323321404)) ;
#50600 = CARTESIAN_POINT('Ctrl Pts',(-19.3600373542584,-11.8733291170662,
122.206909440911)) ;
#50601 = CARTESIAN_POINT('Ctrl Pts',(-19.347720607516,-11.6933400365858,121.905682077626)) ;
#50602 = CARTESIAN_POINT('Ctrl Pts',(-19.150888532225,-11.8833585539634,122.233670381781)) ;
#50603 = CARTESIAN_POINT('Ctrl Pts',(-19.0862848802304,-11.7033694734829,
121.93913503971)) ;
#50604 = CARTESIAN_POINT('Ctrl Pts',(-18.9496827788183,-11.8933904318963,
122.296907578933)) ;
#50605 = CARTESIAN_POINT('Ctrl Pts',(-18.8347782583479,-11.7134013514158,
122.018183058997)) ;
#50606 = CARTESIAN_POINT('Ctrl Pts',(-18.7661111079611,-11.9032200550018,
122.391777133203)) ;
#50607 = CARTESIAN_POINT('Ctrl Pts',(-18.6053133474058,-11.7232309745213,
122.13677215079)) ;
#50608 = CARTESIAN_POINT('Ctrl Pts',(-18.5987322084384,-11.9132095261549,
122.518627177409)) ;
#50609 = CARTESIAN_POINT('Ctrl Pts',(-18.3960907643913,-11.7332204456744,
122.295336373426)) ;
#50610 = CARTESIAN_POINT('Ctrl Pts',(-18.4555426602971,-11.9232533749173,
122.673809920536)) ;
#50611 = CARTESIAN_POINT('Ctrl Pts',(-18.2171052461789,-11.7432642944368,
122.489315907923)) ;
#50612 = CARTESIAN_POINT('Ctrl Pts',(-18.3436356389824,-11.933075080449,122.847337567212)) ;
#50613 = CARTESIAN_POINT('Ctrl Pts',(-18.0772224087066,-11.7530859999685,
122.70622755982)) ;
#50614 = CARTESIAN_POINT('Ctrl Pts',(-18.2613427697256,-11.9431101202768,
123.041592805838)) ;
#50615 = CARTESIAN_POINT('Ctrl Pts',(-17.9743582754355,-11.7631210397963,
122.949047319972)) ;
#50616 = CARTESIAN_POINT('Ctrl Pts',(-18.2146441937951,-11.9531348271682,
123.247112574505)) ;
#50617 = CARTESIAN_POINT('Ctrl Pts',(-17.9159869174325,-11.7731457466878,
123.205947428696)) ;
#50618 = CARTESIAN_POINT('Ctrl Pts',(-18.2040790572873,-11.962987531509,123.453976992299)) ;
#50619 = CARTESIAN_POINT('Ctrl Pts',(-17.9027824758796,-11.7829984510285,
123.464529062491)) ;
#50620 = CARTESIAN_POINT('Ctrl Pts',(-18.2295779813126,-11.9729756537167,
123.662389605254)) ;
#50621 = CARTESIAN_POINT('Ctrl Pts',(-17.9346582753254,-11.7929865732362,
123.725044751931)) ;
#50622 = CARTESIAN_POINT('Ctrl Pts',(-18.2905062794645,-11.982904123824,123.862032052655)) ;
#50623 = CARTESIAN_POINT('Ctrl Pts',(-18.0108208428839,-11.8029150433435,
123.974597685058)) ;
#50624 = CARTESIAN_POINT('Ctrl Pts',(-18.3854419619658,-11.9928931009912,
124.049358952293)) ;
#50625 = CARTESIAN_POINT('Ctrl Pts',(-18.1294925170237,-11.8129040205107,
124.208755459254)) ;
#50626 = CARTESIAN_POINT('Ctrl Pts',(-18.51235689706,-12.0029309082709,124.217948281748)) ;
#50627 = CARTESIAN_POINT('Ctrl Pts',(-18.288137840982,-11.8229418277904,124.419490767738)) ;
#50628 = CARTESIAN_POINT('Ctrl Pts',(-18.6634476701596,-12.0127772091342,
124.359445076949)) ;
#50629 = CARTESIAN_POINT('Ctrl Pts',(-18.4770035095754,-11.8327881286537,
124.596360779369)) ;
#50630 = CARTESIAN_POINT('Ctrl Pts',(-18.8397147754035,-12.0228029525135,
124.475014140463)) ;
#50631 = CARTESIAN_POINT('Ctrl Pts',(-18.6973386410408,-11.842813872033,124.740820127215)) ;
#50632 = CARTESIAN_POINT('Ctrl Pts',(-19.03368933323,-12.0328338189525,124.557760416671)) ;
#50633 = CARTESIAN_POINT('Ctrl Pts',(-18.9398076656581,-11.852844738472,124.844250930718)) ;
#50634 = CARTESIAN_POINT('Ctrl Pts',(-19.2350138531615,-12.0426711777513,
124.605047798355)) ;
#50635 = CARTESIAN_POINT('Ctrl Pts',(-19.191464763686,-11.8626820972708,124.903358127503)) ;
#50636 = CARTESIAN_POINT('Ctrl Pts',(-19.4447121805973,-12.052663138685,124.61740552715)) ;
#50637 = CARTESIAN_POINT('Ctrl Pts',(-19.4535879451902,-11.8726740582045,
124.918802860039)) ;
#50638 = CARTESIAN_POINT('Ctrl Pts',(-19.654174209039,-12.0626955012416,124.59264506007)) ;
#50639 = CARTESIAN_POINT('Ctrl Pts',(-19.7154151681685,-11.8827064207611,
124.887849956872)) ;
#50640 = CARTESIAN_POINT('Ctrl Pts',(-19.8528431822894,-12.072560661816,124.53314903407)) ;
#50641 = CARTESIAN_POINT('Ctrl Pts',(-19.9637513982511,-11.8925715813355,
124.813477415279)) ;
#50642 = CARTESIAN_POINT('Ctrl Pts',(-20.0402625333132,-12.0825225663937,
124.439673578487)) ;
#50643 = CARTESIAN_POINT('Ctrl Pts',(-20.1980246865614,-11.9025334859132,
124.696630723516)) ;
#50644 = CARTESIAN_POINT('Ctrl Pts',(-20.2096190237234,-12.0925574964694,
124.313895264945)) ;
#50645 = CARTESIAN_POINT('Ctrl Pts',(-20.4097188089495,-11.9125684159889,
124.539405883278)) ;
#50646 = CARTESIAN_POINT('Ctrl Pts',(-20.3526800116948,-12.102442443323,124.163124144137)) ;
#50647 = CARTESIAN_POINT('Ctrl Pts',(-20.5885436052506,-11.9224533628425,
124.350939834847)) ;
#50648 = CARTESIAN_POINT('Ctrl Pts',(-20.4694104296519,-12.1125081196345,
123.986661950019)) ;
#50649 = CARTESIAN_POINT('Ctrl Pts',(-20.7344544463685,-11.932519039154,124.13036082969)) ;
#50650 = CARTESIAN_POINT('Ctrl Pts',(-20.5520515995571,-12.1223470392694,
123.797005493285)) ;
#50651 = CARTESIAN_POINT('Ctrl Pts',(-20.8377538537587,-11.9423579587889,
123.893288587483)) ;
#50652 = CARTESIAN_POINT('Ctrl Pts',(-20.6018640316816,-12.1324105490038,
123.591417354039)) ;
#50653 = CARTESIAN_POINT('Ctrl Pts',(-20.9000168315464,-11.9524214685233,
123.636302931618)) ;
#50654 = CARTESIAN_POINT('Ctrl Pts',(-20.6148291614051,-12.1423041621656,
123.383802604213)) ;
#50655 = CARTESIAN_POINT('Ctrl Pts',(-20.9162207083321,-11.9623150816851,
123.376783859031)) ;
#50656 = CARTESIAN_POINT('Ctrl Pts',(-20.5919863900176,-12.152248168979,123.176028489943)) ;
#50657 = CARTESIAN_POINT('Ctrl Pts',(-20.8876645645134,-11.9722590884985,
123.117066234062)) ;
#50658 = CARTESIAN_POINT('Ctrl Pts',(-20.5331562624697,-12.1622491233333,
122.974141880329)) ;
#50659 = CARTESIAN_POINT('Ctrl Pts',(-20.8141243157822,-11.9822600428528,
122.864708641729)) ;
#50660 = CARTESIAN_POINT('Ctrl Pts',(-20.4394990832698,-12.1722878810256,
122.785036123018)) ;
#50661 = CARTESIAN_POINT('Ctrl Pts',(-20.6970504998674,-11.9922988005451,
122.628327620901)) ;
#50662 = CARTESIAN_POINT('Ctrl Pts',(-20.3174467550257,-12.1821120651956,
122.618401426981)) ;
#50663 = CARTESIAN_POINT('Ctrl Pts',(-20.5444825753375,-12.0021229847151,
122.420035360874)) ;
#50664 = CARTESIAN_POINT('Ctrl Pts',(-20.1650056351834,-12.192170130795,122.471888778406)) ;
#50665 = CARTESIAN_POINT('Ctrl Pts',(-20.353929339677,-12.0121810503145,122.236896566172)) ;
#50666 = CARTESIAN_POINT('Ctrl Pts',(-19.9914963261328,-12.2021001775697,
122.355781356402)) ;
#50667 = CARTESIAN_POINT('Ctrl Pts',(-20.1370409748098,-12.0221110970892,
122.09176436784)) ;
#50668 = CARTESIAN_POINT('Ctrl Pts',(-19.8002835579305,-12.2120516199068,
122.270882760811)) ;
#50669 = CARTESIAN_POINT('Ctrl Pts',(-19.8980237232306,-12.0320625394263,
121.985643564512)) ;
#50670 = CARTESIAN_POINT('Ctrl Pts',(-19.5952237413981,-12.2220984170861,
122.220273264171)) ;
#50671 = CARTESIAN_POINT('Ctrl Pts',(-19.641698308601,-12.0421093366056,121.922384338782)) ;
#50672 = CARTESIAN_POINT('Ctrl Pts',(-19.388673024252,-12.2319463577662,122.206126303153)) ;
#50673 = CARTESIAN_POINT('Ctrl Pts',(-19.3835093232641,-12.0519572772857,
121.904703348146)) ;
#50674 = CARTESIAN_POINT('Ctrl Pts',(-19.180367514707,-12.2419079891088,122.227663750523)) ;
#50675 = CARTESIAN_POINT('Ctrl Pts',(-19.1231275996939,-12.0619189086283,
121.931627958094)) ;
#50676 = CARTESIAN_POINT('Ctrl Pts',(-18.9776624918692,-12.2519366484847,
122.285690175812)) ;
#50677 = CARTESIAN_POINT('Ctrl Pts',(-18.869747044192,-12.0719475680042,122.004163670663)) ;
#50678 = CARTESIAN_POINT('Ctrl Pts',(-18.7903389023048,-12.2618469513729,
122.376871314838)) ;
#50679 = CARTESIAN_POINT('Ctrl Pts',(-18.6355935849324,-12.0818578708924,
122.118142692973)) ;
#50680 = CARTESIAN_POINT('Ctrl Pts',(-18.6209407245683,-12.2717818459351,
122.499062432989)) ;
#50681 = CARTESIAN_POINT('Ctrl Pts',(-18.4238474018539,-12.0917927654546,
122.270883952905)) ;
#50682 = CARTESIAN_POINT('Ctrl Pts',(-18.4739251947791,-12.281822944602,122.650538595866)) ;
#50683 = CARTESIAN_POINT('Ctrl Pts',(-18.2400799716367,-12.1018338641215,
122.460231143075)) ;
#50684 = CARTESIAN_POINT('Ctrl Pts',(-18.3571294374524,-12.2917102271064,
122.822498446866)) ;
#50685 = CARTESIAN_POINT('Ctrl Pts',(-18.094087509158,-12.1117211466259,122.67518267211)) ;
#50686 = CARTESIAN_POINT('Ctrl Pts',(-18.270751539422,-12.3017019676169,123.013960222828)) ;
#50687 = CARTESIAN_POINT('Ctrl Pts',(-17.9861176821352,-12.1217128871364,
122.914511116754)) ;
#50688 = CARTESIAN_POINT('Ctrl Pts',(-18.2192070084759,-12.3116525168523,
123.216713043698)) ;
#50689 = CARTESIAN_POINT('Ctrl Pts',(-17.9216897294066,-12.1316634363718,
123.167952928698)) ;
#50690 = CARTESIAN_POINT('Ctrl Pts',(-18.203364387181,-12.3215881944871,123.424977839185)) ;
#50691 = CARTESIAN_POINT('Ctrl Pts',(-17.9018892646537,-12.1415991140066,
123.42828420322)) ;
#50692 = CARTESIAN_POINT('Ctrl Pts',(-18.2238062767761,-12.3315736122799,
123.63392140019)) ;
#50693 = CARTESIAN_POINT('Ctrl Pts',(-17.9274444396139,-12.1515845317994,
123.689463440915)) ;
#50694 = CARTESIAN_POINT('Ctrl Pts',(-18.2807096673845,-12.3416024051504,
123.83693264531)) ;
#50695 = CARTESIAN_POINT('Ctrl Pts',(-17.9985764203864,-12.1616133246699,
123.943226816806)) ;
#50696 = CARTESIAN_POINT('Ctrl Pts',(-18.3704393887249,-12.3514819163783,
124.024245376824)) ;
#50697 = CARTESIAN_POINT('Ctrl Pts',(-18.1107411248912,-12.1714928358979,
124.177366527478)) ;
#50698 = CARTESIAN_POINT('Ctrl Pts',(-18.4923386110279,-12.3614754530513,
124.195371559684)) ;
#50699 = CARTESIAN_POINT('Ctrl Pts',(-18.2631174663862,-12.1814863725708,
124.391272663602)) ;
#50700 = CARTESIAN_POINT('Ctrl Pts',(-18.6429752247149,-12.3715077213151,
124.342978657029)) ;
#50701 = CARTESIAN_POINT('Ctrl Pts',(-18.4514152852325,-12.1915186408346,
124.575779592157)) ;
#50702 = CARTESIAN_POINT('Ctrl Pts',(-18.8138083567616,-12.381371683321,124.460571682728)) ;
#50703 = CARTESIAN_POINT('Ctrl Pts',(-18.6649582254015,-12.2013826028405,
124.722768521465)) ;
#50704 = CARTESIAN_POINT('Ctrl Pts',(-19.0063512318433,-12.3914417446659,
124.548529857693)) ;
#50705 = CARTESIAN_POINT('Ctrl Pts',(-18.905638121289,-12.2114526641854,124.832713751757)) ;
#50706 = CARTESIAN_POINT('Ctrl Pts',(-19.2066412567903,-12.4012841090146,
124.600516981642)) ;
#50707 = CARTESIAN_POINT('Ctrl Pts',(-19.1560012005411,-12.2212950285341,
124.897694900769)) ;
#50708 = CARTESIAN_POINT('Ctrl Pts',(-19.4153191948693,-12.4112447815171,
124.61790415066)) ;
#50709 = CARTESIAN_POINT('Ctrl Pts',(-19.4168488001027,-12.2312557010366,
124.919426126901)) ;
#50710 = CARTESIAN_POINT('Ctrl Pts',(-19.6254227673264,-12.4212828525849,
124.598226325567)) ;
#50711 = CARTESIAN_POINT('Ctrl Pts',(-19.6794781670687,-12.2412937721044,
124.894826056609)) ;
#50712 = CARTESIAN_POINT('Ctrl Pts',(-19.8257277780076,-12.4311564675453,
124.54365478677)) ;
#50713 = CARTESIAN_POINT('Ctrl Pts',(-19.9298584470985,-12.2511673870648,
124.826609084916)) ;
#50714 = CARTESIAN_POINT('Ctrl Pts',(-20.0172039066253,-12.4412287021266,
124.453332611574)) ;
#50715 = CARTESIAN_POINT('Ctrl Pts',(-20.1692027686534,-12.2612396216461,
124.713703675033)) ;
#50716 = CARTESIAN_POINT('Ctrl Pts',(-20.1860304534501,-12.4510527205754,
124.334292333234)) ;
#50717 = CARTESIAN_POINT('Ctrl Pts',(-20.3802336085828,-12.2710636400949,
124.56490174171)) ;
#50718 = CARTESIAN_POINT('Ctrl Pts',(-20.3353241205461,-12.4611176415514,
124.184411186943)) ;
#50719 = CARTESIAN_POINT('Ctrl Pts',(-20.5668505340547,-12.2811285610709,
124.377546847526)) ;
#50720 = CARTESIAN_POINT('Ctrl Pts',(-20.4942292788694,-12.4743279398461,
123.956554640027)) ;
#50721 = CARTESIAN_POINT('Ctrl Pts',(-20.7654710390159,-12.2943388593657,
124.092731380787)) ;
#50722 = CARTESIAN_POINT('Ctrl Pts',(-20.5910323234022,-12.4876433865781,
123.690569761034)) ;
#50723 = CARTESIAN_POINT('Ctrl Pts',(-20.8864681736876,-12.3076543060976,
123.760293059377)) ;
#50724 = CARTESIAN_POINT('Ctrl Pts',(-20.6153241142933,-12.5009336318454,
123.412181900129)) ;
#50725 = CARTESIAN_POINT('Ctrl Pts',(-20.9168412404455,-12.3209445513649,
123.412248798329)) ;
#50726 = CARTESIAN_POINT('Ctrl Pts',(-20.5967460044986,-12.5109843814525,
123.20173674764)) ;
#50727 = CARTESIAN_POINT('Ctrl Pts',(-20.8936136566243,-12.330995300972,123.149204261549)) ;
#50728 = CARTESIAN_POINT('Ctrl Pts',(-20.5435845802291,-12.5207969884347,
123.002381741764)) ;
#50729 = CARTESIAN_POINT('Ctrl Pts',(-20.8271599102325,-12.3408079079542,
122.900008574039)) ;
#50730 = CARTESIAN_POINT('Ctrl Pts',(-20.4546049045706,-12.530868086429,122.81028950204)) ;
#50731 = CARTESIAN_POINT('Ctrl Pts',(-20.71593398742,-12.3508790059485,122.659895486336)) ;
#50732 = CARTESIAN_POINT('Ctrl Pts',(-20.3356089336191,-12.5407576592038,
122.639785901111)) ;
#50733 = CARTESIAN_POINT('Ctrl Pts',(-20.5671825472654,-12.3607685787234,
122.446765213206)) ;
#50734 = CARTESIAN_POINT('Ctrl Pts',(-20.1392326312349,-12.5540277660071,
122.441591528531)) ;
#50735 = CARTESIAN_POINT('Ctrl Pts',(-20.3217335959038,-12.3740386855267,
122.199036770017)) ;
#50736 = CARTESIAN_POINT('Ctrl Pts',(-19.8341063016993,-12.5706444529296,
122.263562945351)) ;
#50737 = CARTESIAN_POINT('Ctrl Pts',(-19.9402799223981,-12.3906553724492,
121.976489962995)) ;
#50738 = CARTESIAN_POINT('Ctrl Pts',(-19.4873858216236,-12.5872184962459,
122.20023473755)) ;
#50739 = CARTESIAN_POINT('Ctrl Pts',(-19.5069560654211,-12.4072294157654,
121.897341845689)) ;
#50740 = CARTESIAN_POINT('Ctrl Pts',(-19.208770852032,-12.6005150636777,122.222555120843)) ;
#50741 = CARTESIAN_POINT('Ctrl Pts',(-19.1586250795814,-12.4205259831972,
121.925240968507)) ;
#50742 = CARTESIAN_POINT('Ctrl Pts',(-19.004699994285,-12.6105451272551,122.27569208682)) ;
#50743 = CARTESIAN_POINT('Ctrl Pts',(-18.9035497914933,-12.4305560467746,
121.99166480072)) ;
#50744 = CARTESIAN_POINT('Ctrl Pts',(-18.8155802354143,-12.6204390191043,
122.362230085653)) ;
#50745 = CARTESIAN_POINT('Ctrl Pts',(-18.6671468528082,-12.4404499386238,
122.099840645801)) ;
#50746 = CARTESIAN_POINT('Ctrl Pts',(-18.5855888789982,-12.6336917748899,
122.519603205496)) ;
#50747 = CARTESIAN_POINT('Ctrl Pts',(-18.3796682059846,-12.4537026944094,
122.29654963732)) ;
#50748 = CARTESIAN_POINT('Ctrl Pts',(-18.354522049861,-12.6504198798823,122.789922613237)) ;
#50749 = CARTESIAN_POINT('Ctrl Pts',(-18.0908280311932,-12.4704307994018,
122.634462100616)) ;
#50750 = CARTESIAN_POINT('Ctrl Pts',(-18.2063394457701,-12.6702507163608,
123.184767083892)) ;
#50751 = CARTESIAN_POINT('Ctrl Pts',(-17.9056069775823,-12.4902616358803,
123.128014485486)) ;
#50752 = CARTESIAN_POINT('Ctrl Pts',(-18.2007363155492,-12.690176108251,123.608303510177)) ;
#50753 = CARTESIAN_POINT('Ctrl Pts',(-17.8986058472055,-12.5101870277705,
123.657435239702)) ;
#50754 = CARTESIAN_POINT('Ctrl Pts',(-18.3400998829644,-12.710101321603,124.008460954811)) ;
#50755 = CARTESIAN_POINT('Ctrl Pts',(-18.072813481075,-12.5301122411225,124.157630024527)) ;
#50756 = CARTESIAN_POINT('Ctrl Pts',(-18.6074924622381,-12.7300263350881,
124.337014382701)) ;
#50757 = CARTESIAN_POINT('Ctrl Pts',(-18.4070561282593,-12.5500372546076,
124.568319257499)) ;
#50758 = CARTESIAN_POINT('Ctrl Pts',(-18.9698313696597,-12.7499028067881,
124.554607895198)) ;
#50759 = CARTESIAN_POINT('Ctrl Pts',(-18.8599799730538,-12.5699137263076,
124.840308097152)) ;
#50760 = CARTESIAN_POINT('Ctrl Pts',(-19.3867523160162,-12.7698821246969,
124.636089846791)) ;
#50761 = CARTESIAN_POINT('Ctrl Pts',(-19.3811313633257,-12.5898930442165,
124.942158139895)) ;
#50762 = CARTESIAN_POINT('Ctrl Pts',(-19.8054691433214,-12.7898151282729,
124.570240660478)) ;
#50763 = CARTESIAN_POINT('Ctrl Pts',(-19.904526260389,-12.6098260477925,124.859844414658)) ;
#50764 = CARTESIAN_POINT('Ctrl Pts',(-20.1760444374323,-12.8097103983006,
124.366269150013)) ;
#50765 = CARTESIAN_POINT('Ctrl Pts',(-20.3677432425444,-12.6297213178202,
124.604878989456)) ;
#50766 = CARTESIAN_POINT('Ctrl Pts',(-20.4554911510886,-12.8296317362065,
124.047921898696)) ;
#50767 = CARTESIAN_POINT('Ctrl Pts',(-20.7170498597673,-12.649642655726,124.206944794391)) ;
#50768 = CARTESIAN_POINT('Ctrl Pts',(-20.6097246596929,-12.8495893594727,
123.652566976865)) ;
#50769 = CARTESIAN_POINT('Ctrl Pts',(-20.9098403567553,-12.6696002789922,
123.712751204381)) ;
#50770 = CARTESIAN_POINT('Ctrl Pts',(-20.6198419912611,-12.8694691914299,
123.23005419397)) ;
#50771 = CARTESIAN_POINT('Ctrl Pts',(-20.9224859852008,-12.6894801109494,
123.18461209714)) ;
#50772 = CARTESIAN_POINT('Ctrl Pts',(-20.4862162340303,-12.8893510427268,
122.828900869269)) ;
#50773 = CARTESIAN_POINT('Ctrl Pts',(-20.755454544681,-12.7093619622463,122.683172172741)) ;
#50774 = CARTESIAN_POINT('Ctrl Pts',(-20.2206736454974,-12.9094220598306,
122.494883082429)) ;
#50775 = CARTESIAN_POINT('Ctrl Pts',(-20.4235254245616,-12.7294329793501,
122.265649140896)) ;
#50776 = CARTESIAN_POINT('Ctrl Pts',(-19.8617901510047,-12.9292292835837,
122.274337723655)) ;
#50777 = CARTESIAN_POINT('Ctrl Pts',(-19.974923765594,-12.7492402031032,121.989968961296)) ;
#50778 = CARTESIAN_POINT('Ctrl Pts',(-19.4458827143192,-12.9492104191524,
122.187802603992)) ;
#50779 = CARTESIAN_POINT('Ctrl Pts',(-19.4550399386843,-12.769221338672,121.881799009353)) ;
#50780 = CARTESIAN_POINT('Ctrl Pts',(-19.0266575984833,-12.9691379124917,
122.249044591949)) ;
#50781 = CARTESIAN_POINT('Ctrl Pts',(-18.9310095255051,-12.7891488320112,
121.958350587115)) ;
#50782 = CARTESIAN_POINT('Ctrl Pts',(-18.6546793341104,-12.9889585738495,
122.447395484881)) ;
#50783 = CARTESIAN_POINT('Ctrl Pts',(-18.466037843445,-12.808969493369,122.206286369056)) ;
#50784 = CARTESIAN_POINT('Ctrl Pts',(-18.3694697209431,-13.0090557630713,
122.765395487489)) ;
#50785 = CARTESIAN_POINT('Ctrl Pts',(-18.109523705677,-12.8290666825908,122.6037861273)) ;
#50786 = CARTESIAN_POINT('Ctrl Pts',(-18.2121462510153,-13.0288194420796,
123.155285689063)) ;
#50787 = CARTESIAN_POINT('Ctrl Pts',(-17.912868524015,-12.8488303615991,123.091145395835)) ;
#50788 = CARTESIAN_POINT('Ctrl Pts',(-18.1966161351743,-13.0488767207527,
123.581287391373)) ;
#50789 = CARTESIAN_POINT('Ctrl Pts',(-17.8934532248138,-12.8688876402722,
123.623648070262)) ;
#50790 = CARTESIAN_POINT('Ctrl Pts',(-18.3260055582142,-13.0686721445001,
123.981930815811)) ;
#50791 = CARTESIAN_POINT('Ctrl Pts',(-18.0551868056977,-12.8886830640196,
124.124451004314)) ;
#50792 = CARTESIAN_POINT('Ctrl Pts',(-18.585401546907,-13.0886357892277,124.317872249246)) ;
#50793 = CARTESIAN_POINT('Ctrl Pts',(-18.3794288062783,-12.9086467087472,
124.544379679974)) ;
#50794 = CARTESIAN_POINT('Ctrl Pts',(-18.9448204747835,-13.1086192805018,
124.544510743668)) ;
#50795 = CARTESIAN_POINT('Ctrl Pts',(-18.8287006510793,-12.9286302000213,
124.82768037988)) ;
#50796 = CARTESIAN_POINT('Ctrl Pts',(-19.3561968961379,-13.1284267756511,
124.634949141891)) ;
#50797 = CARTESIAN_POINT('Ctrl Pts',(-19.3429186866214,-12.9484376951706,
124.94073162018)) ;
#50798 = CARTESIAN_POINT('Ctrl Pts',(-19.7773691623945,-13.1484093663712,
124.579587344744)) ;
#50799 = CARTESIAN_POINT('Ctrl Pts',(-19.8693844497786,-12.9684202858907,
124.871533418585)) ;
#50800 = CARTESIAN_POINT('Ctrl Pts',(-20.1526165065807,-13.1682920203624,
124.384654627234)) ;
#50801 = CARTESIAN_POINT('Ctrl Pts',(-20.3384447755885,-12.988302939882,124.627871581508)) ;
#50802 = CARTESIAN_POINT('Ctrl Pts',(-20.4400164199857,-13.1882502652255,
124.072540016501)) ;
#50803 = CARTESIAN_POINT('Ctrl Pts',(-20.6976976849805,-13.008261184745,124.237731507752)) ;
#50804 = CARTESIAN_POINT('Ctrl Pts',(-20.6032765964651,-13.2081258522671,
123.682670644288)) ;
#50805 = CARTESIAN_POINT('Ctrl Pts',(-20.9017768871207,-13.0281367717866,
123.750397269488)) ;
#50806 = CARTESIAN_POINT('Ctrl Pts',(-20.6240984710499,-13.2281067404023,
123.258361807286)) ;
#50807 = CARTESIAN_POINT('Ctrl Pts',(-20.9278087945966,-13.0481176599219,
123.220011471901)) ;
#50808 = CARTESIAN_POINT('Ctrl Pts',(-20.498818644834,-13.2480418815133,122.853364041742)) ;
#50809 = CARTESIAN_POINT('Ctrl Pts',(-20.7712144055599,-13.0680528010329,
122.713763278136)) ;
#50810 = CARTESIAN_POINT('Ctrl Pts',(-20.2434545299471,-13.2679538995244,
122.515712779495)) ;
#50811 = CARTESIAN_POINT('Ctrl Pts',(-20.4520106817377,-13.0879648190439,
122.291696114126)) ;
#50812 = CARTESIAN_POINT('Ctrl Pts',(-19.8888180187742,-13.287842117768,122.285335601894)) ;
#50813 = CARTESIAN_POINT('Ctrl Pts',(-20.00872858781,-13.1078530372875,122.003722192525)) ;
#50814 = CARTESIAN_POINT('Ctrl Pts',(-19.5451472567373,-13.3044404216149,
122.205327702706)) ;
#50815 = CARTESIAN_POINT('Ctrl Pts',(-19.5791090604786,-13.1244513411344,
121.903703056024)) ;
#50816 = CARTESIAN_POINT('Ctrl Pts',(-19.2662111497509,-13.3177130115177,
122.214345970221)) ;
#50817 = CARTESIAN_POINT('Ctrl Pts',(-19.2304680801221,-13.1377239310372,
121.914976366428)) ;
#50818 = CARTESIAN_POINT('Ctrl Pts',(-19.0602727562378,-13.3277204264686,
122.257344197933)) ;
#50819 = CARTESIAN_POINT('Ctrl Pts',(-18.9730360738755,-13.1477313459881,
121.968723010214)) ;
#50820 = CARTESIAN_POINT('Ctrl Pts',(-18.8649743558658,-13.3377277732012,
122.335630979356)) ;
#50821 = CARTESIAN_POINT('Ctrl Pts',(-18.7289237746943,-13.1577386927207,
122.066570256141)) ;
#50822 = CARTESIAN_POINT('Ctrl Pts',(-18.6279877995192,-13.3509941330028,
122.482594738179)) ;
#50823 = CARTESIAN_POINT('Ctrl Pts',(-18.4326373530418,-13.1710050525223,
122.25031691369)) ;
#50824 = CARTESIAN_POINT('Ctrl Pts',(-18.38714068302,-13.3675087906257,122.738147005354)) ;
#50825 = CARTESIAN_POINT('Ctrl Pts',(-18.1316373286166,-13.1875197101453,
122.569692622174)) ;
#50826 = CARTESIAN_POINT('Ctrl Pts',(-18.2465546320846,-13.3841062238684,
123.06176278507)) ;
#50827 = CARTESIAN_POINT('Ctrl Pts',(-17.9558681005146,-13.2041171433879,
122.974265631434)) ;
#50828 = CARTESIAN_POINT('Ctrl Pts',(-18.2054801703779,-13.3974542210134,
123.339422999475)) ;
#50829 = CARTESIAN_POINT('Ctrl Pts',(-17.9045373894855,-13.2174651405329,
123.321302564881)) ;
#50830 = CARTESIAN_POINT('Ctrl Pts',(-18.2109540995371,-13.407349975365,123.547385217031)) ;
#50831 = CARTESIAN_POINT('Ctrl Pts',(-17.9113737955999,-13.2273608948845,
123.581262925404)) ;
#50832 = CARTESIAN_POINT('Ctrl Pts',(-18.2525836667426,-13.4173379292963,
123.753181102987)) ;
#50833 = CARTESIAN_POINT('Ctrl Pts',(-17.9634088819123,-13.2373488488159,
123.838506352594)) ;
#50834 = CARTESIAN_POINT('Ctrl Pts',(-18.3290068072186,-13.4272951530011,
123.948090648861)) ;
#50835 = CARTESIAN_POINT('Ctrl Pts',(-18.058934973792,-13.2473060725206,124.082144873738)) ;
#50836 = CARTESIAN_POINT('Ctrl Pts',(-18.4390335780382,-13.4373306995577,
124.128090732076)) ;
#50837 = CARTESIAN_POINT('Ctrl Pts',(-18.1964661584521,-13.2573416190773,
124.307146372582)) ;
#50838 = CARTESIAN_POINT('Ctrl Pts',(-18.576478403772,-13.4472178108339,124.284038519252)) ;
#50839 = CARTESIAN_POINT('Ctrl Pts',(-18.3682700532266,-13.2672287303534,
124.502082982848)) ;
#50840 = CARTESIAN_POINT('Ctrl Pts',(-18.7403986017361,-13.4572092159347,
124.415367414347)) ;
#50841 = CARTESIAN_POINT('Ctrl Pts',(-18.5731685999717,-13.2772201354542,
124.666246335996)) ;
#50842 = CARTESIAN_POINT('Ctrl Pts',(-18.9238269690954,-13.4671548371495,
124.515725679001)) ;
#50843 = CARTESIAN_POINT('Ctrl Pts',(-18.8024527486131,-13.287165756669,124.791696662309)) ;
#50844 = CARTESIAN_POINT('Ctrl Pts',(-19.1218420695638,-13.4771040854178,
124.583140773883)) ;
#50845 = CARTESIAN_POINT('Ctrl Pts',(-19.0499707908993,-13.2971150049373,
124.875968223362)) ;
#50846 = CARTESIAN_POINT('Ctrl Pts',(-19.3305917291493,-13.4871505805864,
124.615215322897)) ;
#50847 = CARTESIAN_POINT('Ctrl Pts',(-19.3109074952256,-13.3071615001059,
124.916064204666)) ;
#50848 = CARTESIAN_POINT('Ctrl Pts',(-19.5376622730773,-13.4970019233779,
124.610852955936)) ;
#50849 = CARTESIAN_POINT('Ctrl Pts',(-19.5697458477462,-13.3170128428975,
124.910614060324)) ;
#50850 = CARTESIAN_POINT('Ctrl Pts',(-19.7433819757979,-13.5069737035053,
124.570637442649)) ;
#50851 = CARTESIAN_POINT('Ctrl Pts',(-19.826896127891,-13.3269846230248,124.860347401869)) ;
#50852 = CARTESIAN_POINT('Ctrl Pts',(-19.9394995576033,-13.516968903483,124.495094530682)) ;
#50853 = CARTESIAN_POINT('Ctrl Pts',(-20.0720441859589,-13.3369798230025,
124.765921346822)) ;
#50854 = CARTESIAN_POINT('Ctrl Pts',(-20.1200428835865,-13.527002895179,124.386031569206)) ;
#50855 = CARTESIAN_POINT('Ctrl Pts',(-20.2977248333267,-13.3470138146985,
124.629595035507)) ;
#50856 = CARTESIAN_POINT('Ctrl Pts',(-20.2763242405218,-13.5368583001515,
124.249969630593)) ;
#50857 = CARTESIAN_POINT('Ctrl Pts',(-20.493078540568,-13.356869219671,124.459519571261)) ;
#50858 = CARTESIAN_POINT('Ctrl Pts',(-20.4086965221813,-13.5468575979973,
124.086710547082)) ;
#50859 = CARTESIAN_POINT('Ctrl Pts',(-20.6585461153618,-13.3668685175168,
124.255447402453)) ;
#50860 = CARTESIAN_POINT('Ctrl Pts',(-20.5098783796781,-13.5567527106025,
123.904908826794)) ;
#50861 = CARTESIAN_POINT('Ctrl Pts',(-20.7850259765466,-13.376763630122,124.028196369772)) ;
#50862 = CARTESIAN_POINT('Ctrl Pts',(-20.5790528982995,-13.5668133561375,
123.705062953625)) ;
#50863 = CARTESIAN_POINT('Ctrl Pts',(-20.8714967334466,-13.386824275657,123.778389961167)) ;
#50864 = CARTESIAN_POINT('Ctrl Pts',(-20.6118978850877,-13.5766622331267,
123.500614031643)) ;
#50865 = CARTESIAN_POINT('Ctrl Pts',(-20.9125557496579,-13.3966731526462,
123.522828864956)) ;
#50866 = CARTESIAN_POINT('Ctrl Pts',(-20.6092193159514,-13.5866909442203,
123.289798847138)) ;
#50867 = CARTESIAN_POINT('Ctrl Pts',(-20.9092102413502,-13.4067018637398,
123.259309807944)) ;
#50868 = CARTESIAN_POINT('Ctrl Pts',(-20.5694097322058,-13.5967203454764,
123.082737299415)) ;
#50869 = CARTESIAN_POINT('Ctrl Pts',(-20.8594509752274,-13.4167312649959,
123.000482346226)) ;
#50870 = CARTESIAN_POINT('Ctrl Pts',(-20.4961008853216,-13.6065605372724,
122.889286624956)) ;
#50871 = CARTESIAN_POINT('Ctrl Pts',(-20.7678172837384,-13.4265714567919,
122.758667592089)) ;
#50872 = CARTESIAN_POINT('Ctrl Pts',(-20.3889086577013,-13.6165639664654,
122.708376154055)) ;
#50873 = CARTESIAN_POINT('Ctrl Pts',(-20.6338292438647,-13.4365748859849,
122.532528062918)) ;
#50874 = CARTESIAN_POINT('Ctrl Pts',(-20.2520895253684,-13.6265494789316,
122.549112630056)) ;
#50875 = CARTESIAN_POINT('Ctrl Pts',(-20.4628072719018,-13.4465603984511,
122.333446821007)) ;
#50876 = CARTESIAN_POINT('Ctrl Pts',(-20.0887000777735,-13.6365905753156,
122.415484766701)) ;
#50877 = CARTESIAN_POINT('Ctrl Pts',(-20.258572195346,-13.4566014948351,122.166409914417)) ;
#50878 = CARTESIAN_POINT('Ctrl Pts',(-19.9083265613386,-13.6464337712666,
122.314020661915)) ;
#50879 = CARTESIAN_POINT('Ctrl Pts',(-20.0331061121941,-13.4664446907861,
122.03957718777)) ;
#50880 = CARTESIAN_POINT('Ctrl Pts',(-19.7104267761794,-13.656420082321,122.244041727144)) ;
#50881 = CARTESIAN_POINT('Ctrl Pts',(-19.7857320971964,-13.4764310018405,
121.952101012254)) ;
#50882 = CARTESIAN_POINT('Ctrl Pts',(-19.5044018483537,-13.6663547675787,
122.209514866081)) ;
#50883 = CARTESIAN_POINT('Ctrl Pts',(-19.5282010412024,-13.4863656870982,
121.90893984682)) ;
#50884 = CARTESIAN_POINT('Ctrl Pts',(-19.2929999960134,-13.6764123287957,
122.211492627575)) ;
#50885 = CARTESIAN_POINT('Ctrl Pts',(-19.2639488168424,-13.4964232483152,
121.91140943863)) ;
#50886 = CARTESIAN_POINT('Ctrl Pts',(-19.0899192604328,-13.6862339704043,
122.248938878938)) ;
#50887 = CARTESIAN_POINT('Ctrl Pts',(-19.0100966675006,-13.5062448899238,
121.958214887959)) ;
#50888 = CARTESIAN_POINT('Ctrl Pts',(-18.8917066678072,-13.6962900339953,
122.32241535315)) ;
#50889 = CARTESIAN_POINT('Ctrl Pts',(-18.7623301681439,-13.5163009535148,
122.050058119778)) ;
#50890 = CARTESIAN_POINT('Ctrl Pts',(-18.711524790799,-13.7062307097571,122.428304767284)) ;
#50891 = CARTESIAN_POINT('Ctrl Pts',(-18.5371012424823,-13.5262416292766,
122.182417857127)) ;
#50892 = CARTESIAN_POINT('Ctrl Pts',(-18.5526279674509,-13.7161350685454,
122.562874462865)) ;
#50893 = CARTESIAN_POINT('Ctrl Pts',(-18.338478245471,-13.5361459880649,122.350628473773)) ;
#50894 = CARTESIAN_POINT('Ctrl Pts',(-18.4177132106572,-13.7261817231212,
122.725360080974)) ;
#50895 = CARTESIAN_POINT('Ctrl Pts',(-18.1698329824766,-13.5461926426408,
122.553733855453)) ;
#50896 = CARTESIAN_POINT('Ctrl Pts',(-18.3144502475993,-13.7360773177641,
122.905994660676)) ;
#50897 = CARTESIAN_POINT('Ctrl Pts',(-18.0407519034869,-13.5560882372836,
122.779526388093)) ;
#50898 = CARTESIAN_POINT('Ctrl Pts',(-18.2429366007976,-13.7461392644209,
123.105048153552)) ;
#50899 = CARTESIAN_POINT('Ctrl Pts',(-17.9513576419596,-13.5661501839405,
123.028342279805)) ;
#50900 = CARTESIAN_POINT('Ctrl Pts',(-18.2077846553653,-13.7559888883531,
123.309123594396)) ;
#50901 = CARTESIAN_POINT('Ctrl Pts',(-17.9074152111613,-13.5759998078726,
123.283436990154)) ;
#50902 = CARTESIAN_POINT('Ctrl Pts',(-18.2079178316408,-13.7659521273829,
123.518569880535)) ;
#50903 = CARTESIAN_POINT('Ctrl Pts',(-17.9075794488089,-13.5859630469025,
123.545245160135)) ;
#50904 = CARTESIAN_POINT('Ctrl Pts',(-18.2449311630796,-13.7759767021588,
123.726054826624)) ;
#50905 = CARTESIAN_POINT('Ctrl Pts',(-17.9538438450152,-13.5959876216783,
123.804601716905)) ;
#50906 = CARTESIAN_POINT('Ctrl Pts',(-18.3165097926261,-13.7858952648465,
123.921897886242)) ;
#50907 = CARTESIAN_POINT('Ctrl Pts',(-18.0433151852417,-13.605906184366,124.049406829383)) ;
#50908 = CARTESIAN_POINT('Ctrl Pts',(-18.4214705157971,-13.7958874515705,
124.103877790771)) ;
#50909 = CARTESIAN_POINT('Ctrl Pts',(-18.1745142881597,-13.61589837109,124.276882942917)) ;
#50910 = CARTESIAN_POINT('Ctrl Pts',(-18.5572880042135,-13.8059222501547,
124.265295046581)) ;
#50911 = CARTESIAN_POINT('Ctrl Pts',(-18.3442843562415,-13.6259331696742,
124.478655912856)) ;
#50912 = CARTESIAN_POINT('Ctrl Pts',(-18.7159640539968,-13.8157774408283,
124.398542881549)) ;
#50913 = CARTESIAN_POINT('Ctrl Pts',(-18.5426287177336,-13.6357883603479,
124.645217964171)) ;
#50914 = CARTESIAN_POINT('Ctrl Pts',(-18.8978051688274,-13.8257767889813,
124.503949795873)) ;
#50915 = CARTESIAN_POINT('Ctrl Pts',(-18.7699291705139,-13.6457877085009,
124.776978498032)) ;
#50916 = CARTESIAN_POINT('Ctrl Pts',(-19.0931163675303,-13.8356719146565,
124.575663890585)) ;
#50917 = CARTESIAN_POINT('Ctrl Pts',(-19.0140681533063,-13.655682834176,124.86662328365)) ;
#50918 = CARTESIAN_POINT('Ctrl Pts',(-19.3012793398308,-13.8457324576046,
124.612957137398)) ;
#50919 = CARTESIAN_POINT('Ctrl Pts',(-19.2742712713046,-13.6657433771241,
124.913241818178)) ;
#50920 = CARTESIAN_POINT('Ctrl Pts',(-19.5083568286429,-13.8555817318715,
124.613644904383)) ;
#50921 = CARTESIAN_POINT('Ctrl Pts',(-19.533119164813,-13.675592651391,124.914103545098)) ;
#50922 = CARTESIAN_POINT('Ctrl Pts',(-19.7161637957389,-13.8656089564414,
124.578258675114)) ;
#50923 = CARTESIAN_POINT('Ctrl Pts',(-19.7928781485442,-13.6856198759609,
124.869872597829)) ;
#50924 = CARTESIAN_POINT('Ctrl Pts',(-19.9145234172926,-13.8756373556292,
124.506794850628)) ;
#50925 = CARTESIAN_POINT('Ctrl Pts',(-20.0408282969519,-13.6956482751487,
124.780544744332)) ;
#50926 = CARTESIAN_POINT('Ctrl Pts',(-20.0942981409798,-13.8854831060427,
124.404230045374)) ;
#50927 = CARTESIAN_POINT('Ctrl Pts',(-20.2655486147779,-13.7054940255622,
124.652339842869)) ;
#50928 = CARTESIAN_POINT('Ctrl Pts',(-20.2562410694359,-13.8954718964434,
124.27052516634)) ;
#50929 = CARTESIAN_POINT('Ctrl Pts',(-20.4679785319862,-13.715482815963,124.485209945461)) ;
#50930 = CARTESIAN_POINT('Ctrl Pts',(-20.3928548044161,-13.9055168248431,
124.109502618488)) ;
#50931 = CARTESIAN_POINT('Ctrl Pts',(-20.6387470356566,-13.7255277443626,
124.283933112368)) ;
#50932 = CARTESIAN_POINT('Ctrl Pts',(-20.4975212772136,-13.9153413096321,
123.931431530893)) ;
#50933 = CARTESIAN_POINT('Ctrl Pts',(-20.7695822852688,-13.7353522291516,
124.061344007663)) ;
#50934 = CARTESIAN_POINT('Ctrl Pts',(-20.5716663162285,-13.9253987071733,
123.733438159543)) ;
#50935 = CARTESIAN_POINT('Ctrl Pts',(-20.8622650303472,-13.7454096266928,
123.813853115612)) ;
#50936 = CARTESIAN_POINT('Ctrl Pts',(-20.6095387245746,-13.9353247987595,
123.528210702811)) ;
#50937 = CARTESIAN_POINT('Ctrl Pts',(-20.9096073546648,-13.755335718279,123.557318498523)) ;
#50938 = CARTESIAN_POINT('Ctrl Pts',(-20.6117482503137,-13.945279583904,123.318943735867)) ;
#50939 = CARTESIAN_POINT('Ctrl Pts',(-20.9123708212694,-13.7652905034236,
123.295734355708)) ;
#50940 = CARTESIAN_POINT('Ctrl Pts',(-20.5770731565774,-13.9553169535617,
123.110795951615)) ;
#50941 = CARTESIAN_POINT('Ctrl Pts',(-20.8690285858304,-13.7753278730812,
123.035549479052)) ;
#50942 = CARTESIAN_POINT('Ctrl Pts',(-20.5079730266207,-13.9652057636833,
122.914716225052)) ;
#50943 = CARTESIAN_POINT('Ctrl Pts',(-20.7826546063666,-13.7852166832028,
122.790448432854)) ;
#50944 = CARTESIAN_POINT('Ctrl Pts',(-20.4051720006662,-13.9751951227343,
122.731595284921)) ;
#50945 = CARTESIAN_POINT('Ctrl Pts',(-20.6541544834532,-13.7952060422539,
122.561546360004)) ;
#50946 = CARTESIAN_POINT('Ctrl Pts',(-20.2724273246368,-13.9851536701904,
122.569707167163)) ;
#50947 = CARTESIAN_POINT('Ctrl Pts',(-20.4882245282922,-13.80516458971,122.35918492389)) ;
#50948 = CARTESIAN_POINT('Ctrl Pts',(-20.1148509111908,-13.9950532467415,
122.433733040983)) ;
#50949 = CARTESIAN_POINT('Ctrl Pts',(-20.2912542117038,-13.815064166261,122.189215690004)) ;
#50950 = CARTESIAN_POINT('Ctrl Pts',(-19.9333707547642,-14.0051011585722,
122.32566998488)) ;
#50951 = CARTESIAN_POINT('Ctrl Pts',(-20.0644048945837,-13.8251120780917,
122.054135819747)) ;
#50952 = CARTESIAN_POINT('Ctrl Pts',(-19.738890370448,-14.0149965064327,122.251724804565)) ;
#50953 = CARTESIAN_POINT('Ctrl Pts',(-19.8213040212828,-13.8350074259523,
121.961702812235)) ;
#50954 = CARTESIAN_POINT('Ctrl Pts',(-19.5311506381738,-14.0250581829639,
122.211995828632)) ;
#50955 = CARTESIAN_POINT('Ctrl Pts',(-19.5616299166127,-13.8450691024834,
121.912040392263)) ;
#50956 = CARTESIAN_POINT('Ctrl Pts',(-19.3242027583877,-14.0349027007131,
122.208972747124)) ;
#50957 = CARTESIAN_POINT('Ctrl Pts',(-19.3029437659801,-13.8549136202326,
121.908260248604)) ;
#50958 = CARTESIAN_POINT('Ctrl Pts',(-19.1173623183453,-14.0448631444279,
122.241578718461)) ;
#50959 = CARTESIAN_POINT('Ctrl Pts',(-19.0443926106295,-13.8648740639474,
121.949016797417)) ;
#50960 = CARTESIAN_POINT('Ctrl Pts',(-18.917933653831,-14.0548999772461,122.310497086348)) ;
#50961 = CARTESIAN_POINT('Ctrl Pts',(-18.7951065532493,-13.8749108967656,
122.035163624094)) ;
#50962 = CARTESIAN_POINT('Ctrl Pts',(-18.7362181804366,-14.0647787739929,
122.41109597588)) ;
#50963 = CARTESIAN_POINT('Ctrl Pts',(-18.5679607591708,-13.8847896935124,
122.160911880305)) ;
#50964 = CARTESIAN_POINT('Ctrl Pts',(-18.5717693082948,-14.0748380901212,
122.544026993693)) ;
#50965 = CARTESIAN_POINT('Ctrl Pts',(-18.3623992979497,-13.8948490096408,
122.327074678563)) ;
#50966 = CARTESIAN_POINT('Ctrl Pts',(-18.4354824503582,-14.0847085368744,
122.700520863806)) ;
#50967 = CARTESIAN_POINT('Ctrl Pts',(-18.1920392189904,-13.904719456394,122.522692233356)) ;
#50968 = CARTESIAN_POINT('Ctrl Pts',(-18.3266320599271,-14.0947011751325,
122.880198948747)) ;
#50969 = CARTESIAN_POINT('Ctrl Pts',(-18.0559754685677,-13.914712094652,122.747289602209)) ;
#50970 = CARTESIAN_POINT('Ctrl Pts',(-18.2507605415013,-14.1047331906804,
123.076976227112)) ;
#50971 = CARTESIAN_POINT('Ctrl Pts',(-17.9611352241743,-13.9247441101999,
122.993260746161)) ;
#50972 = CARTESIAN_POINT('Ctrl Pts',(-18.2104322023642,-14.114599046987,123.280449832988)) ;
#50973 = CARTESIAN_POINT('Ctrl Pts',(-17.9107237976247,-13.9346099665065,
123.247603809007)) ;
#50974 = CARTESIAN_POINT('Ctrl Pts',(-18.2059368718994,-14.1246683364561,
123.492066961254)) ;
#50975 = CARTESIAN_POINT('Ctrl Pts',(-17.9051038743598,-13.9446792559756,
123.512124786781)) ;
#50976 = CARTESIAN_POINT('Ctrl Pts',(-18.2375102294898,-14.1345118940074,
123.696598560914)) ;
#50977 = CARTESIAN_POINT('Ctrl Pts',(-17.9445700336421,-13.9545228135269,
123.767790797039)) ;
#50978 = CARTESIAN_POINT('Ctrl Pts',(-18.3043848267997,-14.1444920207952,
123.895462028567)) ;
#50979 = CARTESIAN_POINT('Ctrl Pts',(-18.0281629108298,-13.9645029403147,
124.016370584177)) ;
#50980 = CARTESIAN_POINT('Ctrl Pts',(-18.4055151657071,-14.1545105693952,
124.080209802711)) ;
#50981 = CARTESIAN_POINT('Ctrl Pts',(-18.1545752561932,-13.9745214889147,
124.247305606121)) ;
#50982 = CARTESIAN_POINT('Ctrl Pts',(-18.5350837698109,-14.1643938699184,
124.242672415459)) ;
#50983 = CARTESIAN_POINT('Ctrl Pts',(-18.3165363212011,-13.9844047894379,
124.450385028089)) ;
#50984 = CARTESIAN_POINT('Ctrl Pts',(-18.6938257864244,-14.1744621569665,
124.382634186157)) ;
#50985 = CARTESIAN_POINT('Ctrl Pts',(-18.5149631926093,-13.994473076486,124.625337357564)) ;
#50986 = CARTESIAN_POINT('Ctrl Pts',(-18.8701172743958,-14.1842922799851,
124.490542166158)) ;
#50987 = CARTESIAN_POINT('Ctrl Pts',(-18.735328647287,-14.0043031995047,124.760223493844)) ;
#50988 = CARTESIAN_POINT('Ctrl Pts',(-19.0669291678649,-14.1943588639105,
124.568249490539)) ;
#50989 = CARTESIAN_POINT('Ctrl Pts',(-18.9813430292244,-14.01436978343,124.857357794822)) ;
#50990 = CARTESIAN_POINT('Ctrl Pts',(-19.2706943838824,-14.2042489769249,
124.609750952324)) ;
#50991 = CARTESIAN_POINT('Ctrl Pts',(-19.236050504993,-14.0242598964445,124.909235187497)) ;
#50992 = CARTESIAN_POINT('Ctrl Pts',(-19.4806689201278,-14.2142416656876,
124.615742309981)) ;
#50993 = CARTESIAN_POINT('Ctrl Pts',(-19.4985188781258,-14.0342525852071,
124.916724579679)) ;
#50994 = CARTESIAN_POINT('Ctrl Pts',(-19.6878386126546,-14.2242025540433,
124.585132160337)) ;
#50995 = CARTESIAN_POINT('Ctrl Pts',(-19.7574815058879,-14.0442134735629,
124.878462065285)) ;
#50996 = CARTESIAN_POINT('Ctrl Pts',(-19.8857808498602,-14.2341204989233,
124.519648220953)) ;
#50997 = CARTESIAN_POINT('Ctrl Pts',(-20.0049101278269,-14.0541314184429,
124.796606975694)) ;
#50998 = CARTESIAN_POINT('Ctrl Pts',(-20.0711543280967,-14.2441282520195,
124.42009338198)) ;
#50999 = CARTESIAN_POINT('Ctrl Pts',(-20.2366270329595,-14.0641391715391,
124.672163407257)) ;
#51000 = CARTESIAN_POINT('Ctrl Pts',(-20.2365214427845,-14.2541593459786,
124.289244206464)) ;
#51001 = CARTESIAN_POINT('Ctrl Pts',(-20.4433359396728,-14.0741702654981,
124.50860215391)) ;
#51002 = CARTESIAN_POINT('Ctrl Pts',(-20.3744629268658,-14.2640073140066,
124.134836918703)) ;
#51003 = CARTESIAN_POINT('Ctrl Pts',(-20.615763730972,-14.0840182335261,124.315591986996)) ;
#51004 = CARTESIAN_POINT('Ctrl Pts',(-20.4860083257482,-14.2740692701324,
123.95512196643)) ;
#51005 = CARTESIAN_POINT('Ctrl Pts',(-20.7551952258906,-14.094080189652,124.090948557051)) ;
#51006 = CARTESIAN_POINT('Ctrl Pts',(-20.5631955250995,-14.2839664817336,
123.761889219392)) ;
#51007 = CARTESIAN_POINT('Ctrl Pts',(-20.8516795938104,-14.1039774012531,
123.849406694929)) ;
#51008 = CARTESIAN_POINT('Ctrl Pts',(-20.6064757403202,-14.2938976483982,
123.557644080804)) ;
#51009 = CARTESIAN_POINT('Ctrl Pts',(-20.9057797424506,-14.1139085679177,
123.594099508441)) ;
#51010 = CARTESIAN_POINT('Ctrl Pts',(-20.6134856977865,-14.3039398326024,
123.346645043293)) ;
#51011 = CARTESIAN_POINT('Ctrl Pts',(-20.9145419980729,-14.1239507521219,
123.330350913857)) ;
#51012 = CARTESIAN_POINT('Ctrl Pts',(-20.5843602960543,-14.3138265008555,
123.140837465138)) ;
#51013 = CARTESIAN_POINT('Ctrl Pts',(-20.8781348523199,-14.1338374203751,
123.073090399062)) ;
#51014 = CARTESIAN_POINT('Ctrl Pts',(-20.5195898101172,-14.3238196128338,
122.940995926319)) ;
#51015 = CARTESIAN_POINT('Ctrl Pts',(-20.7971713177884,-14.1438305323533,
122.823288399559)) ;
#51016 = CARTESIAN_POINT('Ctrl Pts',(-20.4214970858592,-14.3337652904496,
122.756344163075)) ;
#51017 = CARTESIAN_POINT('Ctrl Pts',(-20.6745548237651,-14.1537762099691,
122.592473334144)) ;
#51018 = CARTESIAN_POINT('Ctrl Pts',(-20.2931422169085,-14.3437125934346,
122.591232662632)) ;
#51019 = CARTESIAN_POINT('Ctrl Pts',(-20.5141104751308,-14.1637235129541,
122.386083823413)) ;
#51020 = CARTESIAN_POINT('Ctrl Pts',(-20.1363573288779,-14.3537603171813,
122.449682535313)) ;
#51021 = CARTESIAN_POINT('Ctrl Pts',(-20.3181292652433,-14.1737712367009,
122.20914664792)) ;
#51022 = CARTESIAN_POINT('Ctrl Pts',(-19.9610119228354,-14.3636086909439,
122.339593196702)) ;
#51023 = CARTESIAN_POINT('Ctrl Pts',(-20.0989460634751,-14.1836196104634,
122.071534647339)) ;
#51024 = CARTESIAN_POINT('Ctrl Pts',(-19.7673215762674,-14.3735676633896,
122.260098624231)) ;
#51025 = CARTESIAN_POINT('Ctrl Pts',(-19.8568324062144,-14.1935785829091,
121.972166958739)) ;
#51026 = CARTESIAN_POINT('Ctrl Pts',(-19.5610549600458,-14.3836065252707,
122.215459746428)) ;
#51027 = CARTESIAN_POINT('Ctrl Pts',(-19.5989991593869,-14.2036174447902,
121.916368996424)) ;
#51028 = CARTESIAN_POINT('Ctrl Pts',(-19.3535221005735,-14.3934851294425,
122.207111470236)) ;
#51029 = CARTESIAN_POINT('Ctrl Pts',(-19.3395819370179,-14.2134960489621,
121.905934350524)) ;
#51030 = CARTESIAN_POINT('Ctrl Pts',(-19.1441263617507,-14.4035366706458,
122.235315239726)) ;
#51031 = CARTESIAN_POINT('Ctrl Pts',(-19.0778376414323,-14.2235475901654,
121.941189793679)) ;
#51032 = CARTESIAN_POINT('Ctrl Pts',(-18.9458547057129,-14.4134320686262,
122.298408849419)) ;
#51033 = CARTESIAN_POINT('Ctrl Pts',(-18.8299973983688,-14.2334429881457,
122.02005786211)) ;
#51034 = CARTESIAN_POINT('Ctrl Pts',(-18.7586516298394,-14.4234833011715,
122.396359934609)) ;
#51035 = CARTESIAN_POINT('Ctrl Pts',(-18.5959941771249,-14.243494220691,122.142497342869)) ;
#51036 = CARTESIAN_POINT('Ctrl Pts',(-18.5939939088903,-14.4333694917958,
122.523221653132)) ;
#51037 = CARTESIAN_POINT('Ctrl Pts',(-18.3901717061082,-14.2533804113153,
122.301075810648)) ;
#51038 = CARTESIAN_POINT('Ctrl Pts',(-18.4520997591911,-14.4433620311115,
122.678107054398)) ;
#51039 = CARTESIAN_POINT('Ctrl Pts',(-18.2128046215638,-14.2633729506311,
122.494683384561)) ;
#51040 = CARTESIAN_POINT('Ctrl Pts',(-18.3397922812975,-14.4533104770063,
122.854559106031)) ;
#51041 = CARTESIAN_POINT('Ctrl Pts',(-18.0724208012427,-14.2733213965258,
122.715249428695)) ;
#51042 = CARTESIAN_POINT('Ctrl Pts',(-18.2596593833855,-14.4632472795382,
123.047461897236)) ;
#51043 = CARTESIAN_POINT('Ctrl Pts',(-17.9722554345249,-14.2832581990577,
122.956378922606)) ;
#51044 = CARTESIAN_POINT('Ctrl Pts',(-18.2137581958001,-14.4732302869895,
123.252282638572)) ;
#51045 = CARTESIAN_POINT('Ctrl Pts',(-17.9148800448479,-14.293241206509,123.212405357777)) ;
#51046 = CARTESIAN_POINT('Ctrl Pts',(-18.2044493527583,-14.4832741284043,
123.463206431544)) ;
#51047 = CARTESIAN_POINT('Ctrl Pts',(-17.9032450352358,-14.3032850479238,
123.476059954935)) ;
#51048 = CARTESIAN_POINT('Ctrl Pts',(-18.2308383801991,-14.4931023270282,
123.668165335843)) ;
#51049 = CARTESIAN_POINT('Ctrl Pts',(-17.9362327114259,-14.3131132465477,
123.73225986307)) ;
#51050 = CARTESIAN_POINT('Ctrl Pts',(-18.2938523410951,-14.5031789204704,
123.870372485691)) ;
#51051 = CARTESIAN_POINT('Ctrl Pts',(-18.0150012317243,-14.3231898399899,
123.985018013504)) ;
#51052 = CARTESIAN_POINT('Ctrl Pts',(-18.3887993193818,-14.513030919812,124.0544990199)) ;
#51053 = CARTESIAN_POINT('Ctrl Pts',(-18.1336866674195,-14.3330418393315,
124.215176688704)) ;
#51054 = CARTESIAN_POINT('Ctrl Pts',(-18.516907971024,-14.5231045066358,124.223090197898)) ;
#51055 = CARTESIAN_POINT('Ctrl Pts',(-18.2938233160263,-14.3431154261554,
124.425914521078)) ;
#51056 = CARTESIAN_POINT('Ctrl Pts',(-18.6688091775145,-14.5329447317333,
124.363553032254)) ;
#51057 = CARTESIAN_POINT('Ctrl Pts',(-18.4837016927803,-14.3529556512529,
124.601492972364)) ;
#51058 = CARTESIAN_POINT('Ctrl Pts',(-18.8445804362272,-14.542910435762,124.477535027406)) ;
#51059 = CARTESIAN_POINT('Ctrl Pts',(-18.7034169617488,-14.3629213552815,
124.743969337186)) ;
#51060 = CARTESIAN_POINT('Ctrl Pts',(-19.0387987115393,-14.5529370690686,
124.559495745125)) ;
#51061 = CARTESIAN_POINT('Ctrl Pts',(-18.9461903268235,-14.3729479885881,
124.846418837784)) ;
#51062 = CARTESIAN_POINT('Ctrl Pts',(-19.2419467311579,-14.5628513647804,
124.606096057943)) ;
#51063 = CARTESIAN_POINT('Ctrl Pts',(-19.2001264119576,-14.3828622842999,
124.904667897302)) ;
#51064 = CARTESIAN_POINT('Ctrl Pts',(-19.4516521953088,-14.5728396534728,
124.61717510903)) ;
#51065 = CARTESIAN_POINT('Ctrl Pts',(-19.4622585244037,-14.3928505729924,
124.918515058981)) ;
#51066 = CARTESIAN_POINT('Ctrl Pts',(-19.6610834565671,-14.5828783866312,
124.591166378612)) ;
#51067 = CARTESIAN_POINT('Ctrl Pts',(-19.7240472766413,-14.4028893061507,
124.886002641623)) ;
#51068 = CARTESIAN_POINT('Ctrl Pts',(-19.858998903738,-14.5927217184587,124.530728055798)) ;
#51069 = CARTESIAN_POINT('Ctrl Pts',(-19.9714422785436,-14.4127326379783,
124.810452800166)) ;
#51070 = CARTESIAN_POINT('Ctrl Pts',(-20.0470907094626,-14.6027494443383,
124.43551748704)) ;
#51071 = CARTESIAN_POINT('Ctrl Pts',(-20.2065561511846,-14.4227603638579,
124.691438006676)) ;
#51072 = CARTESIAN_POINT('Ctrl Pts',(-20.215531250739,-14.6127817807269,124.308574127084)) ;
#51073 = CARTESIAN_POINT('Ctrl Pts',(-20.4171057820378,-14.4327927002464,
124.532757562509)) ;
#51074 = CARTESIAN_POINT('Ctrl Pts',(-20.3567549827595,-14.6226112810275,
124.157731091938)) ;
#51075 = CARTESIAN_POINT('Ctrl Pts',(-20.5936350312441,-14.442622200547,124.344201635672)) ;
#51076 = CARTESIAN_POINT('Ctrl Pts',(-20.4720182760222,-14.6326007849443,
123.982171250015)) ;
#51077 = CARTESIAN_POINT('Ctrl Pts',(-20.737712608456,-14.4526117044638,124.124750610664)) ;
#51078 = CARTESIAN_POINT('Ctrl Pts',(-20.5550029183584,-14.6426446254567,
123.788010434387)) ;
#51079 = CARTESIAN_POINT('Ctrl Pts',(-20.8414417060553,-14.4626555449762,
123.882049023621)) ;
#51080 = CARTESIAN_POINT('Ctrl Pts',(-20.6023692510491,-14.6524663312247,
123.587034176731)) ;
#51081 = CARTESIAN_POINT('Ctrl Pts',(-20.9006480361569,-14.4724772507443,
123.630827043139)) ;
#51082 = CARTESIAN_POINT('Ctrl Pts',(-20.614891393778,-14.6625013783571,123.376438673923)) ;
#51083 = CARTESIAN_POINT('Ctrl Pts',(-20.9162986356404,-14.4825122978766,
123.367582647653)) ;
#51084 = CARTESIAN_POINT('Ctrl Pts',(-20.5901024671484,-14.672526055794,123.167143676446)) ;
#51085 = CARTESIAN_POINT('Ctrl Pts',(-20.8853105897408,-14.4925369753135,
123.105964149127)) ;
#51086 = CARTESIAN_POINT('Ctrl Pts',(-20.5308125782497,-14.6823788706484,
122.968674050456)) ;
#51087 = CARTESIAN_POINT('Ctrl Pts',(-20.8111959913455,-14.502389790168,122.857876731608)) ;
#51088 = CARTESIAN_POINT('Ctrl Pts',(-20.4370276643577,-14.692366580256,122.780826892626)) ;
#51089 = CARTESIAN_POINT('Ctrl Pts',(-20.6939628550224,-14.5123774997755,
122.623068574683)) ;
#51090 = CARTESIAN_POINT('Ctrl Pts',(-20.3127672555841,-14.7022965902501,
122.613067626526)) ;
#51091 = CARTESIAN_POINT('Ctrl Pts',(-20.5386353140637,-14.5223075097696,
122.413370344733)) ;
#51092 = CARTESIAN_POINT('Ctrl Pts',(-20.1605796757999,-14.7122863454692,
122.468335495329)) ;
#51093 = CARTESIAN_POINT('Ctrl Pts',(-20.3483991861106,-14.5322972649888,
122.232456679477)) ;
#51094 = CARTESIAN_POINT('Ctrl Pts',(-19.9847778139171,-14.7223129541521,
122.352025348161)) ;
#51095 = CARTESIAN_POINT('Ctrl Pts',(-20.1286457022629,-14.5423238736717,
122.08707080773)) ;
#51096 = CARTESIAN_POINT('Ctrl Pts',(-19.7942886748206,-14.732196894174,122.269022419418)) ;
#51097 = CARTESIAN_POINT('Ctrl Pts',(-19.8905327192874,-14.5522078136935,
121.983318872729)) ;
#51098 = CARTESIAN_POINT('Ctrl Pts',(-19.5902331312652,-14.7421861217125,
122.219359207184)) ;
#51099 = CARTESIAN_POINT('Ctrl Pts',(-19.6354625878385,-14.562197041232,121.92124208015)) ;
#51100 = CARTESIAN_POINT('Ctrl Pts',(-19.3795093368715,-14.7522289922362,
122.206246194729)) ;
#51101 = CARTESIAN_POINT('Ctrl Pts',(-19.3720577988247,-14.5722399117557,
121.904853032833)) ;
#51102 = CARTESIAN_POINT('Ctrl Pts',(-19.1740714005142,-14.7620613789916,
122.229097308269)) ;
#51103 = CARTESIAN_POINT('Ctrl Pts',(-19.1152596799946,-14.5820722985111,
121.933419317654)) ;
#51104 = CARTESIAN_POINT('Ctrl Pts',(-18.9723061416938,-14.7720546721632,
122.287639558838)) ;
#51105 = CARTESIAN_POINT('Ctrl Pts',(-18.8630536664399,-14.5920655916827,
122.006599511698)) ;
#51106 = CARTESIAN_POINT('Ctrl Pts',(-18.7832226625352,-14.7820866778116,
122.381086795298)) ;
#51107 = CARTESIAN_POINT('Ctrl Pts',(-18.6267003874203,-14.6020975973311,
122.123410637807)) ;
#51108 = CARTESIAN_POINT('Ctrl Pts',(-18.6159274829548,-14.7919519337806,
122.503651125695)) ;
#51109 = CARTESIAN_POINT('Ctrl Pts',(-18.4175822403367,-14.6119628533001,
122.276618419778)) ;
#51110 = CARTESIAN_POINT('Ctrl Pts',(-18.4706094581403,-14.8019138136881,
122.654469653778)) ;
#51111 = CARTESIAN_POINT('Ctrl Pts',(-18.2359363518528,-14.6219247332076,
122.465143513875)) ;
#51112 = CARTESIAN_POINT('Ctrl Pts',(-18.3531243947538,-14.81194874705,122.829681165894)) ;
#51113 = CARTESIAN_POINT('Ctrl Pts',(-18.0890820794357,-14.6319596665695,
122.684159240986)) ;
#51114 = CARTESIAN_POINT('Ctrl Pts',(-18.2687841779479,-14.8218337054293,
123.019642132794)) ;
#51115 = CARTESIAN_POINT('Ctrl Pts',(-17.983658882904,-14.6418446249488,122.921611991584)) ;
#51116 = CARTESIAN_POINT('Ctrl Pts',(-18.2178545293784,-14.8318993323519,
123.224997323136)) ;
#51117 = CARTESIAN_POINT('Ctrl Pts',(-17.9199993002954,-14.6519102518714,
123.178306439045)) ;
#51118 = CARTESIAN_POINT('Ctrl Pts',(-18.2034666313483,-14.8417384380163,
123.431379104992)) ;
#51119 = CARTESIAN_POINT('Ctrl Pts',(-17.9020169236197,-14.6617493575358,
123.436284553323)) ;
#51120 = CARTESIAN_POINT('Ctrl Pts',(-18.2253374188485,-14.8518012530216,
123.641768968564)) ;
#51121 = CARTESIAN_POINT('Ctrl Pts',(-17.9293579838891,-14.6718121725412,
123.699271479275)) ;
#51122 = CARTESIAN_POINT('Ctrl Pts',(-18.2826422959049,-14.8616974590703,
123.841793280128)) ;
#51123 = CARTESIAN_POINT('Ctrl Pts',(-18.0009916817392,-14.6817083785898,
123.949301618053)) ;
#51124 = CARTESIAN_POINT('Ctrl Pts',(-18.3736753162085,-14.8716382820956,
124.029885460281)) ;
#51125 = CARTESIAN_POINT('Ctrl Pts',(-18.1147854786849,-14.6916492016151,
124.184415931346)) ;
#51126 = CARTESIAN_POINT('Ctrl Pts',(-18.4967554476146,-14.8816428650742,
124.200469969171)) ;
#51127 = CARTESIAN_POINT('Ctrl Pts',(-18.2686378472388,-14.7016537845938,
124.39764506361)) ;
#51128 = CARTESIAN_POINT('Ctrl Pts',(-18.6479893488011,-14.891663759519,124.347127592409)) ;
#51129 = CARTESIAN_POINT('Ctrl Pts',(-18.4576820791071,-14.7116746790385,
124.580965224335)) ;
#51130 = CARTESIAN_POINT('Ctrl Pts',(-18.8200089658471,-14.9015556801084,
124.463997418573)) ;
#51131 = CARTESIAN_POINT('Ctrl Pts',(-18.6727084409181,-14.7215665996279,
124.727050531161)) ;
#51132 = CARTESIAN_POINT('Ctrl Pts',(-19.0115199934511,-14.9115491124538,
124.550366690489)) ;
#51133 = CARTESIAN_POINT('Ctrl Pts',(-18.9120984380812,-14.7315600319733,
124.835009694432)) ;
#51134 = CARTESIAN_POINT('Ctrl Pts',(-19.2141671143431,-14.9214947173536,
124.601860043974)) ;
#51135 = CARTESIAN_POINT('Ctrl Pts',(-19.1654082296755,-14.7415056368732,
124.899373825416)) ;
#51136 = CARTESIAN_POINT('Ctrl Pts',(-19.422692143887,-14.9314419908352,124.617812488144)) ;
#51137 = CARTESIAN_POINT('Ctrl Pts',(-19.4260649276648,-14.7514529103547,
124.919311654215)) ;
#51138 = CARTESIAN_POINT('Ctrl Pts',(-19.6328836255055,-14.9414899053115,
124.596874131456)) ;
#51139 = CARTESIAN_POINT('Ctrl Pts',(-19.6888039980711,-14.7615008248311,
124.89313599866)) ;
#51140 = CARTESIAN_POINT('Ctrl Pts',(-19.8322491561593,-14.9513375456589,
124.541062785767)) ;
#51141 = CARTESIAN_POINT('Ctrl Pts',(-19.9380105597996,-14.7713484651784,
124.823369065598)) ;
#51142 = CARTESIAN_POINT('Ctrl Pts',(-20.0213303949895,-14.9612992610355,
124.451042034006)) ;
#51143 = CARTESIAN_POINT('Ctrl Pts',(-20.1743610166879,-14.781310180555,124.710840541292)) ;
#51144 = CARTESIAN_POINT('Ctrl Pts',(-20.1929184638276,-14.9713278846083,
124.328511186806)) ;
#51145 = CARTESIAN_POINT('Ctrl Pts',(-20.3888445240509,-14.7913388041278,
124.557674698041)) ;
#51146 = CARTESIAN_POINT('Ctrl Pts',(-20.3389145430226,-14.9812382466747,
124.179885799862)) ;
#51147 = CARTESIAN_POINT('Ctrl Pts',(-20.571337784828,-14.8012491661942,124.371890859746)) ;
#51148 = CARTESIAN_POINT('Ctrl Pts',(-20.4576406506801,-14.9911729403271,
124.008044457199)) ;
#51149 = CARTESIAN_POINT('Ctrl Pts',(-20.7197431783026,-14.8111838598466,
124.157087470562)) ;
#51150 = CARTESIAN_POINT('Ctrl Pts',(-20.5454669216902,-15.001214783455,123.816080842499)) ;
#51151 = CARTESIAN_POINT('Ctrl Pts',(-20.8295234846959,-14.8212257029745,
123.917131743908)) ;
#51152 = CARTESIAN_POINT('Ctrl Pts',(-20.5979816592684,-15.0110992890254,
123.615000802519)) ;
#51153 = CARTESIAN_POINT('Ctrl Pts',(-20.8951642261479,-14.8311102085449,
123.66578082451)) ;
#51154 = CARTESIAN_POINT('Ctrl Pts',(-20.6152250273524,-15.0211013928106,
123.405463995573)) ;
#51155 = CARTESIAN_POINT('Ctrl Pts',(-20.9167156316037,-14.8411123123301,
123.403859517349)) ;
#51156 = CARTESIAN_POINT('Ctrl Pts',(-20.5961521969141,-15.0310197442256,
123.197788238171)) ;
#51157 = CARTESIAN_POINT('Ctrl Pts',(-20.8928717592807,-14.8510306637451,
123.144264974563)) ;
#51158 = CARTESIAN_POINT('Ctrl Pts',(-20.5405596861251,-15.0410674002465,
122.994035665252)) ;
#51159 = CARTESIAN_POINT('Ctrl Pts',(-20.8233784418533,-14.861078319766,122.889574983687)) ;
#51160 = CARTESIAN_POINT('Ctrl Pts',(-20.4521948522776,-15.0509385932747,
122.806217337189)) ;
#51161 = CARTESIAN_POINT('Ctrl Pts',(-20.7129195793855,-14.8709495127942,
122.654803032881)) ;
#51162 = CARTESIAN_POINT('Ctrl Pts',(-20.330284242075,-15.0610043064182,122.633308943981)) ;
#51163 = CARTESIAN_POINT('Ctrl Pts',(-20.5605298605741,-14.8810152259377,
122.438669790485)) ;
#51164 = CARTESIAN_POINT('Ctrl Pts',(-20.1834794070481,-15.0708567669908,
122.487109307967)) ;
#51165 = CARTESIAN_POINT('Ctrl Pts',(-20.3770184512462,-14.8908676865104,
122.255919658866)) ;
#51166 = CARTESIAN_POINT('Ctrl Pts',(-19.9518872310143,-15.0842852297134,
122.325790591143)) ;
#51167 = CARTESIAN_POINT('Ctrl Pts',(-20.0875427688117,-14.9042961492329,
122.054287113997)) ;
#51168 = CARTESIAN_POINT('Ctrl Pts',(-19.6903665057396,-15.0973661772305,
122.230682396376)) ;
#51169 = CARTESIAN_POINT('Ctrl Pts',(-19.7606733442006,-14.91737709675,121.935403530336)) ;
#51170 = CARTESIAN_POINT('Ctrl Pts',(-19.4082962992305,-15.110840675465,122.205756665579)) ;
#51171 = CARTESIAN_POINT('Ctrl Pts',(-19.4080294143567,-14.9308515949846,
121.904239537887)) ;
#51172 = CARTESIAN_POINT('Ctrl Pts',(-19.2023473006596,-15.1206727790745,
122.223870629062)) ;
#51173 = CARTESIAN_POINT('Ctrl Pts',(-19.1506048229786,-14.940683698594,121.926886772447)) ;
#51174 = CARTESIAN_POINT('Ctrl Pts',(-18.9998068488561,-15.1306386822012,
122.277363273524)) ;
#51175 = CARTESIAN_POINT('Ctrl Pts',(-18.8974267386482,-14.9506496017207,
121.993755117813)) ;
#51176 = CARTESIAN_POINT('Ctrl Pts',(-18.8085430621808,-15.1406660915114,
122.366073015869)) ;
#51177 = CARTESIAN_POINT('Ctrl Pts',(-18.6583498544115,-14.9606770110309,
122.104643278196)) ;
#51178 = CARTESIAN_POINT('Ctrl Pts',(-18.6376088448104,-15.150577122878,122.48516450023)) ;
#51179 = CARTESIAN_POINT('Ctrl Pts',(-18.4446798400263,-14.9705880423975,
122.253516252839)) ;
#51180 = CARTESIAN_POINT('Ctrl Pts',(-18.4395743724625,-15.163821430499,122.681015377369)) ;
#51181 = CARTESIAN_POINT('Ctrl Pts',(-18.1971580266742,-14.9838323500186,
122.498300087625)) ;
#51182 = CARTESIAN_POINT('Ctrl Pts',(-18.2607335132502,-15.1805219131702,
122.987645959784)) ;
#51183 = CARTESIAN_POINT('Ctrl Pts',(-17.9735883958197,-15.0005328326897,
122.881645823186)) ;
#51184 = CARTESIAN_POINT('Ctrl Pts',(-18.1977869763505,-15.197028742326,123.333061812602)) ;
#51185 = CARTESIAN_POINT('Ctrl Pts',(-17.8949212633086,-15.0170396618455,
123.3133312933)) ;
#51186 = CARTESIAN_POINT('Ctrl Pts',(-18.2199642495241,-15.2103393705636,
123.611928517238)) ;
#51187 = CARTESIAN_POINT('Ctrl Pts',(-17.9226408361223,-15.0303502900831,
123.661981974287)) ;
#51188 = CARTESIAN_POINT('Ctrl Pts',(-18.2726848636332,-15.2203319341037,
123.815325721179)) ;
#51189 = CARTESIAN_POINT('Ctrl Pts',(-17.9885443790157,-15.0403428536232,
123.916213406542)) ;
#51190 = CARTESIAN_POINT('Ctrl Pts',(-18.3604503080189,-15.2303620171052,
124.007021668416)) ;
#51191 = CARTESIAN_POINT('Ctrl Pts',(-18.0982567043705,-15.0503729366247,
124.155839488653)) ;
#51192 = CARTESIAN_POINT('Ctrl Pts',(-18.5172815670806,-15.243535621103,124.235376320227)) ;
#51193 = CARTESIAN_POINT('Ctrl Pts',(-18.2942816286453,-15.0635465406225,
124.441261778011)) ;
#51194 = CARTESIAN_POINT('Ctrl Pts',(-18.785763220475,-15.2601733263344,124.465502936072)) ;
#51195 = CARTESIAN_POINT('Ctrl Pts',(-18.629900480376,-15.0801842458539,124.728937538322)) ;
#51196 = CARTESIAN_POINT('Ctrl Pts',(-19.1813810887829,-15.2800550889018,
124.614910728195)) ;
#51197 = CARTESIAN_POINT('Ctrl Pts',(-19.1244402676743,-15.1000660084213,
124.91568323805)) ;
#51198 = CARTESIAN_POINT('Ctrl Pts',(-19.536304822624,-15.2967514411183,124.619219755491)) ;
#51199 = CARTESIAN_POINT('Ctrl Pts',(-19.5680268437064,-15.1167623606378,
124.921075711026)) ;
#51200 = CARTESIAN_POINT('Ctrl Pts',(-19.8044165799873,-15.3099084689074,
124.551173766666)) ;
#51201 = CARTESIAN_POINT('Ctrl Pts',(-19.9032277012803,-15.1299193884269,
124.836006277141)) ;
#51202 = CARTESIAN_POINT('Ctrl Pts',(-20.0610790101127,-15.3232858235509,
124.436222758126)) ;
#51203 = CARTESIAN_POINT('Ctrl Pts',(-20.2240299228811,-15.1432967430705,
124.692326184218)) ;
#51204 = CARTESIAN_POINT('Ctrl Pts',(-20.3337494420324,-15.3398166578097,
124.214377221525)) ;
#51205 = CARTESIAN_POINT('Ctrl Pts',(-20.5648835409731,-15.1598275773293,
124.415004995592)) ;
#51206 = CARTESIAN_POINT('Ctrl Pts',(-20.552438862062,-15.3597813475528,123.850580679781)) ;
#51207 = CARTESIAN_POINT('Ctrl Pts',(-20.8382356612196,-15.1797922670724,
123.960261264847)) ;
#51208 = CARTESIAN_POINT('Ctrl Pts',(-20.6332747084739,-15.3796978409765,
123.434880640488)) ;
#51209 = CARTESIAN_POINT('Ctrl Pts',(-20.9392779041822,-15.199708760496,123.440635012871)) ;
#51210 = CARTESIAN_POINT('Ctrl Pts',(-20.5683199143235,-15.399587560326,123.016946237213)) ;
#51211 = CARTESIAN_POINT('Ctrl Pts',(-20.858080531106,-15.2195984798456,122.918218801379)) ;
#51212 = CARTESIAN_POINT('Ctrl Pts',(-20.3631949850862,-15.4195942899739,
122.644342249502)) ;
#51213 = CARTESIAN_POINT('Ctrl Pts',(-20.6016712397754,-15.2396052094934,
122.452465436855)) ;
#51214 = CARTESIAN_POINT('Ctrl Pts',(-20.0460283351885,-15.4394323436208,
122.366126910109)) ;
#51215 = CARTESIAN_POINT('Ctrl Pts',(-20.2052118911002,-15.2594432631403,
122.104699831963)) ;
#51216 = CARTESIAN_POINT('Ctrl Pts',(-19.6501954328286,-15.4594256818344,
122.211302972032)) ;
#51217 = CARTESIAN_POINT('Ctrl Pts',(-19.7104197648899,-15.2794366013539,
121.911172705937)) ;
#51218 = CARTESIAN_POINT('Ctrl Pts',(-19.22747548443,-15.479308481241,122.20116645109)) ;
#51219 = CARTESIAN_POINT('Ctrl Pts',(-19.1820210308517,-15.2993194007605,
121.898505003943)) ;
#51220 = CARTESIAN_POINT('Ctrl Pts',(-18.8264426794319,-15.4992006621597,
122.335208188009)) ;
#51221 = CARTESIAN_POINT('Ctrl Pts',(-18.6807320924974,-15.3192115816792,
122.066058969295)) ;
#51222 = CARTESIAN_POINT('Ctrl Pts',(-18.4944215574731,-15.5191028406548,
122.597782843408)) ;
#51223 = CARTESIAN_POINT('Ctrl Pts',(-18.2657076845191,-15.3391137601743,
122.394277865511)) ;
#51224 = CARTESIAN_POINT('Ctrl Pts',(-18.2711780684696,-15.5391401518585,
122.960525542868)) ;
#51225 = CARTESIAN_POINT('Ctrl Pts',(-17.9866547279515,-15.359151071378,122.847707709297)) ;
#51226 = CARTESIAN_POINT('Ctrl Pts',(-18.1854465994955,-15.5589525933994,
123.373166514348)) ;
#51227 = CARTESIAN_POINT('Ctrl Pts',(-17.879492215553,-15.3789635129189,123.363506708318)) ;
#51228 = CARTESIAN_POINT('Ctrl Pts',(-18.2465194115136,-15.5790178341343,
123.795207249882)) ;
#51229 = CARTESIAN_POINT('Ctrl Pts',(-17.9558345968631,-15.3990287536538,
123.891058298206)) ;
#51230 = CARTESIAN_POINT('Ctrl Pts',(-18.4447532133238,-15.5987750389901,
124.16581727744)) ;
#51231 = CARTESIAN_POINT('Ctrl Pts',(-18.2036257716139,-15.4187859585096,
124.354317293493)) ;
#51232 = CARTESIAN_POINT('Ctrl Pts',(-18.7611937431446,-15.6188083116358,
124.450642539288)) ;
#51233 = CARTESIAN_POINT('Ctrl Pts',(-18.5991767272437,-15.4388192311553,
124.710349085209)) ;
#51234 = CARTESIAN_POINT('Ctrl Pts',(-19.1518899017671,-15.6386212200896,
124.608729629548)) ;
#51235 = CARTESIAN_POINT('Ctrl Pts',(-19.0875441523598,-15.4586321396092,
124.907957059647)) ;
#51236 = CARTESIAN_POINT('Ctrl Pts',(-19.5765723952849,-15.6586173662171,
124.624694592537)) ;
#51237 = CARTESIAN_POINT('Ctrl Pts',(-19.6183970906581,-15.4786282857366,
124.927914166643)) ;
#51238 = CARTESIAN_POINT('Ctrl Pts',(-19.9789149548444,-15.6784791194396,
124.495740343834)) ;
#51239 = CARTESIAN_POINT('Ctrl Pts',(-20.1213238856596,-15.4984900389591,
124.766723103384)) ;
#51240 = CARTESIAN_POINT('Ctrl Pts',(-20.3161903072829,-15.6985476365677,
124.234500907358)) ;
#51241 = CARTESIAN_POINT('Ctrl Pts',(-20.5429196527663,-15.5185585560872,
124.440174246545)) ;
#51242 = CARTESIAN_POINT('Ctrl Pts',(-20.5412403283249,-15.7183785095645,
123.877812094549)) ;
#51243 = CARTESIAN_POINT('Ctrl Pts',(-20.8242320697883,-15.538389429084,123.994315885988)) ;
#51244 = CARTESIAN_POINT('Ctrl Pts',(-20.6325525181329,-15.7383004203812,
123.464277815718)) ;
#51245 = CARTESIAN_POINT('Ctrl Pts',(-20.938374323766,-15.5583113399007,123.477399544052)) ;
#51246 = CARTESIAN_POINT('Ctrl Pts',(-20.5770999387733,-15.7582298638165,
123.044097906908)) ;
#51247 = CARTESIAN_POINT('Ctrl Pts',(-20.8690610709312,-15.578240783336,122.952175131957)) ;
#51248 = CARTESIAN_POINT('Ctrl Pts',(-20.3819841700265,-15.7781395339329,
122.668482285981)) ;
#51249 = CARTESIAN_POINT('Ctrl Pts',(-20.6251692264673,-15.5981504534524,
122.482655310818)) ;
#51250 = CARTESIAN_POINT('Ctrl Pts',(-20.071398669403,-15.7980128911957,122.381885903197)) ;
#51251 = CARTESIAN_POINT('Ctrl Pts',(-20.2369405025118,-15.6180238107153,
122.124408326918)) ;
#51252 = CARTESIAN_POINT('Ctrl Pts',(-19.6794075493568,-15.8180044258137,
122.217622884656)) ;
#51253 = CARTESIAN_POINT('Ctrl Pts',(-19.7469529682798,-15.6380153453332,
121.919076471675)) ;
#51254 = CARTESIAN_POINT('Ctrl Pts',(-19.2574526738448,-15.8378700432244,
122.196935178988)) ;
#51255 = CARTESIAN_POINT('Ctrl Pts',(-19.2195107524635,-15.6578809627439,
121.893213319118)) ;
#51256 = CARTESIAN_POINT('Ctrl Pts',(-18.8513755370978,-15.8578509730526,
122.321775663419)) ;
#51257 = CARTESIAN_POINT('Ctrl Pts',(-18.7119132759403,-15.6778618925722,
122.049260143465)) ;
#51258 = CARTESIAN_POINT('Ctrl Pts',(-18.5132612033128,-15.8777894351358,
122.577542069427)) ;
#51259 = CARTESIAN_POINT('Ctrl Pts',(-18.289268421837,-15.6978003546553,122.368964780119)) ;
#51260 = CARTESIAN_POINT('Ctrl Pts',(-18.2826819587382,-15.8976816283575,
122.932185153396)) ;
#51261 = CARTESIAN_POINT('Ctrl Pts',(-18.0010412601392,-15.717692547877,122.812265657322)) ;
#51262 = CARTESIAN_POINT('Ctrl Pts',(-18.1868169762122,-15.9176523433929,
123.34575803658)) ;
#51263 = CARTESIAN_POINT('Ctrl Pts',(-17.8812058281196,-15.7376632629124,
123.329230583623)) ;
#51264 = CARTESIAN_POINT('Ctrl Pts',(-18.2367313458389,-15.937462015059,123.764098817235)) ;
#51265 = CARTESIAN_POINT('Ctrl Pts',(-17.9435942350171,-15.7574729345785,
123.852155946831)) ;
#51266 = CARTESIAN_POINT('Ctrl Pts',(-18.4277666040295,-15.9574552317502,
124.143691492752)) ;
#51267 = CARTESIAN_POINT('Ctrl Pts',(-18.1823832686069,-15.7774661512697,
124.326648974628)) ;
#51268 = CARTESIAN_POINT('Ctrl Pts',(-18.7346680099378,-15.9773061439465,
124.433713845188)) ;
#51269 = CARTESIAN_POINT('Ctrl Pts',(-18.5660086877581,-15.797317063466,124.689180060819)) ;
#51270 = CARTESIAN_POINT('Ctrl Pts',(-19.1263185071962,-15.9973807502655,
124.603150136167)) ;
#51271 = CARTESIAN_POINT('Ctrl Pts',(-19.0555605459573,-15.8173916697851,
124.900980308438)) ;
#51272 = CARTESIAN_POINT('Ctrl Pts',(-19.4769940370043,-16.0138973821489,
124.624006616587)) ;
#51273 = CARTESIAN_POINT('Ctrl Pts',(-19.493934124644,-15.8339083016684,124.927054797122)) ;
#51274 = CARTESIAN_POINT('Ctrl Pts',(-19.7517414985942,-16.027236089843,124.568093364996)) ;
#51275 = CARTESIAN_POINT('Ctrl Pts',(-19.8373421473109,-15.8472470093625,
124.857167360089)) ;
#51276 = CARTESIAN_POINT('Ctrl Pts',(-19.9444057679308,-16.0370784641513,
124.492551498524)) ;
#51277 = CARTESIAN_POINT('Ctrl Pts',(-20.0781804979996,-15.8570893836708,
124.762739876029)) ;
#51278 = CARTESIAN_POINT('Ctrl Pts',(-20.1249049321985,-16.047133484134,124.382567620846)) ;
#51279 = CARTESIAN_POINT('Ctrl Pts',(-20.3037960539398,-15.8671444036535,
124.625272793391)) ;
#51280 = CARTESIAN_POINT('Ctrl Pts',(-20.3337092884455,-16.0603656407916,
124.198785774196)) ;
#51281 = CARTESIAN_POINT('Ctrl Pts',(-20.5648469002763,-15.8803765603111,
124.395495442231)) ;
#51282 = CARTESIAN_POINT('Ctrl Pts',(-20.5299755382867,-16.0769806081367,
123.904990129354)) ;
#51283 = CARTESIAN_POINT('Ctrl Pts',(-20.8101326081078,-15.8969915276562,
124.02832371337)) ;
#51284 = CARTESIAN_POINT('Ctrl Pts',(-20.6139164154991,-16.0935751951479,
123.562338411869)) ;
#51285 = CARTESIAN_POINT('Ctrl Pts',(-20.9150857053266,-15.9135861146674,
123.599951810543)) ;
#51286 = CARTESIAN_POINT('Ctrl Pts',(-20.6085033819079,-16.1068087635033,
123.284128846805)) ;
#51287 = CARTESIAN_POINT('Ctrl Pts',(-20.9083137995466,-15.9268196830228,
123.252228775175)) ;
#51288 = CARTESIAN_POINT('Ctrl Pts',(-20.5678420997152,-16.1168523813119,
123.076956614971)) ;
#51289 = CARTESIAN_POINT('Ctrl Pts',(-20.8574915955287,-15.9368633008315,
122.993254896118)) ;
#51290 = CARTESIAN_POINT('Ctrl Pts',(-20.4930658285917,-16.1267393055468,
122.882997750619)) ;
#51291 = CARTESIAN_POINT('Ctrl Pts',(-20.7640240612381,-15.9467502250663,
122.750807958824)) ;
#51292 = CARTESIAN_POINT('Ctrl Pts',(-20.3849611897659,-16.1367299599936,
122.702938885806)) ;
#51293 = CARTESIAN_POINT('Ctrl Pts',(-20.6288932483085,-15.9567408795131,
122.525730668272)) ;
#51294 = CARTESIAN_POINT('Ctrl Pts',(-20.2475814117215,-16.1466917184475,
122.544854107054)) ;
#51295 = CARTESIAN_POINT('Ctrl Pts',(-20.4571800170958,-15.9667026379671,
122.328129169663)) ;
#51296 = CARTESIAN_POINT('Ctrl Pts',(-20.0298504240982,-16.1600315835148,
122.368082548189)) ;
#51297 = CARTESIAN_POINT('Ctrl Pts',(-20.1849716449942,-15.9800425030343,
122.107130949227)) ;
#51298 = CARTESIAN_POINT('Ctrl Pts',(-19.7713257253914,-16.1733403664281,
122.253045017901)) ;
#51299 = CARTESIAN_POINT('Ctrl Pts',(-19.8618390549998,-15.9933512859476,
121.963354375823)) ;
#51300 = CARTESIAN_POINT('Ctrl Pts',(-19.4973854044494,-16.1865361238721,
122.209149372698)) ;
#51301 = CARTESIAN_POINT('Ctrl Pts',(-19.519435246012,-16.0065470433916,121.908483591754)) ;
#51302 = CARTESIAN_POINT('Ctrl Pts',(-19.2879723974171,-16.1964980075486,
122.211840246962)) ;
#51303 = CARTESIAN_POINT('Ctrl Pts',(-19.257664641132,-16.0165089270682,121.911843867943)) ;
#51304 = CARTESIAN_POINT('Ctrl Pts',(-19.0805966754575,-16.2065411170633,
122.251508529244)) ;
#51305 = CARTESIAN_POINT('Ctrl Pts',(-18.9984455353408,-16.0265520365828,
121.961426597221)) ;
#51306 = CARTESIAN_POINT('Ctrl Pts',(-18.8869132560321,-16.2163933670625,
122.324927691343)) ;
#51307 = CARTESIAN_POINT('Ctrl Pts',(-18.756339852645,-16.036404286582,122.053197919674)) ;
#51308 = CARTESIAN_POINT('Ctrl Pts',(-18.7065271330224,-16.226364904013,122.431685493257)) ;
#51309 = CARTESIAN_POINT('Ctrl Pts',(-18.5308557512395,-16.0463758235325,
122.186642824369)) ;
#51310 = CARTESIAN_POINT('Ctrl Pts',(-18.5470082080786,-16.2363601694905,
122.56851706965)) ;
#51311 = CARTESIAN_POINT('Ctrl Pts',(-18.3314551895401,-16.05637108901,122.357680218266)) ;
#51312 = CARTESIAN_POINT('Ctrl Pts',(-18.413387011108,-16.2463941423641,122.731722217809)) ;
#51313 = CARTESIAN_POINT('Ctrl Pts',(-18.1644264950383,-16.0664050618836,
122.561684900237)) ;
#51314 = CARTESIAN_POINT('Ctrl Pts',(-18.3116651483155,-16.2562495571265,
122.91224766768)) ;
#51315 = CARTESIAN_POINT('Ctrl Pts',(-18.0372716141847,-16.076260476646,122.787340539563)) ;
#51316 = CARTESIAN_POINT('Ctrl Pts',(-18.2415770596379,-16.2662488346353,
123.110397616458)) ;
#51317 = CARTESIAN_POINT('Ctrl Pts',(-17.9496588450067,-16.0862597541548,
123.035027131205)) ;
#51318 = CARTESIAN_POINT('Ctrl Pts',(-18.2070866766184,-16.2761440187983,
123.315582482187)) ;
#51319 = CARTESIAN_POINT('Ctrl Pts',(-17.9065430992982,-16.0961549383178,
123.291508010325)) ;
#51320 = CARTESIAN_POINT('Ctrl Pts',(-18.2087980539472,-16.2862043984391,
123.527047846686)) ;
#51321 = CARTESIAN_POINT('Ctrl Pts',(-17.9086795501049,-16.1062153179586,
123.555839709405)) ;
#51322 = CARTESIAN_POINT('Ctrl Pts',(-18.2462808343881,-16.2960542674472,
123.730723195858)) ;
#51323 = CARTESIAN_POINT('Ctrl Pts',(-17.9555303864305,-16.1160651869667,
123.810434776904)) ;
#51324 = CARTESIAN_POINT('Ctrl Pts',(-18.3194286022039,-16.3060858286551,
123.928512270352)) ;
#51325 = CARTESIAN_POINT('Ctrl Pts',(-18.0469625661562,-16.1260967481746,
124.057672087781)) ;
#51326 = CARTESIAN_POINT('Ctrl Pts',(-18.425966779491,-16.3160962775374,124.110026603965)) ;
#51327 = CARTESIAN_POINT('Ctrl Pts',(-18.1801329407007,-16.1361071970569,
124.284566442548)) ;
#51328 = CARTESIAN_POINT('Ctrl Pts',(-18.560797825782,-16.3260030169544,124.268754201217)) ;
#51329 = CARTESIAN_POINT('Ctrl Pts',(-18.3486698657087,-16.1460139364739,
124.482977937669)) ;
#51330 = CARTESIAN_POINT('Ctrl Pts',(-18.7213836715412,-16.3359410330228,
124.402388892912)) ;
#51331 = CARTESIAN_POINT('Ctrl Pts',(-18.549400664377,-16.1559519525423,124.650023534822)) ;
#51332 = CARTESIAN_POINT('Ctrl Pts',(-18.9039216281586,-16.3459462794739,
124.506949932254)) ;
#51333 = CARTESIAN_POINT('Ctrl Pts',(-18.7775718600517,-16.1659571989935,
124.780727182853)) ;
#51334 = CARTESIAN_POINT('Ctrl Pts',(-19.1025026858816,-16.3559803405302,
124.578083634945)) ;
#51335 = CARTESIAN_POINT('Ctrl Pts',(-19.025797253829,-16.1759912600497,124.869646857172)) ;
#51336 = CARTESIAN_POINT('Ctrl Pts',(-19.3064644872942,-16.3658254215884,
124.613343041828)) ;
#51337 = CARTESIAN_POINT('Ctrl Pts',(-19.2807496064473,-16.1858363411079,
124.913723831407)) ;
#51338 = CARTESIAN_POINT('Ctrl Pts',(-19.5163642119704,-16.3758112275419,
124.61303502221)) ;
#51339 = CARTESIAN_POINT('Ctrl Pts',(-19.5431244270231,-16.1958221470614,
124.91334140973)) ;
#51340 = CARTESIAN_POINT('Ctrl Pts',(-19.7220636700193,-16.3857460480961,
124.576608850265)) ;
#51341 = CARTESIAN_POINT('Ctrl Pts',(-19.8002495182627,-16.2057569676156,
124.86781116913)) ;
#51342 = CARTESIAN_POINT('Ctrl Pts',(-19.9206078791978,-16.3958035732283,
124.503981755754)) ;
#51343 = CARTESIAN_POINT('Ctrl Pts',(-20.0484305676392,-16.2158144927478,
124.777029791005)) ;
#51344 = CARTESIAN_POINT('Ctrl Pts',(-20.0994392626122,-16.4056252238796,
124.400718208666)) ;
#51345 = CARTESIAN_POINT('Ctrl Pts',(-20.2719717474174,-16.2256361433992,
124.647952173923)) ;
#51346 = CARTESIAN_POINT('Ctrl Pts',(-20.2616227730663,-16.4156812873844,
124.265132165577)) ;
#51347 = CARTESIAN_POINT('Ctrl Pts',(-20.4747026405701,-16.2356922069039,
124.478471590854)) ;
#51348 = CARTESIAN_POINT('Ctrl Pts',(-20.3959657201901,-16.4256219544483,
124.105038813883)) ;
#51349 = CARTESIAN_POINT('Ctrl Pts',(-20.6426334924399,-16.2456328739678,
124.278356285914)) ;
#51350 = CARTESIAN_POINT('Ctrl Pts',(-20.5006527032414,-16.4355263481143,
123.925043149726)) ;
#51351 = CARTESIAN_POINT('Ctrl Pts',(-20.7734945783761,-16.2555372676338,
124.053362462571)) ;
#51352 = CARTESIAN_POINT('Ctrl Pts',(-20.5733913233739,-16.4455728718773,
123.726774248668)) ;
#51353 = CARTESIAN_POINT('Ctrl Pts',(-20.8644201158758,-16.2655837913968,
123.805527276541)) ;
#51354 = CARTESIAN_POINT('Ctrl Pts',(-20.6102491313444,-16.4554689548937,
123.521980484657)) ;
#51355 = CARTESIAN_POINT('Ctrl Pts',(-20.9104948423804,-16.2754798744132,
123.549534920319)) ;
#51356 = CARTESIAN_POINT('Ctrl Pts',(-20.6109490500216,-16.4655356541237,
123.310385747446)) ;
#51357 = CARTESIAN_POINT('Ctrl Pts',(-20.9113721564966,-16.2855465736432,
123.28504171042)) ;
#51358 = CARTESIAN_POINT('Ctrl Pts',(-20.5759933517223,-16.4753592645248,
123.106810422099)) ;
#51359 = CARTESIAN_POINT('Ctrl Pts',(-20.8676796984875,-16.2953701840443,
123.030571216628)) ;
#51360 = CARTESIAN_POINT('Ctrl Pts',(-20.504941661928,-16.4854151247023,122.907730675288)) ;
#51361 = CARTESIAN_POINT('Ctrl Pts',(-20.7788672824088,-16.3054260442218,
122.781720920148)) ;
#51362 = CARTESIAN_POINT('Ctrl Pts',(-20.4014184334642,-16.4953482710072,
122.726342025547)) ;
#51363 = CARTESIAN_POINT('Ctrl Pts',(-20.6494650622992,-16.3153591905267,
122.554983567569)) ;
#51364 = CARTESIAN_POINT('Ctrl Pts',(-20.2681709832991,-16.5052935267778,
122.565253208005)) ;
#51365 = CARTESIAN_POINT('Ctrl Pts',(-20.4829072058743,-16.3253044462973,
122.353620794786)) ;
#51366 = CARTESIAN_POINT('Ctrl Pts',(-20.1084390136851,-16.5152768252163,
122.429067661281)) ;
#51367 = CARTESIAN_POINT('Ctrl Pts',(-20.2832435138796,-16.3352877447358,
122.183387066426)) ;
#51368 = CARTESIAN_POINT('Ctrl Pts',(-19.9264011878482,-16.5253140053629,
122.322380814143)) ;
#51369 = CARTESIAN_POINT('Ctrl Pts',(-20.0556974558092,-16.3453249248824,
122.050026596241)) ;
#51370 = CARTESIAN_POINT('Ctrl Pts',(-19.7322826676452,-16.5351685580724,
122.24994521566)) ;
#51371 = CARTESIAN_POINT('Ctrl Pts',(-19.8130492091403,-16.3551794775919,
121.959479734029)) ;
#51372 = CARTESIAN_POINT('Ctrl Pts',(-19.5256465946988,-16.5451680765197,
122.211483731313)) ;
#51373 = CARTESIAN_POINT('Ctrl Pts',(-19.5547543717607,-16.3651789960392,
121.911400782408)) ;
#51374 = CARTESIAN_POINT('Ctrl Pts',(-19.3175976842918,-16.5550631589818,
122.209284349518)) ;
#51375 = CARTESIAN_POINT('Ctrl Pts',(-19.2946925229252,-16.3750740785013,
121.908649507568)) ;
#51376 = CARTESIAN_POINT('Ctrl Pts',(-19.1089595995031,-16.5651237044879,
122.243820775951)) ;
#51377 = CARTESIAN_POINT('Ctrl Pts',(-19.0338948184378,-16.3851346240074,
121.951817978714)) ;
#51378 = CARTESIAN_POINT('Ctrl Pts',(-18.9135973762475,-16.5749730117359,
122.312488918254)) ;
#51379 = CARTESIAN_POINT('Ctrl Pts',(-18.7896903908939,-16.3949839312554,
122.037651600256)) ;
#51380 = CARTESIAN_POINT('Ctrl Pts',(-18.7296234980827,-16.5850001018232,
122.415390660692)) ;
#51381 = CARTESIAN_POINT('Ctrl Pts',(-18.5597221684491,-16.4050110213428,
122.166277137721)) ;
#51382 = CARTESIAN_POINT('Ctrl Pts',(-18.5666258182799,-16.5950290059602,
122.549139612565)) ;
#51383 = CARTESIAN_POINT('Ctrl Pts',(-18.3559738382257,-16.4150399254797,
122.333461717316)) ;
#51384 = CARTESIAN_POINT('Ctrl Pts',(-18.4315607292266,-16.6048728710595,
122.705925530433)) ;
#51385 = CARTESIAN_POINT('Ctrl Pts',(-18.1871403033564,-16.424883790579,122.529443722396)) ;
#51386 = CARTESIAN_POINT('Ctrl Pts',(-18.3236876247588,-16.6148686977679,
122.886268946656)) ;
#51387 = CARTESIAN_POINT('Ctrl Pts',(-18.0522973394285,-16.4348796172874,
122.754872248822)) ;
#51388 = CARTESIAN_POINT('Ctrl Pts',(-18.2489074259559,-16.6248939144169,
123.083322704059)) ;
#51389 = CARTESIAN_POINT('Ctrl Pts',(-17.9588203684048,-16.4449048339364,
123.001188739164)) ;
#51390 = CARTESIAN_POINT('Ctrl Pts',(-18.2097358480084,-16.6347837465745,
123.287518104386)) ;
#51391 = CARTESIAN_POINT('Ctrl Pts',(-17.9098539907051,-16.454794666094,123.256433493442)) ;
#51392 = CARTESIAN_POINT('Ctrl Pts',(-18.2062951743029,-16.6447746026592,
123.497522176624)) ;
#51393 = CARTESIAN_POINT('Ctrl Pts',(-17.905551463918,-16.4647855221787,123.518938743189)) ;
#51394 = CARTESIAN_POINT('Ctrl Pts',(-18.2392588330395,-16.6547196972521,
123.70398395006)) ;
#51395 = CARTESIAN_POINT('Ctrl Pts',(-17.946754439527,-16.4747306167716,123.777016725502)) ;
#51396 = CARTESIAN_POINT('Ctrl Pts',(-18.3072491133093,-16.6646716010202,
123.901857207325)) ;
#51397 = CARTESIAN_POINT('Ctrl Pts',(-18.0317409620989,-16.4846825205397,
124.0243592607)) ;
#51398 = CARTESIAN_POINT('Ctrl Pts',(-18.4095792800101,-16.6747080004896,
124.086372613872)) ;
#51399 = CARTESIAN_POINT('Ctrl Pts',(-18.1596521830573,-16.4947189200091,
124.255004194096)) ;
#51400 = CARTESIAN_POINT('Ctrl Pts',(-18.5403323023959,-16.6845970705783,
124.24801603038)) ;
#51401 = CARTESIAN_POINT('Ctrl Pts',(-18.323092810584,-16.5046079900978,124.457060171017)) ;
#51402 = CARTESIAN_POINT('Ctrl Pts',(-18.6984981846878,-16.6945863599492,
124.386161267394)) ;
#51403 = CARTESIAN_POINT('Ctrl Pts',(-18.5207993713785,-16.5145972794687,
124.629742950679)) ;
#51404 = CARTESIAN_POINT('Ctrl Pts',(-18.8777747357484,-16.7045449261589,
124.494277089496)) ;
#51405 = CARTESIAN_POINT('Ctrl Pts',(-18.7448946530804,-16.5245558456784,
124.764889240913)) ;
#51406 = CARTESIAN_POINT('Ctrl Pts',(-19.071775886629,-16.7144444973757,124.569661405429)) ;
#51407 = CARTESIAN_POINT('Ctrl Pts',(-18.9873964306121,-16.5344554168952,
124.859121188033)) ;
#51408 = CARTESIAN_POINT('Ctrl Pts',(-19.2789592287976,-16.7244924117899,
124.6107434715)) ;
#51409 = CARTESIAN_POINT('Ctrl Pts',(-19.2463751320816,-16.5445033313095,
124.910475054248)) ;
#51410 = CARTESIAN_POINT('Ctrl Pts',(-19.4869725711741,-16.7343877546505,
124.615324364318)) ;
#51411 = CARTESIAN_POINT('Ctrl Pts',(-19.5063926931803,-16.55439867417,124.916202482364)) ;
#51412 = CARTESIAN_POINT('Ctrl Pts',(-19.6960268210127,-16.7444494485979,
124.583223874358)) ;
#51413 = CARTESIAN_POINT('Ctrl Pts',(-19.7677103787035,-16.5644603681175,
124.876078188876)) ;
#51414 = CARTESIAN_POINT('Ctrl Pts',(-19.8920494172545,-16.7542939016821,
124.51680250823)) ;
#51415 = CARTESIAN_POINT('Ctrl Pts',(-20.01274028279,-16.5743048212016,124.793052261306)) ;
#51416 = CARTESIAN_POINT('Ctrl Pts',(-20.0760402865908,-16.7642545866405,
124.416833948505)) ;
#51417 = CARTESIAN_POINT('Ctrl Pts',(-20.2427297442584,-16.5842655061601,
124.668092227986)) ;
#51418 = CARTESIAN_POINT('Ctrl Pts',(-20.2409080973794,-16.7742905191491,
124.285163854322)) ;
#51419 = CARTESIAN_POINT('Ctrl Pts',(-20.4488151081097,-16.5943014386686,
124.50350557831)) ;
#51420 = CARTESIAN_POINT('Ctrl Pts',(-20.3785099430271,-16.7841791348371,
124.129336922064)) ;
#51421 = CARTESIAN_POINT('Ctrl Pts',(-20.620818876143,-16.6041900543566,124.308721851052)) ;
#51422 = CARTESIAN_POINT('Ctrl Pts',(-20.4887120097041,-16.7941935439796,
123.949931511366)) ;
#51423 = CARTESIAN_POINT('Ctrl Pts',(-20.7585722336861,-16.6142044634991,
124.08446554872)) ;
#51424 = CARTESIAN_POINT('Ctrl Pts',(-20.5657191627696,-16.8042273529374,
123.753561423584)) ;
#51425 = CARTESIAN_POINT('Ctrl Pts',(-20.8548321534226,-16.6242382724569,
123.839003471693)) ;
#51426 = CARTESIAN_POINT('Ctrl Pts',(-20.6071867597122,-16.8140578071936,
123.551072730248)) ;
#51427 = CARTESIAN_POINT('Ctrl Pts',(-20.906667816104,-16.6340687267131,123.585891332069)) ;
#51428 = CARTESIAN_POINT('Ctrl Pts',(-20.6130753200358,-16.8241354747718,
123.339330931498)) ;
#51429 = CARTESIAN_POINT('Ctrl Pts',(-20.9140293674957,-16.6441463942913,
123.321214560571)) ;
#51430 = CARTESIAN_POINT('Ctrl Pts',(-20.582897122482,-16.833987342894,123.134379068764)) ;
#51431 = CARTESIAN_POINT('Ctrl Pts',(-20.8763072382661,-16.6539982624135,
123.06502331283)) ;
#51432 = CARTESIAN_POINT('Ctrl Pts',(-20.5163171737132,-16.8440603804594,
122.933388787276)) ;
#51433 = CARTESIAN_POINT('Ctrl Pts',(-20.7930831563984,-16.6640712999789,
122.813785637992)) ;
#51434 = CARTESIAN_POINT('Ctrl Pts',(-20.4180968317784,-16.8539029338102,
122.751244860052)) ;
#51435 = CARTESIAN_POINT('Ctrl Pts',(-20.6703077318771,-16.6739138533298,
122.58610411904)) ;
#51436 = CARTESIAN_POINT('Ctrl Pts',(-20.2885154375274,-16.8638833293037,
122.586232749684)) ;
#51437 = CARTESIAN_POINT('Ctrl Pts',(-20.5083311852049,-16.6838942488232,
122.379838432665)) ;
#51438 = CARTESIAN_POINT('Ctrl Pts',(-20.1313776052616,-16.8739018072815,
122.445995465439)) ;
#51439 = CARTESIAN_POINT('Ctrl Pts',(-20.3119093380775,-16.693912726801,122.204541346618)) ;
#51440 = CARTESIAN_POINT('Ctrl Pts',(-19.9549021525347,-16.8837851215876,
122.336275047287)) ;
#51441 = CARTESIAN_POINT('Ctrl Pts',(-20.0913143431546,-16.7037960411071,
122.067389838445)) ;
#51442 = CARTESIAN_POINT('Ctrl Pts',(-19.7584673745493,-16.8938534241263,
122.257523549518)) ;
#51443 = CARTESIAN_POINT('Ctrl Pts',(-19.8457714437735,-16.7138643436458,
121.968950139383)) ;
#51444 = CARTESIAN_POINT('Ctrl Pts',(-19.5562266361521,-16.9036834713997,
122.214849851963)) ;
#51445 = CARTESIAN_POINT('Ctrl Pts',(-19.5929691002895,-16.7236943909192,
121.915607289787)) ;
#51446 = CARTESIAN_POINT('Ctrl Pts',(-19.3447520721929,-16.9137503428152,
122.207507802747)) ;
#51447 = CARTESIAN_POINT('Ctrl Pts',(-19.3286263043278,-16.7337612623347,
121.906429428128)) ;
#51448 = CARTESIAN_POINT('Ctrl Pts',(-19.1388680110044,-16.9236393816143,
122.236594479174)) ;
#51449 = CARTESIAN_POINT('Ctrl Pts',(-19.0712701351057,-16.7436503011338,
121.942787563432)) ;
#51450 = CARTESIAN_POINT('Ctrl Pts',(-18.9389316545158,-16.9336360797484,
122.301281101622)) ;
#51451 = CARTESIAN_POINT('Ctrl Pts',(-18.8213494437003,-16.7536469992679,
122.023645715545)) ;
#51452 = CARTESIAN_POINT('Ctrl Pts',(-18.7540959744669,-16.9435885054603,
122.39935968639)) ;
#51453 = CARTESIAN_POINT('Ctrl Pts',(-18.5903042631905,-16.7635994249799,
122.146243992507)) ;
#51454 = CARTESIAN_POINT('Ctrl Pts',(-18.5891273339633,-16.9535298076933,
122.527650967993)) ;
#51455 = CARTESIAN_POINT('Ctrl Pts',(-18.3840928902973,-16.7735407272128,
122.306608387276)) ;
#51456 = CARTESIAN_POINT('Ctrl Pts',(-18.4481547796409,-16.9635130467772,
122.683169969797)) ;
#51457 = CARTESIAN_POINT('Ctrl Pts',(-18.2078769997332,-16.7835239662967,
122.501007316653)) ;
#51458 = CARTESIAN_POINT('Ctrl Pts',(-18.3360050079193,-16.9735518483458,
122.861931794176)) ;
#51459 = CARTESIAN_POINT('Ctrl Pts',(-18.067689740393,-16.7935627678653,122.724459360808)) ;
#51460 = CARTESIAN_POINT('Ctrl Pts',(-18.2577181334253,-16.9833999544674,
123.053617948428)) ;
#51461 = CARTESIAN_POINT('Ctrl Pts',(-17.9698306081202,-16.803410873987,122.964068373344)) ;
#51462 = CARTESIAN_POINT('Ctrl Pts',(-18.2127741605597,-16.9934601500428,
123.260266613058)) ;
#51463 = CARTESIAN_POINT('Ctrl Pts',(-17.9136507969245,-16.8134710695623,
123.2223788709)) ;
#51464 = CARTESIAN_POINT('Ctrl Pts',(-18.2047179854304,-17.0033578333542,
123.468199338141)) ;
#51465 = CARTESIAN_POINT('Ctrl Pts',(-17.9035805404894,-16.8233687528737,
123.48229577624)) ;
#51466 = CARTESIAN_POINT('Ctrl Pts',(-18.232302562789,-17.0132888737282,123.675146887286)) ;
#51467 = CARTESIAN_POINT('Ctrl Pts',(-17.9380616313287,-16.8332997932477,
123.740980891387)) ;
#51468 = CARTESIAN_POINT('Ctrl Pts',(-18.2963248753717,-17.0233310913848,
123.876321281435)) ;
#51469 = CARTESIAN_POINT('Ctrl Pts',(-18.0180896344632,-16.8433420109043,
123.992448629491)) ;
#51470 = CARTESIAN_POINT('Ctrl Pts',(-18.3926605695863,-17.0332177521188,
124.06050712681)) ;
#51471 = CARTESIAN_POINT('Ctrl Pts',(-18.1385099719493,-16.8532286716383,
124.222681786436)) ;
#51472 = CARTESIAN_POINT('Ctrl Pts',(-18.5205878645769,-17.0432108607212,
124.227139826993)) ;
#51473 = CARTESIAN_POINT('Ctrl Pts',(-18.2984195186076,-16.8632217802408,
124.43097259029)) ;
#51474 = CARTESIAN_POINT('Ctrl Pts',(-18.674831224359,-17.0531565593595,124.368304779055)) ;
#51475 = CARTESIAN_POINT('Ctrl Pts',(-18.4912243939608,-16.873167478879,124.607428923853)) ;
#51476 = CARTESIAN_POINT('Ctrl Pts',(-18.8510481817693,-17.0631037816305,
124.480927513138)) ;
#51477 = CARTESIAN_POINT('Ctrl Pts',(-18.7114963547142,-16.8831147011501,
124.74820721351)) ;
#51478 = CARTESIAN_POINT('Ctrl Pts',(-19.0461761282001,-17.0731518072107,
124.561829669415)) ;
#51479 = CARTESIAN_POINT('Ctrl Pts',(-18.9554062189033,-16.8931627267302,
124.849334420093)) ;
#51480 = CARTESIAN_POINT('Ctrl Pts',(-19.2482340808857,-17.0829990543536,
124.606880354677)) ;
#51481 = CARTESIAN_POINT('Ctrl Pts',(-19.2079801341209,-16.9030099738731,
124.905647600131)) ;
#51482 = CARTESIAN_POINT('Ctrl Pts',(-19.4574454956206,-17.0929622314443,
124.616933495659)) ;
#51483 = CARTESIAN_POINT('Ctrl Pts',(-19.4694948938914,-16.9129731509638,
124.918213293197)) ;
#51484 = CARTESIAN_POINT('Ctrl Pts',(-19.6665745901204,-17.1029919524777,
124.590015336654)) ;
#51485 = CARTESIAN_POINT('Ctrl Pts',(-19.7309060814968,-16.9230028719973,
124.88456498197)) ;
#51486 = CARTESIAN_POINT('Ctrl Pts',(-19.8654350785867,-17.1128964200106,
124.528216237133)) ;
#51487 = CARTESIAN_POINT('Ctrl Pts',(-19.979482337591,-16.9329073395301,124.807315147101)) ;
#51488 = CARTESIAN_POINT('Ctrl Pts',(-20.0527821290814,-17.1229209058404,
124.431754757046)) ;
#51489 = CARTESIAN_POINT('Ctrl Pts',(-20.2136657522635,-16.9429318253599,
124.686737651533)) ;
#51490 = CARTESIAN_POINT('Ctrl Pts',(-20.2186621175981,-17.1328247409643,
124.305869214479)) ;
#51491 = CARTESIAN_POINT('Ctrl Pts',(-20.4210159640352,-16.9528356604838,
124.529379524933)) ;
#51492 = CARTESIAN_POINT('Ctrl Pts',(-20.362268269371,-17.1428759316743,124.150890987089)) ;
#51493 = CARTESIAN_POINT('Ctrl Pts',(-20.60052287167,-16.9628868511938,124.335656355053)) ;
#51494 = CARTESIAN_POINT('Ctrl Pts',(-20.4749404633162,-17.1527603743326,
123.976262382427)) ;
#51495 = CARTESIAN_POINT('Ctrl Pts',(-20.7413629700132,-16.9727712938521,
124.117369250374)) ;
#51496 = CARTESIAN_POINT('Ctrl Pts',(-20.5568101272468,-17.1627533821844,
123.782806970068)) ;
#51497 = CARTESIAN_POINT('Ctrl Pts',(-20.8436992078529,-16.982764301704,123.875549411277)) ;
#51498 = CARTESIAN_POINT('Ctrl Pts',(-20.6035732599445,-17.1727017019007,
123.578943176126)) ;
#51499 = CARTESIAN_POINT('Ctrl Pts',(-20.9021522989073,-16.9927126214203,
123.620718922307)) ;
#51500 = CARTESIAN_POINT('Ctrl Pts',(-20.6145132332225,-17.1826385406102,
123.370344649638)) ;
#51501 = CARTESIAN_POINT('Ctrl Pts',(-20.9158262171433,-17.0026494601297,
123.35997007018)) ;
#51502 = CARTESIAN_POINT('Ctrl Pts',(-20.589206594443,-17.1926215295298,123.16197490794)) ;
#51503 = CARTESIAN_POINT('Ctrl Pts',(-20.8841917167147,-17.0126324490493,
123.099507780355)) ;
#51504 = CARTESIAN_POINT('Ctrl Pts',(-20.5273748243571,-17.2026654088939,
122.960102497268)) ;
#51505 = CARTESIAN_POINT('Ctrl Pts',(-20.8069010686547,-17.0226763284134,
122.847167752317)) ;
#51506 = CARTESIAN_POINT('Ctrl Pts',(-20.4339045567548,-17.2124934742523,
122.775800529378)) ;
#51507 = CARTESIAN_POINT('Ctrl Pts',(-20.6900614938181,-17.0325043937718,
122.616789554191)) ;
#51508 = CARTESIAN_POINT('Ctrl Pts',(-20.3068302236449,-17.2225705628072,
122.606349678098)) ;
#51509 = CARTESIAN_POINT('Ctrl Pts',(-20.5312178371621,-17.0425814823267,
122.404977089916)) ;
#51510 = CARTESIAN_POINT('Ctrl Pts',(-20.1557656867094,-17.2324207149635,
122.464630719431)) ;
#51511 = CARTESIAN_POINT('Ctrl Pts',(-20.3423853677775,-17.052431634483,122.227828485067)) ;
#51512 = CARTESIAN_POINT('Ctrl Pts',(-19.9784714409174,-17.2425011954158,
122.348631483285)) ;
#51513 = CARTESIAN_POINT('Ctrl Pts',(-20.1207672097145,-17.0625121149354,
122.082830799731)) ;
#51514 = CARTESIAN_POINT('Ctrl Pts',(-19.7888488448021,-17.2523156931847,
122.267175683269)) ;
#51515 = CARTESIAN_POINT('Ctrl Pts',(-19.883737034809,-17.0723266127042,121.98101173803)) ;
#51516 = CARTESIAN_POINT('Ctrl Pts',(-19.582938898268,-17.2623839892048,122.218356656156)) ;
#51517 = CARTESIAN_POINT('Ctrl Pts',(-19.6263495978875,-17.0823949087243,
121.919989507208)) ;
#51518 = CARTESIAN_POINT('Ctrl Pts',(-19.3751318674818,-17.2722828216876,
122.206291542029)) ;
#51519 = CARTESIAN_POINT('Ctrl Pts',(-19.3665898868727,-17.0922937412071,
121.904909547214)) ;
#51520 = CARTESIAN_POINT('Ctrl Pts',(-19.1652559904925,-17.2823357017021,
122.230785552897)) ;
#51521 = CARTESIAN_POINT('Ctrl Pts',(-19.1042454568957,-17.1023466212216,
121.93552853605)) ;
#51522 = CARTESIAN_POINT('Ctrl Pts',(-18.9663707089697,-17.2922055171983,
122.29008319877)) ;
#51523 = CARTESIAN_POINT('Ctrl Pts',(-18.8556383074436,-17.1122164367178,
122.009652399114)) ;
#51524 = CARTESIAN_POINT('Ctrl Pts',(-18.7770326931717,-17.3022781982811,
122.384835344758)) ;
#51525 = CARTESIAN_POINT('Ctrl Pts',(-18.6189668204918,-17.1222891178006,
122.128093849574)) ;
#51526 = CARTESIAN_POINT('Ctrl Pts',(-18.6109839358936,-17.312110676852,122.507981598294)) ;
#51527 = CARTESIAN_POINT('Ctrl Pts',(-18.4114058095582,-17.1321215963716,
122.28202873535)) ;
#51528 = CARTESIAN_POINT('Ctrl Pts',(-18.4655538333765,-17.3221413108381,
122.660674634817)) ;
#51529 = CARTESIAN_POINT('Ctrl Pts',(-18.2296195607227,-17.1421522303577,
122.472896223297)) ;
#51530 = CARTESIAN_POINT('Ctrl Pts',(-18.349337760532,-17.3321728680573,122.83667359108)) ;
#51531 = CARTESIAN_POINT('Ctrl Pts',(-18.0843508672524,-17.1521837875768,
122.692895741802)) ;
#51532 = CARTESIAN_POINT('Ctrl Pts',(-18.2667484940145,-17.342002576929,123.026088129245)) ;
#51533 = CARTESIAN_POINT('Ctrl Pts',(-17.9811153910442,-17.1620134964485,
122.929665784977)) ;
#51534 = CARTESIAN_POINT('Ctrl Pts',(-18.2169009601804,-17.3519920257311,
123.230102550982)) ;
#51535 = CARTESIAN_POINT('Ctrl Pts',(-17.9188078332525,-17.1720029452506,
123.184684449005)) ;
#51536 = CARTESIAN_POINT('Ctrl Pts',(-18.20369487068,-17.3620358781311,123.440840534949)) ;
#51537 = CARTESIAN_POINT('Ctrl Pts',(-17.9023020183694,-17.1820467976506,
123.448106892895)) ;
#51538 = CARTESIAN_POINT('Ctrl Pts',(-18.2263343781215,-17.3718575914632,
123.646078297448)) ;
#51539 = CARTESIAN_POINT('Ctrl Pts',(-17.9306034520585,-17.1918685109827,
123.70465512796)) ;
#51540 = CARTESIAN_POINT('Ctrl Pts',(-18.2850268408009,-17.3818925964519,
123.848716320605)) ;
#51541 = CARTESIAN_POINT('Ctrl Pts',(-18.0039709950905,-17.2019035159714,
123.957951977025)) ;
#51542 = CARTESIAN_POINT('Ctrl Pts',(-18.3784463059481,-17.3919174348995,
124.037642069545)) ;
#51543 = CARTESIAN_POINT('Ctrl Pts',(-18.1207470221514,-17.211928354419,124.194108297335)) ;
#51544 = CARTESIAN_POINT('Ctrl Pts',(-18.5007395484921,-17.4017696478547,
124.204809326343)) ;
#51545 = CARTESIAN_POINT('Ctrl Pts',(-18.2736158123272,-17.2217805673742,
124.40306698236)) ;
#51546 = CARTESIAN_POINT('Ctrl Pts',(-18.6520320192726,-17.4117596040485,
124.350454005425)) ;
#51547 = CARTESIAN_POINT('Ctrl Pts',(-18.4627330155444,-17.231770523568,124.58512141866)) ;
#51548 = CARTESIAN_POINT('Ctrl Pts',(-18.8252452575916,-17.4216877143317,
124.466918774105)) ;
#51549 = CARTESIAN_POINT('Ctrl Pts',(-18.6792511906033,-17.2416986338513,
124.730700896827)) ;
#51550 = CARTESIAN_POINT('Ctrl Pts',(-19.0170751012007,-17.4316763144113,
124.552359737803)) ;
#51551 = CARTESIAN_POINT('Ctrl Pts',(-18.9190395512915,-17.2516872339308,
124.837500136019)) ;
#51552 = CARTESIAN_POINT('Ctrl Pts',(-19.2216700740144,-17.4417029063388,
124.603105177326)) ;
#51553 = CARTESIAN_POINT('Ctrl Pts',(-19.1747837504834,-17.2617138258583,
124.90092984062)) ;
#51554 = CARTESIAN_POINT('Ctrl Pts',(-19.4289770875473,-17.451588034403,124.617568828443)) ;
#51555 = CARTESIAN_POINT('Ctrl Pts',(-19.4339184087877,-17.2715989539225,
124.91900725603)) ;
#51556 = CARTESIAN_POINT('Ctrl Pts',(-19.6379253432582,-17.4615791518765,
124.596058505797)) ;
#51557 = CARTESIAN_POINT('Ctrl Pts',(-19.6951036460035,-17.281590071396,124.89211702281)) ;
#51558 = CARTESIAN_POINT('Ctrl Pts',(-19.8408352338707,-17.4716197677283,
124.537884142129)) ;
#51559 = CARTESIAN_POINT('Ctrl Pts',(-19.948740310109,-17.2916306872478,124.819396963056)) ;
#51560 = CARTESIAN_POINT('Ctrl Pts',(-20.0267858411353,-17.481452758582,124.447583261545)) ;
#51561 = CARTESIAN_POINT('Ctrl Pts',(-20.1811784263094,-17.3014636781015,
124.706518373557)) ;
#51562 = CARTESIAN_POINT('Ctrl Pts',(-20.1973125975978,-17.4914458900323,
124.324881213278)) ;
#51563 = CARTESIAN_POINT('Ctrl Pts',(-20.3943355472786,-17.3114568095518,
124.55313875721)) ;
#51564 = CARTESIAN_POINT('Ctrl Pts',(-20.3442096502401,-17.5014779384677,
124.173532276575)) ;
#51565 = CARTESIAN_POINT('Ctrl Pts',(-20.5779551584514,-17.3214888579872,
124.363950983944)) ;
#51566 = CARTESIAN_POINT('Ctrl Pts',(-20.460827682046,-17.5113431850101,124.002039230905)) ;
#51567 = CARTESIAN_POINT('Ctrl Pts',(-20.7237261255781,-17.3313541045296,
124.1495827215)) ;
#51568 = CARTESIAN_POINT('Ctrl Pts',(-20.5472792275311,-17.5213050598369,
123.811278450178)) ;
#51569 = CARTESIAN_POINT('Ctrl Pts',(-20.8317883622719,-17.3413159793564,
123.911130472961)) ;
#51570 = CARTESIAN_POINT('Ctrl Pts',(-20.5993376398069,-17.5313400229482,
123.606847846578)) ;
#51571 = CARTESIAN_POINT('Ctrl Pts',(-20.8968589919692,-17.3513509424677,
123.655591647141)) ;
#51572 = CARTESIAN_POINT('Ctrl Pts',(-20.615228249655,-17.5412248674106,123.399615410114)) ;
#51573 = CARTESIAN_POINT('Ctrl Pts',(-20.9167197831636,-17.3612357869301,
123.396550342784)) ;
#51574 = CARTESIAN_POINT('Ctrl Pts',(-20.5944747720619,-17.5512909202513,
123.189052375223)) ;
#51575 = CARTESIAN_POINT('Ctrl Pts',(-20.8907754478071,-17.3713018397708,
123.133346946197)) ;
#51576 = CARTESIAN_POINT('Ctrl Pts',(-20.5389734302153,-17.5611284361603,
122.989783502597)) ;
#51577 = CARTESIAN_POINT('Ctrl Pts',(-20.8213961194626,-17.3811393556798,
122.884260853011)) ;
#51578 = CARTESIAN_POINT('Ctrl Pts',(-20.4478531306755,-17.5711971842692,
122.798763312751)) ;
#51579 = CARTESIAN_POINT('Ctrl Pts',(-20.7074934612371,-17.3912081037887,
122.645486865845)) ;
#51580 = CARTESIAN_POINT('Ctrl Pts',(-20.3271452161414,-17.5810777013002,
122.629676892913)) ;
#51581 = CARTESIAN_POINT('Ctrl Pts',(-20.556606167494,-17.4010886208197,122.434129920155)) ;
#51582 = CARTESIAN_POINT('Ctrl Pts',(-20.1775948897127,-17.5910688882346,
122.482227937037)) ;
#51583 = CARTESIAN_POINT('Ctrl Pts',(-20.3696663137793,-17.4110798077542,
122.2498205318)) ;
#51584 = CARTESIAN_POINT('Ctrl Pts',(-20.0053412492469,-17.6010219545096,
122.363377773261)) ;
#51585 = CARTESIAN_POINT('Ctrl Pts',(-20.1543475644743,-17.4210328740291,
122.101259878652)) ;
#51586 = CARTESIAN_POINT('Ctrl Pts',(-19.8135014291807,-17.6110577920422,
122.275600289609)) ;
#51587 = CARTESIAN_POINT('Ctrl Pts',(-19.9145466996496,-17.4310687115617,
121.991540433596)) ;
#51588 = CARTESIAN_POINT('Ctrl Pts',(-19.6123051874755,-17.6209479182536,
122.223092310276)) ;
#51589 = CARTESIAN_POINT('Ctrl Pts',(-19.6630503154373,-17.4409588377731,
121.925907930471)) ;
#51590 = CARTESIAN_POINT('Ctrl Pts',(-19.4029610311012,-17.6309401001616,
122.205808818066)) ;
#51591 = CARTESIAN_POINT('Ctrl Pts',(-19.4013697921705,-17.4509510196811,
121.904306259189)) ;
#51592 = CARTESIAN_POINT('Ctrl Pts',(-19.1947594778902,-17.6408860401002,
122.225118763395)) ;
#51593 = CARTESIAN_POINT('Ctrl Pts',(-19.1411178680451,-17.4608969596197,
121.928446401683)) ;
#51594 = CARTESIAN_POINT('Ctrl Pts',(-18.9929258923836,-17.6508332238642,
122.279886430677)) ;
#51595 = CARTESIAN_POINT('Ctrl Pts',(-18.888826411622,-17.4708441433838,121.99690869262)) ;
#51596 = CARTESIAN_POINT('Ctrl Pts',(-18.8018677982958,-17.6608811621717,
122.369974731862)) ;
#51597 = CARTESIAN_POINT('Ctrl Pts',(-18.6500049663537,-17.4808920816912,
122.109521528189)) ;
#51598 = CARTESIAN_POINT('Ctrl Pts',(-18.6326849760237,-17.670728796912,122.489300515306)) ;
#51599 = CARTESIAN_POINT('Ctrl Pts',(-18.4385276906649,-17.4907397164315,
122.258681232071)) ;
#51600 = CARTESIAN_POINT('Ctrl Pts',(-18.48464394166,-17.6806905108858,122.637419729703)) ;
#51601 = CARTESIAN_POINT('Ctrl Pts',(-18.2534782915333,-17.5007014304053,
122.443832320165)) ;
#51602 = CARTESIAN_POINT('Ctrl Pts',(-18.3639692527773,-17.6907191456766,
122.810318421013)) ;
#51603 = CARTESIAN_POINT('Ctrl Pts',(-18.1026371826534,-17.5107300651962,
122.659957308343)) ;
#51604 = CARTESIAN_POINT('Ctrl Pts',(-18.2761446006497,-17.7006294642738,
122.999238769557)) ;
#51605 = CARTESIAN_POINT('Ctrl Pts',(-17.9928588041681,-17.5206403837933,
122.896109111931)) ;
#51606 = CARTESIAN_POINT('Ctrl Pts',(-18.2217890454544,-17.7105643205853,
123.200911892758)) ;
#51607 = CARTESIAN_POINT('Ctrl Pts',(-17.9249170446057,-17.5305752401048,
123.148201377883)) ;
#51608 = CARTESIAN_POINT('Ctrl Pts',(-18.2032822313656,-17.720605556546,123.411187682898)) ;
#51609 = CARTESIAN_POINT('Ctrl Pts',(-17.9017863179622,-17.5406164760655,
123.411046406639)) ;
#51610 = CARTESIAN_POINT('Ctrl Pts',(-18.2211170108079,-17.730492328126,123.618292553974)) ;
#51611 = CARTESIAN_POINT('Ctrl Pts',(-17.9240826083119,-17.5505032476455,
123.66992741687)) ;
#51612 = CARTESIAN_POINT('Ctrl Pts',(-18.2749965572381,-17.7404925068322,
123.821474487423)) ;
#51613 = CARTESIAN_POINT('Ctrl Pts',(-17.9914347891507,-17.5605034263517,
123.923904178052)) ;
#51614 = CARTESIAN_POINT('Ctrl Pts',(-18.36246816189,-17.7504097850418,124.010768806246)) ;
#51615 = CARTESIAN_POINT('Ctrl Pts',(-18.1007768931829,-17.5704207045613,
124.16052097631)) ;
#51616 = CARTESIAN_POINT('Ctrl Pts',(-18.48305480673,-17.7604570314554,124.184154003306)) ;
#51617 = CARTESIAN_POINT('Ctrl Pts',(-18.2515125584344,-17.580467950975,124.377250917439)) ;
#51618 = CARTESIAN_POINT('Ctrl Pts',(-18.629232331941,-17.7703309204367,124.331582621373)) ;
#51619 = CARTESIAN_POINT('Ctrl Pts',(-18.4342365121,-17.5903418399563,124.561534748493)) ;
#51620 = CARTESIAN_POINT('Ctrl Pts',(-18.8019032378778,-17.7803929380173,
124.453733894309)) ;
#51621 = CARTESIAN_POINT('Ctrl Pts',(-18.650076844081,-17.6004038575368,124.714221581174)) ;
#51622 = CARTESIAN_POINT('Ctrl Pts',(-18.9895800757917,-17.7902639997516,
124.542325237439)) ;
#51623 = CARTESIAN_POINT('Ctrl Pts',(-18.8846741124634,-17.6102749192711,
124.824958215824)) ;
#51624 = CARTESIAN_POINT('Ctrl Pts',(-19.1921134940513,-17.8002580631119,
124.598226493753)) ;
#51625 = CARTESIAN_POINT('Ctrl Pts',(-19.1378416764375,-17.6202689826314,
124.894832090757)) ;
#51626 = CARTESIAN_POINT('Ctrl Pts',(-19.4021121856622,-17.8102902211453,
124.617721341239)) ;
#51627 = CARTESIAN_POINT('Ctrl Pts',(-19.4003404043866,-17.6303011406648,
124.919197850925)) ;
#51628 = CARTESIAN_POINT('Ctrl Pts',(-19.608844588004,-17.8201540973854,124.601197546684)) ;
#51629 = CARTESIAN_POINT('Ctrl Pts',(-19.6587556166783,-17.640165016905,124.898540309073)) ;
#51630 = CARTESIAN_POINT('Ctrl Pts',(-19.8137331839509,-17.8302246120237,
124.54797156307)) ;
#51631 = CARTESIAN_POINT('Ctrl Pts',(-19.9148657636733,-17.6502355315432,
124.832005118478)) ;
#51632 = CARTESIAN_POINT('Ctrl Pts',(-20.0019178911935,-17.8400652489647,
124.461988692631)) ;
#51633 = CARTESIAN_POINT('Ctrl Pts',(-20.1500954777308,-17.6600761684842,
124.72452389297)) ;
#51634 = CARTESIAN_POINT('Ctrl Pts',(-20.1748685848524,-17.8500323778049,
124.343718173055)) ;
#51635 = CARTESIAN_POINT('Ctrl Pts',(-20.3662817218057,-17.6700432973244,
124.576684082019)) ;
#51636 = CARTESIAN_POINT('Ctrl Pts',(-20.3252263227975,-17.8600463509294,
124.196347627969)) ;
#51637 = CARTESIAN_POINT('Ctrl Pts',(-20.5542290544657,-17.6800572704489,
124.392466662775)) ;
#51638 = CARTESIAN_POINT('Ctrl Pts',(-20.4877929513438,-17.8733310847927,
123.96921781494)) ;
#51639 = CARTESIAN_POINT('Ctrl Pts',(-20.7574242466932,-17.6933420043122,
124.108563216924)) ;
#51640 = CARTESIAN_POINT('Ctrl Pts',(-20.5871211093539,-17.8865563495074,
123.706157520284)) ;
#51641 = CARTESIAN_POINT('Ctrl Pts',(-20.8815792329842,-17.706567269027,123.779776387275)) ;
#51642 = CARTESIAN_POINT('Ctrl Pts',(-20.6152234023706,-17.8998668720623,
123.427758973367)) ;
#51643 = CARTESIAN_POINT('Ctrl Pts',(-20.9167156269414,-17.7198777915818,
123.431719811705)) ;
#51644 = CARTESIAN_POINT('Ctrl Pts',(-20.5994871791015,-17.9098955169645,
123.217511431126)) ;
#51645 = CARTESIAN_POINT('Ctrl Pts',(-20.8970403047877,-17.729906436484,123.168922156201)) ;
#51646 = CARTESIAN_POINT('Ctrl Pts',(-20.5484258087731,-17.9197765493184,
123.01615172322)) ;
#51647 = CARTESIAN_POINT('Ctrl Pts',(-20.8332113376201,-17.7397874688379,
122.917220164126)) ;
#51648 = CARTESIAN_POINT('Ctrl Pts',(-20.462715022261,-17.9297575219985,122.82462433537)) ;
#51649 = CARTESIAN_POINT('Ctrl Pts',(-20.7260717928648,-17.749768441518,122.677813694305)) ;
#51650 = CARTESIAN_POINT('Ctrl Pts',(-20.3449102482183,-17.9397386495845,
122.650999042694)) ;
#51651 = CARTESIAN_POINT('Ctrl Pts',(-20.5788081878734,-17.759749569104,122.460780264954)) ;
#51652 = CARTESIAN_POINT('Ctrl Pts',(-20.1513290480844,-17.9529818398459,
122.450788742147)) ;
#51653 = CARTESIAN_POINT('Ctrl Pts',(-20.3368568948601,-17.7729927593654,
122.210535455664)) ;
#51654 = CARTESIAN_POINT('Ctrl Pts',(-19.8474795977767,-17.9696498352067,
122.268601957147)) ;
#51655 = CARTESIAN_POINT('Ctrl Pts',(-19.9569936986042,-17.7896607547262,
121.982786748318)) ;
#51656 = CARTESIAN_POINT('Ctrl Pts',(-19.5025885485555,-17.9861703352187,
122.201337269194)) ;
#51657 = CARTESIAN_POINT('Ctrl Pts',(-19.5259606159794,-17.8061812547382,
121.898720901943)) ;
#51658 = CARTESIAN_POINT('Ctrl Pts',(-19.2234322226272,-17.9994833515347,
122.220261932405)) ;
#51659 = CARTESIAN_POINT('Ctrl Pts',(-19.1769501917379,-17.8194942710542,
121.922374301717)) ;
#51660 = CARTESIAN_POINT('Ctrl Pts',(-19.0209334833378,-18.0093999097677,
122.270017422137)) ;
#51661 = CARTESIAN_POINT('Ctrl Pts',(-18.9238414463317,-17.8294108292872,
121.98457134201)) ;
#51662 = CARTESIAN_POINT('Ctrl Pts',(-18.8281337131634,-18.0194275780706,
122.355152407899)) ;
#51663 = CARTESIAN_POINT('Ctrl Pts',(-18.682836795022,-17.8394384975901,122.090994480556)) ;
#51664 = CARTESIAN_POINT('Ctrl Pts',(-18.5974653025486,-18.0326081678152,
122.508905891752)) ;
#51665 = CARTESIAN_POINT('Ctrl Pts',(-18.3945158970904,-17.8526190873348,
122.283176068274)) ;
#51666 = CARTESIAN_POINT('Ctrl Pts',(-18.3626740824795,-18.0493563069346,
122.776403364024)) ;
#51667 = CARTESIAN_POINT('Ctrl Pts',(-18.1010163557202,-17.8693672264541,
122.617564692442)) ;
#51668 = CARTESIAN_POINT('Ctrl Pts',(-18.2093429381581,-18.0691510494452,
123.168585983566)) ;
#51669 = CARTESIAN_POINT('Ctrl Pts',(-17.909361184376,-17.8891619689647,123.107788785538)) ;
#51670 = CARTESIAN_POINT('Ctrl Pts',(-18.1984950373618,-18.089195442254,123.594497284543)) ;
#51671 = CARTESIAN_POINT('Ctrl Pts',(-17.8958042829193,-17.9092063617735,
123.640179567838)) ;
#51672 = CARTESIAN_POINT('Ctrl Pts',(-18.3326878160101,-18.1090346245527,
123.994538645704)) ;
#51673 = CARTESIAN_POINT('Ctrl Pts',(-18.0635490481216,-17.9290455440722,
124.140228438926)) ;
#51674 = CARTESIAN_POINT('Ctrl Pts',(-18.595526380158,-18.1289599482456,124.326686433183)) ;
#51675 = CARTESIAN_POINT('Ctrl Pts',(-18.3920994918679,-17.9489708677651,
124.555410464807)) ;
#51676 = CARTESIAN_POINT('Ctrl Pts',(-18.9560767803861,-18.1488835862971,
124.549228315396)) ;
#51677 = CARTESIAN_POINT('Ctrl Pts',(-18.842788696295,-17.9688945058166,124.833584548361)) ;
#51678 = CARTESIAN_POINT('Ctrl Pts',(-19.3708100254435,-18.1688084597626,
124.63548572576)) ;
#51679 = CARTESIAN_POINT('Ctrl Pts',(-19.361205130707,-17.9888193792821,124.941403037366)) ;
#51680 = CARTESIAN_POINT('Ctrl Pts',(-19.7892611661208,-18.1886870668415,
124.575714298968)) ;
#51681 = CARTESIAN_POINT('Ctrl Pts',(-19.8842672961857,-18.008697986361,124.866686275216)) ;
#51682 = CARTESIAN_POINT('Ctrl Pts',(-20.1641187112948,-18.2086645096735,
124.375945013966)) ;
#51683 = CARTESIAN_POINT('Ctrl Pts',(-20.3528378764047,-18.028675429193,124.616972672933)) ;
#51684 = CARTESIAN_POINT('Ctrl Pts',(-20.4474662277744,-18.2285963577582,
124.06073373373)) ;
#51685 = CARTESIAN_POINT('Ctrl Pts',(-20.7070199753462,-18.0486072772777,
124.222957551493)) ;
#51686 = CARTESIAN_POINT('Ctrl Pts',(-20.6063082660546,-18.2484916261008,
123.668688283209)) ;
#51687 = CARTESIAN_POINT('Ctrl Pts',(-20.905570212033,-18.0685025456203,123.7329012805)) ;
#51688 = CARTESIAN_POINT('Ctrl Pts',(-20.6223259515978,-18.2684141245129,
123.245374252905)) ;
#51689 = CARTESIAN_POINT('Ctrl Pts',(-20.9255908590547,-18.0884250440324,
123.203759760779)) ;
#51690 = CARTESIAN_POINT('Ctrl Pts',(-20.4925770960382,-18.2883736063889,
122.841276292266)) ;
#51691 = CARTESIAN_POINT('Ctrl Pts',(-20.7634037512627,-18.1083845259084,
122.698638234427)) ;
#51692 = CARTESIAN_POINT('Ctrl Pts',(-20.2338987435689,-18.3082513588482,
122.507109401429)) ;
#51693 = CARTESIAN_POINT('Ctrl Pts',(-20.4400561874545,-18.1282622783678,
122.280931726581)) ;
#51694 = CARTESIAN_POINT('Ctrl Pts',(-19.8771610118705,-18.3281331495828,
122.280132547987)) ;
#51695 = CARTESIAN_POINT('Ctrl Pts',(-19.9941357018043,-18.1481440691023,
121.997211525519)) ;
#51696 = CARTESIAN_POINT('Ctrl Pts',(-19.4603627437856,-18.3482064884338,
122.188495687106)) ;
#51697 = CARTESIAN_POINT('Ctrl Pts',(-19.4731366764473,-18.1682174079533,
121.882665391042)) ;
#51698 = CARTESIAN_POINT('Ctrl Pts',(-19.0428183765593,-18.3680109556696,
122.243747752997)) ;
#51699 = CARTESIAN_POINT('Ctrl Pts',(-18.9512092801426,-18.1880218751891,
121.951729931177)) ;
#51700 = CARTESIAN_POINT('Ctrl Pts',(-18.6655136826897,-18.3879942960774,
122.439019897287)) ;
#51701 = CARTESIAN_POINT('Ctrl Pts',(-18.4795781027084,-18.2080052155969,
122.195819043092)) ;
#51702 = CARTESIAN_POINT('Ctrl Pts',(-18.3789384655421,-18.4079092606754,
122.750760297529)) ;
#51703 = CARTESIAN_POINT('Ctrl Pts',(-18.1213593077318,-18.2279201801949,
122.585493056673)) ;
#51704 = CARTESIAN_POINT('Ctrl Pts',(-18.2152038691917,-18.4277777953917,
123.140286780608)) ;
#51705 = CARTESIAN_POINT('Ctrl Pts',(-17.9166900269877,-18.2477887149113,
123.072398846917)) ;
#51706 = CARTESIAN_POINT('Ctrl Pts',(-18.1947300807791,-18.4478301796035,
123.566037893384)) ;
#51707 = CARTESIAN_POINT('Ctrl Pts',(-17.8910961294277,-18.267841099123,123.60458827601)) ;
#51708 = CARTESIAN_POINT('Ctrl Pts',(-18.3185671471098,-18.4676041433927,
123.96801283456)) ;
#51709 = CARTESIAN_POINT('Ctrl Pts',(-18.0458895720213,-18.2876150629122,
124.10705494621)) ;
#51710 = CARTESIAN_POINT('Ctrl Pts',(-18.5752678737993,-18.487658522414,124.308284568343)) ;
#51711 = CARTESIAN_POINT('Ctrl Pts',(-18.3667637787216,-18.3076694419336,
124.532396665767)) ;
#51712 = CARTESIAN_POINT('Ctrl Pts',(-18.9284212326359,-18.5074552599873,
124.537569903936)) ;
#51713 = CARTESIAN_POINT('Ctrl Pts',(-18.8082021317787,-18.3274661795068,
124.819004328928)) ;
#51714 = CARTESIAN_POINT('Ctrl Pts',(-19.3416803678244,-18.5274230723387,
124.634498823647)) ;
#51715 = CARTESIAN_POINT('Ctrl Pts',(-19.3247749684636,-18.3474339918583,
124.940168786696)) ;
#51716 = CARTESIAN_POINT('Ctrl Pts',(-19.7631205986786,-18.5473820484038,
124.583927911147)) ;
#51717 = CARTESIAN_POINT('Ctrl Pts',(-19.8515753100361,-18.3673929679233,
124.876958419638)) ;
#51718 = CARTESIAN_POINT('Ctrl Pts',(-20.1408243512989,-18.5672769666812,
124.393475715096)) ;
#51719 = CARTESIAN_POINT('Ctrl Pts',(-20.3237057376105,-18.3872878862007,
124.638896796487)) ;
#51720 = CARTESIAN_POINT('Ctrl Pts',(-20.4312496937618,-18.5871732791315,
124.085918903188)) ;
#51721 = CARTESIAN_POINT('Ctrl Pts',(-20.6867396806704,-18.407184198651,124.254454113061)) ;
#51722 = CARTESIAN_POINT('Ctrl Pts',(-20.5998462621265,-18.6070812125056,
123.69761409053)) ;
#51723 = CARTESIAN_POINT('Ctrl Pts',(-20.8974889911539,-18.4270921320251,
123.769075405474)) ;
#51724 = CARTESIAN_POINT('Ctrl Pts',(-20.6258188714983,-18.6270311027941,
123.274258003805)) ;
#51725 = CARTESIAN_POINT('Ctrl Pts',(-20.9299591276609,-18.4470420223136,
123.239880881314)) ;
#51726 = CARTESIAN_POINT('Ctrl Pts',(-20.5065921902261,-18.6469083332954,
122.868736889825)) ;
#51727 = CARTESIAN_POINT('Ctrl Pts',(-20.7809301920066,-18.4669192528149,
122.732978965298)) ;
#51728 = CARTESIAN_POINT('Ctrl Pts',(-20.2550219026943,-18.6668910021664,
122.526359546569)) ;
#51729 = CARTESIAN_POINT('Ctrl Pts',(-20.4664719536268,-18.4869019216859,
122.305004321763)) ;
#51730 = CARTESIAN_POINT('Ctrl Pts',(-19.9023778798508,-18.6868238887468,
122.291166846904)) ;
#51731 = CARTESIAN_POINT('Ctrl Pts',(-20.0256670326926,-18.5068348082663,
122.011010323903)) ;
#51732 = CARTESIAN_POINT('Ctrl Pts',(-19.4912013862512,-18.7067366347647,
122.190280264544)) ;
#51733 = CARTESIAN_POINT('Ctrl Pts',(-19.5117084694542,-18.5267475542842,
121.884894904074)) ;
#51734 = CARTESIAN_POINT('Ctrl Pts',(-19.1409101901299,-18.7233063561065,
122.227714641459)) ;
#51735 = CARTESIAN_POINT('Ctrl Pts',(-19.0738118335659,-18.543317275626,121.931691304887)) ;
#51736 = CARTESIAN_POINT('Ctrl Pts',(-18.8799531775115,-18.7366063674115,
122.328226065219)) ;
#51737 = CARTESIAN_POINT('Ctrl Pts',(-18.7476501459494,-18.556617286931,122.057314468729)) ;
#51738 = CARTESIAN_POINT('Ctrl Pts',(-18.6408115625997,-18.7498765551614,
122.471815662188)) ;
#51739 = CARTESIAN_POINT('Ctrl Pts',(-18.448665698478,-18.5698874746809,122.236842368626)) ;
#51740 = CARTESIAN_POINT('Ctrl Pts',(-18.3949285657691,-18.7665039375268,
122.725952569314)) ;
#51741 = CARTESIAN_POINT('Ctrl Pts',(-18.141372227169,-18.5865148570463,122.554451894984)) ;
#51742 = CARTESIAN_POINT('Ctrl Pts',(-18.2507607995782,-18.783126227272,123.048601698657)) ;
#51743 = CARTESIAN_POINT('Ctrl Pts',(-17.9611265354326,-18.6031371467915,
122.957810899803)) ;
#51744 = CARTESIAN_POINT('Ctrl Pts',(-18.2066124842382,-18.7963714416665,
123.323560231487)) ;
#51745 = CARTESIAN_POINT('Ctrl Pts',(-17.9059528959397,-18.616382361186,123.301475150394)) ;
#51746 = CARTESIAN_POINT('Ctrl Pts',(-18.2091963113951,-18.8062834066272,
123.531933666297)) ;
#51747 = CARTESIAN_POINT('Ctrl Pts',(-17.9091768532067,-18.6262943261467,
123.561948497641)) ;
#51748 = CARTESIAN_POINT('Ctrl Pts',(-18.2487269856474,-18.8163420297916,
123.739647393853)) ;
#51749 = CARTESIAN_POINT('Ctrl Pts',(-17.9585883653442,-18.6363529493112,
123.821589557163)) ;
#51750 = CARTESIAN_POINT('Ctrl Pts',(-18.3218273859011,-18.8261821439075,
123.933204366604)) ;
#51751 = CARTESIAN_POINT('Ctrl Pts',(-18.0499609715988,-18.646193063427,124.063536985095)) ;
#51752 = CARTESIAN_POINT('Ctrl Pts',(-18.4296324438484,-18.8362479288651,
124.115263613763)) ;
#51753 = CARTESIAN_POINT('Ctrl Pts',(-18.1847150491307,-18.6562588483846,
124.291112489709)) ;
#51754 = CARTESIAN_POINT('Ctrl Pts',(-18.5650197569021,-18.846131246653,124.27291340767)) ;
#51755 = CARTESIAN_POINT('Ctrl Pts',(-18.3539469881779,-18.6661421661725,
124.488176476417)) ;
#51756 = CARTESIAN_POINT('Ctrl Pts',(-18.7271216090986,-18.8561206845115,
124.40639870705)) ;
#51757 = CARTESIAN_POINT('Ctrl Pts',(-18.5565725703095,-18.6761316040311,
124.65503529775)) ;
#51758 = CARTESIAN_POINT('Ctrl Pts',(-18.9095316281554,-18.8660843985643,
124.509393822221)) ;
#51759 = CARTESIAN_POINT('Ctrl Pts',(-18.7845837389449,-18.6860953180838,
124.783781642448)) ;
#51760 = CARTESIAN_POINT('Ctrl Pts',(-19.1076061689565,-18.8760794102235,
124.579581320828)) ;
#51761 = CARTESIAN_POINT('Ctrl Pts',(-19.0321760408192,-18.696090329743,124.871518685456)) ;
#51762 = CARTESIAN_POINT('Ctrl Pts',(-19.3157436958266,-18.8861157019177,
124.61412399333)) ;
#51763 = CARTESIAN_POINT('Ctrl Pts',(-19.2923475774005,-18.7061266214373,
124.91469979869)) ;
#51764 = CARTESIAN_POINT('Ctrl Pts',(-19.5227505678203,-18.8959620796112,
124.612380202904)) ;
#51765 = CARTESIAN_POINT('Ctrl Pts',(-19.5511061455556,-18.7159729991307,
124.912522869944)) ;
#51766 = CARTESIAN_POINT('Ctrl Pts',(-19.7292055330348,-18.9059470237619,
124.57459229136)) ;
#51767 = CARTESIAN_POINT('Ctrl Pts',(-19.8091754394727,-18.7259579432814,
124.865290742925)) ;
#51768 = CARTESIAN_POINT('Ctrl Pts',(-19.9251198106704,-18.9158839948918,
124.501974601842)) ;
#51769 = CARTESIAN_POINT('Ctrl Pts',(-20.0540693303344,-18.7358949144114,
124.774521245491)) ;
#51770 = CARTESIAN_POINT('Ctrl Pts',(-20.1073932158431,-18.9259337795236,
124.395175327921)) ;
#51771 = CARTESIAN_POINT('Ctrl Pts',(-20.2819125650072,-18.7459446990431,
124.64102455538)) ;
#51772 = CARTESIAN_POINT('Ctrl Pts',(-20.2652907922645,-18.9357842416011,
124.261160532584)) ;
#51773 = CARTESIAN_POINT('Ctrl Pts',(-20.4792864443041,-18.7557951611206,
124.473508135984)) ;
#51774 = CARTESIAN_POINT('Ctrl Pts',(-20.3995458132042,-18.9457562551215,
124.100179995345)) ;
#51775 = CARTESIAN_POINT('Ctrl Pts',(-20.6471074505212,-18.765767174641,124.272284173965)) ;
#51776 = CARTESIAN_POINT('Ctrl Pts',(-20.5040579564351,-18.9557514022409,
123.91784560784)) ;
#51777 = CARTESIAN_POINT('Ctrl Pts',(-20.7777500988216,-18.7757623217604,
124.044367513439)) ;
#51778 = CARTESIAN_POINT('Ctrl Pts',(-20.5753422248365,-18.965785371977,123.71932854599)) ;
#51779 = CARTESIAN_POINT('Ctrl Pts',(-20.8668580983504,-18.7857962914965,
123.796222100984)) ;
#51780 = CARTESIAN_POINT('Ctrl Pts',(-20.6107665468007,-18.9756409176476,
123.515165091888)) ;
#51781 = CARTESIAN_POINT('Ctrl Pts',(-20.9111412972564,-18.7956518371671,
123.541018035031)) ;
#51782 = CARTESIAN_POINT('Ctrl Pts',(-20.6104909571507,-18.9856396746608,
123.304993816628)) ;
#51783 = CARTESIAN_POINT('Ctrl Pts',(-20.9107995973893,-18.8056505941803,
123.278303845402)) ;
#51784 = CARTESIAN_POINT('Ctrl Pts',(-20.5742854817518,-18.995536809898,123.100067497722)) ;
#51785 = CARTESIAN_POINT('Ctrl Pts',(-20.8655454313835,-18.8155477294175,
123.022145216634)) ;
#51786 = CARTESIAN_POINT('Ctrl Pts',(-20.5019793355474,-19.0055899057376,
122.901496245715)) ;
#51787 = CARTESIAN_POINT('Ctrl Pts',(-20.7751653504057,-18.8256008252571,
122.773930212784)) ;
#51788 = CARTESIAN_POINT('Ctrl Pts',(-20.3980758274042,-19.0154734144682,
122.721542018855)) ;
#51789 = CARTESIAN_POINT('Ctrl Pts',(-20.6452882014999,-18.8354843339877,
122.548985779827)) ;
#51790 = CARTESIAN_POINT('Ctrl Pts',(-20.2633899531571,-19.0254682871143,
122.560268873648)) ;
#51791 = CARTESIAN_POINT('Ctrl Pts',(-20.4769328740491,-18.8454792066338,
122.347392525838)) ;
#51792 = CARTESIAN_POINT('Ctrl Pts',(-20.1021192146536,-19.03548824875,122.424730589061)) ;
#51793 = CARTESIAN_POINT('Ctrl Pts',(-20.2753461931857,-18.8554991682695,
122.177967546713)) ;
#51794 = CARTESIAN_POINT('Ctrl Pts',(-19.9219503779301,-19.0453936125498,
122.320315131971)) ;
#51795 = CARTESIAN_POINT('Ctrl Pts',(-20.0501362496351,-18.8654045320694,
122.047445707067)) ;
#51796 = CARTESIAN_POINT('Ctrl Pts',(-19.725850127901,-19.0553342001574,122.248117440437)) ;
#51797 = CARTESIAN_POINT('Ctrl Pts',(-19.8050116122728,-18.8753451196769,
121.957195984655)) ;
#51798 = CARTESIAN_POINT('Ctrl Pts',(-19.5188889597631,-19.065337018258,122.21070880174)) ;
#51799 = CARTESIAN_POINT('Ctrl Pts',(-19.5463105434704,-18.8853479377776,
121.910432554747)) ;
#51800 = CARTESIAN_POINT('Ctrl Pts',(-19.3079401318783,-19.0753717299822,
122.210144775601)) ;
#51801 = CARTESIAN_POINT('Ctrl Pts',(-19.2826245313251,-18.8953826495017,
121.909724812158)) ;
#51802 = CARTESIAN_POINT('Ctrl Pts',(-19.1039450954541,-19.0852166367195,
122.245193265837)) ;
#51803 = CARTESIAN_POINT('Ctrl Pts',(-19.0276297317247,-18.905227556239,121.953532899753)) ;
#51804 = CARTESIAN_POINT('Ctrl Pts',(-18.9062559735361,-19.0952024892885,
122.315743265558)) ;
#51805 = CARTESIAN_POINT('Ctrl Pts',(-18.7805173028512,-18.915213408808,122.041718001844)) ;
#51806 = CARTESIAN_POINT('Ctrl Pts',(-18.7246158514163,-19.1051372977015,
122.418922406294)) ;
#51807 = CARTESIAN_POINT('Ctrl Pts',(-18.5534655976268,-18.9251482172211,
122.170689853472)) ;
#51808 = CARTESIAN_POINT('Ctrl Pts',(-18.5618355249981,-19.1151948247826,
122.553818901335)) ;
#51809 = CARTESIAN_POINT('Ctrl Pts',(-18.3499886136617,-18.9352057443021,
122.339308389629)) ;
#51810 = CARTESIAN_POINT('Ctrl Pts',(-18.4278858922511,-19.1250164797797,
122.710986226802)) ;
#51811 = CARTESIAN_POINT('Ctrl Pts',(-18.1825491266174,-18.9450273992992,
122.535766487413)) ;
#51812 = CARTESIAN_POINT('Ctrl Pts',(-18.3204432885905,-19.1350725239527,
122.893038269463)) ;
#51813 = CARTESIAN_POINT('Ctrl Pts',(-18.048243794037,-18.9550834434722,122.763330187335)) ;
#51814 = CARTESIAN_POINT('Ctrl Pts',(-18.2474379776068,-19.1450132639979,
123.088867079134)) ;
#51815 = CARTESIAN_POINT('Ctrl Pts',(-17.9569846491174,-18.9650241835174,
123.008115620685)) ;
#51816 = CARTESIAN_POINT('Ctrl Pts',(-18.2090421542517,-19.1549173850707,
123.293514642458)) ;
#51817 = CARTESIAN_POINT('Ctrl Pts',(-17.9089873946553,-18.9749283045903,
123.26392514925)) ;
#51818 = CARTESIAN_POINT('Ctrl Pts',(-18.2068596104492,-19.164964926225,123.504719529866)) ;
#51819 = CARTESIAN_POINT('Ctrl Pts',(-17.9062567712307,-18.9849758457445,
123.527931134962)) ;
#51820 = CARTESIAN_POINT('Ctrl Pts',(-18.2407268057589,-19.1748636778254,
123.710075861997)) ;
#51821 = CARTESIAN_POINT('Ctrl Pts',(-17.9485884794036,-18.9948745973449,
123.784627499361)) ;
#51822 = CARTESIAN_POINT('Ctrl Pts',(-18.3106763440572,-19.1849121567912,
123.909385049677)) ;
#51823 = CARTESIAN_POINT('Ctrl Pts',(-18.0360231029504,-19.0049230763107,
124.033764662997)) ;
#51824 = CARTESIAN_POINT('Ctrl Pts',(-18.4125198148673,-19.1947996538749,
124.09061780245)) ;
#51825 = CARTESIAN_POINT('Ctrl Pts',(-18.1633256706012,-19.0148105733944,
124.26030732657)) ;
#51826 = CARTESIAN_POINT('Ctrl Pts',(-18.5453641416013,-19.204792744173,124.253347261805)) ;
#51827 = CARTESIAN_POINT('Ctrl Pts',(-18.3293793930391,-19.0248036636925,
124.463720725845)) ;
#51828 = CARTESIAN_POINT('Ctrl Pts',(-18.70386501416,-19.2147449142333,124.389942305651)) ;
#51829 = CARTESIAN_POINT('Ctrl Pts',(-18.527504240545,-19.0347558337528,124.634466520031)) ;
#51830 = CARTESIAN_POINT('Ctrl Pts',(-18.8832573055452,-19.2246833341478,
124.497026002691)) ;
#51831 = CARTESIAN_POINT('Ctrl Pts',(-18.7517438316603,-19.0446942536673,
124.768323297008)) ;
#51832 = CARTESIAN_POINT('Ctrl Pts',(-19.0793846745513,-19.2346684642334,
124.571917646202)) ;
#51833 = CARTESIAN_POINT('Ctrl Pts',(-18.996902443479,-19.0546793837529,124.861939963005)) ;
#51834 = CARTESIAN_POINT('Ctrl Pts',(-19.2866263766652,-19.2447051536475,
124.611508315712)) ;
#51835 = CARTESIAN_POINT('Ctrl Pts',(-19.2559540582178,-19.064716073167,124.911430512006)) ;
#51836 = CARTESIAN_POINT('Ctrl Pts',(-19.4937950988768,-19.25455983764,124.614789826941)) ;
#51837 = CARTESIAN_POINT('Ctrl Pts',(-19.5149158429262,-19.0745707571595,
124.915534596148)) ;
#51838 = CARTESIAN_POINT('Ctrl Pts',(-19.7013848668796,-19.2645593216878,
124.581864338488)) ;
#51839 = CARTESIAN_POINT('Ctrl Pts',(-19.7744035154957,-19.0845702412073,
124.874379795897)) ;
#51840 = CARTESIAN_POINT('Ctrl Pts',(-19.8981684622734,-19.2744544104647,
124.514296465217)) ;
#51841 = CARTESIAN_POINT('Ctrl Pts',(-20.0203843649361,-19.0944653299842,
124.789921645823)) ;
#51842 = CARTESIAN_POINT('Ctrl Pts',(-20.0832105036019,-19.2845149651109,
124.411914232186)) ;
#51843 = CARTESIAN_POINT('Ctrl Pts',(-20.2516876996053,-19.1045258846304,
124.661945764523)) ;
#51844 = CARTESIAN_POINT('Ctrl Pts',(-20.2443173608154,-19.2943642294838,
124.281814272574)) ;
#51845 = CARTESIAN_POINT('Ctrl Pts',(-20.453073345448,-19.1143751490033,124.499321729765)) ;
#51846 = CARTESIAN_POINT('Ctrl Pts',(-20.383234603429,-19.3043914819316,124.123263298254)) ;
#51847 = CARTESIAN_POINT('Ctrl Pts',(-20.6267212721774,-19.1244024014511,
124.301134265008)) ;
#51848 = CARTESIAN_POINT('Ctrl Pts',(-20.4920569293237,-19.3144197795018,
123.942681895053)) ;
#51849 = CARTESIAN_POINT('Ctrl Pts',(-20.7627508779272,-19.1344306990213,
124.07540861647)) ;
#51850 = CARTESIAN_POINT('Ctrl Pts',(-20.5668588209695,-19.3242659085078,
123.749683017547)) ;
#51851 = CARTESIAN_POINT('Ctrl Pts',(-20.856255422354,-19.1442768280273,123.83415966172)) ;
#51852 = CARTESIAN_POINT('Ctrl Pts',(-20.608133965986,-19.3342598138698,123.543674588756)) ;
#51853 = CARTESIAN_POINT('Ctrl Pts',(-20.9078510942606,-19.1542707333894,
123.576649296559)) ;
#51854 = CARTESIAN_POINT('Ctrl Pts',(-20.6126495317417,-19.3442839115529,
123.332979210101)) ;
#51855 = CARTESIAN_POINT('Ctrl Pts',(-20.913497410932,-19.1642948310724,123.313280162648)) ;
#51856 = CARTESIAN_POINT('Ctrl Pts',(-20.5812020044249,-19.3541737394069,
123.127452597675)) ;
#51857 = CARTESIAN_POINT('Ctrl Pts',(-20.8741896284399,-19.1741846589264,
123.056370784459)) ;
#51858 = CARTESIAN_POINT('Ctrl Pts',(-20.5141513741435,-19.3641657208373,
122.928386984327)) ;
#51859 = CARTESIAN_POINT('Ctrl Pts',(-20.7903778748862,-19.1841766403569,
122.807538053426)) ;
#51860 = CARTESIAN_POINT('Ctrl Pts',(-20.4139600151984,-19.3741127256032,
122.744833669231)) ;
#51861 = CARTESIAN_POINT('Ctrl Pts',(-20.6651399258501,-19.1941236451227,
122.578095153179)) ;
#51862 = CARTESIAN_POINT('Ctrl Pts',(-20.2836802509689,-19.384062376993,122.581175213375)) ;
#51863 = CARTESIAN_POINT('Ctrl Pts',(-20.5022911488961,-19.2040732965125,
122.373520731154)) ;
#51864 = CARTESIAN_POINT('Ctrl Pts',(-20.1254838491908,-19.3940993799704,
122.441545872889)) ;
#51865 = CARTESIAN_POINT('Ctrl Pts',(-20.3045468223484,-19.2141102994899,
122.198982921327)) ;
#51866 = CARTESIAN_POINT('Ctrl Pts',(-19.9481679622584,-19.4039882884054,
122.332997305238)) ;
#51867 = CARTESIAN_POINT('Ctrl Pts',(-20.0829020054468,-19.2239992079249,
122.063295386197)) ;
#51868 = CARTESIAN_POINT('Ctrl Pts',(-19.7528840797197,-19.4139776208829,
122.255763547514)) ;
#51869 = CARTESIAN_POINT('Ctrl Pts',(-19.8387974858014,-19.2339885404024,
121.966751761662)) ;
#51870 = CARTESIAN_POINT('Ctrl Pts',(-19.5477596783419,-19.42393617632,122.213894358969)) ;
#51871 = CARTESIAN_POINT('Ctrl Pts',(-19.5823918613981,-19.2439470958395,
121.914413714354)) ;
#51872 = CARTESIAN_POINT('Ctrl Pts',(-19.339716261487,-19.4338357475205,122.20779695739)) ;
#51873 = CARTESIAN_POINT('Ctrl Pts',(-19.3223367513791,-19.25384666704,121.90679061317)) ;
#51874 = CARTESIAN_POINT('Ctrl Pts',(-19.1307330189891,-19.4438836727725,
122.238435863334)) ;
#51875 = CARTESIAN_POINT('Ctrl Pts',(-19.0611077173533,-19.263894592292,121.945087876607)) ;
#51876 = CARTESIAN_POINT('Ctrl Pts',(-18.9331863686477,-19.4537789722985,
122.303747134582)) ;
#51877 = CARTESIAN_POINT('Ctrl Pts',(-18.8141731330482,-19.273789891818,122.026726024878)) ;
#51878 = CARTESIAN_POINT('Ctrl Pts',(-18.7469349813943,-19.4638408287464,
122.403975883156)) ;
#51879 = CARTESIAN_POINT('Ctrl Pts',(-18.5813585769284,-19.283851748266,122.152010675275)) ;
#51880 = CARTESIAN_POINT('Ctrl Pts',(-18.5844603918164,-19.4736846751631,
122.532169779838)) ;
#51881 = CARTESIAN_POINT('Ctrl Pts',(-18.3782635157995,-19.2936955946826,
122.31225286632)) ;
#51882 = CARTESIAN_POINT('Ctrl Pts',(-18.444520656928,-19.4836476242911,122.687999610544)) ;
#51883 = CARTESIAN_POINT('Ctrl Pts',(-18.2033377995914,-19.3036585438106,
122.507039819506)) ;
#51884 = CARTESIAN_POINT('Ctrl Pts',(-18.3332595420171,-19.4936816607191,
122.867226494345)) ;
#51885 = CARTESIAN_POINT('Ctrl Pts',(-18.0642605164211,-19.3136925802387,
122.731072712996)) ;
#51886 = CARTESIAN_POINT('Ctrl Pts',(-18.2557552508508,-19.5035690876772,
123.060098414967)) ;
#51887 = CARTESIAN_POINT('Ctrl Pts',(-17.9673787964987,-19.3235800071967,
122.972163161399)) ;
#51888 = CARTESIAN_POINT('Ctrl Pts',(-18.2119716822401,-19.5135835220135,
123.266045020976)) ;
#51889 = CARTESIAN_POINT('Ctrl Pts',(-17.91264845191,-19.3335944415331,123.229596243472)) ;
#51890 = CARTESIAN_POINT('Ctrl Pts',(-18.2051271781336,-19.5236184666485,
123.476886047581)) ;
#51891 = CARTESIAN_POINT('Ctrl Pts',(-17.9040917214434,-19.343629386168,123.493147352369)) ;
#51892 = CARTESIAN_POINT('Ctrl Pts',(-18.2338373099495,-19.5334508166795,
123.681614438135)) ;
#51893 = CARTESIAN_POINT('Ctrl Pts',(-17.9399787129284,-19.353461736199,123.749059430718)) ;
#51894 = CARTESIAN_POINT('Ctrl Pts',(-18.2991584830252,-19.5435262557967,
123.883066110455)) ;
#51895 = CARTESIAN_POINT('Ctrl Pts',(-18.0216292178934,-19.3635371753162,
124.00087385622)) ;
#51896 = CARTESIAN_POINT('Ctrl Pts',(-18.3962015107462,-19.5533787210313,
124.066105872207)) ;
#51897 = CARTESIAN_POINT('Ctrl Pts',(-18.1429328955144,-19.3733896405508,
124.229675102713)) ;
#51898 = CARTESIAN_POINT('Ctrl Pts',(-18.5262180602235,-19.5634515986082,
124.233211940351)) ;
#51899 = CARTESIAN_POINT('Ctrl Pts',(-18.3054527182946,-19.3834625181277,
124.43855780695)) ;
#51900 = CARTESIAN_POINT('Ctrl Pts',(-18.6797419077355,-19.5732941948007,
124.371972025685)) ;
#51901 = CARTESIAN_POINT('Ctrl Pts',(-18.4973580638429,-19.3933051143202,
124.612009431647)) ;
#51902 = CARTESIAN_POINT('Ctrl Pts',(-18.8570829768545,-19.583274578916,124.484089894838)) ;
#51903 = CARTESIAN_POINT('Ctrl Pts',(-18.7190343989905,-19.4032854984355,
124.752157350515)) ;
#51904 = CARTESIAN_POINT('Ctrl Pts',(-19.0520979345884,-19.5932930595648,
124.563638386236)) ;
#51905 = CARTESIAN_POINT('Ctrl Pts',(-18.9628028394282,-19.4133039790843,
124.851593566146)) ;
#51906 = CARTESIAN_POINT('Ctrl Pts',(-19.2551201360957,-19.6031763745651,
124.60795747562)) ;
#51907 = CARTESIAN_POINT('Ctrl Pts',(-19.2165815610686,-19.4231872940847,
124.906993129146)) ;
#51908 = CARTESIAN_POINT('Ctrl Pts',(-19.4665835366487,-19.6132446716556,
124.616412950505)) ;
#51909 = CARTESIAN_POINT('Ctrl Pts',(-19.4809103809794,-19.4332555911751,
124.917562972864)) ;
#51910 = CARTESIAN_POINT('Ctrl Pts',(-19.6714432989599,-19.6230747400279,
124.588929074882)) ;
#51911 = CARTESIAN_POINT('Ctrl Pts',(-19.7369866665315,-19.4430856595474,
124.883208337484)) ;
#51912 = CARTESIAN_POINT('Ctrl Pts',(-19.8731711829206,-19.6331415324963,
124.525058281319)) ;
#51913 = CARTESIAN_POINT('Ctrl Pts',(-19.9891462344997,-19.4531524520158,
124.803370269155)) ;
#51914 = CARTESIAN_POINT('Ctrl Pts',(-20.0574611220455,-19.6430308659848,
124.428741148867)) ;
#51915 = CARTESIAN_POINT('Ctrl Pts',(-20.2195097661445,-19.4630417855043,
124.682973671371)) ;
#51916 = CARTESIAN_POINT('Ctrl Pts',(-20.2242497094466,-19.6530329974009,
124.300749095355)) ;
#51917 = CARTESIAN_POINT('Ctrl Pts',(-20.4279957457152,-19.4730439169204,
124.522983695242)) ;
#51918 = CARTESIAN_POINT('Ctrl Pts',(-20.3653190292274,-19.6629568670219,
124.146990412121)) ;
#51919 = CARTESIAN_POINT('Ctrl Pts',(-20.6043330329384,-19.4829677865414,
124.330784900666)) ;
#51920 = CARTESIAN_POINT('Ctrl Pts',(-20.4788115638029,-19.6730003825391,
123.968976465865)) ;
#51921 = CARTESIAN_POINT('Ctrl Pts',(-20.746198747271,-19.4930113020586,124.108267757333)) ;
#51922 = CARTESIAN_POINT('Ctrl Pts',(-20.5586220167799,-19.6828825954274,
123.777121275203)) ;
#51923 = CARTESIAN_POINT('Ctrl Pts',(-20.8459623355023,-19.5028935149469,
123.868447779249)) ;
#51924 = CARTESIAN_POINT('Ctrl Pts',(-20.6047386809469,-19.6929506726468,
123.570583320886)) ;
#51925 = CARTESIAN_POINT('Ctrl Pts',(-20.9036081811708,-19.5129615921663,
123.61027574671)) ;
#51926 = CARTESIAN_POINT('Ctrl Pts',(-20.6142646304395,-19.702789177381,123.36393271165)) ;
#51927 = CARTESIAN_POINT('Ctrl Pts',(-20.9155157126523,-19.5228000969005,
123.35196100677)) ;
#51928 = CARTESIAN_POINT('Ctrl Pts',(-20.5874658464836,-19.7128519458104,
123.154111705371)) ;
#51929 = CARTESIAN_POINT('Ctrl Pts',(-20.8820171907135,-19.5328628653299,
123.089685129333)) ;
#51930 = CARTESIAN_POINT('Ctrl Pts',(-20.5254497535726,-19.7227489390931,
122.955490377615)) ;
#51931 = CARTESIAN_POINT('Ctrl Pts',(-20.8044967775685,-19.5427598586126,
122.841407511821)) ;
#51932 = CARTESIAN_POINT('Ctrl Pts',(-20.4301860161421,-19.7326801667279,
122.769710863237)) ;
#51933 = CARTESIAN_POINT('Ctrl Pts',(-20.6854165302219,-19.5526910862474,
122.609182603885)) ;
#51934 = CARTESIAN_POINT('Ctrl Pts',(-20.3025172159415,-19.74272232537,122.601572700884)) ;
#51935 = CARTESIAN_POINT('Ctrl Pts',(-20.5258305093351,-19.5627332448896,
122.39901017822)) ;
#51936 = CARTESIAN_POINT('Ctrl Pts',(-20.1500853642892,-19.7526090349011,
122.460258580595)) ;
#51937 = CARTESIAN_POINT('Ctrl Pts',(-20.3352897322211,-19.5726199544206,
122.22236696754)) ;
#51938 = CARTESIAN_POINT('Ctrl Pts',(-19.973762981087,-19.7626020073297,122.346058634074)) ;
#51939 = CARTESIAN_POINT('Ctrl Pts',(-20.1148863728096,-19.5826129268492,
122.079617245332)) ;
#51940 = CARTESIAN_POINT('Ctrl Pts',(-19.7811555655468,-19.7725482018663,
122.26467134964)) ;
#51941 = CARTESIAN_POINT('Ctrl Pts',(-19.8741264227168,-19.5925591213858,
121.977883228999)) ;
#51942 = CARTESIAN_POINT('Ctrl Pts',(-19.577440733495,-19.7824935767178,122.217515204757)) ;
#51943 = CARTESIAN_POINT('Ctrl Pts',(-19.6194821905745,-19.6025044962373,
121.918938430687)) ;
#51944 = CARTESIAN_POINT('Ctrl Pts',(-19.3663571883107,-19.7925484960777,
122.206654014904)) ;
#51945 = CARTESIAN_POINT('Ctrl Pts',(-19.3556280435111,-19.6125594155972,
121.905362356651)) ;
#51946 = CARTESIAN_POINT('Ctrl Pts',(-19.1613655130489,-19.8023700155212,
122.231619206292)) ;
#51947 = CARTESIAN_POINT('Ctrl Pts',(-19.0993869104664,-19.6223809350407,
121.936569596231)) ;
#51948 = CARTESIAN_POINT('Ctrl Pts',(-18.9588961884829,-19.8124357842881,
122.293030078192)) ;
#51949 = CARTESIAN_POINT('Ctrl Pts',(-18.8463008166021,-19.6324467038076,
122.013333704134)) ;
#51950 = CARTESIAN_POINT('Ctrl Pts',(-18.7732037589491,-19.8223377059431,
122.387203432726)) ;
#51951 = CARTESIAN_POINT('Ctrl Pts',(-18.6141847412785,-19.6423486254627,
122.131051370965)) ;
#51952 = CARTESIAN_POINT('Ctrl Pts',(-18.6042436666865,-19.8323807647642,
122.513786536381)) ;
#51953 = CARTESIAN_POINT('Ctrl Pts',(-18.4029852172294,-19.6523916842837,
122.289280682482)) ;
#51954 = CARTESIAN_POINT('Ctrl Pts',(-18.4618641617122,-19.8422867588069,
122.665775366195)) ;
#51955 = CARTESIAN_POINT('Ctrl Pts',(-18.2250106930519,-19.6622976783264,
122.479267826183)) ;
#51956 = CARTESIAN_POINT('Ctrl Pts',(-18.347162029579,-19.8522245318887,122.840394738477)) ;
#51957 = CARTESIAN_POINT('Ctrl Pts',(-18.0816334126947,-19.6722354514082,
122.69754307757)) ;
#51958 = CARTESIAN_POINT('Ctrl Pts',(-18.2638779267283,-19.862264895621,123.034345828099)) ;
#51959 = CARTESIAN_POINT('Ctrl Pts',(-17.9775290974317,-19.6822758151405,
122.939982086256)) ;
#51960 = CARTESIAN_POINT('Ctrl Pts',(-18.2161158206728,-19.8721522393445,
123.236657619917)) ;
#51961 = CARTESIAN_POINT('Ctrl Pts',(-17.9178270662773,-19.692163158864,123.192873036768)) ;
#51962 = CARTESIAN_POINT('Ctrl Pts',(-18.2037362405876,-19.8821444699132,
123.446346397897)) ;
#51963 = CARTESIAN_POINT('Ctrl Pts',(-17.9023535728988,-19.7021553894327,
123.454984271164)) ;
#51964 = CARTESIAN_POINT('Ctrl Pts',(-18.2279073020014,-19.8920929976968,
123.65410610834)) ;
#51965 = CARTESIAN_POINT('Ctrl Pts',(-17.9325684278091,-19.7121039172163,
123.714684335737)) ;
#51966 = CARTESIAN_POINT('Ctrl Pts',(-18.2874238407614,-19.9020297814201,
123.854332451644)) ;
#51967 = CARTESIAN_POINT('Ctrl Pts',(-18.0069653211823,-19.7220407009396,
123.964967568161)) ;
#51968 = CARTESIAN_POINT('Ctrl Pts',(-18.3810183276697,-19.912012782217,124.042211329903)) ;
#51969 = CARTESIAN_POINT('Ctrl Pts',(-18.1239596002325,-19.7320237017366,
124.199815869791)) ;
#51970 = CARTESIAN_POINT('Ctrl Pts',(-18.5068566623067,-19.9220566690578,
124.211741307508)) ;
#51971 = CARTESIAN_POINT('Ctrl Pts',(-18.2812582375545,-19.7420675885773,
124.411727571379)) ;
#51972 = CARTESIAN_POINT('Ctrl Pts',(-18.656625770795,-19.9318846926323,124.354124004755)) ;
#51973 = CARTESIAN_POINT('Ctrl Pts',(-18.4684715102243,-19.7518956121519,
124.58970605607)) ;
#51974 = CARTESIAN_POINT('Ctrl Pts',(-18.8330935902759,-19.941961940846,124.47126421145)) ;
#51975 = CARTESIAN_POINT('Ctrl Pts',(-18.6890566140146,-19.7619728603655,
124.736130030248)) ;
#51976 = CARTESIAN_POINT('Ctrl Pts',(-19.0228690100662,-19.9518114961513,
124.55424093318)) ;
#51977 = CARTESIAN_POINT('Ctrl Pts',(-18.9262775518615,-19.7718224156708,
124.839850242476)) ;
#51978 = CARTESIAN_POINT('Ctrl Pts',(-19.2288113073246,-19.961894204349,124.604205688793)) ;
#51979 = CARTESIAN_POINT('Ctrl Pts',(-19.1837052991387,-19.7819051238685,
124.902304787866)) ;
#51980 = CARTESIAN_POINT('Ctrl Pts',(-19.434720498365,-19.9717067972754,124.617486778315)) ;
#51981 = CARTESIAN_POINT('Ctrl Pts',(-19.4410933758835,-19.791717716795,124.918904855453)) ;
#51982 = CARTESIAN_POINT('Ctrl Pts',(-19.645072882955,-19.9817739895334,124.594577329218)) ;
#51983 = CARTESIAN_POINT('Ctrl Pts',(-19.704033340018,-19.8017849090529,124.890266579547)) ;
#51984 = CARTESIAN_POINT('Ctrl Pts',(-19.8449282407417,-19.991672818996,124.536378177571)) ;
#51985 = CARTESIAN_POINT('Ctrl Pts',(-19.9538529269763,-19.8116837385155,
124.81751598121)) ;
#51986 = CARTESIAN_POINT('Ctrl Pts',(-20.0345223013733,-20.0017268101862,
124.443044256288)) ;
#51987 = CARTESIAN_POINT('Ctrl Pts',(-20.1908446169872,-19.8217377297057,
124.700847328497)) ;
#51988 = CARTESIAN_POINT('Ctrl Pts',(-20.2021184222333,-20.0115985349694,
124.320569621367)) ;
#51989 = CARTESIAN_POINT('Ctrl Pts',(-20.4003396794263,-19.8316094544889,
124.547752149723)) ;
#51990 = CARTESIAN_POINT('Ctrl Pts',(-20.3487795362929,-20.0216689770996,
124.167933913824)) ;
#51991 = CARTESIAN_POINT('Ctrl Pts',(-20.583664674412,-19.8416798966191,124.35695666658)) ;
#51992 = CARTESIAN_POINT('Ctrl Pts',(-20.4640387398854,-20.0315020555299,
123.996302242053)) ;
#51993 = CARTESIAN_POINT('Ctrl Pts',(-20.7277380469989,-19.8515129750494,
124.142415105711)) ;
#51994 = CARTESIAN_POINT('Ctrl Pts',(-20.5499655152487,-20.0415325290313,
123.803739463889)) ;
#51995 = CARTESIAN_POINT('Ctrl Pts',(-20.835144817367,-19.8615434485508,123.901710971222)) ;
#51996 = CARTESIAN_POINT('Ctrl Pts',(-20.6005657766499,-20.0515641283299,
123.59899153)) ;
#51997 = CARTESIAN_POINT('Ctrl Pts',(-20.8983935516064,-19.8715750478495,
123.645775745979)) ;
#51998 = CARTESIAN_POINT('Ctrl Pts',(-20.6149874000634,-20.0613938293681,
123.392858537114)) ;
#51999 = CARTESIAN_POINT('Ctrl Pts',(-20.9164189117006,-19.8814047488876,
123.388108112835)) ;
#52000 = CARTESIAN_POINT('Ctrl Pts',(-20.593669608918,-20.0713832674246,123.183927476953)) ;
#52001 = CARTESIAN_POINT('Ctrl Pts',(-20.8897697073004,-19.8913941869441,
123.126944309938)) ;
#52002 = CARTESIAN_POINT('Ctrl Pts',(-20.5355721040913,-20.0814271706407,
122.980925519128)) ;
#52003 = CARTESIAN_POINT('Ctrl Pts',(-20.817146145232,-19.9014380901602,122.873192498194)) ;
#52004 = CARTESIAN_POINT('Ctrl Pts',(-20.445542899385,-20.0912486914542,122.795106271871)) ;
#52005 = CARTESIAN_POINT('Ctrl Pts',(-20.7046073619337,-19.9112596109737,
122.640918152562)) ;
#52006 = CARTESIAN_POINT('Ctrl Pts',(-20.3223921732371,-20.1012844157013,
122.623800659788)) ;
#52007 = CARTESIAN_POINT('Ctrl Pts',(-20.5506673335657,-19.9212953352208,
122.426787436303)) ;
#52008 = CARTESIAN_POINT('Ctrl Pts',(-20.1711768869751,-20.1113065696338,
122.477056253106)) ;
#52009 = CARTESIAN_POINT('Ctrl Pts',(-20.3616469062413,-19.9313174891533,
122.243358309421)) ;
#52010 = CARTESIAN_POINT('Ctrl Pts',(-19.9997783644996,-20.1211688013911,
122.360421499363)) ;
#52011 = CARTESIAN_POINT('Ctrl Pts',(-20.1473968173766,-19.9411797209106,
122.097565987301)) ;
#52012 = CARTESIAN_POINT('Ctrl Pts',(-19.8090973942944,-20.131127871849,122.273937081549)) ;
#52013 = CARTESIAN_POINT('Ctrl Pts',(-19.9090443946481,-19.9511387913685,
121.989462309613)) ;
#52014 = CARTESIAN_POINT('Ctrl Pts',(-19.6046796800119,-20.1411630442251,
122.221797594559)) ;
#52015 = CARTESIAN_POINT('Ctrl Pts',(-19.6535218175709,-19.9611739637447,
121.9242899919)) ;
#52016 = CARTESIAN_POINT('Ctrl Pts',(-19.3975520285983,-20.1510434293834,
122.205875090006)) ;
#52017 = CARTESIAN_POINT('Ctrl Pts',(-19.3946113132456,-19.9710543489029,
121.904388967312)) ;
#52018 = CARTESIAN_POINT('Ctrl Pts',(-19.1871508596279,-20.1611001439773,
122.226434671735)) ;
#52019 = CARTESIAN_POINT('Ctrl Pts',(-19.1316102592034,-19.9811110634969,
121.930090607087)) ;
#52020 = CARTESIAN_POINT('Ctrl Pts',(-18.9870826370418,-20.1709794125494,
122.28223552978)) ;
#52021 = CARTESIAN_POINT('Ctrl Pts',(-18.8815248169901,-19.9909903320689,
121.999843995858)) ;
#52022 = CARTESIAN_POINT('Ctrl Pts',(-18.7973905879869,-20.1809703700351,
122.372426720586)) ;
#52023 = CARTESIAN_POINT('Ctrl Pts',(-18.6444106248268,-20.0009812895546,
122.112585153675)) ;
#52024 = CARTESIAN_POINT('Ctrl Pts',(-18.6256580137942,-20.1910110286703,
122.495170942343)) ;
#52025 = CARTESIAN_POINT('Ctrl Pts',(-18.4297462674752,-20.0110219481898,
122.266017180196)) ;
#52026 = CARTESIAN_POINT('Ctrl Pts',(-18.4806610276397,-20.2008440083783,
122.642504839744)) ;
#52027 = CARTESIAN_POINT('Ctrl Pts',(-18.2485010033221,-20.0208549278978,
122.450186849421)) ;
#52028 = CARTESIAN_POINT('Ctrl Pts',(-18.3610435893545,-20.210837141628,122.81520973265)) ;
#52029 = CARTESIAN_POINT('Ctrl Pts',(-18.0989811416555,-20.0308480611475,
122.666069459548)) ;
#52030 = CARTESIAN_POINT('Ctrl Pts',(-18.2732819316886,-20.2208691940113,
123.00699894088)) ;
#52031 = CARTESIAN_POINT('Ctrl Pts',(-17.9892812122869,-20.0408801135309,
122.905806909193)) ;
#52032 = CARTESIAN_POINT('Ctrl Pts',(-18.2207950634058,-20.2307344229627,
123.207634736704)) ;
#52033 = CARTESIAN_POINT('Ctrl Pts',(-17.9236747633923,-20.0507453424822,
123.156602970146)) ;
#52034 = CARTESIAN_POINT('Ctrl Pts',(-18.2031854904533,-20.2406963642059,
123.416330007382)) ;
#52035 = CARTESIAN_POINT('Ctrl Pts',(-17.9016652915636,-20.0607072837254,
123.417472522823)) ;
#52036 = CARTESIAN_POINT('Ctrl Pts',(-18.2225552242185,-20.2507310792426,
123.626390528993)) ;
#52037 = CARTESIAN_POINT('Ctrl Pts',(-17.9258798986461,-20.0707419987622,
123.680047915011)) ;
#52038 = CARTESIAN_POINT('Ctrl Pts',(-18.2769648586683,-20.2606168495867,
123.826997944236)) ;
#52039 = CARTESIAN_POINT('Ctrl Pts',(-17.9938945219827,-20.0806277691062,
123.930807070549)) ;
#52040 = CARTESIAN_POINT('Ctrl Pts',(-18.3669425663381,-20.2706794469754,
124.018428595502)) ;
#52041 = CARTESIAN_POINT('Ctrl Pts',(-18.1063688769933,-20.090690366495,124.170094182649)) ;
#52042 = CARTESIAN_POINT('Ctrl Pts',(-18.4861705032572,-20.2805298588107,
124.187769337836)) ;
#52043 = CARTESIAN_POINT('Ctrl Pts',(-18.2554062653276,-20.1005407783302,
124.381769206499)) ;
#52044 = CARTESIAN_POINT('Ctrl Pts',(-18.6352264586599,-20.2905570280966,
124.336825287887)) ;
#52045 = CARTESIAN_POINT('Ctrl Pts',(-18.4417280627902,-20.1105679476161,
124.568087271063)) ;
#52046 = CARTESIAN_POINT('Ctrl Pts',(-18.8082335054071,-20.3005845088108,
124.457297088272)) ;
#52047 = CARTESIAN_POINT('Ctrl Pts',(-18.6579883239994,-20.1205954283303,
124.718674943261)) ;
#52048 = CARTESIAN_POINT('Ctrl Pts',(-18.9958279314293,-20.3104275613901,
124.544623627874)) ;
#52049 = CARTESIAN_POINT('Ctrl Pts',(-18.8924830332573,-20.1304384809096,
124.827831022369)) ;
#52050 = CARTESIAN_POINT('Ctrl Pts',(-19.19866746115,-20.3204214648287,124.599389527813)) ;
#52051 = CARTESIAN_POINT('Ctrl Pts',(-19.1460332395822,-20.1404323843482,
124.896285826052)) ;
#52052 = CARTESIAN_POINT('Ctrl Pts',(-19.4086704937467,-20.3304485876051,
124.617780480722)) ;
#52053 = CARTESIAN_POINT('Ctrl Pts',(-19.4085372828639,-20.1504595071246,
124.919271899914)) ;
#52054 = CARTESIAN_POINT('Ctrl Pts',(-19.6158404873169,-20.3403392924971,
124.599938377875)) ;
#52055 = CARTESIAN_POINT('Ctrl Pts',(-19.6674999586841,-20.1603502120167,
124.896966576289)) ;
#52056 = CARTESIAN_POINT('Ctrl Pts',(-19.8188925643533,-20.3503313193475,
124.546143797245)) ;
#52057 = CARTESIAN_POINT('Ctrl Pts',(-19.9213144644297,-20.170342238867,124.829720703372)) ;
#52058 = CARTESIAN_POINT('Ctrl Pts',(-20.0086203150577,-20.360277300836,124.458257930678)) ;
#52059 = CARTESIAN_POINT('Ctrl Pts',(-20.1584732284019,-20.1802882203555,
124.719860821216)) ;
#52060 = CARTESIAN_POINT('Ctrl Pts',(-20.1804782509526,-20.3702244734579,
124.339088999519)) ;
#52061 = CARTESIAN_POINT('Ctrl Pts',(-20.3732942472186,-20.1902353929774,
124.570897282549)) ;
#52062 = CARTESIAN_POINT('Ctrl Pts',(-20.3303594599015,-20.3802724147841,
124.190244480905)) ;
#52063 = CARTESIAN_POINT('Ctrl Pts',(-20.560643830539,-20.2002833343036,124.384839709469)) ;
#52064 = CARTESIAN_POINT('Ctrl Pts',(-20.4498405364493,-20.3901200485918,
124.021171300404)) ;
#52065 = CARTESIAN_POINT('Ctrl Pts',(-20.7099931678964,-20.2101309681114,
124.173496321079)) ;
#52066 = CARTESIAN_POINT('Ctrl Pts',(-20.5397614536319,-20.4000817632769,
123.832042454196)) ;
#52067 = CARTESIAN_POINT('Ctrl Pts',(-20.8223918372433,-20.2200926827964,
123.937083946843)) ;
#52068 = CARTESIAN_POINT('Ctrl Pts',(-20.5955998308358,-20.4101103961554,
123.628724338267)) ;
#52069 = CARTESIAN_POINT('Ctrl Pts',(-20.8921871414343,-20.2301213156749,
123.682935524413)) ;
#52070 = CARTESIAN_POINT('Ctrl Pts',(-20.6151216491279,-20.4200207216905,
123.421303306592)) ;
#52071 = CARTESIAN_POINT('Ctrl Pts',(-20.9165866655154,-20.2400316412101,
123.423658765386)) ;
#52072 = CARTESIAN_POINT('Ctrl Pts',(-20.5988309906371,-20.4299555521623,
123.213073747542)) ;
#52073 = CARTESIAN_POINT('Ctrl Pts',(-20.8962205048612,-20.2499664716818,
123.163371888236)) ;
#52074 = CARTESIAN_POINT('Ctrl Pts',(-20.5458999153234,-20.4399968845442,
123.008717300108)) ;
#52075 = CARTESIAN_POINT('Ctrl Pts',(-20.830054005879,-20.2600078040638,122.907927043648)) ;
#52076 = CARTESIAN_POINT('Ctrl Pts',(-20.4596544020495,-20.4498897579831,
122.819465298956)) ;
#52077 = CARTESIAN_POINT('Ctrl Pts',(-20.7222442143101,-20.2699006775026,
122.671362855036)) ;
#52078 = CARTESIAN_POINT('Ctrl Pts',(-20.3413828244053,-20.459858923801,122.646430648159)) ;
#52079 = CARTESIAN_POINT('Ctrl Pts',(-20.5744033926892,-20.2798698433205,
122.455071839325)) ;
#52080 = CARTESIAN_POINT('Ctrl Pts',(-20.1937587502541,-20.4698876575175,
122.49593053107)) ;
#52081 = CARTESIAN_POINT('Ctrl Pts',(-20.3898674158491,-20.289898577037,122.266945763513)) ;
#52082 = CARTESIAN_POINT('Ctrl Pts',(-19.9684033928012,-20.4830801762886,
122.334134273859)) ;
#52083 = CARTESIAN_POINT('Ctrl Pts',(-20.1081899356053,-20.3030910958082,
122.064717611177)) ;
#52084 = CARTESIAN_POINT('Ctrl Pts',(-19.7027899632007,-20.4964400443313,
122.233638145416)) ;
#52085 = CARTESIAN_POINT('Ctrl Pts',(-19.7762004294729,-20.3164509638508,
121.939098029861)) ;
#52086 = CARTESIAN_POINT('Ctrl Pts',(-19.4261080021341,-20.5096653814802,
122.206033322011)) ;
#52087 = CARTESIAN_POINT('Ctrl Pts',(-19.4302944299203,-20.3296763009997,
121.904585070662)) ;
#52088 = CARTESIAN_POINT('Ctrl Pts',(-19.2168158322053,-20.5196466073208,
122.221163224534)) ;
#52089 = CARTESIAN_POINT('Ctrl Pts',(-19.1686900557135,-20.3396575268403,
121.923502397254)) ;
#52090 = CARTESIAN_POINT('Ctrl Pts',(-19.0123335437991,-20.5296821743037,
122.273082359298)) ;
#52091 = CARTESIAN_POINT('Ctrl Pts',(-18.9130849261336,-20.3496930938232,
121.988403504141)) ;
#52092 = CARTESIAN_POINT('Ctrl Pts',(-18.8230767712462,-20.5395452522658,
122.357856292057)) ;
#52093 = CARTESIAN_POINT('Ctrl Pts',(-18.6765159439737,-20.3595561717853,
122.094373600116)) ;
#52094 = CARTESIAN_POINT('Ctrl Pts',(-18.6478204664462,-20.5496155510669,
122.476584772983)) ;
#52095 = CARTESIAN_POINT('Ctrl Pts',(-18.4574468060373,-20.3696264705864,
122.242786566347)) ;
#52096 = CARTESIAN_POINT('Ctrl Pts',(-18.4992676427898,-20.5594578496347,
122.620634851231)) ;
#52097 = CARTESIAN_POINT('Ctrl Pts',(-18.2717579004152,-20.3794687691542,
122.42285107559)) ;
#52098 = CARTESIAN_POINT('Ctrl Pts',(-18.3759064700005,-20.5694185478045,
122.789841274378)) ;
#52099 = CARTESIAN_POINT('Ctrl Pts',(-18.1175586645594,-20.389429467324,122.634360677971)) ;
#52100 = CARTESIAN_POINT('Ctrl Pts',(-18.283462315847,-20.579456581984,122.979538516165)) ;
#52101 = CARTESIAN_POINT('Ctrl Pts',(-18.0020059070318,-20.3994675015035,
122.871483585711)) ;
#52102 = CARTESIAN_POINT('Ctrl Pts',(-18.2259264092377,-20.5893303188304,
123.179010973159)) ;
#52103 = CARTESIAN_POINT('Ctrl Pts',(-17.9300887191848,-20.40934123835,123.120824683872)) ;
#52104 = CARTESIAN_POINT('Ctrl Pts',(-18.203489149074,-20.5994021027557,123.389529384903)) ;
#52105 = CARTESIAN_POINT('Ctrl Pts',(-17.9020448472088,-20.4194130222752,
123.383973224122)) ;
#52106 = CARTESIAN_POINT('Ctrl Pts',(-18.217479141793,-20.6092342239569,123.595777992507)) ;
#52107 = CARTESIAN_POINT('Ctrl Pts',(-17.9195350317834,-20.4292451434764,
123.641783391218)) ;
#52108 = CARTESIAN_POINT('Ctrl Pts',(-18.2675235725742,-20.6192672479823,
123.800670607276)) ;
#52109 = CARTESIAN_POINT('Ctrl Pts',(-17.9820931574861,-20.4392781675018,
123.897898640848)) ;
#52110 = CARTESIAN_POINT('Ctrl Pts',(-18.3527418081313,-20.629283128179,123.993235721321)) ;
#52111 = CARTESIAN_POINT('Ctrl Pts',(-18.0886185612783,-20.4492940476985,
124.138604141941)) ;
#52112 = CARTESIAN_POINT('Ctrl Pts',(-18.4682220622006,-20.6391666472732,
124.165972783851)) ;
#52113 = CARTESIAN_POINT('Ctrl Pts',(-18.2329706507137,-20.4591775667927,
124.354523332002)) ;
#52114 = CARTESIAN_POINT('Ctrl Pts',(-18.6132891948029,-20.6491570596368,
124.317833664429)) ;
#52115 = CARTESIAN_POINT('Ctrl Pts',(-18.4143074090082,-20.4691679791564,
124.544348991668)) ;
#52116 = CARTESIAN_POINT('Ctrl Pts',(-18.8379391592786,-20.6624202228403,
124.483045377824)) ;
#52117 = CARTESIAN_POINT('Ctrl Pts',(-18.6951170309133,-20.4824311423598,
124.750853866939)) ;
#52118 = CARTESIAN_POINT('Ctrl Pts',(-19.1007465541756,-20.6756977930915,
124.586193595685)) ;
#52119 = CARTESIAN_POINT('Ctrl Pts',(-19.0235816254098,-20.495708712611,124.879780338638)) ;
#52120 = CARTESIAN_POINT('Ctrl Pts',(-19.3792304841943,-20.6890280955981,
124.617392370144)) ;
#52121 = CARTESIAN_POINT('Ctrl Pts',(-19.3717460245729,-20.5090390151176,
124.918788838466)) ;
#52122 = CARTESIAN_POINT('Ctrl Pts',(-19.5869463660609,-20.6989267774145,
124.604614305006)) ;
#52123 = CARTESIAN_POINT('Ctrl Pts',(-19.631378352173,-20.518937696934,124.90281115376)) ;
#52124 = CARTESIAN_POINT('Ctrl Pts',(-19.7911870424571,-20.708916292462,124.555761796128)) ;
#52125 = CARTESIAN_POINT('Ctrl Pts',(-19.8866819314184,-20.5289272119815,
124.841743662689)) ;
#52126 = CARTESIAN_POINT('Ctrl Pts',(-19.9830582667155,-20.718864344237,124.472519591824)) ;
#52127 = CARTESIAN_POINT('Ctrl Pts',(-20.1265183760902,-20.5388752637566,
124.737689396251)) ;
#52128 = CARTESIAN_POINT('Ctrl Pts',(-20.1575675432332,-20.7288057475155,
124.357539674552)) ;
#52129 = CARTESIAN_POINT('Ctrl Pts',(-20.3446556458458,-20.5488166670351,
124.593959706132)) ;
#52130 = CARTESIAN_POINT('Ctrl Pts',(-20.3608485699155,-20.7420924122965,
124.165903707027)) ;
#52131 = CARTESIAN_POINT('Ctrl Pts',(-20.5987445477632,-20.562103331816,124.354427858085)) ;
#52132 = CARTESIAN_POINT('Ctrl Pts',(-20.5464483543658,-20.7587028339513,
123.865472903908)) ;
#52133 = CARTESIAN_POINT('Ctrl Pts',(-20.830752172196,-20.5787137534708,123.978870507254)) ;
#52134 = CARTESIAN_POINT('Ctrl Pts',(-20.6330141955444,-20.7786140962021,
123.451029395144)) ;
#52135 = CARTESIAN_POINT('Ctrl Pts',(-20.9389514262488,-20.5986250157216,
123.460821316343)) ;
#52136 = CARTESIAN_POINT('Ctrl Pts',(-20.5730157601791,-20.7985582253669,
123.03120703151)) ;
#52137 = CARTESIAN_POINT('Ctrl Pts',(-20.8639502683867,-20.6185691448865,
122.936042849548)) ;
#52138 = CARTESIAN_POINT('Ctrl Pts',(-20.3735473898492,-20.8184813879721,
122.657531564048)) ;
#52139 = CARTESIAN_POINT('Ctrl Pts',(-20.6146112120165,-20.6384923074917,
122.468951374425)) ;
#52140 = CARTESIAN_POINT('Ctrl Pts',(-20.0594536899428,-20.8383715103787,
122.374229560323)) ;
#52141 = CARTESIAN_POINT('Ctrl Pts',(-20.2219924332169,-20.6583824298982,
122.114827126758)) ;
#52142 = CARTESIAN_POINT('Ctrl Pts',(-19.6652757918242,-20.8583764639788,
122.21454943932)) ;
#52143 = CARTESIAN_POINT('Ctrl Pts',(-19.7292685933043,-20.6783873834983,
121.915230361373)) ;
#52144 = CARTESIAN_POINT('Ctrl Pts',(-19.2436756516205,-20.8782147209944,
122.198755207655)) ;
#52145 = CARTESIAN_POINT('Ctrl Pts',(-19.2022698837424,-20.6982256405139,
121.895490958005)) ;
#52146 = CARTESIAN_POINT('Ctrl Pts',(-18.8388276678669,-20.8982090217809,
122.328339296805)) ;
#52147 = CARTESIAN_POINT('Ctrl Pts',(-18.6962108823091,-20.7182199413004,
122.05747386277)) ;
#52148 = CARTESIAN_POINT('Ctrl Pts',(-18.5045195812377,-20.9180942638254,
122.587219380678)) ;
#52149 = CARTESIAN_POINT('Ctrl Pts',(-18.2783285951133,-20.7381051833449,
122.381075560739)) ;
#52150 = CARTESIAN_POINT('Ctrl Pts',(-18.2777383338491,-20.9379692103013,
122.943809989293)) ;
#52151 = CARTESIAN_POINT('Ctrl Pts',(-17.9948546691342,-20.7579801298208,
122.826813664057)) ;
#52152 = CARTESIAN_POINT('Ctrl Pts',(-18.1858465710656,-20.9580022802424,
123.359778806522)) ;
#52153 = CARTESIAN_POINT('Ctrl Pts',(-17.8799919146204,-20.7780131997619,
123.34677562979)) ;
#52154 = CARTESIAN_POINT('Ctrl Pts',(-18.2415322925881,-20.9778907871428,
123.778943620506)) ;
#52155 = CARTESIAN_POINT('Ctrl Pts',(-17.9496011376497,-20.7979017066623,
123.870729922747)) ;
#52156 = CARTESIAN_POINT('Ctrl Pts',(-18.4353283530407,-20.9977456469241,
124.154075261847)) ;
#52157 = CARTESIAN_POINT('Ctrl Pts',(-18.1918462217504,-20.8177565664436,
124.339642131921)) ;
#52158 = CARTESIAN_POINT('Ctrl Pts',(-18.7489158886705,-21.0177964807118,
124.442758777326)) ;
#52159 = CARTESIAN_POINT('Ctrl Pts',(-18.5838321067188,-20.8378074002313,
124.700496054301)) ;
#52160 = CARTESIAN_POINT('Ctrl Pts',(-19.136624015985,-21.037562422601,124.605282240514)) ;
#52161 = CARTESIAN_POINT('Ctrl Pts',(-19.0684642767864,-20.8575733421206,
124.903648312077)) ;
#52162 = CARTESIAN_POINT('Ctrl Pts',(-19.5614777516072,-21.0575751540604,
124.626836375853)) ;
#52163 = CARTESIAN_POINT('Ctrl Pts',(-19.5995315082897,-20.8775860735799,
124.930591112367)) ;
#52164 = CARTESIAN_POINT('Ctrl Pts',(-19.9658070655714,-21.0774679890039,
124.50224819763)) ;
#52165 = CARTESIAN_POINT('Ctrl Pts',(-20.1049415620224,-20.8974789085235,
124.77485635548)) ;
#52166 = CARTESIAN_POINT('Ctrl Pts',(-20.3038411949213,-21.0973750123435,
124.247672615778)) ;
#52167 = CARTESIAN_POINT('Ctrl Pts',(-20.5274834957616,-20.917385931863,124.45663837145)) ;
#52168 = CARTESIAN_POINT('Ctrl Pts',(-20.5353184672274,-21.1172902772442,
123.892968169314)) ;
#52169 = CARTESIAN_POINT('Ctrl Pts',(-20.8168305786149,-20.9373011967637,
124.013259477154)) ;
#52170 = CARTESIAN_POINT('Ctrl Pts',(-20.6318648780347,-21.1373219694039,
123.478162570319)) ;
#52171 = CARTESIAN_POINT('Ctrl Pts',(-20.9375148306312,-20.9573328889234,
123.494752291658)) ;
#52172 = CARTESIAN_POINT('Ctrl Pts',(-20.5815599947794,-21.1571650159769,
123.059210144883)) ;
#52173 = CARTESIAN_POINT('Ctrl Pts',(-20.874635385849,-20.9771759354964,122.971063764394)) ;
#52174 = CARTESIAN_POINT('Ctrl Pts',(-20.3915208487305,-21.1770815638767,
122.680835228278)) ;
#52175 = CARTESIAN_POINT('Ctrl Pts',(-20.6370889548768,-20.9970924833962,
122.498095047605)) ;
#52176 = CARTESIAN_POINT('Ctrl Pts',(-20.083403861949,-21.197013806868,122.389779528303)) ;
#52177 = CARTESIAN_POINT('Ctrl Pts',(-20.2519449230364,-21.0170247263875,
122.134274226548)) ;
#52178 = CARTESIAN_POINT('Ctrl Pts',(-19.69516019848,-21.2169176416773,122.221394595349)) ;
#52179 = CARTESIAN_POINT('Ctrl Pts',(-19.7666424549111,-21.0369285611968,
121.923791009996)) ;
#52180 = CARTESIAN_POINT('Ctrl Pts',(-19.2728466795046,-21.2368180418648,
122.195076901029)) ;
#52181 = CARTESIAN_POINT('Ctrl Pts',(-19.2387517746074,-21.0568289613843,
121.890890792198)) ;
#52182 = CARTESIAN_POINT('Ctrl Pts',(-18.8658292690085,-21.2567677182441,
122.314583734304)) ;
#52183 = CARTESIAN_POINT('Ctrl Pts',(-18.7299794805959,-21.0767786377636,
122.040270945646)) ;
#52184 = CARTESIAN_POINT('Ctrl Pts',(-18.5243803368553,-21.2767002424645,
122.565662246867)) ;
#52185 = CARTESIAN_POINT('Ctrl Pts',(-18.3031667101425,-21.096711161984,122.354115893551)) ;
#52186 = CARTESIAN_POINT('Ctrl Pts',(-18.288939857507,-21.2966202514507,122.917786612455)) ;
#52187 = CARTESIAN_POINT('Ctrl Pts',(-18.0088633207704,-21.1166311709702,
122.794268679454)) ;
#52188 = CARTESIAN_POINT('Ctrl Pts',(-18.1876872131217,-21.3165771576268,
123.329823315717)) ;
#52189 = CARTESIAN_POINT('Ctrl Pts',(-17.8822937306169,-21.1365880771464,
123.309313272752)) ;
#52190 = CARTESIAN_POINT('Ctrl Pts',(-18.2325869540117,-21.3364629971283,
123.750340197414)) ;
#52191 = CARTESIAN_POINT('Ctrl Pts',(-17.9384143244842,-21.1564739166479,
123.834958994866)) ;
#52192 = CARTESIAN_POINT('Ctrl Pts',(-18.4190587415346,-21.3564341692642,
124.131743478507)) ;
#52193 = CARTESIAN_POINT('Ctrl Pts',(-18.1714993858125,-21.1764450887837,
124.311714842778)) ;
#52194 = CARTESIAN_POINT('Ctrl Pts',(-18.721795903564,-21.3762483662486,124.42483382689)) ;
#52195 = CARTESIAN_POINT('Ctrl Pts',(-18.5499193846094,-21.1962592857681,
124.678080172102)) ;
#52196 = CARTESIAN_POINT('Ctrl Pts',(-19.109257994725,-21.3962295522168,124.59893775336)) ;
#52197 = CARTESIAN_POINT('Ctrl Pts',(-19.0342352621433,-21.2162404717363,
124.895714964124)) ;
#52198 = CARTESIAN_POINT('Ctrl Pts',(-19.460775786385,-21.4128050576061,124.624819419925)) ;
#52199 = CARTESIAN_POINT('Ctrl Pts',(-19.4736619237856,-21.2328159771256,
124.928069751386)) ;
#52200 = CARTESIAN_POINT('Ctrl Pts',(-19.7357438512233,-21.4261145054697,
124.572846707991)) ;
#52201 = CARTESIAN_POINT('Ctrl Pts',(-19.8173383619621,-21.2461254249892,
124.863112509831)) ;
#52202 = CARTESIAN_POINT('Ctrl Pts',(-19.9985231275647,-21.4394822032463,
124.473349278481)) ;
#52203 = CARTESIAN_POINT('Ctrl Pts',(-20.1458733463898,-21.2594931227658,
124.73871434383)) ;
#52204 = CARTESIAN_POINT('Ctrl Pts',(-20.2833722213967,-21.4559727749122,
124.268798347122)) ;
#52205 = CARTESIAN_POINT('Ctrl Pts',(-20.5018728443593,-21.2759836944317,
124.483060829802)) ;
#52206 = CARTESIAN_POINT('Ctrl Pts',(-20.5233223205152,-21.475893047245,123.919846821527)) ;
#52207 = CARTESIAN_POINT('Ctrl Pts',(-20.8018337603635,-21.2959039667645,
124.046874735423)) ;
#52208 = CARTESIAN_POINT('Ctrl Pts',(-20.6120012444767,-21.492510082966,123.577832825468)) ;
#52209 = CARTESIAN_POINT('Ctrl Pts',(-20.9126872839273,-21.3125210024855,
123.619326861739)) ;
#52210 = CARTESIAN_POINT('Ctrl Pts',(-20.6099160380865,-21.5058009332471,
123.298380195676)) ;
#52211 = CARTESIAN_POINT('Ctrl Pts',(-20.9100801366087,-21.3258118527666,
123.27004113055)) ;
#52212 = CARTESIAN_POINT('Ctrl Pts',(-20.5720819647299,-21.5157699784016,
123.092270132128)) ;
#52213 = CARTESIAN_POINT('Ctrl Pts',(-20.8627908878946,-21.3357808979211,
123.012396956888)) ;
#52214 = CARTESIAN_POINT('Ctrl Pts',(-20.499885467458,-21.5256733690351,122.8969600671)) ;
#52215 = CARTESIAN_POINT('Ctrl Pts',(-20.7725483588989,-21.3456842885546,
122.768260657527)) ;
#52216 = CARTESIAN_POINT('Ctrl Pts',(-20.3931639686196,-21.5357311551478,
122.714452129114)) ;
#52217 = CARTESIAN_POINT('Ctrl Pts',(-20.6391462594904,-21.3557420746674,
122.540122041308)) ;
#52218 = CARTESIAN_POINT('Ctrl Pts',(-20.2592745444822,-21.5455831917976,
122.556386418772)) ;
#52219 = CARTESIAN_POINT('Ctrl Pts',(-20.4717962814078,-21.3655941113171,
122.342544854286)) ;
#52220 = CARTESIAN_POINT('Ctrl Pts',(-20.0435430288408,-21.5589483159408,
122.376446565359)) ;
#52221 = CARTESIAN_POINT('Ctrl Pts',(-20.2020865685586,-21.3789592354603,
122.117585029482)) ;
#52222 = CARTESIAN_POINT('Ctrl Pts',(-19.7882330766326,-21.5721743789038,
122.25842779773)) ;
#52223 = CARTESIAN_POINT('Ctrl Pts',(-19.8829746643488,-21.3921852984233,
121.970083355878)) ;
#52224 = CARTESIAN_POINT('Ctrl Pts',(-19.512730849252,-21.5854780271861,122.210256078633)) ;
#52225 = CARTESIAN_POINT('Ctrl Pts',(-19.5386166648438,-21.4054889467056,
121.909867161661)) ;
#52226 = CARTESIAN_POINT('Ctrl Pts',(-19.3026540676817,-21.5954695583491,
122.210450686566)) ;
#52227 = CARTESIAN_POINT('Ctrl Pts',(-19.2760167649021,-21.4154804778686,
121.910107183446)) ;
#52228 = CARTESIAN_POINT('Ctrl Pts',(-19.0948968921359,-21.6055090061484,
122.247567522211)) ;
#52229 = CARTESIAN_POINT('Ctrl Pts',(-19.0163207495948,-21.4255199256679,
121.956500605288)) ;
#52230 = CARTESIAN_POINT('Ctrl Pts',(-18.9004687004283,-21.6153527816622,
122.318496927726)) ;
#52231 = CARTESIAN_POINT('Ctrl Pts',(-18.7732843138488,-21.4353637011818,
122.04515967745)) ;
#52232 = CARTESIAN_POINT('Ctrl Pts',(-18.7185579083454,-21.6253384230499,
122.423213533386)) ;
#52233 = CARTESIAN_POINT('Ctrl Pts',(-18.5458944196074,-21.4453493425694,
122.17605303618)) ;
#52234 = CARTESIAN_POINT('Ctrl Pts',(-18.5582565476501,-21.6352752074117,
122.557220506057)) ;
#52235 = CARTESIAN_POINT('Ctrl Pts',(-18.3455158401512,-21.4552861269312,
122.343559635606)) ;
#52236 = CARTESIAN_POINT('Ctrl Pts',(-18.4222459587121,-21.645325041879,122.718871713832)) ;
#52237 = CARTESIAN_POINT('Ctrl Pts',(-18.1755004122376,-21.4653359613986,
122.545621876998)) ;
#52238 = CARTESIAN_POINT('Ctrl Pts',(-18.3183162605906,-21.6551754913822,
122.898008987532)) ;
#52239 = CARTESIAN_POINT('Ctrl Pts',(-18.0455857950081,-21.4751864109017,
122.769542152805)) ;
#52240 = CARTESIAN_POINT('Ctrl Pts',(-18.2456911500029,-21.6651475053643,
123.09464249712)) ;
#52241 = CARTESIAN_POINT('Ctrl Pts',(-17.9548017335226,-21.4851584248838,
123.015333175384)) ;
#52242 = CARTESIAN_POINT('Ctrl Pts',(-18.2082412582699,-21.6751426632114,
123.301442369805)) ;
#52243 = CARTESIAN_POINT('Ctrl Pts',(-17.9079865987969,-21.4951535827309,
123.273832595286)) ;
#52244 = CARTESIAN_POINT('Ctrl Pts',(-18.2075185297832,-21.6851765895751,
123.512368066183)) ;
#52245 = CARTESIAN_POINT('Ctrl Pts',(-17.9070803716444,-21.5051875090946,
123.537489745404)) ;
#52246 = CARTESIAN_POINT('Ctrl Pts',(-18.2424799085402,-21.6950322980075,
123.716614333339)) ;
#52247 = CARTESIAN_POINT('Ctrl Pts',(-17.9507793756721,-21.515043217527,123.792798278283)) ;
#52248 = CARTESIAN_POINT('Ctrl Pts',(-18.3130824839469,-21.7050304473461,
123.914559389374)) ;
#52249 = CARTESIAN_POINT('Ctrl Pts',(-18.0390300006346,-21.5250413668657,
124.040230621224)) ;
#52250 = CARTESIAN_POINT('Ctrl Pts',(-18.4158251214299,-21.7149298505197,
124.095582065844)) ;
#52251 = CARTESIAN_POINT('Ctrl Pts',(-18.1674560176647,-21.5349407700392,
124.266510551727)) ;
#52252 = CARTESIAN_POINT('Ctrl Pts',(-18.5504028728454,-21.7249810474082,
124.258463624392)) ;
#52253 = CARTESIAN_POINT('Ctrl Pts',(-18.3356760698946,-21.5449919669277,
124.470114255126)) ;
#52254 = CARTESIAN_POINT('Ctrl Pts',(-18.7085246366495,-21.734863371221,124.393249383885)) ;
#52255 = CARTESIAN_POINT('Ctrl Pts',(-18.5333267196021,-21.5548742907406,
124.638598757011)) ;
#52256 = CARTESIAN_POINT('Ctrl Pts',(-18.8894290935753,-21.7448582668776,
124.500128199222)) ;
#52257 = CARTESIAN_POINT('Ctrl Pts',(-18.7594560017684,-21.5648691863972,
124.772199668162)) ;
#52258 = CARTESIAN_POINT('Ctrl Pts',(-19.0867831919036,-21.7548793662602,
124.573882631177)) ;
#52259 = CARTESIAN_POINT('Ctrl Pts',(-19.0061476935039,-21.5748902857797,
124.864395292446)) ;
#52260 = CARTESIAN_POINT('Ctrl Pts',(-19.2915499840716,-21.7647866341222,
124.611973404616)) ;
#52261 = CARTESIAN_POINT('Ctrl Pts',(-19.2621059878413,-21.5847975536418,
124.912011501778)) ;
#52262 = CARTESIAN_POINT('Ctrl Pts',(-19.5004581738309,-21.7747249779475,
124.614356734753)) ;
#52263 = CARTESIAN_POINT('Ctrl Pts',(-19.5232414618439,-21.594735897467,124.914993347379)) ;
#52264 = CARTESIAN_POINT('Ctrl Pts',(-19.7080148034449,-21.784728397248,124.580333186118)) ;
#52265 = CARTESIAN_POINT('Ctrl Pts',(-19.782687760914,-21.6047393167675,124.872466522489)) ;
#52266 = CARTESIAN_POINT('Ctrl Pts',(-19.9069801683133,-21.7947629479551,
124.510252770105)) ;
#52267 = CARTESIAN_POINT('Ctrl Pts',(-20.0313953526975,-21.6147738674746,
124.784868563619)) ;
#52268 = CARTESIAN_POINT('Ctrl Pts',(-20.0874764819987,-21.8046078975607,
124.408942640164)) ;
#52269 = CARTESIAN_POINT('Ctrl Pts',(-20.2570175362163,-21.6246188170802,
124.658232944639)) ;
#52270 = CARTESIAN_POINT('Ctrl Pts',(-20.2501460126216,-21.8145937396736,
124.276289518342)) ;
#52271 = CARTESIAN_POINT('Ctrl Pts',(-20.4603562192985,-21.6346046591931,
124.492418458019)) ;
#52272 = CARTESIAN_POINT('Ctrl Pts',(-20.3867706955757,-21.8245285470427,
124.118261781283)) ;
#52273 = CARTESIAN_POINT('Ctrl Pts',(-20.6311392303299,-21.6445394665622,
124.294885221629)) ;
#52274 = CARTESIAN_POINT('Ctrl Pts',(-20.4950064678875,-21.834586088756,123.936658959793)) ;
#52275 = CARTESIAN_POINT('Ctrl Pts',(-20.766436127896,-21.6545970082755,124.067883129763)) ;
#52276 = CARTESIAN_POINT('Ctrl Pts',(-20.568620634059,-21.8444076862681,123.743721916865)) ;
#52277 = CARTESIAN_POINT('Ctrl Pts',(-20.8584564950463,-21.6644186057876,
123.826712005231)) ;
#52278 = CARTESIAN_POINT('Ctrl Pts',(-20.6089246273583,-21.8544639457486,
123.53620346997)) ;
#52279 = CARTESIAN_POINT('Ctrl Pts',(-20.9088388980703,-21.6744748652681,
123.567314526505)) ;
#52280 = CARTESIAN_POINT('Ctrl Pts',(-20.6121758192455,-21.864403882049,123.327248711453)) ;
#52281 = CARTESIAN_POINT('Ctrl Pts',(-20.9129054423695,-21.6844148015685,
123.306120784304)) ;
#52282 = CARTESIAN_POINT('Ctrl Pts',(-20.5798268668381,-21.8743110027934,
123.121499920529)) ;
#52283 = CARTESIAN_POINT('Ctrl Pts',(-20.8724715627851,-21.6943219223129,
123.048933898869)) ;
#52284 = CARTESIAN_POINT('Ctrl Pts',(-20.5112454372603,-21.8843539087187,
122.921820528397)) ;
#52285 = CARTESIAN_POINT('Ctrl Pts',(-20.7867471088795,-21.7043648282382,
122.799333949638)) ;
#52286 = CARTESIAN_POINT('Ctrl Pts',(-20.4104399306398,-21.8942616898179,
122.739536472857)) ;
#52287 = CARTESIAN_POINT('Ctrl Pts',(-20.6607421012304,-21.7142726093374,
122.571477249499)) ;
#52288 = CARTESIAN_POINT('Ctrl Pts',(-20.2784482766661,-21.9042720588203,
122.57561542797)) ;
#52289 = CARTESIAN_POINT('Ctrl Pts',(-20.4957543257105,-21.7242829783398,
122.366574426196)) ;
#52290 = CARTESIAN_POINT('Ctrl Pts',(-20.1193995034889,-21.9143028973891,
122.437148355259)) ;
#52291 = CARTESIAN_POINT('Ctrl Pts',(-20.2969450013414,-21.7343138169086,
122.19348877068)) ;
#52292 = CARTESIAN_POINT('Ctrl Pts',(-19.9421174960905,-21.9241557370288,
122.33000905002)) ;
#52293 = CARTESIAN_POINT('Ctrl Pts',(-20.0753430041324,-21.7441666565483,
122.059562188737)) ;
#52294 = CARTESIAN_POINT('Ctrl Pts',(-19.7464337621037,-21.9341437381937,
122.253902994198)) ;
#52295 = CARTESIAN_POINT('Ctrl Pts',(-19.8307389892566,-21.7541546577133,
121.964427436232)) ;
#52296 = CARTESIAN_POINT('Ctrl Pts',(-19.5417073868984,-21.9440725571729,
122.213164409012)) ;
#52297 = CARTESIAN_POINT('Ctrl Pts',(-19.574830987795,-21.7640834766924,121.913501885693)) ;
#52298 = CARTESIAN_POINT('Ctrl Pts',(-19.3317819851724,-21.9540602598952,
122.208211065697)) ;
#52299 = CARTESIAN_POINT('Ctrl Pts',(-19.3124241042316,-21.7740711794147,
121.907308023859)) ;
#52300 = CARTESIAN_POINT('Ctrl Pts',(-19.1232546991255,-21.9640962596979,
122.240283219505)) ;
#52301 = CARTESIAN_POINT('Ctrl Pts',(-19.0517647366953,-21.7841071792174,
121.94739595785)) ;
#52302 = CARTESIAN_POINT('Ctrl Pts',(-18.9269352967466,-21.9739511294993,
122.306534700964)) ;
#52303 = CARTESIAN_POINT('Ctrl Pts',(-18.8063639186395,-21.7939620490188,
122.030208536967)) ;
#52304 = CARTESIAN_POINT('Ctrl Pts',(-18.7423427052336,-21.9839505599228,
122.407048270959)) ;
#52305 = CARTESIAN_POINT('Ctrl Pts',(-18.5756220535138,-21.8039614794424,
122.155848712689)) ;
#52306 = CARTESIAN_POINT('Ctrl Pts',(-18.5795278154634,-21.9938456773881,
122.536588268655)) ;
#52307 = CARTESIAN_POINT('Ctrl Pts',(-18.3721015981138,-21.8138565969077,
122.31777256952)) ;
#52308 = CARTESIAN_POINT('Ctrl Pts',(-18.4394307306069,-22.0039061709051,
122.695002768727)) ;
#52309 = CARTESIAN_POINT('Ctrl Pts',(-18.1969788649172,-21.8239170904246,
122.515789156967)) ;
#52310 = CARTESIAN_POINT('Ctrl Pts',(-18.3311666833367,-22.0137556511063,
122.871529628342)) ;
#52311 = CARTESIAN_POINT('Ctrl Pts',(-18.0616465447384,-21.8337665706258,
122.736447563555)) ;
#52312 = CARTESIAN_POINT('Ctrl Pts',(-18.253333217475,-22.0237821013701,123.067418185129)) ;
#52313 = CARTESIAN_POINT('Ctrl Pts',(-17.9643529995753,-21.8437930208896,
122.981307539506)) ;
#52314 = CARTESIAN_POINT('Ctrl Pts',(-18.2112421000978,-22.0338133918482,
123.274069161545)) ;
#52315 = CARTESIAN_POINT('Ctrl Pts',(-17.9117371291873,-21.8538243113677,
123.239620782799)) ;
#52316 = CARTESIAN_POINT('Ctrl Pts',(-18.2053271335064,-22.0436547795,123.480882845049)) ;
#52317 = CARTESIAN_POINT('Ctrl Pts',(-17.9043414973988,-21.8636656990195,
123.498138969847)) ;
#52318 = CARTESIAN_POINT('Ctrl Pts',(-18.235499498762,-22.0536581803912,123.688988918486)) ;
#52319 = CARTESIAN_POINT('Ctrl Pts',(-17.9420552178321,-21.8736690999107,
123.758271923752)) ;
#52320 = CARTESIAN_POINT('Ctrl Pts',(-18.3013232908441,-22.0636425631824,
123.88834285791)) ;
#52321 = CARTESIAN_POINT('Ctrl Pts',(-18.0243333210938,-21.8836534827019,
124.007465107923)) ;
#52322 = CARTESIAN_POINT('Ctrl Pts',(-18.4014559554124,-22.0736816531958,
124.074106712805)) ;
#52323 = CARTESIAN_POINT('Ctrl Pts',(-18.1494974493961,-21.8936925727153,
124.239670692976)) ;
#52324 = CARTESIAN_POINT('Ctrl Pts',(-18.5295972273494,-22.0835274621049,
124.236682169581)) ;
#52325 = CARTESIAN_POINT('Ctrl Pts',(-18.3096733741346,-21.9035383816245,
124.442892027309)) ;
#52326 = CARTESIAN_POINT('Ctrl Pts',(-18.6858761362846,-22.0935118849239,
124.376767470781)) ;
#52327 = CARTESIAN_POINT('Ctrl Pts',(-18.5050211084145,-21.9135228044435,
124.6180000343)) ;
#52328 = CARTESIAN_POINT('Ctrl Pts',(-18.8633080302938,-22.1034515101651,
124.487199990123)) ;
#52329 = CARTESIAN_POINT('Ctrl Pts',(-18.7268105925925,-21.9234624296847,
124.756042327827)) ;
#52330 = CARTESIAN_POINT('Ctrl Pts',(-19.0591476044493,-22.1134911996838,
124.565868443362)) ;
#52331 = CARTESIAN_POINT('Ctrl Pts',(-18.97160932169,-21.9335021192033,124.854379340784)) ;
#52332 = CARTESIAN_POINT('Ctrl Pts',(-19.2625612087232,-22.1233793881024,
124.608789289149)) ;
#52333 = CARTESIAN_POINT('Ctrl Pts',(-19.2258769015398,-21.9433903076219,
124.908032136519)) ;
#52334 = CARTESIAN_POINT('Ctrl Pts',(-19.4724346347167,-22.1333689141044,
124.616203338408)) ;
#52335 = CARTESIAN_POINT('Ctrl Pts',(-19.4882188467866,-21.953379833624,124.91730115363)) ;
#52336 = CARTESIAN_POINT('Ctrl Pts',(-19.6797404481245,-22.1433274154596,
124.586994703036)) ;
#52337 = CARTESIAN_POINT('Ctrl Pts',(-19.7473517520764,-21.9633383349792,
124.880791790202)) ;
#52338 = CARTESIAN_POINT('Ctrl Pts',(-19.8778238010788,-22.1532270094633,
124.523101680733)) ;
#52339 = CARTESIAN_POINT('Ctrl Pts',(-19.9949571853938,-21.9732379289828,
124.800926502776)) ;
#52340 = CARTESIAN_POINT('Ctrl Pts',(-20.0644952954339,-22.1632748975846,
124.424277452298)) ;
#52341 = CARTESIAN_POINT('Ctrl Pts',(-20.2282969936015,-21.9832858171041,
124.677397513745)) ;
#52342 = CARTESIAN_POINT('Ctrl Pts',(-20.2287857483374,-22.1731703228301,
124.296606248266)) ;
#52343 = CARTESIAN_POINT('Ctrl Pts',(-20.4336615726803,-21.9931812423496,
124.517808969355)) ;
#52344 = CARTESIAN_POINT('Ctrl Pts',(-20.3707381562611,-22.1832317135307,
124.139823950091)) ;
#52345 = CARTESIAN_POINT('Ctrl Pts',(-20.6111028162825,-22.0032426330502,
124.3218322011)) ;
#52346 = CARTESIAN_POINT('Ctrl Pts',(-20.4809482851262,-22.1930772972174,
123.964606584726)) ;
#52347 = CARTESIAN_POINT('Ctrl Pts',(-20.7488672565389,-22.0130882167369,
124.102810049163)) ;
#52348 = CARTESIAN_POINT('Ctrl Pts',(-20.5606363459277,-22.2030402705266,
123.770920839856)) ;
#52349 = CARTESIAN_POINT('Ctrl Pts',(-20.8484784323989,-22.0230511900461,
123.860702848423)) ;
#52350 = CARTESIAN_POINT('Ctrl Pts',(-20.605498138732,-22.2130659373523,123.564965764745)) ;
#52351 = CARTESIAN_POINT('Ctrl Pts',(-20.9045567469638,-22.0330768568719,
123.603259320329)) ;
#52352 = CARTESIAN_POINT('Ctrl Pts',(-20.6139362962588,-22.2229804152186,
123.356710312389)) ;
#52353 = CARTESIAN_POINT('Ctrl Pts',(-20.9151055480402,-22.0429913347382,
123.342939247578)) ;
#52354 = CARTESIAN_POINT('Ctrl Pts',(-20.5862899774463,-22.2329689298936,
123.148530954525)) ;
#52355 = CARTESIAN_POINT('Ctrl Pts',(-20.8805485315078,-22.0529798494131,
123.082714706899)) ;
#52356 = CARTESIAN_POINT('Ctrl Pts',(-20.5221446354155,-22.2430130408091,
122.947370956092)) ;
#52357 = CARTESIAN_POINT('Ctrl Pts',(-20.8003679519831,-22.0630239603286,
122.831264561791)) ;
#52358 = CARTESIAN_POINT('Ctrl Pts',(-20.4265781092213,-22.2528411784036,
122.764149083107)) ;
#52359 = CARTESIAN_POINT('Ctrl Pts',(-20.6809098954698,-22.0728520979232,
122.602235481541)) ;
#52360 = CARTESIAN_POINT('Ctrl Pts',(-20.2975883675018,-22.2629177464626,
122.596160440805)) ;
#52361 = CARTESIAN_POINT('Ctrl Pts',(-20.5196736796909,-22.0829286659821,
122.392249516322)) ;
#52362 = CARTESIAN_POINT('Ctrl Pts',(-20.1448753794696,-22.2727699083667,
122.456169185964)) ;
#52363 = CARTESIAN_POINT('Ctrl Pts',(-20.3287820285072,-22.0927808278863,
122.217258955641)) ;
#52364 = CARTESIAN_POINT('Ctrl Pts',(-19.9664229552607,-22.2828428703236,
122.342221971823)) ;
#52365 = CARTESIAN_POINT('Ctrl Pts',(-20.1057172726509,-22.1028537898431,
122.074824536813)) ;
#52366 = CARTESIAN_POINT('Ctrl Pts',(-19.7753081970072,-22.2926854323265,
122.26285604015)) ;
#52367 = CARTESIAN_POINT('Ctrl Pts',(-19.8668228113996,-22.112696351846,121.975615871241)) ;
#52368 = CARTESIAN_POINT('Ctrl Pts',(-19.5706672880173,-22.3026658688203,
122.216568225967)) ;
#52369 = CARTESIAN_POINT('Ctrl Pts',(-19.6110214816396,-22.1226767883398,
121.91775555396)) ;
#52370 = CARTESIAN_POINT('Ctrl Pts',(-19.3602768856682,-22.3126841741447,
122.206883478724)) ;
#52371 = CARTESIAN_POINT('Ctrl Pts',(-19.3480335183731,-22.1326950936642,
121.90564896849)) ;
#52372 = CARTESIAN_POINT('Ctrl Pts',(-19.1541230507367,-22.3225681380641,
122.233089766057)) ;
#52373 = CARTESIAN_POINT('Ctrl Pts',(-19.0903400796923,-22.1425790575837,
121.938406486908)) ;
#52374 = CARTESIAN_POINT('Ctrl Pts',(-18.9520588230378,-22.3326340148027,
122.295865398734)) ;
#52375 = CARTESIAN_POINT('Ctrl Pts',(-18.8377600204012,-22.1526449343222,
122.016875429247)) ;
#52376 = CARTESIAN_POINT('Ctrl Pts',(-18.7681011669116,-22.3424731156636,
122.390486931831)) ;
#52377 = CARTESIAN_POINT('Ctrl Pts',(-18.6078114381129,-22.1624840351831,
122.135152615045)) ;
#52378 = CARTESIAN_POINT('Ctrl Pts',(-18.5998200970519,-22.3525061985293,
122.517638100478)) ;
#52379 = CARTESIAN_POINT('Ctrl Pts',(-18.3974600456383,-22.1725171180488,
122.29409131668)) ;
#52380 = CARTESIAN_POINT('Ctrl Pts',(-18.4567024912476,-22.3625278838048,
122.672277268552)) ;
#52381 = CARTESIAN_POINT('Ctrl Pts',(-18.2185627412109,-22.1825388033243,
122.487389938012)) ;
#52382 = CARTESIAN_POINT('Ctrl Pts',(-18.3441099722616,-22.3723945789033,
122.846470293017)) ;
#52383 = CARTESIAN_POINT('Ctrl Pts',(-18.0778211452312,-22.1924054984228,
122.705132096587)) ;
#52384 = CARTESIAN_POINT('Ctrl Pts',(-18.2621912773549,-22.3823544686378,
123.039178686657)) ;
#52385 = CARTESIAN_POINT('Ctrl Pts',(-17.97542250724,-22.2023653881573,122.946017980709)) ;
#52386 = CARTESIAN_POINT('Ctrl Pts',(-18.214942034536,-22.3923894564633,123.2447729843)) ;
#52387 = CARTESIAN_POINT('Ctrl Pts',(-17.9163607640091,-22.2124003759828,
123.203010659007)) ;
#52388 = CARTESIAN_POINT('Ctrl Pts',(-18.2039207070877,-22.4022761605376,
123.452359252462)) ;
#52389 = CARTESIAN_POINT('Ctrl Pts',(-17.9025839572868,-22.2222870800571,
123.462494584702)) ;
#52390 = CARTESIAN_POINT('Ctrl Pts',(-18.2296104639163,-22.4123413047705,
123.662360780197)) ;
#52391 = CARTESIAN_POINT('Ctrl Pts',(-17.9346959978912,-22.23235222429,123.724996117195)) ;
#52392 = CARTESIAN_POINT('Ctrl Pts',(-18.2898035554938,-22.422180595499,123.860294782693)) ;
#52393 = CARTESIAN_POINT('Ctrl Pts',(-18.009937769009,-22.2421915150186,123.972415043935)) ;
#52394 = CARTESIAN_POINT('Ctrl Pts',(-18.3852909858274,-22.4322431529375,
124.049037318576)) ;
#52395 = CARTESIAN_POINT('Ctrl Pts',(-18.1292969689133,-22.252254072457,124.208342841575)) ;
#52396 = CARTESIAN_POINT('Ctrl Pts',(-18.5102142780944,-22.4421402041896,
124.215443211625)) ;
#52397 = CARTESIAN_POINT('Ctrl Pts',(-18.2854516847869,-22.2621511237091,
124.416351010957)) ;
#52398 = CARTESIAN_POINT('Ctrl Pts',(-18.6621688535695,-22.4520714109378,
124.358617696287)) ;
#52399 = CARTESIAN_POINT('Ctrl Pts',(-18.4753956188901,-22.2720823304574,
124.595319409378)) ;
#52400 = CARTESIAN_POINT('Ctrl Pts',(-18.8387544421233,-22.4621135951567,
124.474321570263)) ;
#52401 = CARTESIAN_POINT('Ctrl Pts',(-18.6961275310475,-22.2821245146762,
124.739948983759)) ;
#52402 = CARTESIAN_POINT('Ctrl Pts',(-19.0296939400006,-22.4720002232676,
124.556460841573)) ;
#52403 = CARTESIAN_POINT('Ctrl Pts',(-18.9348029986145,-22.2920111427871,
124.842623278303)) ;
#52404 = CARTESIAN_POINT('Ctrl Pts',(-19.234076559489,-22.4819934958,124.605048925011)) ;
#52405 = CARTESIAN_POINT('Ctrl Pts',(-19.1902815584304,-22.3020044153195,
124.903358057962)) ;
#52406 = CARTESIAN_POINT('Ctrl Pts',(-19.4427962027987,-22.4919385713414,
124.617281907534)) ;
#52407 = CARTESIAN_POINT('Ctrl Pts',(-19.4511817330651,-22.311949490861,124.918648968721)) ;
#52408 = CARTESIAN_POINT('Ctrl Pts',(-19.6506180805942,-22.5018881220697,
124.593481317551)) ;
#52409 = CARTESIAN_POINT('Ctrl Pts',(-19.7109595709045,-22.3218990415892,
124.888897659365)) ;
#52410 = CARTESIAN_POINT('Ctrl Pts',(-19.8528843773795,-22.5119274569177,
124.5332335477)) ;
#52411 = CARTESIAN_POINT('Ctrl Pts',(-19.9637921602865,-22.3319383764372,
124.813587576332)) ;
#52412 = CARTESIAN_POINT('Ctrl Pts',(-20.0388462005348,-22.5218135958616,
124.440381350932)) ;
#52413 = CARTESIAN_POINT('Ctrl Pts',(-20.1962451731678,-22.3418245153811,
124.697521392997)) ;
#52414 = CARTESIAN_POINT('Ctrl Pts',(-20.2078788172091,-22.5318117088353,
124.315489125279)) ;
#52415 = CARTESIAN_POINT('Ctrl Pts',(-20.407535706162,-22.3518226283548,124.541405526316)) ;
#52416 = CARTESIAN_POINT('Ctrl Pts',(-20.3516487618174,-22.5417314711877,
124.164389810808)) ;
#52417 = CARTESIAN_POINT('Ctrl Pts',(-20.5872481936241,-22.3617423907073,
124.352530361896)) ;
#52418 = CARTESIAN_POINT('Ctrl Pts',(-20.4684258196986,-22.5517708668004,
123.98859191938)) ;
#52419 = CARTESIAN_POINT('Ctrl Pts',(-20.7332188477992,-22.3717817863199,
124.13278276774)) ;
#52420 = CARTESIAN_POINT('Ctrl Pts',(-20.5517552452748,-22.5616800525887,
123.797660250607)) ;
#52421 = CARTESIAN_POINT('Ctrl Pts',(-20.8373803850382,-22.3816909721082,
123.894117096707)) ;
#52422 = CARTESIAN_POINT('Ctrl Pts',(-20.6013649615286,-22.5716152367462,
123.594766848094)) ;
#52423 = CARTESIAN_POINT('Ctrl Pts',(-20.8993918234264,-22.3916261562657,
123.640499494851)) ;
#52424 = CARTESIAN_POINT('Ctrl Pts',(-20.6149297753148,-22.5816562941321,
123.384113634597)) ;
#52425 = CARTESIAN_POINT('Ctrl Pts',(-20.9163470245203,-22.4016672136516,
123.377183112354)) ;
#52426 = CARTESIAN_POINT('Ctrl Pts',(-20.5922146510685,-22.5915434521654,
123.177488411578)) ;
#52427 = CARTESIAN_POINT('Ctrl Pts',(-20.8879521473968,-22.4115543716849,
123.118900643908)) ;
#52428 = CARTESIAN_POINT('Ctrl Pts',(-20.5336910768669,-22.6015357318413,
122.975751109046)) ;
#52429 = CARTESIAN_POINT('Ctrl Pts',(-20.8147966668249,-22.4215466513608,
122.866729097571)) ;
#52430 = CARTESIAN_POINT('Ctrl Pts',(-20.4413703874593,-22.6114842488863,
122.788067427756)) ;
#52431 = CARTESIAN_POINT('Ctrl Pts',(-20.6993946934881,-22.4314951684059,
122.632124438187)) ;
#52432 = CARTESIAN_POINT('Ctrl Pts',(-20.3182652486574,-22.6214210264567,
122.619313417233)) ;
#52433 = CARTESIAN_POINT('Ctrl Pts',(-20.5455120188652,-22.4414319459763,
122.4211820476)) ;
#52434 = CARTESIAN_POINT('Ctrl Pts',(-20.1671801256002,-22.6314040626037,
122.473601909739)) ;
#52435 = CARTESIAN_POINT('Ctrl Pts',(-20.3566546114606,-22.4514149821232,
122.239043334053)) ;
#52436 = CARTESIAN_POINT('Ctrl Pts',(-19.991856607727,-22.6414478141974,122.355972854816)) ;
#52437 = CARTESIAN_POINT('Ctrl Pts',(-20.137499793827,-22.4614587337169,122.092007982287)) ;
#52438 = CARTESIAN_POINT('Ctrl Pts',(-19.8030570092897,-22.65127634341,122.271939115384)) ;
#52439 = CARTESIAN_POINT('Ctrl Pts',(-19.9014984820513,-22.4712872629295,
121.986966332183)) ;
#52440 = CARTESIAN_POINT('Ctrl Pts',(-19.5975962709593,-22.6613517043187,
122.220614922131)) ;
#52441 = CARTESIAN_POINT('Ctrl Pts',(-19.6446726698257,-22.4813626238382,
121.922812414235)) ;
#52442 = CARTESIAN_POINT('Ctrl Pts',(-19.3908522666017,-22.6712083032059,
122.205989042453)) ;
#52443 = CARTESIAN_POINT('Ctrl Pts',(-19.3862413607588,-22.4912192227254,
121.904531259396)) ;
#52444 = CARTESIAN_POINT('Ctrl Pts',(-19.1804545485629,-22.6812712972238,
122.227705733918)) ;
#52445 = CARTESIAN_POINT('Ctrl Pts',(-19.1232446772798,-22.5012822167433,
121.931678446453)) ;
#52446 = CARTESIAN_POINT('Ctrl Pts',(-18.9806951570671,-22.6911492315132,
122.284594628893)) ;
#52447 = CARTESIAN_POINT('Ctrl Pts',(-18.8735448281078,-22.5111601510327,
122.002791143705)) ;
#52448 = CARTESIAN_POINT('Ctrl Pts',(-18.7914526517928,-22.7011498790713,
122.376106438856)) ;
#52449 = CARTESIAN_POINT('Ctrl Pts',(-18.6369922198873,-22.5211607985908,
122.117182285902)) ;
#52450 = CARTESIAN_POINT('Ctrl Pts',(-18.6222332954635,-22.7110677255094,
122.497984639726)) ;
#52451 = CARTESIAN_POINT('Ctrl Pts',(-18.425468334263,-22.5310786450289,122.269531684328)) ;
#52452 = CARTESIAN_POINT('Ctrl Pts',(-18.474883672655,-22.721118842515,122.649391564558)) ;
#52453 = CARTESIAN_POINT('Ctrl Pts',(-18.2412825267933,-22.5411297620345,
122.458791235445)) ;
#52454 = CARTESIAN_POINT('Ctrl Pts',(-18.3579599908217,-22.7309895778256,
122.820875939281)) ;
#52455 = CARTESIAN_POINT('Ctrl Pts',(-18.0951286475045,-22.5510004973451,
122.673148447016)) ;
#52456 = CARTESIAN_POINT('Ctrl Pts',(-18.270849081835,-22.7410602850686,123.013805427642)) ;
#52457 = CARTESIAN_POINT('Ctrl Pts',(-17.98624161006,-22.5610712045881,122.914310640353)) ;
#52458 = CARTESIAN_POINT('Ctrl Pts',(-18.2196899669182,-22.7508932925205,
123.214115396645)) ;
#52459 = CARTESIAN_POINT('Ctrl Pts',(-17.9222939722818,-22.57090421204,123.16469974728)) ;
#52460 = CARTESIAN_POINT('Ctrl Pts',(-18.203176745519,-22.7609237848228,123.42433279345)) ;
#52461 = CARTESIAN_POINT('Ctrl Pts',(-17.9016542677263,-22.5809347043423,
123.427471548308)) ;
#52462 = CARTESIAN_POINT('Ctrl Pts',(-18.2240311555207,-22.7709553798962,
123.634206914964)) ;
#52463 = CARTESIAN_POINT('Ctrl Pts',(-17.9277238839754,-22.5909662994157,
123.689813957238)) ;
#52464 = CARTESIAN_POINT('Ctrl Pts',(-18.2794406669794,-22.7807850790344,
123.83327619676)) ;
#52465 = CARTESIAN_POINT('Ctrl Pts',(-17.9969878121301,-22.6007959985539,
123.938651312499)) ;
#52466 = CARTESIAN_POINT('Ctrl Pts',(-18.3694648397809,-22.790774528916,124.023019043572)) ;
#52467 = CARTESIAN_POINT('Ctrl Pts',(-18.1095198727546,-22.6107854484355,
124.175829192089)) ;
#52468 = CARTESIAN_POINT('Ctrl Pts',(-18.4921611930021,-22.8008183867317,
124.194863216364)) ;
#52469 = CARTESIAN_POINT('Ctrl Pts',(-18.2628916856146,-22.6208293062512,
124.39063324651)) ;
#52470 = CARTESIAN_POINT('Ctrl Pts',(-18.6391999982746,-22.8106400773219,
124.339828342554)) ;
#52471 = CARTESIAN_POINT('Ctrl Pts',(-18.4466924341392,-22.6306509968414,
124.571839161944)) ;
#52472 = CARTESIAN_POINT('Ctrl Pts',(-18.8125751270944,-22.8206751678623,
124.460026469785)) ;
#52473 = CARTESIAN_POINT('Ctrl Pts',(-18.6634124376899,-22.6406860873818,
124.722085054606)) ;
#52474 = CARTESIAN_POINT('Ctrl Pts',(-19.0042354854205,-22.830699686845,124.547700241937)) ;
#52475 = CARTESIAN_POINT('Ctrl Pts',(-18.9029886661836,-22.6507106063645,
124.831675526202)) ;
#52476 = CARTESIAN_POINT('Ctrl Pts',(-19.2047392934395,-22.8405595322552,
124.600226995631)) ;
#52477 = CARTESIAN_POINT('Ctrl Pts',(-19.153619877724,-22.6605704517747,124.897332264316)) ;
#52478 = CARTESIAN_POINT('Ctrl Pts',(-19.4133825738018,-22.8505193085708,
124.617890170241)) ;
#52479 = CARTESIAN_POINT('Ctrl Pts',(-19.4144244913009,-22.6705302280904,
124.919409093164)) ;
#52480 = CARTESIAN_POINT('Ctrl Pts',(-19.6233229031397,-22.8605475058855,
124.598638239538)) ;
#52481 = CARTESIAN_POINT('Ctrl Pts',(-19.6768496651642,-22.680558425405,124.895342097839)) ;
#52482 = CARTESIAN_POINT('Ctrl Pts',(-19.8243679055007,-22.8704550481758,
124.544126078897)) ;
#52483 = CARTESIAN_POINT('Ctrl Pts',(-19.9281559636795,-22.6904659676953,
124.827199647168)) ;
#52484 = CARTESIAN_POINT('Ctrl Pts',(-20.0152757096399,-22.8804876987396,
124.454494142613)) ;
#52485 = CARTESIAN_POINT('Ctrl Pts',(-20.1667897462987,-22.7004986182592,
124.715157775253)) ;
#52486 = CARTESIAN_POINT('Ctrl Pts',(-20.1852178949266,-22.8903716551663,
124.33491330894)) ;
#52487 = CARTESIAN_POINT('Ctrl Pts',(-20.379216821132,-22.7103825746858,124.565679509401)) ;
#52488 = CARTESIAN_POINT('Ctrl Pts',(-20.3337523313298,-22.9003613565281,
124.186436934306)) ;
#52489 = CARTESIAN_POINT('Ctrl Pts',(-20.5648833311247,-22.7203722760477,
124.380082284195)) ;
#52490 = CARTESIAN_POINT('Ctrl Pts',(-20.4544985548872,-22.9104023518042,
124.013286908638)) ;
#52491 = CARTESIAN_POINT('Ctrl Pts',(-20.7158142405199,-22.7304132713237,
124.163643560049)) ;
#52492 = CARTESIAN_POINT('Ctrl Pts',(-20.5418120177757,-22.9202352410725,
123.825917664307)) ;
#52493 = CARTESIAN_POINT('Ctrl Pts',(-20.8249543881168,-22.7402461605921,
123.929430163631)) ;
#52494 = CARTESIAN_POINT('Ctrl Pts',(-20.5967197719903,-22.93022839944,123.623135595412)) ;
#52495 = CARTESIAN_POINT('Ctrl Pts',(-20.8935867561145,-22.7502393189595,
123.675951817877)) ;
#52496 = CARTESIAN_POINT('Ctrl Pts',(-20.6152207366922,-22.9402604417921,
123.413033506782)) ;
#52497 = CARTESIAN_POINT('Ctrl Pts',(-20.9167106284998,-22.7602713613116,
123.413324039136)) ;
#52498 = CARTESIAN_POINT('Ctrl Pts',(-20.5975204253957,-22.9501256857505,
123.2064025244)) ;
#52499 = CARTESIAN_POINT('Ctrl Pts',(-20.8945827855904,-22.77013660527,123.155034786058)) ;
#52500 = CARTESIAN_POINT('Ctrl Pts',(-20.5442580745083,-22.9600875769965,
123.003852214581)) ;
#52501 = CARTESIAN_POINT('Ctrl Pts',(-20.8280023410754,-22.780098496516,122.901847296174)) ;
#52502 = CARTESIAN_POINT('Ctrl Pts',(-20.4556884997879,-22.970122477015,122.812391064617)) ;
#52503 = CARTESIAN_POINT('Ctrl Pts',(-20.717288160566,-22.7901333965345,122.662521920289)) ;
#52504 = CARTESIAN_POINT('Ctrl Pts',(-20.3372800803288,-22.9800075574296,
122.641575983214)) ;
#52505 = CARTESIAN_POINT('Ctrl Pts',(-20.5692752426324,-22.8000184769491,
122.449004039096)) ;
#52506 = CARTESIAN_POINT('Ctrl Pts',(-20.1883694042385,-22.9900727295544,
122.491279319789)) ;
#52507 = CARTESIAN_POINT('Ctrl Pts',(-20.3831352082,-22.8100836490739,122.261135086105)) ;
#52508 = CARTESIAN_POINT('Ctrl Pts',(-20.0193951599007,-22.9999199642779,
122.37164075247)) ;
#52509 = CARTESIAN_POINT('Ctrl Pts',(-20.1719153766987,-22.8199308837974,
122.111588554318)) ;
#52510 = CARTESIAN_POINT('Ctrl Pts',(-19.8289685430891,-23.0099507755956,
122.281076764927)) ;
#52511 = CARTESIAN_POINT('Ctrl Pts',(-19.9338810020407,-22.8299616951152,
121.998385955038)) ;
#52512 = CARTESIAN_POINT('Ctrl Pts',(-19.6259877305142,-23.0199603915091,
122.225477205925)) ;
#52513 = CARTESIAN_POINT('Ctrl Pts',(-19.6801542546596,-22.8399713110287,
121.928888950518)) ;
#52514 = CARTESIAN_POINT('Ctrl Pts',(-19.4185677638405,-23.0298711709128,
122.205958909889)) ;
#52515 = CARTESIAN_POINT('Ctrl Pts',(-19.4208786354212,-22.8498820904324,
121.904493618235)) ;
#52516 = CARTESIAN_POINT('Ctrl Pts',(-19.2104507212989,-23.0398004367019,
122.222263809827)) ;
#52517 = CARTESIAN_POINT('Ctrl Pts',(-19.1607322268029,-22.8598113562214,
121.924877430704)) ;
#52518 = CARTESIAN_POINT('Ctrl Pts',(-19.0060800631454,-23.0498431300145,
122.275221685096)) ;
#52519 = CARTESIAN_POINT('Ctrl Pts',(-18.9052696005558,-22.869854049534,121.991077325466)) ;
#52520 = CARTESIAN_POINT('Ctrl Pts',(-18.816920652705,-23.0597296627092,122.361382751279)) ;
#52521 = CARTESIAN_POINT('Ctrl Pts',(-18.6688210507499,-22.8797405822288,
122.098781259374)) ;
#52522 = CARTESIAN_POINT('Ctrl Pts',(-18.6435653180198,-23.0697228078125,
122.480041622256)) ;
#52523 = CARTESIAN_POINT('Ctrl Pts',(-18.4521283291421,-22.889733727332,122.247107144834)) ;
#52524 = CARTESIAN_POINT('Ctrl Pts',(-18.4942067621472,-23.0796684884866,
122.626365687683)) ;
#52525 = CARTESIAN_POINT('Ctrl Pts',(-18.2654318574781,-22.8996794080061,
122.430014319101)) ;
#52526 = CARTESIAN_POINT('Ctrl Pts',(-18.3721507507593,-23.0896157461133,
122.796186530113)) ;
#52527 = CARTESIAN_POINT('Ctrl Pts',(-18.1128639586572,-22.9096266656328,
122.642292140885)) ;
#52528 = CARTESIAN_POINT('Ctrl Pts',(-18.280738860759,-23.0996636482348,122.986614485634)) ;
#52529 = CARTESIAN_POINT('Ctrl Pts',(-17.9986015570663,-22.9196745677543,
122.880328253764)) ;
#52530 = CARTESIAN_POINT('Ctrl Pts',(-18.2247452921894,-23.1095113538565,
123.185929489645)) ;
#52531 = CARTESIAN_POINT('Ctrl Pts',(-17.9286121289633,-22.929522273376,123.129473138882)) ;
#52532 = CARTESIAN_POINT('Ctrl Pts',(-18.203315371917,-23.1194728204906,123.394243964455)) ;
#52533 = CARTESIAN_POINT('Ctrl Pts',(-17.9018275040741,-22.9394837400101,
123.389866643999)) ;
#52534 = CARTESIAN_POINT('Ctrl Pts',(-18.2187690231212,-23.1295023737588,
123.604537566451)) ;
#52535 = CARTESIAN_POINT('Ctrl Pts',(-17.9211473397104,-22.9495132932783,
123.652733485407)) ;
#52536 = CARTESIAN_POINT('Ctrl Pts',(-18.2697520445231,-23.1394092657862,
123.806478018759)) ;
#52537 = CARTESIAN_POINT('Ctrl Pts',(-17.9848788715612,-22.9594201853057,
123.905158576466)) ;
#52538 = CARTESIAN_POINT('Ctrl Pts',(-18.3549970966278,-23.1493569098992,
123.997428173794)) ;
#52539 = CARTESIAN_POINT('Ctrl Pts',(-18.0914378076412,-22.9693678294187,
124.143845240132)) ;
#52540 = CARTESIAN_POINT('Ctrl Pts',(-18.4726356234465,-23.1593569529281,
124.171699257656)) ;
#52541 = CARTESIAN_POINT('Ctrl Pts',(-18.2384883380865,-22.9793678724476,
124.361682579546)) ;
#52542 = CARTESIAN_POINT('Ctrl Pts',(-18.6195515746322,-23.1693957189221,
124.323190189224)) ;
#52543 = CARTESIAN_POINT('Ctrl Pts',(-18.4221353270186,-22.9894066384416,
124.551044334256)) ;
#52544 = CARTESIAN_POINT('Ctrl Pts',(-18.7866669271075,-23.1792207809443,
124.444609990743)) ;
#52545 = CARTESIAN_POINT('Ctrl Pts',(-18.6310313254401,-22.9992317004638,
124.702816918919)) ;
#52546 = CARTESIAN_POINT('Ctrl Pts',(-18.9764845901678,-23.1892753282707,
124.537586105056)) ;
#52547 = CARTESIAN_POINT('Ctrl Pts',(-18.868304680293,-23.0092862477902,124.819034540594)) ;
#52548 = CARTESIAN_POINT('Ctrl Pts',(-19.1774335204479,-23.1992185717199,
124.595200515695)) ;
#52549 = CARTESIAN_POINT('Ctrl Pts',(-19.1194917232944,-23.0192294912394,
124.891049871391)) ;
#52550 = CARTESIAN_POINT('Ctrl Pts',(-19.3844025852747,-23.2091207433278,
124.617601381638)) ;
#52551 = CARTESIAN_POINT('Ctrl Pts',(-19.3782034066437,-23.0291316628473,
124.919048155935)) ;
#52552 = CARTESIAN_POINT('Ctrl Pts',(-19.5952575378545,-23.219173578938,124.603384824931)) ;
#52553 = CARTESIAN_POINT('Ctrl Pts',(-19.6417720055843,-23.0391844984575,
124.901274622995)) ;
#52554 = CARTESIAN_POINT('Ctrl Pts',(-19.796808082773,-23.2290466366235,124.553754633832)) ;
#52555 = CARTESIAN_POINT('Ctrl Pts',(-19.8937094830556,-23.049057556143,124.839234191646)) ;
#52556 = CARTESIAN_POINT('Ctrl Pts',(-19.9892291256445,-23.2390418981492,
124.469324547835)) ;
#52557 = CARTESIAN_POINT('Ctrl Pts',(-20.1342348699008,-23.0590528176687,
124.733693798557)) ;
#52558 = CARTESIAN_POINT('Ctrl Pts',(-20.1643902735447,-23.2490672675697,
124.352097383469)) ;
#52559 = CARTESIAN_POINT('Ctrl Pts',(-20.3531841876872,-23.0690781870892,
124.587158170286)) ;
#52560 = CARTESIAN_POINT('Ctrl Pts',(-20.3146713289308,-23.2589571000963,
124.208405044587)) ;
#52561 = CARTESIAN_POINT('Ctrl Pts',(-20.5410358789933,-23.0789680196158,
124.407538040095)) ;
#52562 = CARTESIAN_POINT('Ctrl Pts',(-20.4803738058375,-23.2722550709057,
123.98326749613)) ;
#52563 = CARTESIAN_POINT('Ctrl Pts',(-20.7481493172849,-23.0922659904252,
124.126127329856)) ;
#52564 = CARTESIAN_POINT('Ctrl Pts',(-20.5831671550575,-23.2854534660148,
123.722071678799)) ;
#52565 = CARTESIAN_POINT('Ctrl Pts',(-20.8766367897417,-23.1054643855344,
123.799667857784)) ;
#52566 = CARTESIAN_POINT('Ctrl Pts',(-20.6148571245368,-23.2988489082943,
123.442305301246)) ;
#52567 = CARTESIAN_POINT('Ctrl Pts',(-20.9162580763179,-23.1188598278138,
123.449902418927)) ;
#52568 = CARTESIAN_POINT('Ctrl Pts',(-20.6022321518531,-23.3087247465333,
123.235027259948)) ;
#52569 = CARTESIAN_POINT('Ctrl Pts',(-20.9004717405058,-23.1287356660528,
123.190816756839)) ;
#52570 = CARTESIAN_POINT('Ctrl Pts',(-20.5530100746428,-23.318786149131,123.029348117295)) ;
#52571 = CARTESIAN_POINT('Ctrl Pts',(-20.8389416668189,-23.1387970686505,
122.933714938976)) ;
#52572 = CARTESIAN_POINT('Ctrl Pts',(-20.470495204662,-23.3286512060661,122.839039896976)) ;
#52573 = CARTESIAN_POINT('Ctrl Pts',(-20.7357971608877,-23.1486621255857,
122.695832837286)) ;
#52574 = CARTESIAN_POINT('Ctrl Pts',(-20.3548367842642,-23.3386633020149,
122.663215896037)) ;
#52575 = CARTESIAN_POINT('Ctrl Pts',(-20.5912157871722,-23.1586742215345,
122.476050346765)) ;
#52576 = CARTESIAN_POINT('Ctrl Pts',(-20.1631967914319,-23.3519406111604,
122.460187922931)) ;
#52577 = CARTESIAN_POINT('Ctrl Pts',(-20.3516936595275,-23.1719515306799,
122.222286259261)) ;
#52578 = CARTESIAN_POINT('Ctrl Pts',(-19.8630377268875,-23.3685396366677,
122.274632914981)) ;
#52579 = CARTESIAN_POINT('Ctrl Pts',(-19.9764398068349,-23.1885505561872,
121.990323874469)) ;
#52580 = CARTESIAN_POINT('Ctrl Pts',(-19.517487437228,-23.3851386847007,122.202591928007)) ;
#52581 = CARTESIAN_POINT('Ctrl Pts',(-19.5445846288438,-23.2051496042202,
121.900290049093)) ;
#52582 = CARTESIAN_POINT('Ctrl Pts',(-19.23951312528,-23.3983820967316,122.217815968059)) ;
#52583 = CARTESIAN_POINT('Ctrl Pts',(-19.1970504323452,-23.2183930162512,
121.919316506711)) ;
#52584 = CARTESIAN_POINT('Ctrl Pts',(-19.0339916765018,-23.4084195244201,
122.265667627133)) ;
#52585 = CARTESIAN_POINT('Ctrl Pts',(-18.9401631490547,-23.2284304439396,
121.979134289516)) ;
#52586 = CARTESIAN_POINT('Ctrl Pts',(-18.8424913044911,-23.4183238263757,
122.347410808801)) ;
#52587 = CARTESIAN_POINT('Ctrl Pts',(-18.7007825061689,-23.2383347458952,
122.081317818087)) ;
#52588 = CARTESIAN_POINT('Ctrl Pts',(-18.6084602838952,-23.4315906663508,
122.499189778994)) ;
#52589 = CARTESIAN_POINT('Ctrl Pts',(-18.408261872732,-23.2516015858704,122.271030307372)) ;
#52590 = CARTESIAN_POINT('Ctrl Pts',(-18.3717345959788,-23.4482168644408,
122.761707590166)) ;
#52591 = CARTESIAN_POINT('Ctrl Pts',(-18.1123399886004,-23.2682277839603,
122.599191193648)) ;
#52592 = CARTESIAN_POINT('Ctrl Pts',(-18.2123565640676,-23.4681359798242,
123.154114455554)) ;
#52593 = CARTESIAN_POINT('Ctrl Pts',(-17.9131297579677,-23.2881468993437,
123.089717711746)) ;
#52594 = CARTESIAN_POINT('Ctrl Pts',(-18.1988208253406,-23.4847424029584,
123.506996953541)) ;
#52595 = CARTESIAN_POINT('Ctrl Pts',(-17.8962057485835,-23.3047533224779,
123.530754190481)) ;
#52596 = CARTESIAN_POINT('Ctrl Pts',(-18.2607588524776,-23.4980386234541,
123.779530753442)) ;
#52597 = CARTESIAN_POINT('Ctrl Pts',(-17.9736383078827,-23.3180495429737,
123.871481315145)) ;
#52598 = CARTESIAN_POINT('Ctrl Pts',(-18.3683238744161,-23.5113074557956,
124.036997547401)) ;
#52599 = CARTESIAN_POINT('Ctrl Pts',(-18.1080876893351,-23.3313183753151,
124.193291225541)) ;
#52600 = CARTESIAN_POINT('Ctrl Pts',(-18.585515956159,-23.5279987038287,124.31755527357)) ;
#52601 = CARTESIAN_POINT('Ctrl Pts',(-18.3795904844463,-23.3480096233482,
124.544002089777)) ;
#52602 = CARTESIAN_POINT('Ctrl Pts',(-18.9413317824027,-23.5478084355015,
124.543077586913)) ;
#52603 = CARTESIAN_POINT('Ctrl Pts',(-18.824358003802,-23.367819355021,124.825895671739)) ;
#52604 = CARTESIAN_POINT('Ctrl Pts',(-19.3559796542478,-23.56778604283,124.635208528437)) ;
#52605 = CARTESIAN_POINT('Ctrl Pts',(-19.3426692477334,-23.3877969623496,
124.941057197869)) ;
#52606 = CARTESIAN_POINT('Ctrl Pts',(-19.7759608022422,-23.5877123518879,
124.579685890579)) ;
#52607 = CARTESIAN_POINT('Ctrl Pts',(-19.8676443127225,-23.4077232714074,
124.871649885416)) ;
#52608 = CARTESIAN_POINT('Ctrl Pts',(-20.1505472402133,-23.6075292120526,
124.386491448277)) ;
#52609 = CARTESIAN_POINT('Ctrl Pts',(-20.3358743902777,-23.4275401315721,
124.630155280744)) ;
#52610 = CARTESIAN_POINT('Ctrl Pts',(-20.4401428515061,-23.6276290276466,
124.072390207339)) ;
#52611 = CARTESIAN_POINT('Ctrl Pts',(-20.6978674017851,-23.4476399471661,
124.237525821871)) ;
#52612 = CARTESIAN_POINT('Ctrl Pts',(-20.6026657871358,-23.6473859915291,
123.684825873049)) ;
#52613 = CARTESIAN_POINT('Ctrl Pts',(-20.9010174943812,-23.4673969110487,
123.753071870161)) ;
#52614 = CARTESIAN_POINT('Ctrl Pts',(-20.6242876059637,-23.6674229175986,
123.259481688023)) ;
#52615 = CARTESIAN_POINT('Ctrl Pts',(-20.9280426937593,-23.4874338371181,
123.221391133689)) ;
#52616 = CARTESIAN_POINT('Ctrl Pts',(-20.4997957023964,-23.6872924999801,
122.855645078802)) ;
#52617 = CARTESIAN_POINT('Ctrl Pts',(-20.7724260969431,-23.5073034194996,
122.716597558687)) ;
#52618 = CARTESIAN_POINT('Ctrl Pts',(-20.2454865673464,-23.7071970717333,
122.517448321673)) ;
#52619 = CARTESIAN_POINT('Ctrl Pts',(-20.4545393934971,-23.5272079912528,
122.293853596945)) ;
#52620 = CARTESIAN_POINT('Ctrl Pts',(-19.8900271158853,-23.7271496739318,
122.285727883188)) ;
#52621 = CARTESIAN_POINT('Ctrl Pts',(-20.0102149505342,-23.5471605934513,
122.004204373787)) ;
#52622 = CARTESIAN_POINT('Ctrl Pts',(-19.4778464728188,-23.747059164902,122.189596892363)) ;
#52623 = CARTESIAN_POINT('Ctrl Pts',(-19.4949902617054,-23.5670700844216,
121.884042017014)) ;
#52624 = CARTESIAN_POINT('Ctrl Pts',(-19.0585021845433,-23.7669105336015,
122.238587168872)) ;
#52625 = CARTESIAN_POINT('Ctrl Pts',(-18.9708122647086,-23.586921453121,121.945279500449)) ;
#52626 = CARTESIAN_POINT('Ctrl Pts',(-18.6771515985997,-23.7869907297375,
122.43039174872)) ;
#52627 = CARTESIAN_POINT('Ctrl Pts',(-18.4941229339348,-23.607001649257,122.185035924184)) ;
#52628 = CARTESIAN_POINT('Ctrl Pts',(-18.3880786328134,-23.8067916733129,
122.736642917923)) ;
#52629 = CARTESIAN_POINT('Ctrl Pts',(-18.1327837983887,-23.6268025928324,
122.567847534477)) ;
#52630 = CARTESIAN_POINT('Ctrl Pts',(-18.2185138748618,-23.8267756498224,
123.126183556028)) ;
#52631 = CARTESIAN_POINT('Ctrl Pts',(-17.920826926211,-23.6467865693419,123.054772698321)) ;
#52632 = CARTESIAN_POINT('Ctrl Pts',(-18.1928000702527,-23.846691612798,123.54886807584)) ;
#52633 = CARTESIAN_POINT('Ctrl Pts',(-17.8886839108745,-23.6667025323175,
123.583127051789)) ;
#52634 = CARTESIAN_POINT('Ctrl Pts',(-18.3114981929088,-23.8665620476199,
123.954437415859)) ;
#52635 = CARTESIAN_POINT('Ctrl Pts',(-18.0370543004863,-23.6865729671394,
124.090087584611)) ;
#52636 = CARTESIAN_POINT('Ctrl Pts',(-18.5641851710754,-23.886612332853,124.297650548748)) ;
#52637 = CARTESIAN_POINT('Ctrl Pts',(-18.352912073492,-23.7066232523725,124.519105466917)) ;
#52638 = CARTESIAN_POINT('Ctrl Pts',(-18.9138459519034,-23.9063863016123,
124.531438448419)) ;
#52639 = CARTESIAN_POINT('Ctrl Pts',(-18.789984541193,-23.7263972211318,124.811340608037)) ;
#52640 = CARTESIAN_POINT('Ctrl Pts',(-19.327728107229,-23.9264427597318,124.633511754983)) ;
#52641 = CARTESIAN_POINT('Ctrl Pts',(-19.3073372095481,-23.7464536792514,
124.938934907489)) ;
#52642 = CARTESIAN_POINT('Ctrl Pts',(-19.7463440551213,-23.9462376427228,
124.588636490226)) ;
#52643 = CARTESIAN_POINT('Ctrl Pts',(-19.8306051755594,-23.7662485622424,
124.882843707718)) ;
#52644 = CARTESIAN_POINT('Ctrl Pts',(-20.128134455108,-23.9662042980252,124.403168082798)) ;
#52645 = CARTESIAN_POINT('Ctrl Pts',(-20.3078444226172,-23.7862152175447,
124.651011447884)) ;
#52646 = CARTESIAN_POINT('Ctrl Pts',(-20.4232185491835,-23.9861632681017,
124.098054033906)) ;
#52647 = CARTESIAN_POINT('Ctrl Pts',(-20.6767016463538,-23.8061741876212,
124.269621393474)) ;
#52648 = CARTESIAN_POINT('Ctrl Pts',(-20.5961622014183,-24.0060593556918,
123.711998667547)) ;
#52649 = CARTESIAN_POINT('Ctrl Pts',(-20.8928840689229,-23.8260702752113,
123.787054530361)) ;
#52650 = CARTESIAN_POINT('Ctrl Pts',(-20.6274889819743,-24.0259575256034,
123.290106766545)) ;
#52651 = CARTESIAN_POINT('Ctrl Pts',(-20.9320464016076,-23.8459684451229,
123.2596908132)) ;
#52652 = CARTESIAN_POINT('Ctrl Pts',(-20.513337763902,-24.0458633609705,122.882506566483)) ;
#52653 = CARTESIAN_POINT('Ctrl Pts',(-20.7893616370779,-23.86587428049,122.75019007212)) ;
#52654 = CARTESIAN_POINT('Ctrl Pts',(-20.266431677999,-24.0658132859084,122.537627079781)) ;
#52655 = CARTESIAN_POINT('Ctrl Pts',(-20.4807327589992,-23.8858242054279,
122.319088447541)) ;
#52656 = CARTESIAN_POINT('Ctrl Pts',(-19.9180548383199,-24.0856924758188,
122.298181469176)) ;
#52657 = CARTESIAN_POINT('Ctrl Pts',(-20.0452649317032,-23.9057033953383,
122.019778092057)) ;
#52658 = CARTESIAN_POINT('Ctrl Pts',(-19.5069122512383,-24.1056738000994,
122.191249797151)) ;
#52659 = CARTESIAN_POINT('Ctrl Pts',(-19.5313379425127,-23.9256847196189,
121.886108845858)) ;
#52660 = CARTESIAN_POINT('Ctrl Pts',(-19.0849454561733,-24.1256035843077,
122.231166566416)) ;
#52661 = CARTESIAN_POINT('Ctrl Pts',(-19.0038793189648,-23.9456145038272,
121.936000230664)) ;
#52662 = CARTESIAN_POINT('Ctrl Pts',(-18.7022509031181,-24.1455235736985,
122.412432300618)) ;
#52663 = CARTESIAN_POINT('Ctrl Pts',(-18.5255093849516,-23.965534493218,122.162577000511)) ;
#52664 = CARTESIAN_POINT('Ctrl Pts',(-18.4045331289834,-24.1653787690525,
122.711900017558)) ;
#52665 = CARTESIAN_POINT('Ctrl Pts',(-18.1533588422071,-23.985389688572,122.536910497454)) ;
#52666 = CARTESIAN_POINT('Ctrl Pts',(-18.2256300026401,-24.1854247707119,
123.098661615411)) ;
#52667 = CARTESIAN_POINT('Ctrl Pts',(-17.9297252153932,-24.0054356902314,
123.020349675048)) ;
#52668 = CARTESIAN_POINT('Ctrl Pts',(-18.1956840876194,-24.2019245179217,
123.448290706154)) ;
#52669 = CARTESIAN_POINT('Ctrl Pts',(-17.8922881635453,-24.0219354374412,
123.457418896118)) ;
#52670 = CARTESIAN_POINT('Ctrl Pts',(-18.244751099481,-24.2153131223698,123.725437756677)) ;
#52671 = CARTESIAN_POINT('Ctrl Pts',(-17.9536182367235,-24.0353240418893,
123.803823185487)) ;
#52672 = CARTESIAN_POINT('Ctrl Pts',(-18.3158010212771,-24.2251749507047,
123.92021291796)) ;
#52673 = CARTESIAN_POINT('Ctrl Pts',(-18.0424306540763,-24.0451858702242,
124.047300970939)) ;
#52674 = CARTESIAN_POINT('Ctrl Pts',(-18.4201246805275,-24.2351410934622,
124.101932284297)) ;
#52675 = CARTESIAN_POINT('Ctrl Pts',(-18.1728224346428,-24.0551520129818,
124.274441107822)) ;
#52676 = CARTESIAN_POINT('Ctrl Pts',(-18.600479700421,-24.2485028395872,124.317163919076)) ;
#52677 = CARTESIAN_POINT('Ctrl Pts',(-18.3983154768799,-24.0685137591067,
124.543527593529)) ;
#52678 = CARTESIAN_POINT('Ctrl Pts',(-18.8864879871126,-24.2649571685423,
124.518993893139)) ;
#52679 = CARTESIAN_POINT('Ctrl Pts',(-18.7557534013296,-24.0849680880618,
124.795766078485)) ;
#52680 = CARTESIAN_POINT('Ctrl Pts',(-19.2302450355489,-24.2817244135906,
124.612794594497)) ;
#52681 = CARTESIAN_POINT('Ctrl Pts',(-19.1855079887439,-24.1017353331101,
124.913045707211)) ;
#52682 = CARTESIAN_POINT('Ctrl Pts',(-19.5076006939437,-24.2949109788646,
124.613694249436)) ;
#52683 = CARTESIAN_POINT('Ctrl Pts',(-19.5321625872062,-24.1149218983841,
124.914163508311)) ;
#52684 = CARTESIAN_POINT('Ctrl Pts',(-19.714585996907,-24.3049004376092,124.57853472076)) ;
#52685 = CARTESIAN_POINT('Ctrl Pts',(-19.7909027433766,-24.1249113571287,
124.870218955484)) ;
#52686 = CARTESIAN_POINT('Ctrl Pts',(-19.9117282679633,-24.3148542100903,
124.508226632481)) ;
#52687 = CARTESIAN_POINT('Ctrl Pts',(-20.0373293988633,-24.1348651296098,
124.782335916297)) ;
#52688 = CARTESIAN_POINT('Ctrl Pts',(-20.0952429868065,-24.324902026623,124.40366816945)) ;
#52689 = CARTESIAN_POINT('Ctrl Pts',(-20.2667248445847,-24.1449129461425,
124.651640371413)) ;
#52690 = CARTESIAN_POINT('Ctrl Pts',(-20.2546683283464,-24.3347435597455,
124.271759801232)) ;
#52691 = CARTESIAN_POINT('Ctrl Pts',(-20.4660081193213,-24.154754479265,124.486757064612)) ;
#52692 = CARTESIAN_POINT('Ctrl Pts',(-20.3910452829839,-24.3447298019652,
124.112189741865)) ;
#52693 = CARTESIAN_POINT('Ctrl Pts',(-20.6364815532312,-24.1647407214847,
124.287296273957)) ;
#52694 = CARTESIAN_POINT('Ctrl Pts',(-20.4972397987561,-24.3546664253901,
123.932255968931)) ;
#52695 = CARTESIAN_POINT('Ctrl Pts',(-20.7692271458693,-24.1746773449096,
124.062380425014)) ;
#52696 = CARTESIAN_POINT('Ctrl Pts',(-20.5712954604918,-24.3647163027731,
123.73440257886)) ;
#52697 = CARTESIAN_POINT('Ctrl Pts',(-20.8617993884923,-24.1847272222926,
123.815064619635)) ;
#52698 = CARTESIAN_POINT('Ctrl Pts',(-20.6092665986412,-24.3745667415506,
123.530810616257)) ;
#52699 = CARTESIAN_POINT('Ctrl Pts',(-20.9092661002677,-24.1945776610702,
123.560575071878)) ;
#52700 = CARTESIAN_POINT('Ctrl Pts',(-20.6118828892727,-24.3845387555194,
123.321210192378)) ;
#52701 = CARTESIAN_POINT('Ctrl Pts',(-20.9125392725062,-24.2045496750389,
123.298574461704)) ;
#52702 = CARTESIAN_POINT('Ctrl Pts',(-20.5779494879227,-24.3945339241455,
123.113804511949)) ;
#52703 = CARTESIAN_POINT('Ctrl Pts',(-20.8701252719288,-24.214544843665,123.03931683066)) ;
#52704 = CARTESIAN_POINT('Ctrl Pts',(-20.5080285322928,-24.4045678074067,
122.914803419106)) ;
#52705 = CARTESIAN_POINT('Ctrl Pts',(-20.7827267212142,-24.2245787269262,
122.790564493733)) ;
#52706 = CARTESIAN_POINT('Ctrl Pts',(-20.4067104297543,-24.41442367747,122.734046050817)) ;
#52707 = CARTESIAN_POINT('Ctrl Pts',(-20.6560814229748,-24.2344345969895,
122.564616215034)) ;
#52708 = CARTESIAN_POINT('Ctrl Pts',(-20.2739437816179,-24.4244212233872,
122.571137981273)) ;
#52709 = CARTESIAN_POINT('Ctrl Pts',(-20.4901252099915,-24.2444321429067,
122.360979293762)) ;
#52710 = CARTESIAN_POINT('Ctrl Pts',(-20.1163503321144,-24.4343293502864,
122.434915065284)) ;
#52711 = CARTESIAN_POINT('Ctrl Pts',(-20.2931350358495,-24.254340269806,122.190698398369)) ;
#52712 = CARTESIAN_POINT('Ctrl Pts',(-19.9358381554827,-24.4443397218086,
122.326707961461)) ;
#52713 = CARTESIAN_POINT('Ctrl Pts',(-20.0674961655237,-24.2643506413281,
122.055437128018)) ;
#52714 = CARTESIAN_POINT('Ctrl Pts',(-19.7387342050816,-24.454370164556,122.251783176735)) ;
#52715 = CARTESIAN_POINT('Ctrl Pts',(-19.8211172047794,-24.2743810840756,
121.961778537546)) ;
#52716 = CARTESIAN_POINT('Ctrl Pts',(-19.5354521664302,-24.4642181171093,
122.212461214448)) ;
#52717 = CARTESIAN_POINT('Ctrl Pts',(-19.5670147879019,-24.2842290366288,
121.91262331826)) ;
#52718 = CARTESIAN_POINT('Ctrl Pts',(-19.3239551652899,-24.4742807861303,
122.208794045191)) ;
#52719 = CARTESIAN_POINT('Ctrl Pts',(-19.3026436245649,-24.2942917056498,
121.908036630812)) ;
#52720 = CARTESIAN_POINT('Ctrl Pts',(-19.1185123192759,-24.4841751615942,
122.241504281932)) ;
#52721 = CARTESIAN_POINT('Ctrl Pts',(-19.045839313324,-24.3041860811137,121.948921771681)) ;
#52722 = CARTESIAN_POINT('Ctrl Pts',(-18.9207873898694,-24.4941169599123,
122.309170126325)) ;
#52723 = CARTESIAN_POINT('Ctrl Pts',(-18.7986820357959,-24.3141278794319,
122.033501629662)) ;
#52724 = CARTESIAN_POINT('Ctrl Pts',(-18.7366115575641,-24.5041194536396,
122.410711220208)) ;
#52725 = CARTESIAN_POINT('Ctrl Pts',(-18.5684608874913,-24.3241303731592,
122.160425707756)) ;
#52726 = CARTESIAN_POINT('Ctrl Pts',(-18.5725769314898,-24.5141542521466,
122.543347790697)) ;
#52727 = CARTESIAN_POINT('Ctrl Pts',(-18.3634159133862,-24.3341651716661,
122.326219304036)) ;
#52728 = CARTESIAN_POINT('Ctrl Pts',(-18.4364059179355,-24.5239991361259,
122.699231885075)) ;
#52729 = CARTESIAN_POINT('Ctrl Pts',(-18.1931997742607,-24.3440100556455,
122.521073096057)) ;
#52730 = CARTESIAN_POINT('Ctrl Pts',(-18.3275230682562,-24.533984992944,122.878683232876)) ;
#52731 = CARTESIAN_POINT('Ctrl Pts',(-18.057093903249,-24.3539959124635,122.745386068075)) ;
#52732 = CARTESIAN_POINT('Ctrl Pts',(-18.2516769257629,-24.5439198071187,
123.073327761756)) ;
#52733 = CARTESIAN_POINT('Ctrl Pts',(-17.9622837119148,-24.3639307266383,
122.988691099146)) ;
#52734 = CARTESIAN_POINT('Ctrl Pts',(-18.2104726947077,-24.5539773069041,
123.280683690247)) ;
#52735 = CARTESIAN_POINT('Ctrl Pts',(-17.9107758864736,-24.3739882264236,
123.247885387982)) ;
#52736 = CARTESIAN_POINT('Ctrl Pts',(-18.2056888743538,-24.5637990653224,
123.487134857633)) ;
#52737 = CARTESIAN_POINT('Ctrl Pts',(-17.9047935450164,-24.3838099848419,
123.505950068642)) ;
#52738 = CARTESIAN_POINT('Ctrl Pts',(-18.2371668828863,-24.5738547231064,
123.696162130977)) ;
#52739 = CARTESIAN_POINT('Ctrl Pts',(-17.9441385893979,-24.3938656426259,
123.767234420961)) ;
#52740 = CARTESIAN_POINT('Ctrl Pts',(-18.3040695591823,-24.5837969052864,
123.894192986261)) ;
#52741 = CARTESIAN_POINT('Ctrl Pts',(-18.0277646256718,-24.4038078248059,
124.014774122558)) ;
#52742 = CARTESIAN_POINT('Ctrl Pts',(-18.4034039808886,-24.5937021139811,
124.07720850749)) ;
#52743 = CARTESIAN_POINT('Ctrl Pts',(-18.1519307757942,-24.4137130335006,
124.243545142441)) ;
#52744 = CARTESIAN_POINT('Ctrl Pts',(-18.5348467278453,-24.6037439049435,
124.242401635363)) ;
#52745 = CARTESIAN_POINT('Ctrl Pts',(-18.316232248357,-24.4237548244631,124.450038001012)) ;
#52746 = CARTESIAN_POINT('Ctrl Pts',(-18.6908591823526,-24.6136516794158,
124.380420797567)) ;
#52747 = CARTESIAN_POINT('Ctrl Pts',(-18.5112465950193,-24.4336625989353,
124.622564118321)) ;
#52748 = CARTESIAN_POINT('Ctrl Pts',(-18.8701202015806,-24.6236631796434,
124.490724089556)) ;
#52749 = CARTESIAN_POINT('Ctrl Pts',(-18.7353216881692,-24.4436740991629,
124.760445263061)) ;
#52750 = CARTESIAN_POINT('Ctrl Pts',(-19.0663816760572,-24.6336959400361,
124.567979438688)) ;
#52751 = CARTESIAN_POINT('Ctrl Pts',(-18.9806475911172,-24.4537068595556,
124.8570167095)) ;
#52752 = CARTESIAN_POINT('Ctrl Pts',(-19.2692552137906,-24.643546509171,124.609578863151)) ;
#52753 = CARTESIAN_POINT('Ctrl Pts',(-19.2342398512218,-24.4635574286905,
124.909018470008)) ;
#52754 = CARTESIAN_POINT('Ctrl Pts',(-19.4791376987757,-24.6535351187009,
124.615797717259)) ;
#52755 = CARTESIAN_POINT('Ctrl Pts',(-19.4965930730634,-24.4735460382204,
124.916794313041)) ;
#52756 = CARTESIAN_POINT('Ctrl Pts',(-19.6856874087961,-24.663463774725,124.585656540183)) ;
#52757 = CARTESIAN_POINT('Ctrl Pts',(-19.7547810174489,-24.4834746942445,
124.879120016073)) ;
#52758 = CARTESIAN_POINT('Ctrl Pts',(-19.8851618333618,-24.6734515209028,
124.520055763717)) ;
#52759 = CARTESIAN_POINT('Ctrl Pts',(-20.0041249025935,-24.4934624404223,
124.797121058293)) ;
#52760 = CARTESIAN_POINT('Ctrl Pts',(-20.0709240901513,-24.6834875098385,
124.420032910437)) ;
#52761 = CARTESIAN_POINT('Ctrl Pts',(-20.2363287244765,-24.503498429358,124.672094532665)) ;
#52762 = CARTESIAN_POINT('Ctrl Pts',(-20.2337420876468,-24.6933423796521,
124.291888982276)) ;
#52763 = CARTESIAN_POINT('Ctrl Pts',(-20.4398532895244,-24.5133532991716,
124.511915769027)) ;
#52764 = CARTESIAN_POINT('Ctrl Pts',(-20.3740410207416,-24.7033418208939,
124.135384425764)) ;
#52765 = CARTESIAN_POINT('Ctrl Pts',(-20.6152286147795,-24.5233527404134,
124.316286380267)) ;
#52766 = CARTESIAN_POINT('Ctrl Pts',(-20.4841026431737,-24.713236895074,123.958818728685)) ;
#52767 = CARTESIAN_POINT('Ctrl Pts',(-20.7528077613622,-24.5332478145935,
124.095579716456)) ;
#52768 = CARTESIAN_POINT('Ctrl Pts',(-20.5630911584333,-24.7232975509137,
123.762644267269)) ;
#52769 = CARTESIAN_POINT('Ctrl Pts',(-20.851545217851,-24.5433084704332,123.850362627653)) ;
#52770 = CARTESIAN_POINT('Ctrl Pts',(-20.6060224074376,-24.7331464251093,
123.560073880987)) ;
#52771 = CARTESIAN_POINT('Ctrl Pts',(-20.9052114658555,-24.5531573446288,
123.59714904621)) ;
#52772 = CARTESIAN_POINT('Ctrl Pts',(-20.6137892692649,-24.7431751370725,
123.349384846586)) ;
#52773 = CARTESIAN_POINT('Ctrl Pts',(-20.9149218986309,-24.5631860565921,
123.333787858273)) ;
#52774 = CARTESIAN_POINT('Ctrl Pts',(-20.5842846845228,-24.7532045376556,
123.140605694628)) ;
#52775 = CARTESIAN_POINT('Ctrl Pts',(-20.8780431869163,-24.5732154571752,
123.072813707574)) ;
#52776 = CARTESIAN_POINT('Ctrl Pts',(-20.5206480631986,-24.7630447312725,
122.943761957022)) ;
#52777 = CARTESIAN_POINT('Ctrl Pts',(-20.7984988602342,-24.583055650792,122.826757371382)) ;
#52778 = CARTESIAN_POINT('Ctrl Pts',(-20.4225485419105,-24.7730481538477,
122.757764156564)) ;
#52779 = CARTESIAN_POINT('Ctrl Pts',(-20.6758759733845,-24.5930590733672,
122.594259198526)) ;
#52780 = CARTESIAN_POINT('Ctrl Pts',(-20.2937856669965,-24.7830336909408,
122.591919417926)) ;
#52781 = CARTESIAN_POINT('Ctrl Pts',(-20.5149236680147,-24.6030446104603,
122.386952011193)) ;
#52782 = CARTESIAN_POINT('Ctrl Pts',(-20.1372175607481,-24.7930746954276,
122.450362162771)) ;
#52783 = CARTESIAN_POINT('Ctrl Pts',(-20.3192148830929,-24.6130856149471,
122.210004149915)) ;
#52784 = CARTESIAN_POINT('Ctrl Pts',(-19.9620847517272,-24.8029182343688,
122.340090117792)) ;
#52785 = CARTESIAN_POINT('Ctrl Pts',(-20.1002988243913,-24.6229291538883,
122.07216197411)) ;
#52786 = CARTESIAN_POINT('Ctrl Pts',(-19.7679204826026,-24.8129032653596,
122.260388804538)) ;
#52787 = CARTESIAN_POINT('Ctrl Pts',(-19.8575938758335,-24.6329141848791,
121.972533729718)) ;
#52788 = CARTESIAN_POINT('Ctrl Pts',(-19.5637613025099,-24.8228427278816,
122.215721170497)) ;
#52789 = CARTESIAN_POINT('Ctrl Pts',(-19.6023947115002,-24.6428536474011,
121.916697509379)) ;
#52790 = CARTESIAN_POINT('Ctrl Pts',(-19.3528855208101,-24.8328824601054,
122.207143938468)) ;
#52791 = CARTESIAN_POINT('Ctrl Pts',(-19.3388001962124,-24.6528933796249,
121.905974359141)) ;
#52792 = CARTESIAN_POINT('Ctrl Pts',(-19.1468393604488,-24.8427706404226,
122.234788301827)) ;
#52793 = CARTESIAN_POINT('Ctrl Pts',(-19.0812413724602,-24.6627815599421,
121.940528367414)) ;
#52794 = CARTESIAN_POINT('Ctrl Pts',(-18.9465910465543,-24.8527601561251,
122.298052941285)) ;
#52795 = CARTESIAN_POINT('Ctrl Pts',(-18.8309303395174,-24.6727710756446,
122.019607849722)) ;
#52796 = CARTESIAN_POINT('Ctrl Pts',(-18.7610210692701,-24.8627187067798,
122.394969542259)) ;
#52797 = CARTESIAN_POINT('Ctrl Pts',(-18.5989667872647,-24.6827296262993,
122.140752466129)) ;
#52798 = CARTESIAN_POINT('Ctrl Pts',(-18.5957514950734,-24.8726181138848,
122.521477714569)) ;
#52799 = CARTESIAN_POINT('Ctrl Pts',(-18.3923783175925,-24.6926290334043,
122.298887165085)) ;
#52800 = CARTESIAN_POINT('Ctrl Pts',(-18.4529280511965,-24.8826667003011,
122.677100505805)) ;
#52801 = CARTESIAN_POINT('Ctrl Pts',(-18.2138481635963,-24.7026776198206,
122.493414575647)) ;
#52802 = CARTESIAN_POINT('Ctrl Pts',(-18.3408505972411,-24.8925595192655,
122.85234593428)) ;
#52803 = CARTESIAN_POINT('Ctrl Pts',(-18.0737497674036,-24.7125704387851,
122.712471449021)) ;
#52804 = CARTESIAN_POINT('Ctrl Pts',(-18.2595668677293,-24.9026306367953,
123.047801925644)) ;
#52805 = CARTESIAN_POINT('Ctrl Pts',(-17.9721440402677,-24.7226415563149,
122.9567905855)) ;
#52806 = CARTESIAN_POINT('Ctrl Pts',(-18.2143360447103,-24.9124463307614,
123.249180345051)) ;
#52807 = CARTESIAN_POINT('Ctrl Pts',(-17.9156039985749,-24.7324572502809,
123.208514840496)) ;
#52808 = CARTESIAN_POINT('Ctrl Pts',(-18.2042126503118,-24.9225127082587,
123.460520176297)) ;
#52809 = CARTESIAN_POINT('Ctrl Pts',(-17.9029486723776,-24.7425236277782,
123.472689210437)) ;
#52810 = CARTESIAN_POINT('Ctrl Pts',(-18.2305681873623,-24.9324116943406,
123.667004534321)) ;
#52811 = CARTESIAN_POINT('Ctrl Pts',(-17.9358920953055,-24.7524226138601,
123.730795685759)) ;
#52812 = CARTESIAN_POINT('Ctrl Pts',(-18.2932377700678,-24.9424658743341,
123.868822725467)) ;
#52813 = CARTESIAN_POINT('Ctrl Pts',(-18.0142279452828,-24.7624767938536,
123.983068491453)) ;
#52814 = CARTESIAN_POINT('Ctrl Pts',(-18.3880943306794,-24.9523366872668,
124.053444339054)) ;
#52815 = CARTESIAN_POINT('Ctrl Pts',(-18.1327982651776,-24.7723476067863,
124.21384699712)) ;
#52816 = CARTESIAN_POINT('Ctrl Pts',(-18.5160928318226,-24.9624105881206,
124.222110708763)) ;
#52817 = CARTESIAN_POINT('Ctrl Pts',(-18.2927953164419,-24.7824215076401,
124.424680232179)) ;
#52818 = CARTESIAN_POINT('Ctrl Pts',(-18.6674180149936,-24.9722307435072,
124.362618007818)) ;
#52819 = CARTESIAN_POINT('Ctrl Pts',(-18.4819523061609,-24.7922416630268,
124.600316091069)) ;
#52820 = CARTESIAN_POINT('Ctrl Pts',(-18.8452136411496,-24.9823094504595,
124.477780776126)) ;
#52821 = CARTESIAN_POINT('Ctrl Pts',(-18.7041959808431,-24.802320369979,124.74427000949)) ;
#52822 = CARTESIAN_POINT('Ctrl Pts',(-19.0359724593799,-24.9921610389983,
124.558567319872)) ;
#52823 = CARTESIAN_POINT('Ctrl Pts',(-18.9426453969579,-24.8121719585178,
124.845254460415)) ;
#52824 = CARTESIAN_POINT('Ctrl Pts',(-19.2422734738344,-25.0022341555233,
124.606210580914)) ;
#52825 = CARTESIAN_POINT('Ctrl Pts',(-19.2005210691097,-24.8222450750428,
124.904809172746)) ;
#52826 = CARTESIAN_POINT('Ctrl Pts',(-19.4489294427733,-25.0120766726191,
124.617025230768)) ;
#52827 = CARTESIAN_POINT('Ctrl Pts',(-19.4588424041229,-24.8320875921386,
124.918328324967)) ;
#52828 = CARTESIAN_POINT('Ctrl Pts',(-19.6572595399181,-25.022057134173,124.592142989449)) ;
#52829 = CARTESIAN_POINT('Ctrl Pts',(-19.7192553918332,-24.8420680536926,
124.887225976324)) ;
#52830 = CARTESIAN_POINT('Ctrl Pts',(-19.858754508053,-25.0320753841638,124.530845580541)) ;
#52831 = CARTESIAN_POINT('Ctrl Pts',(-19.9711242826763,-24.8520863036833,
124.810604842255)) ;
#52832 = CARTESIAN_POINT('Ctrl Pts',(-20.0442458404208,-25.0419595443576,
124.437141256552)) ;
#52833 = CARTESIAN_POINT('Ctrl Pts',(-20.2029896411673,-24.8619704638771,
124.693474375356)) ;
#52834 = CARTESIAN_POINT('Ctrl Pts',(-20.2136336533158,-25.0520246913326,
124.310362839137)) ;
#52835 = CARTESIAN_POINT('Ctrl Pts',(-20.4147243952556,-24.8720356108521,
124.53500199197)) ;
#52836 = CARTESIAN_POINT('Ctrl Pts',(-20.3553327642867,-25.0618665149734,
124.159573795063)) ;
#52837 = CARTESIAN_POINT('Ctrl Pts',(-20.5918496188217,-24.8818774344929,
124.34651493067)) ;
#52838 = CARTESIAN_POINT('Ctrl Pts',(-20.4713227735349,-25.0718959874342,
123.98349792825)) ;
#52839 = CARTESIAN_POINT('Ctrl Pts',(-20.7368372686807,-24.8919069069537,
124.126420308734)) ;
#52840 = CARTESIAN_POINT('Ctrl Pts',(-20.5544183696664,-25.0819228426962,
123.789765828092)) ;
#52841 = CARTESIAN_POINT('Ctrl Pts',(-20.8407071586523,-24.9019337622158,
123.884255456055)) ;
#52842 = CARTESIAN_POINT('Ctrl Pts',(-20.6022129333517,-25.0917660928068,
123.58842207058)) ;
#52843 = CARTESIAN_POINT('Ctrl Pts',(-20.9004509564866,-24.9117770123263,
123.632574419176)) ;
#52844 = CARTESIAN_POINT('Ctrl Pts',(-20.6148605428865,-25.1018145323899,
123.377557024283)) ;
#52845 = CARTESIAN_POINT('Ctrl Pts',(-20.9162606114389,-24.9218254519095,
123.368993380638)) ;
#52846 = CARTESIAN_POINT('Ctrl Pts',(-20.590610957124,-25.1117640266378,123.16979691793)) ;
#52847 = CARTESIAN_POINT('Ctrl Pts',(-20.8859488525621,-24.9317749461574,
123.109292637729)) ;
#52848 = CARTESIAN_POINT('Ctrl Pts',(-20.5315027514083,-25.1216718823638,
122.970053451003)) ;
#52849 = CARTESIAN_POINT('Ctrl Pts',(-20.8120633746983,-24.9416828018834,
122.859612422468)) ;
#52850 = CARTESIAN_POINT('Ctrl Pts',(-20.4370028959412,-25.1317313590138,
122.780884060618)) ;
#52851 = CARTESIAN_POINT('Ctrl Pts',(-20.6939388266364,-24.9517422785333,
122.623150935538)) ;
#52852 = CARTESIAN_POINT('Ctrl Pts',(-20.3140267459724,-25.1415721684225,
122.614484936629)) ;
#52853 = CARTESIAN_POINT('Ctrl Pts',(-20.5402177798436,-24.961583087942,122.415150839197)) ;
#52854 = CARTESIAN_POINT('Ctrl Pts',(-20.1608696779371,-25.1516343187233,
122.46860151475)) ;
#52855 = CARTESIAN_POINT('Ctrl Pts',(-20.348771652223,-24.9716452382428,122.232796879371)) ;
#52856 = CARTESIAN_POINT('Ctrl Pts',(-19.9874513742878,-25.1615314798458,
122.353608540262)) ;
#52857 = CARTESIAN_POINT('Ctrl Pts',(-20.1319979379793,-24.9815423993653,
122.089055106544)) ;
#52858 = CARTESIAN_POINT('Ctrl Pts',(-19.7963375421497,-25.1714626542499,
122.269557911198)) ;
#52859 = CARTESIAN_POINT('Ctrl Pts',(-19.8931048763315,-24.9914735737694,
121.983991783482)) ;
#52860 = CARTESIAN_POINT('Ctrl Pts',(-19.5912085972719,-25.1815048579749,
122.219637399699)) ;
#52861 = CARTESIAN_POINT('Ctrl Pts',(-19.6366938542674,-25.0015157774944,
121.921591372191)) ;
#52862 = CARTESIAN_POINT('Ctrl Pts',(-19.3837898601191,-25.1913914404053,
122.206149497569)) ;
#52863 = CARTESIAN_POINT('Ctrl Pts',(-19.3774193320278,-25.0114023599249,
121.904731667555)) ;
#52864 = CARTESIAN_POINT('Ctrl Pts',(-19.174930617181,-25.2013848761537,122.228779671047)) ;
#52865 = CARTESIAN_POINT('Ctrl Pts',(-19.1163451180377,-25.0213957956732,
121.933019785875)) ;
#52866 = CARTESIAN_POINT('Ctrl Pts',(-18.9741668937736,-25.2113293445118,
122.287109961351)) ;
#52867 = CARTESIAN_POINT('Ctrl Pts',(-18.8653899853022,-25.0313402640314,
122.005933155517)) ;
#52868 = CARTESIAN_POINT('Ctrl Pts',(-18.7862616744613,-25.2212811607574,
122.379130251146)) ;
#52869 = CARTESIAN_POINT('Ctrl Pts',(-18.6305081903496,-25.0412920802769,
122.120959220952)) ;
#52870 = CARTESIAN_POINT('Ctrl Pts',(-18.6158633692364,-25.2313185968719,
122.503584025425)) ;
#52871 = CARTESIAN_POINT('Ctrl Pts',(-18.4175106983079,-25.0513295163914,
122.276526693717)) ;
#52872 = CARTESIAN_POINT('Ctrl Pts',(-18.4717187038832,-25.2412035560482,
122.653303494758)) ;
#52873 = CARTESIAN_POINT('Ctrl Pts',(-18.2373294885558,-25.0612144755677,
122.463677159448)) ;
#52874 = CARTESIAN_POINT('Ctrl Pts',(-18.3542495988289,-25.2512016742602,
122.827576694392)) ;
#52875 = CARTESIAN_POINT('Ctrl Pts',(-18.0904935271512,-25.0712125937797,
122.681519130247)) ;
#52876 = CARTESIAN_POINT('Ctrl Pts',(-18.2693324752695,-25.2611226067721,
123.018101116052)) ;
#52877 = CARTESIAN_POINT('Ctrl Pts',(-17.984347411207,-25.0811335262917,122.91967563865)) ;
#52878 = CARTESIAN_POINT('Ctrl Pts',(-18.2181276836119,-25.2711639069942,
123.2228864421)) ;
#52879 = CARTESIAN_POINT('Ctrl Pts',(-17.9203421283148,-25.0911748265137,
123.175657289264)) ;
#52880 = CARTESIAN_POINT('Ctrl Pts',(-18.203527625728,-25.2810708253842,123.430650481538)) ;
#52881 = CARTESIAN_POINT('Ctrl Pts',(-17.9020926496286,-25.1010817449037,
123.435363279088)) ;
#52882 = CARTESIAN_POINT('Ctrl Pts',(-18.2246915361504,-25.2910066170932,
123.638458055856)) ;
#52883 = CARTESIAN_POINT('Ctrl Pts',(-17.9285484879378,-25.1110175366128,
123.695123310117)) ;
#52884 = CARTESIAN_POINT('Ctrl Pts',(-18.2824223938012,-25.3010475116711,
123.841496647617)) ;
#52885 = CARTESIAN_POINT('Ctrl Pts',(-18.0007127840701,-25.1210584311907,
123.948921150005)) ;
#52886 = CARTESIAN_POINT('Ctrl Pts',(-18.3729909834067,-25.310934713385,124.028599784085)) ;
#52887 = CARTESIAN_POINT('Ctrl Pts',(-18.1139247513715,-25.1309456329045,
124.182800630761)) ;
#52888 = CARTESIAN_POINT('Ctrl Pts',(-18.4956664931269,-25.3209269811466,
124.19910961797)) ;
#52889 = CARTESIAN_POINT('Ctrl Pts',(-18.2672700655301,-25.1409379006661,
124.395937506981)) ;
#52890 = CARTESIAN_POINT('Ctrl Pts',(-18.6454852083747,-25.3308755021684,
124.345063822644)) ;
#52891 = CARTESIAN_POINT('Ctrl Pts',(-18.45454452636,-25.1508864216879,124.578379945201)) ;
#52892 = CARTESIAN_POINT('Ctrl Pts',(-18.8179761803924,-25.3408122757461,
124.462875898515)) ;
#52893 = CARTESIAN_POINT('Ctrl Pts',(-18.6701593793859,-25.1608231952656,
124.725644505682)) ;
#52894 = CARTESIAN_POINT('Ctrl Pts',(-19.0091199998643,-25.3507953238871,
124.549608305468)) ;
#52895 = CARTESIAN_POINT('Ctrl Pts',(-18.9090898745599,-25.1708062434066,
124.834059046588)) ;
#52896 = CARTESIAN_POINT('Ctrl Pts',(-19.2137039022557,-25.3608390314972,
124.601767255972)) ;
#52897 = CARTESIAN_POINT('Ctrl Pts',(-19.164819826109,-25.1808499510167,124.899256681918)) ;
#52898 = CARTESIAN_POINT('Ctrl Pts',(-19.4197410435178,-25.3706677246505,
124.617749119944)) ;
#52899 = CARTESIAN_POINT('Ctrl Pts',(-19.422367781993,-25.19067864417,124.91923291457)) ;
#52900 = CARTESIAN_POINT('Ctrl Pts',(-19.6305293861476,-25.3807424737799,
124.597364532467)) ;
#52901 = CARTESIAN_POINT('Ctrl Pts',(-19.6858526790908,-25.2007533932995,
124.89375095602)) ;
#52902 = CARTESIAN_POINT('Ctrl Pts',(-19.8303729849827,-25.3906077995755,
124.541808861825)) ;
#52903 = CARTESIAN_POINT('Ctrl Pts',(-19.9356579462846,-25.210618719095,124.824304856749)) ;
#52904 = CARTESIAN_POINT('Ctrl Pts',(-20.0207155288672,-25.4006299739324,
124.451476082817)) ;
#52905 = CARTESIAN_POINT('Ctrl Pts',(-20.1735854694028,-25.2206408934519,
124.711387601756)) ;
#52906 = CARTESIAN_POINT('Ctrl Pts',(-20.1922659082655,-25.4106560271393,
124.328983469291)) ;
#52907 = CARTESIAN_POINT('Ctrl Pts',(-20.3880226562012,-25.2306669466589,
124.558270853534)) ;
#52908 = CARTESIAN_POINT('Ctrl Pts',(-20.3376209909237,-25.4205097239856,
124.181407992117)) ;
#52909 = CARTESIAN_POINT('Ctrl Pts',(-20.5697163880298,-25.2405206435051,
124.373799671804)) ;
#52910 = CARTESIAN_POINT('Ctrl Pts',(-20.4569372871272,-25.4304691287386,
124.009344969333)) ;
#52911 = CARTESIAN_POINT('Ctrl Pts',(-20.718860691556,-25.2504800482581,124.158719634618)) ;
#52912 = CARTESIAN_POINT('Ctrl Pts',(-20.5449097818086,-25.4405073744435,
123.817532980503)) ;
#52913 = CARTESIAN_POINT('Ctrl Pts',(-20.8288249196996,-25.260518293963,123.918954163227)) ;
#52914 = CARTESIAN_POINT('Ctrl Pts',(-20.5977398559491,-25.4503815586055,
123.616753729714)) ;
#52915 = CARTESIAN_POINT('Ctrl Pts',(-20.894861231508,-25.270392478125,123.667978712709)) ;
#52916 = CARTESIAN_POINT('Ctrl Pts',(-20.6152318947396,-25.4604513417434,
123.405808054371)) ;
#52917 = CARTESIAN_POINT('Ctrl Pts',(-20.9167246663165,-25.2804622612629,
123.404296836378)) ;
#52918 = CARTESIAN_POINT('Ctrl Pts',(-20.5963934662247,-25.4702845967642,
123.199925169976)) ;
#52919 = CARTESIAN_POINT('Ctrl Pts',(-20.8931748952391,-25.2902955162837,
123.146942101497)) ;
#52920 = CARTESIAN_POINT('Ctrl Pts',(-20.5415866211297,-25.4803150228959,
122.99630793319)) ;
#52921 = CARTESIAN_POINT('Ctrl Pts',(-20.824664603681,-25.3003259424154,122.892421113354)) ;
#52922 = CARTESIAN_POINT('Ctrl Pts',(-20.4516839654255,-25.4903466350829,
122.805521136802)) ;
#52923 = CARTESIAN_POINT('Ctrl Pts',(-20.7122848540759,-25.3103575546024,
122.653938383704)) ;
#52924 = CARTESIAN_POINT('Ctrl Pts',(-20.3328358727724,-25.5001763319375,
122.636482789407)) ;
#52925 = CARTESIAN_POINT('Ctrl Pts',(-20.5637225649554,-25.320187251457,122.442640422349)) ;
#52926 = CARTESIAN_POINT('Ctrl Pts',(-20.1844921702679,-25.51016577384,122.487819824173)) ;
#52927 = CARTESIAN_POINT('Ctrl Pts',(-20.3782914260521,-25.3301766933595,
122.256812972949)) ;
#52928 = CARTESIAN_POINT('Ctrl Pts',(-20.0113511337868,-25.5202096658556,
122.366957918595)) ;
#52929 = CARTESIAN_POINT('Ctrl Pts',(-20.1618642263382,-25.3402205853752,
122.105737144848)) ;
#52930 = CARTESIAN_POINT('Ctrl Pts',(-19.8242733803076,-25.5300312276249,
122.279578448375)) ;
#52931 = CARTESIAN_POINT('Ctrl Pts',(-19.9280150892942,-25.3500421471444,
121.996514020371)) ;
#52932 = CARTESIAN_POINT('Ctrl Pts',(-19.6206530982633,-25.5400667992491,
122.2243313612)) ;
#52933 = CARTESIAN_POINT('Ctrl Pts',(-19.6734892887198,-25.3600777187686,
121.927457195512)) ;
#52934 = CARTESIAN_POINT('Ctrl Pts',(-19.4106109576734,-25.5500960735309,
122.205921274925)) ;
#52935 = CARTESIAN_POINT('Ctrl Pts',(-19.4109364974857,-25.3701069930504,
121.904446478551)) ;
#52936 = CARTESIAN_POINT('Ctrl Pts',(-19.2046030647571,-25.5599299106495,
122.22335172287)) ;
#52937 = CARTESIAN_POINT('Ctrl Pts',(-19.1534256982825,-25.3799408301691,
121.926236678516)) ;
#52938 = CARTESIAN_POINT('Ctrl Pts',(-19.000259823004,-25.5699823067377,122.277212320983)) ;
#52939 = CARTESIAN_POINT('Ctrl Pts',(-18.8979973838233,-25.3899932262572,
121.993564432234)) ;
#52940 = CARTESIAN_POINT('Ctrl Pts',(-18.8106744902198,-25.5799190736882,
122.364971233025)) ;
#52941 = CARTESIAN_POINT('Ctrl Pts',(-18.6610161339955,-25.3999299932077,
122.103265136426)) ;
#52942 = CARTESIAN_POINT('Ctrl Pts',(-18.6389522732557,-25.5898533086675,
122.483834336028)) ;
#52943 = CARTESIAN_POINT('Ctrl Pts',(-18.4463642083147,-25.409864228187,122.251846102257)) ;
#52944 = CARTESIAN_POINT('Ctrl Pts',(-18.4892297183612,-25.5998770719943,
122.632124416292)) ;
#52945 = CARTESIAN_POINT('Ctrl Pts',(-18.2592125480049,-25.4198879915138,
122.437210228585)) ;
#52946 = CARTESIAN_POINT('Ctrl Pts',(-18.3690729527359,-25.6097634133789,
122.801712077461)) ;
#52947 = CARTESIAN_POINT('Ctrl Pts',(-18.1090179639727,-25.4297743328985,
122.649196677297)) ;
#52948 = CARTESIAN_POINT('Ctrl Pts',(-18.2788188736161,-25.6197524621459,
122.991336888981)) ;
#52949 = CARTESIAN_POINT('Ctrl Pts',(-17.9962023975018,-25.4397633816654,
122.886228834254)) ;
#52950 = CARTESIAN_POINT('Ctrl Pts',(-18.2229938244163,-25.6297936828433,
123.194918820965)) ;
#52951 = CARTESIAN_POINT('Ctrl Pts',(-17.9264232478463,-25.4498046023628,
123.140706746034)) ;
#52952 = CARTESIAN_POINT('Ctrl Pts',(-18.2034358522084,-25.6396263230212,
123.400700722428)) ;
#52953 = CARTESIAN_POINT('Ctrl Pts',(-17.9019779828745,-25.4596372425407,
123.397935296116)) ;
#52954 = CARTESIAN_POINT('Ctrl Pts',(-18.2195753607672,-25.6496202523291,
123.610182629394)) ;
#52955 = CARTESIAN_POINT('Ctrl Pts',(-17.9221548128454,-25.4696311718487,
123.659787613436)) ;
#52956 = CARTESIAN_POINT('Ctrl Pts',(-18.2724604743426,-25.6596494600097,
123.814289690547)) ;
#52957 = CARTESIAN_POINT('Ctrl Pts',(-17.988263462569,-25.4796603795292,123.914920832019)) ;
#52958 = CARTESIAN_POINT('Ctrl Pts',(-18.358339643957,-25.6695252717138,124.003328990778)) ;
#52959 = CARTESIAN_POINT('Ctrl Pts',(-18.0956149026414,-25.4895361912333,
124.151219574902)) ;
#52960 = CARTESIAN_POINT('Ctrl Pts',(-18.4769919261622,-25.6795244986852,
124.176823257226)) ;
#52961 = CARTESIAN_POINT('Ctrl Pts',(-18.2439323542707,-25.4995354182047,
124.368086107319)) ;
#52962 = CARTESIAN_POINT('Ctrl Pts',(-18.6225453670208,-25.6894339798409,
124.325912667589)) ;
#52963 = CARTESIAN_POINT('Ctrl Pts',(-18.4258762773874,-25.5094448993604,
124.554446462921)) ;
#52964 = CARTESIAN_POINT('Ctrl Pts',(-18.7942023877807,-25.6994872101418,
124.449174674582)) ;
#52965 = CARTESIAN_POINT('Ctrl Pts',(-18.6404489286503,-25.5194981296613,
124.708521880127)) ;
#52966 = CARTESIAN_POINT('Ctrl Pts',(-18.9811834854639,-25.7093578266928,
124.539201485248)) ;
#52967 = CARTESIAN_POINT('Ctrl Pts',(-18.8741769468847,-25.5293687462124,
124.821053391439)) ;
#52968 = CARTESIAN_POINT('Ctrl Pts',(-19.1838697790237,-25.7193794884249,
124.596699644364)) ;
#52969 = CARTESIAN_POINT('Ctrl Pts',(-19.1275355267002,-25.5393904079444,
124.892923586862)) ;
#52970 = CARTESIAN_POINT('Ctrl Pts',(-19.3935471693339,-25.729402301606,124.617654797258)) ;
#52971 = CARTESIAN_POINT('Ctrl Pts',(-19.3896325300255,-25.5494132211255,
124.919115026399)) ;
#52972 = CARTESIAN_POINT('Ctrl Pts',(-19.6004203943415,-25.7392694660659,
124.60247790701)) ;
#52973 = CARTESIAN_POINT('Ctrl Pts',(-19.6482244565418,-25.5592803855855,
124.900141299554)) ;
#52974 = CARTESIAN_POINT('Ctrl Pts',(-19.804222528808,-25.7492629082859,124.551424075459)) ;
#52975 = CARTESIAN_POINT('Ctrl Pts',(-19.9029765856325,-25.5692738278054,
124.836321404756)) ;
#52976 = CARTESIAN_POINT('Ctrl Pts',(-19.9966241110481,-25.7592945818862,
124.465058729289)) ;
#52977 = CARTESIAN_POINT('Ctrl Pts',(-20.1434775003674,-25.5793055014057,
124.728362358445)) ;
#52978 = CARTESIAN_POINT('Ctrl Pts',(-20.1684200868147,-25.7691610169992,
124.348807750651)) ;
#52979 = CARTESIAN_POINT('Ctrl Pts',(-20.3582214203252,-25.5891719365187,
124.583046155799)) ;
#52980 = CARTESIAN_POINT('Ctrl Pts',(-20.3194620562051,-25.7791484675323,
124.202992595232)) ;
#52981 = CARTESIAN_POINT('Ctrl Pts',(-20.5470220994703,-25.5991593870518,
124.400775187966)) ;
#52982 = CARTESIAN_POINT('Ctrl Pts',(-20.4424893830337,-25.7890933973602,
124.033909844264)) ;
#52983 = CARTESIAN_POINT('Ctrl Pts',(-20.7008042111351,-25.6091043168797,
124.189419968522)) ;
#52984 = CARTESIAN_POINT('Ctrl Pts',(-20.5350834451132,-25.7991382924153,
123.844138661879)) ;
#52985 = CARTESIAN_POINT('Ctrl Pts',(-20.816544361093,-25.6191492119349,123.952204828917)) ;
#52986 = CARTESIAN_POINT('Ctrl Pts',(-20.5924455699357,-25.8090003541012,
123.64488433114)) ;
#52987 = CARTESIAN_POINT('Ctrl Pts',(-20.888244530367,-25.6290112736207,123.703135751178)) ;
#52988 = CARTESIAN_POINT('Ctrl Pts',(-20.6150418051958,-25.818992076888,123.436062409259)) ;
#52989 = CARTESIAN_POINT('Ctrl Pts',(-20.9164870896894,-25.6390029964076,
123.442107956855)) ;
#52990 = CARTESIAN_POINT('Ctrl Pts',(-20.6010425706833,-25.828924291128,123.22772327375)) ;
#52991 = CARTESIAN_POINT('Ctrl Pts',(-20.898985287242,-25.6489352106475,123.181683998665)) ;
#52992 = CARTESIAN_POINT('Ctrl Pts',(-20.5515128182878,-25.8388636096937,
123.024716518231)) ;
#52993 = CARTESIAN_POINT('Ctrl Pts',(-20.8370703425302,-25.6588745292133,
122.927926047606)) ;
#52994 = CARTESIAN_POINT('Ctrl Pts',(-20.4664264572267,-25.8489077844696,
122.831461041933)) ;
#52995 = CARTESIAN_POINT('Ctrl Pts',(-20.7307098428418,-25.6689187039891,
122.686357803528)) ;
#52996 = CARTESIAN_POINT('Ctrl Pts',(-20.3511977884892,-25.8587783385346,
122.658884676041)) ;
#52997 = CARTESIAN_POINT('Ctrl Pts',(-20.5866715411754,-25.6787892580541,
122.470638672497)) ;
#52998 = CARTESIAN_POINT('Ctrl Pts',(-20.2068205658345,-25.8687433208888,
122.507083215677)) ;
#52999 = CARTESIAN_POINT('Ctrl Pts',(-20.406197903006,-25.6887542404083,122.280888722029)) ;
#53000 = CARTESIAN_POINT('Ctrl Pts',(-20.0369803709032,-25.8787740237786,
122.382099598688)) ;
#53001 = CARTESIAN_POINT('Ctrl Pts',(-20.1938959520374,-25.6987849432981,
122.124661424507)) ;
#53002 = CARTESIAN_POINT('Ctrl Pts',(-19.8507320191725,-25.8886663638038,
122.289510710408)) ;
#53003 = CARTESIAN_POINT('Ctrl Pts',(-19.9610841221135,-25.7086772833233,
122.008927766371)) ;
#53004 = CARTESIAN_POINT('Ctrl Pts',(-19.6480507991876,-25.8987195969637,
122.229703855428)) ;
#53005 = CARTESIAN_POINT('Ctrl Pts',(-19.7077317559677,-25.7187305164833,
121.934171888426)) ;
#53006 = CARTESIAN_POINT('Ctrl Pts',(-19.4416056541742,-25.9086008414405,
122.206269923725)) ;
#53007 = CARTESIAN_POINT('Ctrl Pts',(-19.4496748815484,-25.72861176096,121.904882259166)) ;
#53008 = CARTESIAN_POINT('Ctrl Pts',(-19.2311053037005,-25.9186339623115,
122.219073769285)) ;
#53009 = CARTESIAN_POINT('Ctrl Pts',(-19.186549549454,-25.738644881831,121.920889891472)) ;
#53010 = CARTESIAN_POINT('Ctrl Pts',(-19.0290124695695,-25.9285151725866,
122.267326061068)) ;
#53011 = CARTESIAN_POINT('Ctrl Pts',(-18.9339340957259,-25.7485260921061,
121.981208014828)) ;
#53012 = CARTESIAN_POINT('Ctrl Pts',(-18.8349223161673,-25.9385772483559,
122.351365482574)) ;
#53013 = CARTESIAN_POINT('Ctrl Pts',(-18.6913224501782,-25.7585881678754,
122.086259918591)) ;
#53014 = CARTESIAN_POINT('Ctrl Pts',(-18.6618773393018,-25.9484343067377,
122.465428901543)) ;
#53015 = CARTESIAN_POINT('Ctrl Pts',(-18.4750177695224,-25.7684452262572,
122.228841554535)) ;
#53016 = CARTESIAN_POINT('Ctrl Pts',(-18.508920686306,-25.9584288620267,122.609440179343)) ;
#53017 = CARTESIAN_POINT('Ctrl Pts',(-18.2838238475802,-25.7784397815462,
122.408857735578)) ;
#53018 = CARTESIAN_POINT('Ctrl Pts',(-18.3840592104564,-25.9683547495622,
122.776670958682)) ;
#53019 = CARTESIAN_POINT('Ctrl Pts',(-18.1277492564418,-25.7883656690817,
122.617897877515)) ;
#53020 = CARTESIAN_POINT('Ctrl Pts',(-18.2891587151755,-25.9783797695574,
122.964835760839)) ;
#53021 = CARTESIAN_POINT('Ctrl Pts',(-18.0091260992142,-25.798390689077,122.853105228262)) ;
#53022 = CARTESIAN_POINT('Ctrl Pts',(-18.2290682932492,-25.9882771466611,
123.164050381415)) ;
#53023 = CARTESIAN_POINT('Ctrl Pts',(-17.934015776066,-25.8082880661806,123.102124235141)) ;
#53024 = CARTESIAN_POINT('Ctrl Pts',(-18.2037946806714,-25.998267383742,123.3725562714)) ;
#53025 = CARTESIAN_POINT('Ctrl Pts',(-17.9024264990664,-25.8182783032615,
123.362756958179)) ;
#53026 = CARTESIAN_POINT('Ctrl Pts',(-18.2155658880432,-26.0083039965508,
123.583225928318)) ;
#53027 = CARTESIAN_POINT('Ctrl Pts',(-17.9171433200862,-25.8283149160703,
123.626094022958)) ;
#53028 = CARTESIAN_POINT('Ctrl Pts',(-18.2625157876823,-26.0181538799688,
123.784916905059)) ;
#53029 = CARTESIAN_POINT('Ctrl Pts',(-17.9758333007663,-25.8381647994883,
123.878206838419)) ;
#53030 = CARTESIAN_POINT('Ctrl Pts',(-18.3446404620089,-26.0281574968712,
123.978504100519)) ;
#53031 = CARTESIAN_POINT('Ctrl Pts',(-18.0784917993927,-25.8481684163907,
124.120189945172)) ;
#53032 = CARTESIAN_POINT('Ctrl Pts',(-18.4590946254507,-26.0381469086364,
124.154624318019)) ;
#53033 = CARTESIAN_POINT('Ctrl Pts',(-18.2215613396099,-25.8581578281559,
124.340338257024)) ;
#53034 = CARTESIAN_POINT('Ctrl Pts',(-18.6028685076964,-26.0481656699812,
124.308517074879)) ;
#53035 = CARTESIAN_POINT('Ctrl Pts',(-18.4012825633872,-25.8681765895007,
124.53270427943)) ;
#53036 = CARTESIAN_POINT('Ctrl Pts',(-18.8247544491437,-26.0613843453623,
124.475917456974)) ;
#53037 = CARTESIAN_POINT('Ctrl Pts',(-18.6786331145576,-25.8813952648818,
124.741942400174)) ;
#53038 = CARTESIAN_POINT('Ctrl Pts',(-19.0869231326057,-26.074694652607,124.582399606467)) ;
#53039 = CARTESIAN_POINT('Ctrl Pts',(-19.0063037436097,-25.8947055721265,
124.87503799084)) ;
#53040 = CARTESIAN_POINT('Ctrl Pts',(-19.363072798974,-26.087932318833,124.616808325891)) ;
#53041 = CARTESIAN_POINT('Ctrl Pts',(-19.3515492792957,-25.9079432383525,
124.91805906262)) ;
#53042 = CARTESIAN_POINT('Ctrl Pts',(-19.5713918157783,-26.0978520142437,
124.606935546831)) ;
#53043 = CARTESIAN_POINT('Ctrl Pts',(-19.6119358669811,-25.9178629337632,
124.905712873674)) ;
#53044 = CARTESIAN_POINT('Ctrl Pts',(-19.7774861802108,-26.1079048812422,
124.560193148227)) ;
#53045 = CARTESIAN_POINT('Ctrl Pts',(-19.8695568707557,-25.9279158007617,
124.847282647042)) ;
#53046 = CARTESIAN_POINT('Ctrl Pts',(-19.9686281474796,-26.1177602895715,
124.480186051397)) ;
#53047 = CARTESIAN_POINT('Ctrl Pts',(-20.1084811471548,-25.937771209091,124.747272818746)) ;
#53048 = CARTESIAN_POINT('Ctrl Pts',(-20.14637377885,-26.1277989212481,124.366438520996)) ;
#53049 = CARTESIAN_POINT('Ctrl Pts',(-20.3306652048825,-25.9478098407676,
124.605081165826)) ;
#53050 = CARTESIAN_POINT('Ctrl Pts',(-20.3519626171017,-26.1411011035151,
124.176812384291)) ;
#53051 = CARTESIAN_POINT('Ctrl Pts',(-20.5876341490242,-25.9611120230346,
124.368071353143)) ;
#53052 = CARTESIAN_POINT('Ctrl Pts',(-20.5406207798638,-26.157646116598,123.879908726874)) ;
#53053 = CARTESIAN_POINT('Ctrl Pts',(-20.8234715240876,-25.9776570361175,
123.996893725458)) ;
#53054 = CARTESIAN_POINT('Ctrl Pts',(-20.6172088047157,-26.1742981326742,
123.534214772238)) ;
#53055 = CARTESIAN_POINT('Ctrl Pts',(-20.919190598142,-25.9943090521937,123.56485434145)) ;
#53056 = CARTESIAN_POINT('Ctrl Pts',(-20.6051217054238,-26.1875212235794,
123.256506578879)) ;
#53057 = CARTESIAN_POINT('Ctrl Pts',(-20.9040855808188,-26.007532143099,123.21765581557)) ;
#53058 = CARTESIAN_POINT('Ctrl Pts',(-20.5603924279369,-26.1974821831388,
123.05192147308)) ;
#53059 = CARTESIAN_POINT('Ctrl Pts',(-20.8481710290793,-26.0174931026583,
122.961938491769)) ;
#53060 = CARTESIAN_POINT('Ctrl Pts',(-20.4800725687243,-26.2075069798899,
122.857083849691)) ;
#53061 = CARTESIAN_POINT('Ctrl Pts',(-20.747767274539,-26.0275178994094,122.718386742788)) ;
#53062 = CARTESIAN_POINT('Ctrl Pts',(-20.3313987181556,-26.2207314272857,
122.62210740137)) ;
#53063 = CARTESIAN_POINT('Ctrl Pts',(-20.5619333819627,-26.0407423468052,
122.424679164623)) ;
#53064 = CARTESIAN_POINT('Ctrl Pts',(-20.0717140768469,-26.2373652119848,
122.382085717408)) ;
#53065 = CARTESIAN_POINT('Ctrl Pts',(-20.2373134507681,-26.0573761315043,
122.124643357243)) ;
#53066 = CARTESIAN_POINT('Ctrl Pts',(-19.6815099293272,-26.2572678787097,
122.218198924247)) ;
#53067 = CARTESIAN_POINT('Ctrl Pts',(-19.7495611854334,-26.0772787982292,
121.919792632076)) ;
#53068 = CARTESIAN_POINT('Ctrl Pts',(-19.2589510713564,-26.2771681064916,
122.196756051272)) ;
#53069 = CARTESIAN_POINT('Ctrl Pts',(-19.2213622812154,-26.0971790260111,
121.892991857086)) ;
#53070 = CARTESIAN_POINT('Ctrl Pts',(-18.8539777559444,-26.2970855940231,
122.320631928225)) ;
#53071 = CARTESIAN_POINT('Ctrl Pts',(-18.7151476740853,-26.1170965135426,
122.047840068717)) ;
#53072 = CARTESIAN_POINT('Ctrl Pts',(-18.5152044782925,-26.31701511984,122.575227475119)) ;
#53073 = CARTESIAN_POINT('Ctrl Pts',(-18.2916834897623,-26.1370260393595,
122.366086543186)) ;
#53074 = CARTESIAN_POINT('Ctrl Pts',(-18.2833320361407,-26.3369773877262,
122.930774152276)) ;
#53075 = CARTESIAN_POINT('Ctrl Pts',(-18.0018457089775,-26.1569883072458,
122.810521280933)) ;
#53076 = CARTESIAN_POINT('Ctrl Pts',(-18.187043146482,-26.3568675826784,123.342528444568)) ;
#53077 = CARTESIAN_POINT('Ctrl Pts',(-17.8814876926625,-26.176878502198,123.32521358711)) ;
#53078 = CARTESIAN_POINT('Ctrl Pts',(-18.2360005587426,-26.3767578274247,
123.762699469235)) ;
#53079 = CARTESIAN_POINT('Ctrl Pts',(-17.9426863606114,-26.1967687469442,
123.850425839093)) ;
#53080 = CARTESIAN_POINT('Ctrl Pts',(-18.4278756911333,-26.3968321999872,
124.143912754518)) ;
#53081 = CARTESIAN_POINT('Ctrl Pts',(-18.1825328724787,-26.2168431195067,
124.326942241205)) ;
#53082 = CARTESIAN_POINT('Ctrl Pts',(-18.7338400806782,-26.4166175773475,
124.432727082962)) ;
#53083 = CARTESIAN_POINT('Ctrl Pts',(-18.5649877789369,-26.236628496867,124.68795667233)) ;
#53084 = CARTESIAN_POINT('Ctrl Pts',(-19.1228257813227,-26.4365794514146,
124.602461953777)) ;
#53085 = CARTESIAN_POINT('Ctrl Pts',(-19.0512197802809,-26.2565903709341,
124.900124064348)) ;
#53086 = CARTESIAN_POINT('Ctrl Pts',(-19.5468805261724,-26.4565594269051,
124.628280549384)) ;
#53087 = CARTESIAN_POINT('Ctrl Pts',(-19.5812880978611,-26.2765703464246,
124.932395779943)) ;
#53088 = CARTESIAN_POINT('Ctrl Pts',(-19.9511224656437,-26.476371856783,124.509636259826)) ;
#53089 = CARTESIAN_POINT('Ctrl Pts',(-20.0865875255273,-26.2963827763026,
124.784090581465)) ;
#53090 = CARTESIAN_POINT('Ctrl Pts',(-20.2937255390238,-26.4963519648733,
124.258562719939)) ;
#53091 = CARTESIAN_POINT('Ctrl Pts',(-20.5148410358532,-26.3163628843929,
124.470248873586)) ;
#53092 = CARTESIAN_POINT('Ctrl Pts',(-20.5290130856317,-26.5162463484706,
123.906914863893)) ;
#53093 = CARTESIAN_POINT('Ctrl Pts',(-20.8089496482753,-26.3362572679901,
124.030690459126)) ;
#53094 = CARTESIAN_POINT('Ctrl Pts',(-20.6306703899268,-26.5361732764478,
123.495687774504)) ;
#53095 = CARTESIAN_POINT('Ctrl Pts',(-20.9360216457934,-26.3561841959673,
123.516657893166)) ;
#53096 = CARTESIAN_POINT('Ctrl Pts',(-20.58650883794,-26.556068133749,123.074882964739)) ;
#53097 = CARTESIAN_POINT('Ctrl Pts',(-20.8808211230265,-26.3760790532686,
122.99065319296)) ;
#53098 = CARTESIAN_POINT('Ctrl Pts',(-20.3997314232741,-26.5761073273527,
122.691961278104)) ;
#53099 = CARTESIAN_POINT('Ctrl Pts',(-20.6473502028228,-26.3961182468722,
122.512000068487)) ;
#53100 = CARTESIAN_POINT('Ctrl Pts',(-20.0964143874877,-26.5959472952634,
122.39871350997)) ;
#53101 = CARTESIAN_POINT('Ctrl Pts',(-20.2682064550597,-26.415958214783,122.14544089517)) ;
#53102 = CARTESIAN_POINT('Ctrl Pts',(-19.7103017728837,-26.6158621122275,
122.224956806707)) ;
#53103 = CARTESIAN_POINT('Ctrl Pts',(-19.7855675978862,-26.435873031747,121.928243360059)) ;
#53104 = CARTESIAN_POINT('Ctrl Pts',(-19.2874660199691,-26.6358043576238,
122.193640512695)) ;
#53105 = CARTESIAN_POINT('Ctrl Pts',(-19.257023805954,-26.4558152771433,121.889095738547)) ;
#53106 = CARTESIAN_POINT('Ctrl Pts',(-18.8804463278445,-26.6556764057383,
122.30743483587)) ;
#53107 = CARTESIAN_POINT('Ctrl Pts',(-18.7482497387927,-26.4756873252578,
122.031335489751)) ;
#53108 = CARTESIAN_POINT('Ctrl Pts',(-18.534656096257,-26.6756874706924,122.555130633679)) ;
#53109 = CARTESIAN_POINT('Ctrl Pts',(-18.3160101802198,-26.4956983902119,
122.340952921464)) ;
#53110 = CARTESIAN_POINT('Ctrl Pts',(-18.2958118938891,-26.695498994996,122.902353695436)) ;
#53111 = CARTESIAN_POINT('Ctrl Pts',(-18.0174531567046,-26.5155099145155,
122.774978345783)) ;
#53112 = CARTESIAN_POINT('Ctrl Pts',(-18.1886180442207,-26.7155942069594,
123.315793755655)) ;
#53113 = CARTESIAN_POINT('Ctrl Pts',(-17.8834572828486,-26.5356051264789,
123.291778439974)) ;
#53114 = CARTESIAN_POINT('Ctrl Pts',(-18.2284182206714,-26.7353749308792,
123.734667026007)) ;
#53115 = CARTESIAN_POINT('Ctrl Pts',(-17.9332038024577,-26.5553858503987,
123.815368387787)) ;
#53116 = CARTESIAN_POINT('Ctrl Pts',(-18.4096610154177,-26.755366006522,124.118979626269)) ;
#53117 = CARTESIAN_POINT('Ctrl Pts',(-18.1597535328344,-26.5753769260415,
124.295760857053)) ;
#53118 = CARTESIAN_POINT('Ctrl Pts',(-18.7099242034501,-26.775247945565,124.416730191879)) ;
#53119 = CARTESIAN_POINT('Ctrl Pts',(-18.5350790244108,-26.5952588650845,
124.667951356178)) ;
#53120 = CARTESIAN_POINT('Ctrl Pts',(-19.0947640893078,-26.7952005500682,
124.595125233846)) ;
#53121 = CARTESIAN_POINT('Ctrl Pts',(-19.0161267181659,-26.6152114695878,
124.890949085933)) ;
#53122 = CARTESIAN_POINT('Ctrl Pts',(-19.5163545803771,-26.8150994187989,
124.631394180349)) ;
#53123 = CARTESIAN_POINT('Ctrl Pts',(-19.543113858081,-26.6351103383184,124.936289536642)) ;
#53124 = CARTESIAN_POINT('Ctrl Pts',(-19.9249223900067,-26.8349928186085,
124.522185577163)) ;
#53125 = CARTESIAN_POINT('Ctrl Pts',(-20.0538241490257,-26.655003738128,124.799784245875)) ;
#53126 = CARTESIAN_POINT('Ctrl Pts',(-20.2724780813472,-26.8549019494485,
124.28036241543)) ;
#53127 = CARTESIAN_POINT('Ctrl Pts',(-20.4882718451227,-26.674912868968,124.49750710335)) ;
#53128 = CARTESIAN_POINT('Ctrl Pts',(-20.5176077328645,-26.8749340492121,
123.93208451665)) ;
#53129 = CARTESIAN_POINT('Ctrl Pts',(-20.7946862218573,-26.6949449687316,
124.062171882856)) ;
#53130 = CARTESIAN_POINT('Ctrl Pts',(-20.6098098899142,-26.8914661223815,
123.592826429201)) ;
#53131 = CARTESIAN_POINT('Ctrl Pts',(-20.9099487233214,-26.711477041901,123.638071483034)) ;
#53132 = CARTESIAN_POINT('Ctrl Pts',(-20.6110911401444,-26.9048014629875,
123.312495899499)) ;
#53133 = CARTESIAN_POINT('Ctrl Pts',(-20.9115489479595,-26.724812382507,123.287684923659)) ;
#53134 = CARTESIAN_POINT('Ctrl Pts',(-20.5764556782728,-26.9146440215272,
123.108474267684)) ;
#53135 = CARTESIAN_POINT('Ctrl Pts',(-20.8682561093862,-26.7346549410467,
123.032650001393)) ;
#53136 = CARTESIAN_POINT('Ctrl Pts',(-20.505658826445,-26.9246959283771,122.909381601415)) ;
#53137 = CARTESIAN_POINT('Ctrl Pts',(-20.7797708304391,-26.7447068478966,
122.783795004268)) ;
#53138 = CARTESIAN_POINT('Ctrl Pts',(-20.3681524800132,-26.937944442768,122.66718118586)) ;
#53139 = CARTESIAN_POINT('Ctrl Pts',(-20.6078481494887,-26.7579553622875,
122.480989791496)) ;
#53140 = CARTESIAN_POINT('Ctrl Pts',(-20.1207621070725,-26.9545436177157,
122.415419343604)) ;
#53141 = CARTESIAN_POINT('Ctrl Pts',(-20.2986718810643,-26.7745545372353,
122.166348506496)) ;
#53142 = CARTESIAN_POINT('Ctrl Pts',(-19.8026232747545,-26.9711324035108,
122.26320952748)) ;
#53143 = CARTESIAN_POINT('Ctrl Pts',(-19.9009478345659,-26.7911433230303,
121.97604809687)) ;
#53144 = CARTESIAN_POINT('Ctrl Pts',(-19.5282752383854,-26.9844082198528,
122.211739570841)) ;
#53145 = CARTESIAN_POINT('Ctrl Pts',(-19.558049630064,-26.8044191393723,121.911724128013)) ;
#53146 = CARTESIAN_POINT('Ctrl Pts',(-19.318603845964,-26.9943820706466,122.209154533502)) ;
#53147 = CARTESIAN_POINT('Ctrl Pts',(-19.2959531359057,-26.8143929901661,
121.908486612894)) ;
#53148 = CARTESIAN_POINT('Ctrl Pts',(-19.1105694524777,-27.004411102739,122.243420895193)) ;
#53149 = CARTESIAN_POINT('Ctrl Pts',(-19.0359115385964,-26.8244220222585,
121.951317774941)) ;
#53150 = CARTESIAN_POINT('Ctrl Pts',(-18.9143115037935,-27.0143012282409,
122.3121202507)) ;
#53151 = CARTESIAN_POINT('Ctrl Pts',(-18.7905877642444,-26.8343121477604,
122.037189061852)) ;
#53152 = CARTESIAN_POINT('Ctrl Pts',(-18.730980558228,-27.0242937065124,122.414640859144)) ;
#53153 = CARTESIAN_POINT('Ctrl Pts',(-18.5614228029118,-26.8443046260319,
122.165337469909)) ;
#53154 = CARTESIAN_POINT('Ctrl Pts',(-18.5687919015397,-27.0342449216098,
122.546836923164)) ;
#53155 = CARTESIAN_POINT('Ctrl Pts',(-18.3586851594981,-26.8542558411293,
122.330580371029)) ;
#53156 = CARTESIAN_POINT('Ctrl Pts',(-18.4308500276103,-27.0442934233648,
122.706804310669)) ;
#53157 = CARTESIAN_POINT('Ctrl Pts',(-18.1862556412038,-26.8643043428843,
122.53053785768)) ;
#53158 = CARTESIAN_POINT('Ctrl Pts',(-18.324778682574,-27.0541347729816,122.884464775646)) ;
#53159 = CARTESIAN_POINT('Ctrl Pts',(-18.0536640722972,-26.8741456925011,
122.75261195662)) ;
#53160 = CARTESIAN_POINT('Ctrl Pts',(-18.2496811215229,-27.0641210640018,
123.080480376407)) ;
#53161 = CARTESIAN_POINT('Ctrl Pts',(-17.9597894557877,-26.8841319835213,
122.997630523659)) ;
#53162 = CARTESIAN_POINT('Ctrl Pts',(-18.2098424384287,-27.0740576757304,
123.285580848838)) ;
#53163 = CARTESIAN_POINT('Ctrl Pts',(-17.9099883259853,-26.8940685952499,
123.254005646112)) ;
#53164 = CARTESIAN_POINT('Ctrl Pts',(-18.206286456587,-27.084107551098,123.496809557806)) ;
#53165 = CARTESIAN_POINT('Ctrl Pts',(-17.9055405280551,-26.9041184706175,
123.518041545868)) ;
#53166 = CARTESIAN_POINT('Ctrl Pts',(-18.2386548673565,-27.0939580096334,
123.701367310787)) ;
#53167 = CARTESIAN_POINT('Ctrl Pts',(-17.9459982767413,-26.9139689291529,
123.773739288648)) ;
#53168 = CARTESIAN_POINT('Ctrl Pts',(-18.3063479731576,-27.1039299465862,
123.899751686817)) ;
#53169 = CARTESIAN_POINT('Ctrl Pts',(-18.0306120392557,-26.9239408661057,
124.021720774611)) ;
#53170 = CARTESIAN_POINT('Ctrl Pts',(-18.4077546179831,-27.1139254035183,
124.083836779179)) ;
#53171 = CARTESIAN_POINT('Ctrl Pts',(-18.1573679301595,-26.9339363230378,
124.251828560832)) ;
#53172 = CARTESIAN_POINT('Ctrl Pts',(-18.5402337139463,-27.1239582105714,
124.247943977524)) ;
#53173 = CARTESIAN_POINT('Ctrl Pts',(-18.3229646346915,-26.9439691300909,
124.456964358689)) ;
#53174 = CARTESIAN_POINT('Ctrl Pts',(-18.696288367492,-27.1338180971613,124.384394875918)) ;
#53175 = CARTESIAN_POINT('Ctrl Pts',(-18.5180312777449,-26.9538290166809,
124.627530239121)) ;
#53176 = CARTESIAN_POINT('Ctrl Pts',(-18.8757602839204,-27.1438071777266,
124.493403942456)) ;
#53177 = CARTESIAN_POINT('Ctrl Pts',(-18.7423698225916,-26.9638180972461,
124.763794005634)) ;
#53178 = CARTESIAN_POINT('Ctrl Pts',(-19.0703285555277,-27.1537386569357,
124.569162296289)) ;
#53179 = CARTESIAN_POINT('Ctrl Pts',(-18.9855793301058,-26.9737495764553,
124.858494604094)) ;
#53180 = CARTESIAN_POINT('Ctrl Pts',(-19.2761569854026,-27.1637245163817,
124.610551053502)) ;
#53181 = CARTESIAN_POINT('Ctrl Pts',(-19.2428644372017,-26.9837354359012,
124.91023326765)) ;
#53182 = CARTESIAN_POINT('Ctrl Pts',(-19.4871247300181,-27.1737626670289,
124.61522608717)) ;
#53183 = CARTESIAN_POINT('Ctrl Pts',(-19.5065740592413,-26.9937735865484,
124.916079842873)) ;
#53184 = CARTESIAN_POINT('Ctrl Pts',(-19.6918470853474,-27.1836107575333,
124.584217748348)) ;
#53185 = CARTESIAN_POINT('Ctrl Pts',(-19.762477808703,-27.0036216770528,124.877322071589)) ;
#53186 = CARTESIAN_POINT('Ctrl Pts',(-19.8923339922519,-27.1936716660512,
124.516888561277)) ;
#53187 = CARTESIAN_POINT('Ctrl Pts',(-20.0130872707817,-27.0136825855708,
124.793163185026)) ;
#53188 = CARTESIAN_POINT('Ctrl Pts',(-20.0749863200746,-27.2035665132092,
124.417294329767)) ;
#53189 = CARTESIAN_POINT('Ctrl Pts',(-20.2414042797993,-27.0235774327288,
124.668672645465)) ;
#53190 = CARTESIAN_POINT('Ctrl Pts',(-20.2386525978464,-27.2135081852543,
124.287347778684)) ;
#53191 = CARTESIAN_POINT('Ctrl Pts',(-20.4459889976083,-27.0335191047738,
124.506241389388)) ;
#53192 = CARTESIAN_POINT('Ctrl Pts',(-20.3782156387396,-27.2235107123797,
124.130014539962)) ;
#53193 = CARTESIAN_POINT('Ctrl Pts',(-20.62044484462,-27.0435216318993,124.309576543661)) ;
#53194 = CARTESIAN_POINT('Ctrl Pts',(-20.4883897656227,-27.2335455035672,
123.950121732222)) ;
#53195 = CARTESIAN_POINT('Ctrl Pts',(-20.7581648057283,-27.0535564230867,
124.084711962501)) ;
#53196 = CARTESIAN_POINT('Ctrl Pts',(-20.5645263195821,-27.2433903834263,
123.757649358259)) ;
#53197 = CARTESIAN_POINT('Ctrl Pts',(-20.8533381773429,-27.0634013029458,
123.844121950457)) ;
#53198 = CARTESIAN_POINT('Ctrl Pts',(-20.6070596189447,-27.2533762640448,
123.552103054265)) ;
#53199 = CARTESIAN_POINT('Ctrl Pts',(-20.9065073832557,-27.0733871835643,
123.587189440401)) ;
#53200 = CARTESIAN_POINT('Ctrl Pts',(-20.6133781384881,-27.263310987138,123.343300034861)) ;
#53201 = CARTESIAN_POINT('Ctrl Pts',(-20.9144081116271,-27.0833219066575,
123.326185418471)) ;
#53202 = CARTESIAN_POINT('Ctrl Pts',(-20.5827915728053,-27.2733688274492,
123.134108713238)) ;
#53203 = CARTESIAN_POINT('Ctrl Pts',(-20.8761775036442,-27.0933797469687,
123.064696003657)) ;
#53204 = CARTESIAN_POINT('Ctrl Pts',(-20.5182131701365,-27.2831893148457,
122.937983170637)) ;
#53205 = CARTESIAN_POINT('Ctrl Pts',(-20.7954566742065,-27.1032002343652,
122.819537535194)) ;
#53206 = CARTESIAN_POINT('Ctrl Pts',(-20.4185100813219,-27.2932497161908,
122.751485493187)) ;
#53207 = CARTESIAN_POINT('Ctrl Pts',(-20.6708300596876,-27.1132606357103,
122.586414372741)) ;
#53208 = CARTESIAN_POINT('Ctrl Pts',(-20.2893670926231,-27.3031806817437,
122.587408843276)) ;
#53209 = CARTESIAN_POINT('Ctrl Pts',(-20.5094030854592,-27.1231916012632,
122.381316698496)) ;
#53210 = CARTESIAN_POINT('Ctrl Pts',(-20.1339171194866,-27.3131195440802,
122.447821260435)) ;
#53211 = CARTESIAN_POINT('Ctrl Pts',(-20.3150919760581,-27.1331304635997,
122.206830149551)) ;
#53212 = CARTESIAN_POINT('Ctrl Pts',(-19.9557909141703,-27.3231052750064,
122.336681000777)) ;
#53213 = CARTESIAN_POINT('Ctrl Pts',(-20.0924353594494,-27.1431161945259,
122.067902692348)) ;
#53214 = CARTESIAN_POINT('Ctrl Pts',(-19.7602720484493,-27.3331296604338,
122.258075382976)) ;
#53215 = CARTESIAN_POINT('Ctrl Pts',(-19.8480377025749,-27.1531405799533,
121.969643384991)) ;
#53216 = CARTESIAN_POINT('Ctrl Pts',(-19.5565899889511,-27.3430329447871,
122.214817299832)) ;
#53217 = CARTESIAN_POINT('Ctrl Pts',(-19.5934350819641,-27.1630438643066,
121.915568323224)) ;
#53218 = CARTESIAN_POINT('Ctrl Pts',(-19.3452475882926,-27.3530929493651,
122.207539583544)) ;
#53219 = CARTESIAN_POINT('Ctrl Pts',(-19.3292573389798,-27.1731038688846,
121.906468774083)) ;
#53220 = CARTESIAN_POINT('Ctrl Pts',(-19.1402979082901,-27.3629362184342,
122.236294727092)) ;
#53221 = CARTESIAN_POINT('Ctrl Pts',(-19.0730690560102,-27.1829471379537,
121.942410468897)) ;
#53222 = CARTESIAN_POINT('Ctrl Pts',(-18.9404022090521,-27.3729267840419,
122.300676483571)) ;
#53223 = CARTESIAN_POINT('Ctrl Pts',(-18.8231985705939,-27.1929377035614,
122.022885561969)) ;
#53224 = CARTESIAN_POINT('Ctrl Pts',(-18.7558672982378,-27.3828549158207,
122.398221029593)) ;
#53225 = CARTESIAN_POINT('Ctrl Pts',(-18.5925284414569,-27.2028658353402,
122.144814464852)) ;
#53226 = CARTESIAN_POINT('Ctrl Pts',(-18.5898557423788,-27.3928428029016,
122.526807079815)) ;
#53227 = CARTESIAN_POINT('Ctrl Pts',(-18.3850125183994,-27.2128537224211,
122.305545417157)) ;
#53228 = CARTESIAN_POINT('Ctrl Pts',(-18.4482910581977,-27.4028787524703,
122.68324070113)) ;
#53229 = CARTESIAN_POINT('Ctrl Pts',(-18.2080550366544,-27.2228896719898,
122.501085855534)) ;
#53230 = CARTESIAN_POINT('Ctrl Pts',(-18.3377591304148,-27.4127336388491,
122.858492901612)) ;
#53231 = CARTESIAN_POINT('Ctrl Pts',(-18.0698877943292,-27.2327445583686,
122.720150718042)) ;
#53232 = CARTESIAN_POINT('Ctrl Pts',(-18.2579406650141,-27.422733053197,123.052931220241)) ;
#53233 = CARTESIAN_POINT('Ctrl Pts',(-17.9701127118475,-27.2427439727165,
122.963197940017)) ;
#53234 = CARTESIAN_POINT('Ctrl Pts',(-18.2133303124607,-27.4326282183875,
123.256154680513)) ;
#53235 = CARTESIAN_POINT('Ctrl Pts',(-17.9143476219476,-27.252639137907,123.217227543727)) ;
#53236 = CARTESIAN_POINT('Ctrl Pts',(-18.204564058286,-27.4426885370794,123.467444615832)) ;
#53237 = CARTESIAN_POINT('Ctrl Pts',(-17.9033877646461,-27.262699456599,123.481339637192)) ;
#53238 = CARTESIAN_POINT('Ctrl Pts',(-18.2319167259409,-27.4525386688555,
123.672729223044)) ;
#53239 = CARTESIAN_POINT('Ctrl Pts',(-17.9375767427707,-27.272549588375,123.737946697401)) ;
#53240 = CARTESIAN_POINT('Ctrl Pts',(-18.2951613085268,-27.4625692393058,
123.87388597203)) ;
#53241 = CARTESIAN_POINT('Ctrl Pts',(-18.0166306720555,-27.2825801588253,
123.989393136794)) ;
#53242 = CARTESIAN_POINT('Ctrl Pts',(-18.392639370384,-27.4725833899786,124.060501742582)) ;
#53243 = CARTESIAN_POINT('Ctrl Pts',(-18.1384764759036,-27.2925943094981,
124.222663794601)) ;
#53244 = CARTESIAN_POINT('Ctrl Pts',(-18.5192133454885,-27.482476323524,124.225536129967)) ;
#53245 = CARTESIAN_POINT('Ctrl Pts',(-18.2966929163298,-27.3024872430435,
124.428958569374)) ;
#53246 = CARTESIAN_POINT('Ctrl Pts',(-18.6738373848897,-27.4924658375142,
124.367619074625)) ;
#53247 = CARTESIAN_POINT('Ctrl Pts',(-18.4899718702957,-27.3124767570338,
124.606563738886)) ;
#53248 = CARTESIAN_POINT('Ctrl Pts',(-18.8501175734663,-27.5024196081667,
124.480434768082)) ;
#53249 = CARTESIAN_POINT('Ctrl Pts',(-18.7103215044996,-27.3224305276862,
124.747585098985)) ;
#53250 = CARTESIAN_POINT('Ctrl Pts',(-19.0451588516024,-27.5124673768272,
124.561494657488)) ;
#53251 = CARTESIAN_POINT('Ctrl Pts',(-18.9541222140301,-27.3324782963468,
124.84891159702)) ;
#53252 = CARTESIAN_POINT('Ctrl Pts',(-19.2470679046849,-27.522309103267,124.606762346263)) ;
#53253 = CARTESIAN_POINT('Ctrl Pts',(-19.20650929812,-27.3423200227866,124.905498198181)) ;
#53254 = CARTESIAN_POINT('Ctrl Pts',(-19.4567187804264,-27.5322946200898,
124.616878516761)) ;
#53255 = CARTESIAN_POINT('Ctrl Pts',(-19.468573060207,-27.3523055396093,124.918145049147)) ;
#53256 = CARTESIAN_POINT('Ctrl Pts',(-19.6640500637913,-27.5422339517853,
124.590629381917)) ;
#53257 = CARTESIAN_POINT('Ctrl Pts',(-19.7277379052966,-27.3622448713049,
124.885335148881)) ;
#53258 = CARTESIAN_POINT('Ctrl Pts',(-19.8656328349993,-27.5522737214829,
124.52812532427)) ;
#53259 = CARTESIAN_POINT('Ctrl Pts',(-19.9797167084176,-27.3722846410024,
124.807206664891)) ;
#53260 = CARTESIAN_POINT('Ctrl Pts',(-20.050539305733,-27.5621618827317,124.433105551511)) ;
#53261 = CARTESIAN_POINT('Ctrl Pts',(-20.2108513393927,-27.3821728022512,
124.688432935448)) ;
#53262 = CARTESIAN_POINT('Ctrl Pts',(-20.2180592426687,-27.5721514372341,
124.306460221141)) ;
#53263 = CARTESIAN_POINT('Ctrl Pts',(-20.4202523050526,-27.3921623567536,
124.530127299279)) ;
#53264 = CARTESIAN_POINT('Ctrl Pts',(-20.3604835812191,-27.5821098517577,
124.153021019065)) ;
#53265 = CARTESIAN_POINT('Ctrl Pts',(-20.5982841262608,-27.4021207712772,
124.338329003616)) ;
#53266 = CARTESIAN_POINT('Ctrl Pts',(-20.473871725562,-27.5920097645871,123.978479224777)) ;
#53267 = CARTESIAN_POINT('Ctrl Pts',(-20.7400208954016,-27.4120206841066,
124.120151747233)) ;
#53268 = CARTESIAN_POINT('Ctrl Pts',(-20.5563690525815,-27.602056464237,123.784065248068)) ;
#53269 = CARTESIAN_POINT('Ctrl Pts',(-20.8431437132464,-27.4220673837565,
123.877134998745)) ;
#53270 = CARTESIAN_POINT('Ctrl Pts',(-20.6033030576586,-27.6119563245426,
123.581267591945)) ;
#53271 = CARTESIAN_POINT('Ctrl Pts',(-20.9018126857167,-27.4319672440621,
123.623637353375)) ;
#53272 = CARTESIAN_POINT('Ctrl Pts',(-20.6145464495285,-27.622007728748,123.370284273142)) ;
#53273 = CARTESIAN_POINT('Ctrl Pts',(-20.9158681863817,-27.4420186482676,
123.359908517839)) ;
#53274 = CARTESIAN_POINT('Ctrl Pts',(-20.5894865428159,-27.6318887656692,
123.164040601756)) ;
#53275 = CARTESIAN_POINT('Ctrl Pts',(-20.8845444217385,-27.4518996851887,
123.102102763074)) ;
#53276 = CARTESIAN_POINT('Ctrl Pts',(-20.5285619224102,-27.6418885978467,
122.96287053044)) ;
#53277 = CARTESIAN_POINT('Ctrl Pts',(-20.8083897019526,-27.4618995173662,
122.850639705346)) ;
#53278 = CARTESIAN_POINT('Ctrl Pts',(-20.4345314205031,-27.6518066008316,
122.776728506564)) ;
#53279 = CARTESIAN_POINT('Ctrl Pts',(-20.6908521997633,-27.4718175203511,
122.617961007216)) ;
#53280 = CARTESIAN_POINT('Ctrl Pts',(-20.307917816095,-27.6618579067061,122.607595735028)) ;
#53281 = CARTESIAN_POINT('Ctrl Pts',(-20.5325862277936,-27.4818688262257,
122.406544566008)) ;
#53282 = CARTESIAN_POINT('Ctrl Pts',(-20.1567577654715,-27.6717277300977,
122.465387827078)) ;
#53283 = CARTESIAN_POINT('Ctrl Pts',(-20.3436360269097,-27.4917386496172,
122.228783160542)) ;
#53284 = CARTESIAN_POINT('Ctrl Pts',(-19.979678811247,-27.681801896148,122.349293202809)) ;
#53285 = CARTESIAN_POINT('Ctrl Pts',(-20.1222882554318,-27.5018128156675,
122.083664260518)) ;
#53286 = CARTESIAN_POINT('Ctrl Pts',(-19.7900524651862,-27.6916219802896,
122.267545505754)) ;
#53287 = CARTESIAN_POINT('Ctrl Pts',(-19.8852542609095,-27.5116328998091,
121.981478175887)) ;
#53288 = CARTESIAN_POINT('Ctrl Pts',(-19.5839641602467,-27.7017007070255,
122.218539726718)) ;
#53289 = CARTESIAN_POINT('Ctrl Pts',(-19.6276445349011,-27.521711626545,121.92022023308)) ;
#53290 = CARTESIAN_POINT('Ctrl Pts',(-19.3771678744328,-27.711552287675,122.206266541028)) ;
#53291 = CARTESIAN_POINT('Ctrl Pts',(-19.3691479103132,-27.5315632071945,
121.904877852162)) ;
#53292 = CARTESIAN_POINT('Ctrl Pts',(-19.1668198410956,-27.7216254159734,
122.230427368706)) ;
#53293 = CARTESIAN_POINT('Ctrl Pts',(-19.1062132173185,-27.5416363354929,
121.93507808783)) ;
#53294 = CARTESIAN_POINT('Ctrl Pts',(-18.9684654062851,-27.7314678938648,
122.289410143151)) ;
#53295 = CARTESIAN_POINT('Ctrl Pts',(-18.8582685979339,-27.5514788133843,
122.008806224701)) ;
#53296 = CARTESIAN_POINT('Ctrl Pts',(-18.7804810737789,-27.7414485004629,
122.382594626151)) ;
#53297 = CARTESIAN_POINT('Ctrl Pts',(-18.6232876860456,-27.5614594199824,
122.125286522703)) ;
#53298 = CARTESIAN_POINT('Ctrl Pts',(-18.6111314469125,-27.7514662094817,
122.50779197817)) ;
#53299 = CARTESIAN_POINT('Ctrl Pts',(-18.4116002703336,-27.5714771290012,
122.281782687831)) ;
#53300 = CARTESIAN_POINT('Ctrl Pts',(-18.46769289707,-27.7613523885191,122.65822099697)) ;
#53301 = CARTESIAN_POINT('Ctrl Pts',(-18.2323009869276,-27.5813633080386,
122.469819398419)) ;
#53302 = CARTESIAN_POINT('Ctrl Pts',(-18.3505632690495,-27.7714100010914,
122.834235024386)) ;
#53303 = CARTESIAN_POINT('Ctrl Pts',(-18.0858887220002,-27.591420920611,122.689836403978)) ;
#53304 = CARTESIAN_POINT('Ctrl Pts',(-18.2672711578626,-27.7812863944636,
123.024442583232)) ;
#53305 = CARTESIAN_POINT('Ctrl Pts',(-17.9817726805274,-27.6012973139831,
122.927596725617)) ;
#53306 = CARTESIAN_POINT('Ctrl Pts',(-18.2171766731924,-27.791281422614,123.228504736778)) ;
#53307 = CARTESIAN_POINT('Ctrl Pts',(-17.9191542663906,-27.6112923421335,
123.182674524713)) ;
#53308 = CARTESIAN_POINT('Ctrl Pts',(-18.2035981744951,-27.80130216946,123.438743704045)) ;
#53309 = CARTESIAN_POINT('Ctrl Pts',(-17.9021807328002,-27.6213130889795,
123.445473162296)) ;
#53310 = CARTESIAN_POINT('Ctrl Pts',(-18.2262128560997,-27.8112042381264,
123.645681904527)) ;
#53311 = CARTESIAN_POINT('Ctrl Pts',(-17.9304488695077,-27.6312151576459,
123.704146901877)) ;
#53312 = CARTESIAN_POINT('Ctrl Pts',(-18.284639933744,-27.8211949779461,123.847429809037)) ;
#53313 = CARTESIAN_POINT('Ctrl Pts',(-18.0034825910525,-27.6412058974656,
123.9563320642)) ;
#53314 = CARTESIAN_POINT('Ctrl Pts',(-18.3770881160731,-27.8311581741564,
124.035370273374)) ;
#53315 = CARTESIAN_POINT('Ctrl Pts',(-18.1190427860943,-27.6511690936759,
124.19125816354)) ;
#53316 = CARTESIAN_POINT('Ctrl Pts',(-18.4996327245681,-27.8410623584565,
124.203730145458)) ;
#53317 = CARTESIAN_POINT('Ctrl Pts',(-18.2722240569279,-27.661073277976,124.401708795507)) ;
#53318 = CARTESIAN_POINT('Ctrl Pts',(-18.652006072211,-27.8511228188474,124.350375168077)) ;
#53319 = CARTESIAN_POINT('Ctrl Pts',(-18.4626903999136,-27.6711337383669,
124.585014918637)) ;
#53320 = CARTESIAN_POINT('Ctrl Pts',(-18.8235862046144,-27.8609633647182,
124.466005825925)) ;
#53321 = CARTESIAN_POINT('Ctrl Pts',(-18.6771667744732,-27.6809742842377,
124.729554078446)) ;
#53322 = CARTESIAN_POINT('Ctrl Pts',(-19.0167402747536,-27.8710255854299,
124.552208647531)) ;
#53323 = CARTESIAN_POINT('Ctrl Pts',(-18.9186090602696,-27.6910365049495,
124.837307374996)) ;
#53324 = CARTESIAN_POINT('Ctrl Pts',(-19.2186463887635,-27.8809227284465,
124.602519019844)) ;
#53325 = CARTESIAN_POINT('Ctrl Pts',(-19.1709926750218,-27.700933647966,124.900195583921)) ;
#53326 = CARTESIAN_POINT('Ctrl Pts',(-19.4268700305496,-27.8908539048637,
124.617749388412)) ;
#53327 = CARTESIAN_POINT('Ctrl Pts',(-19.4312729665514,-27.7108648243832,
124.919233320845)) ;
#53328 = CARTESIAN_POINT('Ctrl Pts',(-19.6368755079311,-27.9008961186423,
124.596126506695)) ;
#53329 = CARTESIAN_POINT('Ctrl Pts',(-19.6937795869261,-27.7209070381618,
124.892204557448)) ;
#53330 = CARTESIAN_POINT('Ctrl Pts',(-19.8368447731837,-27.910782658845,124.539408291931)) ;
#53331 = CARTESIAN_POINT('Ctrl Pts',(-19.9437421484284,-27.7307935783645,
124.821306255873)) ;
#53332 = CARTESIAN_POINT('Ctrl Pts',(-20.026076968928,-27.9207762534504,124.448165743483)) ;
#53333 = CARTESIAN_POINT('Ctrl Pts',(-20.1802824077118,-27.74078717297,124.707252644304)) ;
#53334 = CARTESIAN_POINT('Ctrl Pts',(-20.1957478692997,-27.930720128608,124.326020666064)) ;
#53335 = CARTESIAN_POINT('Ctrl Pts',(-20.3923713221862,-27.7507310481275,
124.554570637575)) ;
#53336 = CARTESIAN_POINT('Ctrl Pts',(-20.3420563337105,-27.9406806647228,
124.176229596615)) ;
#53337 = CARTESIAN_POINT('Ctrl Pts',(-20.5752568935258,-27.7606915842423,
124.367331130145)) ;
#53338 = CARTESIAN_POINT('Ctrl Pts',(-20.4606861174511,-27.9506772680455,
124.002726210929)) ;
#53339 = CARTESIAN_POINT('Ctrl Pts',(-20.7235437792058,-27.7706881875651,
124.150451479983)) ;
#53340 = CARTESIAN_POINT('Ctrl Pts',(-20.5474206151358,-27.960710351,123.810462365008)) ;
#53341 = CARTESIAN_POINT('Ctrl Pts',(-20.8319614752254,-27.7807212705196,
123.910121632777)) ;
#53342 = CARTESIAN_POINT('Ctrl Pts',(-20.5987649896307,-27.9705615197016,
123.609829364369)) ;
#53343 = CARTESIAN_POINT('Ctrl Pts',(-20.8961417942239,-27.7905724392211,
123.659328927923)) ;
#53344 = CARTESIAN_POINT('Ctrl Pts',(-20.6152871156439,-27.9805240104005,
123.401046818215)) ;
#53345 = CARTESIAN_POINT('Ctrl Pts',(-20.9167937430027,-27.80053492992,123.398350225032)) ;
#53346 = CARTESIAN_POINT('Ctrl Pts',(-20.5949125271602,-27.9905524388182,
123.191192264674)) ;
#53347 = CARTESIAN_POINT('Ctrl Pts',(-20.8913248729586,-27.8105633583378,
123.136032193831)) ;
#53348 = CARTESIAN_POINT('Ctrl Pts',(-20.53914584983,-28.0004628061828,122.990457378277)) ;
#53349 = CARTESIAN_POINT('Ctrl Pts',(-20.821615644239,-27.8204737257023,122.885112920353)) ;
#53350 = CARTESIAN_POINT('Ctrl Pts',(-20.4496374418431,-28.0103976737979,
122.801740219199)) ;
#53351 = CARTESIAN_POINT('Ctrl Pts',(-20.7097290523873,-27.8304085933174,
122.649216253035)) ;
#53352 = CARTESIAN_POINT('Ctrl Pts',(-20.3272748886815,-28.0204388157769,
122.629733634215)) ;
#53353 = CARTESIAN_POINT('Ctrl Pts',(-20.5567753119051,-27.8404497352964,
122.434208642508)) ;
#53354 = CARTESIAN_POINT('Ctrl Pts',(-20.1793010965195,-28.0303259519801,
122.483741362788)) ;
#53355 = CARTESIAN_POINT('Ctrl Pts',(-20.3718067250228,-27.8503368714996,
122.251718186762)) ;
#53356 = CARTESIAN_POINT('Ctrl Pts',(-20.0066274113567,-28.0403182343835,
122.364130675041)) ;
#53357 = CARTESIAN_POINT('Ctrl Pts',(-20.1559638842904,-27.860329153903,122.102205529622)) ;
#53358 = CARTESIAN_POINT('Ctrl Pts',(-19.8165954509597,-28.0502667623487,
122.276745364225)) ;
#53359 = CARTESIAN_POINT('Ctrl Pts',(-19.9184230348921,-27.8702776818682,
121.992974547454)) ;
#53360 = CARTESIAN_POINT('Ctrl Pts',(-19.6146202820985,-28.0602034935108,
122.223467272798)) ;
#53361 = CARTESIAN_POINT('Ctrl Pts',(-19.6659531803205,-27.8802144130303,
121.926377817634)) ;
#53362 = CARTESIAN_POINT('Ctrl Pts',(-19.4054676734705,-28.0701867043708,
122.205721541684)) ;
#53363 = CARTESIAN_POINT('Ctrl Pts',(-19.4045120642442,-27.8901976238903,
121.904196806999)) ;
#53364 = CARTESIAN_POINT('Ctrl Pts',(-19.1952379005433,-28.0802298035207,
122.225046803646)) ;
#53365 = CARTESIAN_POINT('Ctrl Pts',(-19.1417251311324,-27.9002407230402,
121.928354401077)) ;
#53366 = CARTESIAN_POINT('Ctrl Pts',(-18.9956932343111,-28.0900607677956,
122.278974247708)) ;
#53367 = CARTESIAN_POINT('Ctrl Pts',(-18.8922932247184,-27.9100716873151,
121.995765252323)) ;
#53368 = CARTESIAN_POINT('Ctrl Pts',(-18.8039248705908,-28.1001336201815,
122.368723820022)) ;
#53369 = CARTESIAN_POINT('Ctrl Pts',(-18.6525836804044,-27.920144539701,122.107953193198)) ;
#53370 = CARTESIAN_POINT('Ctrl Pts',(-18.6342195703199,-28.1099977478933,
122.487946903188)) ;
#53371 = CARTESIAN_POINT('Ctrl Pts',(-18.4404518361072,-27.9300086674128,
122.25698372832)) ;
#53372 = CARTESIAN_POINT('Ctrl Pts',(-18.4851003678343,-28.1200199500282,
122.636789063921)) ;
#53373 = CARTESIAN_POINT('Ctrl Pts',(-18.2540538809201,-27.9400308695477,
122.443037416563)) ;
#53374 = CARTESIAN_POINT('Ctrl Pts',(-18.3644270649533,-28.1300471429966,
122.809651509413)) ;
#53375 = CARTESIAN_POINT('Ctrl Pts',(-18.1032133228676,-27.9500580625161,
122.659116134809)) ;
#53376 = CARTESIAN_POINT('Ctrl Pts',(-18.2768385867952,-28.1399027369636,
122.997405819395)) ;
#53377 = CARTESIAN_POINT('Ctrl Pts',(-17.9937284541553,-27.9599136564831,
122.893810711227)) ;
#53378 = CARTESIAN_POINT('Ctrl Pts',(-18.2220200004676,-28.1498599088289,
123.199439317662)) ;
#53379 = CARTESIAN_POINT('Ctrl Pts',(-17.9252066475916,-27.9698708283484,
123.146353412734)) ;
#53380 = CARTESIAN_POINT('Ctrl Pts',(-18.2033226183059,-28.1598987528273,
123.409644983658)) ;
#53381 = CARTESIAN_POINT('Ctrl Pts',(-17.9018363924116,-27.9799096723468,
123.409110487333)) ;
#53382 = CARTESIAN_POINT('Ctrl Pts',(-18.2207487622362,-28.1697727767028,
123.616522805315)) ;
#53383 = CARTESIAN_POINT('Ctrl Pts',(-17.9236207435737,-27.9897836962224,
123.667708642649)) ;
#53384 = CARTESIAN_POINT('Ctrl Pts',(-18.2748756328717,-28.1798426026932,
123.821155710981)) ;
#53385 = CARTESIAN_POINT('Ctrl Pts',(-17.9912807795422,-27.9998535222128,
123.923499029308)) ;
#53386 = CARTESIAN_POINT('Ctrl Pts',(-18.3615430076775,-28.1896758465905,
124.008855877301)) ;
#53387 = CARTESIAN_POINT('Ctrl Pts',(-18.0996170114153,-28.00968676611,124.158124720537)) ;
#53388 = CARTESIAN_POINT('Ctrl Pts',(-18.4813453459947,-28.1997062743635,
124.18238158238)) ;
#53389 = CARTESIAN_POINT('Ctrl Pts',(-18.2493713826694,-28.0197171938831,
124.37503074541)) ;
#53390 = CARTESIAN_POINT('Ctrl Pts',(-18.6299243812976,-28.2097378911087,
124.332069289836)) ;
#53391 = CARTESIAN_POINT('Ctrl Pts',(-18.4350962679651,-28.0297488106282,
124.562139179393)) ;
#53392 = CARTESIAN_POINT('Ctrl Pts',(-18.7984985629321,-28.2195675680894,
124.451573981328)) ;
#53393 = CARTESIAN_POINT('Ctrl Pts',(-18.6458160518969,-28.0395784876089,
124.711519341909)) ;
#53394 = CARTESIAN_POINT('Ctrl Pts',(-18.9880488787878,-28.2295570849293,
124.542006375535)) ;
#53395 = CARTESIAN_POINT('Ctrl Pts',(-18.8827549499808,-28.0495680044489,
124.824558144054)) ;
#53396 = CARTESIAN_POINT('Ctrl Pts',(-19.1916515256229,-28.2396006970691,
124.597937925507)) ;
#53397 = CARTESIAN_POINT('Ctrl Pts',(-19.1372585886768,-28.0596116165886,
124.894470815725)) ;
#53398 = CARTESIAN_POINT('Ctrl Pts',(-19.3972114936263,-28.2494233034044,
124.617664945189)) ;
#53399 = CARTESIAN_POINT('Ctrl Pts',(-19.3942099817859,-28.0694342229239,
124.919127791887)) ;
#53400 = CARTESIAN_POINT('Ctrl Pts',(-19.6076212256826,-28.2594615333036,
124.601522484725)) ;
#53401 = CARTESIAN_POINT('Ctrl Pts',(-19.6572218646358,-28.0794724528232,
124.898947663215)) ;
#53402 = CARTESIAN_POINT('Ctrl Pts',(-19.8113776911949,-28.2694725680956,
124.548753711217)) ;
#53403 = CARTESIAN_POINT('Ctrl Pts',(-19.9119170105172,-28.0894834876151,
124.832984826556)) ;
#53404 = CARTESIAN_POINT('Ctrl Pts',(-20.0008298539462,-28.2793702990627,
124.462706665286)) ;
#53405 = CARTESIAN_POINT('Ctrl Pts',(-20.1487320478173,-28.0993812185822,
124.725423875452)) ;
#53406 = CARTESIAN_POINT('Ctrl Pts',(-20.1742139857442,-28.2893599269132,
124.344205140818)) ;
#53407 = CARTESIAN_POINT('Ctrl Pts',(-20.3654611749712,-28.1093708464327,
124.577295140952)) ;
#53408 = CARTESIAN_POINT('Ctrl Pts',(-20.3238283363393,-28.2993157173592,
124.19784376409)) ;
#53409 = CARTESIAN_POINT('Ctrl Pts',(-20.5524779417521,-28.1193266368787,
124.394341663562)) ;
#53410 = CARTESIAN_POINT('Ctrl Pts',(-20.4457396566452,-28.3092431159212,
124.028437006786)) ;
#53411 = CARTESIAN_POINT('Ctrl Pts',(-20.704865620646,-28.1292540354408,124.182581520384)) ;
#53412 = CARTESIAN_POINT('Ctrl Pts',(-20.5372193180134,-28.3192687110311,
123.838562812821)) ;
#53413 = CARTESIAN_POINT('Ctrl Pts',(-20.8192132353029,-28.1392796305506,
123.945237856662)) ;
#53414 = CARTESIAN_POINT('Ctrl Pts',(-20.5936698159923,-28.3291545617007,
123.638543561245)) ;
#53415 = CARTESIAN_POINT('Ctrl Pts',(-20.8897744389928,-28.1491654812202,
123.695212486605)) ;
#53416 = CARTESIAN_POINT('Ctrl Pts',(-20.6152462524492,-28.3391437415449,
123.429645094941)) ;
#53417 = CARTESIAN_POINT('Ctrl Pts',(-20.9167426864684,-28.1591546610644,
123.434089007645)) ;
#53418 = CARTESIAN_POINT('Ctrl Pts',(-20.5997049484337,-28.3491849286484,
123.219121094953)) ;
#53419 = CARTESIAN_POINT('Ctrl Pts',(-20.8973138531456,-28.169195848168,123.170934263091)) ;
#53420 = CARTESIAN_POINT('Ctrl Pts',(-20.5492532199071,-28.3590175721244,
123.018663279547)) ;
#53421 = CARTESIAN_POINT('Ctrl Pts',(-20.834246726357,-28.1790284916439,122.920361624785)) ;
#53422 = CARTESIAN_POINT('Ctrl Pts',(-20.4639239618416,-28.3690115218339,
122.826668029978)) ;
#53423 = CARTESIAN_POINT('Ctrl Pts',(-20.7275828727774,-28.1890224413534,
122.680368443555)) ;
#53424 = CARTESIAN_POINT('Ctrl Pts',(-20.3457702484628,-28.3790406446104,
122.652037807507)) ;
#53425 = CARTESIAN_POINT('Ctrl Pts',(-20.579888806851,-28.1990515641299,122.46208199399)) ;
#53426 = CARTESIAN_POINT('Ctrl Pts',(-20.2015610995993,-28.3889167755291,
122.502648999928)) ;
#53427 = CARTESIAN_POINT('Ctrl Pts',(-20.3996251642612,-28.2089276950486,
122.275347174398)) ;
#53428 = CARTESIAN_POINT('Ctrl Pts',(-20.0317039479304,-28.3989148105461,
122.37888357769)) ;
#53429 = CARTESIAN_POINT('Ctrl Pts',(-20.1873021800458,-28.2189257300656,
122.120642324578)) ;
#53430 = CARTESIAN_POINT('Ctrl Pts',(-19.8445504166726,-28.4088287403048,
122.287101606991)) ;
#53431 = CARTESIAN_POINT('Ctrl Pts',(-19.9533587456366,-28.2288396598243,
122.00591689841)) ;
#53432 = CARTESIAN_POINT('Ctrl Pts',(-19.6417453548372,-28.4188719280426,
122.228424618647)) ;
#53433 = CARTESIAN_POINT('Ctrl Pts',(-19.6998517914313,-28.2388828475621,
121.932573093112)) ;
#53434 = CARTESIAN_POINT('Ctrl Pts',(-19.4348032819945,-28.428771770183,122.206158950053)) ;
#53435 = CARTESIAN_POINT('Ctrl Pts',(-19.441173435824,-28.2487826897025,121.904743447041)) ;
#53436 = CARTESIAN_POINT('Ctrl Pts',(-19.225199951328,-28.438763036991,122.219845479332)) ;
#53437 = CARTESIAN_POINT('Ctrl Pts',(-19.1791693222261,-28.2587739565105,
121.921854203863)) ;
#53438 = CARTESIAN_POINT('Ctrl Pts',(-19.0204087974407,-28.4487951391229,
122.270276783567)) ;
#53439 = CARTESIAN_POINT('Ctrl Pts',(-18.9231809982585,-28.2688060586425,
121.984895781266)) ;
#53440 = CARTESIAN_POINT('Ctrl Pts',(-18.8305583447142,-28.4586620200777,
122.353843034253)) ;
#53441 = CARTESIAN_POINT('Ctrl Pts',(-18.6858684266711,-28.2786729395972,
122.089356190467)) ;
#53442 = CARTESIAN_POINT('Ctrl Pts',(-18.6556330787561,-28.4686538113658,
122.470151417965)) ;
#53443 = CARTESIAN_POINT('Ctrl Pts',(-18.4672132263357,-28.2886647308854,
122.234743944221)) ;
#53444 = CARTESIAN_POINT('Ctrl Pts',(-18.5032314430184,-28.4786859272774,
122.61594277691)) ;
#53445 = CARTESIAN_POINT('Ctrl Pts',(-18.276712974009,-28.2986968467969,122.416985014453)) ;
#53446 = CARTESIAN_POINT('Ctrl Pts',(-18.380260915545,-28.4885522440774,122.782991829368)) ;
#53447 = CARTESIAN_POINT('Ctrl Pts',(-18.1230016339298,-28.3085631635969,
122.625798314926)) ;
#53448 = CARTESIAN_POINT('Ctrl Pts',(-18.286740408124,-28.498539725551,122.970954331532)) ;
#53449 = CARTESIAN_POINT('Ctrl Pts',(-18.0061033567244,-28.3185506450705,
122.860752752778)) ;
#53450 = CARTESIAN_POINT('Ctrl Pts',(-18.2274077058308,-28.5084846499299,
123.171464369965)) ;
#53451 = CARTESIAN_POINT('Ctrl Pts',(-17.931940003729,-28.3284955694494,123.111391293671)) ;
#53452 = CARTESIAN_POINT('Ctrl Pts',(-18.2036772806348,-28.5185295358406,
123.381282408305)) ;
#53453 = CARTESIAN_POINT('Ctrl Pts',(-17.9022796486701,-28.3385404553601,
123.373664123606)) ;
#53454 = CARTESIAN_POINT('Ctrl Pts',(-18.2163217636226,-28.5283916395532,
123.588243745579)) ;
#53455 = CARTESIAN_POINT('Ctrl Pts',(-17.9180879854139,-28.3484025590727,
123.632366059938)) ;
#53456 = CARTESIAN_POINT('Ctrl Pts',(-18.2649253863527,-28.5383832033776,
123.792581695052)) ;
#53457 = CARTESIAN_POINT('Ctrl Pts',(-17.9788452221271,-28.3583941228972,
123.887787950783)) ;
#53458 = CARTESIAN_POINT('Ctrl Pts',(-18.3478659471332,-28.5483160114405,
123.984221813374)) ;
#53459 = CARTESIAN_POINT('Ctrl Pts',(-18.0825235358457,-28.3683269309601,
124.127337211431)) ;
#53460 = CARTESIAN_POINT('Ctrl Pts',(-18.4624497179601,-28.5582531136769,
124.158918671784)) ;
#53461 = CARTESIAN_POINT('Ctrl Pts',(-18.2257556809892,-28.3782640331964,
124.345706898359)) ;
#53462 = CARTESIAN_POINT('Ctrl Pts',(-18.6074717807451,-28.5683055599473,
124.312619227432)) ;
#53463 = CARTESIAN_POINT('Ctrl Pts',(-18.4070352869244,-28.3883164794668,
124.537830699445)) ;
#53464 = CARTESIAN_POINT('Ctrl Pts',(-18.7733489453358,-28.5781516755289,
124.436472624767)) ;
#53465 = CARTESIAN_POINT('Ctrl Pts',(-18.6143836430854,-28.3981625950484,
124.692645379623)) ;
#53466 = CARTESIAN_POINT('Ctrl Pts',(-18.9618249797804,-28.5881996952438,
124.531831590146)) ;
#53467 = CARTESIAN_POINT('Ctrl Pts',(-18.8499799672981,-28.4082106147633,
124.811841582675)) ;
#53468 = CARTESIAN_POINT('Ctrl Pts',(-19.1619711895627,-28.5981416468727,
124.592099396301)) ;
#53469 = CARTESIAN_POINT('Ctrl Pts',(-19.1001636768918,-28.4181525663922,
124.887173703538)) ;
#53470 = CARTESIAN_POINT('Ctrl Pts',(-19.36940458292,-28.6080804278718,124.617204452178)) ;
#53471 = CARTESIAN_POINT('Ctrl Pts',(-19.3594558684191,-28.4280913473913,
124.918552242727)) ;
#53472 = CARTESIAN_POINT('Ctrl Pts',(-19.5798534901081,-28.6181064765979,
124.605652962537)) ;
#53473 = CARTESIAN_POINT('Ctrl Pts',(-19.6225169288704,-28.4381173961174,
124.904110048559)) ;
#53474 = CARTESIAN_POINT('Ctrl Pts',(-19.7823487906233,-28.6279933370061,
124.558649540917)) ;
#53475 = CARTESIAN_POINT('Ctrl Pts',(-19.8756354818893,-28.4480042565256,
124.845353062541)) ;
#53476 = CARTESIAN_POINT('Ctrl Pts',(-19.9763812601013,-28.6380246121379,
124.476122124052)) ;
#53477 = CARTESIAN_POINT('Ctrl Pts',(-20.1181752201208,-28.4580355316574,
124.742190925263)) ;
#53478 = CARTESIAN_POINT('Ctrl Pts',(-20.1507052106711,-28.6479075894383,
124.362992233123)) ;
#53479 = CARTESIAN_POINT('Ctrl Pts',(-20.3360779498188,-28.4679185089578,
124.600777052441)) ;
#53480 = CARTESIAN_POINT('Ctrl Pts',(-20.3053443200726,-28.6579644428455,
124.218890410107)) ;
#53481 = CARTESIAN_POINT('Ctrl Pts',(-20.5293776950201,-28.477975362365,124.420644315049)) ;
#53482 = CARTESIAN_POINT('Ctrl Pts',(-20.4724604666755,-28.6711326839214,
123.998058155589)) ;
#53483 = CARTESIAN_POINT('Ctrl Pts',(-20.738256336222,-28.4911436034409,124.144618304064)) ;
#53484 = CARTESIAN_POINT('Ctrl Pts',(-20.5799131365806,-28.6845337131479,
123.73425819107)) ;
#53485 = CARTESIAN_POINT('Ctrl Pts',(-20.8725696185319,-28.5045446326674,
123.814898573048)) ;
#53486 = CARTESIAN_POINT('Ctrl Pts',(-20.6142236375671,-28.6977466298788,
123.458567013862)) ;
#53487 = CARTESIAN_POINT('Ctrl Pts',(-20.9154664866282,-28.5177575493983,
123.470229804434)) ;
#53488 = CARTESIAN_POINT('Ctrl Pts',(-20.604352967794,-28.707675024332,123.250109379369)) ;
#53489 = CARTESIAN_POINT('Ctrl Pts',(-20.9031228606174,-28.5276859438515,
123.209668872552)) ;
#53490 = CARTESIAN_POINT('Ctrl Pts',(-20.5583282587321,-28.7176565244601,
123.045346923892)) ;
#53491 = CARTESIAN_POINT('Ctrl Pts',(-20.8455899285438,-28.5376674439796,
122.953713451743)) ;
#53492 = CARTESIAN_POINT('Ctrl Pts',(-20.4767166915395,-28.7276970677302,
122.850689815527)) ;
#53493 = CARTESIAN_POINT('Ctrl Pts',(-20.7435726951601,-28.5477079872497,
122.710393832247)) ;
#53494 = CARTESIAN_POINT('Ctrl Pts',(-20.3649428036905,-28.7375463995133,
122.676381992891)) ;
#53495 = CARTESIAN_POINT('Ctrl Pts',(-20.6038530331542,-28.5575573190328,
122.492510433852)) ;
#53496 = CARTESIAN_POINT('Ctrl Pts',(-20.2229203006753,-28.747541803985,122.521509294334)) ;
#53497 = CARTESIAN_POINT('Ctrl Pts',(-20.4263234255606,-28.5675527235045,
122.298921849141)) ;
#53498 = CARTESIAN_POINT('Ctrl Pts',(-20.0555849748291,-28.7575581314336,
122.393679057562)) ;
#53499 = CARTESIAN_POINT('Ctrl Pts',(-20.2171504398344,-28.5775690509531,
122.139134607409)) ;
#53500 = CARTESIAN_POINT('Ctrl Pts',(-19.8088912325934,-28.7707817886001,
122.265428926498)) ;
#53501 = CARTESIAN_POINT('Ctrl Pts',(-19.9087920778577,-28.5907927081196,
121.978832990084)) ;
#53502 = CARTESIAN_POINT('Ctrl Pts',(-19.5330216381452,-28.7840760799895,
122.203967929054)) ;
#53503 = CARTESIAN_POINT('Ctrl Pts',(-19.5639959876234,-28.604086999509,121.902007063373)) ;
#53504 = CARTESIAN_POINT('Ctrl Pts',(-19.2539859157199,-28.797360430921,122.215868648645)) ;
#53505 = CARTESIAN_POINT('Ctrl Pts',(-19.2151418343441,-28.6173713504405,
121.916882629458)) ;
#53506 = CARTESIAN_POINT('Ctrl Pts',(-19.0492445151565,-28.8073328119828,
122.260874137876)) ;
#53507 = CARTESIAN_POINT('Ctrl Pts',(-18.9592277476723,-28.6273437315023,
121.973142750564)) ;
#53508 = CARTESIAN_POINT('Ctrl Pts',(-18.8564919194603,-28.8172411916084,
122.339917001314)) ;
#53509 = CARTESIAN_POINT('Ctrl Pts',(-18.7182849242685,-28.6372521111279,
122.071948770138)) ;
#53510 = CARTESIAN_POINT('Ctrl Pts',(-18.6778931742279,-28.8272951903564,
122.452918665696)) ;
#53511 = CARTESIAN_POINT('Ctrl Pts',(-18.4950390576537,-28.647306109876,122.213201779879)) ;
#53512 = CARTESIAN_POINT('Ctrl Pts',(-18.524471696003,-28.8371573874727,122.592405825859)) ;
#53513 = CARTESIAN_POINT('Ctrl Pts',(-18.3032620687074,-28.6571683069923,
122.387567726256)) ;
#53514 = CARTESIAN_POINT('Ctrl Pts',(-18.3524307607685,-28.8505045138469,
122.814082154856)) ;
#53515 = CARTESIAN_POINT('Ctrl Pts',(-18.0882237965495,-28.6705154333664,
122.664637872048)) ;
#53516 = CARTESIAN_POINT('Ctrl Pts',(-18.2159876348167,-28.8670414794883,
123.138150036716)) ;
#53517 = CARTESIAN_POINT('Ctrl Pts',(-17.9176634710199,-28.6870523990078,
123.069772556829)) ;
#53518 = CARTESIAN_POINT('Ctrl Pts',(-18.1976653162901,-28.8836760836622,
123.491362438096)) ;
#53519 = CARTESIAN_POINT('Ctrl Pts',(-17.8947632867105,-28.7036870031818,
123.511208297094)) ;
#53520 = CARTESIAN_POINT('Ctrl Pts',(-18.2560525173173,-28.8969658769049,
123.764590199396)) ;
#53521 = CARTESIAN_POINT('Ctrl Pts',(-17.9677541224921,-28.7169767964244,
123.852806493827)) ;
#53522 = CARTESIAN_POINT('Ctrl Pts',(-18.3343741631932,-28.9069185081643,
123.958600107731)) ;
#53523 = CARTESIAN_POINT('Ctrl Pts',(-18.0656567607898,-28.7269294276838,
124.095304375522)) ;
#53524 = CARTESIAN_POINT('Ctrl Pts',(-18.4449965967694,-28.916870475469,124.136207394979)) ;
#53525 = CARTESIAN_POINT('Ctrl Pts',(-18.2039394801543,-28.7368813949885,
124.317317362376)) ;
#53526 = CARTESIAN_POINT('Ctrl Pts',(-18.6328431511708,-28.9302377339328,
124.345197379133)) ;
#53527 = CARTESIAN_POINT('Ctrl Pts',(-18.4387363199644,-28.7502486534523,
124.578542730308)) ;
#53528 = CARTESIAN_POINT('Ctrl Pts',(-18.9269841780433,-28.9467545458819,
124.537227554656)) ;
#53529 = CARTESIAN_POINT('Ctrl Pts',(-18.8064292375309,-28.7667654654015,
124.818587726068)) ;
#53530 = CARTESIAN_POINT('Ctrl Pts',(-19.3414615997305,-28.9667804408883,
124.634301072555)) ;
#53531 = CARTESIAN_POINT('Ctrl Pts',(-19.3245222155823,-28.7867913604078,
124.939922033255)) ;
#53532 = CARTESIAN_POINT('Ctrl Pts',(-19.759850235118,-28.9865911710184,124.584749330712)) ;
#53533 = CARTESIAN_POINT('Ctrl Pts',(-19.8475073461012,-28.806602090538,124.877979440318)) ;
#53534 = CARTESIAN_POINT('Ctrl Pts',(-20.1396804889429,-29.0065683871483,
124.394678367115)) ;
#53535 = CARTESIAN_POINT('Ctrl Pts',(-20.322293027408,-28.8265793066678,124.640387404806)) ;
#53536 = CARTESIAN_POINT('Ctrl Pts',(-20.4305598017003,-29.0264952625436,
124.086638339135)) ;
#53537 = CARTESIAN_POINT('Ctrl Pts',(-20.6858890815036,-28.8465061820631,
124.255335344435)) ;
#53538 = CARTESIAN_POINT('Ctrl Pts',(-20.5992504484349,-29.0463167240198,
123.700349376274)) ;
#53539 = CARTESIAN_POINT('Ctrl Pts',(-20.8967489378324,-28.8663276435394,
123.772474684078)) ;
#53540 = CARTESIAN_POINT('Ctrl Pts',(-20.626046085885,-29.0663910418292,123.274422117827)) ;
#53541 = CARTESIAN_POINT('Ctrl Pts',(-20.9302406515358,-28.8864019613487,
123.24006458239)) ;
#53542 = CARTESIAN_POINT('Ctrl Pts',(-20.506795066352,-29.0862390108371,122.869477985307)) ;
#53543 = CARTESIAN_POINT('Ctrl Pts',(-20.7811745277581,-28.9062499303566,
122.73388681703)) ;
#53544 = CARTESIAN_POINT('Ctrl Pts',(-20.2560944539261,-29.1061860449003,
122.527490551716)) ;
#53545 = CARTESIAN_POINT('Ctrl Pts',(-20.467797326148,-28.9261969644198,122.306404432427)) ;
#53546 = CARTESIAN_POINT('Ctrl Pts',(-19.9044790885967,-29.1260819958724,
122.292205363375)) ;
#53547 = CARTESIAN_POINT('Ctrl Pts',(-20.028278033369,-28.946092915392,122.012300463349)) ;
#53548 = CARTESIAN_POINT('Ctrl Pts',(-19.493912747964,-29.1459774754907,122.190368785616)) ;
#53549 = CARTESIAN_POINT('Ctrl Pts',(-19.5150711784691,-28.9659883950102,
121.885006524989)) ;
#53550 = CARTESIAN_POINT('Ctrl Pts',(-19.0718902420119,-29.1659335864555,
122.234795537404)) ;
#53551 = CARTESIAN_POINT('Ctrl Pts',(-18.9875437561079,-28.985944505975,121.940541079164)) ;
#53552 = CARTESIAN_POINT('Ctrl Pts',(-18.6914823643913,-29.1858381344955,
122.420160422829)) ;
#53553 = CARTESIAN_POINT('Ctrl Pts',(-18.5120357099676,-29.005849054015,122.172247469313)) ;
#53554 = CARTESIAN_POINT('Ctrl Pts',(-18.3967545767849,-29.2057122588146,
122.723103992137)) ;
#53555 = CARTESIAN_POINT('Ctrl Pts',(-18.1436273508337,-29.0257231783341,
122.550925494711)) ;
#53556 = CARTESIAN_POINT('Ctrl Pts',(-18.2221384336728,-29.2257667888136,
123.11205184558)) ;
#53557 = CARTESIAN_POINT('Ctrl Pts',(-17.9253569899085,-29.0457777083331,
123.037111210443)) ;
#53558 = CARTESIAN_POINT('Ctrl Pts',(-18.190981362348,-29.2455743025736,123.532149795036)) ;
#53559 = CARTESIAN_POINT('Ctrl Pts',(-17.8864107134353,-29.0655852220931,
123.562230606224)) ;
#53560 = CARTESIAN_POINT('Ctrl Pts',(-18.3051612613185,-29.2655576583413,
123.941359506721)) ;
#53561 = CARTESIAN_POINT('Ctrl Pts',(-18.0291344863836,-29.0855685778608,
124.073742812839)) ;
#53562 = CARTESIAN_POINT('Ctrl Pts',(-18.5518768276411,-29.2854759609252,
124.285589142629)) ;
#53563 = CARTESIAN_POINT('Ctrl Pts',(-18.337527532579,-29.1054868804448,124.504029337641)) ;
#53564 = CARTESIAN_POINT('Ctrl Pts',(-18.8998033234493,-29.305344176371,124.525350894694)) ;
#53565 = CARTESIAN_POINT('Ctrl Pts',(-18.7724331767163,-29.1253550958905,
124.803732067833)) ;
#53566 = CARTESIAN_POINT('Ctrl Pts',(-19.3123749934706,-29.3253944931673,
124.632263603809)) ;
#53567 = CARTESIAN_POINT('Ctrl Pts',(-19.2881479518997,-29.1454054126868,
124.937374691363)) ;
#53568 = CARTESIAN_POINT('Ctrl Pts',(-19.7312061051285,-29.3451705550497,
124.593056434788)) ;
#53569 = CARTESIAN_POINT('Ctrl Pts',(-19.8116842877083,-29.1651814745693,
124.888368150248)) ;
#53570 = CARTESIAN_POINT('Ctrl Pts',(-20.1166949902579,-29.3652251607422,
124.411179447447)) ;
#53571 = CARTESIAN_POINT('Ctrl Pts',(-20.2935470560524,-29.1852360802617,
124.661024000832)) ;
#53572 = CARTESIAN_POINT('Ctrl Pts',(-20.413193850282,-29.3850188498981,124.112306030586)) ;
#53573 = CARTESIAN_POINT('Ctrl Pts',(-20.6641709205852,-29.2050297694176,
124.28743570741)) ;
#53574 = CARTESIAN_POINT('Ctrl Pts',(-20.5924104104792,-29.4049855414925,
123.727541429383)) ;
#53575 = CARTESIAN_POINT('Ctrl Pts',(-20.888194638405,-29.224996461012,123.806481690376)) ;
#53576 = CARTESIAN_POINT('Ctrl Pts',(-20.6289121024175,-29.4249455872434,
123.304630992729)) ;
#53577 = CARTESIAN_POINT('Ctrl Pts',(-20.9338249695065,-29.244956506763,123.277844260725)) ;
#53578 = CARTESIAN_POINT('Ctrl Pts',(-20.5195428798539,-29.4448438473937,
122.895946670909)) ;
#53579 = CARTESIAN_POINT('Ctrl Pts',(-20.7971171358388,-29.2648547669132,
122.766988876723)) ;
#53580 = CARTESIAN_POINT('Ctrl Pts',(-20.2777340208433,-29.4647387629429,
122.548875500711)) ;
#53581 = CARTESIAN_POINT('Ctrl Pts',(-20.4948597931304,-29.2847496824624,
122.333148374869)) ;
#53582 = CARTESIAN_POINT('Ctrl Pts',(-19.9319526108886,-29.4846489433565,
122.30463596634)) ;
#53583 = CARTESIAN_POINT('Ctrl Pts',(-20.0626359965801,-29.304659862876,122.027845909541)) ;
#53584 = CARTESIAN_POINT('Ctrl Pts',(-19.5230900240382,-29.5045847424707,
122.192721165908)) ;
#53585 = CARTESIAN_POINT('Ctrl Pts',(-19.5515593327358,-29.3245956619903,
121.887948224183)) ;
#53586 = CARTESIAN_POINT('Ctrl Pts',(-19.1005503152697,-29.5245226041249,
122.227022561574)) ;
#53587 = CARTESIAN_POINT('Ctrl Pts',(-19.023384693824,-29.3445335236444,121.930820616893)) ;
#53588 = CARTESIAN_POINT('Ctrl Pts',(-18.7153085805982,-29.5444416507625,
122.403062773862)) ;
#53589 = CARTESIAN_POINT('Ctrl Pts',(-18.5418309888662,-29.3644525702821,
122.150865733139)) ;
#53590 = CARTESIAN_POINT('Ctrl Pts',(-18.4127914875677,-29.5643905488167,
122.700380117268)) ;
#53591 = CARTESIAN_POINT('Ctrl Pts',(-18.1636813292534,-29.3844014683362,
122.52251140325)) ;
#53592 = CARTESIAN_POINT('Ctrl Pts',(-18.2301756318706,-29.5842963762597,
123.082237752554)) ;
#53593 = CARTESIAN_POINT('Ctrl Pts',(-17.9354075382581,-29.4043072957793,
122.99982127121)) ;
#53594 = CARTESIAN_POINT('Ctrl Pts',(-18.1953684956847,-29.600879071625,123.433028159498)) ;
#53595 = CARTESIAN_POINT('Ctrl Pts',(-17.8918934977912,-29.4208899911446,
123.438338526595)) ;
#53596 = CARTESIAN_POINT('Ctrl Pts',(-18.24027601235,-29.6141532853487,123.708522208439)) ;
#53597 = CARTESIAN_POINT('Ctrl Pts',(-17.9480247350242,-29.4341642048682,
123.78267941021)) ;
#53598 = CARTESIAN_POINT('Ctrl Pts',(-18.3100397706379,-29.624200004548,123.907851703837)) ;
#53599 = CARTESIAN_POINT('Ctrl Pts',(-18.0352295819817,-29.4442109240675,
124.031850013709)) ;
#53600 = CARTESIAN_POINT('Ctrl Pts',(-18.4110966673818,-29.6340440391937,
124.088481382499)) ;
#53601 = CARTESIAN_POINT('Ctrl Pts',(-18.1615379685972,-29.4540549587132,
124.257627504453)) ;
#53602 = CARTESIAN_POINT('Ctrl Pts',(-18.5878370635189,-29.6473784240982,
124.305998065082)) ;
#53603 = CARTESIAN_POINT('Ctrl Pts',(-18.3825117399585,-29.4673893436177,
124.529570908678)) ;
#53604 = CARTESIAN_POINT('Ctrl Pts',(-18.8736671997377,-29.663965641398,124.512799362027)) ;
#53605 = CARTESIAN_POINT('Ctrl Pts',(-18.7397290348442,-29.4839765609175,
124.788022651668)) ;
#53606 = CARTESIAN_POINT('Ctrl Pts',(-19.2135861785788,-29.6805988534359,
124.610126724355)) ;
#53607 = CARTESIAN_POINT('Ctrl Pts',(-19.1646822605497,-29.5006097729554,
124.909710774765)) ;
#53608 = CARTESIAN_POINT('Ctrl Pts',(-19.4928463617671,-29.6938812957081,
124.61484124617)) ;
#53609 = CARTESIAN_POINT('Ctrl Pts',(-19.5137203885411,-29.5138922152276,
124.915596996321)) ;
#53610 = CARTESIAN_POINT('Ctrl Pts',(-19.6985621110543,-29.7037871836223,
124.582563757789)) ;
#53611 = CARTESIAN_POINT('Ctrl Pts',(-19.7708729287918,-29.5237981031418,
124.875254844547)) ;
#53612 = CARTESIAN_POINT('Ctrl Pts',(-19.8973061665422,-29.7137756017274,
124.514736011145)) ;
#53613 = CARTESIAN_POINT('Ctrl Pts',(-20.0193014855349,-29.5337865212469,
124.790472867402)) ;
#53614 = CARTESIAN_POINT('Ctrl Pts',(-20.0817838352029,-29.7237990289661,
124.412880710944)) ;
#53615 = CARTESIAN_POINT('Ctrl Pts',(-20.2499022752962,-29.5438099484857,
124.663153811416)) ;
#53616 = CARTESIAN_POINT('Ctrl Pts',(-20.2438922250525,-29.7337034600831,
124.282207760991)) ;
#53617 = CARTESIAN_POINT('Ctrl Pts',(-20.4525327561427,-29.5537143796027,
124.499823981735)) ;
#53618 = CARTESIAN_POINT('Ctrl Pts',(-20.4278473297483,-29.7469666126936,
124.072677307792)) ;
#53619 = CARTESIAN_POINT('Ctrl Pts',(-20.682512025619,-29.5669775322131,124.237867726939)) ;
#53620 = CARTESIAN_POINT('Ctrl Pts',(-20.5532267657517,-29.7602915105975,
123.81863575924)) ;
#53621 = CARTESIAN_POINT('Ctrl Pts',(-20.8392151518599,-29.580302430117,123.920338199566)) ;
#53622 = CARTESIAN_POINT('Ctrl Pts',(-20.607805933461,-29.7735472542131,123.545295424663)) ;
#53623 = CARTESIAN_POINT('Ctrl Pts',(-20.9074394906536,-29.5935581737326,
123.578684401669)) ;
#53624 = CARTESIAN_POINT('Ctrl Pts',(-20.6128379852353,-29.7835066276604,
123.336009205538)) ;
#53625 = CARTESIAN_POINT('Ctrl Pts',(-20.9137330390343,-29.6035175471799,
123.317072430931)) ;
#53626 = CARTESIAN_POINT('Ctrl Pts',(-20.5817572009049,-29.7934504515873,
123.129255120168)) ;
#53627 = CARTESIAN_POINT('Ctrl Pts',(-20.8748846543688,-29.6134613711069,
123.058630457407)) ;
#53628 = CARTESIAN_POINT('Ctrl Pts',(-20.5143943920179,-29.8034983957346,
122.929061237664)) ;
#53629 = CARTESIAN_POINT('Ctrl Pts',(-20.7906838439836,-29.6235093152542,
122.808386846906)) ;
#53630 = CARTESIAN_POINT('Ctrl Pts',(-20.4154235821622,-29.8133493669528,
122.747128077914)) ;
#53631 = CARTESIAN_POINT('Ctrl Pts',(-20.6669727396954,-29.6333602864723,
122.580969032537)) ;
#53632 = CARTESIAN_POINT('Ctrl Pts',(-20.2852290763675,-29.8233211843949,
122.582848316609)) ;
#53633 = CARTESIAN_POINT('Ctrl Pts',(-20.504231739186,-29.6433321039144,122.375617475075)) ;
#53634 = CARTESIAN_POINT('Ctrl Pts',(-20.128053971246,-29.833316606687,122.443331037292)) ;
#53635 = CARTESIAN_POINT('Ctrl Pts',(-20.3077646579128,-29.6533275262065,
122.201218734591)) ;
#53636 = CARTESIAN_POINT('Ctrl Pts',(-19.9482825221474,-29.8433496718107,
122.333015974272)) ;
#53637 = CARTESIAN_POINT('Ctrl Pts',(-20.0830517817784,-29.6633605913302,
122.063322482912)) ;
#53638 = CARTESIAN_POINT('Ctrl Pts',(-19.7554396738521,-29.8532150044759,
122.25669701737)) ;
#53639 = CARTESIAN_POINT('Ctrl Pts',(-19.8419990548365,-29.6732259239954,
121.967921099517)) ;
#53640 = CARTESIAN_POINT('Ctrl Pts',(-19.5504291193949,-29.8631755470735,
122.214013364722)) ;
#53641 = CARTESIAN_POINT('Ctrl Pts',(-19.5857362753766,-29.683186466593,121.914563791376)) ;
#53642 = CARTESIAN_POINT('Ctrl Pts',(-19.3395885460387,-29.8732092325752,
122.207884141582)) ;
#53643 = CARTESIAN_POINT('Ctrl Pts',(-19.3221856204141,-29.6932201520947,
121.90689947155)) ;
#53644 = CARTESIAN_POINT('Ctrl Pts',(-19.1338922316553,-29.8830940645654,
122.237651972592)) ;
#53645 = CARTESIAN_POINT('Ctrl Pts',(-19.0650645565471,-29.703104984085,121.944106565147)) ;
#53646 = CARTESIAN_POINT('Ctrl Pts',(-18.93291875455,-29.8931614913253,122.303910124113)) ;
#53647 = CARTESIAN_POINT('Ctrl Pts',(-18.8138468784148,-29.7131724108448,
122.026926609258)) ;
#53648 = CARTESIAN_POINT('Ctrl Pts',(-18.7505843551157,-29.9029999804841,
122.40163291113)) ;
#53649 = CARTESIAN_POINT('Ctrl Pts',(-18.5859272207128,-29.7230109000037,
122.149077864622)) ;
#53650 = CARTESIAN_POINT('Ctrl Pts',(-18.5841468216196,-29.9130634616742,
122.532193860216)) ;
#53651 = CARTESIAN_POINT('Ctrl Pts',(-18.3778786569488,-29.7330743811938,
122.312276880498)) ;
#53652 = CARTESIAN_POINT('Ctrl Pts',(-18.445382712112,-29.9229576194894,122.687180679488)) ;
#53653 = CARTESIAN_POINT('Ctrl Pts',(-18.2044212591461,-29.7429685390089,
122.506008819954)) ;
#53654 = CARTESIAN_POINT('Ctrl Pts',(-18.3346512088788,-29.9328994762337,
122.864415832755)) ;
#53655 = CARTESIAN_POINT('Ctrl Pts',(-18.0660044706819,-29.7529103957532,
122.727551566379)) ;
#53656 = CARTESIAN_POINT('Ctrl Pts',(-18.2558045501675,-29.9429019539051,
123.059389134583)) ;
#53657 = CARTESIAN_POINT('Ctrl Pts',(-17.9674436494209,-29.7629128734246,
122.971267274044)) ;
#53658 = CARTESIAN_POINT('Ctrl Pts',(-18.2122015809126,-29.9529367582094,
123.265783338575)) ;
#53659 = CARTESIAN_POINT('Ctrl Pts',(-17.9129372900069,-29.7729476777289,
123.22925945364)) ;
#53660 = CARTESIAN_POINT('Ctrl Pts',(-18.204883750954,-29.962781635055,123.472638058067)) ;
#53661 = CARTESIAN_POINT('Ctrl Pts',(-17.9037873255447,-29.7827925545746,
123.487828320686)) ;
#53662 = CARTESIAN_POINT('Ctrl Pts',(-18.2336070809338,-29.9727675146106,
123.680563989553)) ;
#53663 = CARTESIAN_POINT('Ctrl Pts',(-17.9396889312473,-29.7927784341301,
123.747736250566)) ;
#53664 = CARTESIAN_POINT('Ctrl Pts',(-18.2975455094374,-29.9827022449691,
123.879438238451)) ;
#53665 = CARTESIAN_POINT('Ctrl Pts',(-18.019609620223,-29.8027131644886,123.99633015856)) ;
#53666 = CARTESIAN_POINT('Ctrl Pts',(-18.3963927749203,-29.992760057282,124.066318685816)) ;
#53667 = CARTESIAN_POINT('Ctrl Pts',(-18.1431663385628,-29.8127709768015,
124.229931834542)) ;
#53668 = CARTESIAN_POINT('Ctrl Pts',(-18.5228873624992,-30.0025806494063,
124.229532798022)) ;
#53669 = CARTESIAN_POINT('Ctrl Pts',(-18.3012830486464,-29.8225915689259,
124.433951657035)) ;
#53670 = CARTESIAN_POINT('Ctrl Pts',(-18.6793976240298,-30.0126472350161,
124.371920994788)) ;
#53671 = CARTESIAN_POINT('Ctrl Pts',(-18.4969190822941,-29.8326581545357,
124.611938648336)) ;
#53672 = CARTESIAN_POINT('Ctrl Pts',(-18.8553834505121,-30.0225468155979,
124.483111642296)) ;
#53673 = CARTESIAN_POINT('Ctrl Pts',(-18.7169004532694,-29.8425577351175,
124.75092934053)) ;
#53674 = CARTESIAN_POINT('Ctrl Pts',(-19.0508479412311,-30.0325984152762,
124.563308795256)) ;
#53675 = CARTESIAN_POINT('Ctrl Pts',(-18.9612300161591,-29.8526093347957,
124.851178041724)) ;
#53676 = CARTESIAN_POINT('Ctrl Pts',(-19.2536676439756,-30.0424726016932,
124.607724013289)) ;
#53677 = CARTESIAN_POINT('Ctrl Pts',(-19.2147547487628,-29.8624835212127,
124.906699600906)) ;
#53678 = CARTESIAN_POINT('Ctrl Pts',(-19.4648637458808,-30.0525290775741,
124.616538418553)) ;
#53679 = CARTESIAN_POINT('Ctrl Pts',(-19.4787496446914,-29.8725399970936,
124.91772003209)) ;
#53680 = CARTESIAN_POINT('Ctrl Pts',(-19.6710664677573,-30.0624220088767,
124.589069886953)) ;
#53681 = CARTESIAN_POINT('Ctrl Pts',(-19.7365039466891,-29.8824329283962,
124.883386678024)) ;
#53682 = CARTESIAN_POINT('Ctrl Pts',(-19.8727094603673,-30.0724847875893,
124.525198764561)) ;
#53683 = CARTESIAN_POINT('Ctrl Pts',(-19.9885582401686,-29.8924957071088,
124.803550123814)) ;
#53684 = CARTESIAN_POINT('Ctrl Pts',(-20.0561959945725,-30.0823273131705,
124.429495466673)) ;
#53685 = CARTESIAN_POINT('Ctrl Pts',(-20.217918273044,-29.90233823269,124.683922711897)) ;
#53686 = CARTESIAN_POINT('Ctrl Pts',(-20.2230137933602,-30.0923180785953,
124.301917210482)) ;
#53687 = CARTESIAN_POINT('Ctrl Pts',(-20.4264420363515,-29.9123289981149,
124.524451584386)) ;
#53688 = CARTESIAN_POINT('Ctrl Pts',(-20.364251196426,-30.1022461545934,124.148229737283)) ;
#53689 = CARTESIAN_POINT('Ctrl Pts',(-20.6029907906799,-29.9222570741129,
124.332343420945)) ;
#53690 = CARTESIAN_POINT('Ctrl Pts',(-20.4776444590878,-30.1122340649804,
123.971491927839)) ;
#53691 = CARTESIAN_POINT('Ctrl Pts',(-20.7447343010342,-29.9322449844999,
124.111422181951)) ;
#53692 = CARTESIAN_POINT('Ctrl Pts',(-20.5586797306925,-30.1222699771053,
123.776696813867)) ;
#53693 = CARTESIAN_POINT('Ctrl Pts',(-20.8460304547474,-29.9422808966249,
123.867929241438)) ;
#53694 = CARTESIAN_POINT('Ctrl Pts',(-20.6041716223551,-30.132124989953,123.57455346389)) ;
#53695 = CARTESIAN_POINT('Ctrl Pts',(-20.902897647784,-29.9521359094725,123.615249639807)) ;
#53696 = CARTESIAN_POINT('Ctrl Pts',(-20.6143059846248,-30.1421239358693,
123.364622415793)) ;
#53697 = CARTESIAN_POINT('Ctrl Pts',(-20.9155677103917,-29.9621348553888,
123.352835793809)) ;
#53698 = CARTESIAN_POINT('Ctrl Pts',(-20.5882986886202,-30.1520208483173,
123.158157718472)) ;
#53699 = CARTESIAN_POINT('Ctrl Pts',(-20.8830605296324,-29.9720317678368,
123.094753953374)) ;
#53700 = CARTESIAN_POINT('Ctrl Pts',(-20.5259041849406,-30.1620746464108,
122.956241447257)) ;
#53701 = CARTESIAN_POINT('Ctrl Pts',(-20.8050694041104,-29.9820855659303,
122.842358190255)) ;
#53702 = CARTESIAN_POINT('Ctrl Pts',(-20.4310894011429,-30.1719555672375,
122.771388410386)) ;
#53703 = CARTESIAN_POINT('Ctrl Pts',(-20.6865523393541,-29.991966486757,122.611290225727)) ;
#53704 = CARTESIAN_POINT('Ctrl Pts',(-20.3043799559765,-30.1819600932352,
122.603543945781)) ;
#53705 = CARTESIAN_POINT('Ctrl Pts',(-20.5281670017028,-30.0019710127547,
122.401483413238)) ;
#53706 = CARTESIAN_POINT('Ctrl Pts',(-20.1506815547945,-30.1919440568527,
122.460549966187)) ;
#53707 = CARTESIAN_POINT('Ctrl Pts',(-20.3360451641608,-30.0119549763722,
122.222739387046)) ;
#53708 = CARTESIAN_POINT('Ctrl Pts',(-19.9734411230241,-30.201983697404,122.345973899521)) ;
#53709 = CARTESIAN_POINT('Ctrl Pts',(-20.1144958156502,-30.0219946169235,
122.079517699013)) ;
#53710 = CARTESIAN_POINT('Ctrl Pts',(-19.782871813628,-30.2118277230187,122.26527172513)) ;
#53711 = CARTESIAN_POINT('Ctrl Pts',(-19.8762838855184,-30.0318386425382,
121.978637774514)) ;
#53712 = CARTESIAN_POINT('Ctrl Pts',(-19.5783094050863,-30.221818728836,122.217602614152)) ;
#53713 = CARTESIAN_POINT('Ctrl Pts',(-19.6205810796765,-30.0418296483556,
121.919049659153)) ;
#53714 = CARTESIAN_POINT('Ctrl Pts',(-19.3675704704491,-30.2318565203682,
122.206603916104)) ;
#53715 = CARTESIAN_POINT('Ctrl Pts',(-19.3571576412079,-30.0518674398877,
121.905299415955)) ;
#53716 = CARTESIAN_POINT('Ctrl Pts',(-19.1621069099491,-30.2417009201566,
122.231506538147)) ;
#53717 = CARTESIAN_POINT('Ctrl Pts',(-19.10032681686,-30.0617118396761,121.93642608354)) ;
#53718 = CARTESIAN_POINT('Ctrl Pts',(-18.9611771135097,-30.2516857207133,
122.292157840187)) ;
#53719 = CARTESIAN_POINT('Ctrl Pts',(-18.8491638610565,-30.0716966402329,
122.012238721506)) ;
#53720 = CARTESIAN_POINT('Ctrl Pts',(-18.7745889266096,-30.2616252441245,
122.386291238736)) ;
#53721 = CARTESIAN_POINT('Ctrl Pts',(-18.6159274222133,-30.081636163644,122.129904287597)) ;
#53722 = CARTESIAN_POINT('Ctrl Pts',(-18.6055578608464,-30.2716649632255,
122.512666339246)) ;
#53723 = CARTESIAN_POINT('Ctrl Pts',(-18.4046377385621,-30.091675882745,122.2878717801)) ;
#53724 = CARTESIAN_POINT('Ctrl Pts',(-18.4631237680064,-30.2815531351448,
122.664098676228)) ;
#53725 = CARTESIAN_POINT('Ctrl Pts',(-18.2265933388627,-30.1015640546643,
122.477161788212)) ;
#53726 = CARTESIAN_POINT('Ctrl Pts',(-18.3476602750316,-30.2915426975618,
122.839512639782)) ;
#53727 = CARTESIAN_POINT('Ctrl Pts',(-18.0822626444727,-30.1115536170813,
122.696428624347)) ;
#53728 = CARTESIAN_POINT('Ctrl Pts',(-18.264811021222,-30.3015010697565,123.031774138297)) ;
#53729 = CARTESIAN_POINT('Ctrl Pts',(-17.9786995240026,-30.121511989276,122.936755300646)) ;
#53730 = CARTESIAN_POINT('Ctrl Pts',(-18.2163954880168,-30.3114011439872,
123.234202863219)) ;
#53731 = CARTESIAN_POINT('Ctrl Pts',(-17.9181786120005,-30.1314120635067,
123.189791746327)) ;
#53732 = CARTESIAN_POINT('Ctrl Pts',(-18.2037078203567,-30.3214472403608,
123.445012427325)) ;
#53733 = CARTESIAN_POINT('Ctrl Pts',(-17.9023177044386,-30.1414581598803,
123.45330342739)) ;
#53734 = CARTESIAN_POINT('Ctrl Pts',(-18.2274762171961,-30.3313558243579,
123.651971116123)) ;
#53735 = CARTESIAN_POINT('Ctrl Pts',(-17.9320269695146,-30.1513667438774,
123.712002752109)) ;
#53736 = CARTESIAN_POINT('Ctrl Pts',(-18.2870541787712,-30.3413664029488,
123.853819127414)) ;
#53737 = CARTESIAN_POINT('Ctrl Pts',(-18.0064982863463,-30.1613773224683,
123.964313150679)) ;
#53738 = CARTESIAN_POINT('Ctrl Pts',(-18.3813325232713,-30.3513955610616,
124.042419862782)) ;
#53739 = CARTESIAN_POINT('Ctrl Pts',(-18.1243449646427,-30.1714064805811,
124.200064581448)) ;
#53740 = CARTESIAN_POINT('Ctrl Pts',(-18.5044666604839,-30.3612484428997,
124.20896945013)) ;
#53741 = CARTESIAN_POINT('Ctrl Pts',(-18.2782623862379,-30.1812593624192,
124.408253321778)) ;
#53742 = CARTESIAN_POINT('Ctrl Pts',(-18.6558439163059,-30.3712080040507,
124.353634907533)) ;
#53743 = CARTESIAN_POINT('Ctrl Pts',(-18.4674836003833,-30.1912189235702,
124.589086196553)) ;
#53744 = CARTESIAN_POINT('Ctrl Pts',(-18.8316171646393,-30.3812464386398,
124.470406891884)) ;
#53745 = CARTESIAN_POINT('Ctrl Pts',(-18.6871993887316,-30.2012573581593,
124.735052040907)) ;
#53746 = CARTESIAN_POINT('Ctrl Pts',(-19.0216991726386,-30.3911197108669,
124.553872844899)) ;
#53747 = CARTESIAN_POINT('Ctrl Pts',(-18.9248025260445,-30.2111306303864,
124.83938585053)) ;
#53748 = CARTESIAN_POINT('Ctrl Pts',(-19.2274128061745,-30.4011929528604,
124.603980425918)) ;
#53749 = CARTESIAN_POINT('Ctrl Pts',(-19.1819439102714,-30.22120387238,124.902021224063)) ;
#53750 = CARTESIAN_POINT('Ctrl Pts',(-19.4334667110816,-30.4110132843935,
124.617542684811)) ;
#53751 = CARTESIAN_POINT('Ctrl Pts',(-19.4395127810957,-30.231024203913,124.918975069789)) ;
#53752 = CARTESIAN_POINT('Ctrl Pts',(-19.64406951049,-30.4210919456203,124.594736003978)) ;
#53753 = CARTESIAN_POINT('Ctrl Pts',(-19.7027659038787,-30.2411028651398,
124.890467615941)) ;
#53754 = CARTESIAN_POINT('Ctrl Pts',(-19.8430448442677,-30.4309435409145,
124.537080259069)) ;
#53755 = CARTESIAN_POINT('Ctrl Pts',(-19.9514865661145,-30.250954460434,124.818398357454)) ;
#53756 = CARTESIAN_POINT('Ctrl Pts',(-20.0331712259711,-30.4410166761433,
124.443902678436)) ;
#53757 = CARTESIAN_POINT('Ctrl Pts',(-20.1891444821242,-30.2610275956628,
124.701927251244)) ;
#53758 = CARTESIAN_POINT('Ctrl Pts',(-20.200339647076,-30.4508591116683,124.32192778539)) ;
#53759 = CARTESIAN_POINT('Ctrl Pts',(-20.3981066043222,-30.2708700311879,
124.549458419515)) ;
#53760 = CARTESIAN_POINT('Ctrl Pts',(-20.3462888347876,-30.4608398808017,
124.171191115801)) ;
#53761 = CARTESIAN_POINT('Ctrl Pts',(-20.5805436589418,-30.2808508003213,
124.361037704532)) ;
#53762 = CARTESIAN_POINT('Ctrl Pts',(-20.4639585613339,-30.4708569820456,
123.996541687798)) ;
#53763 = CARTESIAN_POINT('Ctrl Pts',(-20.7276313528828,-30.2908679015651,
124.142726286221)) ;
#53764 = CARTESIAN_POINT('Ctrl Pts',(-20.5487810389583,-30.4807454296474,
123.806730562509)) ;
#53765 = CARTESIAN_POINT('Ctrl Pts',(-20.8336603365764,-30.300756349167,123.905461600879)) ;
#53766 = CARTESIAN_POINT('Ctrl Pts',(-20.6002259549947,-30.4908011438283,
123.601702375123)) ;
#53767 = CARTESIAN_POINT('Ctrl Pts',(-20.8979668751286,-30.3108120633478,
123.649176788009)) ;
#53768 = CARTESIAN_POINT('Ctrl Pts',(-20.615052892875,-30.5006763502421,123.394610916813)) ;
#53769 = CARTESIAN_POINT('Ctrl Pts',(-20.916501105686,-30.3206872697617,123.390311340074)) ;
#53770 = CARTESIAN_POINT('Ctrl Pts',(-20.5939426510148,-30.5106714027149,
123.185552599972)) ;
#53771 = CARTESIAN_POINT('Ctrl Pts',(-20.8901135579896,-30.3306823222344,
123.128988240025)) ;
#53772 = CARTESIAN_POINT('Ctrl Pts',(-20.536367759922,-30.520693286677,122.982872051517)) ;
#53773 = CARTESIAN_POINT('Ctrl Pts',(-20.8181453545947,-30.3407042061965,
122.87563748438)) ;
#53774 = CARTESIAN_POINT('Ctrl Pts',(-20.4457706611139,-30.5305972592063,
122.795404854875)) ;
#53775 = CARTESIAN_POINT('Ctrl Pts',(-20.7048988529436,-30.3506081787258,
122.641302484479)) ;
#53776 = CARTESIAN_POINT('Ctrl Pts',(-20.3232033140456,-30.5405857558672,
122.624895059131)) ;
#53777 = CARTESIAN_POINT('Ctrl Pts',(-20.5516896931054,-30.3605966753867,
122.428164932553)) ;
#53778 = CARTESIAN_POINT('Ctrl Pts',(-20.1731729387286,-30.5505495531152,
122.478730184432)) ;
#53779 = CARTESIAN_POINT('Ctrl Pts',(-20.3641515812298,-30.3705604726347,
122.245458339138)) ;
#53780 = CARTESIAN_POINT('Ctrl Pts',(-20.0013435844137,-30.5604535764232,
122.361105057577)) ;
#53781 = CARTESIAN_POINT('Ctrl Pts',(-20.1493641424933,-30.3804644959427,
122.098426355187)) ;
#53782 = CARTESIAN_POINT('Ctrl Pts',(-19.8086729775666,-30.5705140797448,
122.27392287476)) ;
#53783 = CARTESIAN_POINT('Ctrl Pts',(-19.90852625773,-30.3905249992643,121.989448658522)) ;
#53784 = CARTESIAN_POINT('Ctrl Pts',(-19.6082855481598,-30.5803546148847,
122.222396123201)) ;
#53785 = CARTESIAN_POINT('Ctrl Pts',(-19.6580405513247,-30.4003655344042,
121.925039834597)) ;
#53786 = CARTESIAN_POINT('Ctrl Pts',(-19.3974190538605,-30.5904168355893,
122.20582075455)) ;
#53787 = CARTESIAN_POINT('Ctrl Pts',(-19.3944577950554,-30.4104277551088,
121.904320739898)) ;
#53788 = CARTESIAN_POINT('Ctrl Pts',(-19.1903195961826,-30.6003139893655,
122.225997239462)) ;
#53789 = CARTESIAN_POINT('Ctrl Pts',(-19.1355824752847,-30.420324908885,121.929541441992)) ;
#53790 = CARTESIAN_POINT('Ctrl Pts',(-18.9890100939322,-30.610245122751,122.281343791059)) ;
#53791 = CARTESIAN_POINT('Ctrl Pts',(-18.8839449757313,-30.4302560422705,
121.998725089829)) ;
#53792 = CARTESIAN_POINT('Ctrl Pts',(-18.7983550338524,-30.6202874978967,
122.372017641209)) ;
#53793 = CARTESIAN_POINT('Ctrl Pts',(-18.645626417901,-30.4402984174162,122.112067478711)) ;
#53794 = CARTESIAN_POINT('Ctrl Pts',(-18.6289139729558,-30.6301734356628,
122.492389628347)) ;
#53795 = CARTESIAN_POINT('Ctrl Pts',(-18.4338243468279,-30.4501843551824,
122.26253329297)) ;
#53796 = CARTESIAN_POINT('Ctrl Pts',(-18.4811125942436,-30.6401692786477,
122.641749676501)) ;
#53797 = CARTESIAN_POINT('Ctrl Pts',(-18.2490727522653,-30.4601801981672,
122.449233759655)) ;
#53798 = CARTESIAN_POINT('Ctrl Pts',(-18.3621388083306,-30.6501112565263,
122.813609855738)) ;
#53799 = CARTESIAN_POINT('Ctrl Pts',(-18.1003554684514,-30.4701221760458,
122.664059702163)) ;
#53800 = CARTESIAN_POINT('Ctrl Pts',(-18.2744107318474,-30.6600706310073,
123.003708981063)) ;
#53801 = CARTESIAN_POINT('Ctrl Pts',(-17.9906956058916,-30.4800815505268,
122.901684237727)) ;
#53802 = CARTESIAN_POINT('Ctrl Pts',(-18.2207100016037,-30.6700672468411,
123.206915248933)) ;
#53803 = CARTESIAN_POINT('Ctrl Pts',(-17.9235701571925,-30.4900781663606,
123.155692351236)) ;
#53804 = CARTESIAN_POINT('Ctrl Pts',(-18.2033237827632,-30.6801014654146,
123.4171423923)) ;
#53805 = CARTESIAN_POINT('Ctrl Pts',(-17.9018377985399,-30.5001123849341,
123.418476175523)) ;
#53806 = CARTESIAN_POINT('Ctrl Pts',(-18.2221037500632,-30.6899545326252,
123.623428518409)) ;
#53807 = CARTESIAN_POINT('Ctrl Pts',(-17.9253133850039,-30.5099654521447,
123.676335153536)) ;
#53808 = CARTESIAN_POINT('Ctrl Pts',(-18.2764164848045,-30.6999147905028,
123.825650685452)) ;
#53809 = CARTESIAN_POINT('Ctrl Pts',(-17.9932051452733,-30.5199257100223,
123.929113115031)) ;
#53810 = CARTESIAN_POINT('Ctrl Pts',(-18.3658619188668,-30.7099438172084,
124.016591993771)) ;
#53811 = CARTESIAN_POINT('Ctrl Pts',(-18.1050124819291,-30.5299547367279,
124.167789386679)) ;
#53812 = CARTESIAN_POINT('Ctrl Pts',(-18.4856036512729,-30.7198540242428,
124.187076921124)) ;
#53813 = CARTESIAN_POINT('Ctrl Pts',(-18.2546907013589,-30.5398649437623,
124.38089587769)) ;
#53814 = CARTESIAN_POINT('Ctrl Pts',(-18.6331183540979,-30.7297889348904,
124.334947217682)) ;
#53815 = CARTESIAN_POINT('Ctrl Pts',(-18.4390851724794,-30.5497998544099,
124.565733592128)) ;
#53816 = CARTESIAN_POINT('Ctrl Pts',(-18.805998293057,-30.7398300650696,124.456072455855)) ;
#53817 = CARTESIAN_POINT('Ctrl Pts',(-18.6551854057715,-30.5598409845892,
124.71713937116)) ;
#53818 = CARTESIAN_POINT('Ctrl Pts',(-18.9943042437929,-30.7497172054396,
124.544111417618)) ;
#53819 = CARTESIAN_POINT('Ctrl Pts',(-18.8905691521537,-30.5697281249591,
124.82718773236)) ;
#53820 = CARTESIAN_POINT('Ctrl Pts',(-19.1970545158081,-30.7597094829755,
124.599022917554)) ;
#53821 = CARTESIAN_POINT('Ctrl Pts',(-19.1440074489892,-30.5797204024951,
124.895826199373)) ;
#53822 = CARTESIAN_POINT('Ctrl Pts',(-19.4053746987768,-30.7696580262439,
124.617756988556)) ;
#53823 = CARTESIAN_POINT('Ctrl Pts',(-19.4044083048236,-30.5896689457634,
124.919242869129)) ;
#53824 = CARTESIAN_POINT('Ctrl Pts',(-19.6135329763721,-30.7795947010611,
124.60035612135)) ;
#53825 = CARTESIAN_POINT('Ctrl Pts',(-19.6646066985411,-30.5996056205806,
124.897490651167)) ;
#53826 = CARTESIAN_POINT('Ctrl Pts',(-19.8165585167842,-30.7895781219974,
124.5470606735)) ;
#53827 = CARTESIAN_POINT('Ctrl Pts',(-19.9183885697259,-30.609589041517,124.830870141042)) ;
#53828 = CARTESIAN_POINT('Ctrl Pts',(-20.0081989085124,-30.7996204371867,
124.458507416817)) ;
#53829 = CARTESIAN_POINT('Ctrl Pts',(-20.1579384639164,-30.6196313567062,
124.720177687005)) ;
#53830 = CARTESIAN_POINT('Ctrl Pts',(-20.1782668651698,-30.8094607546259,
124.340716223305)) ;
#53831 = CARTESIAN_POINT('Ctrl Pts',(-20.3705238610805,-30.6294716741454,
124.572936952077)) ;
#53832 = CARTESIAN_POINT('Ctrl Pts',(-20.328476682033,-30.8194904586834,124.192735300873)) ;
#53833 = CARTESIAN_POINT('Ctrl Pts',(-20.5582851077413,-30.6395013782029,
124.387959911914)) ;
#53834 = CARTESIAN_POINT('Ctrl Pts',(-20.4501392005903,-30.8295114154059,
124.020744611247)) ;
#53835 = CARTESIAN_POINT('Ctrl Pts',(-20.7103623024763,-30.6495223349254,
124.172970910652)) ;
#53836 = CARTESIAN_POINT('Ctrl Pts',(-20.5391909200879,-30.8393779577095,
123.833391228608)) ;
#53837 = CARTESIAN_POINT('Ctrl Pts',(-20.8216762308141,-30.659388877229,123.93877758456)) ;
#53838 = CARTESIAN_POINT('Ctrl Pts',(-20.595495855653,-30.8494490576546,123.629308992589)) ;
#53839 = CARTESIAN_POINT('Ctrl Pts',(-20.892056009971,-30.6694599771742,123.683674797214)) ;
#53840 = CARTESIAN_POINT('Ctrl Pts',(-20.6150525003595,-30.8592911318322,
123.423316450362)) ;
#53841 = CARTESIAN_POINT('Ctrl Pts',(-20.9165006066991,-30.6793020513517,
123.426182698948)) ;
#53842 = CARTESIAN_POINT('Ctrl Pts',(-20.5991170580468,-30.8692519264192,
123.214521188728)) ;
#53843 = CARTESIAN_POINT('Ctrl Pts',(-20.8965796708066,-30.6892628459388,
123.165188338034)) ;
#53844 = CARTESIAN_POINT('Ctrl Pts',(-20.546363865341,-30.8792897993201,123.010200870518)) ;
#53845 = CARTESIAN_POINT('Ctrl Pts',(-20.8306367980833,-30.6993007188396,
122.909788435374)) ;
#53846 = CARTESIAN_POINT('Ctrl Pts',(-20.4606968836195,-30.8891640848642,
122.821085418058)) ;
#53847 = CARTESIAN_POINT('Ctrl Pts',(-20.7235512012954,-30.7091750043837,
122.673393853038)) ;
#53848 = CARTESIAN_POINT('Ctrl Pts',(-20.3411946934181,-30.8992338352781,
122.646376318982)) ;
#53849 = CARTESIAN_POINT('Ctrl Pts',(-20.5741723490804,-30.7192447547976,
122.455008665835)) ;
#53850 = CARTESIAN_POINT('Ctrl Pts',(-20.19669738145,-30.9090671198127,122.498514065535)) ;
#53851 = CARTESIAN_POINT('Ctrl Pts',(-20.3935486502023,-30.7290780393323,
122.27018106757)) ;
#53852 = CARTESIAN_POINT('Ctrl Pts',(-20.025723038719,-30.9190974606128,122.375099669013)) ;
#53853 = CARTESIAN_POINT('Ctrl Pts',(-20.179829726815,-30.7391083801323,122.11591459953)) ;
#53854 = CARTESIAN_POINT('Ctrl Pts',(-19.8356036746159,-30.9291293846124,
122.283783083488)) ;
#53855 = CARTESIAN_POINT('Ctrl Pts',(-19.9421798973241,-30.7491403041319,
122.001770363294)) ;
#53856 = CARTESIAN_POINT('Ctrl Pts',(-19.6367747487569,-30.9389579195483,
122.227591752257)) ;
#53857 = CARTESIAN_POINT('Ctrl Pts',(-19.6936420289628,-30.7589688390678,
121.931532551654)) ;
#53858 = CARTESIAN_POINT('Ctrl Pts',(-19.4278031799893,-30.948951697313,122.205853025162)) ;
#53859 = CARTESIAN_POINT('Ctrl Pts',(-19.4324272173877,-30.7689626168325,
121.904361062246)) ;
#53860 = CARTESIAN_POINT('Ctrl Pts',(-19.2175414225101,-30.9589794077985,
122.221194257031)) ;
#53861 = CARTESIAN_POINT('Ctrl Pts',(-19.1696001927494,-30.778990327318,121.923539411805)) ;
#53862 = CARTESIAN_POINT('Ctrl Pts',(-19.0159184250757,-30.9688678186325,
122.271841404524)) ;
#53863 = CARTESIAN_POINT('Ctrl Pts',(-18.9175710994201,-30.788878738152,121.986850390242)) ;
#53864 = CARTESIAN_POINT('Ctrl Pts',(-18.8243211742747,-30.978844669168,122.357145110244)) ;
#53865 = CARTESIAN_POINT('Ctrl Pts',(-18.678075116747,-30.7988555886875,122.093481958208)) ;
#53866 = CARTESIAN_POINT('Ctrl Pts',(-18.6501372622533,-30.9888364657185,
122.474607486696)) ;
#53867 = CARTESIAN_POINT('Ctrl Pts',(-18.4603462227314,-30.808847385238,122.240311680626)) ;
#53868 = CARTESIAN_POINT('Ctrl Pts',(-18.4985386548746,-30.9988724718122,
122.621327863081)) ;
#53869 = CARTESIAN_POINT('Ctrl Pts',(-18.2708493728752,-30.8188833913317,
122.423713476581)) ;
#53870 = CARTESIAN_POINT('Ctrl Pts',(-18.3767267027261,-31.008723206075,122.788826198165)) ;
#53871 = CARTESIAN_POINT('Ctrl Pts',(-18.1185854661369,-30.8287341255945,
122.633088418343)) ;
#53872 = CARTESIAN_POINT('Ctrl Pts',(-18.2842463817907,-31.0187144646032,
122.977386152329)) ;
#53873 = CARTESIAN_POINT('Ctrl Pts',(-18.0029869056345,-30.8387253841227,
122.868789450523)) ;
#53874 = CARTESIAN_POINT('Ctrl Pts',(-18.2262044455862,-31.0286323595064,
123.177677702795)) ;
#53875 = CARTESIAN_POINT('Ctrl Pts',(-17.9304363999913,-30.8486432790259,
123.119155041234)) ;
#53876 = CARTESIAN_POINT('Ctrl Pts',(-18.2035238002497,-31.0386605011694,
123.387260137324)) ;
#53877 = CARTESIAN_POINT('Ctrl Pts',(-17.9020877612529,-30.8586714206889,
123.381133283296)) ;
#53878 = CARTESIAN_POINT('Ctrl Pts',(-18.2172919464805,-31.0485456692853,
123.594625950143)) ;
#53879 = CARTESIAN_POINT('Ctrl Pts',(-17.9193001862951,-30.8685565888048,
123.640341140652)) ;
#53880 = CARTESIAN_POINT('Ctrl Pts',(-18.2668826506638,-31.0585350327913,
123.79869899324)) ;
#53881 = CARTESIAN_POINT('Ctrl Pts',(-17.9812908653985,-30.8785459523108,
123.895432047614)) ;
#53882 = CARTESIAN_POINT('Ctrl Pts',(-18.3519971283237,-31.0685761678013,
123.991875632271)) ;
#53883 = CARTESIAN_POINT('Ctrl Pts',(-18.0876859529692,-30.8885870873209,
124.136901868432)) ;
#53884 = CARTESIAN_POINT('Ctrl Pts',(-18.4666381472819,-31.0784088359894,
124.163882158032)) ;
#53885 = CARTESIAN_POINT('Ctrl Pts',(-18.2309896741229,-30.8984197555089,
124.351909547832)) ;
#53886 = CARTESIAN_POINT('Ctrl Pts',(-18.6113111204173,-31.0884027389439,
124.31623927594)) ;
#53887 = CARTESIAN_POINT('Ctrl Pts',(-18.4118327451302,-30.9084136584634,
124.542354351797)) ;
#53888 = CARTESIAN_POINT('Ctrl Pts',(-18.7811066172618,-31.0984320240284,
124.441246279883)) ;
#53889 = CARTESIAN_POINT('Ctrl Pts',(-18.6240784847037,-30.9184429435479,
124.698611210705)) ;
#53890 = CARTESIAN_POINT('Ctrl Pts',(-18.9669894085724,-31.1083075524703,
124.533744474352)) ;
#53891 = CARTESIAN_POINT('Ctrl Pts',(-18.8564336547338,-30.9283184719898,
124.814232094109)) ;
#53892 = CARTESIAN_POINT('Ctrl Pts',(-19.1685234135853,-31.1183078350863,
124.593519235339)) ;
#53893 = CARTESIAN_POINT('Ctrl Pts',(-19.1083519713198,-30.9383187546059,
124.888948210997)) ;
#53894 = CARTESIAN_POINT('Ctrl Pts',(-19.3755624886653,-31.1282198511434,
124.617355261767)) ;
#53895 = CARTESIAN_POINT('Ctrl Pts',(-19.3671515658149,-30.9482307706629,
124.918740815905)) ;
#53896 = CARTESIAN_POINT('Ctrl Pts',(-19.5862881147713,-31.1382619264824,
124.604773299215)) ;
#53897 = CARTESIAN_POINT('Ctrl Pts',(-19.6305583757135,-30.9582728460019,
124.903010863219)) ;
#53898 = CARTESIAN_POINT('Ctrl Pts',(-19.7887432035316,-31.1481617591385,
124.556475850266)) ;
#53899 = CARTESIAN_POINT('Ctrl Pts',(-19.8836271404046,-30.968172678658,124.842636497184)) ;
#53900 = CARTESIAN_POINT('Ctrl Pts',(-19.9816984118981,-31.1581541597165,
124.473418066137)) ;
#53901 = CARTESIAN_POINT('Ctrl Pts',(-20.1248202353964,-30.978165079236,124.738811837859)) ;
#53902 = CARTESIAN_POINT('Ctrl Pts',(-20.1578289058847,-31.1681881814759,
124.357322944161)) ;
#53903 = CARTESIAN_POINT('Ctrl Pts',(-20.3449819507396,-30.9881991009954,
124.593690836026)) ;
#53904 = CARTESIAN_POINT('Ctrl Pts',(-20.3087153180884,-31.1780527923171,
124.215054802295)) ;
#53905 = CARTESIAN_POINT('Ctrl Pts',(-20.5335886316018,-30.9980637118366,
124.415853378538)) ;
#53906 = CARTESIAN_POINT('Ctrl Pts',(-20.4346283251563,-31.1880451917782,
124.046895705598)) ;
#53907 = CARTESIAN_POINT('Ctrl Pts',(-20.6909778267488,-31.0080561112978,
124.205652827249)) ;
#53908 = CARTESIAN_POINT('Ctrl Pts',(-20.5294345452315,-31.1980771451111,
123.858502766262)) ;
#53909 = CARTESIAN_POINT('Ctrl Pts',(-20.8094832864475,-31.0180880646307,
123.97016048948)) ;
#53910 = CARTESIAN_POINT('Ctrl Pts',(-20.5893954841832,-31.2079435040528,
123.659927548445)) ;
#53911 = CARTESIAN_POINT('Ctrl Pts',(-20.8844320814046,-31.0279544235723,
123.721940205766)) ;
#53912 = CARTESIAN_POINT('Ctrl Pts',(-20.6146037556417,-31.2179309795386,
123.451503773627)) ;
#53913 = CARTESIAN_POINT('Ctrl Pts',(-20.915939761088,-31.0379418990581,123.461410041665)) ;
#53914 = CARTESIAN_POINT('Ctrl Pts',(-20.6033971471085,-31.2278758857271,
123.24270000188)) ;
#53915 = CARTESIAN_POINT('Ctrl Pts',(-20.9019287888384,-31.0478868052466,
123.200405236552)) ;
#53916 = CARTESIAN_POINT('Ctrl Pts',(-20.5555242405054,-31.2379208503873,
123.037041915201)) ;
#53917 = CARTESIAN_POINT('Ctrl Pts',(-20.842085039233,-31.0579317699068,122.943333258372)) ;
#53918 = CARTESIAN_POINT('Ctrl Pts',(-20.4743386324737,-31.2477826572922,
122.846253520561)) ;
#53919 = CARTESIAN_POINT('Ctrl Pts',(-20.7406003648983,-31.0677935768117,
122.704848430347)) ;
#53920 = CARTESIAN_POINT('Ctrl Pts',(-20.360117950421,-31.2577753295979,122.669966551316)) ;
#53921 = CARTESIAN_POINT('Ctrl Pts',(-20.5978221442473,-31.0777862491175,
122.484491140152)) ;
#53922 = CARTESIAN_POINT('Ctrl Pts',(-20.2178975470522,-31.2677040005433,
122.51716583229)) ;
#53923 = CARTESIAN_POINT('Ctrl Pts',(-20.4200444704518,-31.0877149200628,
122.293491950862)) ;
#53924 = CARTESIAN_POINT('Ctrl Pts',(-20.0511349253016,-31.2776565427686,
122.390821276081)) ;
#53925 = CARTESIAN_POINT('Ctrl Pts',(-20.2115893828886,-31.0976674622881,
122.13556337995)) ;
#53926 = CARTESIAN_POINT('Ctrl Pts',(-19.8640731557152,-31.2876578987645,
122.294767252677)) ;
#53927 = CARTESIAN_POINT('Ctrl Pts',(-19.9777608299036,-31.107668818284,122.015498299197)) ;
#53928 = CARTESIAN_POINT('Ctrl Pts',(-19.6625721454269,-31.2976865110392,
122.232767913839)) ;
#53929 = CARTESIAN_POINT('Ctrl Pts',(-19.7258837090917,-31.1176974305587,
121.938001760738)) ;
#53930 = CARTESIAN_POINT('Ctrl Pts',(-19.4568083883109,-31.3075508455887,
122.20682000382)) ;
#53931 = CARTESIAN_POINT('Ctrl Pts',(-19.4686784023227,-31.1275617651082,
121.905569609597)) ;
#53932 = CARTESIAN_POINT('Ctrl Pts',(-19.2470034323369,-31.3175431696653,
122.216797567056)) ;
#53933 = CARTESIAN_POINT('Ctrl Pts',(-19.2064222622947,-31.1375540891848,
121.918044378249)) ;
#53934 = CARTESIAN_POINT('Ctrl Pts',(-19.0433631987087,-31.3274706620311,
122.26264289437)) ;
#53935 = CARTESIAN_POINT('Ctrl Pts',(-18.951872457949,-31.1474815815507,121.97535381061)) ;
#53936 = CARTESIAN_POINT('Ctrl Pts',(-18.8488944828603,-31.337498020582,122.343946304587)) ;
#53937 = CARTESIAN_POINT('Ctrl Pts',(-18.7087875924264,-31.1575089401015,
122.07698569699)) ;
#53938 = CARTESIAN_POINT('Ctrl Pts',(-18.6738227975292,-31.3473844386331,
122.456025056537)) ;
#53939 = CARTESIAN_POINT('Ctrl Pts',(-18.489949403028,-31.1673953581526,122.217086575843)) ;
#53940 = CARTESIAN_POINT('Ctrl Pts',(-18.5185992416469,-31.3574161733685,
122.598745584505)) ;
#53941 = CARTESIAN_POINT('Ctrl Pts',(-18.2959218217005,-31.177427092888,122.395489361633)) ;
#53942 = CARTESIAN_POINT('Ctrl Pts',(-18.3922256515261,-31.3672977546117,
122.76367605931)) ;
#53943 = CARTESIAN_POINT('Ctrl Pts',(-18.1379570316175,-31.1873086741313,
122.601654223981)) ;
#53944 = CARTESIAN_POINT('Ctrl Pts',(-18.2946472022262,-31.3773597326441,
122.951323265286)) ;
#53945 = CARTESIAN_POINT('Ctrl Pts',(-18.0159864386177,-31.1973706521636,
122.836214609503)) ;
#53946 = CARTESIAN_POINT('Ctrl Pts',(-18.2323356671991,-31.3872168110058,
123.148990652215)) ;
#53947 = CARTESIAN_POINT('Ctrl Pts',(-17.9380997060772,-31.2072277305253,
123.083299705049)) ;
#53948 = CARTESIAN_POINT('Ctrl Pts',(-18.2045044604485,-31.3972113841118,
123.357222538529)) ;
#53949 = CARTESIAN_POINT('Ctrl Pts',(-17.90331347904,-31.2172223036313,123.343589981837)) ;
#53950 = CARTESIAN_POINT('Ctrl Pts',(-18.2131184967394,-31.4071371803994,
123.565745265259)) ;
#53951 = CARTESIAN_POINT('Ctrl Pts',(-17.9140838361603,-31.2271480999189,
123.604243273505)) ;
#53952 = CARTESIAN_POINT('Ctrl Pts',(-18.2581923238068,-31.4171625475691,
123.771616644239)) ;
#53953 = CARTESIAN_POINT('Ctrl Pts',(-17.9704288395072,-31.2371734670886,
123.861581949302)) ;
#53954 = CARTESIAN_POINT('Ctrl Pts',(-18.3372215849961,-31.427058627223,123.964077719536)) ;
#53955 = CARTESIAN_POINT('Ctrl Pts',(-18.0692181288422,-31.2470695467425,
124.102157307158)) ;
#53956 = CARTESIAN_POINT('Ctrl Pts',(-18.4492191595014,-31.4370537069285,
124.141874347234)) ;
#53957 = CARTESIAN_POINT('Ctrl Pts',(-18.2092168771544,-31.2570646264481,
124.324401075106)) ;
#53958 = CARTESIAN_POINT('Ctrl Pts',(-18.5910734083571,-31.4470787947444,
124.297744881585)) ;
#53959 = CARTESIAN_POINT('Ctrl Pts',(-18.3865390044903,-31.2670897142639,
124.519239587028)) ;
#53960 = CARTESIAN_POINT('Ctrl Pts',(-18.8100884239902,-31.4602626171116,
124.467625344121)) ;
#53961 = CARTESIAN_POINT('Ctrl Pts',(-18.6602990639884,-31.2802735366311,
124.73157647326)) ;
#53962 = CARTESIAN_POINT('Ctrl Pts',(-19.0709153029651,-31.4735847352576,
124.578138378408)) ;
#53963 = CARTESIAN_POINT('Ctrl Pts',(-18.9862948593756,-31.2935956547771,
124.869711357503)) ;
#53964 = CARTESIAN_POINT('Ctrl Pts',(-19.3495941389619,-31.4869639448852,
124.6162385658)) ;
#53965 = CARTESIAN_POINT('Ctrl Pts',(-19.3347015527478,-31.3069748644047,
124.917347223375)) ;
#53966 = CARTESIAN_POINT('Ctrl Pts',(-19.5563094575702,-31.4968021821294,
124.608810856145)) ;
#53967 = CARTESIAN_POINT('Ctrl Pts',(-19.5930836021452,-31.3168131016489,
124.908057132505)) ;
#53968 = CARTESIAN_POINT('Ctrl Pts',(-19.763395166937,-31.5068751053881,124.564668379505)) ;
#53969 = CARTESIAN_POINT('Ctrl Pts',(-19.8519437779816,-31.3268860249076,
124.852876717883)) ;
#53970 = CARTESIAN_POINT('Ctrl Pts',(-19.9554908372654,-31.5167317468432,
124.486904342967)) ;
#53971 = CARTESIAN_POINT('Ctrl Pts',(-20.0920602273854,-31.3367426663627,
124.755670606854)) ;
#53972 = CARTESIAN_POINT('Ctrl Pts',(-20.1337307856986,-31.5267171223493,
124.376027908366)) ;
#53973 = CARTESIAN_POINT('Ctrl Pts',(-20.3148623985469,-31.3467280418688,
124.617067390202)) ;
#53974 = CARTESIAN_POINT('Ctrl Pts',(-20.3414635779869,-31.5400011538097,
124.189405170033)) ;
#53975 = CARTESIAN_POINT('Ctrl Pts',(-20.5745088880955,-31.3600120733292,
124.383813943101)) ;
#53976 = CARTESIAN_POINT('Ctrl Pts',(-20.5342357011611,-31.55651994568,123.895695798079)) ;
#53977 = CARTESIAN_POINT('Ctrl Pts',(-20.8154916494353,-31.3765308651996,
124.01662607274)) ;
#53978 = CARTESIAN_POINT('Ctrl Pts',(-20.615702601322,-31.5733056626867,123.5482462708)) ;
#53979 = CARTESIAN_POINT('Ctrl Pts',(-20.9173070494684,-31.3933165822062,
123.582394229606)) ;
#53980 = CARTESIAN_POINT('Ctrl Pts',(-20.607065235222,-31.5864188111957,123.272686183113)) ;
#53981 = CARTESIAN_POINT('Ctrl Pts',(-20.9065152950927,-31.4064297307152,
123.237879258035)) ;
#53982 = CARTESIAN_POINT('Ctrl Pts',(-20.5647775941507,-31.5964543602758,
123.066008473396)) ;
#53983 = CARTESIAN_POINT('Ctrl Pts',(-20.8536524125432,-31.4164652797954,
122.979546305353)) ;
#53984 = CARTESIAN_POINT('Ctrl Pts',(-20.4868139035535,-31.6064704164553,
122.870382663184)) ;
#53985 = CARTESIAN_POINT('Ctrl Pts',(-20.7561932615581,-31.4264813359748,
122.735008678701)) ;
#53986 = CARTESIAN_POINT('Ctrl Pts',(-20.3416392377526,-31.6196484523213,
122.634448176635)) ;
#53987 = CARTESIAN_POINT('Ctrl Pts',(-20.5747356332259,-31.4396593718408,
122.440107128051)) ;
#53988 = CARTESIAN_POINT('Ctrl Pts',(-20.0859156395753,-31.6362503295084,
122.3910420022)) ;
#53989 = CARTESIAN_POINT('Ctrl Pts',(-20.2550642402357,-31.4562612490279,
122.135837120471)) ;
#53990 = CARTESIAN_POINT('Ctrl Pts',(-19.6946086357507,-31.6563134741243,
122.221176683087)) ;
#53991 = CARTESIAN_POINT('Ctrl Pts',(-19.7659328720363,-31.4763243936438,
121.923514400553)) ;
#53992 = CARTESIAN_POINT('Ctrl Pts',(-19.2743459249407,-31.676114364208,122.195122229128)) ;
#53993 = CARTESIAN_POINT('Ctrl Pts',(-19.2406043647654,-31.4961252837275,
121.890949553411)) ;
#53994 = CARTESIAN_POINT('Ctrl Pts',(-18.8673343999719,-31.6960574894867,
122.313844662609)) ;
#53995 = CARTESIAN_POINT('Ctrl Pts',(-18.7318418663585,-31.5160684090062,
122.039356586045)) ;
#53996 = CARTESIAN_POINT('Ctrl Pts',(-18.5261587627728,-31.7159555346063,
122.564031122159)) ;
#53997 = CARTESIAN_POINT('Ctrl Pts',(-18.305375239822,-31.5359664541258,122.352092202797)) ;
#53998 = CARTESIAN_POINT('Ctrl Pts',(-18.2900690142787,-31.735841294233,122.914876518788)) ;
#53999 = CARTESIAN_POINT('Ctrl Pts',(-18.0102664112651,-31.5558522137526,
122.790649876847)) ;
#54000 = CARTESIAN_POINT('Ctrl Pts',(-18.1876243917938,-31.7559064694129,
123.328998046209)) ;
#54001 = CARTESIAN_POINT('Ctrl Pts',(-17.8822137795074,-31.5759173889324,
123.308303291757)) ;
#54002 = CARTESIAN_POINT('Ctrl Pts',(-18.2322702694616,-31.7757331125157,
123.748268184179)) ;
#54003 = CARTESIAN_POINT('Ctrl Pts',(-17.9380242801486,-31.5957440320352,
123.832388879156)) ;
#54004 = CARTESIAN_POINT('Ctrl Pts',(-18.4169480013837,-31.7956418219641,
124.129048330367)) ;
#54005 = CARTESIAN_POINT('Ctrl Pts',(-18.1688732798574,-31.6156527414836,
124.308361931799)) ;
#54006 = CARTESIAN_POINT('Ctrl Pts',(-18.7212311690732,-31.8155936589959,
124.424824302643)) ;
#54007 = CARTESIAN_POINT('Ctrl Pts',(-18.5492284833839,-31.6356045785154,
124.678079899821)) ;
#54008 = CARTESIAN_POINT('Ctrl Pts',(-19.109410695338,-31.835602133699,124.59881362796)) ;
#54009 = CARTESIAN_POINT('Ctrl Pts',(-19.034454048953,-31.6556130532185,124.895564294194)) ;
#54010 = CARTESIAN_POINT('Ctrl Pts',(-19.5292929940374,-31.8554035924605,
124.630074904832)) ;
#54011 = CARTESIAN_POINT('Ctrl Pts',(-19.5593044715077,-31.67541451198,124.934638681304)) ;
#54012 = CARTESIAN_POINT('Ctrl Pts',(-19.9381051953959,-31.8753604806964,
124.516346944635)) ;
#54013 = CARTESIAN_POINT('Ctrl Pts',(-20.0703188208076,-31.695371400216,124.792477849263)) ;
#54014 = CARTESIAN_POINT('Ctrl Pts',(-20.2834627517452,-31.8953443181105,
124.268832628097)) ;
#54015 = CARTESIAN_POINT('Ctrl Pts',(-20.5020147232158,-31.7153552376301,
124.483083842068)) ;
#54016 = CARTESIAN_POINT('Ctrl Pts',(-20.5222631166498,-31.9151527573315,
123.921823635472)) ;
#54017 = CARTESIAN_POINT('Ctrl Pts',(-20.8005129695027,-31.735163676851,124.049324638418)) ;
#54018 = CARTESIAN_POINT('Ctrl Pts',(-20.6296391609579,-31.9351384667117,
123.510794184968)) ;
#54019 = CARTESIAN_POINT('Ctrl Pts',(-20.934732846759,-31.7551493862312,123.535538119672)) ;
#54020 = CARTESIAN_POINT('Ctrl Pts',(-20.5906472244068,-31.955007989727,123.089943615466)) ;
#54021 = CARTESIAN_POINT('Ctrl Pts',(-20.885993395325,-31.7750189092465,123.0094768274)) ;
#54022 = CARTESIAN_POINT('Ctrl Pts',(-20.4089954990554,-31.9750287288442,
122.705129085206)) ;
#54023 = CARTESIAN_POINT('Ctrl Pts',(-20.6589290214595,-31.7950396483637,
122.528458277059)) ;
#54024 = CARTESIAN_POINT('Ctrl Pts',(-20.1103555337929,-31.9948327938211,
122.408035535206)) ;
#54025 = CARTESIAN_POINT('Ctrl Pts',(-20.2856318118138,-31.8148437133407,
122.157092624872)) ;
#54026 = CARTESIAN_POINT('Ctrl Pts',(-19.7236013982933,-32.0148947575519,
122.228362978264)) ;
#54027 = CARTESIAN_POINT('Ctrl Pts',(-19.8021889397508,-31.8349056770714,
121.932500294305)) ;
#54028 = CARTESIAN_POINT('Ctrl Pts',(-19.3033421555285,-32.0347279378404,
122.192269701717)) ;
#54029 = CARTESIAN_POINT('Ctrl Pts',(-19.2768672597533,-31.8547388573599,
121.887382590581)) ;
#54030 = CARTESIAN_POINT('Ctrl Pts',(-18.8940840487304,-32.0546471351664,
122.301037263848)) ;
#54031 = CARTESIAN_POINT('Ctrl Pts',(-18.7652950498026,-31.874658054686,122.023339534989)) ;
#54032 = CARTESIAN_POINT('Ctrl Pts',(-18.5462767706842,-32.0745851602798,
122.543427443625)) ;
#54033 = CARTESIAN_POINT('Ctrl Pts',(-18.3305352275354,-31.8945960797993,
122.326324931548)) ;
#54034 = CARTESIAN_POINT('Ctrl Pts',(-18.3022836708014,-32.0944632063358,
122.888601365163)) ;
#54035 = CARTESIAN_POINT('Ctrl Pts',(-18.0255423059027,-31.9144741258554,
122.757789608099)) ;
#54036 = CARTESIAN_POINT('Ctrl Pts',(-18.1901182041216,-32.1144479406239,
123.298403225457)) ;
#54037 = CARTESIAN_POINT('Ctrl Pts',(-17.8853325729404,-31.9344588601434,
123.270040998392)) ;
#54038 = CARTESIAN_POINT('Ctrl Pts',(-18.2243400099676,-32.1343587573024,
123.720498462101)) ;
#54039 = CARTESIAN_POINT('Ctrl Pts',(-17.9281065572994,-31.9543696768219,
123.797659471974)) ;
#54040 = CARTESIAN_POINT('Ctrl Pts',(-18.4014838664741,-32.1543577328211,
124.106965037813)) ;
#54041 = CARTESIAN_POINT('Ctrl Pts',(-18.1495333780784,-31.9743686523406,
124.280744001322)) ;
#54042 = CARTESIAN_POINT('Ctrl Pts',(-18.6967305235978,-32.1741626534663,
124.40735164037)) ;
#54043 = CARTESIAN_POINT('Ctrl Pts',(-18.5185878609863,-31.9941735729858,
124.656228575554)) ;
#54044 = CARTESIAN_POINT('Ctrl Pts',(-19.0797563575211,-32.1941466137575,
124.59108153163)) ;
#54045 = CARTESIAN_POINT('Ctrl Pts',(-18.9973682959692,-32.0141575332771,
124.885894562839)) ;
#54046 = CARTESIAN_POINT('Ctrl Pts',(-19.500620909332,-32.2140328174815,124.632705731497)) ;
#54047 = CARTESIAN_POINT('Ctrl Pts',(-19.5234477413733,-32.034043737001,124.937928873815)) ;
#54048 = CARTESIAN_POINT('Ctrl Pts',(-19.91172625123,-32.2339819958047,124.528376651481)) ;
#54049 = CARTESIAN_POINT('Ctrl Pts',(-20.0373301586455,-32.0539929153242,
124.807521706338)) ;
#54050 = CARTESIAN_POINT('Ctrl Pts',(-20.2616847114276,-32.2538837950442,
124.290492641391)) ;
#54051 = CARTESIAN_POINT('Ctrl Pts',(-20.4747803852408,-32.0738947145637,
124.510171457573)) ;
#54052 = CARTESIAN_POINT('Ctrl Pts',(-20.5099132977842,-32.2737624000966,
123.948363389314)) ;
#54053 = CARTESIAN_POINT('Ctrl Pts',(-20.7850691734418,-32.0937733196161,
124.082510674381)) ;
#54054 = CARTESIAN_POINT('Ctrl Pts',(-20.627203071623,-32.2937947598223,123.538857802633)) ;
#54055 = CARTESIAN_POINT('Ctrl Pts',(-20.9316880821038,-32.1138056793418,
123.570639459005)) ;
#54056 = CARTESIAN_POINT('Ctrl Pts',(-20.6022414190364,-32.3103764857783,
123.187181314506)) ;
#54057 = CARTESIAN_POINT('Ctrl Pts',(-20.9004840930374,-32.1303874052979,
123.131013871443)) ;
#54058 = CARTESIAN_POINT('Ctrl Pts',(-20.5124528604533,-32.3235706560763,
122.924720422985)) ;
#54059 = CARTESIAN_POINT('Ctrl Pts',(-20.788262838901,-32.1435815755958,122.802971043115)) ;
#54060 = CARTESIAN_POINT('Ctrl Pts',(-20.3776944343899,-32.3368828341695,
122.679500006612)) ;
#54061 = CARTESIAN_POINT('Ctrl Pts',(-20.6197762200585,-32.156893753689,122.496386987727)) ;
#54062 = CARTESIAN_POINT('Ctrl Pts',(-20.1339928139378,-32.3534490137628,
122.425047262597)) ;
#54063 = CARTESIAN_POINT('Ctrl Pts',(-20.3152084468331,-32.1734599332823,
122.178383590779)) ;
#54064 = CARTESIAN_POINT('Ctrl Pts',(-19.8172190621121,-32.370077208623,122.268225534679)) ;
#54065 = CARTESIAN_POINT('Ctrl Pts',(-19.9191951146559,-32.1900881281425,
121.98231868388)) ;
#54066 = CARTESIAN_POINT('Ctrl Pts',(-19.5432299461013,-32.3833657903327,
122.213296215293)) ;
#54067 = CARTESIAN_POINT('Ctrl Pts',(-19.576742054398,-32.2033767098523,121.913670003135)) ;
#54068 = CARTESIAN_POINT('Ctrl Pts',(-19.3337508719107,-32.3933340384363,
122.208232309393)) ;
#54069 = CARTESIAN_POINT('Ctrl Pts',(-19.3148866166722,-32.2133449579559,
121.90733429029)) ;
#54070 = CARTESIAN_POINT('Ctrl Pts',(-19.1276189549108,-32.4032487946925,
122.239193486121)) ;
#54071 = CARTESIAN_POINT('Ctrl Pts',(-19.0572238635517,-32.223259714212,121.946033185413)) ;
#54072 = CARTESIAN_POINT('Ctrl Pts',(-18.9279557063151,-32.4132619453437,
122.305913698926)) ;
#54073 = CARTESIAN_POINT('Ctrl Pts',(-18.8076409321752,-32.2332728648632,
122.029433371211)) ;
#54074 = CARTESIAN_POINT('Ctrl Pts',(-18.7430842089401,-32.4232746525457,
122.406578399065)) ;
#54075 = CARTESIAN_POINT('Ctrl Pts',(-18.5765593856167,-32.2432855720652,
122.155251711997)) ;
#54076 = CARTESIAN_POINT('Ctrl Pts',(-18.5254677572598,-32.436493941237,122.579410532713)) ;
#54077 = CARTESIAN_POINT('Ctrl Pts',(-18.3044914720328,-32.2565048607565,
122.371339808038)) ;
#54078 = CARTESIAN_POINT('Ctrl Pts',(-18.3148360496128,-32.453112622235,122.863088731423)) ;
#54079 = CARTESIAN_POINT('Ctrl Pts',(-18.041252038348,-32.2731235417546,122.725865755934)) ;
#54080 = CARTESIAN_POINT('Ctrl Pts',(-18.2135427727924,-32.4696775300085,
123.200444286709)) ;
#54081 = CARTESIAN_POINT('Ctrl Pts',(-17.9146049568551,-32.289688449528,123.147620680701)) ;
#54082 = CARTESIAN_POINT('Ctrl Pts',(-18.2053428109417,-32.4830760016193,
123.482028619465)) ;
#54083 = CARTESIAN_POINT('Ctrl Pts',(-17.9043631043354,-32.3030869211388,
123.499558748913)) ;
#54084 = CARTESIAN_POINT('Ctrl Pts',(-18.2351263930126,-32.4929172571063,
123.686778633759)) ;
#54085 = CARTESIAN_POINT('Ctrl Pts',(-17.9415874187144,-32.3129281766258,
123.755505137596)) ;
#54086 = CARTESIAN_POINT('Ctrl Pts',(-18.3005104295691,-32.5029035726945,
123.886247272274)) ;
#54087 = CARTESIAN_POINT('Ctrl Pts',(-18.0233154438323,-32.322914492214,124.00483961092)) ;
#54088 = CARTESIAN_POINT('Ctrl Pts',(-18.3989864711992,-32.5128401802809,
124.070517770327)) ;
#54089 = CARTESIAN_POINT('Ctrl Pts',(-18.1464078761575,-32.3328510998004,
124.235179732808)) ;
#54090 = CARTESIAN_POINT('Ctrl Pts',(-18.5294794836623,-32.5228900476492,
124.236655331214)) ;
#54091 = CARTESIAN_POINT('Ctrl Pts',(-18.3095220074042,-32.3429009671687,
124.442853309995)) ;
#54092 = CARTESIAN_POINT('Ctrl Pts',(-18.6836393496476,-32.532740542324,124.374955006091)) ;
#54093 = CARTESIAN_POINT('Ctrl Pts',(-18.50222003047,-32.3527514618435,124.615730119601)) ;
#54094 = CARTESIAN_POINT('Ctrl Pts',(-18.8613101056891,-32.5427123427185,
124.486175930194)) ;
#54095 = CARTESIAN_POINT('Ctrl Pts',(-18.7243070866431,-32.362723262238,124.754758703811)) ;
#54096 = CARTESIAN_POINT('Ctrl Pts',(-19.0561314475104,-32.5527083097443,
124.565050529732)) ;
#54097 = CARTESIAN_POINT('Ctrl Pts',(-18.9678327867977,-32.3727192292638,
124.853354582607)) ;
#54098 = CARTESIAN_POINT('Ctrl Pts',(-19.2625472172633,-32.5627457691255,
124.608788649609)) ;
#54099 = CARTESIAN_POINT('Ctrl Pts',(-19.225851948972,-32.382756688645,124.908029995055)) ;
#54100 = CARTESIAN_POINT('Ctrl Pts',(-19.4693094256783,-32.5725864700262,
124.616272691469)) ;
#54101 = CARTESIAN_POINT('Ctrl Pts',(-19.4843048557994,-32.3925973895458,
124.917387851591)) ;
#54102 = CARTESIAN_POINT('Ctrl Pts',(-19.6785662287874,-32.5826344912936,
124.587453910695)) ;
#54103 = CARTESIAN_POINT('Ctrl Pts',(-19.7458762677244,-32.4026454108131,
124.881367125457)) ;
#54104 = CARTESIAN_POINT('Ctrl Pts',(-19.8775350367199,-32.5925818843763,
124.523064897387)) ;
#54105 = CARTESIAN_POINT('Ctrl Pts',(-19.9945882738826,-32.4125928038958,
124.80088348232)) ;
#54106 = CARTESIAN_POINT('Ctrl Pts',(-20.0619149648412,-32.6024920304227,
124.426032573854)) ;
#54107 = CARTESIAN_POINT('Ctrl Pts',(-20.225064686472,-32.4225029499422,124.679595400819)) ;
#54108 = CARTESIAN_POINT('Ctrl Pts',(-20.2289464125442,-32.6125509442723,
124.296375819046)) ;
#54109 = CARTESIAN_POINT('Ctrl Pts',(-20.4338556736144,-32.4325618637918,
124.517526669095)) ;
#54110 = CARTESIAN_POINT('Ctrl Pts',(-20.3680971425257,-32.6223917145616,
124.143243416164)) ;
#54111 = CARTESIAN_POINT('Ctrl Pts',(-20.607796392533,-32.4424026340811,124.326112710897)) ;
#54112 = CARTESIAN_POINT('Ctrl Pts',(-20.4812183694655,-32.6324545841402,
123.964505832737)) ;
#54113 = CARTESIAN_POINT('Ctrl Pts',(-20.7492002052201,-32.4524655036597,
124.102692225439)) ;
#54114 = CARTESIAN_POINT('Ctrl Pts',(-20.5601018658738,-32.6423489072707,
123.772009901321)) ;
#54115 = CARTESIAN_POINT('Ctrl Pts',(-20.8478072364981,-32.4623598267902,
123.86207304764)) ;
#54116 = CARTESIAN_POINT('Ctrl Pts',(-20.6051186285884,-32.6522907143652,
123.567933795961)) ;
#54117 = CARTESIAN_POINT('Ctrl Pts',(-20.9040808604004,-32.4723016338847,
123.606978235619)) ;
#54118 = CARTESIAN_POINT('Ctrl Pts',(-20.6141529517269,-32.6622932253205,
123.357815073032)) ;
#54119 = CARTESIAN_POINT('Ctrl Pts',(-20.9153764260027,-32.48230414484,123.344329862461)) ;
#54120 = CARTESIAN_POINT('Ctrl Pts',(-20.5861553370163,-32.6723279461389,
123.148732523265)) ;
#54121 = CARTESIAN_POINT('Ctrl Pts',(-20.8803820949981,-32.4923388656584,
123.082976330961)) ;
#54122 = CARTESIAN_POINT('Ctrl Pts',(-20.5238045844199,-32.6821731236446,
122.95135818224)) ;
#54123 = CARTESIAN_POINT('Ctrl Pts',(-20.8024460214919,-32.5021840431641,
122.83625706854)) ;
#54124 = CARTESIAN_POINT('Ctrl Pts',(-20.4271596502256,-32.6921578840457,
122.76505202383)) ;
#54125 = CARTESIAN_POINT('Ctrl Pts',(-20.6816420859839,-32.5121688035652,
122.603373026508)) ;
#54126 = CARTESIAN_POINT('Ctrl Pts',(-20.3002621335287,-32.7020967903621,
122.599012732577)) ;
#54127 = CARTESIAN_POINT('Ctrl Pts',(-20.5230220509735,-32.5221077098816,
122.395822102311)) ;
#54128 = CARTESIAN_POINT('Ctrl Pts',(-20.1448530384785,-32.7121390179978,
122.456148065448)) ;
#54129 = CARTESIAN_POINT('Ctrl Pts',(-20.328762473054,-32.5321499375173,122.217239391445)) ;
#54130 = CARTESIAN_POINT('Ctrl Pts',(-19.9698227420243,-32.7220242295822,
122.344065587158)) ;
#54131 = CARTESIAN_POINT('Ctrl Pts',(-20.1099755421832,-32.5420351491017,
122.077133850243)) ;
#54132 = CARTESIAN_POINT('Ctrl Pts',(-19.7759374579204,-32.7320231597841,
122.262927443023)) ;
#54133 = CARTESIAN_POINT('Ctrl Pts',(-19.8676198088022,-32.5520340793036,
121.975708802641)) ;
#54134 = CARTESIAN_POINT('Ctrl Pts',(-19.5725517032629,-32.7419405826945,
122.216894103156)) ;
#54135 = CARTESIAN_POINT('Ctrl Pts',(-19.6133877400385,-32.5619515022141,
121.918164610046)) ;
#54136 = CARTESIAN_POINT('Ctrl Pts',(-19.3615855045364,-32.7519885147733,
122.206786949472)) ;
#54137 = CARTESIAN_POINT('Ctrl Pts',(-19.3496802081886,-32.5719994342928,
121.905528177567)) ;
#54138 = CARTESIAN_POINT('Ctrl Pts',(-19.1555344402761,-32.7618658905827,
122.232817208028)) ;
#54139 = CARTESIAN_POINT('Ctrl Pts',(-19.0921154350127,-32.5818768101022,
121.938063647228)) ;
#54140 = CARTESIAN_POINT('Ctrl Pts',(-18.9536242961126,-32.7719197837506,
122.29520263043)) ;
#54141 = CARTESIAN_POINT('Ctrl Pts',(-18.839727160302,-32.5919307032701,122.01604306292)) ;
#54142 = CARTESIAN_POINT('Ctrl Pts',(-18.7684970290784,-32.7818134070039,
122.390109939971)) ;
#54143 = CARTESIAN_POINT('Ctrl Pts',(-18.6083164556516,-32.6018243265234,
122.134675323862)) ;
#54144 = CARTESIAN_POINT('Ctrl Pts',(-18.5998696574853,-32.7918760006269,
122.517792698711)) ;
#54145 = CARTESIAN_POINT('Ctrl Pts',(-18.3975309340417,-32.6118869201464,
122.294276744004)) ;
#54146 = CARTESIAN_POINT('Ctrl Pts',(-18.4590017312758,-32.8017185746159,
122.669394023076)) ;
#54147 = CARTESIAN_POINT('Ctrl Pts',(-18.2214436962378,-32.6217294941355,
122.483777412006)) ;
#54148 = CARTESIAN_POINT('Ctrl Pts',(-18.3445119360111,-32.8117093314989,
122.845452008546)) ;
#54149 = CARTESIAN_POINT('Ctrl Pts',(-18.078329458085,-32.6317202510184,122.703848805808)) ;
#54150 = CARTESIAN_POINT('Ctrl Pts',(-18.2628657738663,-32.8216373932568,
123.037550195113)) ;
#54151 = CARTESIAN_POINT('Ctrl Pts',(-17.9762694760485,-32.6416483127763,
122.943971098603)) ;
#54152 = CARTESIAN_POINT('Ctrl Pts',(-18.2151746216112,-32.831625369146,123.242049850644)) ;
#54153 = CARTESIAN_POINT('Ctrl Pts',(-17.9166533725228,-32.6516362886655,
123.199595350713)) ;
#54154 = CARTESIAN_POINT('Ctrl Pts',(-18.2040142138472,-32.8416610335024,
123.452729593888)) ;
#54155 = CARTESIAN_POINT('Ctrl Pts',(-17.902700600024,-32.6616719530219,123.462944824455)) ;
#54156 = CARTESIAN_POINT('Ctrl Pts',(-18.2288249971323,-32.8515169719221,
123.658452238389)) ;
#54157 = CARTESIAN_POINT('Ctrl Pts',(-17.9337120199493,-32.6715278914416,
123.720099296894)) ;
#54158 = CARTESIAN_POINT('Ctrl Pts',(-18.2894914318515,-32.861512463319,123.859618101424)) ;
#54159 = CARTESIAN_POINT('Ctrl Pts',(-18.009543101011,-32.6815233828385,123.971557376393)) ;
#54160 = CARTESIAN_POINT('Ctrl Pts',(-18.3833118947942,-32.8714222682724,
124.045643520541)) ;
#54161 = CARTESIAN_POINT('Ctrl Pts',(-18.1268171253965,-32.691433187792,124.204090672423)) ;
#54162 = CARTESIAN_POINT('Ctrl Pts',(-18.509018904418,-32.8814344905392,124.214478322823)) ;
#54163 = CARTESIAN_POINT('Ctrl Pts',(-18.2839493309718,-32.7014454100587,
124.415135395411)) ;
#54164 = CARTESIAN_POINT('Ctrl Pts',(-18.6626514296269,-32.891462371232,124.358845529882)) ;
#54165 = CARTESIAN_POINT('Ctrl Pts',(-18.4759885041055,-32.7114732907515,
124.59559589002)) ;
#54166 = CARTESIAN_POINT('Ctrl Pts',(-18.8358044204708,-32.9013187672146,
124.472662632877)) ;
#54167 = CARTESIAN_POINT('Ctrl Pts',(-18.6924294795772,-32.7213296867342,
124.737869481036)) ;
#54168 = CARTESIAN_POINT('Ctrl Pts',(-19.0291703242302,-32.9113435643946,
124.556493615886)) ;
#54169 = CARTESIAN_POINT('Ctrl Pts',(-18.934136091911,-32.7313544839141,124.842659911789)) ;
#54170 = CARTESIAN_POINT('Ctrl Pts',(-19.2344039020975,-32.9213744943784,
124.605003116564)) ;
#54171 = CARTESIAN_POINT('Ctrl Pts',(-19.1906775296452,-32.7413854138979,
124.903298739033)) ;
#54172 = CARTESIAN_POINT('Ctrl Pts',(-19.4409936637498,-32.931219096887,124.617286306071)) ;
#54173 = CARTESIAN_POINT('Ctrl Pts',(-19.4489157332681,-32.7512300164066,
124.91865469574)) ;
#54174 = CARTESIAN_POINT('Ctrl Pts',(-19.6497118954831,-32.9412099481111,
124.593725011282)) ;
#54175 = CARTESIAN_POINT('Ctrl Pts',(-19.7098139114921,-32.7612208676307,
124.889204775852)) ;
#54176 = CARTESIAN_POINT('Ctrl Pts',(-19.8519756476524,-32.9512477811224,
124.533550068226)) ;
#54177 = CARTESIAN_POINT('Ctrl Pts',(-19.9626440103273,-32.7712587006419,
124.813987935886)) ;
#54178 = CARTESIAN_POINT('Ctrl Pts',(-20.0372510161014,-32.9610921695878,
124.441308298038)) ;
#54179 = CARTESIAN_POINT('Ctrl Pts',(-20.1942400545334,-32.7811030891073,
124.698686780633)) ;
#54180 = CARTESIAN_POINT('Ctrl Pts',(-20.206287933549,-32.9710769739574,124.316898276306)) ;
#54181 = CARTESIAN_POINT('Ctrl Pts',(-20.4055373691669,-32.7910878934769,
124.543175419321)) ;
#54182 = CARTESIAN_POINT('Ctrl Pts',(-20.3506030576117,-32.9810164934402,
124.165738129342)) ;
#54183 = CARTESIAN_POINT('Ctrl Pts',(-20.5859328056416,-32.8010274129597,
124.354225946112)) ;
#54184 = CARTESIAN_POINT('Ctrl Pts',(-20.4675814605525,-32.9910562244416,
123.990072866531)) ;
#54185 = CARTESIAN_POINT('Ctrl Pts',(-20.7321570746235,-32.8110671439611,
124.134645385933)) ;
#54186 = CARTESIAN_POINT('Ctrl Pts',(-20.5511100440207,-33.0009443526879,
123.799699797302)) ;
#54187 = CARTESIAN_POINT('Ctrl Pts',(-20.836569622994,-32.8209552722074,123.896678841639)) ;
#54188 = CARTESIAN_POINT('Ctrl Pts',(-20.6011952592599,-33.0109340778964,
123.595752254043)) ;
#54189 = CARTESIAN_POINT('Ctrl Pts',(-20.8991776005845,-32.8309449974159,
123.641744550618)) ;
#54190 = CARTESIAN_POINT('Ctrl Pts',(-20.6149126949009,-33.0208918425979,
123.386861704438)) ;
#54191 = CARTESIAN_POINT('Ctrl Pts',(-20.9163259245573,-32.8409027621174,
123.380631029214)) ;
#54192 = CARTESIAN_POINT('Ctrl Pts',(-20.5927628252155,-33.0307941840099,
123.179858179155)) ;
#54193 = CARTESIAN_POINT('Ctrl Pts',(-20.8886398163687,-32.8508051035294,
123.121875613537)) ;
#54194 = CARTESIAN_POINT('Ctrl Pts',(-20.5341646522333,-33.0408383797163,
122.977001703688)) ;
#54195 = CARTESIAN_POINT('Ctrl Pts',(-20.81539343834,-32.8608492992358,122.868304834781)) ;
#54196 = CARTESIAN_POINT('Ctrl Pts',(-20.4425109806158,-33.0507457804755,
122.789954482795)) ;
#54197 = CARTESIAN_POINT('Ctrl Pts',(-20.700827186029,-32.870756699995,122.63449448841)) ;
#54198 = CARTESIAN_POINT('Ctrl Pts',(-20.3187974646894,-33.0607563803499,
122.619697924543)) ;
#54199 = CARTESIAN_POINT('Ctrl Pts',(-20.546186232137,-32.8807672998694,122.421673048436)) ;
#54200 = CARTESIAN_POINT('Ctrl Pts',(-20.1668178861132,-33.0707866762621,
122.473511957559)) ;
#54201 = CARTESIAN_POINT('Ctrl Pts',(-20.3562127677828,-32.8907975957816,
122.238939688334)) ;
#54202 = CARTESIAN_POINT('Ctrl Pts',(-19.9950035419231,-33.0806414559118,
122.357764747843)) ;
#54203 = CARTESIAN_POINT('Ctrl Pts',(-20.1414444852479,-32.9006523754313,
122.094253937415)) ;
#54204 = CARTESIAN_POINT('Ctrl Pts',(-19.8039737443084,-33.0905987841293,
122.272141541311)) ;
#54205 = CARTESIAN_POINT('Ctrl Pts',(-19.9026572209187,-32.9106097036488,
121.987223818312)) ;
#54206 = CARTESIAN_POINT('Ctrl Pts',(-19.5992424579009,-33.1006378170362,
122.220935616222)) ;
#54207 = CARTESIAN_POINT('Ctrl Pts',(-19.6467435512456,-32.9206487365557,
121.923215339334)) ;
#54208 = CARTESIAN_POINT('Ctrl Pts',(-19.3921897280463,-33.1105109289255,
122.205912912299)) ;
#54209 = CARTESIAN_POINT('Ctrl Pts',(-19.3879265897739,-32.930521848445,121.904435880023)) ;
#54210 = CARTESIAN_POINT('Ctrl Pts',(-19.1815696557166,-33.1205842139526,
122.227554268862)) ;
#54211 = CARTESIAN_POINT('Ctrl Pts',(-19.1246518187716,-32.9405951334721,
121.931486510067)) ;
#54212 = CARTESIAN_POINT('Ctrl Pts',(-18.9828627675349,-33.1304045336893,
122.283747306268)) ;
#54213 = CARTESIAN_POINT('Ctrl Pts',(-18.8762664626598,-32.9504154532089,
122.001727342334)) ;
#54214 = CARTESIAN_POINT('Ctrl Pts',(-18.7920430269983,-33.1404831990678,
122.37573379343)) ;
#54215 = CARTESIAN_POINT('Ctrl Pts',(-18.6377418414176,-32.9604941185873,
122.116709479796)) ;
#54216 = CARTESIAN_POINT('Ctrl Pts',(-18.6238449944928,-33.1503347895516,
122.496666905546)) ;
#54217 = CARTESIAN_POINT('Ctrl Pts',(-18.4274927505842,-32.9703457090711,
122.267875972223)) ;
#54218 = CARTESIAN_POINT('Ctrl Pts',(-18.4758763515475,-33.1604079398705,
122.648110975471)) ;
#54219 = CARTESIAN_POINT('Ctrl Pts',(-18.2425317132548,-32.98041885939,122.457180219299)) ;
#54220 = CARTESIAN_POINT('Ctrl Pts',(-18.3591783280429,-33.1702503198455,
122.8190052862)) ;
#54221 = CARTESIAN_POINT('Ctrl Pts',(-18.0966577528387,-32.9902612393651,
122.670798846568)) ;
#54222 = CARTESIAN_POINT('Ctrl Pts',(-18.2721117533038,-33.1802312960886,
123.009903540524)) ;
#54223 = CARTESIAN_POINT('Ctrl Pts',(-17.9878239541792,-33.0002422156081,
122.909421733985)) ;
#54224 = CARTESIAN_POINT('Ctrl Pts',(-18.2196648188066,-33.1902476244439,
123.213853808958)) ;
#54225 = CARTESIAN_POINT('Ctrl Pts',(-17.9222646670359,-33.0102585439634,
123.164359426885)) ;
#54226 = CARTESIAN_POINT('Ctrl Pts',(-18.2033572918697,-33.200145421435,123.421288579882)) ;
#54227 = CARTESIAN_POINT('Ctrl Pts',(-17.9018796511205,-33.0201563409545,
123.423653833824)) ;
#54228 = CARTESIAN_POINT('Ctrl Pts',(-18.223190034098,-33.2101579781671,123.630863236516)) ;
#54229 = CARTESIAN_POINT('Ctrl Pts',(-17.9266701884675,-33.0301688976866,
123.685622214874)) ;
#54230 = CARTESIAN_POINT('Ctrl Pts',(-18.2796939241535,-33.2201900130135,
123.834047999503)) ;
#54231 = CARTESIAN_POINT('Ctrl Pts',(-17.9972994487156,-33.0402009325331,
123.93960319975)) ;
#54232 = CARTESIAN_POINT('Ctrl Pts',(-18.3684191094839,-33.230029413829,124.020926505679)) ;
#54233 = CARTESIAN_POINT('Ctrl Pts',(-18.1082062114621,-33.0500403333485,
124.173202825663)) ;
#54234 = CARTESIAN_POINT('Ctrl Pts',(-18.4908474188606,-33.2400951994806,
124.193500366468)) ;
#54235 = CARTESIAN_POINT('Ctrl Pts',(-18.2612411135515,-33.0601061190001,
124.388920029592)) ;
#54236 = CARTESIAN_POINT('Ctrl Pts',(-18.6388594412923,-33.2499856545952,
124.339567692069)) ;
#54237 = CARTESIAN_POINT('Ctrl Pts',(-18.4462566310089,-33.0699965741147,
124.571505177055)) ;
#54238 = CARTESIAN_POINT('Ctrl Pts',(-18.8114608537052,-33.2599777732309,
124.459283778179)) ;
#54239 = CARTESIAN_POINT('Ctrl Pts',(-18.6620084680312,-33.0799886927505,
124.721150558887)) ;
#54240 = CARTESIAN_POINT('Ctrl Pts',(-19.0017546265229,-33.269940599994,124.546778303222)) ;
#54241 = CARTESIAN_POINT('Ctrl Pts',(-18.8998759882666,-33.0899515195135,
124.830519144868)) ;
#54242 = CARTESIAN_POINT('Ctrl Pts',(-19.2030467259017,-33.2798448832669,
124.600106280176)) ;
#54243 = CARTESIAN_POINT('Ctrl Pts',(-19.1514920072806,-33.0998558027864,
124.897179406919)) ;
#54244 = CARTESIAN_POINT('Ctrl Pts',(-19.4137849185456,-33.289905317214,124.617764888055)) ;
#54245 = CARTESIAN_POINT('Ctrl Pts',(-19.414914385357,-33.1099162367335,124.919252762314)) ;
#54246 = CARTESIAN_POINT('Ctrl Pts',(-19.6198604520968,-33.2997458698872,
124.599243558957)) ;
#54247 = CARTESIAN_POINT('Ctrl Pts',(-19.6725102686999,-33.1197567894067,
124.896100987935)) ;
#54248 = CARTESIAN_POINT('Ctrl Pts',(-19.8241111476887,-33.3098080898329,
124.544278855776)) ;
#54249 = CARTESIAN_POINT('Ctrl Pts',(-19.9278232585895,-33.1298190093524,
124.827395120553)) ;
#54250 = CARTESIAN_POINT('Ctrl Pts',(-20.0125096552998,-33.3197052291114,
124.455943774085)) ;
#54251 = CARTESIAN_POINT('Ctrl Pts',(-20.163322301102,-33.139716148631,124.716975844288)) ;
#54252 = CARTESIAN_POINT('Ctrl Pts',(-20.1836814999991,-33.3296364212465,
124.336404331942)) ;
#54253 = CARTESIAN_POINT('Ctrl Pts',(-20.3772875394294,-33.149647340766,124.567550900736)) ;
#54254 = CARTESIAN_POINT('Ctrl Pts',(-20.3329814659399,-33.3396785758916,
124.187146312258)) ;
#54255 = CARTESIAN_POINT('Ctrl Pts',(-20.5639122195022,-33.1596894954111,
124.380978397001)) ;
#54256 = CARTESIAN_POINT('Ctrl Pts',(-20.4523759830474,-33.3495653369109,
124.016987842125)) ;
#54257 = CARTESIAN_POINT('Ctrl Pts',(-20.7131557899143,-33.1695762564304,
124.168279265577)) ;
#54258 = CARTESIAN_POINT('Ctrl Pts',(-20.5416382969896,-33.3595646386281,
123.826694295305)) ;
#54259 = CARTESIAN_POINT('Ctrl Pts',(-20.8247334247518,-33.1795755581476,
123.930412036579)) ;
#54260 = CARTESIAN_POINT('Ctrl Pts',(-20.596223942968,-33.3694854367949,123.625368027277)) ;
#54261 = CARTESIAN_POINT('Ctrl Pts',(-20.8929652908593,-33.1894963563144,
123.678753341758)) ;
#54262 = CARTESIAN_POINT('Ctrl Pts',(-20.615255722677,-33.3795194903916,123.415304326235)) ;
#54263 = CARTESIAN_POINT('Ctrl Pts',(-20.9167545832082,-33.1995304099111,
123.416173818306)) ;
#54264 = CARTESIAN_POINT('Ctrl Pts',(-20.5978416091603,-33.389442607958,123.207385396435)) ;
#54265 = CARTESIAN_POINT('Ctrl Pts',(-20.8949864128072,-33.2094535274775,
123.156274431538)) ;
#54266 = CARTESIAN_POINT('Ctrl Pts',(-20.5438456870571,-33.3994987314571,
123.003007585044)) ;
#54267 = CARTESIAN_POINT('Ctrl Pts',(-20.827491153676,-33.2195096509766,122.90080257036)) ;
#54268 = CARTESIAN_POINT('Ctrl Pts',(-20.4571105200585,-33.4093441731119,
122.81506612472)) ;
#54269 = CARTESIAN_POINT('Ctrl Pts',(-20.7190711620445,-33.2293550926315,
122.665874666399)) ;
#54270 = CARTESIAN_POINT('Ctrl Pts',(-20.3382374891591,-33.4193064742361,
122.642647202006)) ;
#54271 = CARTESIAN_POINT('Ctrl Pts',(-20.5704789954929,-33.2393173937556,
122.450351068565)) ;
#54272 = CARTESIAN_POINT('Ctrl Pts',(-20.1900385777374,-33.4293349535112,
122.492672258745)) ;
#54273 = CARTESIAN_POINT('Ctrl Pts',(-20.3852299652996,-33.2493458730307,
122.262882911192)) ;
#54274 = CARTESIAN_POINT('Ctrl Pts',(-20.0201373732377,-33.4392453070209,
122.372100343306)) ;
#54275 = CARTESIAN_POINT('Ctrl Pts',(-20.1728523554748,-33.2592562265404,
122.11216805785)) ;
#54276 = CARTESIAN_POINT('Ctrl Pts',(-19.8316354394708,-33.4491801791981,
122.282138877027)) ;
#54277 = CARTESIAN_POINT('Ctrl Pts',(-19.9372239610113,-33.2691910987176,
121.999716737743)) ;
#54278 = CARTESIAN_POINT('Ctrl Pts',(-19.628183907834,-33.4592213167838,122.225869096708)) ;
#54279 = CARTESIAN_POINT('Ctrl Pts',(-19.6829095120336,-33.2792322363033,
121.929380340376)) ;
#54280 = CARTESIAN_POINT('Ctrl Pts',(-19.4212710659109,-33.4691084659983,
122.205941031249)) ;
#54281 = CARTESIAN_POINT('Ctrl Pts',(-19.4242673412654,-33.2891193855178,
121.904471017687)) ;
#54282 = CARTESIAN_POINT('Ctrl Pts',(-19.2118367929156,-33.4791007007494,
122.222063506245)) ;
#54283 = CARTESIAN_POINT('Ctrl Pts',(-19.162474373459,-33.2991116202689,121.924625119876)) ;
#54284 = CARTESIAN_POINT('Ctrl Pts',(-19.0092605385172,-33.4890494063124,
122.274143933396)) ;
#54285 = CARTESIAN_POINT('Ctrl Pts',(-18.9092537721428,-33.3090603258319,
121.989726729729)) ;
#54286 = CARTESIAN_POINT('Ctrl Pts',(-18.8189440039273,-33.4989854747361,
122.360209294255)) ;
#54287 = CARTESIAN_POINT('Ctrl Pts',(-18.6713579682493,-33.3189963942556,
122.097309682297)) ;
#54288 = CARTESIAN_POINT('Ctrl Pts',(-18.6454357357952,-33.5089711589519,
122.478422695815)) ;
#54289 = CARTESIAN_POINT('Ctrl Pts',(-18.4544730862203,-33.3289820784714,
122.245077547326)) ;
#54290 = CARTESIAN_POINT('Ctrl Pts',(-18.4945213063124,-33.5190115855205,
122.625987981149)) ;
#54291 = CARTESIAN_POINT('Ctrl Pts',(-18.2658309060889,-33.33902250504,122.429534786595)) ;
#54292 = CARTESIAN_POINT('Ctrl Pts',(-18.3736983247787,-33.5288506989843,
122.793886133219)) ;
#54293 = CARTESIAN_POINT('Ctrl Pts',(-18.1148023369346,-33.3488616185038,
122.639409270506)) ;
#54294 = CARTESIAN_POINT('Ctrl Pts',(-18.28169524401,-33.5388804331601,122.983614959474)) ;
#54295 = CARTESIAN_POINT('Ctrl Pts',(-17.9997997483841,-33.3588913526796,
122.876570796128)) ;
#54296 = CARTESIAN_POINT('Ctrl Pts',(-18.2246058172832,-33.548902532666,123.186427396069)) ;
#54297 = CARTESIAN_POINT('Ctrl Pts',(-17.9284390775416,-33.3689134521855,
123.130086625276)) ;
#54298 = CARTESIAN_POINT('Ctrl Pts',(-18.2034007562052,-33.5587709725594,
123.392821859869)) ;
#54299 = CARTESIAN_POINT('Ctrl Pts',(-17.9019339656912,-33.3787818920789,
123.388080969436)) ;
#54300 = CARTESIAN_POINT('Ctrl Pts',(-18.218661353348,-33.568839837245,123.603931402573)) ;
#54301 = CARTESIAN_POINT('Ctrl Pts',(-17.9210110193747,-33.3888507567645,
123.651967424945)) ;
#54302 = CARTESIAN_POINT('Ctrl Pts',(-18.2691838785988,-33.5786825103436,
123.804599750498)) ;
#54303 = CARTESIAN_POINT('Ctrl Pts',(-17.9841657908949,-33.3986934298632,
123.902803793716)) ;
#54304 = CARTESIAN_POINT('Ctrl Pts',(-18.3540908209291,-33.5886431445061,
123.996012857149)) ;
#54305 = CARTESIAN_POINT('Ctrl Pts',(-18.0903011026082,-33.4086540640256,
124.142069897889)) ;
#54306 = CARTESIAN_POINT('Ctrl Pts',(-18.472193287036,-33.5986810601842,124.170889366581)) ;
#54307 = CARTESIAN_POINT('Ctrl Pts',(-18.2379303216479,-33.4186919797037,
124.360664605596)) ;
#54308 = CARTESIAN_POINT('Ctrl Pts',(-18.6162214398664,-33.6085553350436,
124.320419679324)) ;
#54309 = CARTESIAN_POINT('Ctrl Pts',(-18.4179673637611,-33.4285662545632,
124.54757712207)) ;
#54310 = CARTESIAN_POINT('Ctrl Pts',(-18.787310591261,-33.6186250854188,124.445049310116)) ;
#54311 = CARTESIAN_POINT('Ctrl Pts',(-18.6318294559716,-33.4386360049383,
124.703362669326)) ;
#54312 = CARTESIAN_POINT('Ctrl Pts',(-18.9729667813463,-33.6284583807933,
124.536013927551)) ;
#54313 = CARTESIAN_POINT('Ctrl Pts',(-18.8639015605702,-33.4484693003128,
124.817067545996)) ;
#54314 = CARTESIAN_POINT('Ctrl Pts',(-19.1753880863516,-33.6384886782729,
124.595078783209)) ;
#54315 = CARTESIAN_POINT('Ctrl Pts',(-19.1169286180659,-33.4584995977924,
124.890896843037)) ;
#54316 = CARTESIAN_POINT('Ctrl Pts',(-19.385109828368,-33.6485207647143,124.61748724909)) ;
#54317 = CARTESIAN_POINT('Ctrl Pts',(-19.3790808832722,-33.4685316842339,
124.918905806976)) ;
#54318 = CARTESIAN_POINT('Ctrl Pts',(-19.5912662914409,-33.6583486932033,
124.603887833734)) ;
#54319 = CARTESIAN_POINT('Ctrl Pts',(-19.6367776217956,-33.4783596127228,
124.901904690763)) ;
#54320 = CARTESIAN_POINT('Ctrl Pts',(-19.7955034306806,-33.668344734314,124.554404004129)) ;
#54321 = CARTESIAN_POINT('Ctrl Pts',(-19.8920737335829,-33.4883556538336,
124.840047977271)) ;
#54322 = CARTESIAN_POINT('Ctrl Pts',(-19.9884633521273,-33.6783705464153,
124.469582265232)) ;
#54323 = CARTESIAN_POINT('Ctrl Pts',(-20.1332728673906,-33.4983814659348,
124.734019156347)) ;
#54324 = CARTESIAN_POINT('Ctrl Pts',(-20.1614882739156,-33.6882577813101,
124.354388322665)) ;
#54325 = CARTESIAN_POINT('Ctrl Pts',(-20.3495536622814,-33.5082687008296,
124.590024686067)) ;
#54326 = CARTESIAN_POINT('Ctrl Pts',(-20.3134732484457,-33.6982346475211,
124.209865201567)) ;
#54327 = CARTESIAN_POINT('Ctrl Pts',(-20.5395336849811,-33.5182455670407,
124.409369155067)) ;
#54328 = CARTESIAN_POINT('Ctrl Pts',(-20.4383121739259,-33.7082275913929,
124.040861571576)) ;
#54329 = CARTESIAN_POINT('Ctrl Pts',(-20.6955808168167,-33.5282385109124,
124.198113299949)) ;
#54330 = CARTESIAN_POINT('Ctrl Pts',(-20.5320713712117,-33.7182655140643,
123.851823217952)) ;
#54331 = CARTESIAN_POINT('Ctrl Pts',(-20.8127780413242,-33.5382764335838,
123.961814580509)) ;
#54332 = CARTESIAN_POINT('Ctrl Pts',(-20.5907682106731,-33.728113978326,123.653255911294)) ;
#54333 = CARTESIAN_POINT('Ctrl Pts',(-20.8861474400935,-33.5481248978455,
123.713603887081)) ;
#54334 = CARTESIAN_POINT('Ctrl Pts',(-20.6148023086895,-33.73810584507,123.444605714219)) ;
#54335 = CARTESIAN_POINT('Ctrl Pts',(-20.9161879633385,-33.5581167645895,
123.452790730193)) ;
#54336 = CARTESIAN_POINT('Ctrl Pts',(-20.6024505201895,-33.7480235771112,
123.236442898067)) ;
#54337 = CARTESIAN_POINT('Ctrl Pts',(-20.900746037756,-33.5680344966307,123.192586764759)) ;
#54338 = CARTESIAN_POINT('Ctrl Pts',(-20.5536692961249,-33.7580517620064,
123.031357793843)) ;
#54339 = CARTESIAN_POINT('Ctrl Pts',(-20.8397673982171,-33.578062681526,122.936230922727)) ;
#54340 = CARTESIAN_POINT('Ctrl Pts',(-20.4712833025613,-33.7679369200553,
122.840563071159)) ;
#54341 = CARTESIAN_POINT('Ctrl Pts',(-20.7367825954241,-33.5879478395748,
122.697737712705)) ;
#54342 = CARTESIAN_POINT('Ctrl Pts',(-20.3562437198245,-33.777926280597,122.664861804041)) ;
#54343 = CARTESIAN_POINT('Ctrl Pts',(-20.5929810835893,-33.5979372001165,
122.478112272329)) ;
#54344 = CARTESIAN_POINT('Ctrl Pts',(-20.2113763674384,-33.7879674375313,
122.511319512586)) ;
#54345 = CARTESIAN_POINT('Ctrl Pts',(-20.4118953448351,-33.6079783570509,
122.286185995833)) ;
#54346 = CARTESIAN_POINT('Ctrl Pts',(-20.0457742353741,-33.7978000209865,
122.38760905629)) ;
#54347 = CARTESIAN_POINT('Ctrl Pts',(-20.2048905332661,-33.617810940506,122.131549195)) ;
#54348 = CARTESIAN_POINT('Ctrl Pts',(-19.8584418259696,-33.8077942409485,
122.29246902554)) ;
#54349 = CARTESIAN_POINT('Ctrl Pts',(-19.9707238078469,-33.627805160468,122.012626278641)) ;
#54350 = CARTESIAN_POINT('Ctrl Pts',(-19.6566211003262,-33.8178223427358,
122.23150371137)) ;
#54351 = CARTESIAN_POINT('Ctrl Pts',(-19.7184472437474,-33.6378332622553,
121.936421881453)) ;
#54352 = CARTESIAN_POINT('Ctrl Pts',(-19.4504107987317,-33.8277022873588,
122.206582828826)) ;
#54353 = CARTESIAN_POINT('Ctrl Pts',(-19.460683413275,-33.6477132068784,121.905273090368)) ;
#54354 = CARTESIAN_POINT('Ctrl Pts',(-19.2406868639278,-33.8376926139159,
122.21764677824)) ;
#54355 = CARTESIAN_POINT('Ctrl Pts',(-19.1985284828869,-33.6577035334354,
121.919105510714)) ;
#54356 = CARTESIAN_POINT('Ctrl Pts',(-19.0370644043963,-33.8476335455702,
122.264726339862)) ;
#54357 = CARTESIAN_POINT('Ctrl Pts',(-18.9440006247054,-33.6676444650897,
121.97795745275)) ;
#54358 = CARTESIAN_POINT('Ctrl Pts',(-18.8436891463967,-33.8576206640731,
122.346553932478)) ;
#54359 = CARTESIAN_POINT('Ctrl Pts',(-18.7022824095767,-33.6776315835926,
122.08024433432)) ;
#54360 = CARTESIAN_POINT('Ctrl Pts',(-18.6668496652182,-33.8676539969703,
122.461506020677)) ;
#54361 = CARTESIAN_POINT('Ctrl Pts',(-18.4812344247497,-33.6876649164898,
122.223936502133)) ;
#54362 = CARTESIAN_POINT('Ctrl Pts',(-18.5149208707951,-33.877520101415,122.602747192623)) ;
#54363 = CARTESIAN_POINT('Ctrl Pts',(-18.2913247033585,-33.6975310209345,
122.400490262721)) ;
#54364 = CARTESIAN_POINT('Ctrl Pts',(-18.3872775083727,-33.8875862152953,
122.77150901783)) ;
#54365 = CARTESIAN_POINT('Ctrl Pts',(-18.1317726323046,-33.7075971348149,
122.611443968916)) ;
#54366 = CARTESIAN_POINT('Ctrl Pts',(-18.2928599718456,-33.8974422270637,
122.955967537504)) ;
#54367 = CARTESIAN_POINT('Ctrl Pts',(-18.0137527033652,-33.7174531465833,
122.842018843036)) ;
#54368 = CARTESIAN_POINT('Ctrl Pts',(-18.2304603251342,-33.9074369306951,
123.156602452202)) ;
#54369 = CARTESIAN_POINT('Ctrl Pts',(-17.9357556598601,-33.7274478502146,
123.092813373059)) ;
#54370 = CARTESIAN_POINT('Ctrl Pts',(-18.2041945369859,-33.9174682664199,
123.365854471469)) ;
#54371 = CARTESIAN_POINT('Ctrl Pts',(-17.9029259939187,-33.7374791859395,
123.354378720202)) ;
#54372 = CARTESIAN_POINT('Ctrl Pts',(-18.2141592542206,-33.9273347916236,
123.573047505969)) ;
#54373 = CARTESIAN_POINT('Ctrl Pts',(-17.9153845547752,-33.7473457111431,
123.613370405328)) ;
#54374 = CARTESIAN_POINT('Ctrl Pts',(-18.2601719129641,-33.9373222196694,
123.777885455416)) ;
#54375 = CARTESIAN_POINT('Ctrl Pts',(-17.9729030334191,-33.7573331391889,
123.869417371862)) ;
#54376 = CARTESIAN_POINT('Ctrl Pts',(-18.3406253597855,-33.9472671493558,
123.970893068674)) ;
#54377 = CARTESIAN_POINT('Ctrl Pts',(-18.0734724274163,-33.7672780688754,
124.110676065963)) ;
#54378 = CARTESIAN_POINT('Ctrl Pts',(-18.4545761365393,-33.9573120674643,
124.148662539094)) ;
#54379 = CARTESIAN_POINT('Ctrl Pts',(-18.2159131528349,-33.7773229869839,
124.332886434406)) ;
#54380 = CARTESIAN_POINT('Ctrl Pts',(-18.5949446142755,-33.9671740370782,
124.301270643735)) ;
#54381 = CARTESIAN_POINT('Ctrl Pts',(-18.3913760379142,-33.7871849565978,
124.52364504647)) ;
#54382 = CARTESIAN_POINT('Ctrl Pts',(-18.7615730312214,-33.9771661050995,
124.42915104515)) ;
#54383 = CARTESIAN_POINT('Ctrl Pts',(-18.5996633148228,-33.797177024619,124.683493416248)) ;
#54384 = CARTESIAN_POINT('Ctrl Pts',(-18.946781772386,-33.987097030474,124.525545967815)) ;
#54385 = CARTESIAN_POINT('Ctrl Pts',(-18.8311757133962,-33.8071079499936,
124.803984732283)) ;
#54386 = CARTESIAN_POINT('Ctrl Pts',(-19.1461772309718,-33.9970476586975,
124.588768735179)) ;
#54387 = CARTESIAN_POINT('Ctrl Pts',(-19.080421032467,-33.817058578217,124.883010582699)) ;
#54388 = CARTESIAN_POINT('Ctrl Pts',(-19.3545768509614,-34.0070478977566,
124.616672563708)) ;
#54389 = CARTESIAN_POINT('Ctrl Pts',(-19.3409209971834,-33.8270588172761,
124.917887618158)) ;
#54390 = CARTESIAN_POINT('Ctrl Pts',(-19.5652047456883,-34.0170763531258,
124.607640135001)) ;
#54391 = CARTESIAN_POINT('Ctrl Pts',(-19.6042058083347,-33.8370872726453,
124.906594291066)) ;
#54392 = CARTESIAN_POINT('Ctrl Pts',(-19.7678153879952,-34.026942387709,124.563211304919)) ;
#54393 = CARTESIAN_POINT('Ctrl Pts',(-19.8574687091983,-33.8469533072286,
124.851055548432)) ;
#54394 = CARTESIAN_POINT('Ctrl Pts',(-19.9621929863248,-34.0369347094565,
124.483598324612)) ;
#54395 = CARTESIAN_POINT('Ctrl Pts',(-20.1004399416366,-33.856945628976,124.751536397109)) ;
#54396 = CARTESIAN_POINT('Ctrl Pts',(-20.1387770996676,-34.0468669991335,
124.372126827251)) ;
#54397 = CARTESIAN_POINT('Ctrl Pts',(-20.3211678424855,-33.866877918653,124.61219566423)) ;
#54398 = CARTESIAN_POINT('Ctrl Pts',(-20.2945220917022,-34.0568686441042,
124.230877087231)) ;
#54399 = CARTESIAN_POINT('Ctrl Pts',(-20.5158504185811,-33.8768795636238,
124.435627300018)) ;
#54400 = CARTESIAN_POINT('Ctrl Pts',(-20.4659642035819,-34.0701812775203,
124.009619570015)) ;
#54401 = CARTESIAN_POINT('Ctrl Pts',(-20.7301343443236,-33.8901921970398,
124.159073181108)) ;
#54402 = CARTESIAN_POINT('Ctrl Pts',(-20.575254365758,-34.0834130269018,123.750361749611)) ;
#54403 = CARTESIAN_POINT('Ctrl Pts',(-20.8667466132401,-33.9034239464214,
123.835025634204)) ;
#54404 = CARTESIAN_POINT('Ctrl Pts',(-20.6136526413231,-34.0967362917189,
123.472950552117)) ;
#54405 = CARTESIAN_POINT('Ctrl Pts',(-20.9147529610491,-33.9167472112384,
123.488209575834)) ;
#54406 = CARTESIAN_POINT('Ctrl Pts',(-20.6062950710004,-34.1066119979366,
123.265445897535)) ;
#54407 = CARTESIAN_POINT('Ctrl Pts',(-20.9055507235774,-33.9266229174561,
123.228839180909)) ;
#54408 = CARTESIAN_POINT('Ctrl Pts',(-20.5627942065194,-34.1166015890366,
123.060012974967)) ;
#54409 = CARTESIAN_POINT('Ctrl Pts',(-20.8511725359358,-33.9366125085561,
122.972045792708)) ;
#54410 = CARTESIAN_POINT('Ctrl Pts',(-20.4848858375353,-34.126528685492,122.866373888595)) ;
#54411 = CARTESIAN_POINT('Ctrl Pts',(-20.7537843024981,-33.9465396050116,
122.72999873478)) ;
#54412 = CARTESIAN_POINT('Ctrl Pts',(-20.3734933893588,-34.1365538339966,
122.687478257524)) ;
#54413 = CARTESIAN_POINT('Ctrl Pts',(-20.6145413558421,-33.9565647535161,
122.506380398479)) ;
#54414 = CARTESIAN_POINT('Ctrl Pts',(-20.2346205228606,-34.1464494881433,
122.532553580072)) ;
#54415 = CARTESIAN_POINT('Ctrl Pts',(-20.4409482370739,-33.9664604076628,
122.312726536622)) ;
#54416 = CARTESIAN_POINT('Ctrl Pts',(-20.0693873756585,-34.1564530225215,
122.402484078199)) ;
#54417 = CARTESIAN_POINT('Ctrl Pts',(-20.2344050443968,-33.976463942041,122.150141790944)) ;
#54418 = CARTESIAN_POINT('Ctrl Pts',(-19.8843645713023,-34.1664381609615,
122.303256991677)) ;
#54419 = CARTESIAN_POINT('Ctrl Pts',(-20.0031251937535,-33.9864490804811,
122.026110363536)) ;
#54420 = CARTESIAN_POINT('Ctrl Pts',(-19.6838837822579,-34.1764740855569,
122.237544345005)) ;
#54421 = CARTESIAN_POINT('Ctrl Pts',(-19.7525232072663,-33.9964850050764,
121.94397216807)) ;
#54422 = CARTESIAN_POINT('Ctrl Pts',(-19.4789063239412,-34.1863253609846,
122.207945323593)) ;
#54423 = CARTESIAN_POINT('Ctrl Pts',(-19.4963012262231,-34.0063362805041,
121.906976170145)) ;
#54424 = CARTESIAN_POINT('Ctrl Pts',(-19.2689143031909,-34.1963176221459,
122.213879430628)) ;
#54425 = CARTESIAN_POINT('Ctrl Pts',(-19.2338112579513,-34.0163285416655,
121.914396519775)) ;
#54426 = CARTESIAN_POINT('Ctrl Pts',(-19.0622877357805,-34.2063575061635,
122.256906073786)) ;
#54427 = CARTESIAN_POINT('Ctrl Pts',(-18.9755284714105,-34.0263684256831,
121.968182550154)) ;
#54428 = CARTESIAN_POINT('Ctrl Pts',(-18.8700474354873,-34.216192280666,122.33308360955)) ;
#54429 = CARTESIAN_POINT('Ctrl Pts',(-18.7352293588114,-34.0362032001855,
122.063406917974)) ;
#54430 = CARTESIAN_POINT('Ctrl Pts',(-18.6896382083871,-34.2262686616863,
122.444048971715)) ;
#54431 = CARTESIAN_POINT('Ctrl Pts',(-18.5097194263312,-34.0462795812058,
122.202115742268)) ;
#54432 = CARTESIAN_POINT('Ctrl Pts',(-18.5347718576947,-34.2361149348369,
122.581438980249)) ;
#54433 = CARTESIAN_POINT('Ctrl Pts',(-18.3161370096554,-34.0561258543564,
122.373856170524)) ;
#54434 = CARTESIAN_POINT('Ctrl Pts',(-18.3597451156534,-34.2494794561221,
122.801234068625)) ;
#54435 = CARTESIAN_POINT('Ctrl Pts',(-18.0973641719139,-34.0694903756417,
122.648596301471)) ;
#54436 = CARTESIAN_POINT('Ctrl Pts',(-18.2477846712695,-34.2626857005566,
123.058779918869)) ;
#54437 = CARTESIAN_POINT('Ctrl Pts',(-17.9574233665507,-34.0826966200761,
122.970485787003)) ;
#54438 = CARTESIAN_POINT('Ctrl Pts',(-18.205709003732,-34.2759506552338,123.334400391849)) ;
#54439 = CARTESIAN_POINT('Ctrl Pts',(-17.9048166902023,-34.0959615747533,
123.315069758411)) ;
#54440 = CARTESIAN_POINT('Ctrl Pts',(-18.2106566690873,-34.2859829357855,
123.545267006591)) ;
#54441 = CARTESIAN_POINT('Ctrl Pts',(-17.9110068530417,-34.105993855305,123.578641444101)) ;
#54442 = CARTESIAN_POINT('Ctrl Pts',(-18.2516149367393,-34.2958916693034,
123.749507046798)) ;
#54443 = CARTESIAN_POINT('Ctrl Pts',(-17.9622064693986,-34.1159025888229,
123.833943903039)) ;
#54444 = CARTESIAN_POINT('Ctrl Pts',(-18.3271317964583,-34.3058292201709,
123.944308961896)) ;
#54445 = CARTESIAN_POINT('Ctrl Pts',(-18.0566040743328,-34.1258401396904,
124.07744363058)) ;
#54446 = CARTESIAN_POINT('Ctrl Pts',(-18.4364641233543,-34.3158590677648,
124.124581975054)) ;
#54447 = CARTESIAN_POINT('Ctrl Pts',(-18.1932746079544,-34.1358699872843,
124.302786499538)) ;
#54448 = CARTESIAN_POINT('Ctrl Pts',(-18.6196354097619,-34.3290942076852,
124.334139196948)) ;
#54449 = CARTESIAN_POINT('Ctrl Pts',(-18.4222258927744,-34.1491051272048,
124.564718290422)) ;
#54450 = CARTESIAN_POINT('Ctrl Pts',(-18.9138855860305,-34.3457626720564,
124.531468794228)) ;
#54451 = CARTESIAN_POINT('Ctrl Pts',(-18.7900532730175,-34.1657735915759,
124.811391879021)) ;
#54452 = CARTESIAN_POINT('Ctrl Pts',(-19.3240781905893,-34.3656336839303,
124.633306467972)) ;
#54453 = CARTESIAN_POINT('Ctrl Pts',(-19.3028100031517,-34.1856446034498,
124.938674735145)) ;
#54454 = CARTESIAN_POINT('Ctrl Pts',(-19.6773043637108,-34.3823407683133,
124.596000454904)) ;
#54455 = CARTESIAN_POINT('Ctrl Pts',(-19.7442781237966,-34.2023516878328,
124.892055705593)) ;
#54456 = CARTESIAN_POINT('Ctrl Pts',(-19.9358882444672,-34.3955180496239,
124.496604146033)) ;
#54457 = CARTESIAN_POINT('Ctrl Pts',(-20.0675644893515,-34.2155289691434,
124.767792583742)) ;
#54458 = CARTESIAN_POINT('Ctrl Pts',(-20.1754272741693,-34.408785510138,124.353698894968)) ;
#54459 = CARTESIAN_POINT('Ctrl Pts',(-20.3669683529045,-34.2287964296575,
124.589169379413)) ;
#54460 = CARTESIAN_POINT('Ctrl Pts',(-20.4216795722527,-34.4253994008252,
124.10043464984)) ;
#54461 = CARTESIAN_POINT('Ctrl Pts',(-20.6747925425545,-34.2454103203447,
124.272577564644)) ;
#54462 = CARTESIAN_POINT('Ctrl Pts',(-20.5958914665089,-34.4453482002526,
123.713647161789)) ;
#54463 = CARTESIAN_POINT('Ctrl Pts',(-20.8925501701662,-34.2653591197721,
123.789095141657)) ;
#54464 = CARTESIAN_POINT('Ctrl Pts',(-20.6275282466341,-34.4652693117834,
123.291312891227)) ;
#54465 = CARTESIAN_POINT('Ctrl Pts',(-20.9320934630028,-34.285280231303,123.26117694891)) ;
#54466 = CARTESIAN_POINT('Ctrl Pts',(-20.5142733747202,-34.4851357599563,
122.884295294386)) ;
#54467 = CARTESIAN_POINT('Ctrl Pts',(-20.7905220575369,-34.3051466794758,
122.75240729887)) ;
#54468 = CARTESIAN_POINT('Ctrl Pts',(-20.2668055992271,-34.5051621065734,
122.537830920578)) ;
#54469 = CARTESIAN_POINT('Ctrl Pts',(-20.4811847889919,-34.325173026093,122.319328242643)) ;
#54470 = CARTESIAN_POINT('Ctrl Pts',(-19.9186956223332,-34.525024150963,122.298589670166)) ;
#54471 = CARTESIAN_POINT('Ctrl Pts',(-20.0460469290827,-34.3450350704825,
122.020279911525)) ;
#54472 = CARTESIAN_POINT('Ctrl Pts',(-19.5084246289227,-34.5449694536441,
122.191442824304)) ;
#54473 = CARTESIAN_POINT('Ctrl Pts',(-19.5332082975816,-34.3649803731636,
121.886348768435)) ;
#54474 = CARTESIAN_POINT('Ctrl Pts',(-19.0872125174688,-34.564864760703,122.230706330331)) ;
#54475 = CARTESIAN_POINT('Ctrl Pts',(-19.0066946738637,-34.3848756802225,
121.935430157897)) ;
#54476 = CARTESIAN_POINT('Ctrl Pts',(-18.7043989473763,-34.5847580308706,
122.410642685401)) ;
#54477 = CARTESIAN_POINT('Ctrl Pts',(-18.5281796662199,-34.4047689503901,
122.160351280571)) ;
#54478 = CARTESIAN_POINT('Ctrl Pts',(-18.4049696018283,-34.604723623551,122.711540803692)) ;
#54479 = CARTESIAN_POINT('Ctrl Pts',(-18.1538942483531,-34.4247345430706,
122.536474463816)) ;
#54480 = CARTESIAN_POINT('Ctrl Pts',(-18.2267125295678,-34.6245989472359,
123.094736417654)) ;
#54481 = CARTESIAN_POINT('Ctrl Pts',(-17.9310744455895,-34.4446098667554,
123.015467619805)) ;
#54482 = CARTESIAN_POINT('Ctrl Pts',(-18.1893069394518,-34.6445740098108,
123.517829036567)) ;
#54483 = CARTESIAN_POINT('Ctrl Pts',(-17.8843177628342,-34.4645849293304,
123.544333074614)) ;
#54484 = CARTESIAN_POINT('Ctrl Pts',(-18.299019392422,-34.6645264194419,123.927638801905)) ;
#54485 = CARTESIAN_POINT('Ctrl Pts',(-18.0214586109173,-34.4845373389615,
124.05659443004)) ;
#54486 = CARTESIAN_POINT('Ctrl Pts',(-18.5399052285237,-34.684362473678,124.273849716243)) ;
#54487 = CARTESIAN_POINT('Ctrl Pts',(-18.3225640750526,-34.5043733931976,
124.489356119952)) ;
#54488 = CARTESIAN_POINT('Ctrl Pts',(-18.8866675177332,-34.7043403850956,
124.51920099619)) ;
#54489 = CARTESIAN_POINT('Ctrl Pts',(-18.7560161141913,-34.5243513046151,
124.79604584641)) ;
#54490 = CARTESIAN_POINT('Ctrl Pts',(-19.2952182234732,-34.7242584345991,
124.630665769838)) ;
#54491 = CARTESIAN_POINT('Ctrl Pts',(-19.2667030759053,-34.5442693541186,
124.935377333796)) ;
#54492 = CARTESIAN_POINT('Ctrl Pts',(-19.7164297540769,-34.7441265783672,
124.597207733981)) ;
#54493 = CARTESIAN_POINT('Ctrl Pts',(-19.793215907895,-34.5641374978867,124.893556756238)) ;
#54494 = CARTESIAN_POINT('Ctrl Pts',(-20.1040277686893,-34.7641774349545,
124.419895888455)) ;
#54495 = CARTESIAN_POINT('Ctrl Pts',(-20.2777146691707,-34.584188354474,124.671918199702)) ;
#54496 = CARTESIAN_POINT('Ctrl Pts',(-20.404229106633,-34.7839578714104,124.125155942307)) ;
#54497 = CARTESIAN_POINT('Ctrl Pts',(-20.652965881669,-34.6039687909299,124.303496686961)) ;
#54498 = CARTESIAN_POINT('Ctrl Pts',(-20.5886433658768,-34.8039879270882,
123.741366661607)) ;
#54499 = CARTESIAN_POINT('Ctrl Pts',(-20.8834863292564,-34.6239988466077,
123.823760909385)) ;
#54500 = CARTESIAN_POINT('Ctrl Pts',(-20.630003600706,-34.823869032263,123.320595871531)) ;
#54501 = CARTESIAN_POINT('Ctrl Pts',(-20.9351889707772,-34.6438799517825,
123.297798988616)) ;
#54502 = CARTESIAN_POINT('Ctrl Pts',(-20.5264818869687,-34.8437494946307,
122.91079906104)) ;
#54503 = CARTESIAN_POINT('Ctrl Pts',(-20.8057903345395,-34.6637604141503,
122.785553366813)) ;
#54504 = CARTESIAN_POINT('Ctrl Pts',(-20.2879555038815,-34.8637346417751,
122.55910414027)) ;
#54505 = CARTESIAN_POINT('Ctrl Pts',(-20.5076352221649,-34.6837455612946,
122.345932909906)) ;
#54506 = CARTESIAN_POINT('Ctrl Pts',(-19.9453039790159,-34.8836252203115,
122.311181550038)) ;
#54507 = CARTESIAN_POINT('Ctrl Pts',(-20.0793236956332,-34.703636139831,122.036027426937)) ;
#54508 = CARTESIAN_POINT('Ctrl Pts',(-19.5387683050646,-34.9035192401859,
122.194334979435)) ;
#54509 = CARTESIAN_POINT('Ctrl Pts',(-19.5711560383647,-34.7235301597054,
121.889965636104)) ;
#54510 = CARTESIAN_POINT('Ctrl Pts',(-19.1162346707492,-34.9234406849123,
122.223156044862)) ;
#54511 = CARTESIAN_POINT('Ctrl Pts',(-19.0429893283305,-34.7434516044318,
121.925987779697)) ;
#54512 = CARTESIAN_POINT('Ctrl Pts',(-18.7288788831415,-34.9433388229677,
122.393621819122)) ;
#54513 = CARTESIAN_POINT('Ctrl Pts',(-18.5587933442167,-34.7633497424872,
122.139065599235)) ;
#54514 = CARTESIAN_POINT('Ctrl Pts',(-18.4209986101695,-34.9634095781838,
122.68903279055)) ;
#54515 = CARTESIAN_POINT('Ctrl Pts',(-18.1739396122675,-34.7834204977033,
122.508326536784)) ;
#54516 = CARTESIAN_POINT('Ctrl Pts',(-18.2348330469421,-34.983195128235,123.066398593346)) ;
#54517 = CARTESIAN_POINT('Ctrl Pts',(-17.941229131582,-34.8032060477545,122.980030562327)) ;
#54518 = CARTESIAN_POINT('Ctrl Pts',(-18.1871490528402,-35.0031782031124,
123.488530219856)) ;
#54519 = CARTESIAN_POINT('Ctrl Pts',(-17.8816194220909,-34.8231891226319,
123.507694573203)) ;
#54520 = CARTESIAN_POINT('Ctrl Pts',(-18.2866725644005,-35.0230872857583,
123.899991070555)) ;
#54521 = CARTESIAN_POINT('Ctrl Pts',(-18.0060182321643,-34.8430982052778,
124.022021160938)) ;
#54522 = CARTESIAN_POINT('Ctrl Pts',(-18.5190486689243,-35.0429458448811,
124.252608438494)) ;
#54523 = CARTESIAN_POINT('Ctrl Pts',(-18.2964865244947,-34.8629567644006,
124.462795927105)) ;
#54524 = CARTESIAN_POINT('Ctrl Pts',(-18.8611531383577,-35.0629892887198,
124.506625814478)) ;
#54525 = CARTESIAN_POINT('Ctrl Pts',(-18.7241036773249,-34.8830002082393,
124.7803195884)) ;
#54526 = CARTESIAN_POINT('Ctrl Pts',(-19.1973105599933,-35.079489353449,124.60730897235)) ;
#54527 = CARTESIAN_POINT('Ctrl Pts',(-19.144331436189,-34.8995002729685,124.906184977658)) ;
#54528 = CARTESIAN_POINT('Ctrl Pts',(-19.4786570547526,-35.0928790932979,
124.615810466112)) ;
#54529 = CARTESIAN_POINT('Ctrl Pts',(-19.4959856145802,-34.9128900128174,
124.916808895359)) ;
#54530 = CARTESIAN_POINT('Ctrl Pts',(-19.6837596141147,-35.1027359945063,
124.58607447705)) ;
#54531 = CARTESIAN_POINT('Ctrl Pts',(-19.7523697501932,-34.9227469140258,
124.879642738746)) ;
#54532 = CARTESIAN_POINT('Ctrl Pts',(-19.8833526181919,-35.1127275203528,
124.520719105362)) ;
#54533 = CARTESIAN_POINT('Ctrl Pts',(-20.0018598352572,-34.9327384398723,
124.797951435971)) ;
#54534 = CARTESIAN_POINT('Ctrl Pts',(-20.0674176518561,-35.1226522008037,
124.422401605199)) ;
#54535 = CARTESIAN_POINT('Ctrl Pts',(-20.2319445662063,-34.9426631203233,
124.675054574964)) ;
#54536 = CARTESIAN_POINT('Ctrl Pts',(-20.2330436349176,-35.1326627908481,
124.292596619006)) ;
#54537 = CARTESIAN_POINT('Ctrl Pts',(-20.4389718039225,-34.9526737103677,
124.512809926757)) ;
#54538 = CARTESIAN_POINT('Ctrl Pts',(-20.4195165261857,-35.1459220515518,
124.085363429725)) ;
#54539 = CARTESIAN_POINT('Ctrl Pts',(-20.6720998992785,-34.9659329710713,
124.253723717985)) ;
#54540 = CARTESIAN_POINT('Ctrl Pts',(-20.5482036535186,-35.1592731267021,
123.832398852526)) ;
#54541 = CARTESIAN_POINT('Ctrl Pts',(-20.8329350807849,-34.9792840462216,
123.937545082325)) ;
#54542 = CARTESIAN_POINT('Ctrl Pts',(-20.6059607274363,-35.1724794359369,
123.560762637728)) ;
#54543 = CARTESIAN_POINT('Ctrl Pts',(-20.905132938759,-34.9924903554564,123.598017654273)) ;
#54544 = CARTESIAN_POINT('Ctrl Pts',(-20.6137261119894,-35.1824662695272,
123.350990307265)) ;
#54545 = CARTESIAN_POINT('Ctrl Pts',(-20.9148428909647,-35.0024771890467,
123.335798885084)) ;
#54546 = CARTESIAN_POINT('Ctrl Pts',(-20.5851416406984,-35.1924189970233,
123.143676946331)) ;
#54547 = CARTESIAN_POINT('Ctrl Pts',(-20.8791149642013,-35.0124299165428,
123.07665769436)) ;
#54548 = CARTESIAN_POINT('Ctrl Pts',(-20.5202297895318,-35.2024670938648,
122.942679277039)) ;
#54549 = CARTESIAN_POINT('Ctrl Pts',(-20.7979778137979,-35.0224780133844,
122.825409407631)) ;
#54550 = CARTESIAN_POINT('Ctrl Pts',(-20.4236321858874,-35.2123085507367,
122.75969231486)) ;
#54551 = CARTESIAN_POINT('Ctrl Pts',(-20.6772333063753,-35.0323194702562,
122.596674503309)) ;
#54552 = CARTESIAN_POINT('Ctrl Pts',(-20.2952501726806,-35.2222948176502,
122.593621170823)) ;
#54553 = CARTESIAN_POINT('Ctrl Pts',(-20.5167579762687,-35.0423057371697,
122.389083764368)) ;
#54554 = CARTESIAN_POINT('Ctrl Pts',(-20.1407744583381,-35.2322314185506,
122.45294261696)) ;
#54555 = CARTESIAN_POINT('Ctrl Pts',(-20.3236651758771,-35.0522423380701,
122.213233449122)) ;
#54556 = CARTESIAN_POINT('Ctrl Pts',(-19.9621957115618,-35.2422813613376,
122.340068651411)) ;
#54557 = CARTESIAN_POINT('Ctrl Pts',(-20.1004431976586,-35.0622922808572,
122.072138574531)) ;
#54558 = CARTESIAN_POINT('Ctrl Pts',(-19.77064229135,-35.2521315610234,122.261352205955)) ;
#54559 = CARTESIAN_POINT('Ctrl Pts',(-19.86100238911,-35.0721424805429,121.973740369695)) ;
#54560 = CARTESIAN_POINT('Ctrl Pts',(-19.5659662743928,-35.2621044659555,
122.216007869496)) ;
#54561 = CARTESIAN_POINT('Ctrl Pts',(-19.605157861446,-35.082115385475,121.917057182898)) ;
#54562 = CARTESIAN_POINT('Ctrl Pts',(-19.3559388586588,-35.2721028404351,
122.20693299255)) ;
#54563 = CARTESIAN_POINT('Ctrl Pts',(-19.342623637523,-35.0921137599546,121.90571078375)) ;
#54564 = CARTESIAN_POINT('Ctrl Pts',(-19.1471235458461,-35.2821230143051,
122.234669898377)) ;
#54565 = CARTESIAN_POINT('Ctrl Pts',(-19.081604071815,-35.1021339338246,121.940379135676)) ;
#54566 = CARTESIAN_POINT('Ctrl Pts',(-18.9486182041443,-35.2920240582471,
122.297318677213)) ;
#54567 = CARTESIAN_POINT('Ctrl Pts',(-18.8334713867569,-35.1120349777666,
122.018687487652)) ;
#54568 = CARTESIAN_POINT('Ctrl Pts',(-18.7622230203345,-35.3020128619714,
122.394038689284)) ;
#54569 = CARTESIAN_POINT('Ctrl Pts',(-18.6004760332833,-35.1220237814909,
122.139585076105)) ;
#54570 = CARTESIAN_POINT('Ctrl Pts',(-18.5959401033665,-35.3119783288032,
122.521468994438)) ;
#54571 = CARTESIAN_POINT('Ctrl Pts',(-18.3926205881844,-35.1319892483227,
122.298870810869)) ;
#54572 = CARTESIAN_POINT('Ctrl Pts',(-18.4547977142894,-35.3218818910762,
122.674558023421)) ;
#54573 = CARTESIAN_POINT('Ctrl Pts',(-18.2161904039979,-35.1418928105957,
122.490230413614)) ;
#54574 = CARTESIAN_POINT('Ctrl Pts',(-18.3407694318747,-35.3319425689542,
122.852663128969)) ;
#54575 = CARTESIAN_POINT('Ctrl Pts',(-18.0736527310918,-35.1519534884737,
122.712860272197)) ;
#54576 = CARTESIAN_POINT('Ctrl Pts',(-18.2609128534862,-35.3417828669036,
123.043535459525)) ;
#54577 = CARTESIAN_POINT('Ctrl Pts',(-17.9738293170937,-35.1617937864232,
122.951450001356)) ;
#54578 = CARTESIAN_POINT('Ctrl Pts',(-18.2141440011338,-35.3518458618131,
123.24982878148)) ;
#54579 = CARTESIAN_POINT('Ctrl Pts',(-17.9153656041691,-35.1718567813326,
123.209316008957)) ;
#54580 = CARTESIAN_POINT('Ctrl Pts',(-18.2042462712093,-35.3617401559602,
123.457624789983)) ;
#54581 = CARTESIAN_POINT('Ctrl Pts',(-17.9029906879273,-35.1817510754797,
123.469061216254)) ;
#54582 = CARTESIAN_POINT('Ctrl Pts',(-18.2301365974252,-35.3716819536571,
123.66499700929)) ;
#54583 = CARTESIAN_POINT('Ctrl Pts',(-17.9353509722978,-35.1916928731766,
123.728277083057)) ;
#54584 = CARTESIAN_POINT('Ctrl Pts',(-18.2919583226803,-35.3816845311862,
123.866019002124)) ;
#54585 = CARTESIAN_POINT('Ctrl Pts',(-18.012625610303,-35.2016954507057,123.979555436283)) ;
#54586 = CARTESIAN_POINT('Ctrl Pts',(-18.38832214789,-35.3917189951073,124.053667683726)) ;
#54587 = CARTESIAN_POINT('Ctrl Pts',(-18.1330779755077,-35.2117299146268,
124.214117512358)) ;
#54588 = CARTESIAN_POINT('Ctrl Pts',(-18.5131632869251,-35.4015651336283,
124.218788839764)) ;
#54589 = CARTESIAN_POINT('Ctrl Pts',(-18.2891276128659,-35.2215760531479,
124.420521008523)) ;
#54590 = CARTESIAN_POINT('Ctrl Pts',(-18.6665221671683,-35.4115463068653,
124.361984621255)) ;
#54591 = CARTESIAN_POINT('Ctrl Pts',(-18.480824570798,-35.2315572263849,124.599517750325)) ;
#54592 = CARTESIAN_POINT('Ctrl Pts',(-18.8419525073359,-35.4214986008226,
124.476017082833)) ;
#54593 = CARTESIAN_POINT('Ctrl Pts',(-18.7001113065776,-35.2415095203421,
124.74206065123)) ;
#54594 = CARTESIAN_POINT('Ctrl Pts',(-19.0353199148675,-35.4314973959572,
124.558494549662)) ;
#54595 = CARTESIAN_POINT('Ctrl Pts',(-18.9418196621868,-35.2515083154767,
124.845159871899)) ;
#54596 = CARTESIAN_POINT('Ctrl Pts',(-19.2409602408548,-35.441536504218,124.605934758552)) ;
#54597 = CARTESIAN_POINT('Ctrl Pts',(-19.1988694219931,-35.2615474237375,
124.904462677019)) ;
#54598 = CARTESIAN_POINT('Ctrl Pts',(-19.4472187958602,-35.4513614456571,
124.617157941758)) ;
#54599 = CARTESIAN_POINT('Ctrl Pts',(-19.4566932433176,-35.2713723651767,
124.918494235353)) ;
#54600 = CARTESIAN_POINT('Ctrl Pts',(-19.6571046505334,-35.4614161327315,
124.59216665789)) ;
#54601 = CARTESIAN_POINT('Ctrl Pts',(-19.7190507496458,-35.2814270522511,
124.887257605478)) ;
#54602 = CARTESIAN_POINT('Ctrl Pts',(-19.8571259179256,-35.4713589376717,
124.531443581548)) ;
#54603 = CARTESIAN_POINT('Ctrl Pts',(-19.9690783925862,-35.2913698571912,
124.81135610388)) ;
#54604 = CARTESIAN_POINT('Ctrl Pts',(-20.0431203480413,-35.4812627236682,
124.437854636446)) ;
#54605 = CARTESIAN_POINT('Ctrl Pts',(-20.2015729913914,-35.3012736431877,
124.69437184444)) ;
#54606 = CARTESIAN_POINT('Ctrl Pts',(-20.2123551288087,-35.491309540233,124.31150595345)) ;
#54607 = CARTESIAN_POINT('Ctrl Pts',(-20.4131178491441,-35.3113204597525,
124.536438012433)) ;
#54608 = CARTESIAN_POINT('Ctrl Pts',(-20.355073515676,-35.5012050597117,124.160099178899)) ;
#54609 = CARTESIAN_POINT('Ctrl Pts',(-20.591517979772,-35.3212159792312,124.347180770875)) ;
#54610 = CARTESIAN_POINT('Ctrl Pts',(-20.471223424041,-35.5112671450361,123.983338753384)) ;
#54611 = CARTESIAN_POINT('Ctrl Pts',(-20.7367072780887,-35.3312780645556,
124.126231712347)) ;
#54612 = CARTESIAN_POINT('Ctrl Pts',(-20.5532221554608,-35.521109855994,123.793329340615)) ;
#54613 = CARTESIAN_POINT('Ctrl Pts',(-20.8392082179323,-35.3411207755136,
123.888720097038)) ;
#54614 = CARTESIAN_POINT('Ctrl Pts',(-20.6021745079103,-35.5311005733001,
123.589104323875)) ;
#54615 = CARTESIAN_POINT('Ctrl Pts',(-20.9004009018937,-35.3511114928196,
123.633439183878)) ;
#54616 = CARTESIAN_POINT('Ctrl Pts',(-20.6148094254628,-35.5410286563966,
123.380757851225)) ;
#54617 = CARTESIAN_POINT('Ctrl Pts',(-20.9161968440808,-35.3610395759162,
123.373005745106)) ;
#54618 = CARTESIAN_POINT('Ctrl Pts',(-20.5912974926631,-35.5510165865084,
123.172091972982)) ;
#54619 = CARTESIAN_POINT('Ctrl Pts',(-20.8868090727188,-35.3710275060279,
123.112172972214)) ;
#54620 = CARTESIAN_POINT('Ctrl Pts',(-20.5312904374153,-35.5610524126357,
122.969827521401)) ;
#54621 = CARTESIAN_POINT('Ctrl Pts',(-20.811802454658,-35.3810633321552,122.859341843746)) ;
#54622 = CARTESIAN_POINT('Ctrl Pts',(-20.4390581243751,-35.5709077497493,
122.78428606231)) ;
#54623 = CARTESIAN_POINT('Ctrl Pts',(-20.6965136131226,-35.3909186692688,
122.627413231222)) ;
#54624 = CARTESIAN_POINT('Ctrl Pts',(-20.3145205708958,-35.5809054845995,
122.614998952204)) ;
#54625 = CARTESIAN_POINT('Ctrl Pts',(-20.5408432693508,-35.400916404119,122.415802978902)) ;
#54626 = CARTESIAN_POINT('Ctrl Pts',(-20.1638726572033,-35.5908133885839,
122.471137864884)) ;
#54627 = CARTESIAN_POINT('Ctrl Pts',(-20.3525343321425,-35.4108243081035,
122.235974665486)) ;
#54628 = CARTESIAN_POINT('Ctrl Pts',(-19.9889273945464,-35.6008244631324,
122.354124867634)) ;
#54629 = CARTESIAN_POINT('Ctrl Pts',(-20.1338538120552,-35.4208353826519,
122.089706748465)) ;
#54630 = CARTESIAN_POINT('Ctrl Pts',(-19.7958300056756,-35.610852318668,122.269519731036)) ;
#54631 = CARTESIAN_POINT('Ctrl Pts',(-19.8924829762107,-35.4308632381875,
121.983948431032)) ;
#54632 = CARTESIAN_POINT('Ctrl Pts',(-19.5945466869052,-35.6207099125732,
122.220212795873)) ;
#54633 = CARTESIAN_POINT('Ctrl Pts',(-19.6408783355384,-35.4407208320928,
121.922312589221)) ;
#54634 = CARTESIAN_POINT('Ctrl Pts',(-19.3842341645356,-35.6307365994113,
122.205941341897)) ;
#54635 = CARTESIAN_POINT('Ctrl Pts',(-19.3779878358336,-35.4507475189309,
121.904471410675)) ;
#54636 = CARTESIAN_POINT('Ctrl Pts',(-19.1746497432009,-35.6407652685651,
122.228931469731)) ;
#54637 = CARTESIAN_POINT('Ctrl Pts',(-19.1160071597397,-35.4607761880846,
121.933207053127)) ;
#54638 = CARTESIAN_POINT('Ctrl Pts',(-18.9758531060999,-35.6506104768465,
122.286508207348)) ;
#54639 = CARTESIAN_POINT('Ctrl Pts',(-18.8675097602176,-35.470621396366,122.005176454094)) ;
#54640 = CARTESIAN_POINT('Ctrl Pts',(-18.78706524933,-35.6606011658096,122.378575193346)) ;
#54641 = CARTESIAN_POINT('Ctrl Pts',(-18.6315240045379,-35.4806120853291,
122.120258716074)) ;
#54642 = CARTESIAN_POINT('Ctrl Pts',(-18.6166109529874,-35.6706390420919,
122.502982907208)) ;
#54643 = CARTESIAN_POINT('Ctrl Pts',(-18.4184551335349,-35.4906499616114,
122.275766762395)) ;
#54644 = CARTESIAN_POINT('Ctrl Pts',(-18.4728999980008,-35.6804834197341,
122.651921164381)) ;
#54645 = CARTESIAN_POINT('Ctrl Pts',(-18.2388143579608,-35.5004943392536,
122.461939201164)) ;
#54646 = CARTESIAN_POINT('Ctrl Pts',(-18.3552581448824,-35.6904682241255,
122.825736375078)) ;
#54647 = CARTESIAN_POINT('Ctrl Pts',(-18.0917605508585,-35.5104791436451,
122.679207506843)) ;
#54648 = CARTESIAN_POINT('Ctrl Pts',(-18.2698663052676,-35.7004077543441,
123.016483700906)) ;
#54649 = CARTESIAN_POINT('Ctrl Pts',(-17.9850190704585,-35.5204186738636,
122.917641507228)) ;
#54650 = CARTESIAN_POINT('Ctrl Pts',(-18.218436347525,-35.710447442381,123.221171010836)) ;
#54651 = CARTESIAN_POINT('Ctrl Pts',(-17.9207300901003,-35.5304583619005,
123.173500108582)) ;
#54652 = CARTESIAN_POINT('Ctrl Pts',(-18.2034516389984,-35.7203357317493,
123.428524856059)) ;
#54653 = CARTESIAN_POINT('Ctrl Pts',(-17.9019975598686,-35.5403466512688,
123.432693219793)) ;
#54654 = CARTESIAN_POINT('Ctrl Pts',(-18.2245179381264,-35.7303248554341,
123.637461026191)) ;
#54655 = CARTESIAN_POINT('Ctrl Pts',(-17.9283290132215,-35.5503357749536,
123.693863790516)) ;
#54656 = CARTESIAN_POINT('Ctrl Pts',(-18.281534545644,-35.7402848651087,123.838935805631)) ;
#54657 = CARTESIAN_POINT('Ctrl Pts',(-17.9995984431471,-35.5602957846282,
123.945708092145)) ;
#54658 = CARTESIAN_POINT('Ctrl Pts',(-18.3716800461657,-35.7501852948129,
124.026546743199)) ;
#54659 = CARTESIAN_POINT('Ctrl Pts',(-18.1122794987908,-35.5701962143325,
124.180223126185)) ;
#54660 = CARTESIAN_POINT('Ctrl Pts',(-18.4947794817171,-35.7602283762197,
124.198074355247)) ;
#54661 = CARTESIAN_POINT('Ctrl Pts',(-18.2661525938325,-35.5802392957392,
124.394633262603)) ;
#54662 = CARTESIAN_POINT('Ctrl Pts',(-18.6437627494517,-35.7701357701273,
124.343645611898)) ;
#54663 = CARTESIAN_POINT('Ctrl Pts',(-18.4523813315997,-35.5901466896469,
124.576598857815)) ;
#54664 = CARTESIAN_POINT('Ctrl Pts',(-18.8173428519059,-35.7801475011165,
124.462690565596)) ;
#54665 = CARTESIAN_POINT('Ctrl Pts',(-18.6693558213399,-35.600158420636,124.725406064514)) ;
#54666 = CARTESIAN_POINT('Ctrl Pts',(-19.0095259153143,-35.7901797188313,
124.549587699707)) ;
#54667 = CARTESIAN_POINT('Ctrl Pts',(-18.9095840015123,-35.6101906383508,
124.834028669411)) ;
#54668 = CARTESIAN_POINT('Ctrl Pts',(-19.2101294613733,-35.8000322280774,
124.601126477445)) ;
#54669 = CARTESIAN_POINT('Ctrl Pts',(-19.1603393482341,-35.620043147597,124.898453661871)) ;
#54670 = CARTESIAN_POINT('Ctrl Pts',(-19.4188119264436,-35.8099901646204,
124.617871878663)) ;
#54671 = CARTESIAN_POINT('Ctrl Pts',(-19.4211928177101,-35.63000108414,124.91938645452)) ;
#54672 = CARTESIAN_POINT('Ctrl Pts',(-19.6288700822666,-35.8200290346287,
124.59759241421)) ;
#54673 = CARTESIAN_POINT('Ctrl Pts',(-19.6837654584886,-35.6400399541482,
124.894038281402)) ;
#54674 = CARTESIAN_POINT('Ctrl Pts',(-19.8290080686716,-35.829902189787,124.542441752005)) ;
#54675 = CARTESIAN_POINT('Ctrl Pts',(-19.933939291435,-35.6499131093065,124.825100619604)) ;
#54676 = CARTESIAN_POINT('Ctrl Pts',(-20.0202339068438,-35.8399754646367,
124.45154743179)) ;
#54677 = CARTESIAN_POINT('Ctrl Pts',(-20.1729716448793,-35.6599863841562,
124.711483830442)) ;
#54678 = CARTESIAN_POINT('Ctrl Pts',(-20.1886685597443,-35.8497957818141,
124.332082596939)) ;
#54679 = CARTESIAN_POINT('Ctrl Pts',(-20.3835167616475,-35.6698067013336,
124.562152640152)) ;
#54680 = CARTESIAN_POINT('Ctrl Pts',(-20.3376896490082,-35.8598744676076,
124.181528608811)) ;
#54681 = CARTESIAN_POINT('Ctrl Pts',(-20.5697933971552,-35.6798853871271,
124.373961088732)) ;
#54682 = CARTESIAN_POINT('Ctrl Pts',(-20.455705088691,-35.8697259789907,124.011272096574)) ;
#54683 = CARTESIAN_POINT('Ctrl Pts',(-20.7173141231935,-35.6897368985102,
124.161139832875)) ;
#54684 = CARTESIAN_POINT('Ctrl Pts',(-20.5444435166218,-35.8797994252973,
123.81902845343)) ;
#54685 = CARTESIAN_POINT('Ctrl Pts',(-20.8282376599489,-35.6998103448168,
123.920835993623)) ;
#54686 = CARTESIAN_POINT('Ctrl Pts',(-20.5972105460148,-35.889640700422,123.618952464279)) ;
#54687 = CARTESIAN_POINT('Ctrl Pts',(-20.8941975464092,-35.7096516199415,
123.670739828083)) ;
#54688 = CARTESIAN_POINT('Ctrl Pts',(-20.6153373392273,-35.8996258000788,
123.409838328814)) ;
#54689 = CARTESIAN_POINT('Ctrl Pts',(-20.9168565668158,-35.7196367195983,
123.409346913404)) ;
#54690 = CARTESIAN_POINT('Ctrl Pts',(-20.5965431076934,-35.9096332762131,
123.200274922463)) ;
#54691 = CARTESIAN_POINT('Ctrl Pts',(-20.8933643887222,-35.7296441957326,
123.147392528931)) ;
#54692 = CARTESIAN_POINT('Ctrl Pts',(-20.5423042520483,-35.919555863922,122.998856521941)) ;
#54693 = CARTESIAN_POINT('Ctrl Pts',(-20.8255661489224,-35.7395667834416,
122.895618637202)) ;
#54694 = CARTESIAN_POINT('Ctrl Pts',(-20.453642398187,-35.9295424681954,122.808524797024)) ;
#54695 = CARTESIAN_POINT('Ctrl Pts',(-20.7147391060273,-35.7495533877149,
122.657703592471)) ;
#54696 = CARTESIAN_POINT('Ctrl Pts',(-20.3323311287311,-35.9395825965295,
122.635813523666)) ;
#54697 = CARTESIAN_POINT('Ctrl Pts',(-20.5631005959352,-35.759593516049,122.441814323604)) ;
#54698 = CARTESIAN_POINT('Ctrl Pts',(-20.1861543358301,-35.9494220310629,
122.48942292078)) ;
#54699 = CARTESIAN_POINT('Ctrl Pts',(-20.3803788348249,-35.7694329505824,
122.258824742426)) ;
#54700 = CARTESIAN_POINT('Ctrl Pts',(-20.0130523083208,-35.9594860855539,
122.367808286558)) ;
#54701 = CARTESIAN_POINT('Ctrl Pts',(-20.1640017995225,-35.7794970050734,
122.106806406587)) ;
#54702 = CARTESIAN_POINT('Ctrl Pts',(-19.8246772259409,-35.969377004791,122.279705165194)) ;
#54703 = CARTESIAN_POINT('Ctrl Pts',(-19.9285321534077,-35.7893879243106,
121.996676734267)) ;
#54704 = CARTESIAN_POINT('Ctrl Pts',(-19.6219619525249,-35.9793689980971,
122.224671937856)) ;
#54705 = CARTESIAN_POINT('Ctrl Pts',(-19.6751379025847,-35.7993799176166,
121.92788496596)) ;
#54706 = CARTESIAN_POINT('Ctrl Pts',(-19.4133577856184,-35.9893318620564,
122.205921690186)) ;
#54707 = CARTESIAN_POINT('Ctrl Pts',(-19.4143822634364,-35.8093427815759,
121.904446853198)) ;
#54708 = CARTESIAN_POINT('Ctrl Pts',(-19.2058271684787,-35.9992361218741,
122.223048719964)) ;
#54709 = CARTESIAN_POINT('Ctrl Pts',(-19.1549680514659,-35.8192470413937,
121.925855666003)) ;
#54710 = CARTESIAN_POINT('Ctrl Pts',(-19.0013346182317,-36.0092966124456,
122.276950648324)) ;
#54711 = CARTESIAN_POINT('Ctrl Pts',(-18.899352673556,-35.8293075319651,121.993232864525)) ;
#54712 = CARTESIAN_POINT('Ctrl Pts',(-18.8133472495276,-36.0191369620766,
122.363379425987)) ;
#54713 = CARTESIAN_POINT('Ctrl Pts',(-18.664367118394,-35.8391478815961,122.101269435699)) ;
#54714 = CARTESIAN_POINT('Ctrl Pts',(-18.639274963066,-36.0291999375666,122.483558189516)) ;
#54715 = CARTESIAN_POINT('Ctrl Pts',(-18.4467771152488,-35.8492108570861,
122.251492745577)) ;
#54716 = CARTESIAN_POINT('Ctrl Pts',(-18.4913225975558,-36.03909425771,122.629802380059)) ;
#54717 = CARTESIAN_POINT('Ctrl Pts',(-18.2618359405732,-35.8591051772295,
122.434298711793)) ;
#54718 = CARTESIAN_POINT('Ctrl Pts',(-18.3700032350797,-36.0490359708416,
122.799959594122)) ;
#54719 = CARTESIAN_POINT('Ctrl Pts',(-18.1101865599637,-35.8690468903611,
122.646995886901)) ;
#54720 = CARTESIAN_POINT('Ctrl Pts',(-18.2794097534421,-36.0590388606357,
122.98977331008)) ;
#54721 = CARTESIAN_POINT('Ctrl Pts',(-17.9969449045447,-35.8790497801552,
122.884263259447)) ;
#54722 = CARTESIAN_POINT('Ctrl Pts',(-18.2233291545152,-36.0690787177962,
123.193235333935)) ;
#54723 = CARTESIAN_POINT('Ctrl Pts',(-17.9268443212934,-35.8890896373157,
123.138590645368)) ;
#54724 = CARTESIAN_POINT('Ctrl Pts',(-18.2033834024276,-36.0789028986338,
123.39882135021)) ;
#54725 = CARTESIAN_POINT('Ctrl Pts',(-17.9019122827158,-35.8989138181533,
123.39557478234)) ;
#54726 = CARTESIAN_POINT('Ctrl Pts',(-18.2195239600936,-36.088959872137,123.609616533739)) ;
#54727 = CARTESIAN_POINT('Ctrl Pts',(-17.9220883776684,-35.9089707916565,
123.659068393651)) ;
#54728 = CARTESIAN_POINT('Ctrl Pts',(-18.271611751821,-36.0988879963241,123.811744957845)) ;
#54729 = CARTESIAN_POINT('Ctrl Pts',(-17.9871986047235,-35.9188989158436,
123.911729558155)) ;
#54730 = CARTESIAN_POINT('Ctrl Pts',(-18.3577130799816,-36.1088416913975,
124.002470019801)) ;
#54731 = CARTESIAN_POINT('Ctrl Pts',(-18.0948259749401,-35.928852610917,124.150136156894)) ;
#54732 = CARTESIAN_POINT('Ctrl Pts',(-18.4769655018994,-36.1188878849728,
124.176781923495)) ;
#54733 = CARTESIAN_POINT('Ctrl Pts',(-18.2438917114054,-35.9388988044923,
124.36802560012)) ;
#54734 = CARTESIAN_POINT('Ctrl Pts',(-18.6216180385642,-36.1287359873327,
124.324902759185)) ;
#54735 = CARTESIAN_POINT('Ctrl Pts',(-18.4247087144062,-35.9487469068522,
124.553177298517)) ;
#54736 = CARTESIAN_POINT('Ctrl Pts',(-18.7913448950173,-36.1386975755603,
124.447570338406)) ;
#54737 = CARTESIAN_POINT('Ctrl Pts',(-18.6368680942363,-35.9587084950798,
124.706511430825)) ;
#54738 = CARTESIAN_POINT('Ctrl Pts',(-18.9811968842923,-36.1487262457165,
124.539290730649)) ;
#54739 = CARTESIAN_POINT('Ctrl Pts',(-18.8741832744098,-35.9687371652361,
124.821161297462)) ;
#54740 = CARTESIAN_POINT('Ctrl Pts',(-19.181656131435,-36.1586365485983,124.596034870755)) ;
#54741 = CARTESIAN_POINT('Ctrl Pts',(-19.1247583601736,-35.9786474681178,
124.892091064712)) ;
#54742 = CARTESIAN_POINT('Ctrl Pts',(-19.3893970231701,-36.1685714324062,
124.617709477038)) ;
#54743 = CARTESIAN_POINT('Ctrl Pts',(-19.3844352240791,-35.9885823519257,
124.919183512204)) ;
#54744 = CARTESIAN_POINT('Ctrl Pts',(-19.5999475350248,-36.1786125740968,
124.602631344921)) ;
#54745 = CARTESIAN_POINT('Ctrl Pts',(-19.6476231191819,-35.9986234936163,
124.90033505526)) ;
#54746 = CARTESIAN_POINT('Ctrl Pts',(-19.801594360988,-36.1884996952608,124.552149971975)) ;
#54747 = CARTESIAN_POINT('Ctrl Pts',(-19.8996824513604,-36.0085106147803,
124.837232249488)) ;
#54748 = CARTESIAN_POINT('Ctrl Pts',(-19.9935521891846,-36.1984920381093,
124.466851568675)) ;
#54749 = CARTESIAN_POINT('Ctrl Pts',(-20.1396295183763,-36.0185029576288,
124.730608252314)) ;
#54750 = CARTESIAN_POINT('Ctrl Pts',(-20.1670027855748,-36.2084403393333,
124.34997292154)) ;
#54751 = CARTESIAN_POINT('Ctrl Pts',(-20.3564426704474,-36.0284512588528,
124.584508836264)) ;
#54752 = CARTESIAN_POINT('Ctrl Pts',(-20.317556983034,-36.2183779170154,124.205144373366)) ;
#54753 = CARTESIAN_POINT('Ctrl Pts',(-20.5446351271139,-36.0383888365349,
124.403471920544)) ;
#54754 = CARTESIAN_POINT('Ctrl Pts',(-20.4414732897196,-36.228364491466,124.035646668692)) ;
#54755 = CARTESIAN_POINT('Ctrl Pts',(-20.6995297069063,-36.0483754109855,
124.19159891356)) ;
#54756 = CARTESIAN_POINT('Ctrl Pts',(-20.5342434755889,-36.2383933013744,
123.846317983117)) ;
#54757 = CARTESIAN_POINT('Ctrl Pts',(-20.8154914358056,-36.0584042208939,
123.954937669218)) ;
#54758 = CARTESIAN_POINT('Ctrl Pts',(-20.5920471788539,-36.2482716226812,
123.646853844354)) ;
#54759 = CARTESIAN_POINT('Ctrl Pts',(-20.8877452576722,-36.0682825422007,
123.705606150798)) ;
#54760 = CARTESIAN_POINT('Ctrl Pts',(-20.6150868311933,-36.2582632700286,
123.438058171806)) ;
#54761 = CARTESIAN_POINT('Ctrl Pts',(-20.9165435266129,-36.0782741895481,
123.444611225453)) ;
#54762 = CARTESIAN_POINT('Ctrl Pts',(-20.6010348993728,-36.2682977934664,
123.22757890962)) ;
#54763 = CARTESIAN_POINT('Ctrl Pts',(-20.8989774527681,-36.0883087129859,
123.181512331506)) ;
#54764 = CARTESIAN_POINT('Ctrl Pts',(-20.5519217356949,-36.278161150345,123.026098209884)) ;
#54765 = CARTESIAN_POINT('Ctrl Pts',(-20.8375844349343,-36.0981720698645,
122.929660650863)) ;
#54766 = CARTESIAN_POINT('Ctrl Pts',(-20.4668785726101,-36.2882313770253,
122.832246771308)) ;
#54767 = CARTESIAN_POINT('Ctrl Pts',(-20.7312794063302,-36.1082422965448,
122.687347241453)) ;
#54768 = CARTESIAN_POINT('Ctrl Pts',(-20.3520998438178,-36.2980736851599,
122.660073371831)) ;
#54769 = CARTESIAN_POINT('Ctrl Pts',(-20.5878041612683,-36.1180846046795,
122.472130151179)) ;
#54770 = CARTESIAN_POINT('Ctrl Pts',(-20.2080189864902,-36.3080344171834,
122.508121261806)) ;
#54771 = CARTESIAN_POINT('Ctrl Pts',(-20.4077016434096,-36.1280453367029,
122.282190823974)) ;
#54772 = CARTESIAN_POINT('Ctrl Pts',(-20.038192664759,-36.3180723063815,122.382865970972)) ;
#54773 = CARTESIAN_POINT('Ctrl Pts',(-20.1954179814077,-36.138083225901,122.125622966208)) ;
#54774 = CARTESIAN_POINT('Ctrl Pts',(-19.8524204650629,-36.3279465893003,
122.290172252973)) ;
#54775 = CARTESIAN_POINT('Ctrl Pts',(-19.9632011128443,-36.1479575088198,
122.009756791183)) ;
#54776 = CARTESIAN_POINT('Ctrl Pts',(-19.6494833161937,-36.3380163339178,
122.23000096421)) ;
#54777 = CARTESIAN_POINT('Ctrl Pts',(-19.7095295605724,-36.1580272534373,
121.934544304087)) ;
#54778 = CARTESIAN_POINT('Ctrl Pts',(-19.4440883718789,-36.3478496442634,
122.206429346095)) ;
#54779 = CARTESIAN_POINT('Ctrl Pts',(-19.4527844207029,-36.1678605637829,
121.905081249553)) ;
#54780 = CARTESIAN_POINT('Ctrl Pts',(-19.2335726861195,-36.3578798876161,
122.218526616125)) ;
#54781 = CARTESIAN_POINT('Ctrl Pts',(-19.1896400044676,-36.1778908071356,
121.920204651242)) ;
#54782 = CARTESIAN_POINT('Ctrl Pts',(-19.0284500534322,-36.3679121755945,
122.267618772406)) ;
#54783 = CARTESIAN_POINT('Ctrl Pts',(-18.9332371753586,-36.187923095114,121.981571396535)) ;
#54784 = CARTESIAN_POINT('Ctrl Pts',(-18.838731464373,-36.3777393520626,122.349413172309)) ;
#54785 = CARTESIAN_POINT('Ctrl Pts',(-18.6960884546393,-36.1977502715821,
122.083816541711)) ;
#54786 = CARTESIAN_POINT('Ctrl Pts',(-18.66275010468,-36.3877447349294,122.464585531392)) ;
#54787 = CARTESIAN_POINT('Ctrl Pts',(-18.4761127315903,-36.207755654449,122.227783640355)) ;
#54788 = CARTESIAN_POINT('Ctrl Pts',(-18.5097875290952,-36.3977273739222,
122.608332945589)) ;
#54789 = CARTESIAN_POINT('Ctrl Pts',(-18.2849106464476,-36.2177382934417,
122.407469429926)) ;
#54790 = CARTESIAN_POINT('Ctrl Pts',(-18.3835787051131,-36.4077714410588,
122.777596314135)) ;
#54791 = CARTESIAN_POINT('Ctrl Pts',(-18.1271511614665,-36.2277823605783,
122.619049598976)) ;
#54792 = CARTESIAN_POINT('Ctrl Pts',(-18.2904495023674,-36.4175926598628,
122.961880766302)) ;
#54793 = CARTESIAN_POINT('Ctrl Pts',(-18.0107408055752,-36.2376035793823,
122.849407145881)) ;
#54794 = CARTESIAN_POINT('Ctrl Pts',(-18.2289081179151,-36.4276294988008,
123.163709417083)) ;
#54795 = CARTESIAN_POINT('Ctrl Pts',(-17.9338160939365,-36.2476404183204,
123.101693464105)) ;
#54796 = CARTESIAN_POINT('Ctrl Pts',(-18.2039726595456,-36.4376539108986,
123.372981004564)) ;
#54797 = CARTESIAN_POINT('Ctrl Pts',(-17.9026486630072,-36.2576648304181,
123.363283148377)) ;
#54798 = CARTESIAN_POINT('Ctrl Pts',(-18.215091683057,-36.4475059953039,123.579807254946)) ;
#54799 = CARTESIAN_POINT('Ctrl Pts',(-17.9165495301555,-36.2675169148234,
123.621816862749)) ;
#54800 = CARTESIAN_POINT('Ctrl Pts',(-18.2622958006013,-36.457496892047,123.784448454171)) ;
#54801 = CARTESIAN_POINT('Ctrl Pts',(-17.975556789951,-36.2775078115666,123.877618050294)) ;
#54802 = CARTESIAN_POINT('Ctrl Pts',(-18.3436111264905,-36.467414883948,123.976473263927)) ;
#54803 = CARTESIAN_POINT('Ctrl Pts',(-18.0772031607077,-36.2874258034675,
124.117648747835)) ;
#54804 = CARTESIAN_POINT('Ctrl Pts',(-18.4582275633681,-36.477442999405,124.153397817123)) ;
#54805 = CARTESIAN_POINT('Ctrl Pts',(-18.2204755142129,-36.2974539189245,
124.338803226339)) ;
#54806 = CARTESIAN_POINT('Ctrl Pts',(-18.5997258463659,-36.4873281753471,
124.305609353233)) ;
#54807 = CARTESIAN_POINT('Ctrl Pts',(-18.3973504808242,-36.3073390948666,
124.529066690708)) ;
#54808 = CARTESIAN_POINT('Ctrl Pts',(-18.7669421447371,-36.497317533754,124.432667569944)) ;
#54809 = CARTESIAN_POINT('Ctrl Pts',(-18.606372387143,-36.3173284532735,124.68788770339)) ;
#54810 = CARTESIAN_POINT('Ctrl Pts',(-18.9548477278309,-36.5073586813343,
124.528860622711)) ;
#54811 = CARTESIAN_POINT('Ctrl Pts',(-18.8412552933677,-36.3273696008538,
124.808127004954)) ;
#54812 = CARTESIAN_POINT('Ctrl Pts',(-19.1523079783713,-36.5171913043407,
124.590003139352)) ;
#54813 = CARTESIAN_POINT('Ctrl Pts',(-19.088082204659,-36.3372022238602,124.884553235607)) ;
#54814 = CARTESIAN_POINT('Ctrl Pts',(-19.3606753506828,-36.5271853754515,
124.616945728491)) ;
#54815 = CARTESIAN_POINT('Ctrl Pts',(-19.3485418518574,-36.347196294971,124.918229067427)) ;
#54816 = CARTESIAN_POINT('Ctrl Pts',(-19.5712789350383,-36.5372140330923,
124.606849592832)) ;
#54817 = CARTESIAN_POINT('Ctrl Pts',(-19.6117962054508,-36.3572249526119,
124.90560655703)) ;
#54818 = CARTESIAN_POINT('Ctrl Pts',(-19.7740000727098,-36.5470983592851,
124.561235915968)) ;
#54819 = CARTESIAN_POINT('Ctrl Pts',(-19.865197731046,-36.3671092788047,124.848586979742)) ;
#54820 = CARTESIAN_POINT('Ctrl Pts',(-19.9675160561407,-36.5570641027758,
124.48092624152)) ;
#54821 = CARTESIAN_POINT('Ctrl Pts',(-20.1070919689581,-36.3770750222953,
124.748197482169)) ;
#54822 = CARTESIAN_POINT('Ctrl Pts',(-20.1450804636381,-36.567092481907,124.36727939808)) ;
#54823 = CARTESIAN_POINT('Ctrl Pts',(-20.3290461477536,-36.3871034014265,
124.606136879455)) ;
#54824 = CARTESIAN_POINT('Ctrl Pts',(-20.2984821281396,-36.5769933281139,
124.226551618622)) ;
#54825 = CARTESIAN_POINT('Ctrl Pts',(-20.5207969132898,-36.3970042476334,
124.430224963502)) ;
#54826 = CARTESIAN_POINT('Ctrl Pts',(-20.4270554223315,-36.587051985531,124.058705204649)) ;
#54827 = CARTESIAN_POINT('Ctrl Pts',(-20.6815114755978,-36.4070629050505,
124.220415524701)) ;
#54828 = CARTESIAN_POINT('Ctrl Pts',(-20.5228088976676,-36.5969095483129,
123.874874545121)) ;
#54829 = CARTESIAN_POINT('Ctrl Pts',(-20.8012013745424,-36.4169204678324,
123.990625446884)) ;
#54830 = CARTESIAN_POINT('Ctrl Pts',(-20.5866346710282,-36.6069779508661,
123.673090041248)) ;
#54831 = CARTESIAN_POINT('Ctrl Pts',(-20.8809810996104,-36.4269888703856,
123.738394192425)) ;
#54832 = CARTESIAN_POINT('Ctrl Pts',(-20.6138518765132,-36.6168333496057,
123.46767623189)) ;
#54833 = CARTESIAN_POINT('Ctrl Pts',(-20.9150001539312,-36.4368442691252,
123.481625971237)) ;
#54834 = CARTESIAN_POINT('Ctrl Pts',(-20.6054955842666,-36.6268282166796,
123.257725834414)) ;
#54835 = CARTESIAN_POINT('Ctrl Pts',(-20.9045521216092,-36.4468391361991,
123.219187981006)) ;
#54836 = CARTESIAN_POINT('Ctrl Pts',(-20.5602021180779,-36.636859511663,123.051753465069)) ;
#54837 = CARTESIAN_POINT('Ctrl Pts',(-20.8479327598171,-36.4568704311826,
122.961723074827)) ;
#54838 = CARTESIAN_POINT('Ctrl Pts',(-20.4814585623447,-36.6467260363896,
122.859848018416)) ;
#54839 = CARTESIAN_POINT('Ctrl Pts',(-20.7495006732723,-36.4667369559091,
122.721841788976)) ;
#54840 = CARTESIAN_POINT('Ctrl Pts',(-20.3695334272533,-36.6567135070853,
122.682228468216)) ;
#54841 = CARTESIAN_POINT('Ctrl Pts',(-20.6095919098438,-36.4767244266048,
122.499818683147)) ;
#54842 = CARTESIAN_POINT('Ctrl Pts',(-20.2291188401914,-36.6666582666492,
122.527284926112)) ;
#54843 = CARTESIAN_POINT('Ctrl Pts',(-20.4340715147881,-36.4866691861687,
122.306140896001)) ;
#54844 = CARTESIAN_POINT('Ctrl Pts',(-20.0622231051933,-36.676703822598,122.397914061097)) ;
#54845 = CARTESIAN_POINT('Ctrl Pts',(-20.2254502143185,-36.4967147421175,
122.14442945412)) ;
#54846 = CARTESIAN_POINT('Ctrl Pts',(-19.8789187763763,-36.6865634109731,
122.301092451122)) ;
#54847 = CARTESIAN_POINT('Ctrl Pts',(-19.9963181528089,-36.5065743304926,
122.023404638847)) ;
#54848 = CARTESIAN_POINT('Ctrl Pts',(-19.6789119610615,-36.6965643661092,
122.23637511333)) ;
#54849 = CARTESIAN_POINT('Ctrl Pts',(-19.7463087038037,-36.5165752856287,
121.94251056244)) ;
#54850 = CARTESIAN_POINT('Ctrl Pts',(-19.4726764661033,-36.7064685933867,
122.207479051172)) ;
#54851 = CARTESIAN_POINT('Ctrl Pts',(-19.4885136890364,-36.5264795129063,
121.906393184978)) ;
#54852 = CARTESIAN_POINT('Ctrl Pts',(-19.2617182497028,-36.7165106702819,
122.214872705184)) ;
#54853 = CARTESIAN_POINT('Ctrl Pts',(-19.2248160076973,-36.5365215898014,
121.915638023178)) ;
#54854 = CARTESIAN_POINT('Ctrl Pts',(-19.057927154021,-36.726418282968,122.2581086562)) ;
#54855 = CARTESIAN_POINT('Ctrl Pts',(-18.970077488326,-36.5464292024876,121.96968572627)) ;
#54856 = CARTESIAN_POINT('Ctrl Pts',(-18.8619321432003,-36.7364728135838,
122.337188886544)) ;
#54857 = CARTESIAN_POINT('Ctrl Pts',(-18.7250847626907,-36.5564837331033,
122.068538595293)) ;
#54858 = CARTESIAN_POINT('Ctrl Pts',(-18.6859875564324,-36.7463336001326,
122.446869658722)) ;
#54859 = CARTESIAN_POINT('Ctrl Pts',(-18.5051552711901,-36.5663445196522,
122.205642070878)) ;
#54860 = CARTESIAN_POINT('Ctrl Pts',(-18.5294655824155,-36.7563273552037,
122.586972488339)) ;
#54861 = CARTESIAN_POINT('Ctrl Pts',(-18.3095046248543,-36.5763382747232,
122.380772756603)) ;
#54862 = CARTESIAN_POINT('Ctrl Pts',(-18.4004150751371,-36.7662527154437,
122.750983302961)) ;
#54863 = CARTESIAN_POINT('Ctrl Pts',(-18.1481936175837,-36.5862636349632,
122.585788118816)) ;
#54864 = CARTESIAN_POINT('Ctrl Pts',(-18.3008055717462,-36.776280644839,122.936753966816)) ;
#54865 = CARTESIAN_POINT('Ctrl Pts',(-18.0236841920842,-36.5962915643585,
122.818002834803)) ;
#54866 = CARTESIAN_POINT('Ctrl Pts',(-18.2356726374387,-36.7861669116383,
123.134158053417)) ;
#54867 = CARTESIAN_POINT('Ctrl Pts',(-17.9422706634272,-36.6061778311578,
123.0647589423)) ;
#54868 = CARTESIAN_POINT('Ctrl Pts',(-18.2052669474954,-36.7961986805365,
123.342818627154)) ;
#54869 = CARTESIAN_POINT('Ctrl Pts',(-17.904266334052,-36.6162096000561,123.32558512975)) ;
#54870 = CARTESIAN_POINT('Ctrl Pts',(-18.2112586660847,-36.8060802763801,
123.550511838692)) ;
#54871 = CARTESIAN_POINT('Ctrl Pts',(-17.911758818048,-36.6260911958997,123.585201643674)) ;
#54872 = CARTESIAN_POINT('Ctrl Pts',(-18.2539211094933,-36.8161421618481,
123.757665242363)) ;
#54873 = CARTESIAN_POINT('Ctrl Pts',(-17.9650896018875,-36.6361530813676,
123.844142860301)) ;
#54874 = CARTESIAN_POINT('Ctrl Pts',(-18.3302768913769,-36.825999595867,123.950348541592)) ;
#54875 = CARTESIAN_POINT('Ctrl Pts',(-18.0605371632043,-36.6460105153865,
124.08499614466)) ;
#54876 = CARTESIAN_POINT('Ctrl Pts',(-18.4400202960657,-36.8359928389089,
124.129465514795)) ;
#54877 = CARTESIAN_POINT('Ctrl Pts',(-18.1977180727596,-36.6560037584285,
124.308890236718)) ;
#54878 = CARTESIAN_POINT('Ctrl Pts',(-18.5783392874067,-36.8459235997953,
124.285860530243)) ;
#54879 = CARTESIAN_POINT('Ctrl Pts',(-18.370621788701,-36.6659345193148,124.504384734835)) ;
#54880 = CARTESIAN_POINT('Ctrl Pts',(-18.7977945098984,-36.8592725919925,
124.460845444457)) ;
#54881 = CARTESIAN_POINT('Ctrl Pts',(-18.644928888487,-36.679283511512,124.723100111771)) ;
#54882 = CARTESIAN_POINT('Ctrl Pts',(-19.0564575910086,-36.8725409648089,
124.573487171901)) ;
#54883 = CARTESIAN_POINT('Ctrl Pts',(-18.968224608499,-36.6925518843284,124.863897618204)) ;
#54884 = CARTESIAN_POINT('Ctrl Pts',(-19.332518152077,-36.8858239061933,124.615432948066)) ;
#54885 = CARTESIAN_POINT('Ctrl Pts',(-19.3133563776391,-36.7058348257128,
124.9163404754)) ;
#54886 = CARTESIAN_POINT('Ctrl Pts',(-19.5435804177348,-36.8958666920355,
124.610274690913)) ;
#54887 = CARTESIAN_POINT('Ctrl Pts',(-19.5771730601829,-36.715877611555,124.909887095996)) ;
#54888 = CARTESIAN_POINT('Ctrl Pts',(-19.7466220723449,-36.9057166345876,
124.569566521813)) ;
#54889 = CARTESIAN_POINT('Ctrl Pts',(-19.8309776236468,-36.7257275541071,
124.858999538759)) ;
#54890 = CARTESIAN_POINT('Ctrl Pts',(-19.9425753325179,-36.9157138675065,
124.493590570334)) ;
#54891 = CARTESIAN_POINT('Ctrl Pts',(-20.075916339916,-36.7357247870261,124.764028514529)) ;
#54892 = CARTESIAN_POINT('Ctrl Pts',(-20.1225212109622,-36.9257287628411,
124.384267908977)) ;
#54893 = CARTESIAN_POINT('Ctrl Pts',(-20.3008516833001,-36.7457396823606,
124.627366616368)) ;
#54894 = CARTESIAN_POINT('Ctrl Pts',(-20.3318880894533,-36.9389684394793,
124.200821795761)) ;
#54895 = CARTESIAN_POINT('Ctrl Pts',(-20.562537162733,-36.7589793589988,124.398087289578)) ;
#54896 = CARTESIAN_POINT('Ctrl Pts',(-20.528163224449,-36.9555156638846,123.9088995619)) ;
#54897 = CARTESIAN_POINT('Ctrl Pts',(-20.8079029755518,-36.7755265834041,
124.033128787437)) ;
#54898 = CARTESIAN_POINT('Ctrl Pts',(-20.6137528393046,-36.9721631010157,
123.56536786537)) ;
#54899 = CARTESIAN_POINT('Ctrl Pts',(-20.9148689310472,-36.7921740205352,
123.603796766495)) ;
#54900 = CARTESIAN_POINT('Ctrl Pts',(-20.6085683059766,-36.9854525984939,
123.286061986322)) ;
#54901 = CARTESIAN_POINT('Ctrl Pts',(-20.9083945689062,-36.8054635180134,
123.254597757702)) ;
#54902 = CARTESIAN_POINT('Ctrl Pts',(-20.5693560188396,-36.9953260063163,
123.082217819628)) ;
#54903 = CARTESIAN_POINT('Ctrl Pts',(-20.859374951537,-36.8153369258358,122.999807024166)) ;
#54904 = CARTESIAN_POINT('Ctrl Pts',(-20.4940428412356,-37.005378383909,122.884773388024)) ;
#54905 = CARTESIAN_POINT('Ctrl Pts',(-20.7652312034385,-36.8253893034285,
122.752998369453)) ;
#54906 = CARTESIAN_POINT('Ctrl Pts',(-20.3871047058436,-37.0152820374499,
122.706108282335)) ;
#54907 = CARTESIAN_POINT('Ctrl Pts',(-20.631557772952,-36.8352929569694,122.529670136068)) ;
#54908 = CARTESIAN_POINT('Ctrl Pts',(-20.2506236096731,-37.0252263064452,
122.547784485508)) ;
#54909 = CARTESIAN_POINT('Ctrl Pts',(-20.4609498468853,-36.8452372259647,
122.331765024377)) ;
#54910 = CARTESIAN_POINT('Ctrl Pts',(-20.0335787700198,-37.0385573147779,
122.37035520076)) ;
#54911 = CARTESIAN_POINT('Ctrl Pts',(-20.1896663856543,-36.8585682342974,
122.109990345153)) ;
#54912 = CARTESIAN_POINT('Ctrl Pts',(-19.7113303634737,-37.0551788953021,
122.225449965275)) ;
#54913 = CARTESIAN_POINT('Ctrl Pts',(-19.7868089892428,-36.8751898148217,
121.928852787529)) ;
#54914 = CARTESIAN_POINT('Ctrl Pts',(-19.3605381967804,-37.0717215660005,
122.198625173765)) ;
#54915 = CARTESIAN_POINT('Ctrl Pts',(-19.3483970122116,-36.8917324855201,
121.895325330495)) ;
#54916 = CARTESIAN_POINT('Ctrl Pts',(-19.084756283337,-37.0850707255635,122.250326858334)) ;
#54917 = CARTESIAN_POINT('Ctrl Pts',(-19.0036058958539,-36.905081645083,121.959959179047)) ;
#54918 = CARTESIAN_POINT('Ctrl Pts',(-18.8243006026364,-37.098298875723,122.34794994263)) ;
#54919 = CARTESIAN_POINT('Ctrl Pts',(-18.6780618919625,-36.9183097952425,
122.081981866891)) ;
#54920 = CARTESIAN_POINT('Ctrl Pts',(-18.5364100435384,-37.1149295528605,
122.553165444984)) ;
#54921 = CARTESIAN_POINT('Ctrl Pts',(-18.3181836589945,-36.93494047238,122.338513488411)) ;
#54922 = CARTESIAN_POINT('Ctrl Pts',(-18.2963005996991,-37.1348324921486,
122.901714167161)) ;
#54923 = CARTESIAN_POINT('Ctrl Pts',(-18.0180562106174,-36.9548434116681,
122.774198058381)) ;
#54924 = CARTESIAN_POINT('Ctrl Pts',(-18.1891582578052,-37.1547353587518,
123.311031502207)) ;
#54925 = CARTESIAN_POINT('Ctrl Pts',(-17.8841306986637,-36.9747462782714,
123.285845641878)) ;
#54926 = CARTESIAN_POINT('Ctrl Pts',(-18.2275156867731,-37.1746485238567,
123.732793359214)) ;
#54927 = CARTESIAN_POINT('Ctrl Pts',(-17.9320811339268,-36.9946594433762,
123.813046654379)) ;
#54928 = CARTESIAN_POINT('Ctrl Pts',(-18.409140585469,-37.194684352998,124.118086353196)) ;
#54929 = CARTESIAN_POINT('Ctrl Pts',(-18.1591155084676,-37.0146952725175,
124.294661831233)) ;
#54930 = CARTESIAN_POINT('Ctrl Pts',(-18.7080016710259,-37.2145029278761,
124.41531311931)) ;
#54931 = CARTESIAN_POINT('Ctrl Pts',(-18.5326928559691,-37.0345138473956,
124.666191700612)) ;
#54932 = CARTESIAN_POINT('Ctrl Pts',(-19.0927718739483,-37.2344732289181,
124.594578380774)) ;
#54933 = CARTESIAN_POINT('Ctrl Pts',(-19.0136563926728,-37.0544841484376,
124.890270640094)) ;
#54934 = CARTESIAN_POINT('Ctrl Pts',(-19.5142339391822,-37.2543647612826,
124.631795562197)) ;
#54935 = CARTESIAN_POINT('Ctrl Pts',(-19.5404829664687,-37.0743756808021,
124.936789595379)) ;
#54936 = CARTESIAN_POINT('Ctrl Pts',(-19.9254766838517,-37.2743878590991,
124.521993821233)) ;
#54937 = CARTESIAN_POINT('Ctrl Pts',(-20.0545360586969,-37.0943987786187,
124.799534983249)) ;
#54938 = CARTESIAN_POINT('Ctrl Pts',(-20.2709110278147,-37.2941846120191,
124.281362408259)) ;
#54939 = CARTESIAN_POINT('Ctrl Pts',(-20.486325645581,-37.1141955315386,124.498745537958)) ;
#54940 = CARTESIAN_POINT('Ctrl Pts',(-20.5163858033962,-37.3141457005079,
123.935170853578)) ;
#54941 = CARTESIAN_POINT('Ctrl Pts',(-20.7931678601018,-37.1341566200274,
124.066005974711)) ;
#54942 = CARTESIAN_POINT('Ctrl Pts',(-20.6282493094601,-37.33412396944,123.52533621411)) ;
#54943 = CARTESIAN_POINT('Ctrl Pts',(-20.9329957736471,-37.1541348889596,
123.55371250196)) ;
#54944 = CARTESIAN_POINT('Ctrl Pts',(-20.5944348756213,-37.353943984231,123.105306555051)) ;
#54945 = CARTESIAN_POINT('Ctrl Pts',(-20.8907271347711,-37.1739549037506,
123.028678283187)) ;
#54946 = CARTESIAN_POINT('Ctrl Pts',(-20.419241626978,-37.3738823934829,122.719230553153)) ;
#54947 = CARTESIAN_POINT('Ctrl Pts',(-20.671736248065,-37.1938933130024,122.546084069823)) ;
#54948 = CARTESIAN_POINT('Ctrl Pts',(-20.1204934119422,-37.3939295108753,
122.415110115247)) ;
#54949 = CARTESIAN_POINT('Ctrl Pts',(-20.2983002158632,-37.2139404303948,
122.165933042712)) ;
#54950 = CARTESIAN_POINT('Ctrl Pts',(-19.7397550775313,-37.4137757567091,
122.233254243053)) ;
#54951 = CARTESIAN_POINT('Ctrl Pts',(-19.8223796113468,-37.2337866762287,
121.938614397034)) ;
#54952 = CARTESIAN_POINT('Ctrl Pts',(-19.3198536517042,-37.4336247252212,
122.19057464082)) ;
#54953 = CARTESIAN_POINT('Ctrl Pts',(-19.2975051439702,-37.2536356447407,
121.885263707439)) ;
#54954 = CARTESIAN_POINT('Ctrl Pts',(-18.9066386247496,-37.4536750275325,
122.295305344993)) ;
#54955 = CARTESIAN_POINT('Ctrl Pts',(-18.7809853426372,-37.273685947052,122.016176078688)) ;
#54956 = CARTESIAN_POINT('Ctrl Pts',(-18.5576843444494,-37.4735099499637,
122.53234187102)) ;
#54957 = CARTESIAN_POINT('Ctrl Pts',(-18.3447935794492,-37.2935208694832,
122.312469305178)) ;
#54958 = CARTESIAN_POINT('Ctrl Pts',(-18.3088629623989,-37.4934403511896,
122.87517401801)) ;
#54959 = CARTESIAN_POINT('Ctrl Pts',(-18.0337656487318,-37.3134512707091,
122.741007439653)) ;
#54960 = CARTESIAN_POINT('Ctrl Pts',(-18.191627159294,-37.5133252965484,123.281572566289)) ;
#54961 = CARTESIAN_POINT('Ctrl Pts',(-17.8872187176123,-37.333336216068,123.249003693787)) ;
#54962 = CARTESIAN_POINT('Ctrl Pts',(-18.2210576117943,-37.5333979046998,
123.707273120117)) ;
#54963 = CARTESIAN_POINT('Ctrl Pts',(-17.9240043989102,-37.3534088242194,
123.781130410559)) ;
#54964 = CARTESIAN_POINT('Ctrl Pts',(-18.3915612941918,-37.5531892210279,
124.092070927854)) ;
#54965 = CARTESIAN_POINT('Ctrl Pts',(-18.1371306276255,-37.3732001405475,
124.26212661135)) ;
#54966 = CARTESIAN_POINT('Ctrl Pts',(-18.6846818237289,-37.5731540107952,
124.399080855856)) ;
#54967 = CARTESIAN_POINT('Ctrl Pts',(-18.5035285317614,-37.3931649303147,
124.645891221395)) ;
#54968 = CARTESIAN_POINT('Ctrl Pts',(-19.0658286606464,-37.5931369665455,
124.5868719561)) ;
#54969 = CARTESIAN_POINT('Ctrl Pts',(-18.9799605391269,-37.413147886065,124.880632850392)) ;
#54970 = CARTESIAN_POINT('Ctrl Pts',(-19.4844281526955,-37.6129454885216,
124.633785399383)) ;
#54971 = CARTESIAN_POINT('Ctrl Pts',(-19.5032077670289,-37.4329564080412,
124.93927814101)) ;
#54972 = CARTESIAN_POINT('Ctrl Pts',(-19.8975569980139,-37.6329310632575,
124.534652953361)) ;
#54973 = CARTESIAN_POINT('Ctrl Pts',(-20.0196196743676,-37.452941982777,124.815366561409)) ;
#54974 = CARTESIAN_POINT('Ctrl Pts',(-20.2503434108889,-37.6528137033259,
124.301519197252)) ;
#54975 = CARTESIAN_POINT('Ctrl Pts',(-20.4606042548216,-37.4728246228454,
124.523953284012)) ;
#54976 = CARTESIAN_POINT('Ctrl Pts',(-20.503477443757,-37.6727690154578,123.96110057976)) ;
#54977 = CARTESIAN_POINT('Ctrl Pts',(-20.7770251298979,-37.4927799349773,
124.098432868024)) ;
#54978 = CARTESIAN_POINT('Ctrl Pts',(-20.6250594607957,-37.6926433720656,
123.556310778876)) ;
#54979 = CARTESIAN_POINT('Ctrl Pts',(-20.9290068710013,-37.5126542915851,
123.592447664167)) ;
#54980 = CARTESIAN_POINT('Ctrl Pts',(-20.60136228044,-37.7126255789266,123.132144136794)) ;
#54981 = CARTESIAN_POINT('Ctrl Pts',(-20.8993899563802,-37.5326364984462,
123.062239130168)) ;
#54982 = CARTESIAN_POINT('Ctrl Pts',(-20.4345064783654,-37.7325566568766,
122.742488170039)) ;
#54983 = CARTESIAN_POINT('Ctrl Pts',(-20.6908254812165,-37.5525675763961,
122.575167631135)) ;
#54984 = CARTESIAN_POINT('Ctrl Pts',(-20.1449218342173,-37.7524836317316,
122.433312486334)) ;
#54985 = CARTESIAN_POINT('Ctrl Pts',(-20.3288457046536,-37.5724945512511,
122.188694790746)) ;
#54986 = CARTESIAN_POINT('Ctrl Pts',(-19.769249258697,-37.7723160906805,122.241620195832)) ;
#54987 = CARTESIAN_POINT('Ctrl Pts',(-19.8592684234008,-37.5923270102,121.949075641498)) ;
#54988 = CARTESIAN_POINT('Ctrl Pts',(-19.417912839103,-37.7889737748557,122.197692406398)) ;
#54989 = CARTESIAN_POINT('Ctrl Pts',(-19.4200658004677,-37.6089846943752,
121.894159881011)) ;
#54990 = CARTESIAN_POINT('Ctrl Pts',(-19.1419000183344,-37.8022229987628,
122.235811998342)) ;
#54991 = CARTESIAN_POINT('Ctrl Pts',(-19.0750788995196,-37.6222339182823,
121.941806794184)) ;
#54992 = CARTESIAN_POINT('Ctrl Pts',(-18.9408249504578,-37.812272020214,122.300516733024)) ;
#54993 = CARTESIAN_POINT('Ctrl Pts',(-18.8237258576414,-37.6322829397335,
122.022687580553)) ;
#54994 = CARTESIAN_POINT('Ctrl Pts',(-18.75748940626,-37.8221320284445,122.39727315745)) ;
#54995 = CARTESIAN_POINT('Ctrl Pts',(-18.5945663207733,-37.642142947964,122.143620576973)) ;
#54996 = CARTESIAN_POINT('Ctrl Pts',(-18.5363454819024,-37.8354155416691,
122.567770253279)) ;
#54997 = CARTESIAN_POINT('Ctrl Pts',(-18.3180876792533,-37.6554264611886,
122.356789242031)) ;
#54998 = CARTESIAN_POINT('Ctrl Pts',(-18.3218393831635,-37.8520614606699,
122.849331128677)) ;
#54999 = CARTESIAN_POINT('Ctrl Pts',(-18.0500066417951,-37.6720723801894,
122.708670183336)) ;
#55000 = CARTESIAN_POINT('Ctrl Pts',(-18.2164325706239,-37.868615438486,123.185138476082)) ;
#55001 = CARTESIAN_POINT('Ctrl Pts',(-17.9182173114303,-37.6886263580055,
123.128486091663)) ;
#55002 = CARTESIAN_POINT('Ctrl Pts',(-18.2044905733032,-37.8819751674576,
123.465776368873)) ;
#55003 = CARTESIAN_POINT('Ctrl Pts',(-17.9032980829134,-37.7019860869771,
123.479244069044)) ;
#55004 = CARTESIAN_POINT('Ctrl Pts',(-18.2317111895261,-37.8918682192543,
123.671978883509)) ;
#55005 = CARTESIAN_POINT('Ctrl Pts',(-17.9373186785882,-37.7118791387738,
123.73700538151)) ;
#55006 = CARTESIAN_POINT('Ctrl Pts',(-18.294652658177,-37.9018581845353,123.87232240774)) ;
#55007 = CARTESIAN_POINT('Ctrl Pts',(-18.0159935015514,-37.7218691040548,
123.98743356225)) ;
#55008 = CARTESIAN_POINT('Ctrl Pts',(-18.3909713233348,-37.9118100653962,
124.058088930702)) ;
#55009 = CARTESIAN_POINT('Ctrl Pts',(-18.1363891803224,-37.7318209849157,
124.219643590577)) ;
#55010 = CARTESIAN_POINT('Ctrl Pts',(-18.5194225453027,-37.921858417088,124.225768775159)) ;
#55011 = CARTESIAN_POINT('Ctrl Pts',(-18.2969510923513,-37.7418693366075,
124.429245026213)) ;
#55012 = CARTESIAN_POINT('Ctrl Pts',(-18.671696215703,-37.9316997011942,124.365864629888)) ;
#55013 = CARTESIAN_POINT('Ctrl Pts',(-18.4872912315041,-37.7517106207137,
124.604366917906)) ;
#55014 = CARTESIAN_POINT('Ctrl Pts',(-18.8482704727161,-37.9416864043198,
124.479380726251)) ;
#55015 = CARTESIAN_POINT('Ctrl Pts',(-18.7080075971483,-37.7616973238393,
124.746264446641)) ;
#55016 = CARTESIAN_POINT('Ctrl Pts',(-19.0408922738897,-37.9516214331373,
124.560242685434)) ;
#55017 = CARTESIAN_POINT('Ctrl Pts',(-18.9487838243204,-37.7716323526568,
124.847344520191)) ;
#55018 = CARTESIAN_POINT('Ctrl Pts',(-19.2470723983466,-37.9616772280442,
124.606804319472)) ;
#55019 = CARTESIAN_POINT('Ctrl Pts',(-19.2065084133188,-37.7816881475637,
124.905549326719)) ;
#55020 = CARTESIAN_POINT('Ctrl Pts',(-19.4534751390395,-37.9715055913335,
124.616954335681)) ;
#55021 = CARTESIAN_POINT('Ctrl Pts',(-19.4645118314084,-37.791516510853,124.918239663779)) ;
#55022 = CARTESIAN_POINT('Ctrl Pts',(-19.6633369830596,-37.9815665612314,
124.590805337205)) ;
#55023 = CARTESIAN_POINT('Ctrl Pts',(-19.7268395349179,-37.8015774807509,
124.88555619889)) ;
#55024 = CARTESIAN_POINT('Ctrl Pts',(-19.8625213753835,-37.9914808401212,
124.529341700821)) ;
#55025 = CARTESIAN_POINT('Ctrl Pts',(-19.9758209773631,-37.8114917596407,
124.808729302438)) ;
#55026 = CARTESIAN_POINT('Ctrl Pts',(-20.0499508132267,-38.0014898345894,
124.433695820454)) ;
#55027 = CARTESIAN_POINT('Ctrl Pts',(-20.2101091149585,-37.821500754109,124.689174409478)) ;
#55028 = CARTESIAN_POINT('Ctrl Pts',(-20.2180109913369,-38.0115196691532,
124.306354445413)) ;
#55029 = CARTESIAN_POINT('Ctrl Pts',(-20.4201860706059,-37.8315305886727,
124.52999991223)) ;
#55030 = CARTESIAN_POINT('Ctrl Pts',(-20.3592543198836,-38.0213778992254,
124.154667140303)) ;
#55031 = CARTESIAN_POINT('Ctrl Pts',(-20.5967424361881,-37.8413888187449,
124.340392519034)) ;
#55032 = CARTESIAN_POINT('Ctrl Pts',(-20.4738072405077,-38.0313766049678,
123.978459990424)) ;
#55033 = CARTESIAN_POINT('Ctrl Pts',(-20.7399359739768,-37.8513875244874,
124.120135025815)) ;
#55034 = CARTESIAN_POINT('Ctrl Pts',(-20.5554252299828,-38.0412712608866,
123.787082603069)) ;
#55035 = CARTESIAN_POINT('Ctrl Pts',(-20.8419611025368,-37.8612821804061,
123.880914136025)) ;
#55036 = CARTESIAN_POINT('Ctrl Pts',(-20.6032952967785,-38.0513343252705,
123.581049295425)) ;
#55037 = CARTESIAN_POINT('Ctrl Pts',(-20.9018013800927,-37.8713452447901,
123.623373162088)) ;
#55038 = CARTESIAN_POINT('Ctrl Pts',(-20.6146442268699,-38.0611739835504,
123.374466194036)) ;
#55039 = CARTESIAN_POINT('Ctrl Pts',(-20.9159903079656,-37.88118490307,123.365144028709)) ;
#55040 = CARTESIAN_POINT('Ctrl Pts',(-20.5896648476914,-38.0712371506323,
123.164415788226)) ;
#55041 = CARTESIAN_POINT('Ctrl Pts',(-20.8847687944641,-37.8912480701518,
123.102580743013)) ;
#55042 = CARTESIAN_POINT('Ctrl Pts',(-20.5294350178213,-38.0811313957594,
122.965294396189)) ;
#55043 = CARTESIAN_POINT('Ctrl Pts',(-20.809484036309,-37.9011423152789,122.853677895815)) ;
#55044 = CARTESIAN_POINT('Ctrl Pts',(-20.4356240821456,-38.091073217364,122.778550856413)) ;
#55045 = CARTESIAN_POINT('Ctrl Pts',(-20.6922226403838,-37.9110841368836,
122.620247034485)) ;
#55046 = CARTESIAN_POINT('Ctrl Pts',(-20.3100810134852,-38.1010757482821,
122.609819097008)) ;
#55047 = CARTESIAN_POINT('Ctrl Pts',(-20.5352958892359,-37.9210866678016,
122.409330679749)) ;
#55048 = CARTESIAN_POINT('Ctrl Pts',(-20.1564607952852,-38.1111103747396,
122.465250449914)) ;
#55049 = CARTESIAN_POINT('Ctrl Pts',(-20.3432724836737,-37.9311212942591,
122.228617908564)) ;
#55050 = CARTESIAN_POINT('Ctrl Pts',(-19.9835623722376,-38.120955909726,122.351445881566)) ;
#55051 = CARTESIAN_POINT('Ctrl Pts',(-20.1271504516508,-37.9409668292455,
122.086359667513)) ;
#55052 = CARTESIAN_POINT('Ctrl Pts',(-19.7910718790852,-38.130939334565,122.267833463766)) ;
#55053 = CARTESIAN_POINT('Ctrl Pts',(-19.8865382084565,-37.9509502540846,
121.981841696221)) ;
#55054 = CARTESIAN_POINT('Ctrl Pts',(-19.5876306579575,-38.1408897249301,
122.219111287809)) ;
#55055 = CARTESIAN_POINT('Ctrl Pts',(-19.6322370248883,-37.9609006444496,
121.920936388754)) ;
#55056 = CARTESIAN_POINT('Ctrl Pts',(-19.377833549305,-38.1508873652272,122.206109169437)) ;
#55057 = CARTESIAN_POINT('Ctrl Pts',(-19.3699906918026,-37.9708982847467,
121.90468118913)) ;
#55058 = CARTESIAN_POINT('Ctrl Pts',(-19.1681777198956,-38.1609264457904,
122.230248686122)) ;
#55059 = CARTESIAN_POINT('Ctrl Pts',(-19.1079206635879,-37.9809373653099,
121.93485297098)) ;
#55060 = CARTESIAN_POINT('Ctrl Pts',(-18.9700348987054,-38.1707525965595,
122.288711476729)) ;
#55061 = CARTESIAN_POINT('Ctrl Pts',(-18.8602406825813,-37.990763516079,122.007929238397)) ;
#55062 = CARTESIAN_POINT('Ctrl Pts',(-18.7805861370791,-38.1808091714886,
122.382535043644)) ;
#55063 = CARTESIAN_POINT('Ctrl Pts',(-18.623428724634,-38.0008200910081,122.125206427379)) ;
#55064 = CARTESIAN_POINT('Ctrl Pts',(-18.6124721251259,-38.1907497108689,
122.506687338433)) ;
#55065 = CARTESIAN_POINT('Ctrl Pts',(-18.4132844277735,-38.0107606303884,
122.280394942129)) ;
#55066 = CARTESIAN_POINT('Ctrl Pts',(-18.4685228176919,-38.2006541038453,
122.657141441856)) ;
#55067 = CARTESIAN_POINT('Ctrl Pts',(-18.2333456789751,-38.0206650233648,
122.468461282775)) ;
#55068 = CARTESIAN_POINT('Ctrl Pts',(-18.3513466171436,-38.2107007580502,
122.832848241972)) ;
#55069 = CARTESIAN_POINT('Ctrl Pts',(-18.0868734494844,-38.0307116775697,
122.688093340376)) ;
#55070 = CARTESIAN_POINT('Ctrl Pts',(-18.2675409912502,-38.2205963199886,
123.023293670157)) ;
#55071 = CARTESIAN_POINT('Ctrl Pts',(-17.9821139833367,-38.0406072395081,
122.92614968841)) ;
#55072 = CARTESIAN_POINT('Ctrl Pts',(-18.2172590198728,-38.2306583978341,
123.228736388666)) ;
#55073 = CARTESIAN_POINT('Ctrl Pts',(-17.9192592234014,-38.0506693173537,
123.182952338468)) ;
#55074 = CARTESIAN_POINT('Ctrl Pts',(-18.203592355486,-38.2405010962479,123.435232302293)) ;
#55075 = CARTESIAN_POINT('Ctrl Pts',(-17.9021734626821,-38.0605120157674,
123.44107293395)) ;
#55076 = CARTESIAN_POINT('Ctrl Pts',(-18.2258256609928,-38.2504918712094,
123.644062640654)) ;
#55077 = CARTESIAN_POINT('Ctrl Pts',(-17.9299628605626,-38.0705027907289,
123.702111270624)) ;
#55078 = CARTESIAN_POINT('Ctrl Pts',(-18.2836555871143,-38.2604197362285,
123.844617912795)) ;
#55079 = CARTESIAN_POINT('Ctrl Pts',(-18.0022482228255,-38.080430655748,123.95280645731)) ;
#55080 = CARTESIAN_POINT('Ctrl Pts',(-18.3756740561465,-38.2704084809947,
124.033382785649)) ;
#55081 = CARTESIAN_POINT('Ctrl Pts',(-18.1172694268296,-38.0904194005142,
124.188763665589)) ;
#55082 = CARTESIAN_POINT('Ctrl Pts',(-18.4998651142318,-38.2804412665816,
124.203869104548)) ;
#55083 = CARTESIAN_POINT('Ctrl Pts',(-18.2725063778356,-38.1004521861012,
124.401872837014)) ;
#55084 = CARTESIAN_POINT('Ctrl Pts',(-18.649102754769,-38.2903079512023,124.347923475099)) ;
#55085 = CARTESIAN_POINT('Ctrl Pts',(-18.459052515942,-38.1103188707218,124.581942987267)) ;
#55086 = CARTESIAN_POINT('Ctrl Pts',(-18.8224168744023,-38.3002698433654,
124.465501995061)) ;
#55087 = CARTESIAN_POINT('Ctrl Pts',(-18.675694305883,-38.1202807628849,124.728918023426)) ;
#55088 = CARTESIAN_POINT('Ctrl Pts',(-19.0150124373623,-38.310303320278,124.551507630539)) ;
#55089 = CARTESIAN_POINT('Ctrl Pts',(-18.9164378070298,-38.1303142397975,
124.836426983445)) ;
#55090 = CARTESIAN_POINT('Ctrl Pts',(-19.2165276853303,-38.3201876615263,
124.602331746933)) ;
#55091 = CARTESIAN_POINT('Ctrl Pts',(-19.1683321359432,-38.1401985810458,
124.899959302576)) ;
#55092 = CARTESIAN_POINT('Ctrl Pts',(-19.4274995678866,-38.3302506036474,
124.617665373522)) ;
#55093 = CARTESIAN_POINT('Ctrl Pts',(-19.4320465863477,-38.1502615231669,
124.919128358912)) ;
#55094 = CARTESIAN_POINT('Ctrl Pts',(-19.6335365424027,-38.340101005267,124.596684953135)) ;
#55095 = CARTESIAN_POINT('Ctrl Pts',(-19.68959404648,-38.1601119247865,124.892904734161)) ;
#55096 = CARTESIAN_POINT('Ctrl Pts',(-19.8364952866382,-38.3501278940566,
124.539756466439)) ;
#55097 = CARTESIAN_POINT('Ctrl Pts',(-19.9432929414861,-38.1701388135762,
124.82174592566)) ;
#55098 = CARTESIAN_POINT('Ctrl Pts',(-20.0262936192823,-38.3601565090128,
124.447932183891)) ;
#55099 = CARTESIAN_POINT('Ctrl Pts',(-20.1805416770714,-38.1801674285324,
124.706967424804)) ;
#55100 = CARTESIAN_POINT('Ctrl Pts',(-20.1943496803359,-38.3700017321329,
124.327134832878)) ;
#55101 = CARTESIAN_POINT('Ctrl Pts',(-20.3906137722075,-38.1900126516524,
124.555971632354)) ;
#55102 = CARTESIAN_POINT('Ctrl Pts',(-20.3414292534082,-38.3799924159389,
124.17718516851)) ;
#55103 = CARTESIAN_POINT('Ctrl Pts',(-20.5744646118342,-38.2000033354584,
124.368535624798)) ;
#55104 = CARTESIAN_POINT('Ctrl Pts',(-20.4604073331127,-38.3900302980113,
124.002897673385)) ;
#55105 = CARTESIAN_POINT('Ctrl Pts',(-20.7231886885052,-38.2100412175308,
124.150677424897)) ;
#55106 = CARTESIAN_POINT('Ctrl Pts',(-20.5459739903831,-38.3998746576501,
123.814446734929)) ;
#55107 = CARTESIAN_POINT('Ctrl Pts',(-20.8301490998756,-38.2198855771697,
123.915113415529)) ;
#55108 = CARTESIAN_POINT('Ctrl Pts',(-20.5986469705977,-38.4098595282649,
123.611278948678)) ;
#55109 = CARTESIAN_POINT('Ctrl Pts',(-20.8959919670517,-38.2298704477844,
123.661153850846)) ;
#55110 = CARTESIAN_POINT('Ctrl Pts',(-20.6152674854277,-38.4197988115935,
123.402955218507)) ;
#55111 = CARTESIAN_POINT('Ctrl Pts',(-20.9167692458508,-38.2398097311131,
123.400748772404)) ;
#55112 = CARTESIAN_POINT('Ctrl Pts',(-20.5952009161257,-38.4298394209667,
123.192847662507)) ;
#55113 = CARTESIAN_POINT('Ctrl Pts',(-20.8916876627849,-38.2498503404862,
123.138114322818)) ;
#55114 = CARTESIAN_POINT('Ctrl Pts',(-20.5399668125986,-38.4397242718799,
122.992486933)) ;
#55115 = CARTESIAN_POINT('Ctrl Pts',(-20.8226462973431,-38.2597351913994,
122.887662089178)) ;
#55116 = CARTESIAN_POINT('Ctrl Pts',(-20.4499783459561,-38.4497262280487,
122.802478082637)) ;
#55117 = CARTESIAN_POINT('Ctrl Pts',(-20.710161993943,-38.2697371475682,122.650150261845)) ;
#55118 = CARTESIAN_POINT('Ctrl Pts',(-20.3294778320045,-38.4596448247692,
122.632260562364)) ;
#55119 = CARTESIAN_POINT('Ctrl Pts',(-20.5595370996362,-38.2796557442887,
122.437376954851)) ;
#55120 = CARTESIAN_POINT('Ctrl Pts',(-20.1793517400514,-38.469691646845,122.483728376265)) ;
#55121 = CARTESIAN_POINT('Ctrl Pts',(-20.3718806511006,-38.2897025663645,
122.25171084503)) ;
#55122 = CARTESIAN_POINT('Ctrl Pts',(-20.0087562410276,-38.4795659279577,
122.365386621562)) ;
#55123 = CARTESIAN_POINT('Ctrl Pts',(-20.1586361997854,-38.2995768474772,
122.103781929922)) ;
#55124 = CARTESIAN_POINT('Ctrl Pts',(-19.8168874460983,-38.4896201280023,
122.27679388918)) ;
#55125 = CARTESIAN_POINT('Ctrl Pts',(-19.9188009997021,-38.3096310475218,
121.993039913908)) ;
#55126 = CARTESIAN_POINT('Ctrl Pts',(-19.6157267682506,-38.4995155576375,
122.223611335087)) ;
#55127 = CARTESIAN_POINT('Ctrl Pts',(-19.6673495935341,-38.319526477157,121.926560228881)) ;
#55128 = CARTESIAN_POINT('Ctrl Pts',(-19.4049744065646,-38.5095771859549,
122.2058271605)) ;
#55129 = CARTESIAN_POINT('Ctrl Pts',(-19.4039095755323,-38.3295881054744,
121.904328761278)) ;
#55130 = CARTESIAN_POINT('Ctrl Pts',(-19.198843636696,-38.5194218147848,122.224471407226)) ;
#55131 = CARTESIAN_POINT('Ctrl Pts',(-19.1462446839781,-38.3394327343043,
121.927632919868)) ;
#55132 = CARTESIAN_POINT('Ctrl Pts',(-18.9965533130945,-38.5293818623904,
122.278528162173)) ;
#55133 = CARTESIAN_POINT('Ctrl Pts',(-18.8933810810185,-38.3493927819099,
121.995203018635)) ;
#55134 = CARTESIAN_POINT('Ctrl Pts',(-18.8054118271966,-38.5394201685644,
122.367955384898)) ;
#55135 = CARTESIAN_POINT('Ctrl Pts',(-18.6544538828599,-38.359431088084,122.106985936602)) ;
#55136 = CARTESIAN_POINT('Ctrl Pts',(-18.63527681131,-38.5492934679971,122.48691582821)) ;
#55137 = CARTESIAN_POINT('Ctrl Pts',(-18.4417836191752,-38.3693043875166,
122.255686315576)) ;
#55138 = CARTESIAN_POINT('Ctrl Pts',(-18.4855083632064,-38.5593667295834,
122.636576989724)) ;
#55139 = CARTESIAN_POINT('Ctrl Pts',(-18.2545726342141,-38.3793776491029,
122.442761738762)) ;
#55140 = CARTESIAN_POINT('Ctrl Pts',(-18.3667777956026,-38.5691869555401,
122.805528697943)) ;
#55141 = CARTESIAN_POINT('Ctrl Pts',(-18.1061577774749,-38.3891978750596,
122.653952115925)) ;
#55142 = CARTESIAN_POINT('Ctrl Pts',(-18.2767515118799,-38.5792660194796,
122.997287213327)) ;
#55143 = CARTESIAN_POINT('Ctrl Pts',(-17.9936243508535,-38.3992769389991,
122.893649468744)) ;
#55144 = CARTESIAN_POINT('Ctrl Pts',(-18.2225229813274,-38.5891161094994,
123.197198324746)) ;
#55145 = CARTESIAN_POINT('Ctrl Pts',(-17.9258375542978,-38.4091270290189,
123.143539427557)) ;
#55146 = CARTESIAN_POINT('Ctrl Pts',(-18.2032956686347,-38.5991948631132,
123.408157950958)) ;
#55147 = CARTESIAN_POINT('Ctrl Pts',(-17.9018026836596,-38.4192057826327,
123.407238410019)) ;
#55148 = CARTESIAN_POINT('Ctrl Pts',(-18.2203875577578,-38.6090163303726,
123.613973329019)) ;
#55149 = CARTESIAN_POINT('Ctrl Pts',(-17.9231669693498,-38.4290272498922,
123.664509279114)) ;
#55150 = CARTESIAN_POINT('Ctrl Pts',(-18.2739238887591,-38.6190819287303,
123.818650277656)) ;
#55151 = CARTESIAN_POINT('Ctrl Pts',(-17.9900867205332,-38.4390928482498,
123.920355248538)) ;
#55152 = CARTESIAN_POINT('Ctrl Pts',(-18.3608489444241,-38.628984584505,124.007876019705)) ;
#55153 = CARTESIAN_POINT('Ctrl Pts',(-18.098742864272,-38.4489955040245,124.156888509169)) ;
#55154 = CARTESIAN_POINT('Ctrl Pts',(-18.4809742235416,-38.6390354103346,
124.181656276088)) ;
#55155 = CARTESIAN_POINT('Ctrl Pts',(-18.2488988279935,-38.4590463298541,
124.37411393973)) ;
#55156 = CARTESIAN_POINT('Ctrl Pts',(-18.6267574232004,-38.6489096146735,
124.329501799845)) ;
#55157 = CARTESIAN_POINT('Ctrl Pts',(-18.4311282811755,-38.468920534193,124.558922029352)) ;
#55158 = CARTESIAN_POINT('Ctrl Pts',(-18.7993133903288,-38.6589820647126,
124.452162400167)) ;
#55159 = CARTESIAN_POINT('Ctrl Pts',(-18.6468225999744,-38.4789929842321,
124.712247945198)) ;
#55160 = CARTESIAN_POINT('Ctrl Pts',(-18.9859137942603,-38.6688110814861,
124.541017706794)) ;
#55161 = CARTESIAN_POINT('Ctrl Pts',(-18.8800743167086,-38.4888220010056,
124.823318123798)) ;
#55162 = CARTESIAN_POINT('Ctrl Pts',(-19.1897774494704,-38.6788779274009,
124.597717051206)) ;
#55163 = CARTESIAN_POINT('Ctrl Pts',(-19.1349034186217,-38.4988888469204,
124.894192497998)) ;
#55164 = CARTESIAN_POINT('Ctrl Pts',(-19.3967662896624,-38.6887680987027,
124.617671141115)) ;
#55165 = CARTESIAN_POINT('Ctrl Pts',(-19.3936404772035,-38.5087790182222,
124.919135574794)) ;
#55166 = CARTESIAN_POINT('Ctrl Pts',(-19.6062117856198,-38.6987602923265,
124.601677520649)) ;
#55167 = CARTESIAN_POINT('Ctrl Pts',(-19.6554475745954,-38.518771211846,124.899143715599)) ;
#55168 = CARTESIAN_POINT('Ctrl Pts',(-19.8090578521169,-38.7087231029499,
124.549518835879)) ;
#55169 = CARTESIAN_POINT('Ctrl Pts',(-19.9090056650938,-38.5287340224695,
124.83394550148)) ;
#55170 = CARTESIAN_POINT('Ctrl Pts',(-19.9988839578665,-38.7186273757934,
124.463912950195)) ;
#55171 = CARTESIAN_POINT('Ctrl Pts',(-20.1462891749534,-38.5386382953129,
124.726937805379)) ;
#55172 = CARTESIAN_POINT('Ctrl Pts',(-20.1735373576463,-38.728687867598,124.344670095455)) ;
#55173 = CARTESIAN_POINT('Ctrl Pts',(-20.3646057035926,-38.5486987871175,
124.577884540357)) ;
#55174 = CARTESIAN_POINT('Ctrl Pts',(-20.3217496628908,-38.7385281992703,
124.200302181168)) ;
#55175 = CARTESIAN_POINT('Ctrl Pts',(-20.54987215141,-38.5585391187898,124.397423633177)) ;
#55176 = CARTESIAN_POINT('Ctrl Pts',(-20.4455536404309,-38.7485912453621,
124.028786981094)) ;
#55177 = CARTESIAN_POINT('Ctrl Pts',(-20.7046268370077,-38.5686021648816,
124.183029887367)) ;
#55178 = CARTESIAN_POINT('Ctrl Pts',(-20.5360148595755,-38.7584853010572,
123.841460701052)) ;
#55179 = CARTESIAN_POINT('Ctrl Pts',(-20.8177037945612,-38.5784962205767,
123.948871113701)) ;
#55180 = CARTESIAN_POINT('Ctrl Pts',(-20.5933924658413,-38.7684280013801,
123.640487605806)) ;
#55181 = CARTESIAN_POINT('Ctrl Pts',(-20.8894257460655,-38.5884389208997,
123.697654055574)) ;
#55182 = CARTESIAN_POINT('Ctrl Pts',(-20.6151860212168,-38.7784337423077,
123.431245299403)) ;
#55183 = CARTESIAN_POINT('Ctrl Pts',(-20.9166674417384,-38.5984446618273,
123.436101061359)) ;
#55184 = CARTESIAN_POINT('Ctrl Pts',(-20.6000592508299,-38.7884546528233,
123.221122882198)) ;
#55185 = CARTESIAN_POINT('Ctrl Pts',(-20.8977588229699,-38.6084655723428,
123.173448091031)) ;
#55186 = CARTESIAN_POINT('Ctrl Pts',(-20.5495758365941,-38.7983453882732,
123.0194036364)) ;
#55187 = CARTESIAN_POINT('Ctrl Pts',(-20.8346540512189,-38.6183563077928,
122.921298084057)) ;
#55188 = CARTESIAN_POINT('Ctrl Pts',(-20.4642602817029,-38.8083369290021,
122.827465431094)) ;
#55189 = CARTESIAN_POINT('Ctrl Pts',(-20.7280091758248,-38.6283478485216,
122.681375284284)) ;
#55190 = CARTESIAN_POINT('Ctrl Pts',(-20.3473737278901,-38.8182847894237,
122.654045824063)) ;
#55191 = CARTESIAN_POINT('Ctrl Pts',(-20.5819003600427,-38.6382957089433,
122.464600480947)) ;
#55192 = CARTESIAN_POINT('Ctrl Pts',(-20.202456742999,-38.8282314586101,122.503277801019)) ;
#55193 = CARTESIAN_POINT('Ctrl Pts',(-20.4007533562876,-38.6482423781296,
122.276140396703)) ;
#55194 = CARTESIAN_POINT('Ctrl Pts',(-20.0317199746376,-38.8382795347457,
122.378903058221)) ;
#55195 = CARTESIAN_POINT('Ctrl Pts',(-20.1873323483246,-38.6582904542652,
122.120672459441)) ;
#55196 = CARTESIAN_POINT('Ctrl Pts',(-19.8458354362141,-38.8481271327513,
122.287756233757)) ;
#55197 = CARTESIAN_POINT('Ctrl Pts',(-19.9549752002144,-38.6681380522708,
122.006738756022)) ;
#55198 = CARTESIAN_POINT('Ctrl Pts',(-19.6448376579705,-38.8580888558358,
122.228975330459)) ;
#55199 = CARTESIAN_POINT('Ctrl Pts',(-19.7037273294594,-38.6780997753553,
121.933263220513)) ;
#55200 = CARTESIAN_POINT('Ctrl Pts',(-19.4352361415482,-38.8681174909188,
122.206096194231)) ;
#55201 = CARTESIAN_POINT('Ctrl Pts',(-19.4417254602137,-38.6881284104383,
121.904664952519)) ;
#55202 = CARTESIAN_POINT('Ctrl Pts',(-19.2273465752442,-38.8780277992368,
122.219725256983)) ;
#55203 = CARTESIAN_POINT('Ctrl Pts',(-19.1818626712833,-38.6980387187563,
121.921702009087)) ;
#55204 = CARTESIAN_POINT('Ctrl Pts',(-19.0243342885466,-38.8879626963727,
122.26883883605)) ;
#55205 = CARTESIAN_POINT('Ctrl Pts',(-18.9280968781403,-38.7079736158922,
121.983094997283)) ;
#55206 = CARTESIAN_POINT('Ctrl Pts',(-18.8309772013695,-38.8980037793153,
122.353523961238)) ;
#55207 = CARTESIAN_POINT('Ctrl Pts',(-18.686401014824,-38.7180146988348,122.088952068099)) ;
#55208 = CARTESIAN_POINT('Ctrl Pts',(-18.6578590680997,-38.9078911221435,
122.468595150492)) ;
#55209 = CARTESIAN_POINT('Ctrl Pts',(-18.4700029593095,-38.727902041663,122.232792348651)) ;
#55210 = CARTESIAN_POINT('Ctrl Pts',(-18.5055317513843,-38.9178826370828,
122.613211351364)) ;
#55211 = CARTESIAN_POINT('Ctrl Pts',(-18.2795943516708,-38.7378935566024,
122.413563464107)) ;
#55212 = CARTESIAN_POINT('Ctrl Pts',(-18.3811911630624,-38.9278340282793,
122.781466926608)) ;
#55213 = CARTESIAN_POINT('Ctrl Pts',(-18.124169074107,-38.7478449477989,122.623883938995)) ;
#55214 = CARTESIAN_POINT('Ctrl Pts',(-18.2878097045155,-38.9377665616119,
122.968234846333)) ;
#55215 = CARTESIAN_POINT('Ctrl Pts',(-18.0074429395974,-38.7577774811314,
122.857344924751)) ;
#55216 = CARTESIAN_POINT('Ctrl Pts',(-18.2278106534503,-38.9477637195114,
123.1696520482)) ;
#55217 = CARTESIAN_POINT('Ctrl Pts',(-17.9324451629911,-38.7677746390309,
123.109116894478)) ;
#55218 = CARTESIAN_POINT('Ctrl Pts',(-18.2036416355779,-38.9577487296749,
123.378205341425)) ;
#55219 = CARTESIAN_POINT('Ctrl Pts',(-17.902235014903,-38.7777596491944,123.369808873094)) ;
#55220 = CARTESIAN_POINT('Ctrl Pts',(-18.2164291819651,-38.9677915562447,
123.588920968376)) ;
#55221 = CARTESIAN_POINT('Ctrl Pts',(-17.9182204759992,-38.7878024757642,
123.63320316215)) ;
#55222 = CARTESIAN_POINT('Ctrl Pts',(-18.2641206916243,-38.9776217905496,
123.790038485593)) ;
#55223 = CARTESIAN_POINT('Ctrl Pts',(-17.9778363798766,-38.7976327100692,
123.884601181675)) ;
#55224 = CARTESIAN_POINT('Ctrl Pts',(-18.3479385843405,-38.9876978157843,
123.984532944223)) ;
#55225 = CARTESIAN_POINT('Ctrl Pts',(-18.0826097271677,-38.8077087353038,
124.12771836113)) ;
#55226 = CARTESIAN_POINT('Ctrl Pts',(-18.4616277736015,-38.9975500522752,
124.157720560445)) ;
#55227 = CARTESIAN_POINT('Ctrl Pts',(-18.2247229697952,-38.8175609717947,
124.344203206761)) ;
#55228 = CARTESIAN_POINT('Ctrl Pts',(-18.6066621317061,-39.0076232587093,
124.31198450881)) ;
#55229 = CARTESIAN_POINT('Ctrl Pts',(-18.4060166291239,-38.8276341782288,
124.537031921043)) ;
#55230 = CARTESIAN_POINT('Ctrl Pts',(-18.7724492303032,-39.0174647682165,
124.435789163625)) ;
#55231 = CARTESIAN_POINT('Ctrl Pts',(-18.6132523457077,-38.837475687736,124.691787453299)) ;
#55232 = CARTESIAN_POINT('Ctrl Pts',(-18.9590824114606,-39.0274257149963,
124.530751648875)) ;
#55233 = CARTESIAN_POINT('Ctrl Pts',(-18.8465449134313,-38.8474366345158,
124.810489310477)) ;
#55234 = CARTESIAN_POINT('Ctrl Pts',(-19.1610387527157,-39.0374635437963,
124.591933966622)) ;
#55235 = CARTESIAN_POINT('Ctrl Pts',(-19.0989906357257,-38.8574744633158,
124.886965770445)) ;
#55236 = CARTESIAN_POINT('Ctrl Pts',(-19.3671221533313,-39.0473378535508,
124.617096782991)) ;
#55237 = CARTESIAN_POINT('Ctrl Pts',(-19.3565960865102,-38.8673487730703,
124.918417832492)) ;
#55238 = CARTESIAN_POINT('Ctrl Pts',(-19.5784931233021,-39.0574075512239,
124.605867995762)) ;
#55239 = CARTESIAN_POINT('Ctrl Pts',(-19.6208093649066,-38.8774184707435,
124.904380279425)) ;
#55240 = CARTESIAN_POINT('Ctrl Pts',(-19.7799321898415,-39.0672410225113,
124.55932535313)) ;
#55241 = CARTESIAN_POINT('Ctrl Pts',(-19.8726090819343,-38.8872519420309,
124.846200104138)) ;
#55242 = CARTESIAN_POINT('Ctrl Pts',(-19.9742453524244,-39.0772706690413,
124.477468158144)) ;
#55243 = CARTESIAN_POINT('Ctrl Pts',(-20.1154997479825,-38.8972815885608,
124.74387696496)) ;
#55244 = CARTESIAN_POINT('Ctrl Pts',(-20.1511369807371,-39.0873051833686,
124.36251502401)) ;
#55245 = CARTESIAN_POINT('Ctrl Pts',(-20.3366133293652,-38.9073161028882,
124.600184240841)) ;
#55246 = CARTESIAN_POINT('Ctrl Pts',(-20.3025021754356,-39.0971304688395,
124.221961302064)) ;
#55247 = CARTESIAN_POINT('Ctrl Pts',(-20.5258195612179,-38.9171413883591,
124.424489905095)) ;
#55248 = CARTESIAN_POINT('Ctrl Pts',(-20.4297743163725,-39.1071347103881,
124.05455039433)) ;
#55249 = CARTESIAN_POINT('Ctrl Pts',(-20.6849082650607,-38.9271456299076,
124.21522504281)) ;
#55250 = CARTESIAN_POINT('Ctrl Pts',(-20.5257881932866,-39.1171173554672,
123.867889590297)) ;
#55251 = CARTESIAN_POINT('Ctrl Pts',(-20.8049240328739,-38.9371282749867,
123.98189798355)) ;
#55252 = CARTESIAN_POINT('Ctrl Pts',(-20.588074926157,-39.1271625525587,123.666125982417)) ;
#55253 = CARTESIAN_POINT('Ctrl Pts',(-20.8827806721499,-38.9471734720782,
123.729693087469)) ;
#55254 = CARTESIAN_POINT('Ctrl Pts',(-20.6141505417572,-39.1369856683188,
123.461258677549)) ;
#55255 = CARTESIAN_POINT('Ctrl Pts',(-20.9153734466188,-38.9569965878383,
123.473607472972)) ;
#55256 = CARTESIAN_POINT('Ctrl Pts',(-20.60457754197,-39.1470202801191,123.250519610856)) ;
#55257 = CARTESIAN_POINT('Ctrl Pts',(-20.9034051258679,-38.9670311996386,
123.210183840075)) ;
#55258 = CARTESIAN_POINT('Ctrl Pts',(-20.5580262468952,-39.1570452888922,
123.044960994217)) ;
#55259 = CARTESIAN_POINT('Ctrl Pts',(-20.8452141571095,-38.9770562084118,
122.953236014132)) ;
#55260 = CARTESIAN_POINT('Ctrl Pts',(-20.478316885892,-39.1668972137338,122.853791086259)) ;
#55261 = CARTESIAN_POINT('Ctrl Pts',(-20.7455751868361,-38.9869081332533,
122.714273478648)) ;
#55262 = CARTESIAN_POINT('Ctrl Pts',(-20.3653360181163,-39.1768881520565,
122.676754747224)) ;
#55263 = CARTESIAN_POINT('Ctrl Pts',(-20.6043472153885,-38.996899071576,122.492979055613)) ;
#55264 = CARTESIAN_POINT('Ctrl Pts',(-20.2244345622947,-39.186806137203,122.523026316099)) ;
#55265 = CARTESIAN_POINT('Ctrl Pts',(-20.4282184152407,-39.0068170567225,
122.300819554093)) ;
#55266 = CARTESIAN_POINT('Ctrl Pts',(-20.0572079878956,-39.1968342380985,
122.394673439318)) ;
#55267 = CARTESIAN_POINT('Ctrl Pts',(-20.2191839000679,-39.016845157618,122.140380206169)) ;
#55268 = CARTESIAN_POINT('Ctrl Pts',(-19.8729210552735,-39.2067194790411,
122.298607224345)) ;
#55269 = CARTESIAN_POINT('Ctrl Pts',(-19.9888235634407,-39.0267303985606,
122.020299045186)) ;
#55270 = CARTESIAN_POINT('Ctrl Pts',(-19.6728247514948,-39.2167085920077,
122.234848345753)) ;
#55271 = CARTESIAN_POINT('Ctrl Pts',(-19.7387023265823,-39.0367195115272,
121.940602617531)) ;
#55272 = CARTESIAN_POINT('Ctrl Pts',(-19.4635439074029,-39.2267506563485,
122.207112896328)) ;
#55273 = CARTESIAN_POINT('Ctrl Pts',(-19.4771010747328,-39.046761575868,121.905935512341)) ;
#55274 = CARTESIAN_POINT('Ctrl Pts',(-19.2570678726038,-39.236579857753,122.215554269047)) ;
#55275 = CARTESIAN_POINT('Ctrl Pts',(-19.2190051557527,-39.0565907772725,
121.916489575375)) ;
#55276 = CARTESIAN_POINT('Ctrl Pts',(-19.0514789396674,-39.2465866985112,
122.260060325551)) ;
#55277 = CARTESIAN_POINT('Ctrl Pts',(-18.9620194272015,-39.0665976180307,
121.972124528351)) ;
#55278 = CARTESIAN_POINT('Ctrl Pts',(-18.857109213024,-39.2565742227031,122.33957226792)) ;
#55279 = CARTESIAN_POINT('Ctrl Pts',(-18.7190580246023,-39.0765851422226,
122.071516725931)) ;
#55280 = CARTESIAN_POINT('Ctrl Pts',(-18.6788723961599,-39.2666038685117,
122.452193066981)) ;
#55281 = CARTESIAN_POINT('Ctrl Pts',(-18.4962632861033,-39.0866147880312,
122.212294698753)) ;
#55282 = CARTESIAN_POINT('Ctrl Pts',(-18.5251202819395,-39.2764778992504,
122.591691852542)) ;
#55283 = CARTESIAN_POINT('Ctrl Pts',(-18.3040742601302,-39.09648881877,122.386670420962)) ;
#55284 = CARTESIAN_POINT('Ctrl Pts',(-18.3961396998256,-39.2864772221145,
122.757647081456)) ;
#55285 = CARTESIAN_POINT('Ctrl Pts',(-18.1428504125895,-39.1064881416341,
122.594116058495)) ;
#55286 = CARTESIAN_POINT('Ctrl Pts',(-18.2985886975645,-39.2963880576901,
122.941797700532)) ;
#55287 = CARTESIAN_POINT('Ctrl Pts',(-18.0209136489367,-39.1163989772096,
122.824305926484)) ;
#55288 = CARTESIAN_POINT('Ctrl Pts',(-18.2336609868071,-39.3064423056642,
123.142915425112)) ;
#55289 = CARTESIAN_POINT('Ctrl Pts',(-17.939756418394,-39.1264532251837,123.075703741518)) ;
#55290 = CARTESIAN_POINT('Ctrl Pts',(-18.2049530968866,-39.3163010499269,
123.348215710506)) ;
#55291 = CARTESIAN_POINT('Ctrl Pts',(-17.9038739771922,-39.1363119694464,
123.332330097251)) ;
#55292 = CARTESIAN_POINT('Ctrl Pts',(-18.2123561541688,-39.3263691359999,
123.559718460866)) ;
#55293 = CARTESIAN_POINT('Ctrl Pts',(-17.9131303554343,-39.1463800555194,
123.596708290332)) ;
#55294 = CARTESIAN_POINT('Ctrl Pts',(-18.2554666856692,-39.3362246191794,
123.762394729141)) ;
#55295 = CARTESIAN_POINT('Ctrl Pts',(-17.9670211521301,-39.1562355386989,
123.850053708721)) ;
#55296 = CARTESIAN_POINT('Ctrl Pts',(-18.333618279946,-39.3462194649736,123.957436253623)) ;
#55297 = CARTESIAN_POINT('Ctrl Pts',(-18.0647131558998,-39.1662303844931,
124.093854715397)) ;
#55298 = CARTESIAN_POINT('Ctrl Pts',(-18.4452442598356,-39.3562507606361,
124.136365747188)) ;
#55299 = CARTESIAN_POINT('Ctrl Pts',(-18.2042478279912,-39.1762616801557,
124.317515212328)) ;
#55300 = CARTESIAN_POINT('Ctrl Pts',(-18.5836826690354,-39.366117303926,124.290842760862)) ;
#55301 = CARTESIAN_POINT('Ctrl Pts',(-18.3772981540665,-39.1861282234455,
124.510610102778)) ;
#55302 = CARTESIAN_POINT('Ctrl Pts',(-18.748604585584,-39.3761046996894,124.420751361441)) ;
#55303 = CARTESIAN_POINT('Ctrl Pts',(-18.5834523132856,-39.1961156192089,
124.67299381361)) ;
#55304 = CARTESIAN_POINT('Ctrl Pts',(-18.9327894876098,-39.3860497404194,
124.519754705833)) ;
#55305 = CARTESIAN_POINT('Ctrl Pts',(-18.8136849280441,-39.2060606599389,
124.796745724835)) ;
#55306 = CARTESIAN_POINT('Ctrl Pts',(-19.1333404381493,-39.3960942466361,
124.585800268565)) ;
#55307 = CARTESIAN_POINT('Ctrl Pts',(-19.0643744384591,-39.2161051661556,
124.879300116025)) ;
#55308 = CARTESIAN_POINT('Ctrl Pts',(-19.3385607919778,-39.4059577527734,
124.615667658985)) ;
#55309 = CARTESIAN_POINT('Ctrl Pts',(-19.3209006976824,-39.2259686722929,
124.916631731361)) ;
#55310 = CARTESIAN_POINT('Ctrl Pts',(-19.5485278972259,-39.4159506136095,
124.609740631774)) ;
#55311 = CARTESIAN_POINT('Ctrl Pts',(-19.5833595972731,-39.235961533129,124.909220187346)) ;
#55312 = CARTESIAN_POINT('Ctrl Pts',(-19.7529825851974,-39.4258768073284,
124.567812438431)) ;
#55313 = CARTESIAN_POINT('Ctrl Pts',(-19.8389276222592,-39.2458877268479,
124.85680719715)) ;
#55314 = CARTESIAN_POINT('Ctrl Pts',(-19.9488284655848,-39.435895733361,124.490360997072)) ;
#55315 = CARTESIAN_POINT('Ctrl Pts',(-20.0837340013322,-39.2559066528805,
124.759990302527)) ;
#55316 = CARTESIAN_POINT('Ctrl Pts',(-20.126540851108,-39.4458107327286,124.381363000925)) ;
#55317 = CARTESIAN_POINT('Ctrl Pts',(-20.3058732170671,-39.2658216522481,
124.62374032262)) ;
#55318 = CARTESIAN_POINT('Ctrl Pts',(-20.2847556242028,-39.4558655042859,
124.241221421377)) ;
#55319 = CARTESIAN_POINT('Ctrl Pts',(-20.5036398439855,-39.2758764238054,
124.448561262126)) ;
#55320 = CARTESIAN_POINT('Ctrl Pts',(-20.4138101110339,-39.4657244665834,
124.079002697982)) ;
#55321 = CARTESIAN_POINT('Ctrl Pts',(-20.6649559415589,-39.285735386103,124.245785908766)) ;
#55322 = CARTESIAN_POINT('Ctrl Pts',(-20.514413173183,-39.4757187104213,123.894581207319)) ;
#55323 = CARTESIAN_POINT('Ctrl Pts',(-20.7907073339488,-39.2957296299408,
124.015257630094)) ;
#55324 = CARTESIAN_POINT('Ctrl Pts',(-20.5811176261202,-39.4856439398455,
123.69683639536)) ;
#55325 = CARTESIAN_POINT('Ctrl Pts',(-20.8740852788276,-39.305654859365,123.768075589586)) ;
#55326 = CARTESIAN_POINT('Ctrl Pts',(-20.6127981685667,-39.495671903737,123.488439172828)) ;
#55327 = CARTESIAN_POINT('Ctrl Pts',(-20.9136831803521,-39.3156828232565,
123.507578576401)) ;
#55328 = CARTESIAN_POINT('Ctrl Pts',(-20.6080961840771,-39.5055581633674,
123.280620724186)) ;
#55329 = CARTESIAN_POINT('Ctrl Pts',(-20.9078028796021,-39.3255690828869,
123.24780545798)) ;
#55330 = CARTESIAN_POINT('Ctrl Pts',(-20.5669027528603,-39.5155899264452,
123.073819312021)) ;
#55331 = CARTESIAN_POINT('Ctrl Pts',(-20.8563083057196,-39.3356008459647,
122.989304179159)) ;
#55332 = CARTESIAN_POINT('Ctrl Pts',(-20.4917344516677,-39.5254715527393,
122.880112689592)) ;
#55333 = CARTESIAN_POINT('Ctrl Pts',(-20.7623452756417,-39.3454824722589,
122.747171858432)) ;
#55334 = CARTESIAN_POINT('Ctrl Pts',(-20.3821947597893,-39.5355333222255,
122.69919029706)) ;
#55335 = CARTESIAN_POINT('Ctrl Pts',(-20.6254182000016,-39.355544241745,122.521020259929)) ;
#55336 = CARTESIAN_POINT('Ctrl Pts',(-20.2457369593962,-39.545391189721,122.543178844289)) ;
#55337 = CARTESIAN_POINT('Ctrl Pts',(-20.4548438166612,-39.3654021092405,
122.326007789972)) ;
#55338 = CARTESIAN_POINT('Ctrl Pts',(-20.0824035138093,-39.5553828148383,
122.411136991431)) ;
#55339 = CARTESIAN_POINT('Ctrl Pts',(-20.2506752049855,-39.3753937343579,
122.160957633179)) ;
#55340 = CARTESIAN_POINT('Ctrl Pts',(-19.8995811867269,-39.5653196139466,
122.310034299086)) ;
#55341 = CARTESIAN_POINT('Ctrl Pts',(-20.0221459359936,-39.3853305334661,
122.034581725354)) ;
#55342 = CARTESIAN_POINT('Ctrl Pts',(-19.7010155069493,-39.5753104435039,
122.241558693215)) ;
#55343 = CARTESIAN_POINT('Ctrl Pts',(-19.7739378813006,-39.3953213630234,
121.948989845614)) ;
#55344 = CARTESIAN_POINT('Ctrl Pts',(-19.492862253122,-39.5853336792171,122.208735174446)) ;
#55345 = CARTESIAN_POINT('Ctrl Pts',(-19.5137457792946,-39.4053445987366,
121.907963203133)) ;
#55346 = CARTESIAN_POINT('Ctrl Pts',(-19.2848447608836,-39.5952300272463,
122.212328557573)) ;
#55347 = CARTESIAN_POINT('Ctrl Pts',(-19.2537240353336,-39.4152409467658,
121.91245773756)) ;
#55348 = CARTESIAN_POINT('Ctrl Pts',(-19.0785873856562,-39.6052195897488,
122.251922424187)) ;
#55349 = CARTESIAN_POINT('Ctrl Pts',(-18.9959028450038,-39.4252305092683,
121.961952758409)) ;
#55350 = CARTESIAN_POINT('Ctrl Pts',(-18.8815126411,-39.6152598974333,122.327498065648)) ;
#55351 = CARTESIAN_POINT('Ctrl Pts',(-18.7495601439939,-39.4352708169529,
122.05642510042)) ;
#55352 = CARTESIAN_POINT('Ctrl Pts',(-18.7038945149076,-39.6251022007805,
122.433676485987)) ;
#55353 = CARTESIAN_POINT('Ctrl Pts',(-18.5275396487683,-39.4451131203,122.189149904719)) ;
#55354 = CARTESIAN_POINT('Ctrl Pts',(-18.5443823308829,-39.6351259090596,
122.571330211097)) ;
#55355 = CARTESIAN_POINT('Ctrl Pts',(-18.328149190755,-39.4551368285791,122.361220908042)) ;
#55356 = CARTESIAN_POINT('Ctrl Pts',(-18.3685442000014,-39.6483480865273,
122.786691141863)) ;
#55357 = CARTESIAN_POINT('Ctrl Pts',(-18.1083641387058,-39.4683590060468,
122.630415698237)) ;
#55358 = CARTESIAN_POINT('Ctrl Pts',(-18.2520900531708,-39.6616406715866,
123.044166683935)) ;
#55359 = CARTESIAN_POINT('Ctrl Pts',(-17.9628051139688,-39.4816515911061,
122.952220149181)) ;
#55360 = CARTESIAN_POINT('Ctrl Pts',(-18.2067947635487,-39.6749255275082,
123.319772585123)) ;
#55361 = CARTESIAN_POINT('Ctrl Pts',(-17.9061735338517,-39.4949364470277,
123.296785705757)) ;
#55362 = CARTESIAN_POINT('Ctrl Pts',(-18.2090712913271,-39.684897754681,123.529386284599)) ;
#55363 = CARTESIAN_POINT('Ctrl Pts',(-17.9090249685685,-39.5049086742005,
123.558791097675)) ;
#55364 = CARTESIAN_POINT('Ctrl Pts',(-18.2471189349561,-39.69480637112,123.734216590928)) ;
#55365 = CARTESIAN_POINT('Ctrl Pts',(-17.9565864887432,-39.5148172906395,
123.814831513913)) ;
#55366 = CARTESIAN_POINT('Ctrl Pts',(-18.3212835409877,-39.7048595765037,
123.932106036806)) ;
#55367 = CARTESIAN_POINT('Ctrl Pts',(-18.049293676017,-39.5248704960232,124.06219099881)) ;
#55368 = CARTESIAN_POINT('Ctrl Pts',(-18.4265731448462,-39.714724710264,124.110805164923)) ;
#55369 = CARTESIAN_POINT('Ctrl Pts',(-18.1809125136437,-39.5347356297835,
124.285566479099)) ;
#55370 = CARTESIAN_POINT('Ctrl Pts',(-18.6083337458461,-39.7280637678903,
124.324363825404)) ;
#55371 = CARTESIAN_POINT('Ctrl Pts',(-18.408091089116,-39.5480746874098,124.552496993476)) ;
#55372 = CARTESIAN_POINT('Ctrl Pts',(-18.8983167375147,-39.7446329552234,
124.524458458027)) ;
#55373 = CARTESIAN_POINT('Ctrl Pts',(-18.7706176278326,-39.564643874743,124.802631869108)) ;
#55374 = CARTESIAN_POINT('Ctrl Pts',(-19.2406669716427,-39.7612780950745,
124.61423815662)) ;
#55375 = CARTESIAN_POINT('Ctrl Pts',(-19.1984775012309,-39.581289014594,124.914837427828)) ;
#55376 = CARTESIAN_POINT('Ctrl Pts',(-19.5196867167119,-39.7745503975479,
124.61271922313)) ;
#55377 = CARTESIAN_POINT('Ctrl Pts',(-19.5473160626287,-39.5945613170674,
124.912945050873)) ;
#55378 = CARTESIAN_POINT('Ctrl Pts',(-19.7261653450185,-39.7845313609955,
124.575425604287)) ;
#55379 = CARTESIAN_POINT('Ctrl Pts',(-19.8054003622426,-39.604542280515,124.866324423839)) ;
#55380 = CARTESIAN_POINT('Ctrl Pts',(-19.9223292162796,-39.7944731930648,
124.503237795506)) ;
#55381 = CARTESIAN_POINT('Ctrl Pts',(-20.0506098850726,-39.6144841125843,
124.776085831231)) ;
#55382 = CARTESIAN_POINT('Ctrl Pts',(-20.1643724086472,-39.8077927622802,
124.362474521717)) ;
#55383 = CARTESIAN_POINT('Ctrl Pts',(-20.3531494020375,-39.6278036817997,
124.600140542085)) ;
#55384 = CARTESIAN_POINT('Ctrl Pts',(-20.412637735221,-39.824322917213,124.113575614291)) ;
#55385 = CARTESIAN_POINT('Ctrl Pts',(-20.6634916789973,-39.6443338367325,
124.28900205587)) ;
#55386 = CARTESIAN_POINT('Ctrl Pts',(-20.5921614259415,-39.8443446427051,
123.727677934125)) ;
#55387 = CARTESIAN_POINT('Ctrl Pts',(-20.8878880490218,-39.6643555622246,
123.806632140342)) ;
#55388 = CARTESIAN_POINT('Ctrl Pts',(-20.62909002806,-39.8641560393119,123.307952932077)) ;
#55389 = CARTESIAN_POINT('Ctrl Pts',(-20.9340458412992,-39.6841669588314,
123.281975948005)) ;
#55390 = CARTESIAN_POINT('Ctrl Pts',(-20.5203568846511,-39.8841412880207,
122.897261125277)) ;
#55391 = CARTESIAN_POINT('Ctrl Pts',(-20.7981256342363,-39.7041522075403,
122.768612564849)) ;
#55392 = CARTESIAN_POINT('Ctrl Pts',(-20.2787761694729,-39.9040353506567,
122.549947579521)) ;
#55393 = CARTESIAN_POINT('Ctrl Pts',(-20.4961474224209,-39.7240462701762,
122.334473379661)) ;
#55394 = CARTESIAN_POINT('Ctrl Pts',(-19.9329494436863,-39.9239670298303,
122.304988298998)) ;
#55395 = CARTESIAN_POINT('Ctrl Pts',(-20.0638627447484,-39.7439779493498,
122.028277249593)) ;
#55396 = CARTESIAN_POINT('Ctrl Pts',(-19.5235438881534,-39.9439310843023,
122.192828842814)) ;
#55397 = CARTESIAN_POINT('Ctrl Pts',(-19.5521053130937,-39.7639420038218,
121.888081012705)) ;
#55398 = CARTESIAN_POINT('Ctrl Pts',(-19.1021579397527,-39.9638119860652,
122.226651373111)) ;
#55399 = CARTESIAN_POINT('Ctrl Pts',(-19.0253744539521,-39.7838229055847,
121.930361826918)) ;
#55400 = CARTESIAN_POINT('Ctrl Pts',(-18.7163649280739,-39.9837506476736,
122.402373200005)) ;
#55401 = CARTESIAN_POINT('Ctrl Pts',(-18.5431348408587,-39.8037615671931,
122.150015941179)) ;
#55402 = CARTESIAN_POINT('Ctrl Pts',(-18.4142773535418,-40.0036471729289,
122.698534548937)) ;
#55403 = CARTESIAN_POINT('Ctrl Pts',(-18.1655278031791,-39.8236580924484,
122.520218221222)) ;
#55404 = CARTESIAN_POINT('Ctrl Pts',(-18.2307652703842,-40.0235422113832,
123.07969577924)) ;
#55405 = CARTESIAN_POINT('Ctrl Pts',(-17.9361396475794,-39.8435531309027,
122.996669054395)) ;
#55406 = CARTESIAN_POINT('Ctrl Pts',(-18.1882574040753,-40.0435060346893,
123.502015421763)) ;
#55407 = CARTESIAN_POINT('Ctrl Pts',(-17.8830061323076,-39.8635169542088,
123.524568225162)) ;
#55408 = CARTESIAN_POINT('Ctrl Pts',(-18.29165985598,-40.0633801588183,123.911779372075)) ;
#55409 = CARTESIAN_POINT('Ctrl Pts',(-18.0122595315461,-39.8833910783379,
124.036771136699)) ;
#55410 = CARTESIAN_POINT('Ctrl Pts',(-18.5295568784576,-40.0833552345456,
124.263648018593)) ;
#55411 = CARTESIAN_POINT('Ctrl Pts',(-18.3096308449976,-39.9033661540651,
124.476606505177)) ;
#55412 = CARTESIAN_POINT('Ctrl Pts',(-18.873213806286,-40.1033088039022,124.512438604021)) ;
#55413 = CARTESIAN_POINT('Ctrl Pts',(-18.7392016864746,-39.9233197234217,
124.787593898658)) ;
#55414 = CARTESIAN_POINT('Ctrl Pts',(-19.2785655362842,-40.12314671409,124.629117591118)) ;
#55415 = CARTESIAN_POINT('Ctrl Pts',(-19.2458886960496,-39.9431576336096,
124.933442272178)) ;
#55416 = CARTESIAN_POINT('Ctrl Pts',(-19.7023551259677,-40.143122542661,124.600718350869)) ;
#55417 = CARTESIAN_POINT('Ctrl Pts',(-19.775625440603,-39.9631334621805,124.897944226838)) ;
#55418 = CARTESIAN_POINT('Ctrl Pts',(-20.0896769698093,-40.1630405873712,
124.429488132005)) ;
#55419 = CARTESIAN_POINT('Ctrl Pts',(-20.2597769713751,-39.9830515068908,
124.683907753037)) ;
#55420 = CARTESIAN_POINT('Ctrl Pts',(-20.3954104326446,-40.1829108331589,
124.137764071626)) ;
#55421 = CARTESIAN_POINT('Ctrl Pts',(-20.6419438142498,-40.0029217526784,
124.319255201606)) ;
#55422 = CARTESIAN_POINT('Ctrl Pts',(-20.5842765338552,-40.2029598362585,
123.755710496064)) ;
#55423 = CARTESIAN_POINT('Ctrl Pts',(-20.8780281938708,-40.022970755778,123.841688417909)) ;
#55424 = CARTESIAN_POINT('Ctrl Pts',(-20.6312875915322,-40.2227390774993,
123.337660256565)) ;
#55425 = CARTESIAN_POINT('Ctrl Pts',(-20.936793816344,-40.0427499970188,123.319128562733)) ;
#55426 = CARTESIAN_POINT('Ctrl Pts',(-20.532247620092,-40.2427691412082,122.923541794563)) ;
#55427 = CARTESIAN_POINT('Ctrl Pts',(-20.812996407082,-40.0627800607277,122.801479468749)) ;
#55428 = CARTESIAN_POINT('Ctrl Pts',(-20.2989045718909,-40.2626514261102,
122.570943457578)) ;
#55429 = CARTESIAN_POINT('Ctrl Pts',(-20.5213204072867,-40.0826623456297,
122.360731281986)) ;
#55430 = CARTESIAN_POINT('Ctrl Pts',(-19.9600279754679,-40.2825337270031,
122.318257760773)) ;
#55431 = CARTESIAN_POINT('Ctrl Pts',(-20.0977276288373,-40.1025446465226,
122.044872252557)) ;
#55432 = CARTESIAN_POINT('Ctrl Pts',(-19.5531288014987,-40.3025168366215,
122.195882017085)) ;
#55433 = CARTESIAN_POINT('Ctrl Pts',(-19.5891047472239,-40.122527756141,121.891899364453)) ;
#55434 = CARTESIAN_POINT('Ctrl Pts',(-19.1308454732642,-40.3224072319994,
122.219647803408)) ;
#55435 = CARTESIAN_POINT('Ctrl Pts',(-19.0612513999883,-40.1424181515189,
121.921603035478)) ;
#55436 = CARTESIAN_POINT('Ctrl Pts',(-18.7417231158238,-40.3423040220336,
122.38552655651)) ;
#55437 = CARTESIAN_POINT('Ctrl Pts',(-18.5748477162323,-40.1623149415532,
122.128947492221)) ;
#55438 = CARTESIAN_POINT('Ctrl Pts',(-18.4318742792953,-40.3622210759752,
122.674244241734)) ;
#55439 = CARTESIAN_POINT('Ctrl Pts',(-18.187534217096,-40.1822319954948,122.489841093105)) ;
#55440 = CARTESIAN_POINT('Ctrl Pts',(-18.2384227273083,-40.3822246241788,
123.053097596815)) ;
#55441 = CARTESIAN_POINT('Ctrl Pts',(-17.9457158454956,-40.2022355436983,
122.963405930275)) ;
#55442 = CARTESIAN_POINT('Ctrl Pts',(-18.1866699600762,-40.4021629178314,
123.473848629645)) ;
#55443 = CARTESIAN_POINT('Ctrl Pts',(-17.8810209347116,-40.2221738373509,
123.489343815261)) ;
#55444 = CARTESIAN_POINT('Ctrl Pts',(-18.280049631561,-40.4219844052643,123.884838555175)) ;
#55445 = CARTESIAN_POINT('Ctrl Pts',(-17.99774005357,-40.2419953247838,124.003081008406)) ;
#55446 = CARTESIAN_POINT('Ctrl Pts',(-18.5094838644823,-40.4419627982552,
124.242285334387)) ;
#55447 = CARTESIAN_POINT('Ctrl Pts',(-18.2845312146954,-40.2619737177747,
124.449892679484)) ;
#55448 = CARTESIAN_POINT('Ctrl Pts',(-18.8460247213349,-40.4618611798689,
124.498817471921)) ;
#55449 = CARTESIAN_POINT('Ctrl Pts',(-18.7051945464138,-40.2818720993884,
124.770559205583)) ;
#55450 = CARTESIAN_POINT('Ctrl Pts',(-19.1823032913064,-40.4784441105988,
124.604500943763)) ;
#55451 = CARTESIAN_POINT('Ctrl Pts',(-19.1255703487447,-40.2984550301183,
124.902674539656)) ;
#55452 = CARTESIAN_POINT('Ctrl Pts',(-19.4611720898915,-40.4917183461876,
124.616752614585)) ;
#55453 = CARTESIAN_POINT('Ctrl Pts',(-19.4741295857848,-40.3117292657071,
124.917986772881)) ;
#55454 = CARTESIAN_POINT('Ctrl Pts',(-19.6705355947193,-40.5017647636438,
124.589137634991)) ;
#55455 = CARTESIAN_POINT('Ctrl Pts',(-19.735842546372,-40.3217756831633,124.883469686386)) ;
#55456 = CARTESIAN_POINT('Ctrl Pts',(-19.8680131387049,-40.5116099888631,
124.527058907304)) ;
#55457 = CARTESIAN_POINT('Ctrl Pts',(-19.9826774778884,-40.3316209083826,
124.805881778766)) ;
#55458 = CARTESIAN_POINT('Ctrl Pts',(-20.1170123821962,-40.5249449599025,
124.398409715662)) ;
#55459 = CARTESIAN_POINT('Ctrl Pts',(-20.2939829336976,-40.344955879422,124.645032732069)) ;
#55460 = CARTESIAN_POINT('Ctrl Pts',(-20.3777873292751,-40.5415278166951,
124.160882668887)) ;
#55461 = CARTESIAN_POINT('Ctrl Pts',(-20.6198884115965,-40.3615387362146,
124.348182656348)) ;
#55462 = CARTESIAN_POINT('Ctrl Pts',(-20.5424028350229,-40.5581708190445,
123.847768971427)) ;
#55463 = CARTESIAN_POINT('Ctrl Pts',(-20.8256972517839,-40.378181738564,123.956743051222)) ;
#55464 = CARTESIAN_POINT('Ctrl Pts',(-20.6040438140094,-40.5714145500762,
123.576158500164)) ;
#55465 = CARTESIAN_POINT('Ctrl Pts',(-20.9027340824699,-40.3914254695957,
123.617264907902)) ;
#55466 = CARTESIAN_POINT('Ctrl Pts',(-20.6143139077877,-40.5814689447508,
123.36507953087)) ;
#55467 = CARTESIAN_POINT('Ctrl Pts',(-20.9155780419708,-40.4014798642703,
123.353409333883)) ;
#55468 = CARTESIAN_POINT('Ctrl Pts',(-20.5885990189638,-40.5913100061393,
123.159754071886)) ;
#55469 = CARTESIAN_POINT('Ctrl Pts',(-20.8834362368491,-40.4113209256588,
123.096754250321)) ;
#55470 = CARTESIAN_POINT('Ctrl Pts',(-20.5264471958815,-40.6013762304958,
122.957500488943)) ;
#55471 = CARTESIAN_POINT('Ctrl Pts',(-20.8057493251585,-40.4213871500153,
122.843935791852)) ;
#55472 = CARTESIAN_POINT('Ctrl Pts',(-20.4318111963384,-40.6112568434155,
122.772550933144)) ;
#55473 = CARTESIAN_POINT('Ctrl Pts',(-20.6874567829705,-40.431267762935,122.612747828755)) ;
#55474 = CARTESIAN_POINT('Ctrl Pts',(-20.3054294573994,-40.6212501365751,
122.604767036362)) ;
#55475 = CARTESIAN_POINT('Ctrl Pts',(-20.5294818313547,-40.4412610560946,
122.403016184021)) ;
#55476 = CARTESIAN_POINT('Ctrl Pts',(-20.1524873681173,-40.6312011447987,
122.461975515907)) ;
#55477 = CARTESIAN_POINT('Ctrl Pts',(-20.3383061145798,-40.4512120643182,
122.22452473296)) ;
#55478 = CARTESIAN_POINT('Ctrl Pts',(-19.9753190448652,-40.6412496591607,
122.346959912909)) ;
#55479 = CARTESIAN_POINT('Ctrl Pts',(-20.1168471521644,-40.4612605786802,
122.080752823269)) ;
#55480 = CARTESIAN_POINT('Ctrl Pts',(-19.7849296325353,-40.6510911652234,
122.265920115438)) ;
#55481 = CARTESIAN_POINT('Ctrl Pts',(-19.878861530971,-40.4711020847429,121.979450513718)) ;
#55482 = CARTESIAN_POINT('Ctrl Pts',(-19.5805644894003,-40.6610768178531,
122.218048516374)) ;
#55483 = CARTESIAN_POINT('Ctrl Pts',(-19.623405666542,-40.4810877373726,121.919608246859)) ;
#55484 = CARTESIAN_POINT('Ctrl Pts',(-19.3719102404823,-40.671015826698,122.206359844049)) ;
#55485 = CARTESIAN_POINT('Ctrl Pts',(-19.3625879444229,-40.4910267462175,
121.904994592829)) ;
#55486 = CARTESIAN_POINT('Ctrl Pts',(-19.1623259439942,-40.681056751991,122.231380193141)) ;
#55487 = CARTESIAN_POINT('Ctrl Pts',(-19.1006071741464,-40.5010676715105,
121.936267236799)) ;
#55488 = CARTESIAN_POINT('Ctrl Pts',(-18.9632287027856,-40.6909470737459,
122.291388692216)) ;
#55489 = CARTESIAN_POINT('Ctrl Pts',(-18.851734717605,-40.5109579932654,122.01127519242)) ;
#55490 = CARTESIAN_POINT('Ctrl Pts',(-18.7754842627344,-40.7009430470793,
122.385762996334)) ;
#55491 = CARTESIAN_POINT('Ctrl Pts',(-18.6170528303436,-40.5209539665988,
122.129240595498)) ;
#55492 = CARTESIAN_POINT('Ctrl Pts',(-18.6080361030909,-40.7108744466613,
122.51049410798)) ;
#55493 = CARTESIAN_POINT('Ctrl Pts',(-18.4077408549979,-40.5308853661809,
122.285152304377)) ;
#55494 = CARTESIAN_POINT('Ctrl Pts',(-18.4635012584254,-40.7208799871384,
122.663335115609)) ;
#55495 = CARTESIAN_POINT('Ctrl Pts',(-18.2270702112574,-40.5408909066579,
122.47620169738)) ;
#55496 = CARTESIAN_POINT('Ctrl Pts',(-18.3477150281808,-40.7309129710697,
122.839629729903)) ;
#55497 = CARTESIAN_POINT('Ctrl Pts',(-18.0823350469109,-40.5509238905892,
122.696568451424)) ;
#55498 = CARTESIAN_POINT('Ctrl Pts',(-18.2654267208358,-40.7407686018965,
123.029802709535)) ;
#55499 = CARTESIAN_POINT('Ctrl Pts',(-17.9794720035791,-40.5607795214161,
122.934283776496)) ;
#55500 = CARTESIAN_POINT('Ctrl Pts',(-18.2164553752564,-40.7507680040897,
123.234201010115)) ;
#55501 = CARTESIAN_POINT('Ctrl Pts',(-17.9182550887959,-40.5707789236092,
123.189781090298)) ;
#55502 = CARTESIAN_POINT('Ctrl Pts',(-18.2036080978333,-40.7606624734508,
123.441855570182)) ;
#55503 = CARTESIAN_POINT('Ctrl Pts',(-17.9021932200711,-40.5806733929703,
123.449349378985)) ;
#55504 = CARTESIAN_POINT('Ctrl Pts',(-18.2274647702079,-40.770725587615,123.652027977728)) ;
#55505 = CARTESIAN_POINT('Ctrl Pts',(-17.932011300752,-40.5907365071345,123.712065167688)) ;
#55506 = CARTESIAN_POINT('Ctrl Pts',(-18.2859206509781,-40.7805652333314,
123.85049263691)) ;
#55507 = CARTESIAN_POINT('Ctrl Pts',(-18.0050786318831,-40.6005761528509,
123.960147159126)) ;
#55508 = CARTESIAN_POINT('Ctrl Pts',(-18.3797695061755,-40.7906284008871,
124.040064614096)) ;
#55509 = CARTESIAN_POINT('Ctrl Pts',(-18.1223872399659,-40.6106393204066,
124.19711330026)) ;
#55510 = CARTESIAN_POINT('Ctrl Pts',(-18.5031774126307,-40.800522656682,124.207538533751)) ;
#55511 = CARTESIAN_POINT('Ctrl Pts',(-18.2766451103513,-40.6205335762015,
124.406457589714)) ;
#55512 = CARTESIAN_POINT('Ctrl Pts',(-18.654084810904,-40.8104644351417,124.352107908462)) ;
#55513 = CARTESIAN_POINT('Ctrl Pts',(-18.4652776965624,-40.6304753546612,
124.587171422897)) ;
#55514 = CARTESIAN_POINT('Ctrl Pts',(-18.828869034011,-40.8204671279719,124.469083088964)) ;
#55515 = CARTESIAN_POINT('Ctrl Pts',(-18.6837565651691,-40.6404780474914,
124.733392656357)) ;
#55516 = CARTESIAN_POINT('Ctrl Pts',(-19.0220064357381,-40.8305011499257,
124.553889575478)) ;
#55517 = CARTESIAN_POINT('Ctrl Pts',(-18.9251772147006,-40.6505120694452,
124.839403238466)) ;
#55518 = CARTESIAN_POINT('Ctrl Pts',(-19.223072436617,-40.8403489410147,124.603257935098)) ;
#55519 = CARTESIAN_POINT('Ctrl Pts',(-19.1765096235955,-40.6603598605342,
124.90111640687)) ;
#55520 = CARTESIAN_POINT('Ctrl Pts',(-19.4324060765276,-40.8503304655638,
124.617611036992)) ;
#55521 = CARTESIAN_POINT('Ctrl Pts',(-19.4381766703686,-40.6703413850833,
124.919060383803)) ;
#55522 = CARTESIAN_POINT('Ctrl Pts',(-19.6403984022838,-40.8602796890547,
124.595436731621)) ;
#55523 = CARTESIAN_POINT('Ctrl Pts',(-19.6981676205083,-40.6802906085742,
124.891345054845)) ;
#55524 = CARTESIAN_POINT('Ctrl Pts',(-19.842443083507,-40.8702773452713,124.537454340177)) ;
#55525 = CARTESIAN_POINT('Ctrl Pts',(-19.9507242765241,-40.6902882647908,
124.818869487643)) ;
#55526 = CARTESIAN_POINT('Ctrl Pts',(-20.0319489132289,-40.8803175583263,
124.444528163005)) ;
#55527 = CARTESIAN_POINT('Ctrl Pts',(-20.187607666279,-40.7003284778458,124.702714148817)) ;
#55528 = CARTESIAN_POINT('Ctrl Pts',(-20.1991246682804,-40.8901456056026,
124.323088911922)) ;
#55529 = CARTESIAN_POINT('Ctrl Pts',(-20.396579474449,-40.7101565251221,124.550916691175)) ;
#55530 = CARTESIAN_POINT('Ctrl Pts',(-20.346201088897,-40.9001999526349,124.171290921794)) ;
#55531 = CARTESIAN_POINT('Ctrl Pts',(-20.5804267073695,-40.7202108721545,
124.36117100516)) ;
#55532 = CARTESIAN_POINT('Ctrl Pts',(-20.4630696212735,-40.9101410889635,
123.998019997422)) ;
#55533 = CARTESIAN_POINT('Ctrl Pts',(-20.7265146725956,-40.730152008483,124.144583500133)) ;
#55534 = CARTESIAN_POINT('Ctrl Pts',(-20.5483504789561,-40.9200453220432,
123.808062649806)) ;
#55535 = CARTESIAN_POINT('Ctrl Pts',(-20.833118168539,-40.7400562415627,123.907137322088)) ;
#55536 = CARTESIAN_POINT('Ctrl Pts',(-20.5999532572044,-40.9300920188868,
123.60326863494)) ;
#55537 = CARTESIAN_POINT('Ctrl Pts',(-20.8976239888789,-40.7501029384063,
123.651145500474)) ;
#55538 = CARTESIAN_POINT('Ctrl Pts',(-20.6151760608575,-40.9399875701671,
123.395757075014)) ;
#55539 = CARTESIAN_POINT('Ctrl Pts',(-20.9166549331708,-40.7599984896866,
123.391755647876)) ;
#55540 = CARTESIAN_POINT('Ctrl Pts',(-20.5937893271631,-40.9500496480066,
123.185334655096)) ;
#55541 = CARTESIAN_POINT('Ctrl Pts',(-20.8899239297409,-40.7700605675261,
123.128727559456)) ;
#55542 = CARTESIAN_POINT('Ctrl Pts',(-20.5375466139094,-40.9598923571026,
122.986176025129)) ;
#55543 = CARTESIAN_POINT('Ctrl Pts',(-20.819622592751,-40.7799032766222,122.879777795648)) ;
#55544 = CARTESIAN_POINT('Ctrl Pts',(-20.4466945331734,-40.9698830893411,
122.796834964654)) ;
#55545 = CARTESIAN_POINT('Ctrl Pts',(-20.7060594584752,-40.7898940088606,
122.643100332415)) ;
#55546 = CARTESIAN_POINT('Ctrl Pts',(-20.32506530426,-40.9798111145698,122.627205149371)) ;
#55547 = CARTESIAN_POINT('Ctrl Pts',(-20.5540244826966,-40.7998220340894,
122.431061345362)) ;
#55548 = CARTESIAN_POINT('Ctrl Pts',(-20.1751809243749,-40.9897992612204,
122.480136248305)) ;
#55549 = CARTESIAN_POINT('Ctrl Pts',(-20.3666704075686,-40.8098101807399,
122.247223536346)) ;
#55550 = CARTESIAN_POINT('Ctrl Pts',(-20.0010440003547,-40.9998342790604,
122.361035774299)) ;
#55551 = CARTESIAN_POINT('Ctrl Pts',(-20.1490005901625,-40.8198451985799,
122.098346117447)) ;
#55552 = CARTESIAN_POINT('Ctrl Pts',(-19.8122322682539,-41.0096990761655,
122.275263236687)) ;
#55553 = CARTESIAN_POINT('Ctrl Pts',(-19.912986052844,-40.8297099956851,121.991128079495)) ;
#55554 = CARTESIAN_POINT('Ctrl Pts',(-19.6095835568502,-41.0196598085217,
122.222477105135)) ;
#55555 = CARTESIAN_POINT('Ctrl Pts',(-19.6596753422363,-40.8396707280412,
121.925143350188)) ;
#55556 = CARTESIAN_POINT('Ctrl Pts',(-19.3993089283046,-41.0296932709187,
122.205909546878)) ;
#55557 = CARTESIAN_POINT('Ctrl Pts',(-19.3968323127526,-40.8497041904382,
121.904431778366)) ;
#55558 = CARTESIAN_POINT('Ctrl Pts',(-19.1923814571992,-41.0395788051301,
122.225463175371)) ;
#55559 = CARTESIAN_POINT('Ctrl Pts',(-19.1381719931382,-40.8595897246496,
121.928871855483)) ;
#55560 = CARTESIAN_POINT('Ctrl Pts',(-18.9884081997025,-41.0496436458101,
122.281644422525)) ;
#55561 = CARTESIAN_POINT('Ctrl Pts',(-18.8832051234226,-40.8696545653296,
121.999096372835)) ;
#55562 = CARTESIAN_POINT('Ctrl Pts',(-18.8013257411855,-41.0594917775389,
122.370368828685)) ;
#55563 = CARTESIAN_POINT('Ctrl Pts',(-18.6493502438061,-40.8795026970585,
122.110000505637)) ;
#55564 = CARTESIAN_POINT('Ctrl Pts',(-18.6291184084903,-41.0695192745291,
122.491953508965)) ;
#55565 = CARTESIAN_POINT('Ctrl Pts',(-18.4340900375309,-40.8895301940486,
122.261979815377)) ;
#55566 = CARTESIAN_POINT('Ctrl Pts',(-18.4810087173521,-41.0795477265741,
122.642011387807)) ;
#55567 = CARTESIAN_POINT('Ctrl Pts',(-18.2489515310926,-40.8995586460937,
122.449550692896)) ;
#55568 = CARTESIAN_POINT('Ctrl Pts',(-18.3630810655382,-41.0893929931382,
122.812094313911)) ;
#55569 = CARTESIAN_POINT('Ctrl Pts',(-18.1015397639368,-40.9094039126578,
122.662154181668)) ;
#55570 = CARTESIAN_POINT('Ctrl Pts',(-18.2746791888148,-41.0993836660792,
123.00262605961)) ;
#55571 = CARTESIAN_POINT('Ctrl Pts',(-17.9910357648319,-40.9193945855987,
122.900318312465)) ;
#55572 = CARTESIAN_POINT('Ctrl Pts',(-18.2209040134384,-41.1094215481676,
123.206685229747)) ;
#55573 = CARTESIAN_POINT('Ctrl Pts',(-17.9238150124732,-40.9294324676872,
123.155391667979)) ;
#55574 = CARTESIAN_POINT('Ctrl Pts',(-18.2033541254263,-41.1192659186073,
123.412907134102)) ;
#55575 = CARTESIAN_POINT('Ctrl Pts',(-17.9018757957966,-40.9392768381268,
123.413170064838)) ;
#55576 = CARTESIAN_POINT('Ctrl Pts',(-18.2217257491831,-41.1292507460027,
123.621985540264)) ;
#55577 = CARTESIAN_POINT('Ctrl Pts',(-17.9248387220261,-40.9492616655222,
123.674518463703)) ;
#55578 = CARTESIAN_POINT('Ctrl Pts',(-18.2757990112521,-41.139190191408,123.82385763404)) ;
#55579 = CARTESIAN_POINT('Ctrl Pts',(-17.9924288978271,-40.9592011109275,
123.926859520064)) ;
#55580 = CARTESIAN_POINT('Ctrl Pts',(-18.3650287174585,-41.1492301956939,
124.01511881118)) ;
#55581 = CARTESIAN_POINT('Ctrl Pts',(-18.1039644975563,-40.9692411152134,
124.165936540867)) ;
#55582 = CARTESIAN_POINT('Ctrl Pts',(-18.4841771963513,-41.1591173048795,
124.18546666406)) ;
#55583 = CARTESIAN_POINT('Ctrl Pts',(-18.2528993473601,-40.979128224399,124.378873025841)) ;
#55584 = CARTESIAN_POINT('Ctrl Pts',(-18.6325483512414,-41.169117364782,124.334363428523)) ;
#55585 = CARTESIAN_POINT('Ctrl Pts',(-18.438362340865,-40.9891282843015,124.564995129855)) ;
#55586 = CARTESIAN_POINT('Ctrl Pts',(-18.8030499054225,-41.1790347806967,
124.45442108235)) ;
#55587 = CARTESIAN_POINT('Ctrl Pts',(-18.6514890496474,-40.9990457002162,
124.715068773003)) ;
#55588 = CARTESIAN_POINT('Ctrl Pts',(-18.9942377867766,-41.1890815954375,
124.544124964319)) ;
#55589 = CARTESIAN_POINT('Ctrl Pts',(-18.8904730959717,-41.009092514957,124.827199842494)) ;
#55590 = CARTESIAN_POINT('Ctrl Pts',(-19.194625243992,-41.1989570726341,124.59855210773)) ;
#55591 = CARTESIAN_POINT('Ctrl Pts',(-19.1409580664775,-41.0189679921537,
124.895235368281)) ;
#55592 = CARTESIAN_POINT('Ctrl Pts',(-19.4051209957553,-41.2090131683554,
124.617812738333)) ;
#55593 = CARTESIAN_POINT('Ctrl Pts',(-19.4040773768782,-41.0290240878749,
124.919312459518)) ;
#55594 = CARTESIAN_POINT('Ctrl Pts',(-19.612431639119,-41.2189063303704,124.600588284095)) ;
#55595 = CARTESIAN_POINT('Ctrl Pts',(-19.6632167072964,-41.03891724989,124.897783110664)) ;
#55596 = CARTESIAN_POINT('Ctrl Pts',(-19.8169921171162,-41.228968566393,124.546802146257)) ;
#55597 = CARTESIAN_POINT('Ctrl Pts',(-19.9189173139236,-41.0489794859126,
124.830551761056)) ;
#55598 = CARTESIAN_POINT('Ctrl Pts',(-20.0049876675589,-41.238813032022,124.460234593198)) ;
#55599 = CARTESIAN_POINT('Ctrl Pts',(-20.15391348363,-41.0588239515415,124.72234292479)) ;
#55600 = CARTESIAN_POINT('Ctrl Pts',(-20.1775149384373,-41.2487731247261,
124.341583226709)) ;
#55601 = CARTESIAN_POINT('Ctrl Pts',(-20.3695735132211,-41.0687840442456,
124.574029279079)) ;
#55602 = CARTESIAN_POINT('Ctrl Pts',(-20.3276957983037,-41.2588114137072,
124.193333688779)) ;
#55603 = CARTESIAN_POINT('Ctrl Pts',(-20.5573002808556,-41.0788223332267,
124.388718288929)) ;
#55604 = CARTESIAN_POINT('Ctrl Pts',(-20.4481963084003,-41.2686847368134,
124.024285690543)) ;
#55605 = CARTESIAN_POINT('Ctrl Pts',(-20.7079273848566,-41.0886956563329,
124.177407956331)) ;
#55606 = CARTESIAN_POINT('Ctrl Pts',(-20.5392295552627,-41.2787579208985,
123.833127087447)) ;
#55607 = CARTESIAN_POINT('Ctrl Pts',(-20.8217196877489,-41.098768840418,123.938460528992)) ;
#55608 = CARTESIAN_POINT('Ctrl Pts',(-20.5945544507421,-41.2885784331864,
123.634173535179)) ;
#55609 = CARTESIAN_POINT('Ctrl Pts',(-20.8908771122864,-41.1085893527059,
123.68976734053)) ;
#55610 = CARTESIAN_POINT('Ctrl Pts',(-20.6152109322945,-41.2986564293022,
123.4233616068)) ;
#55611 = CARTESIAN_POINT('Ctrl Pts',(-20.9166985132169,-41.1186673488217,
123.426252975596)) ;
#55612 = CARTESIAN_POINT('Ctrl Pts',(-20.5993528249516,-41.3085105042855,
123.216758416183)) ;
#55613 = CARTESIAN_POINT('Ctrl Pts',(-20.8968766072787,-41.128521423805,123.167997632814)) ;
#55614 = CARTESIAN_POINT('Ctrl Pts',(-20.5470119355056,-41.3185743858692,
123.011801977239)) ;
#55615 = CARTESIAN_POINT('Ctrl Pts',(-20.831451299186,-41.1385853053887,122.911802236361)) ;
#55616 = CARTESIAN_POINT('Ctrl Pts',(-20.4613754347014,-41.3284578118429,
122.822450585418)) ;
#55617 = CARTESIAN_POINT('Ctrl Pts',(-20.7244059190907,-41.1484687313624,
122.675111706998)) ;
#55618 = CARTESIAN_POINT('Ctrl Pts',(-20.3430903346169,-41.338458415764,122.648681232655)) ;
#55619 = CARTESIAN_POINT('Ctrl Pts',(-20.5765499861908,-41.1584693352835,
122.457899543833)) ;
#55620 = CARTESIAN_POINT('Ctrl Pts',(-20.1976579653882,-41.3483782001018,
122.49916106268)) ;
#55621 = CARTESIAN_POINT('Ctrl Pts',(-20.3947593961203,-41.1683891196214,
122.270998373783)) ;
#55622 = CARTESIAN_POINT('Ctrl Pts',(-20.0263274877781,-41.3584255504587,
122.375678234952)) ;
#55623 = CARTESIAN_POINT('Ctrl Pts',(-20.1805968422946,-41.1784364699782,
122.116644489868)) ;
#55624 = CARTESIAN_POINT('Ctrl Pts',(-19.8394159318229,-41.368302892693,122.285119868391)) ;
#55625 = CARTESIAN_POINT('Ctrl Pts',(-19.9469565781688,-41.1883138122125,
122.003445575587)) ;
#55626 = CARTESIAN_POINT('Ctrl Pts',(-19.6358016808575,-41.3783727737676,
122.227321629888)) ;
#55627 = CARTESIAN_POINT('Ctrl Pts',(-19.6924393111022,-41.1983836932871,
121.931197405143)) ;
#55628 = CARTESIAN_POINT('Ctrl Pts',(-19.4302105986271,-41.3882024789693,
122.206046078144)) ;
#55629 = CARTESIAN_POINT('Ctrl Pts',(-19.435448966812,-41.2082133984888,121.904602386657)) ;
#55630 = CARTESIAN_POINT('Ctrl Pts',(-19.2191313622272,-41.3982691401357,
122.220859081126)) ;
#55631 = CARTESIAN_POINT('Ctrl Pts',(-19.1716002965502,-41.2182800596552,
121.923118301368)) ;
#55632 = CARTESIAN_POINT('Ctrl Pts',(-19.0174028500584,-41.408159362003,122.271341345919)) ;
#55633 = CARTESIAN_POINT('Ctrl Pts',(-18.9194385507333,-41.2281702815225,
121.986221032295)) ;
#55634 = CARTESIAN_POINT('Ctrl Pts',(-18.8253933440022,-41.4181515381132,
122.356520476582)) ;
#55635 = CARTESIAN_POINT('Ctrl Pts',(-18.6794263981433,-41.2381624576327,
122.092694864997)) ;
#55636 = CARTESIAN_POINT('Ctrl Pts',(-18.6517079385557,-41.4281143682258,
122.473569637497)) ;
#55637 = CARTESIAN_POINT('Ctrl Pts',(-18.4623191157253,-41.2481252877453,
122.239006352162)) ;
#55638 = CARTESIAN_POINT('Ctrl Pts',(-18.5014870756419,-41.4380185806261,
122.61777683837)) ;
#55639 = CARTESIAN_POINT('Ctrl Pts',(-18.274542323602,-41.2580295001457,122.419265967065)) ;
#55640 = CARTESIAN_POINT('Ctrl Pts',(-18.3768239906411,-41.448079294714,122.788607618059)) ;
#55641 = CARTESIAN_POINT('Ctrl Pts',(-18.1187135737905,-41.2680902142335,
122.63280407958)) ;
#55642 = CARTESIAN_POINT('Ctrl Pts',(-18.2854831726733,-41.4579187976968,
122.974241715456)) ;
#55643 = CARTESIAN_POINT('Ctrl Pts',(-18.0045368873507,-41.2779297172163,
122.864848022224)) ;
#55644 = CARTESIAN_POINT('Ctrl Pts',(-18.2262434983332,-41.4679849362632,
123.177367766874)) ;
#55645 = CARTESIAN_POINT('Ctrl Pts',(-17.9304874744645,-41.2879958557827,
123.118755220522)) ;
#55646 = CARTESIAN_POINT('Ctrl Pts',(-18.2036641637308,-41.4778674507492,
123.383929826508)) ;
#55647 = CARTESIAN_POINT('Ctrl Pts',(-17.902263224138,-41.2978783702687,123.37695892444)) ;
#55648 = CARTESIAN_POINT('Ctrl Pts',(-18.217028771755,-41.4878597501047,123.593541694944)) ;
#55649 = CARTESIAN_POINT('Ctrl Pts',(-17.9189692032096,-41.3078706696243,
123.638973965521)) ;
#55650 = CARTESIAN_POINT('Ctrl Pts',(-18.266354986361,-41.4978128170581,123.796921608966)) ;
#55651 = CARTESIAN_POINT('Ctrl Pts',(-17.9806273075444,-41.3178237365777,
123.893199304631)) ;
#55652 = CARTESIAN_POINT('Ctrl Pts',(-18.3509953062756,-41.5078475252634,
123.990141633652)) ;
#55653 = CARTESIAN_POINT('Ctrl Pts',(-18.0864278198441,-41.3278584447829,
124.134724121269)) ;
#55654 = CARTESIAN_POINT('Ctrl Pts',(-18.4660813786671,-41.5177357461675,
124.16327447273)) ;
#55655 = CARTESIAN_POINT('Ctrl Pts',(-18.2302862076432,-41.3377466656871,
124.351140926681)) ;
#55656 = CARTESIAN_POINT('Ctrl Pts',(-18.6107545882689,-41.527730169198,124.315632016027)) ;
#55657 = CARTESIAN_POINT('Ctrl Pts',(-18.4111281398735,-41.3477410887175,
124.541587743856)) ;
#55658 = CARTESIAN_POINT('Ctrl Pts',(-18.7789136987431,-41.5376755086441,
124.439882085286)) ;
#55659 = CARTESIAN_POINT('Ctrl Pts',(-18.6213277143257,-41.3576864281637,
124.696900401457)) ;
#55660 = CARTESIAN_POINT('Ctrl Pts',(-18.9659468148119,-41.5476228532555,
124.533455179256)) ;
#55661 = CARTESIAN_POINT('Ctrl Pts',(-18.8551198559808,-41.367633772775,124.813866561947)) ;
#55662 = CARTESIAN_POINT('Ctrl Pts',(-19.1684641307119,-41.5576707486665,
124.593501263556)) ;
#55663 = CARTESIAN_POINT('Ctrl Pts',(-19.1082663812095,-41.377681668186,124.888923688679)) ;
#55664 = CARTESIAN_POINT('Ctrl Pts',(-19.3741360186057,-41.5675183941458,
124.617169452633)) ;
#55665 = CARTESIAN_POINT('Ctrl Pts',(-19.365357688916,-41.3875293136654,124.918508594089)) ;
#55666 = CARTESIAN_POINT('Ctrl Pts',(-19.5832145971549,-41.5774801080598,
124.605278842965)) ;
#55667 = CARTESIAN_POINT('Ctrl Pts',(-19.626706323974,-41.3974910275794,124.903644555779)) ;
#55668 = CARTESIAN_POINT('Ctrl Pts',(-19.788383314369,-41.5875087323508,124.556678207782)) ;
#55669 = CARTESIAN_POINT('Ctrl Pts',(-19.8831669773859,-41.4075196518703,
124.842893155846)) ;
#55670 = CARTESIAN_POINT('Ctrl Pts',(-19.979718451431,-41.5974190930075,124.47424697805)) ;
#55671 = CARTESIAN_POINT('Ctrl Pts',(-20.1223364380835,-41.417430012527,124.7398531547)) ;
#55672 = CARTESIAN_POINT('Ctrl Pts',(-20.1545793968166,-41.6073537915808,
124.360016047797)) ;
#55673 = CARTESIAN_POINT('Ctrl Pts',(-20.3409126900121,-41.4273647111003,
124.597063389296)) ;
#55674 = CARTESIAN_POINT('Ctrl Pts',(-20.3084369890171,-41.617395616435,124.215477929178)) ;
#55675 = CARTESIAN_POINT('Ctrl Pts',(-20.5332339906583,-41.4374065359545,
124.416390285441)) ;
#55676 = CARTESIAN_POINT('Ctrl Pts',(-20.4330452256544,-41.6272801901794,
124.04915416565)) ;
#55677 = CARTESIAN_POINT('Ctrl Pts',(-20.6889942204414,-41.4472911096989,
124.208484214662)) ;
#55678 = CARTESIAN_POINT('Ctrl Pts',(-20.5281974762761,-41.6372820395426,
123.861676921121)) ;
#55679 = CARTESIAN_POINT('Ctrl Pts',(-20.80793373482,-41.4572929590621,123.974137087528)) ;
#55680 = CARTESIAN_POINT('Ctrl Pts',(-20.5890105169507,-41.6472013411166,
123.662177464747)) ;
#55681 = CARTESIAN_POINT('Ctrl Pts',(-20.8839492758714,-41.4672122606361,
123.724761737234)) ;
#55682 = CARTESIAN_POINT('Ctrl Pts',(-20.6145770333962,-41.6572454494619,
123.452589429869)) ;
#55683 = CARTESIAN_POINT('Ctrl Pts',(-20.9159063785806,-41.4772563689814,
123.46277677981)) ;
#55684 = CARTESIAN_POINT('Ctrl Pts',(-20.6036034057865,-41.6671298729041,
123.245068543956)) ;
#55685 = CARTESIAN_POINT('Ctrl Pts',(-20.9021882406929,-41.4871407924237,
123.203374700065)) ;
#55686 = CARTESIAN_POINT('Ctrl Pts',(-20.5565952979151,-41.6771462348136,
123.039799079144)) ;
#55687 = CARTESIAN_POINT('Ctrl Pts',(-20.8434269169857,-41.4971571543331,
122.946788139625)) ;
#55688 = CARTESIAN_POINT('Ctrl Pts',(-20.4739898693975,-41.687182890319,122.845651147378)) ;
#55689 = CARTESIAN_POINT('Ctrl Pts',(-20.7401692464129,-41.5071938098385,
122.704103736614)) ;
#55690 = CARTESIAN_POINT('Ctrl Pts',(-20.3617495143391,-41.6970130205083,
122.672097956593)) ;
#55691 = CARTESIAN_POINT('Ctrl Pts',(-20.599866997002,-41.5170239400278,122.487161714405)) ;
#55692 = CARTESIAN_POINT('Ctrl Pts',(-20.2176578236803,-41.7070890735982,
122.516880089597)) ;
#55693 = CARTESIAN_POINT('Ctrl Pts',(-20.4197517581915,-41.5270999931177,
122.293140546941)) ;
#55694 = CARTESIAN_POINT('Ctrl Pts',(-20.0525570282774,-41.716941302784,122.391738375316)) ;
#55695 = CARTESIAN_POINT('Ctrl Pts',(-20.2133740002542,-41.5369522223035,
122.136713686514)) ;
#55696 = CARTESIAN_POINT('Ctrl Pts',(-19.864251762106,-41.7270145105833,122.294921019345)) ;
#55697 = CARTESIAN_POINT('Ctrl Pts',(-19.9779921556695,-41.5470254301028,
122.015693380186)) ;
#55698 = CARTESIAN_POINT('Ctrl Pts',(-19.666587072999,-41.7368560219347,122.233752490588)) ;
#55699 = CARTESIAN_POINT('Ctrl Pts',(-19.7309096531078,-41.5568669414542,
121.93923360609)) ;
#55700 = CARTESIAN_POINT('Ctrl Pts',(-19.458933216277,-41.7468169599722,122.206739976442)) ;
#55701 = CARTESIAN_POINT('Ctrl Pts',(-19.4713417220733,-41.5668278794917,
121.905469506016)) ;
#55702 = CARTESIAN_POINT('Ctrl Pts',(-19.2481470392033,-41.7568548218972,
122.21668888155)) ;
#55703 = CARTESIAN_POINT('Ctrl Pts',(-19.207859203209,-41.5768657414167,121.917907090577)) ;
#55704 = CARTESIAN_POINT('Ctrl Pts',(-19.0455303660746,-41.7667290078943,
122.261958044375)) ;
#55705 = CARTESIAN_POINT('Ctrl Pts',(-18.9545877189541,-41.5867399274138,
121.974495320548)) ;
#55706 = CARTESIAN_POINT('Ctrl Pts',(-18.8501065214671,-41.7767991674721,
122.343300097971)) ;
#55707 = CARTESIAN_POINT('Ctrl Pts',(-18.7103088482893,-41.5968100869917,
122.07617421899)) ;
#55708 = CARTESIAN_POINT('Ctrl Pts',(-18.675884913286,-41.786630914898,122.454554501871)) ;
#55709 = CARTESIAN_POINT('Ctrl Pts',(-18.4925316285938,-41.6066418344175,
122.215244290356)) ;
#55710 = CARTESIAN_POINT('Ctrl Pts',(-18.5201147053539,-41.7966669949693,
122.596849719958)) ;
#55711 = CARTESIAN_POINT('Ctrl Pts',(-18.2978201732453,-41.6166779144888,
122.393114575254)) ;
#55712 = CARTESIAN_POINT('Ctrl Pts',(-18.3920704361308,-41.8066840418218,
122.764054383414)) ;
#55713 = CARTESIAN_POINT('Ctrl Pts',(-18.1377661290135,-41.6266949613413,
122.602121409318)) ;
#55714 = CARTESIAN_POINT('Ctrl Pts',(-18.2959657375201,-41.8165662999884,
122.948249336601)) ;
#55715 = CARTESIAN_POINT('Ctrl Pts',(-18.0176363962618,-41.6365772195079,
122.832366722308)) ;
#55716 = CARTESIAN_POINT('Ctrl Pts',(-18.2324121268901,-41.8265539827847,
123.148349956058)) ;
#55717 = CARTESIAN_POINT('Ctrl Pts',(-17.9381960767732,-41.6465649023042,
123.082493245749)) ;
#55718 = CARTESIAN_POINT('Ctrl Pts',(-18.2045073332423,-41.8365006395015,
123.355622216733)) ;
#55719 = CARTESIAN_POINT('Ctrl Pts',(-17.9033168940831,-41.656511559021,123.341584277099)) ;
#55720 = CARTESIAN_POINT('Ctrl Pts',(-18.2133253026657,-41.8465576975816,
123.566846105413)) ;
#55721 = CARTESIAN_POINT('Ctrl Pts',(-17.9143411681088,-41.6665686171012,
123.605613842776)) ;
#55722 = CARTESIAN_POINT('Ctrl Pts',(-18.2573346938639,-41.8563758771311,
123.768519750159)) ;
#55723 = CARTESIAN_POINT('Ctrl Pts',(-17.9693550453848,-41.6763867966506,
123.857706729718)) ;
#55724 = CARTESIAN_POINT('Ctrl Pts',(-18.3368951497359,-41.86641181157,123.963925455045)) ;
#55725 = CARTESIAN_POINT('Ctrl Pts',(-18.068807500374,-41.6864227310896,124.101962974052)) ;
#55726 = CARTESIAN_POINT('Ctrl Pts',(-18.449568449613,-41.876436465999,124.142036436665)) ;
#55727 = CARTESIAN_POINT('Ctrl Pts',(-18.2096507193238,-41.6964473855186,
124.3246006639)) ;
#55728 = CARTESIAN_POINT('Ctrl Pts',(-18.5886702041934,-41.8862884855786,
124.295499146271)) ;
#55729 = CARTESIAN_POINT('Ctrl Pts',(-18.3835301011167,-41.7062994050981,
124.516428432914)) ;
#55730 = CARTESIAN_POINT('Ctrl Pts',(-18.7543933359487,-41.8962793992935,
124.424504024787)) ;
#55731 = CARTESIAN_POINT('Ctrl Pts',(-18.5906854587006,-41.716290318813,124.677682956572)) ;
#55732 = CARTESIAN_POINT('Ctrl Pts',(-18.9386244083252,-41.9061973881331,
124.522200361594)) ;
#55733 = CARTESIAN_POINT('Ctrl Pts',(-18.8209758180586,-41.7262083076526,
124.79980173712)) ;
#55734 = CARTESIAN_POINT('Ctrl Pts',(-19.1391682617768,-41.9162254988639,
124.587172771734)) ;
#55735 = CARTESIAN_POINT('Ctrl Pts',(-19.0716562720862,-41.7362364183834,
124.881015168382)) ;
#55736 = CARTESIAN_POINT('Ctrl Pts',(-19.3449799514909,-41.9261106967723,
124.616011040742)) ;
#55737 = CARTESIAN_POINT('Ctrl Pts',(-19.3289219205391,-41.7461216162918,
124.917060930375)) ;
#55738 = CARTESIAN_POINT('Ctrl Pts',(-19.554878431118,-41.9360999720403,124.609111482474)) ;
#55739 = CARTESIAN_POINT('Ctrl Pts',(-19.5912951011794,-41.7561108915598,
124.908434150223)) ;
#55740 = CARTESIAN_POINT('Ctrl Pts',(-19.7613596240019,-41.9461414302098,
124.565200707997)) ;
#55741 = CARTESIAN_POINT('Ctrl Pts',(-19.8493960391262,-41.7661523497293,
124.853543537103)) ;
#55742 = CARTESIAN_POINT('Ctrl Pts',(-19.9531398235918,-41.9559728939981,
124.48810716658)) ;
#55743 = CARTESIAN_POINT('Ctrl Pts',(-20.0891213276599,-41.7759838135176,
124.757174105062)) ;
#55744 = CARTESIAN_POINT('Ctrl Pts',(-20.1319364909177,-41.965977826302,124.377372382878)) ;
#55745 = CARTESIAN_POINT('Ctrl Pts',(-20.3126159522147,-41.7859887458215,
124.618753527422)) ;
#55746 = CARTESIAN_POINT('Ctrl Pts',(-20.2884681065489,-41.9759641901967,
124.237408278261)) ;
#55747 = CARTESIAN_POINT('Ctrl Pts',(-20.5082790001988,-41.7959751097162,
124.443796511025)) ;
#55748 = CARTESIAN_POINT('Ctrl Pts',(-20.4187181316533,-41.9859938190826,
124.071617468983)) ;
#55749 = CARTESIAN_POINT('Ctrl Pts',(-20.6710896621926,-41.8060047386021,
124.236556568629)) ;
#55750 = CARTESIAN_POINT('Ctrl Pts',(-20.5169261211042,-41.995869041191,123.888684071241)) ;
#55751 = CARTESIAN_POINT('Ctrl Pts',(-20.7938478465005,-41.8158799607105,
124.00788808418)) ;
#55752 = CARTESIAN_POINT('Ctrl Pts',(-20.5829278692201,-42.0058702535881,
123.689089793923)) ;
#55753 = CARTESIAN_POINT('Ctrl Pts',(-20.8763477235606,-41.8258811731076,
123.7583943576)) ;
#55754 = CARTESIAN_POINT('Ctrl Pts',(-20.6131956145041,-42.0157788328236,
123.482954015089)) ;
#55755 = CARTESIAN_POINT('Ctrl Pts',(-20.9141799976417,-41.8357897523431,
123.500723797935)) ;
#55756 = CARTESIAN_POINT('Ctrl Pts',(-20.6070613238518,-42.0258336853796,
123.271692586383)) ;
#55757 = CARTESIAN_POINT('Ctrl Pts',(-20.9065096444975,-41.8458446048991,
123.236647196721)) ;
#55758 = CARTESIAN_POINT('Ctrl Pts',(-20.5653915462767,-42.0356922676544,
123.068629174948)) ;
#55759 = CARTESIAN_POINT('Ctrl Pts',(-20.8544198066431,-41.8557031871739,
122.982817801533)) ;
#55760 = CARTESIAN_POINT('Ctrl Pts',(-20.4876191246396,-42.0457603970971,
122.871804464288)) ;
#55761 = CARTESIAN_POINT('Ctrl Pts',(-20.7572019523973,-41.8657713166166,
122.736787999736)) ;
#55762 = CARTESIAN_POINT('Ctrl Pts',(-20.3791532075603,-42.0556158687862,
122.695250592433)) ;
#55763 = CARTESIAN_POINT('Ctrl Pts',(-20.621617047781,-41.8756267883057,122.516096462786)) ;
#55764 = CARTESIAN_POINT('Ctrl Pts',(-20.2402233414134,-42.0656107171724,
122.53762013048)) ;
#55765 = CARTESIAN_POINT('Ctrl Pts',(-20.4479526499224,-41.885621636692,122.319060072896)) ;
#55766 = CARTESIAN_POINT('Ctrl Pts',(-20.0751431990478,-42.0756420139569,
122.406377183477)) ;
#55767 = CARTESIAN_POINT('Ctrl Pts',(-20.241600860063,-41.8956529334764,122.155008415633)) ;
#55768 = CARTESIAN_POINT('Ctrl Pts',(-19.8929827389423,-42.085508550167,122.307151426831)) ;
#55769 = CARTESIAN_POINT('Ctrl Pts',(-20.0138985647374,-41.9055194696865,
122.030978291762)) ;
#55770 = CARTESIAN_POINT('Ctrl Pts',(-19.6940889865307,-42.0954959731278,
122.239940435497)) ;
#55771 = CARTESIAN_POINT('Ctrl Pts',(-19.7652803950309,-41.9155068926473,
121.946967065322)) ;
#55772 = CARTESIAN_POINT('Ctrl Pts',(-19.4873935007549,-42.1054409121476,
122.208304514953)) ;
#55773 = CARTESIAN_POINT('Ctrl Pts',(-19.5069103967473,-41.9254518316671,
121.907424800085)) ;
#55774 = CARTESIAN_POINT('Ctrl Pts',(-19.2762891943971,-42.1154857980076,
122.213185852874)) ;
#55775 = CARTESIAN_POINT('Ctrl Pts',(-19.2430300937624,-41.9354967175271,
121.91352916489)) ;
#55776 = CARTESIAN_POINT('Ctrl Pts',(-19.0728324499465,-42.1253543330938,
122.253813361827)) ;
#55777 = CARTESIAN_POINT('Ctrl Pts',(-18.9887092821394,-41.9453652526133,
121.96431628744)) ;
#55778 = CARTESIAN_POINT('Ctrl Pts',(-18.877416228865,-42.1353202011005,122.329344157201)) ;
#55779 = CARTESIAN_POINT('Ctrl Pts',(-18.7444398717798,-41.95533112062,122.058732417951)) ;
#55780 = CARTESIAN_POINT('Ctrl Pts',(-18.697163938135,-42.145342848553,122.438490697059)) ;
#55781 = CARTESIAN_POINT('Ctrl Pts',(-18.5191258959242,-41.9653537680725,
122.195167959674)) ;
#55782 = CARTESIAN_POINT('Ctrl Pts',(-18.5401483686295,-42.1552664875606,
122.575845813976)) ;
#55783 = CARTESIAN_POINT('Ctrl Pts',(-18.322858065657,-41.9752774070801,122.366864085167)) ;
#55784 = CARTESIAN_POINT('Ctrl Pts',(-18.408710854997,-42.1652092125663,122.738393134439)) ;
#55785 = CARTESIAN_POINT('Ctrl Pts',(-18.1585632395934,-41.9852201320858,
122.570050124057)) ;
#55786 = CARTESIAN_POINT('Ctrl Pts',(-18.3066794566052,-42.1752548186182,
122.92328748586)) ;
#55787 = CARTESIAN_POINT('Ctrl Pts',(-18.0310264115202,-41.9952657381377,
122.80116942056)) ;
#55788 = CARTESIAN_POINT('Ctrl Pts',(-18.2393302313391,-42.1851162411393,
123.119379879712)) ;
#55789 = CARTESIAN_POINT('Ctrl Pts',(-17.9468424316427,-42.0051271606588,
123.046286075505)) ;
#55790 = CARTESIAN_POINT('Ctrl Pts',(-18.2062726029867,-42.1951098095885,
123.32682877589)) ;
#55791 = CARTESIAN_POINT('Ctrl Pts',(-17.9055231592109,-42.015120729108,123.305597710678)) ;
#55792 = CARTESIAN_POINT('Ctrl Pts',(-18.2096058519718,-42.2050352803438,
123.53549760296)) ;
#55793 = CARTESIAN_POINT('Ctrl Pts',(-17.9096925517523,-42.0250461998633,
123.5664338487)) ;
#55794 = CARTESIAN_POINT('Ctrl Pts',(-18.2495067475796,-42.2150629542996,
123.742474063571)) ;
#55795 = CARTESIAN_POINT('Ctrl Pts',(-17.9595713837686,-42.0350738738192,
123.825153894816)) ;
#55796 = CARTESIAN_POINT('Ctrl Pts',(-18.3235158516873,-42.2249501323413,
123.936741246355)) ;
#55797 = CARTESIAN_POINT('Ctrl Pts',(-18.0520856875413,-42.0449610518609,
124.067987197566)) ;
#55798 = CARTESIAN_POINT('Ctrl Pts',(-18.4314996605536,-42.2349785117095,
124.117783872996)) ;
#55799 = CARTESIAN_POINT('Ctrl Pts',(-18.1870669886483,-42.054989431229,124.294288291793)) ;
#55800 = CARTESIAN_POINT('Ctrl Pts',(-18.5673819663472,-42.244872754431,124.27530549087)) ;
#55801 = CARTESIAN_POINT('Ctrl Pts',(-18.3569254895816,-42.0648836739505,
124.49119150411)) ;
#55802 = CARTESIAN_POINT('Ctrl Pts',(-18.784709731541,-42.2582256710819,124.452982254129)) ;
#55803 = CARTESIAN_POINT('Ctrl Pts',(-18.6285705557097,-42.0782365906014,
124.71326978059)) ;
#55804 = CARTESIAN_POINT('Ctrl Pts',(-19.0405785225545,-42.2714281888286,
124.568605528917)) ;
#55805 = CARTESIAN_POINT('Ctrl Pts',(-18.9483775262258,-42.0914391083481,
124.857795814355)) ;
#55806 = CARTESIAN_POINT('Ctrl Pts',(-19.3175485571435,-42.2847840941096,
124.614299554858)) ;
#55807 = CARTESIAN_POINT('Ctrl Pts',(-19.294644250491,-42.1047950136291,124.91492401597)) ;
#55808 = CARTESIAN_POINT('Ctrl Pts',(-19.5256323724528,-42.2946807427474,
124.612199384341)) ;
#55809 = CARTESIAN_POINT('Ctrl Pts',(-19.5547381910791,-42.1146916622669,
124.912293117335)) ;
#55810 = CARTESIAN_POINT('Ctrl Pts',(-19.7332792605488,-42.3047288807999,
124.573491321626)) ;
#55811 = CARTESIAN_POINT('Ctrl Pts',(-19.8142993016721,-42.1247398003194,
124.86390602364)) ;
#55812 = CARTESIAN_POINT('Ctrl Pts',(-19.9279820672216,-42.3146198409776,
124.500461827482)) ;
#55813 = CARTESIAN_POINT('Ctrl Pts',(-20.057675936975,-42.1346307604971,124.772616402216)) ;
#55814 = CARTESIAN_POINT('Ctrl Pts',(-20.1091567639837,-42.3246126768544,
124.394101946924)) ;
#55815 = CARTESIAN_POINT('Ctrl Pts',(-20.2841432704492,-42.1446235963739,
124.639664036503)) ;
#55816 = CARTESIAN_POINT('Ctrl Pts',(-20.2695244297562,-42.334651771856,124.256910080624)) ;
#55817 = CARTESIAN_POINT('Ctrl Pts',(-20.4846006079943,-42.1546626913755,
124.468172605397)) ;
#55818 = CARTESIAN_POINT('Ctrl Pts',(-20.4013315978798,-42.3444891277071,
124.097515807606)) ;
#55819 = CARTESIAN_POINT('Ctrl Pts',(-20.6493590679593,-42.1645000472267,
124.268925825714)) ;
#55820 = CARTESIAN_POINT('Ctrl Pts',(-20.5404892382136,-42.3578820756379,
123.852779647777)) ;
#55821 = CARTESIAN_POINT('Ctrl Pts',(-20.8232941425912,-42.1778929951574,
123.963015567239)) ;
#55822 = CARTESIAN_POINT('Ctrl Pts',(-20.6114090444013,-42.3710487520648,
123.581847669317)) ;
#55823 = CARTESIAN_POINT('Ctrl Pts',(-20.9119427188423,-42.1910596715843,
123.624389608254)) ;
#55824 = CARTESIAN_POINT('Ctrl Pts',(-20.6101088531211,-42.3844335334716,
123.300551825487)) ;
#55825 = CARTESIAN_POINT('Ctrl Pts',(-20.9103198256763,-42.2044444529911,
123.272710611939)) ;
#55826 = CARTESIAN_POINT('Ctrl Pts',(-20.5732425145346,-42.3942953161154,
123.096486655904)) ;
#55827 = CARTESIAN_POINT('Ctrl Pts',(-20.8642332431022,-42.214306235635,123.017641919717)) ;
#55828 = CARTESIAN_POINT('Ctrl Pts',(-20.5008532734841,-42.4042944640685,
122.899177214063)) ;
#55829 = CARTESIAN_POINT('Ctrl Pts',(-20.7737441305226,-42.224305383588,122.77100264939)) ;
#55830 = CARTESIAN_POINT('Ctrl Pts',(-20.3964434183661,-42.4141972566856,
122.719010769963)) ;
#55831 = CARTESIAN_POINT('Ctrl Pts',(-20.6432311628392,-42.2342081762051,
122.545797674163)) ;
#55832 = CARTESIAN_POINT('Ctrl Pts',(-20.2603721575889,-42.4242468365765,
122.5574632317)) ;
#55833 = CARTESIAN_POINT('Ctrl Pts',(-20.4731343578492,-42.244257756096,122.343862138609)) ;
#55834 = CARTESIAN_POINT('Ctrl Pts',(-20.0479239998599,-42.437433910386,122.379158143776)) ;
#55835 = CARTESIAN_POINT('Ctrl Pts',(-20.2076003348036,-42.2574448299055,
122.120995609412)) ;
#55836 = CARTESIAN_POINT('Ctrl Pts',(-19.7251865030468,-42.4541867003572,
122.228834167967)) ;
#55837 = CARTESIAN_POINT('Ctrl Pts',(-19.804126587439,-42.2741976198767,121.9330813858)) ;
#55838 = CARTESIAN_POINT('Ctrl Pts',(-19.3757249735959,-42.4706753524519,
122.198219597745)) ;
#55839 = CARTESIAN_POINT('Ctrl Pts',(-19.3673812946773,-42.2906862719714,
121.894819463327)) ;
#55840 = CARTESIAN_POINT('Ctrl Pts',(-19.0992014727295,-42.4840321786353,
122.246369143376)) ;
#55841 = CARTESIAN_POINT('Ctrl Pts',(-19.0216618584567,-42.3040430981548,
121.955010873832)) ;
#55842 = CARTESIAN_POINT('Ctrl Pts',(-18.9034559148771,-42.4939285635132,
122.317028660144)) ;
#55843 = CARTESIAN_POINT('Ctrl Pts',(-18.7769948828561,-42.3139394830327,
122.043336388444)) ;
#55844 = CARTESIAN_POINT('Ctrl Pts',(-18.7209921103284,-42.5039350780337,
122.42160568978)) ;
#55845 = CARTESIAN_POINT('Ctrl Pts',(-18.5489107992119,-42.3239459975532,
122.174062497267)) ;
#55846 = CARTESIAN_POINT('Ctrl Pts',(-18.5074778701341,-42.5171252015501,
122.598716946262)) ;
#55847 = CARTESIAN_POINT('Ctrl Pts',(-18.2820313954693,-42.3371361210696,
122.395439854776)) ;
#55848 = CARTESIAN_POINT('Ctrl Pts',(-18.3017330813565,-42.5338917626996,
122.889684627251)) ;
#55849 = CARTESIAN_POINT('Ctrl Pts',(-18.0248416305318,-42.3539026822191,
122.759167368691)) ;
#55850 = CARTESIAN_POINT('Ctrl Pts',(-18.1906918477385,-42.5536762514077,
123.295564658477)) ;
#55851 = CARTESIAN_POINT('Ctrl Pts',(-17.886048514908,-42.3736871709272,123.266512292197)) ;
#55852 = CARTESIAN_POINT('Ctrl Pts',(-18.2237744744841,-42.5736216990041,
123.718259239701)) ;
#55853 = CARTESIAN_POINT('Ctrl Pts',(-17.9274046619368,-42.3936326185237,
123.794881012017)) ;
#55854 = CARTESIAN_POINT('Ctrl Pts',(-18.3992319347338,-42.5935333611601,
124.103576998798)) ;
#55855 = CARTESIAN_POINT('Ctrl Pts',(-18.1467300051219,-42.4135442806796,
124.276525573087)) ;
#55856 = CARTESIAN_POINT('Ctrl Pts',(-18.6947270079494,-42.6134255531789,
124.406289323311)) ;
#55857 = CARTESIAN_POINT('Ctrl Pts',(-18.5161004762394,-42.4334364726985,
124.654913018596)) ;
#55858 = CARTESIAN_POINT('Ctrl Pts',(-19.078800891227,-42.6334666837336,124.590739441501)) ;
#55859 = CARTESIAN_POINT('Ctrl Pts',(-18.996194781245,-42.4534776032531,124.885472692746)) ;
#55860 = CARTESIAN_POINT('Ctrl Pts',(-19.4981893983463,-42.6532850183492,
124.632822667758)) ;
#55861 = CARTESIAN_POINT('Ctrl Pts',(-19.5204288936221,-42.4732959378687,
124.938073342143)) ;
#55862 = CARTESIAN_POINT('Ctrl Pts',(-19.9098714360872,-42.6732575835688,
124.529182144137)) ;
#55863 = CARTESIAN_POINT('Ctrl Pts',(-20.0350303911881,-42.4932685030883,
124.808520139821)) ;
#55864 = CARTESIAN_POINT('Ctrl Pts',(-20.2603190889311,-42.6931467997404,
124.292190471673)) ;
#55865 = CARTESIAN_POINT('Ctrl Pts',(-20.4730875844101,-42.5131577192599,
124.512279231806)) ;
#55866 = CARTESIAN_POINT('Ctrl Pts',(-20.5101445680897,-42.7131703740631,
123.947568704461)) ;
#55867 = CARTESIAN_POINT('Ctrl Pts',(-20.7853676286801,-42.5331812935826,
124.081500341505)) ;
#55868 = CARTESIAN_POINT('Ctrl Pts',(-20.6263908959112,-42.7329675371513,
123.542918161152)) ;
#55869 = CARTESIAN_POINT('Ctrl Pts',(-20.9306728528494,-42.5529784566708,
123.575689148458)) ;
#55870 = CARTESIAN_POINT('Ctrl Pts',(-20.5983617331869,-42.7529330309751,
123.119413546413)) ;
#55871 = CARTESIAN_POINT('Ctrl Pts',(-20.8956352698519,-42.5729439504946,
123.046309019431)) ;
#55872 = CARTESIAN_POINT('Ctrl Pts',(-20.4270355343715,-42.7728867387165,
122.731150195956)) ;
#55873 = CARTESIAN_POINT('Ctrl Pts',(-20.6814765721563,-42.592897658236,122.560980844295)) ;
#55874 = CARTESIAN_POINT('Ctrl Pts',(-20.1343395660946,-42.7927941154431,
122.425505425646)) ;
#55875 = CARTESIAN_POINT('Ctrl Pts',(-20.3156068295359,-42.6128050349627,
122.178926648433)) ;
#55876 = CARTESIAN_POINT('Ctrl Pts',(-19.7563159918193,-42.8126463269917,
122.237523332506)) ;
#55877 = CARTESIAN_POINT('Ctrl Pts',(-19.8430795029076,-42.6326572465112,
121.943950043666)) ;
#55878 = CARTESIAN_POINT('Ctrl Pts',(-19.3322246512801,-42.8327187139374,
122.189721479614)) ;
#55879 = CARTESIAN_POINT('Ctrl Pts',(-19.3129641321296,-42.6527296334569,
121.884197616029)) ;
#55880 = CARTESIAN_POINT('Ctrl Pts',(-18.9222367590498,-42.8525565835777,
122.288891061449)) ;
#55881 = CARTESIAN_POINT('Ctrl Pts',(-18.800481895984,-42.6725675030972,122.008159119898)) ;
#55882 = CARTESIAN_POINT('Ctrl Pts',(-18.5694696067115,-42.8724072381308,
122.520633431099)) ;
#55883 = CARTESIAN_POINT('Ctrl Pts',(-18.3595239814835,-42.6924181576503,
122.297834684981)) ;
#55884 = CARTESIAN_POINT('Ctrl Pts',(-18.314918147968,-42.8924591724712,122.862621733189)) ;
#55885 = CARTESIAN_POINT('Ctrl Pts',(-18.0413332376484,-42.7124700919908,
122.725319925663)) ;
#55886 = CARTESIAN_POINT('Ctrl Pts',(-18.1937042551041,-42.9122923600373,
123.266633949038)) ;
#55887 = CARTESIAN_POINT('Ctrl Pts',(-17.8898151800707,-42.7323032795568,
123.230332622444)) ;
#55888 = CARTESIAN_POINT('Ctrl Pts',(-18.2168953535135,-42.932221572268,123.689590915752)) ;
#55889 = CARTESIAN_POINT('Ctrl Pts',(-17.9188018273465,-42.7522324917875,
123.759028000048)) ;
#55890 = CARTESIAN_POINT('Ctrl Pts',(-18.382321733306,-42.9521065374824,124.078869953119)) ;
#55891 = CARTESIAN_POINT('Ctrl Pts',(-18.1255818944321,-42.7721174570019,
124.245626671934)) ;
#55892 = CARTESIAN_POINT('Ctrl Pts',(-18.6737062137308,-42.972180278627,124.390635608847)) ;
#55893 = CARTESIAN_POINT('Ctrl Pts',(-18.489811290908,-42.7921911981465,124.635336040402)) ;
#55894 = CARTESIAN_POINT('Ctrl Pts',(-19.0487871348763,-42.9919734604074,
124.581662444527)) ;
#55895 = CARTESIAN_POINT('Ctrl Pts',(-18.958659155968,-42.8119843799269,124.874120892294)) ;
#55896 = CARTESIAN_POINT('Ctrl Pts',(-19.4698565957341,-43.0119361684101,
124.634936091618)) ;
#55897 = CARTESIAN_POINT('Ctrl Pts',(-19.4849952307128,-42.8319470879296,
124.940716397795)) ;
#55898 = CARTESIAN_POINT('Ctrl Pts',(-19.88406254428,-43.0319191201525,124.540216705959)) ;
#55899 = CARTESIAN_POINT('Ctrl Pts',(-20.0027532085991,-42.851930039672,124.822320272926)) ;
#55900 = CARTESIAN_POINT('Ctrl Pts',(-20.2384793849242,-43.0517297399247,
124.312505833384)) ;
#55901 = CARTESIAN_POINT('Ctrl Pts',(-20.4457748040066,-42.8717406594442,
124.537685736339)) ;
#55902 = CARTESIAN_POINT('Ctrl Pts',(-20.4964670998854,-43.0717134559576,
123.975002267441)) ;
#55903 = CARTESIAN_POINT('Ctrl Pts',(-20.7682626056657,-42.8917243754771,
124.115808826953)) ;
#55904 = CARTESIAN_POINT('Ctrl Pts',(-20.6231390461281,-43.0915949198549,
123.571582193787)) ;
#55905 = CARTESIAN_POINT('Ctrl Pts',(-20.9266062654661,-42.9116058393744,
123.611535793627)) ;
#55906 = CARTESIAN_POINT('Ctrl Pts',(-20.6047789342682,-43.1115502496993,
123.147760811554)) ;
#55907 = CARTESIAN_POINT('Ctrl Pts',(-20.9036603574372,-42.9315611692188,
123.081759157325)) ;
#55908 = CARTESIAN_POINT('Ctrl Pts',(-20.4437676887391,-43.1314257105047,
122.756956257546)) ;
#55909 = CARTESIAN_POINT('Ctrl Pts',(-20.7024014512796,-42.9514366300243,
122.593252469654)) ;
#55910 = CARTESIAN_POINT('Ctrl Pts',(-20.1577658156796,-43.1514100305563,
122.442758918448)) ;
#55911 = CARTESIAN_POINT('Ctrl Pts',(-20.3449003202566,-42.9714209500758,
122.200502446531)) ;
#55912 = CARTESIAN_POINT('Ctrl Pts',(-19.7825309062967,-43.1713380633459,
122.245718411537)) ;
#55913 = CARTESIAN_POINT('Ctrl Pts',(-19.8758679529114,-42.9913489828654,
121.954198379395)) ;
#55914 = CARTESIAN_POINT('Ctrl Pts',(-19.4327161765644,-43.1879468252857,
122.19803250865)) ;
#55915 = CARTESIAN_POINT('Ctrl Pts',(-19.4385731677958,-43.0079577448052,
121.894584975443)) ;
#55916 = CARTESIAN_POINT('Ctrl Pts',(-19.1575751517247,-43.2011344639758,
122.232458878335)) ;
#55917 = CARTESIAN_POINT('Ctrl Pts',(-19.0946716816628,-43.0211453834953,
121.937615802905)) ;
#55918 = CARTESIAN_POINT('Ctrl Pts',(-18.9568164762122,-43.2111208983359,
122.29383159449)) ;
#55919 = CARTESIAN_POINT('Ctrl Pts',(-18.843715306556,-43.0311318178554,122.014331379883)) ;
#55920 = CARTESIAN_POINT('Ctrl Pts',(-18.7693989059073,-43.2211302722953,
122.389560213479)) ;
#55921 = CARTESIAN_POINT('Ctrl Pts',(-18.609452700806,-43.0411411918148,122.133980200338)) ;
#55922 = CARTESIAN_POINT('Ctrl Pts',(-18.5463444276645,-43.2344203058605,
122.557741103274)) ;
#55923 = CARTESIAN_POINT('Ctrl Pts',(-18.3305857335314,-43.05443122538,122.34425230643)) ;
#55924 = CARTESIAN_POINT('Ctrl Pts',(-18.3288675857434,-43.251014293523,122.835683924907)) ;
#55925 = CARTESIAN_POINT('Ctrl Pts',(-18.0587919010383,-43.0710252130425,
122.691613440042)) ;
#55926 = CARTESIAN_POINT('Ctrl Pts',(-18.2190954075611,-43.2676465487985,
123.171796668551)) ;
#55927 = CARTESIAN_POINT('Ctrl Pts',(-17.9215463022561,-43.087657468318,123.111805423973)) ;
#55928 = CARTESIAN_POINT('Ctrl Pts',(-18.2039836097742,-43.2808889324664,
123.449819348037)) ;
#55929 = CARTESIAN_POINT('Ctrl Pts',(-17.9026645541855,-43.1008998519859,
123.459298795029)) ;
#55930 = CARTESIAN_POINT('Ctrl Pts',(-18.2283482509571,-43.2908031406938,
123.656820558235)) ;
#55931 = CARTESIAN_POINT('Ctrl Pts',(-17.9331154382768,-43.1108140602133,
123.718057560314)) ;
#55932 = CARTESIAN_POINT('Ctrl Pts',(-18.289369033941,-43.3008597799655,123.85923089601)) ;
#55933 = CARTESIAN_POINT('Ctrl Pts',(-18.0093888246454,-43.120870699485,123.971069080762)) ;
#55934 = CARTESIAN_POINT('Ctrl Pts',(-18.382402147398,-43.3107055863856,124.044152684337)) ;
#55935 = CARTESIAN_POINT('Ctrl Pts',(-18.1256798999717,-43.1307165059051,
124.202224696527)) ;
#55936 = CARTESIAN_POINT('Ctrl Pts',(-18.5083351564249,-43.3207505860188,
124.213670912525)) ;
#55937 = CARTESIAN_POINT('Ctrl Pts',(-18.2830849969303,-43.1407615055383,
124.414117164606)) ;
#55938 = CARTESIAN_POINT('Ctrl Pts',(-18.7114677451612,-43.3340316083915,
124.405150502509)) ;
#55939 = CARTESIAN_POINT('Ctrl Pts',(-18.53704325182,-43.1540425279111,124.653504054392)) ;
#55940 = CARTESIAN_POINT('Ctrl Pts',(-18.9580635205512,-43.3472290549162,
124.539134994554)) ;
#55941 = CARTESIAN_POINT('Ctrl Pts',(-18.8452649772685,-43.1672399744357,
124.820961905395)) ;
#55942 = CARTESIAN_POINT('Ctrl Pts',(-19.232360254932,-43.3606433527231,124.60475396977)) ;
#55943 = CARTESIAN_POINT('Ctrl Pts',(-19.1881152199753,-43.1806542722426,
124.902985566176)) ;
#55944 = CARTESIAN_POINT('Ctrl Pts',(-19.4388332017117,-43.3704824181259,
124.617341847239)) ;
#55945 = CARTESIAN_POINT('Ctrl Pts',(-19.4462101896793,-43.1904933376454,
124.918723959534)) ;
#55946 = CARTESIAN_POINT('Ctrl Pts',(-19.6473989067929,-43.3804656244036,
124.594097451494)) ;
#55947 = CARTESIAN_POINT('Ctrl Pts',(-19.7069166424804,-43.2004765439231,
124.889671061008)) ;
#55948 = CARTESIAN_POINT('Ctrl Pts',(-19.8481271767385,-43.3904168593164,
124.535103924099)) ;
#55949 = CARTESIAN_POINT('Ctrl Pts',(-19.9578281238951,-43.2104277788359,
124.815931888834)) ;
#55950 = CARTESIAN_POINT('Ctrl Pts',(-20.0366117400743,-43.400417859018,124.441917217521)) ;
#55951 = CARTESIAN_POINT('Ctrl Pts',(-20.1934350690971,-43.2204287785375,
124.699450982089)) ;
#55952 = CARTESIAN_POINT('Ctrl Pts',(-20.2063611151425,-43.4104492048053,
124.316781602561)) ;
#55953 = CARTESIAN_POINT('Ctrl Pts',(-20.4056235279798,-43.2304601243249,
124.543033701489)) ;
#55954 = CARTESIAN_POINT('Ctrl Pts',(-20.3494415293354,-43.4203029695104,
124.166967548006)) ;
#55955 = CARTESIAN_POINT('Ctrl Pts',(-20.5844761557595,-43.2403138890299,
124.3557679957)) ;
#55956 = CARTESIAN_POINT('Ctrl Pts',(-20.4660990695742,-43.4302736231787,
123.992841247419)) ;
#55957 = CARTESIAN_POINT('Ctrl Pts',(-20.7303004789797,-43.2502845426982,
124.138111587167)) ;
#55958 = CARTESIAN_POINT('Ctrl Pts',(-20.550990914283,-43.4402708668359,123.800540309338)) ;
#55959 = CARTESIAN_POINT('Ctrl Pts',(-20.8364178791155,-43.2602817863554,
123.897736473004)) ;
#55960 = CARTESIAN_POINT('Ctrl Pts',(-20.6011102529221,-43.4503043227801,
123.595664099876)) ;
#55961 = CARTESIAN_POINT('Ctrl Pts',(-20.8990697975969,-43.2703152422996,
123.641641842394)) ;
#55962 = CARTESIAN_POINT('Ctrl Pts',(-20.614988288072,-43.4601598270805,123.388915446738)) ;
#55963 = CARTESIAN_POINT('Ctrl Pts',(-20.9164201486326,-43.2801707466,123.383205983388)) ;
#55964 = CARTESIAN_POINT('Ctrl Pts',(-20.5927177301591,-43.4701592633666,
123.179916340754)) ;
#55965 = CARTESIAN_POINT('Ctrl Pts',(-20.8885847144271,-43.2901701828861,
123.121956715674)) ;
#55966 = CARTESIAN_POINT('Ctrl Pts',(-20.5353148533199,-43.4800537228825,
122.979940150803)) ;
#55967 = CARTESIAN_POINT('Ctrl Pts',(-20.8168337007792,-43.300064642402,122.871985466882)) ;
#55968 = CARTESIAN_POINT('Ctrl Pts',(-20.4424830563002,-43.4901168423341,
122.789877503651)) ;
#55969 = CARTESIAN_POINT('Ctrl Pts',(-20.7007964616095,-43.3101277618536,
122.634405970991)) ;
#55970 = CARTESIAN_POINT('Ctrl Pts',(-20.3209670354075,-43.4999564767461,
122.622428572666)) ;
#55971 = CARTESIAN_POINT('Ctrl Pts',(-20.5489034191562,-43.3199673962656,
122.425092863686)) ;
#55972 = CARTESIAN_POINT('Ctrl Pts',(-20.1690754221766,-43.5100196842319,
122.475206765639)) ;
#55973 = CARTESIAN_POINT('Ctrl Pts',(-20.359040830139,-43.3300306037514,122.241063678947)) ;
#55974 = CARTESIAN_POINT('Ctrl Pts',(-19.9967306491501,-43.5199137916111,
122.358701622462)) ;
#55975 = CARTESIAN_POINT('Ctrl Pts',(-20.1436111274981,-43.3399247111306,
122.095429795522)) ;
#55976 = CARTESIAN_POINT('Ctrl Pts',(-19.8061253691053,-43.5298561238035,
122.272988374327)) ;
#55977 = CARTESIAN_POINT('Ctrl Pts',(-19.9053553865689,-43.349867043323,121.988285685906)) ;
#55978 = CARTESIAN_POINT('Ctrl Pts',(-19.6023104751595,-43.5398567501185,
122.221256111772)) ;
#55979 = CARTESIAN_POINT('Ctrl Pts',(-19.6505873376654,-43.359867669638,121.92361775973)) ;
#55980 = CARTESIAN_POINT('Ctrl Pts',(-19.3917705372051,-43.5498984844004,
122.206031467105)) ;
#55981 = CARTESIAN_POINT('Ctrl Pts',(-19.3874126433925,-43.3699094039199,
121.904584247332)) ;
#55982 = CARTESIAN_POINT('Ctrl Pts',(-19.1862281430007,-43.5597239103495,
122.226676883472)) ;
#55983 = CARTESIAN_POINT('Ctrl Pts',(-19.1304837624119,-43.379734829869,121.930388446453)) ;
#55984 = CARTESIAN_POINT('Ctrl Pts',(-18.9826551708029,-43.5697807368771,
122.283706162221)) ;
#55985 = CARTESIAN_POINT('Ctrl Pts',(-18.8760169233883,-43.3897916563967,
122.001672515838)) ;
#55986 = CARTESIAN_POINT('Ctrl Pts',(-18.7946320656292,-43.5797081699987,
122.374314662117)) ;
#55987 = CARTESIAN_POINT('Ctrl Pts',(-18.6409865991805,-43.3997190895182,
122.114930896961)) ;
#55988 = CARTESIAN_POINT('Ctrl Pts',(-18.6244661109234,-43.5896581624049,
122.495982615423)) ;
#55989 = CARTESIAN_POINT('Ctrl Pts',(-18.4282774407069,-43.4096690819245,
122.267013929231)) ;
#55990 = CARTESIAN_POINT('Ctrl Pts',(-18.4767445700098,-43.5997133634789,
122.647173613548)) ;
#55991 = CARTESIAN_POINT('Ctrl Pts',(-18.2436237168024,-43.4197242829985,
122.456000772566)) ;
#55992 = CARTESIAN_POINT('Ctrl Pts',(-18.3599557995264,-43.6095356375312,
122.817488686517)) ;
#55993 = CARTESIAN_POINT('Ctrl Pts',(-18.0976352135923,-43.4295465570507,
122.66889381585)) ;
#55994 = CARTESIAN_POINT('Ctrl Pts',(-18.2721502560574,-43.6195915314905,
123.009781982913)) ;
#55995 = CARTESIAN_POINT('Ctrl Pts',(-17.9878760752162,-43.43960245101,122.909259307955)) ;
#55996 = CARTESIAN_POINT('Ctrl Pts',(-18.2200294874752,-43.6295322533356,
123.212171534823)) ;
#55997 = CARTESIAN_POINT('Ctrl Pts',(-17.9227225615872,-43.4495431728551,
123.162245934138)) ;
#55998 = CARTESIAN_POINT('Ctrl Pts',(-18.2032511636616,-43.6394365974222,
123.419718607872)) ;
#55999 = CARTESIAN_POINT('Ctrl Pts',(-17.9017472034625,-43.4594475169417,
123.421680109375)) ;
#56000 = CARTESIAN_POINT('Ctrl Pts',(-18.2231767398449,-43.6494832647217,
123.629971456285)) ;
#56001 = CARTESIAN_POINT('Ctrl Pts',(-17.9266517282372,-43.4694941842412,
123.684496298962)) ;
#56002 = CARTESIAN_POINT('Ctrl Pts',(-18.2782926714603,-43.6593788231716,
123.830608023793)) ;
#56003 = CARTESIAN_POINT('Ctrl Pts',(-17.9955444785647,-43.4793897426911,
123.935293204453)) ;
#56004 = CARTESIAN_POINT('Ctrl Pts',(-18.368880857869,-43.6694409018763,124.021733140042)) ;
#56005 = CARTESIAN_POINT('Ctrl Pts',(-18.1087774584325,-43.4894518213958,
124.174200467556)) ;
#56006 = CARTESIAN_POINT('Ctrl Pts',(-18.4885436290757,-43.6792836003421,
124.19057641474)) ;
#56007 = CARTESIAN_POINT('Ctrl Pts',(-18.2583544803866,-43.4992945198616,
124.385256639868)) ;
#56008 = CARTESIAN_POINT('Ctrl Pts',(-18.637534073092,-43.6892743742365,124.338585277532)) ;
#56009 = CARTESIAN_POINT('Ctrl Pts',(-18.4445910636902,-43.5092852937561,
124.570269448584)) ;
#56010 = CARTESIAN_POINT('Ctrl Pts',(-18.8089243606345,-43.6992022434715,
124.457711598807)) ;
#56011 = CARTESIAN_POINT('Ctrl Pts',(-18.6588280253007,-43.519213162991,124.719179491645)) ;
#56012 = CARTESIAN_POINT('Ctrl Pts',(-18.9994025238417,-43.7091909724413,
124.546144010481)) ;
#56013 = CARTESIAN_POINT('Ctrl Pts',(-18.8969249829765,-43.5292018919608,
124.829722059201)) ;
#56014 = CARTESIAN_POINT('Ctrl Pts',(-19.2034513375471,-43.7192303744251,
124.600051021114)) ;
#56015 = CARTESIAN_POINT('Ctrl Pts',(-19.1519853154671,-43.5392412939446,
124.897107997112)) ;
#56016 = CARTESIAN_POINT('Ctrl Pts',(-19.4095740593302,-43.7290705421618,
124.617767680818)) ;
#56017 = CARTESIAN_POINT('Ctrl Pts',(-19.4096395220042,-43.5490814616814,
124.919256070327)) ;
#56018 = CARTESIAN_POINT('Ctrl Pts',(-19.6200056310843,-43.7391187525363,
124.599348020896)) ;
#56019 = CARTESIAN_POINT('Ctrl Pts',(-19.6726790144309,-43.5591296720559,
124.89623358848)) ;
#56020 = CARTESIAN_POINT('Ctrl Pts',(-19.8219167217474,-43.7490659228241,
124.544896993531)) ;
#56021 = CARTESIAN_POINT('Ctrl Pts',(-19.9250688422979,-43.5690768423436,
124.828171804212)) ;
#56022 = CARTESIAN_POINT('Ctrl Pts',(-20.0108816230602,-43.7589767710792,
124.457103125973)) ;
#56023 = CARTESIAN_POINT('Ctrl Pts',(-20.1612764163773,-43.5789876905987,
124.718431010764)) ;
#56024 = CARTESIAN_POINT('Ctrl Pts',(-20.1841105037693,-43.7690330987569,
124.335929383685)) ;
#56025 = CARTESIAN_POINT('Ctrl Pts',(-20.3778135164832,-43.5890440182765,
124.566965650393)) ;
#56026 = CARTESIAN_POINT('Ctrl Pts',(-20.3307480730598,-43.7788835115255,
124.189689219311)) ;
#56027 = CARTESIAN_POINT('Ctrl Pts',(-20.5611126311556,-43.598894431045,124.384166137604)) ;
#56028 = CARTESIAN_POINT('Ctrl Pts',(-20.4523107242859,-43.7889103973592,
124.017478146335)) ;
#56029 = CARTESIAN_POINT('Ctrl Pts',(-20.7130674437929,-43.6089213168787,
124.168903399387)) ;
#56030 = CARTESIAN_POINT('Ctrl Pts',(-20.5416506384017,-43.79893901299,123.826498737951)) ;
#56031 = CARTESIAN_POINT('Ctrl Pts',(-20.8247441403498,-43.6189499325095,
123.930180059091)) ;
#56032 = CARTESIAN_POINT('Ctrl Pts',(-20.5958423754753,-43.8087842363675,
123.626753384018)) ;
#56033 = CARTESIAN_POINT('Ctrl Pts',(-20.892485943734,-43.628795155887,123.680497788547)) ;
#56034 = CARTESIAN_POINT('Ctrl Pts',(-20.6153678869501,-43.8187749184691,
123.417621815396)) ;
#56035 = CARTESIAN_POINT('Ctrl Pts',(-20.9168945754122,-43.6387858379886,
123.419083293923)) ;
#56036 = CARTESIAN_POINT('Ctrl Pts',(-20.5977356287722,-43.8288128071015,
123.207333737344)) ;
#56037 = CARTESIAN_POINT('Ctrl Pts',(-20.8948561362001,-43.648823726621,123.156223171612)) ;
#56038 = CARTESIAN_POINT('Ctrl Pts',(-20.5452446975445,-43.8386571422047,
123.007134061094)) ;
#56039 = CARTESIAN_POINT('Ctrl Pts',(-20.8292438815407,-43.6586680617242,
122.905971997051)) ;
#56040 = CARTESIAN_POINT('Ctrl Pts',(-20.4579454357753,-43.8486421044022,
122.816264363838)) ;
#56041 = CARTESIAN_POINT('Ctrl Pts',(-20.7201211841822,-43.6686530239217,
122.667383970088)) ;
#56042 = CARTESIAN_POINT('Ctrl Pts',(-20.3394267685731,-43.8585810459356,
122.644144630097)) ;
#56043 = CARTESIAN_POINT('Ctrl Pts',(-20.5719738574173,-43.6785919654551,
122.452232948962)) ;
#56044 = CARTESIAN_POINT('Ctrl Pts',(-20.1912921885784,-43.868622930907,122.493758530072)) ;
#56045 = CARTESIAN_POINT('Ctrl Pts',(-20.3868068905947,-43.6886338504265,
122.264249292206)) ;
#56046 = CARTESIAN_POINT('Ctrl Pts',(-20.0220013238299,-43.8785094788153,
122.373139062939)) ;
#56047 = CARTESIAN_POINT('Ctrl Pts',(-20.1751934661885,-43.6985203983348,
122.113473137148)) ;
#56048 = CARTESIAN_POINT('Ctrl Pts',(-19.8324762444945,-43.8885034043153,
122.282516116147)) ;
#56049 = CARTESIAN_POINT('Ctrl Pts',(-19.9382875920439,-43.7085143238348,
122.00019304693)) ;
#56050 = CARTESIAN_POINT('Ctrl Pts',(-19.6312362520306,-43.8984394954417,
122.226393147008)) ;
#56051 = CARTESIAN_POINT('Ctrl Pts',(-19.6867374287928,-43.7184504149613,
121.930037797362)) ;
#56052 = CARTESIAN_POINT('Ctrl Pts',(-19.4214139020312,-43.9084687644217,
122.205920422731)) ;
#56053 = CARTESIAN_POINT('Ctrl Pts',(-19.4244597082915,-43.7284796839412,
121.904445450295)) ;
#56054 = CARTESIAN_POINT('Ctrl Pts',(-19.2142240963958,-43.918351146981,122.221693374748)) ;
#56055 = CARTESIAN_POINT('Ctrl Pts',(-19.1654713411927,-43.7383620665005,
121.924160359609)) ;
#56056 = CARTESIAN_POINT('Ctrl Pts',(-19.009498669417,-43.9284036640689,122.274004896839)) ;
#56057 = CARTESIAN_POINT('Ctrl Pts',(-18.9095644693227,-43.7484145835884,
121.989548405927)) ;
#56058 = CARTESIAN_POINT('Ctrl Pts',(-18.819892626088,-43.9382977848928,122.359628820028)) ;
#56059 = CARTESIAN_POINT('Ctrl Pts',(-18.6725555426517,-43.7583087044123,
122.096577505199)) ;
#56060 = CARTESIAN_POINT('Ctrl Pts',(-18.6451418431221,-43.9483597643132,
122.478785235648)) ;
#56061 = CARTESIAN_POINT('Ctrl Pts',(-18.4541166119163,-43.7683706838327,
122.245521781282)) ;
#56062 = CARTESIAN_POINT('Ctrl Pts',(-18.4969665742692,-43.9582042975421,
122.623287056138)) ;
#56063 = CARTESIAN_POINT('Ctrl Pts',(-18.2688956917454,-43.7782152170616,
122.426149066414)) ;
#56064 = CARTESIAN_POINT('Ctrl Pts',(-18.3741086579576,-43.9681643764484,
122.792844278905)) ;
#56065 = CARTESIAN_POINT('Ctrl Pts',(-18.1153222213205,-43.7881752959679,
122.638095379869)) ;
#56066 = CARTESIAN_POINT('Ctrl Pts',(-18.2822146957173,-43.978202653021,122.982811873734)) ;
#56067 = CARTESIAN_POINT('Ctrl Pts',(-18.0004538037263,-43.7982135725405,
122.875554226901)) ;
#56068 = CARTESIAN_POINT('Ctrl Pts',(-18.2252522008148,-43.9880760395588,
123.182444364765)) ;
#56069 = CARTESIAN_POINT('Ctrl Pts',(-17.929249415048,-43.8080869590783,123.125095646741)) ;
#56070 = CARTESIAN_POINT('Ctrl Pts',(-18.2034535742499,-43.9981489823259,
123.393043925117)) ;
#56071 = CARTESIAN_POINT('Ctrl Pts',(-17.902000155015,-43.8181599018454,123.388344568527)) ;
#56072 = CARTESIAN_POINT('Ctrl Pts',(-18.2179298683599,-44.0079703964542,
123.599052536948)) ;
#56073 = CARTESIAN_POINT('Ctrl Pts',(-17.9200947060071,-43.8279813159737,
123.645856942406)) ;
#56074 = CARTESIAN_POINT('Ctrl Pts',(-18.2689797272042,-44.0180450265265,
123.804569296683)) ;
#56075 = CARTESIAN_POINT('Ctrl Pts',(-17.9839061109843,-43.8380559460461,
123.902752660096)) ;
#56076 = CARTESIAN_POINT('Ctrl Pts',(-18.3532690236661,-44.0279116638434,
123.994127168066)) ;
#56077 = CARTESIAN_POINT('Ctrl Pts',(-18.0892674355446,-43.8479225833629,
124.139701464818)) ;
#56078 = CARTESIAN_POINT('Ctrl Pts',(-18.4705660574724,-44.0379352092152,
124.169178578053)) ;
#56079 = CARTESIAN_POINT('Ctrl Pts',(-18.2358881549288,-43.8579461287347,
124.35851605704)) ;
#56080 = CARTESIAN_POINT('Ctrl Pts',(-18.6168901850746,-44.0479609607324,
124.320901604425)) ;
#56081 = CARTESIAN_POINT('Ctrl Pts',(-18.4187926356605,-43.8679718802519,
124.548170374758)) ;
#56082 = CARTESIAN_POINT('Ctrl Pts',(-18.7841854234927,-44.0578145477417,
124.443049390508)) ;
#56083 = CARTESIAN_POINT('Ctrl Pts',(-18.6279123308095,-43.8778254672613,
124.700856473596)) ;
#56084 = CARTESIAN_POINT('Ctrl Pts',(-18.9722447032616,-44.0677915079697,
124.535943542531)) ;
#56085 = CARTESIAN_POINT('Ctrl Pts',(-18.8629865022729,-43.8878024274892,
124.816974766447)) ;
#56086 = CARTESIAN_POINT('Ctrl Pts',(-19.1745538584046,-44.0778126509981,
124.594687633836)) ;
#56087 = CARTESIAN_POINT('Ctrl Pts',(-19.1158727505766,-43.8978235705177,
124.890405499311)) ;
#56088 = CARTESIAN_POINT('Ctrl Pts',(-19.3810867415163,-44.0876952570181,
124.617517604128)) ;
#56089 = CARTESIAN_POINT('Ctrl Pts',(-19.3740398930838,-43.9077061765376,
124.918943559921)) ;
#56090 = CARTESIAN_POINT('Ctrl Pts',(-19.5922777528914,-44.0977637276508,
124.603809178215)) ;
#56091 = CARTESIAN_POINT('Ctrl Pts',(-19.638028281114,-43.9177746471703,124.901808569108)) ;
#56092 = CARTESIAN_POINT('Ctrl Pts',(-19.7931371162424,-44.1075938108345,
124.555043900469)) ;
#56093 = CARTESIAN_POINT('Ctrl Pts',(-19.8891040806807,-43.927604730354,124.840852016009)) ;
#56094 = CARTESIAN_POINT('Ctrl Pts',(-19.9870797834277,-44.1176603705148,
124.470429298828)) ;
#56095 = CARTESIAN_POINT('Ctrl Pts',(-20.1315321755762,-43.9376712900344,
124.735084209579)) ;
#56096 = CARTESIAN_POINT('Ctrl Pts',(-20.1602737104804,-44.1275506203441,
124.355334521144)) ;
#56097 = CARTESIAN_POINT('Ctrl Pts',(-20.3480256594393,-43.9475615398636,
124.591215461536)) ;
#56098 = CARTESIAN_POINT('Ctrl Pts',(-20.3126945664649,-44.1375427860929,
124.210797364723)) ;
#56099 = CARTESIAN_POINT('Ctrl Pts',(-20.5385520109249,-43.9575537056124,
124.410544001641)) ;
#56100 = CARTESIAN_POINT('Ctrl Pts',(-20.4371805511039,-44.147505629689,124.042362117162)) ;
#56101 = CARTESIAN_POINT('Ctrl Pts',(-20.6941599749357,-43.9675165492085,
124.199999732296)) ;
#56102 = CARTESIAN_POINT('Ctrl Pts',(-20.5304651406943,-44.1574097985167,
123.856190907026)) ;
#56103 = CARTESIAN_POINT('Ctrl Pts',(-20.8107661787907,-43.9774207180363,
123.967284902407)) ;
#56104 = CARTESIAN_POINT('Ctrl Pts',(-20.5907535668492,-44.1674706734111,
123.653482764697)) ;
#56105 = CARTESIAN_POINT('Ctrl Pts',(-20.8861267323837,-43.9874815929306,
123.713900101314)) ;
#56106 = CARTESIAN_POINT('Ctrl Pts',(-20.6146904777119,-44.1773095767404,
123.447994903833)) ;
#56107 = CARTESIAN_POINT('Ctrl Pts',(-20.9160480545107,-43.99732049626,123.45703880834)) ;
#56108 = CARTESIAN_POINT('Ctrl Pts',(-20.6025093175598,-44.1873779531143,
123.236711105022)) ;
#56109 = CARTESIAN_POINT('Ctrl Pts',(-20.9008215571062,-44.0073888726339,
123.192934464728)) ;
#56110 = CARTESIAN_POINT('Ctrl Pts',(-20.5546520539257,-44.197258569747,123.034546463508)) ;
#56111 = CARTESIAN_POINT('Ctrl Pts',(-20.84099967691,-44.0172694892665,122.940227571267)) ;
#56112 = CARTESIAN_POINT('Ctrl Pts',(-20.4719127587511,-44.207249729976,122.841516718461)) ;
#56113 = CARTESIAN_POINT('Ctrl Pts',(-20.7375752828072,-44.0272606494955,
122.6989402697)) ;
#56114 = CARTESIAN_POINT('Ctrl Pts',(-20.3573466961592,-44.2172028034081,
122.666384942682)) ;
#56115 = CARTESIAN_POINT('Ctrl Pts',(-20.5943672384386,-44.0372137229276,
122.480025241696)) ;
#56116 = CARTESIAN_POINT('Ctrl Pts',(-20.2129041498641,-44.2272386390207,
122.512619796291)) ;
#56117 = CARTESIAN_POINT('Ctrl Pts',(-20.4138140211742,-44.0472495585402,
122.287819048033)) ;
#56118 = CARTESIAN_POINT('Ctrl Pts',(-20.0464710387891,-44.2371287657509,
122.387973352536)) ;
#56119 = CARTESIAN_POINT('Ctrl Pts',(-20.2057716276786,-44.0571396852704,
122.132010547307)) ;
#56120 = CARTESIAN_POINT('Ctrl Pts',(-19.8591825427843,-44.2471209475202,
122.292859773078)) ;
#56121 = CARTESIAN_POINT('Ctrl Pts',(-19.9716606493578,-44.0671318670397,
122.013118819214)) ;
#56122 = CARTESIAN_POINT('Ctrl Pts',(-19.6591233355574,-44.2570668874946,
122.232057906524)) ;
#56123 = CARTESIAN_POINT('Ctrl Pts',(-19.7215859697298,-44.0770778070142,
121.937116648818)) ;
#56124 = CARTESIAN_POINT('Ctrl Pts',(-19.4515603480813,-44.2670140712541,
122.206490694919)) ;
#56125 = CARTESIAN_POINT('Ctrl Pts',(-19.4621316011772,-44.0870249907736,
121.90515807925)) ;
#56126 = CARTESIAN_POINT('Ctrl Pts',(-19.2406254966303,-44.2770620095444,
122.217696911722)) ;
#56127 = CARTESIAN_POINT('Ctrl Pts',(-19.1984633098211,-44.097072929064,121.919166261235)) ;
#56128 = CARTESIAN_POINT('Ctrl Pts',(-19.0388958129296,-44.286909644358,122.264239155619)) ;
#56129 = CARTESIAN_POINT('Ctrl Pts',(-18.9462999516527,-44.1069205638775,
121.977344862589)) ;
#56130 = CARTESIAN_POINT('Ctrl Pts',(-18.8458583821311,-44.296871358056,122.345428988857)) ;
#56131 = CARTESIAN_POINT('Ctrl Pts',(-18.7050030348697,-44.1168822775755,
122.078833023452)) ;
#56132 = CARTESIAN_POINT('Ctrl Pts',(-18.6687933154075,-44.3068999938771,
122.459902791905)) ;
#56133 = CARTESIAN_POINT('Ctrl Pts',(-18.4836721333782,-44.1269109133967,
122.221925766882)) ;
#56134 = CARTESIAN_POINT('Ctrl Pts',(-18.5160880962946,-44.3168103086289,
122.601623849684)) ;
#56135 = CARTESIAN_POINT('Ctrl Pts',(-18.2927904239115,-44.1368212281484,
122.399078178037)) ;
#56136 = CARTESIAN_POINT('Ctrl Pts',(-18.3895506603922,-44.3267451792916,
122.767800295044)) ;
#56137 = CARTESIAN_POINT('Ctrl Pts',(-18.1346189319372,-44.1467560988111,
122.606799797155)) ;
#56138 = CARTESIAN_POINT('Ctrl Pts',(-18.2929514113174,-44.3367863616933,
122.955488189601)) ;
#56139 = CARTESIAN_POINT('Ctrl Pts',(-18.0138706729909,-44.1567972812129,
122.841409864053)) ;
#56140 = CARTESIAN_POINT('Ctrl Pts',(-18.2312003577601,-44.3466733331581,
123.153977478668)) ;
#56141 = CARTESIAN_POINT('Ctrl Pts',(-17.9366823753341,-44.1666842526776,
123.089522739971)) ;
#56142 = CARTESIAN_POINT('Ctrl Pts',(-18.2042924362549,-44.3566727654207,
123.362440492209)) ;
#56143 = CARTESIAN_POINT('Ctrl Pts',(-17.9030484192292,-44.1766836849402,
123.350101781401)) ;
#56144 = CARTESIAN_POINT('Ctrl Pts',(-18.2137740339436,-44.3665928306773,
123.5708007757)) ;
#56145 = CARTESIAN_POINT('Ctrl Pts',(-17.9149014699475,-44.1866037501968,
123.610552838734)) ;
#56146 = CARTESIAN_POINT('Ctrl Pts',(-18.2597764971867,-44.3766296832615,
123.776719598034)) ;
#56147 = CARTESIAN_POINT('Ctrl Pts',(-17.9724055288839,-44.196640602781,123.867950986219)) ;
#56148 = CARTESIAN_POINT('Ctrl Pts',(-18.3398426561002,-44.3865423426014,
123.969124187214)) ;
#56149 = CARTESIAN_POINT('Ctrl Pts',(-18.0724894957903,-44.206553262121,124.108457083401)) ;
#56150 = CARTESIAN_POINT('Ctrl Pts',(-18.4526095787518,-44.3965335545164,
124.146348677994)) ;
#56151 = CARTESIAN_POINT('Ctrl Pts',(-18.2134492760252,-44.2165444740359,
124.329987229938)) ;
#56152 = CARTESIAN_POINT('Ctrl Pts',(-18.5954817229628,-44.4065751959195,
124.301740665686)) ;
#56153 = CARTESIAN_POINT('Ctrl Pts',(-18.3920400926591,-44.226586115439,124.524226386443)) ;
#56154 = CARTESIAN_POINT('Ctrl Pts',(-18.7593291885529,-44.4164039901265,
124.427686436395)) ;
#56155 = CARTESIAN_POINT('Ctrl Pts',(-18.5968513117596,-44.236414909646,124.681658511702)) ;
#56156 = CARTESIAN_POINT('Ctrl Pts',(-18.9470682784548,-44.4264804012478,
124.525725017682)) ;
#56157 = CARTESIAN_POINT('Ctrl Pts',(-18.8315253712674,-44.2464913207673,
124.804205426369)) ;
#56158 = CARTESIAN_POINT('Ctrl Pts',(-19.1445330347221,-44.4363325342902,
124.588381426749)) ;
#56159 = CARTESIAN_POINT('Ctrl Pts',(-19.0783578845123,-44.2563434538097,
124.882525082165)) ;
#56160 = CARTESIAN_POINT('Ctrl Pts',(-19.3543837050247,-44.4464057686315,
124.616582421442)) ;
#56161 = CARTESIAN_POINT('Ctrl Pts',(-19.3406710041986,-44.2664166881511,
124.917774929088)) ;
#56162 = CARTESIAN_POINT('Ctrl Pts',(-19.561120757118,-44.4562472699582,124.608057607434)) ;
#56163 = CARTESIAN_POINT('Ctrl Pts',(-19.599093568999,-44.2762581894777,124.907117526601)) ;
#56164 = CARTESIAN_POINT('Ctrl Pts',(-19.7658378555304,-44.466208221553,124.564003318983)) ;
#56165 = CARTESIAN_POINT('Ctrl Pts',(-19.8549900005781,-44.2862191410725,
124.852048008168)) ;
#56166 = CARTESIAN_POINT('Ctrl Pts',(-19.9611338445933,-44.4762460392736,
124.484072288273)) ;
#56167 = CARTESIAN_POINT('Ctrl Pts',(-20.0991093096949,-44.2962569587932,
124.752132918217)) ;
#56168 = CARTESIAN_POINT('Ctrl Pts',(-20.1369108495217,-44.4861203885307,
124.373589262142)) ;
#56169 = CARTESIAN_POINT('Ctrl Pts',(-20.3188305769576,-44.3061313080502,
124.614027246397)) ;
#56170 = CARTESIAN_POINT('Ctrl Pts',(-20.2938275249447,-44.4961899392729,
124.231536291723)) ;
#56171 = CARTESIAN_POINT('Ctrl Pts',(-20.5149750945058,-44.3162008587924,
124.43646009178)) ;
#56172 = CARTESIAN_POINT('Ctrl Pts',(-20.4207811078669,-44.5060239587815,
124.068339987398)) ;
#56173 = CARTESIAN_POINT('Ctrl Pts',(-20.6736665784538,-44.326034878301,124.232462693822)) ;
#56174 = CARTESIAN_POINT('Ctrl Pts',(-20.5199150721139,-44.516058113361,123.882148162082)) ;
#56175 = CARTESIAN_POINT('Ctrl Pts',(-20.7975823822247,-44.3360690328805,
123.99972215947)) ;
#56176 = CARTESIAN_POINT('Ctrl Pts',(-20.5846066652837,-44.5260740391835,
123.68175257298)) ;
#56177 = CARTESIAN_POINT('Ctrl Pts',(-20.8784453198303,-44.346084958703,123.749227159108)) ;
#56178 = CARTESIAN_POINT('Ctrl Pts',(-20.6135027473333,-44.5359562943777,
123.476012739199)) ;
#56179 = CARTESIAN_POINT('Ctrl Pts',(-20.9145638048627,-44.3559672138973,
123.492051220725)) ;
#56180 = CARTESIAN_POINT('Ctrl Pts',(-20.6064192234333,-44.5459451008887,
123.266159254011)) ;
#56181 = CARTESIAN_POINT('Ctrl Pts',(-20.9057075529971,-44.3659560204082,
123.229734225015)) ;
#56182 = CARTESIAN_POINT('Ctrl Pts',(-20.5633248096925,-44.5558936681514,
123.061463359673)) ;
#56183 = CARTESIAN_POINT('Ctrl Pts',(-20.851837594289,-44.3759045876709,122.973864297995)) ;
#56184 = CARTESIAN_POINT('Ctrl Pts',(-20.4843220668197,-44.5659484734534,
122.865422401674)) ;
#56185 = CARTESIAN_POINT('Ctrl Pts',(-20.7530825572401,-44.3859593929729,
122.728813985254)) ;
#56186 = CARTESIAN_POINT('Ctrl Pts',(-20.3753421768984,-44.575767256717,122.69010150794)) ;
#56187 = CARTESIAN_POINT('Ctrl Pts',(-20.6168554016268,-44.3957781762364,
122.509662800766)) ;
#56188 = CARTESIAN_POINT('Ctrl Pts',(-20.2349634944572,-44.5858030290775,
122.532602841201)) ;
#56189 = CARTESIAN_POINT('Ctrl Pts',(-20.4413805690355,-44.4058139485971,
122.312790933982)) ;
#56190 = CARTESIAN_POINT('Ctrl Pts',(-20.0691703030276,-44.5958277281062,
122.402480939027)) ;
#56191 = CARTESIAN_POINT('Ctrl Pts',(-20.2341379247763,-44.4158386476257,
122.150140067202)) ;
#56192 = CARTESIAN_POINT('Ctrl Pts',(-19.8867241174746,-44.6056797313652,
122.304432926397)) ;
#56193 = CARTESIAN_POINT('Ctrl Pts',(-20.0060783373633,-44.4256906508848,
122.02758136636)) ;
#56194 = CARTESIAN_POINT('Ctrl Pts',(-19.6873786654677,-44.6156706657625,
122.238342902669)) ;
#56195 = CARTESIAN_POINT('Ctrl Pts',(-19.7568956898042,-44.435681585282,121.94497080327)) ;
#56196 = CARTESIAN_POINT('Ctrl Pts',(-19.481074169139,-44.6255885881936,122.207949395056)) ;
#56197 = CARTESIAN_POINT('Ctrl Pts',(-19.4990141869659,-44.4455995077131,
121.906980973268)) ;
#56198 = CARTESIAN_POINT('Ctrl Pts',(-19.2703469798628,-44.6356169438759,
122.213857027712)) ;
#56199 = CARTESIAN_POINT('Ctrl Pts',(-19.2356052976537,-44.4556278633954,
121.914367687732)) ;
#56200 = CARTESIAN_POINT('Ctrl Pts',(-19.0667685393293,-44.6455012283865,
122.255560649441)) ;
#56201 = CARTESIAN_POINT('Ctrl Pts',(-18.9811319609674,-44.465512147906,121.96649952011)) ;
#56202 = CARTESIAN_POINT('Ctrl Pts',(-18.8712365177251,-44.6554939122944,
122.332371985697)) ;
#56203 = CARTESIAN_POINT('Ctrl Pts',(-18.7367176524667,-44.4755048318139,
122.062515901464)) ;
#56204 = CARTESIAN_POINT('Ctrl Pts',(-18.6915565635913,-44.6655226493021,
122.442678617086)) ;
#56205 = CARTESIAN_POINT('Ctrl Pts',(-18.5121188959435,-44.4855335688216,
122.200401078651)) ;
#56206 = CARTESIAN_POINT('Ctrl Pts',(-18.5358279806812,-44.675408045931,122.580307301666)) ;
#56207 = CARTESIAN_POINT('Ctrl Pts',(-18.3174591679759,-44.4954189654505,
122.372439116207)) ;
#56208 = CARTESIAN_POINT('Ctrl Pts',(-18.4048030817091,-44.6853959313449,
122.74436173368)) ;
#56209 = CARTESIAN_POINT('Ctrl Pts',(-18.1536797929132,-44.5054068508644,
122.577508760513)) ;
#56210 = CARTESIAN_POINT('Ctrl Pts',(-18.3045194431609,-44.6953466340055,
122.927987236834)) ;
#56211 = CARTESIAN_POINT('Ctrl Pts',(-18.0283271817099,-44.515357553525,122.807042074235)) ;
#56212 = CARTESIAN_POINT('Ctrl Pts',(-18.2371653977238,-44.7053869521029,
123.128009185341)) ;
#56213 = CARTESIAN_POINT('Ctrl Pts',(-17.9441368872548,-44.5253978716224,
123.057070192323)) ;
#56214 = CARTESIAN_POINT('Ctrl Pts',(-18.2058765293099,-44.7152615174361,
123.333255667552)) ;
#56215 = CARTESIAN_POINT('Ctrl Pts',(-17.9050280764321,-44.5352724369556,
123.313629339714)) ;
#56216 = CARTESIAN_POINT('Ctrl Pts',(-18.2104928246588,-44.7252611774972,
123.543394996734)) ;
#56217 = CARTESIAN_POINT('Ctrl Pts',(-17.9108009161335,-44.5452720970167,
123.576303554665)) ;
#56218 = CARTESIAN_POINT('Ctrl Pts',(-18.2509713151308,-44.7351701726649,
123.747780176754)) ;
#56219 = CARTESIAN_POINT('Ctrl Pts',(-17.9614015774654,-44.5551810921844,
123.831785012539)) ;
#56220 = CARTESIAN_POINT('Ctrl Pts',(-18.3274676749511,-44.7452249138281,
123.944798878115)) ;
#56221 = CARTESIAN_POINT('Ctrl Pts',(-18.0570243117,-44.5652358333477,124.078057381576)) ;
#56222 = CARTESIAN_POINT('Ctrl Pts',(-18.4347054519244,-44.7550835257419,
124.122200708846)) ;
#56223 = CARTESIAN_POINT('Ctrl Pts',(-18.1910740416951,-44.5750944452614,
124.299808917773)) ;
#56224 = CARTESIAN_POINT('Ctrl Pts',(-18.5738749657264,-44.7651516480213,
124.281638187706)) ;
#56225 = CARTESIAN_POINT('Ctrl Pts',(-18.3650377632087,-44.5851625675408,
124.499103963494)) ;
#56226 = CARTESIAN_POINT('Ctrl Pts',(-18.7351819980848,-44.7750071187245,
124.411700343814)) ;
#56227 = CARTESIAN_POINT('Ctrl Pts',(-18.5666736484834,-44.595018038244,124.661680062482)) ;
#56228 = CARTESIAN_POINT('Ctrl Pts',(-18.9188616429352,-44.7850019782178,
124.513733292732)) ;
#56229 = CARTESIAN_POINT('Ctrl Pts',(-18.7962745857108,-44.6050128977374,
124.789218967145)) ;
#56230 = CARTESIAN_POINT('Ctrl Pts',(-19.1183492113281,-44.7950332315598,
124.58214803004)) ;
#56231 = CARTESIAN_POINT('Ctrl Pts',(-19.045634886792,-44.6150441510793,124.874734939647)) ;
#56232 = CARTESIAN_POINT('Ctrl Pts',(-19.323218690417,-44.8048999304329,124.61467366931)) ;
#56233 = CARTESIAN_POINT('Ctrl Pts',(-19.3017226630567,-44.6249108499524,
124.915389460474)) ;
#56234 = CARTESIAN_POINT('Ctrl Pts',(-19.5331246188192,-44.8148867461841,
124.61143594484)) ;
#56235 = CARTESIAN_POINT('Ctrl Pts',(-19.5641051552307,-44.6348976657036,
124.911339609499)) ;
#56236 = CARTESIAN_POINT('Ctrl Pts',(-19.7385308241501,-44.8248339513795,
124.572042427275)) ;
#56237 = CARTESIAN_POINT('Ctrl Pts',(-19.8208626336043,-44.644844870899,124.862095013967)) ;
#56238 = CARTESIAN_POINT('Ctrl Pts',(-19.9357852330403,-44.8348769395058,
124.496793289442)) ;
#56239 = CARTESIAN_POINT('Ctrl Pts',(-20.0674296682668,-44.6548878590253,
124.768031081867)) ;
#56240 = CARTESIAN_POINT('Ctrl Pts',(-20.1138908734245,-44.8447442941273,
124.39042646345)) ;
#56241 = CARTESIAN_POINT('Ctrl Pts',(-20.2900606910525,-44.6647552136468,
124.635070010857)) ;
#56242 = CARTESIAN_POINT('Ctrl Pts',(-20.2727462782933,-44.8547101874254,
124.25383373658)) ;
#56243 = CARTESIAN_POINT('Ctrl Pts',(-20.4886282485058,-44.6747211069449,
124.464326908031)) ;
#56244 = CARTESIAN_POINT('Ctrl Pts',(-20.4060875110616,-44.8647339648015,
124.090636353554)) ;
#56245 = CARTESIAN_POINT('Ctrl Pts',(-20.6553026895756,-44.684744884321,124.260328413018)) ;
#56246 = CARTESIAN_POINT('Ctrl Pts',(-20.5080877736395,-44.8746595127332,
123.908610854612)) ;
#56247 = CARTESIAN_POINT('Ctrl Pts',(-20.78280073358,-44.6946704322527,124.032794984463)) ;
#56248 = CARTESIAN_POINT('Ctrl Pts',(-20.5775102693516,-44.8845999891542,
123.711485460031)) ;
#56249 = CARTESIAN_POINT('Ctrl Pts',(-20.8695762749803,-44.7046109086737,
123.786387153794)) ;
#56250 = CARTESIAN_POINT('Ctrl Pts',(-20.6117719571326,-44.8946461988171,
123.503092758623)) ;
#56251 = CARTESIAN_POINT('Ctrl Pts',(-20.9124006495194,-44.7146571183366,
123.525895807867)) ;
#56252 = CARTESIAN_POINT('Ctrl Pts',(-20.6095960962421,-44.9045074554789,
123.295771336016)) ;
#56253 = CARTESIAN_POINT('Ctrl Pts',(-20.9096780313366,-44.7245183749984,
123.266743788821)) ;
#56254 = CARTESIAN_POINT('Ctrl Pts',(-20.5713071076348,-44.9145010837542,
123.08922311595)) ;
#56255 = CARTESIAN_POINT('Ctrl Pts',(-20.8618140137241,-44.7345120032737,
123.008558951065)) ;
#56256 = CARTESIAN_POINT('Ctrl Pts',(-20.4983191373996,-44.9244264810644,
122.893708018613)) ;
#56257 = CARTESIAN_POINT('Ctrl Pts',(-20.7705763699212,-44.7444374005839,
122.764165937493)) ;
#56258 = CARTESIAN_POINT('Ctrl Pts',(-20.391433863342,-44.9344543889746,122.712025942917)) ;
#56259 = CARTESIAN_POINT('Ctrl Pts',(-20.6369673170847,-44.7544653084941,
122.537064718047)) ;
#56260 = CARTESIAN_POINT('Ctrl Pts',(-20.2566836205498,-44.9443407046438,
122.55374389634)) ;
#56261 = CARTESIAN_POINT('Ctrl Pts',(-20.4685272890457,-44.7643516241633,
122.339213894199)) ;
#56262 = CARTESIAN_POINT('Ctrl Pts',(-20.0942650307571,-44.9543722995476,
122.419270807689)) ;
#56263 = CARTESIAN_POINT('Ctrl Pts',(-20.2655021979111,-44.7743832190671,
122.171124667604)) ;
#56264 = CARTESIAN_POINT('Ctrl Pts',(-19.9137299172441,-44.9642545424993,
122.316394133528)) ;
#56265 = CARTESIAN_POINT('Ctrl Pts',(-20.0398318507275,-44.7842654620188,
122.042531241619)) ;
#56266 = CARTESIAN_POINT('Ctrl Pts',(-19.7146500331995,-44.9743140135291,
122.24510774136)) ;
#56267 = CARTESIAN_POINT('Ctrl Pts',(-19.7909809655389,-44.7943249330486,
121.953425884244)) ;
#56268 = CARTESIAN_POINT('Ctrl Pts',(-19.5101771870513,-44.9841804581923,
122.210176444507)) ;
#56269 = CARTESIAN_POINT('Ctrl Pts',(-19.5353894138437,-44.8041913777118,
121.909764540017)) ;
#56270 = CARTESIAN_POINT('Ctrl Pts',(-19.3006636334398,-44.994146582641,122.210628861832)) ;
#56271 = CARTESIAN_POINT('Ctrl Pts',(-19.2734974473515,-44.8141575021605,
121.910332881096)) ;
#56272 = CARTESIAN_POINT('Ctrl Pts',(-19.0931406754314,-45.0041768260321,
122.248023638702)) ;
#56273 = CARTESIAN_POINT('Ctrl Pts',(-19.0140941941528,-44.8241877455516,
121.957079095909)) ;
#56274 = CARTESIAN_POINT('Ctrl Pts',(-18.8978469326455,-45.0140698609852,
122.319615465346)) ;
#56275 = CARTESIAN_POINT('Ctrl Pts',(-18.7699778545703,-44.8340807805047,
122.046571668212)) ;
#56276 = CARTESIAN_POINT('Ctrl Pts',(-18.7150830259635,-45.024120775222,122.425627543441)) ;
#56277 = CARTESIAN_POINT('Ctrl Pts',(-18.541524921749,-44.8441316947415,122.179088598063)) ;
#56278 = CARTESIAN_POINT('Ctrl Pts',(-18.5560590605076,-45.0340106014466,
122.559577916951)) ;
#56279 = CARTESIAN_POINT('Ctrl Pts',(-18.3427444000537,-44.8540215209661,
122.346531093126)) ;
#56280 = CARTESIAN_POINT('Ctrl Pts',(-18.3758084791143,-45.0473454164935,
122.774344433157)) ;
#56281 = CARTESIAN_POINT('Ctrl Pts',(-18.1174461020188,-44.867356336013,122.614979486919)) ;
#56282 = CARTESIAN_POINT('Ctrl Pts',(-18.2567530669862,-45.060622507665,123.03030649385)) ;
#56283 = CARTESIAN_POINT('Ctrl Pts',(-17.9686335759019,-44.8806334271845,
122.934896659079)) ;
#56284 = CARTESIAN_POINT('Ctrl Pts',(-18.2079946984886,-45.0738707962633,
123.304511382558)) ;
#56285 = CARTESIAN_POINT('Ctrl Pts',(-17.9076731560715,-44.8938817157828,
123.277709414328)) ;
#56286 = CARTESIAN_POINT('Ctrl Pts',(-18.2078213156215,-45.0839256377574,
123.515872423413)) ;
#56287 = CARTESIAN_POINT('Ctrl Pts',(-17.9074623162929,-44.9039365572769,
123.5418995713)) ;
#56288 = CARTESIAN_POINT('Ctrl Pts',(-18.2432033461838,-45.0937566270649,
123.719534287493)) ;
#56289 = CARTESIAN_POINT('Ctrl Pts',(-17.951691989716,-44.9137675465844,123.796479325904)) ;
#56290 = CARTESIAN_POINT('Ctrl Pts',(-18.3149935437228,-45.1038331913881,
123.918803697903)) ;
#56291 = CARTESIAN_POINT('Ctrl Pts',(-18.0414310831757,-44.9238441109076,
124.045563596384)) ;
#56292 = CARTESIAN_POINT('Ctrl Pts',(-18.4179463690853,-45.1136825165221,
124.098479005577)) ;
#56293 = CARTESIAN_POINT('Ctrl Pts',(-18.1701298254122,-44.9336934360416,
124.2701600857)) ;
#56294 = CARTESIAN_POINT('Ctrl Pts',(-18.5971230912793,-45.1270305161593,
124.314496308919)) ;
#56295 = CARTESIAN_POINT('Ctrl Pts',(-18.3940753257468,-44.9470414356789,
124.540160290324)) ;
#56296 = CARTESIAN_POINT('Ctrl Pts',(-18.8849989168967,-45.1436152756959,
124.518050402463)) ;
#56297 = CARTESIAN_POINT('Ctrl Pts',(-18.7539725180067,-44.9636261952154,
124.794623795797)) ;
#56298 = CARTESIAN_POINT('Ctrl Pts',(-19.224601952066,-45.160183827044,124.611932790248)) ;
#56299 = CARTESIAN_POINT('Ctrl Pts',(-19.1783954642699,-44.9801947465635,
124.911954796787)) ;
#56300 = CARTESIAN_POINT('Ctrl Pts',(-19.5054327742707,-45.173543651863,124.613960046694)) ;
#56301 = CARTESIAN_POINT('Ctrl Pts',(-19.5295000394796,-44.9935545713825,
124.914496420961)) ;
#56302 = CARTESIAN_POINT('Ctrl Pts',(-19.7108114161679,-45.1834490606937,
124.579447586727)) ;
#56303 = CARTESIAN_POINT('Ctrl Pts',(-19.7862085515913,-45.0034599802132,
124.871351922951)) ;
#56304 = CARTESIAN_POINT('Ctrl Pts',(-19.9082218453753,-45.1934090872777,
124.509714834404)) ;
#56305 = CARTESIAN_POINT('Ctrl Pts',(-20.0329770476807,-45.0134200067972,
124.784181636003)) ;
#56306 = CARTESIAN_POINT('Ctrl Pts',(-20.1511287525541,-45.206666671463,124.372952742759)) ;
#56307 = CARTESIAN_POINT('Ctrl Pts',(-20.3365929404721,-45.0266775909825,
124.613239797446)) ;
#56308 = CARTESIAN_POINT('Ctrl Pts',(-20.4042739888879,-45.2233178829577,
124.12545280733)) ;
#56309 = CARTESIAN_POINT('Ctrl Pts',(-20.6530388480297,-45.0433288024772,
124.303846929878)) ;
#56310 = CARTESIAN_POINT('Ctrl Pts',(-20.5876289534092,-45.243236097068,123.743705041852)) ;
#56311 = CARTESIAN_POINT('Ctrl Pts',(-20.8822225930643,-45.0632470165875,
123.826665489857)) ;
#56312 = CARTESIAN_POINT('Ctrl Pts',(-20.630530145128,-45.2631138602888,123.323172796485)) ;
#56313 = CARTESIAN_POINT('Ctrl Pts',(-20.9358462102665,-45.0831247798083,
123.300999284678)) ;
#56314 = CARTESIAN_POINT('Ctrl Pts',(-20.5263138562725,-45.283126528076,122.910688719133)) ;
#56315 = CARTESIAN_POINT('Ctrl Pts',(-20.8055712373151,-45.1031374475955,
122.785395465241)) ;
#56316 = CARTESIAN_POINT('Ctrl Pts',(-20.2902208181443,-45.3029390507426,
122.561698389052)) ;
#56317 = CARTESIAN_POINT('Ctrl Pts',(-20.5104525720983,-45.1229499702621,
122.349160972054)) ;
#56318 = CARTESIAN_POINT('Ctrl Pts',(-19.9467946863038,-45.3229223507425,
122.31164395972)) ;
#56319 = CARTESIAN_POINT('Ctrl Pts',(-20.0811678726648,-45.142933270262,122.036595982088)) ;
#56320 = CARTESIAN_POINT('Ctrl Pts',(-19.5402451083145,-45.3428166278438,
122.194572866398)) ;
#56321 = CARTESIAN_POINT('Ctrl Pts',(-19.5729808271212,-45.1628275473633,
121.890260817215)) ;
#56322 = CARTESIAN_POINT('Ctrl Pts',(-19.1173631256665,-45.3627493896015,
122.222652545081)) ;
#56323 = CARTESIAN_POINT('Ctrl Pts',(-19.0443792387682,-45.1827603091211,
121.925363493059)) ;
#56324 = CARTESIAN_POINT('Ctrl Pts',(-18.7289083515365,-45.3827153953663,
122.393915397857)) ;
#56325 = CARTESIAN_POINT('Ctrl Pts',(-18.5588123387542,-45.2027263148858,
122.139444767304)) ;
#56326 = CARTESIAN_POINT('Ctrl Pts',(-18.4233281728612,-45.4025939275311,
122.685968903404)) ;
#56327 = CARTESIAN_POINT('Ctrl Pts',(-18.1768400074142,-45.2226048470507,
122.504512707757)) ;
#56328 = CARTESIAN_POINT('Ctrl Pts',(-18.2348448265652,-45.4225335941915,
123.065690568163)) ;
#56329 = CARTESIAN_POINT('Ctrl Pts',(-17.9412382744807,-45.242544513711,122.97916517486)) ;
#56330 = CARTESIAN_POINT('Ctrl Pts',(-18.1872285477888,-45.4424284688368,
123.486065831409)) ;
#56331 = CARTESIAN_POINT('Ctrl Pts',(-17.8817201355159,-45.2624393883564,
123.504633155364)) ;
#56332 = CARTESIAN_POINT('Ctrl Pts',(-18.2855438839301,-45.4623356081302,
123.897669851793)) ;
#56333 = CARTESIAN_POINT('Ctrl Pts',(-18.0046155635177,-45.2823465276497,
124.019136501182)) ;
#56334 = CARTESIAN_POINT('Ctrl Pts',(-18.5179787925655,-45.4822461562087,
124.251671884329)) ;
#56335 = CARTESIAN_POINT('Ctrl Pts',(-18.2951592683826,-45.3022570757282,
124.461637555515)) ;
#56336 = CARTESIAN_POINT('Ctrl Pts',(-18.8603532025877,-45.5023147415659,
124.506196821107)) ;
#56337 = CARTESIAN_POINT('Ctrl Pts',(-18.7231289191546,-45.3223256610853,
124.779793281065)) ;
#56338 = CARTESIAN_POINT('Ctrl Pts',(-19.2632916538043,-45.5220965388806,
124.627332831793)) ;
#56339 = CARTESIAN_POINT('Ctrl Pts',(-19.2267990765142,-45.3421074584001,
124.931211593352)) ;
#56340 = CARTESIAN_POINT('Ctrl Pts',(-19.6879024854321,-45.5421040858251,
124.604065554752)) ;
#56341 = CARTESIAN_POINT('Ctrl Pts',(-19.7575625515508,-45.3621150053447,
124.902127405383)) ;
#56342 = CARTESIAN_POINT('Ctrl Pts',(-20.0757175915424,-45.561925824128,124.438753736194)) ;
#56343 = CARTESIAN_POINT('Ctrl Pts',(-20.2423289588513,-45.3819367436475,
124.695488931314)) ;
#56344 = CARTESIAN_POINT('Ctrl Pts',(-20.3866991980944,-45.5819058440321,
124.149413523319)) ;
#56345 = CARTESIAN_POINT('Ctrl Pts',(-20.6310564600973,-45.4019167635517,
124.333814619586)) ;
#56346 = CARTESIAN_POINT('Ctrl Pts',(-20.579213898747,-45.6018232952944,123.772183038511)) ;
#56347 = CARTESIAN_POINT('Ctrl Pts',(-20.8717000557852,-45.4218342148139,
123.86227801888)) ;
#56348 = CARTESIAN_POINT('Ctrl Pts',(-20.6323140250136,-45.6216982164671,
123.35290988801)) ;
#56349 = CARTESIAN_POINT('Ctrl Pts',(-20.9380767682915,-45.4417091359866,
123.338188475174)) ;
#56350 = CARTESIAN_POINT('Ctrl Pts',(-20.5381944095279,-45.6417225850179,
122.937699622663)) ;
#56351 = CARTESIAN_POINT('Ctrl Pts',(-20.8204289203156,-45.4617335045374,
122.819174892928)) ;
#56352 = CARTESIAN_POINT('Ctrl Pts',(-20.3096913478822,-45.6615892693914,
122.582336964708)) ;
#56353 = CARTESIAN_POINT('Ctrl Pts',(-20.5348026193638,-45.4816001889109,
122.374971928243)) ;
#56354 = CARTESIAN_POINT('Ctrl Pts',(-19.9728378596493,-45.6815330912376,
122.324818392206)) ;
#56355 = CARTESIAN_POINT('Ctrl Pts',(-20.1137378288441,-45.5015440107571,
122.053072103545)) ;
#56356 = CARTESIAN_POINT('Ctrl Pts',(-19.5689770807575,-45.7014404604891,
122.198058930962)) ;
#56357 = CARTESIAN_POINT('Ctrl Pts',(-19.608913673455,-45.5214513800086,121.89462058423)) ;
#56358 = CARTESIAN_POINT('Ctrl Pts',(-19.1467685091688,-45.7213151582358,
122.215906390113)) ;
#56359 = CARTESIAN_POINT('Ctrl Pts',(-19.0811541091783,-45.5413260777553,
121.916926618802)) ;
#56360 = CARTESIAN_POINT('Ctrl Pts',(-18.7538192203983,-45.7412971007575,
122.377543259028)) ;
#56361 = CARTESIAN_POINT('Ctrl Pts',(-18.5899663031638,-45.5613080202771,
122.118969492211)) ;
#56362 = CARTESIAN_POINT('Ctrl Pts',(-18.4411535486972,-45.7611997676684,
122.662651717635)) ;
#56363 = CARTESIAN_POINT('Ctrl Pts',(-18.1991325994995,-45.5812106871879,
122.475351878632)) ;
#56364 = CARTESIAN_POINT('Ctrl Pts',(-18.2438603449424,-45.7810551252071,
123.035964325074)) ;
#56365 = CARTESIAN_POINT('Ctrl Pts',(-17.9525130134343,-45.6010660447266,
122.941989689319)) ;
#56366 = CARTESIAN_POINT('Ctrl Pts',(-18.1856815046609,-45.8011191639231,
123.458527247341)) ;
#56367 = CARTESIAN_POINT('Ctrl Pts',(-17.879785330471,-45.6211300834426,123.47019336816)) ;
#56368 = CARTESIAN_POINT('Ctrl Pts',(-18.2744755391468,-45.8209743436481,
123.871419259032)) ;
#56369 = CARTESIAN_POINT('Ctrl Pts',(-17.9907738384312,-45.6409852631677,
123.986308188101)) ;
#56370 = CARTESIAN_POINT('Ctrl Pts',(-18.4997930018078,-45.8409544483126,
124.231383616986)) ;
#56371 = CARTESIAN_POINT('Ctrl Pts',(-18.2724161798347,-45.6609653678321,
124.4362659272)) ;
#56372 = CARTESIAN_POINT('Ctrl Pts',(-18.8314673108359,-45.8607635534824,
124.49118909027)) ;
#56373 = CARTESIAN_POINT('Ctrl Pts',(-18.6870078951238,-45.6807744730019,
124.761025281512)) ;
#56374 = CARTESIAN_POINT('Ctrl Pts',(-19.2352299421936,-45.8807561738231,
124.623756846675)) ;
#56375 = CARTESIAN_POINT('Ctrl Pts',(-19.1916999501142,-45.7007670933426,
124.926741075057)) ;
#56376 = CARTESIAN_POINT('Ctrl Pts',(-19.586815630739,-45.8972956563272,124.612921446625)) ;
#56377 = CARTESIAN_POINT('Ctrl Pts',(-19.6312118173661,-45.7173065758467,
124.913196410162)) ;
#56378 = CARTESIAN_POINT('Ctrl Pts',(-19.8558718361537,-45.9106599743914,
124.532044526927)) ;
#56379 = CARTESIAN_POINT('Ctrl Pts',(-19.9674993569513,-45.7306708939109,
124.812112387827)) ;
#56380 = CARTESIAN_POINT('Ctrl Pts',(-20.1042094269978,-45.9238775768929,
124.407362624785)) ;
#56381 = CARTESIAN_POINT('Ctrl Pts',(-20.2779790595756,-45.7438884964124,
124.656227492583)) ;
#56382 = CARTESIAN_POINT('Ctrl Pts',(-20.368961477355,-45.9405351711707,124.172135837994)) ;
#56383 = CARTESIAN_POINT('Ctrl Pts',(-20.6088613727262,-45.7605460906902,
124.362235325877)) ;
#56384 = CARTESIAN_POINT('Ctrl Pts',(-20.5701552804557,-45.9604008732124,
123.800652640584)) ;
#56385 = CARTESIAN_POINT('Ctrl Pts',(-20.8603771683471,-45.7804117927319,
123.897882286037)) ;
#56386 = CARTESIAN_POINT('Ctrl Pts',(-20.6228240088762,-45.9770305999024,
123.451100482239)) ;
#56387 = CARTESIAN_POINT('Ctrl Pts',(-20.9262145453754,-45.797041519422,123.460911151543)) ;
#56388 = CARTESIAN_POINT('Ctrl Pts',(-20.5914361189551,-45.9903197150403,
123.173415800151)) ;
#56389 = CARTESIAN_POINT('Ctrl Pts',(-20.8869828201664,-45.8103306345598,
123.113835882185)) ;
#56390 = CARTESIAN_POINT('Ctrl Pts',(-20.5323594467668,-46.0002840620174,
122.972457040269)) ;
#56391 = CARTESIAN_POINT('Ctrl Pts',(-20.8131372218145,-45.8202949815369,
122.862628157977)) ;
#56392 = CARTESIAN_POINT('Ctrl Pts',(-20.4397374973719,-46.0102124300189,
122.785404683368)) ;
#56393 = CARTESIAN_POINT('Ctrl Pts',(-20.6973720960677,-45.8302233495384,
122.628822672009)) ;
#56394 = CARTESIAN_POINT('Ctrl Pts',(-20.2747057487913,-46.0234958631076,
122.560148912213)) ;
#56395 = CARTESIAN_POINT('Ctrl Pts',(-20.4910362461603,-45.8435067826271,
122.347203200307)) ;
#56396 = CARTESIAN_POINT('Ctrl Pts',(-19.9984819879349,-46.0401479408479,
122.338567938627)) ;
#56397 = CARTESIAN_POINT('Ctrl Pts',(-20.1458260850782,-45.8601588603674,
122.070280119361)) ;
#56398 = CARTESIAN_POINT('Ctrl Pts',(-19.6654083029669,-46.0566993101488,
122.225111293764)) ;
#56399 = CARTESIAN_POINT('Ctrl Pts',(-19.7294257177977,-45.8767102296683,
121.928426697148)) ;
#56400 = CARTESIAN_POINT('Ctrl Pts',(-19.3866709636188,-46.0699867382977,
122.205956450198)) ;
#56401 = CARTESIAN_POINT('Ctrl Pts',(-19.3810452958533,-45.8899976578173,
121.904492705399)) ;
#56402 = CARTESIAN_POINT('Ctrl Pts',(-19.1767289526485,-46.0800312779978,
122.228493274204)) ;
#56403 = CARTESIAN_POINT('Ctrl Pts',(-19.1186091401269,-45.9000421975174,
121.932658290832)) ;
#56404 = CARTESIAN_POINT('Ctrl Pts',(-18.9778591393557,-46.0898741198217,
122.285724273761)) ;
#56405 = CARTESIAN_POINT('Ctrl Pts',(-18.8700233534441,-45.9098850393412,
122.004195044946)) ;
#56406 = CARTESIAN_POINT('Ctrl Pts',(-18.7890949169887,-46.0998584040686,
122.37747258679)) ;
#56407 = CARTESIAN_POINT('Ctrl Pts',(-18.6340661749216,-45.9198693235881,
122.118877741015)) ;
#56408 = CARTESIAN_POINT('Ctrl Pts',(-18.6197187705816,-46.1098080494678,
122.500228764062)) ;
#56409 = CARTESIAN_POINT('Ctrl Pts',(-18.4223444456652,-45.9298189689873,
122.272320772466)) ;
#56410 = CARTESIAN_POINT('Ctrl Pts',(-18.4733104190095,-46.1198078111562,
122.651108437036)) ;
#56411 = CARTESIAN_POINT('Ctrl Pts',(-18.2393318881678,-45.9398187306757,
122.460918444063)) ;
#56412 = CARTESIAN_POINT('Ctrl Pts',(-18.3552472327061,-46.1298391571151,
122.825850445849)) ;
#56413 = CARTESIAN_POINT('Ctrl Pts',(-18.0917505485482,-45.9498500766346,
122.679344429052)) ;
#56414 = CARTESIAN_POINT('Ctrl Pts',(-18.2705494607926,-46.1396941115922,
123.014933391385)) ;
#56415 = CARTESIAN_POINT('Ctrl Pts',(-17.9858757130869,-45.9597050311117,
122.91569706194)) ;
#56416 = CARTESIAN_POINT('Ctrl Pts',(-18.2188977661992,-46.1496666495927,
123.218103084829)) ;
#56417 = CARTESIAN_POINT('Ctrl Pts',(-17.9213083459026,-45.9696775691122,
123.169658598768)) ;
#56418 = CARTESIAN_POINT('Ctrl Pts',(-18.2032838337834,-46.1596616433277,
123.427680803576)) ;
#56419 = CARTESIAN_POINT('Ctrl Pts',(-17.9017881315009,-45.9796725628472,
123.431630618323)) ;
#56420 = CARTESIAN_POINT('Ctrl Pts',(-18.2246312081846,-46.1696957021218,
123.637527281541)) ;
#56421 = CARTESIAN_POINT('Ctrl Pts',(-17.9284695513896,-45.9897066216413,
123.693939039841)) ;
#56422 = CARTESIAN_POINT('Ctrl Pts',(-18.2807599390842,-46.1795510449448,
123.836991427032)) ;
#56423 = CARTESIAN_POINT('Ctrl Pts',(-17.9986278341019,-45.9995619644643,
123.943270201465)) ;
#56424 = CARTESIAN_POINT('Ctrl Pts',(-18.3717042160913,-46.1895505242904,
124.026480311802)) ;
#56425 = CARTESIAN_POINT('Ctrl Pts',(-18.1123057055239,-46.0095614438099,
124.180132595363)) ;
#56426 = CARTESIAN_POINT('Ctrl Pts',(-18.4927341945723,-46.1994449730457,
124.195705746537)) ;
#56427 = CARTESIAN_POINT('Ctrl Pts',(-18.2635910837265,-46.0194558925652,
124.391666206206)) ;
#56428 = CARTESIAN_POINT('Ctrl Pts',(-18.6438307854289,-46.2095080924802,
124.343730651591)) ;
#56429 = CARTESIAN_POINT('Ctrl Pts',(-18.4524598571284,-46.0295190119997,
124.576699295211)) ;
#56430 = CARTESIAN_POINT('Ctrl Pts',(-18.8143876956358,-46.2193477377214,
124.460844662452)) ;
#56431 = CARTESIAN_POINT('Ctrl Pts',(-18.6656547762322,-46.0393586572409,
124.72309430424)) ;
#56432 = CARTESIAN_POINT('Ctrl Pts',(-19.0067961425218,-46.2294109019075,
124.548731031768)) ;
#56433 = CARTESIAN_POINT('Ctrl Pts',(-18.9061641631857,-46.049421821427,124.832954725932)) ;
#56434 = CARTESIAN_POINT('Ctrl Pts',(-19.2082002254343,-46.2393051716563,
124.60082520619)) ;
#56435 = CARTESIAN_POINT('Ctrl Pts',(-19.157918897676,-46.0593160911758,124.898075179846)) ;
#56436 = CARTESIAN_POINT('Ctrl Pts',(-19.4164887508991,-46.2492468976701,
124.617795648775)) ;
#56437 = CARTESIAN_POINT('Ctrl Pts',(-19.4182795982732,-46.0692578171896,
124.919290922876)) ;
#56438 = CARTESIAN_POINT('Ctrl Pts',(-19.625908760725,-46.2592497863295,124.598307790084)) ;
#56439 = CARTESIAN_POINT('Ctrl Pts',(-19.6800549446301,-46.079260705849,124.894933738514)) ;
#56440 = CARTESIAN_POINT('Ctrl Pts',(-19.8293605211461,-46.2692896351235,
124.542189850238)) ;
#56441 = CARTESIAN_POINT('Ctrl Pts',(-19.934370335903,-46.089300554643,124.824788940048)) ;
#56442 = CARTESIAN_POINT('Ctrl Pts',(-20.0161177451334,-46.2791138505843,
124.453953136808)) ;
#56443 = CARTESIAN_POINT('Ctrl Pts',(-20.1678185634973,-46.0991247701039,
124.714495173681)) ;
#56444 = CARTESIAN_POINT('Ctrl Pts',(-20.1888529807882,-46.2891706940779,
124.332063949481)) ;
#56445 = CARTESIAN_POINT('Ctrl Pts',(-20.3837390424516,-46.1091816135974,
124.562135863829)) ;
#56446 = CARTESIAN_POINT('Ctrl Pts',(-20.3357237419567,-46.2990993034739,
124.183735609964)) ;
#56447 = CARTESIAN_POINT('Ctrl Pts',(-20.5673296045431,-46.1191102229934,
124.376727071138)) ;
#56448 = CARTESIAN_POINT('Ctrl Pts',(-20.4553698807106,-46.3090511875118,
124.012092768846)) ;
#56449 = CARTESIAN_POINT('Ctrl Pts',(-20.7168895337345,-46.1290621070313,
124.162174745084)) ;
#56450 = CARTESIAN_POINT('Ctrl Pts',(-20.5439344328811,-46.3191041403194,
123.820215375579)) ;
#56451 = CARTESIAN_POINT('Ctrl Pts',(-20.8275975549194,-46.1391150598389,
123.922329195925)) ;
#56452 = CARTESIAN_POINT('Ctrl Pts',(-20.5969834126444,-46.3289270167856,
123.620621819729)) ;
#56453 = CARTESIAN_POINT('Ctrl Pts',(-20.8939114404305,-46.1489379363051,
123.67283715283)) ;
#56454 = CARTESIAN_POINT('Ctrl Pts',(-20.6153551246027,-46.3389827493557,
123.41003275426)) ;
#56455 = CARTESIAN_POINT('Ctrl Pts',(-20.9168785396569,-46.1589936688752,
123.409601144835)) ;
#56456 = CARTESIAN_POINT('Ctrl Pts',(-20.5967235165246,-46.3489235143433,
123.201871132053)) ;
#56457 = CARTESIAN_POINT('Ctrl Pts',(-20.8935915402099,-46.1689344338629,
123.149398558152)) ;
#56458 = CARTESIAN_POINT('Ctrl Pts',(-20.5430611916777,-46.358827847249,123.000680696278)) ;
#56459 = CARTESIAN_POINT('Ctrl Pts',(-20.8265158342025,-46.1788387667685,
122.897909377553)) ;
#56460 = CARTESIAN_POINT('Ctrl Pts',(-20.4539067996073,-46.3688745161297,
122.809226303737)) ;
#56461 = CARTESIAN_POINT('Ctrl Pts',(-20.715075105304,-46.1888854356492,122.658590446678)) ;
#56462 = CARTESIAN_POINT('Ctrl Pts',(-20.3348107304018,-46.3787700794355,
122.638612779929)) ;
#56463 = CARTESIAN_POINT('Ctrl Pts',(-20.5662066577378,-46.198780998955,122.445321690395)) ;
#56464 = CARTESIAN_POINT('Ctrl Pts',(-20.1854730789962,-46.3888321371358,
122.48883600952)) ;
#56465 = CARTESIAN_POINT('Ctrl Pts',(-20.3795364262878,-46.2088430566553,
122.258099155421)) ;
#56466 = CARTESIAN_POINT('Ctrl Pts',(-20.0161942508695,-46.3986749147633,
122.369786755293)) ;
#56467 = CARTESIAN_POINT('Ctrl Pts',(-20.1679385536693,-46.2186858342828,
122.109285146046)) ;
#56468 = CARTESIAN_POINT('Ctrl Pts',(-19.8262618796166,-46.4086653930151,
122.28019126902)) ;
#56469 = CARTESIAN_POINT('Ctrl Pts',(-19.9305238989034,-46.2286763125346,
121.997288664706)) ;
#56470 = CARTESIAN_POINT('Ctrl Pts',(-19.6248584878059,-46.4185943656587,
122.225294019457)) ;
#56471 = CARTESIAN_POINT('Ctrl Pts',(-19.6787697822152,-46.2386052851782,
121.928664785981)) ;
#56472 = CARTESIAN_POINT('Ctrl Pts',(-19.4157226032529,-46.4285855025382,
122.205756739938)) ;
#56473 = CARTESIAN_POINT('Ctrl Pts',(-19.417349965525,-46.2485964220577,121.904240994479)) ;
#56474 = CARTESIAN_POINT('Ctrl Pts',(-19.2057405057304,-46.4386076200272,
122.223135749663)) ;
#56475 = CARTESIAN_POINT('Ctrl Pts',(-19.1548721753179,-46.2586185395467,
121.925962509056)) ;
#56476 = CARTESIAN_POINT('Ctrl Pts',(-19.0043894905299,-46.4485081304294,
122.275869896389)) ;
#56477 = CARTESIAN_POINT('Ctrl Pts',(-18.9031822161393,-46.2685190499489,
121.991878228629)) ;
#56478 = CARTESIAN_POINT('Ctrl Pts',(-18.813429020907,-46.4584971231755,122.363241063598)) ;
#56479 = CARTESIAN_POINT('Ctrl Pts',(-18.664480581697,-46.278508042695,122.101090338607)) ;
#56480 = CARTESIAN_POINT('Ctrl Pts',(-18.6410397094411,-46.4684623672261,
122.482274292673)) ;
#56481 = CARTESIAN_POINT('Ctrl Pts',(-18.4489924496147,-46.2884732867456,
122.249880282336)) ;
#56482 = CARTESIAN_POINT('Ctrl Pts',(-18.4924874516743,-46.4783666317393,
122.62819862701)) ;
#56483 = CARTESIAN_POINT('Ctrl Pts',(-18.2633002249864,-46.2983775512588,
122.432284741212)) ;
#56484 = CARTESIAN_POINT('Ctrl Pts',(-18.3697789016585,-46.4884247234375,
122.800382922365)) ;
#56485 = CARTESIAN_POINT('Ctrl Pts',(-18.1099129935888,-46.308435642957,122.64751372994)) ;
#56486 = CARTESIAN_POINT('Ctrl Pts',(-18.2805605389299,-46.4982746638659,
122.987267125253)) ;
#56487 = CARTESIAN_POINT('Ctrl Pts',(-17.9983877778313,-46.3182855833854,
122.881119052142)) ;
#56488 = CARTESIAN_POINT('Ctrl Pts',(-18.2236525306218,-46.5083016750394,
123.190235923869)) ;
#56489 = CARTESIAN_POINT('Ctrl Pts',(-17.9272509865239,-46.328312594559,123.134829512504)) ;
#56490 = CARTESIAN_POINT('Ctrl Pts',(-18.2033939632025,-46.5183302616515,
123.400103024954)) ;
#56491 = CARTESIAN_POINT('Ctrl Pts',(-17.901925769239,-46.338341181171,123.397163125624)) ;
#56492 = CARTESIAN_POINT('Ctrl Pts',(-18.2191889497681,-46.5281754757642,
123.606465447685)) ;
#56493 = CARTESIAN_POINT('Ctrl Pts',(-17.9216676870494,-46.3481863952837,
123.655117412485)) ;
#56494 = CARTESIAN_POINT('Ctrl Pts',(-18.2707942324504,-46.5381662239437,
123.810069040328)) ;
#56495 = CARTESIAN_POINT('Ctrl Pts',(-17.9861726595003,-46.3581771434633,
123.909622518331)) ;
#56496 = CARTESIAN_POINT('Ctrl Pts',(-18.357794261464,-46.5482038575292,124.002323055344)) ;
#56497 = CARTESIAN_POINT('Ctrl Pts',(-18.0949209306796,-46.3682147770488,
124.14994069115)) ;
#56498 = CARTESIAN_POINT('Ctrl Pts',(-18.4742897524447,-46.5580491467421,
124.173407953581)) ;
#56499 = CARTESIAN_POINT('Ctrl Pts',(-18.2405394894206,-46.3780600662616,
124.363798772885)) ;
#56500 = CARTESIAN_POINT('Ctrl Pts',(-18.620370895161,-46.568030547548,124.324028601828)) ;
#56501 = CARTESIAN_POINT('Ctrl Pts',(-18.4231399412858,-46.3880414670675,
124.552075901862)) ;
#56502 = CARTESIAN_POINT('Ctrl Pts',(-18.7899363735675,-46.5779827805379,
124.44660926478)) ;
#56503 = CARTESIAN_POINT('Ctrl Pts',(-18.6350962162667,-46.3979937000574,
124.705303330032)) ;
#56504 = CARTESIAN_POINT('Ctrl Pts',(-18.9789812034734,-46.5879815919945,
124.538563788364)) ;
#56505 = CARTESIAN_POINT('Ctrl Pts',(-18.8714017008024,-46.4079925115141,
124.82024792927)) ;
#56506 = CARTESIAN_POINT('Ctrl Pts',(-19.1820191632644,-46.5980206959252,
124.596131546056)) ;
#56507 = CARTESIAN_POINT('Ctrl Pts',(-19.1251985398455,-46.4180316154447,
124.89220920167)) ;
#56508 = CARTESIAN_POINT('Ctrl Pts',(-19.3874680290362,-46.6078456383445,
124.617557565118)) ;
#56509 = CARTESIAN_POINT('Ctrl Pts',(-19.3820108279074,-46.427856557864,124.918993385789)) ;
#56510 = CARTESIAN_POINT('Ctrl Pts',(-19.5983341246022,-46.6179003258204,
124.602993200605)) ;
#56511 = CARTESIAN_POINT('Ctrl Pts',(-19.6455932893009,-46.43791124534,124.900789356914)) ;
#56512 = CARTESIAN_POINT('Ctrl Pts',(-19.8011174374927,-46.6278431281773,
124.552252454525)) ;
#56513 = CARTESIAN_POINT('Ctrl Pts',(-19.8990733416014,-46.4478540476968,
124.837364781707)) ;
#56514 = CARTESIAN_POINT('Ctrl Pts',(-19.9915187465345,-46.637746924117,124.467991218211)) ;
#56515 = CARTESIAN_POINT('Ctrl Pts',(-20.1370762829352,-46.4577578436366,
124.732039091095)) ;
#56516 = CARTESIAN_POINT('Ctrl Pts',(-20.166805154378,-46.6477937034921,124.350181343917)) ;
#56517 = CARTESIAN_POINT('Ctrl Pts',(-20.3561848752623,-46.4678046230116,
124.584777991546)) ;
#56518 = CARTESIAN_POINT('Ctrl Pts',(-20.3168442450622,-46.6576893617867,
124.20602634747)) ;
#56519 = CARTESIAN_POINT('Ctrl Pts',(-20.543735289133,-46.4777002813062,124.40458454626)) ;
#56520 = CARTESIAN_POINT('Ctrl Pts',(-20.4416202810829,-46.6677509290373,
124.035249876144)) ;
#56521 = CARTESIAN_POINT('Ctrl Pts',(-20.6997061795947,-46.4877618485568,
124.191114977129)) ;
#56522 = CARTESIAN_POINT('Ctrl Pts',(-20.5328807367812,-46.6775955734746,
123.849484643393)) ;
#56523 = CARTESIAN_POINT('Ctrl Pts',(-20.8137834734582,-46.4976064929941,
123.958907813388)) ;
#56524 = CARTESIAN_POINT('Ctrl Pts',(-20.5918946295246,-46.6875556197173,
123.64858424823)) ;
#56525 = CARTESIAN_POINT('Ctrl Pts',(-20.8875519246108,-46.5075665392368,
123.707782162161)) ;
#56526 = CARTESIAN_POINT('Ctrl Pts',(-20.6148993357899,-46.6975939157357,
123.43881520395)) ;
#56527 = CARTESIAN_POINT('Ctrl Pts',(-20.9163089329228,-46.5176048352552,
123.445571143077)) ;
#56528 = CARTESIAN_POINT('Ctrl Pts',(-20.6017530846061,-46.707467257154,123.231632331)) ;
#56529 = CARTESIAN_POINT('Ctrl Pts',(-20.899877045935,-46.5274781766735,123.186591367216)) ;
#56530 = CARTESIAN_POINT('Ctrl Pts',(-20.5517975292825,-46.7175403609533,
123.025882379625)) ;
#56531 = CARTESIAN_POINT('Ctrl Pts',(-20.8374336992081,-46.5375512804728,
122.929404099157)) ;
#56532 = CARTESIAN_POINT('Ctrl Pts',(-20.4692073505912,-46.7273611760722,
122.836612568494)) ;
#56533 = CARTESIAN_POINT('Ctrl Pts',(-20.7341962067756,-46.5473720955917,
122.692815045702)) ;
#56534 = CARTESIAN_POINT('Ctrl Pts',(-20.3522770027166,-46.7374380411502,
122.660005076197)) ;
#56535 = CARTESIAN_POINT('Ctrl Pts',(-20.5880342151394,-46.5574489606697,
122.472055591139)) ;
#56536 = CARTESIAN_POINT('Ctrl Pts',(-20.2094265317654,-46.7473027808054,
122.509626266143)) ;
#56537 = CARTESIAN_POINT('Ctrl Pts',(-20.4094709148252,-46.567313700325,122.284080598722)) ;
#56538 = CARTESIAN_POINT('Ctrl Pts',(-20.0403249054971,-46.7573251840468,
122.383941295046)) ;
#56539 = CARTESIAN_POINT('Ctrl Pts',(-20.1980943114784,-46.5773361035663,
122.126973882571)) ;
#56540 = CARTESIAN_POINT('Ctrl Pts',(-19.8516517065092,-46.7673509083353,
122.28995820191)) ;
#56541 = CARTESIAN_POINT('Ctrl Pts',(-19.9622532731343,-46.5873618278548,
122.009494284939)) ;
#56542 = CARTESIAN_POINT('Ctrl Pts',(-19.6531005041751,-46.7772056913566,
122.23083936213)) ;
#56543 = CARTESIAN_POINT('Ctrl Pts',(-19.7140632034774,-46.5972166108761,
121.935594664426)) ;
#56544 = CARTESIAN_POINT('Ctrl Pts',(-19.4447550366577,-46.7871845350798,
122.206249292003)) ;
#56545 = CARTESIAN_POINT('Ctrl Pts',(-19.4536310994528,-46.6071954545993,
121.904856532566)) ;
#56546 = CARTESIAN_POINT('Ctrl Pts',(-19.2345000747721,-46.7972034273165,
122.218618665142)) ;
#56547 = CARTESIAN_POINT('Ctrl Pts',(-19.1908123744356,-46.617214346836,121.92031760061)) ;
#56548 = CARTESIAN_POINT('Ctrl Pts',(-19.0322268033516,-46.8070866363575,
122.266237363921)) ;
#56549 = CARTESIAN_POINT('Ctrl Pts',(-18.9379696063433,-46.627097555877,121.979840758441)) ;
#56550 = CARTESIAN_POINT('Ctrl Pts',(-18.8378107169686,-46.8171549456977,
122.349847749281)) ;
#56551 = CARTESIAN_POINT('Ctrl Pts',(-18.6949496715749,-46.6371658652172,
122.084353103891)) ;
#56552 = CARTESIAN_POINT('Ctrl Pts',(-18.6648606133521,-46.8269850710304,
122.463033827998)) ;
#56553 = CARTESIAN_POINT('Ctrl Pts',(-18.4787605239549,-46.6469959905499,
122.225836194773)) ;
#56554 = CARTESIAN_POINT('Ctrl Pts',(-18.5104293304733,-46.8370516234074,
122.607686193805)) ;
#56555 = CARTESIAN_POINT('Ctrl Pts',(-18.2857214964701,-46.6570625429269,
122.406651152064)) ;
#56556 = CARTESIAN_POINT('Ctrl Pts',(-18.3857520045829,-46.8469418603011,
122.774114785356)) ;
#56557 = CARTESIAN_POINT('Ctrl Pts',(-18.1298739185051,-46.6669527798206,
122.614687511464)) ;
#56558 = CARTESIAN_POINT('Ctrl Pts',(-18.2905056904675,-46.8569340850951,
122.961335246674)) ;
#56559 = CARTESIAN_POINT('Ctrl Pts',(-18.0108157651648,-46.6769450046146,
122.848713195555)) ;
#56560 = CARTESIAN_POINT('Ctrl Pts',(-18.2295789136963,-46.866896705446,123.161719579238)) ;
#56561 = CARTESIAN_POINT('Ctrl Pts',(-17.9346569100172,-46.6869076249655,
123.099193972004)) ;
#56562 = CARTESIAN_POINT('Ctrl Pts',(-18.2040027326687,-46.8768017082092,
123.368391035254)) ;
#56563 = CARTESIAN_POINT('Ctrl Pts',(-17.9026865140043,-46.6968126277287,
123.357534213853)) ;
#56564 = CARTESIAN_POINT('Ctrl Pts',(-18.2150087934461,-46.8868594706073,
123.579531972586)) ;
#56565 = CARTESIAN_POINT('Ctrl Pts',(-17.9164439566252,-46.7068703901268,
123.621460054312)) ;
#56566 = CARTESIAN_POINT('Ctrl Pts',(-18.261371220002,-46.8967099899861,123.781380377064)) ;
#56567 = CARTESIAN_POINT('Ctrl Pts',(-17.9743972613134,-46.7167209095056,
123.873771940626)) ;
#56568 = CARTESIAN_POINT('Ctrl Pts',(-18.3431220571985,-46.9067415669843,
123.975771653837)) ;
#56569 = CARTESIAN_POINT('Ctrl Pts',(-18.0765858905938,-46.7267524865038,
124.116760874247)) ;
#56570 = CARTESIAN_POINT('Ctrl Pts',(-18.4574955443547,-46.9167513020892,
124.152440425366)) ;
#56571 = CARTESIAN_POINT('Ctrl Pts',(-18.2195527490337,-46.7367622216087,
124.337596889066)) ;
#56572 = CARTESIAN_POINT('Ctrl Pts',(-18.5992104285265,-46.9266608787155,
124.305119300968)) ;
#56573 = CARTESIAN_POINT('Ctrl Pts',(-18.3966970017583,-46.746671798235,124.528446109201)) ;
#56574 = CARTESIAN_POINT('Ctrl Pts',(-18.765279645767,-46.9365882645721,124.431541302977)) ;
#56575 = CARTESIAN_POINT('Ctrl Pts',(-18.6042842737246,-46.7565991840916,
124.6864738575)) ;
#56576 = CARTESIAN_POINT('Ctrl Pts',(-18.9530362774689,-46.9466331990624,
124.528179929632)) ;
#56577 = CARTESIAN_POINT('Ctrl Pts',(-18.8389799600017,-46.7666441185819,
124.807271873958)) ;
#56578 = CARTESIAN_POINT('Ctrl Pts',(-19.151511474355,-46.9565191312504,124.589883618221)) ;
#56579 = CARTESIAN_POINT('Ctrl Pts',(-19.0870750670276,-46.7765300507699,
124.88440157674)) ;
#56580 = CARTESIAN_POINT('Ctrl Pts',(-19.3598549427328,-46.9665124372034,
124.616830207834)) ;
#56581 = CARTESIAN_POINT('Ctrl Pts',(-19.3475046537263,-46.7865233567229,
124.918084459642)) ;
#56582 = CARTESIAN_POINT('Ctrl Pts',(-19.5687199932944,-46.9764580749853,
124.607155449397)) ;
#56583 = CARTESIAN_POINT('Ctrl Pts',(-19.6085865454155,-46.7964689945048,
124.90599063429)) ;
#56584 = CARTESIAN_POINT('Ctrl Pts',(-19.7728690713917,-46.9864053433312,
124.561770557663)) ;
#56585 = CARTESIAN_POINT('Ctrl Pts',(-19.8637733414417,-46.8064162628507,
124.849258887938)) ;
#56586 = CARTESIAN_POINT('Ctrl Pts',(-19.9678843674529,-46.9964532454683,
124.480604259967)) ;
#56587 = CARTESIAN_POINT('Ctrl Pts',(-20.1075420667976,-46.8164641649878,
124.747800719833)) ;
#56588 = CARTESIAN_POINT('Ctrl Pts',(-20.1423977281203,-47.0063009403085,
124.369220465197)) ;
#56589 = CARTESIAN_POINT('Ctrl Pts',(-20.3256846822976,-46.826311859828,124.608569806674)) ;
#56590 = CARTESIAN_POINT('Ctrl Pts',(-20.2971232610949,-47.0162624500529,
124.228102585513)) ;
#56591 = CARTESIAN_POINT('Ctrl Pts',(-20.519091428177,-46.8362733695724,124.432171593278)) ;
#56592 = CARTESIAN_POINT('Ctrl Pts',(-20.4256537019022,-47.0262918416617,
124.060947461949)) ;
#56593 = CARTESIAN_POINT('Ctrl Pts',(-20.6797539091981,-46.8463027611812,
124.223227378317)) ;
#56594 = CARTESIAN_POINT('Ctrl Pts',(-20.5221200134929,-47.0361993372165,
123.876344757324)) ;
#56595 = CARTESIAN_POINT('Ctrl Pts',(-20.800336605689,-46.856210256736,123.992472885805)) ;
#56596 = CARTESIAN_POINT('Ctrl Pts',(-20.585700963853,-47.0461447288795,123.677180951145)) ;
#56597 = CARTESIAN_POINT('Ctrl Pts',(-20.8798121651534,-46.866155648399,123.743517316037)) ;
#56598 = CARTESIAN_POINT('Ctrl Pts',(-20.6140236281274,-47.0561466464769,
123.468796635054)) ;
#56599 = CARTESIAN_POINT('Ctrl Pts',(-20.9152146259637,-46.8761575659964,
123.483036674989)) ;
#56600 = CARTESIAN_POINT('Ctrl Pts',(-20.6053144754768,-47.0661867140291,
123.257921725322)) ;
#56601 = CARTESIAN_POINT('Ctrl Pts',(-20.9043274471141,-46.8861976335486,
123.219443241582)) ;
#56602 = CARTESIAN_POINT('Ctrl Pts',(-20.5615451992037,-47.0760110254689,
123.056057517403)) ;
#56603 = CARTESIAN_POINT('Ctrl Pts',(-20.8496146262616,-46.8960219449884,
122.967111685171)) ;
#56604 = CARTESIAN_POINT('Ctrl Pts',(-20.48182941958,-47.086067266625,122.860270767228)) ;
#56605 = CARTESIAN_POINT('Ctrl Pts',(-20.7499690605305,-46.9060781861445,
122.722378927927)) ;
#56606 = CARTESIAN_POINT('Ctrl Pts',(-20.3705003700426,-47.0959981883606,
122.683623151021)) ;
#56607 = CARTESIAN_POINT('Ctrl Pts',(-20.6108065949588,-46.9160091078801,
122.501569334424)) ;
#56608 = CARTESIAN_POINT('Ctrl Pts',(-20.2303667268952,-47.1059414244368,
122.528548074826)) ;
#56609 = CARTESIAN_POINT('Ctrl Pts',(-20.4356383207007,-46.9259523439564,
122.307725777316)) ;
#56610 = CARTESIAN_POINT('Ctrl Pts',(-20.0648823735269,-47.1159227084493,
122.399473602791)) ;
#56611 = CARTESIAN_POINT('Ctrl Pts',(-20.2287819480132,-46.9359336279688,
122.146383449946)) ;
#56612 = CARTESIAN_POINT('Ctrl Pts',(-19.878210560702,-47.125967010075,122.300821311272)) ;
#56613 = CARTESIAN_POINT('Ctrl Pts',(-19.9954418663131,-46.9459779295945,
122.023069093514)) ;
#56614 = CARTESIAN_POINT('Ctrl Pts',(-19.6816640223288,-47.1357950912944,
122.236998796321)) ;
#56615 = CARTESIAN_POINT('Ctrl Pts',(-19.7497569427721,-46.9558060108139,
121.943291660631)) ;
#56616 = CARTESIAN_POINT('Ctrl Pts',(-19.4719363919362,-47.1458716941436,
122.207454533547)) ;
#56617 = CARTESIAN_POINT('Ctrl Pts',(-19.4875976586612,-46.9658826136631,
121.906362635453)) ;
#56618 = CARTESIAN_POINT('Ctrl Pts',(-19.2648901369236,-47.1557237732621,
122.214511172754)) ;
#56619 = CARTESIAN_POINT('Ctrl Pts',(-19.2287886486704,-46.9757346927816,
121.915184765219)) ;
#56620 = CARTESIAN_POINT('Ctrl Pts',(-19.0577050674081,-47.165797031571,122.258180662651)) ;
#56621 = CARTESIAN_POINT('Ctrl Pts',(-18.9698079848751,-46.9858079510905,
121.969772870427)) ;
#56622 = CARTESIAN_POINT('Ctrl Pts',(-18.8657477434276,-47.1756384909513,
122.335414466867)) ;
#56623 = CARTESIAN_POINT('Ctrl Pts',(-18.7298606157997,-46.9956494104708,
122.066316849402)) ;
#56624 = CARTESIAN_POINT('Ctrl Pts',(-18.6875856486329,-47.1855995863637,
122.445455661587)) ;
#56625 = CARTESIAN_POINT('Ctrl Pts',(-18.5071584974101,-47.0056105058832,
122.2038699234)) ;
#56626 = CARTESIAN_POINT('Ctrl Pts',(-18.5303140250955,-47.1956368707604,
122.586136597021)) ;
#56627 = CARTESIAN_POINT('Ctrl Pts',(-18.3105700405219,-47.0156477902799,
122.379722097128)) ;
#56628 = CARTESIAN_POINT('Ctrl Pts',(-18.4016481952308,-47.2055132094957,
122.749125228209)) ;
#56629 = CARTESIAN_POINT('Ctrl Pts',(-18.1497383798912,-47.0255241290152,
122.583459652687)) ;
#56630 = CARTESIAN_POINT('Ctrl Pts',(-18.3013741603539,-47.2155753356489,
122.935356273905)) ;
#56631 = CARTESIAN_POINT('Ctrl Pts',(-18.0243973837538,-47.0355862551685,
122.816248967621)) ;
#56632 = CARTESIAN_POINT('Ctrl Pts',(-18.2361754948208,-47.2254435096255,
123.132331116174)) ;
#56633 = CARTESIAN_POINT('Ctrl Pts',(-17.9429002610054,-47.045454429145,123.06246901578)) ;
#56634 = CARTESIAN_POINT('Ctrl Pts',(-18.205338043931,-47.2354490581293,123.340378376433)) ;
#56635 = CARTESIAN_POINT('Ctrl Pts',(-17.9043551710832,-47.0554599776488,
123.322528432353)) ;
#56636 = CARTESIAN_POINT('Ctrl Pts',(-18.2111535129992,-47.2454316900249,
123.550202526117)) ;
#56637 = CARTESIAN_POINT('Ctrl Pts',(-17.9116262440273,-47.0654426095444,
123.584808795442)) ;
#56638 = CARTESIAN_POINT('Ctrl Pts',(-18.2537758997071,-47.2554756324466,
123.756993471745)) ;
#56639 = CARTESIAN_POINT('Ctrl Pts',(-17.9649058186753,-47.0754865519662,
123.843296984603)) ;
#56640 = CARTESIAN_POINT('Ctrl Pts',(-18.3297319147639,-47.2653037804738,
123.94914374406)) ;
#56641 = CARTESIAN_POINT('Ctrl Pts',(-18.059852938383,-47.0853146999933,124.083485382884)) ;
#56642 = CARTESIAN_POINT('Ctrl Pts',(-18.4391033103602,-47.2752936478482,
124.128436677712)) ;
#56643 = CARTESIAN_POINT('Ctrl Pts',(-18.1965689477864,-47.0953045673677,
124.30760067584)) ;
#56644 = CARTESIAN_POINT('Ctrl Pts',(-18.5791042370888,-47.2853373868037,
124.286501486607)) ;
#56645 = CARTESIAN_POINT('Ctrl Pts',(-18.3715713483285,-47.1053483063232,
124.505180389838)) ;
#56646 = CARTESIAN_POINT('Ctrl Pts',(-18.7405005083197,-47.2951591353416,
124.415289290748)) ;
#56647 = CARTESIAN_POINT('Ctrl Pts',(-18.5733188647652,-47.1151700548612,
124.666164420743)) ;
#56648 = CARTESIAN_POINT('Ctrl Pts',(-18.9254963348016,-47.3051941129514,
124.516697212118)) ;
#56649 = CARTESIAN_POINT('Ctrl Pts',(-18.804564552751,-47.1252050324709,124.792922450559)) ;
#56650 = CARTESIAN_POINT('Ctrl Pts',(-19.1252827024843,-47.3152190257091,
124.583820831396)) ;
#56651 = CARTESIAN_POINT('Ctrl Pts',(-19.0542980945061,-47.1352299452286,
124.87682516283)) ;
#56652 = CARTESIAN_POINT('Ctrl Pts',(-19.3300236054208,-47.3250709688029,
124.615141144271)) ;
#56653 = CARTESIAN_POINT('Ctrl Pts',(-19.3102255315755,-47.1450818883224,
124.915973694134)) ;
#56654 = CARTESIAN_POINT('Ctrl Pts',(-19.5399921824132,-47.335061930132,124.61069150491)) ;
#56655 = CARTESIAN_POINT('Ctrl Pts',(-19.5726863790328,-47.1550728496515,
124.910409513021)) ;
#56656 = CARTESIAN_POINT('Ctrl Pts',(-19.7445687503477,-47.3449798050004,
124.570275657887)) ;
#56657 = CARTESIAN_POINT('Ctrl Pts',(-19.8284072327781,-47.16499072452,124.859887472904)) ;
#56658 = CARTESIAN_POINT('Ctrl Pts',(-19.9411645038063,-47.3550083240017,
124.494169080804)) ;
#56659 = CARTESIAN_POINT('Ctrl Pts',(-20.0741511053129,-47.1750192435212,
124.764752235826)) ;
#56660 = CARTESIAN_POINT('Ctrl Pts',(-20.1190316044298,-47.3648920027995,
124.386736912704)) ;
#56661 = CARTESIAN_POINT('Ctrl Pts',(-20.2964844790858,-47.184902922319,124.630459757824)) ;
#56662 = CARTESIAN_POINT('Ctrl Pts',(-20.2776029483936,-47.3748869462393,
124.248868784575)) ;
#56663 = CARTESIAN_POINT('Ctrl Pts',(-20.4946972414984,-47.1948978657588,
124.458122754322)) ;
#56664 = CARTESIAN_POINT('Ctrl Pts',(-20.4099687757007,-47.3849138000617,
124.084811617486)) ;
#56665 = CARTESIAN_POINT('Ctrl Pts',(-20.660152776237,-47.2049247195812,124.253049913892)) ;
#56666 = CARTESIAN_POINT('Ctrl Pts',(-20.510642437193,-47.3947979644006,123.90302150782)) ;
#56667 = CARTESIAN_POINT('Ctrl Pts',(-20.7859931802032,-47.2148088839201,
124.025810555443)) ;
#56668 = CARTESIAN_POINT('Ctrl Pts',(-20.5791870198789,-47.404786062443,123.704564661141)) ;
#56669 = CARTESIAN_POINT('Ctrl Pts',(-20.8716717236178,-47.2247969819625,
123.777738571902)) ;
#56670 = CARTESIAN_POINT('Ctrl Pts',(-20.6122318337484,-47.4147371689001,
123.497960882242)) ;
#56671 = CARTESIAN_POINT('Ctrl Pts',(-20.9129754354945,-47.2347480884196,
123.519483140442)) ;
#56672 = CARTESIAN_POINT('Ctrl Pts',(-20.6087528151844,-47.4247822200682,
123.286823087064)) ;
#56673 = CARTESIAN_POINT('Ctrl Pts',(-20.908624300568,-47.2447931395877,123.255561025808)) ;
#56674 = CARTESIAN_POINT('Ctrl Pts',(-20.5695080656403,-47.4346439804265,
123.083245164977)) ;
#56675 = CARTESIAN_POINT('Ctrl Pts',(-20.8595658747086,-47.254654899946,123.001088343658)) ;
#56676 = CARTESIAN_POINT('Ctrl Pts',(-20.495357370561,-47.4446067972569,122.88735923458)) ;
#56677 = CARTESIAN_POINT('Ctrl Pts',(-20.7668750534298,-47.2646177167764,
122.756231591743)) ;
#56678 = CARTESIAN_POINT('Ctrl Pts',(-20.3872427945494,-47.4546414785377,
122.706219208448)) ;
#56679 = CARTESIAN_POINT('Ctrl Pts',(-20.6317297455285,-47.2746523980572,
122.529807845268)) ;
#56680 = CARTESIAN_POINT('Ctrl Pts',(-20.2516200642963,-47.4645265083184,
122.548722650758)) ;
#56681 = CARTESIAN_POINT('Ctrl Pts',(-20.4621990514444,-47.284537427838,122.332938363861)) ;
#56682 = CARTESIAN_POINT('Ctrl Pts',(-20.0877899814674,-47.4745921017164,
122.414841028809)) ;
#56683 = CARTESIAN_POINT('Ctrl Pts',(-20.2574099723545,-47.294603021236,122.165588379758)) ;
#56684 = CARTESIAN_POINT('Ctrl Pts',(-19.9073992267312,-47.4844312700779,
122.313551418133)) ;
#56685 = CARTESIAN_POINT('Ctrl Pts',(-20.031919660044,-47.3044421895975,122.038978242705)) ;
#56686 = CARTESIAN_POINT('Ctrl Pts',(-19.7078787306478,-47.4944938678194,
122.243312824082)) ;
#56687 = CARTESIAN_POINT('Ctrl Pts',(-19.7825183008576,-47.3145047873389,
121.951182502059)) ;
#56688 = CARTESIAN_POINT('Ctrl Pts',(-19.5025547915718,-47.5043908802264,
122.209566875106)) ;
#56689 = CARTESIAN_POINT('Ctrl Pts',(-19.5258624977785,-47.3244017997459,
121.909002520812)) ;
#56690 = CARTESIAN_POINT('Ctrl Pts',(-19.2937789957374,-47.514322202052,122.211297493397)) ;
#56691 = CARTESIAN_POINT('Ctrl Pts',(-19.2648924723345,-47.3343331215715,
121.911168475178)) ;
#56692 = CARTESIAN_POINT('Ctrl Pts',(-19.0862316655902,-47.5243639648065,
122.249899659143)) ;
#56693 = CARTESIAN_POINT('Ctrl Pts',(-19.0054588235907,-47.344374884326,121.959423773016)) ;
#56694 = CARTESIAN_POINT('Ctrl Pts',(-18.8914968548924,-47.5342521636972,
122.322686181889)) ;
#56695 = CARTESIAN_POINT('Ctrl Pts',(-18.7620408414669,-47.3542630832167,
122.050409572496)) ;
#56696 = CARTESIAN_POINT('Ctrl Pts',(-18.7102985265331,-47.544246102297,122.429005812639)) ;
#56697 = CARTESIAN_POINT('Ctrl Pts',(-18.5355442146445,-47.3642570218165,
122.183311500729)) ;
#56698 = CARTESIAN_POINT('Ctrl Pts',(-18.5511494828585,-47.5541869233339,
122.564478677246)) ;
#56699 = CARTESIAN_POINT('Ctrl Pts',(-18.3366094810446,-47.3741978428534,
122.352654795869)) ;
#56700 = CARTESIAN_POINT('Ctrl Pts',(-18.4175024086679,-47.5641463056221,
122.725638878256)) ;
#56701 = CARTESIAN_POINT('Ctrl Pts',(-18.1695526328469,-47.3841572251416,
122.554106931922)) ;
#56702 = CARTESIAN_POINT('Ctrl Pts',(-18.3133427089413,-47.5741440652745,
122.90822294444)) ;
#56703 = CARTESIAN_POINT('Ctrl Pts',(-18.0393553530217,-47.394154984794,122.782338451435)) ;
#56704 = CARTESIAN_POINT('Ctrl Pts',(-18.2424783139921,-47.5841802014768,
123.106952131826)) ;
#56705 = CARTESIAN_POINT('Ctrl Pts',(-17.9507774143695,-47.4041911209963,
123.030750867611)) ;
#56706 = CARTESIAN_POINT('Ctrl Pts',(-18.2076066802903,-47.5940309989677,
123.311088085714)) ;
#56707 = CARTESIAN_POINT('Ctrl Pts',(-17.9071905131153,-47.4140419184872,
123.285921661657)) ;
#56708 = CARTESIAN_POINT('Ctrl Pts',(-18.2080983621174,-47.603991864044,123.520488926134)) ;
#56709 = CARTESIAN_POINT('Ctrl Pts',(-17.9078079175125,-47.4240027835635,
123.547672833067)) ;
#56710 = CARTESIAN_POINT('Ctrl Pts',(-18.2454476002955,-47.6140207316744,
123.728004942344)) ;
#56711 = CARTESIAN_POINT('Ctrl Pts',(-17.9544972055366,-47.4340316511939,
123.80706740302)) ;
#56712 = CARTESIAN_POINT('Ctrl Pts',(-18.3173323666115,-47.6239309678108,
123.92354610878)) ;
#56713 = CARTESIAN_POINT('Ctrl Pts',(-18.0443558520564,-47.4439418873303,
124.051493099978)) ;
#56714 = CARTESIAN_POINT('Ctrl Pts',(-18.4218727530156,-47.6338659211253,
124.10437188864)) ;
#56715 = CARTESIAN_POINT('Ctrl Pts',(-18.1750338401117,-47.4538768406448,
124.277524030993)) ;
#56716 = CARTESIAN_POINT('Ctrl Pts',(-18.5577961313791,-47.6439068515349,
124.265872819916)) ;
#56717 = CARTESIAN_POINT('Ctrl Pts',(-18.3449402388069,-47.4639177710544,
124.479398422852)) ;
#56718 = CARTESIAN_POINT('Ctrl Pts',(-18.7171539318421,-47.6537947483165,
124.399365872321)) ;
#56719 = CARTESIAN_POINT('Ctrl Pts',(-18.5441394207863,-47.473805667836,124.646262688005)) ;
#56720 = CARTESIAN_POINT('Ctrl Pts',(-18.8989130954372,-47.6637841999752,
124.504559353168)) ;
#56721 = CARTESIAN_POINT('Ctrl Pts',(-18.7713398490752,-47.4837951194947,
124.777752129431)) ;
#56722 = CARTESIAN_POINT('Ctrl Pts',(-19.0956328686204,-47.6737432903405,
124.57621883154)) ;
#56723 = CARTESIAN_POINT('Ctrl Pts',(-19.017240622354,-47.4937542098601,124.867323859769)) ;
#56724 = CARTESIAN_POINT('Ctrl Pts',(-19.3004544560536,-47.6836406026468,
124.612933945687)) ;
#56725 = CARTESIAN_POINT('Ctrl Pts',(-19.2732681589748,-47.5036515221664,
124.913214982675)) ;
#56726 = CARTESIAN_POINT('Ctrl Pts',(-19.5118542835427,-47.6936970285471,
124.613436471454)) ;
#56727 = CARTESIAN_POINT('Ctrl Pts',(-19.5375180334462,-47.5137079480666,
124.913840319172)) ;
#56728 = CARTESIAN_POINT('Ctrl Pts',(-19.7163232652421,-47.7035670311368,
124.577994785846)) ;
#56729 = CARTESIAN_POINT('Ctrl Pts',(-19.7931038035627,-47.5235779506564,
124.86953541522)) ;
#56730 = CARTESIAN_POINT('Ctrl Pts',(-19.9142840722972,-47.7135709643141,
124.507042269719)) ;
#56731 = CARTESIAN_POINT('Ctrl Pts',(-20.0405538779432,-47.5335818838336,
124.780842159568)) ;
#56732 = CARTESIAN_POINT('Ctrl Pts',(-20.0966064940378,-47.723558224778,124.402844984413)) ;
#56733 = CARTESIAN_POINT('Ctrl Pts',(-20.2684557086324,-47.5435691442975,
124.650592871794)) ;
#56734 = CARTESIAN_POINT('Ctrl Pts',(-20.2585947292332,-47.7335852763637,
124.267974135904)) ;
#56735 = CARTESIAN_POINT('Ctrl Pts',(-20.4709387207198,-47.5535961958832,
124.482002870763)) ;
#56736 = CARTESIAN_POINT('Ctrl Pts',(-20.393034986563,-47.7434763661898,124.109317573844)) ;
#56737 = CARTESIAN_POINT('Ctrl Pts',(-20.638988919599,-47.5634872857093,124.283677447696)) ;
#56738 = CARTESIAN_POINT('Ctrl Pts',(-20.5342723905065,-47.7567741209708,
123.868088225556)) ;
#56739 = CARTESIAN_POINT('Ctrl Pts',(-20.8155222738313,-47.5767850404904,
123.982153460042)) ;
#56740 = CARTESIAN_POINT('Ctrl Pts',(-20.6091851589647,-47.769972180579,123.597577696433)) ;
#56741 = CARTESIAN_POINT('Ctrl Pts',(-20.9091627273331,-47.5899831000985,
123.644050843694)) ;
#56742 = CARTESIAN_POINT('Ctrl Pts',(-20.6114219199646,-47.7833689211482,
123.316008276815)) ;
#56743 = CARTESIAN_POINT('Ctrl Pts',(-20.9119614689893,-47.6033798406677,
123.292030999204)) ;
#56744 = CARTESIAN_POINT('Ctrl Pts',(-20.5772346324987,-47.7932398332216,
123.111276079564)) ;
#56745 = CARTESIAN_POINT('Ctrl Pts',(-20.8692234171749,-47.6132507527411,
123.036128094856)) ;
#56746 = CARTESIAN_POINT('Ctrl Pts',(-20.506620197884,-47.8033133949897,122.911669655053)) ;
#56747 = CARTESIAN_POINT('Ctrl Pts',(-20.7809529680792,-47.6233243145093,
122.786617518438)) ;
#56748 = CARTESIAN_POINT('Ctrl Pts',(-20.4051985250744,-47.8131348075781,
122.731761328968)) ;
#56749 = CARTESIAN_POINT('Ctrl Pts',(-20.6541739491768,-47.6331457270976,
122.561735103806)) ;
#56750 = CARTESIAN_POINT('Ctrl Pts',(-20.2709276734717,-47.8232088248091,
122.568046641826)) ;
#56751 = CARTESIAN_POINT('Ctrl Pts',(-20.4863320287132,-47.6432197443286,
122.357091382024)) ;
#56752 = CARTESIAN_POINT('Ctrl Pts',(-20.0611060975047,-47.8363676117737,
122.387657282842)) ;
#56753 = CARTESIAN_POINT('Ctrl Pts',(-20.2240587468201,-47.6563785312932,
122.131615915142)) ;
#56754 = CARTESIAN_POINT('Ctrl Pts',(-19.805342502725,-47.8497337148678,122.263873713802)) ;
#56755 = CARTESIAN_POINT('Ctrl Pts',(-19.9043966118727,-47.6697446343874,
121.976897634809)) ;
#56756 = CARTESIAN_POINT('Ctrl Pts',(-19.5302562535324,-47.8630476497569,
122.211981763288)) ;
#56757 = CARTESIAN_POINT('Ctrl Pts',(-19.5604802160185,-47.6830585692764,
121.912018372235)) ;
#56758 = CARTESIAN_POINT('Ctrl Pts',(-19.3221676696211,-47.8729476892044,
122.209028722341)) ;
#56759 = CARTESIAN_POINT('Ctrl Pts',(-19.3003815270599,-47.6929586087239,
121.908333182987)) ;
#56760 = CARTESIAN_POINT('Ctrl Pts',(-19.115305104631,-47.8829120923389,122.242126287116)) ;
#56761 = CARTESIAN_POINT('Ctrl Pts',(-19.0418005240328,-47.7029230118584,
121.949706845845)) ;
#56762 = CARTESIAN_POINT('Ctrl Pts',(-18.9160968655024,-47.89294205946,122.311266661747)) ;
#56763 = CARTESIAN_POINT('Ctrl Pts',(-18.7927924421303,-47.7129529789796,
122.036134212996)) ;
#56764 = CARTESIAN_POINT('Ctrl Pts',(-18.7342345587612,-47.9028443360691,
122.412551802451)) ;
#56765 = CARTESIAN_POINT('Ctrl Pts',(-18.5654632172978,-47.7228552555886,
122.162745640166)) ;
#56766 = CARTESIAN_POINT('Ctrl Pts',(-18.5173604794192,-47.9161102652382,
122.58797464885)) ;
#56767 = CARTESIAN_POINT('Ctrl Pts',(-18.2943866084887,-47.7361211847578,
122.382011147295)) ;
#56768 = CARTESIAN_POINT('Ctrl Pts',(-18.309565842614,-47.9327317963447,122.873754193906)) ;
#56769 = CARTESIAN_POINT('Ctrl Pts',(-18.0346303795379,-47.7527427158642,
122.739250673721)) ;
#56770 = CARTESIAN_POINT('Ctrl Pts',(-18.1920101676508,-47.9526066249893,
123.279717316389)) ;
#56771 = CARTESIAN_POINT('Ctrl Pts',(-17.8876997699416,-47.7726175445089,
123.246720784364)) ;
#56772 = CARTESIAN_POINT('Ctrl Pts',(-18.2154597866439,-47.9692798330912,
123.633471891769)) ;
#56773 = CARTESIAN_POINT('Ctrl Pts',(-17.917000592539,-47.7892907526107,123.688848718156)) ;
#56774 = CARTESIAN_POINT('Ctrl Pts',(-18.3053614681726,-47.9825309580725,
123.897116716914)) ;
#56775 = CARTESIAN_POINT('Ctrl Pts',(-18.0293936750279,-47.802541877592,124.018462677766)) ;
#56776 = CARTESIAN_POINT('Ctrl Pts',(-18.4387378594094,-47.9957732768933,
124.141560057195)) ;
#56777 = CARTESIAN_POINT('Ctrl Pts',(-18.1961054878866,-47.8157841964128,
124.323995100867)) ;
#56778 = CARTESIAN_POINT('Ctrl Pts',(-18.6845127413368,-48.0125065172328,
124.39871352638)) ;
#56779 = CARTESIAN_POINT('Ctrl Pts',(-18.5033373265711,-47.8325174367523,
124.645448284726)) ;
#56780 = CARTESIAN_POINT('Ctrl Pts',(-19.0624327367419,-48.0323356654207,
124.585830606366)) ;
#56781 = CARTESIAN_POINT('Ctrl Pts',(-18.9757346112765,-47.8523465849403,
124.879336049471)) ;
#56782 = CARTESIAN_POINT('Ctrl Pts',(-19.4832475920745,-48.0522603605214,
124.633977070229)) ;
#56783 = CARTESIAN_POINT('Ctrl Pts',(-19.5017537469075,-47.8722712800409,
124.939516678405)) ;
#56784 = CARTESIAN_POINT('Ctrl Pts',(-19.8953466515693,-48.0721835891048,
124.53556105767)) ;
#56785 = CARTESIAN_POINT('Ctrl Pts',(-20.0168758620234,-47.8921945086243,
124.816493222276)) ;
#56786 = CARTESIAN_POINT('Ctrl Pts',(-20.2491680892978,-48.0921107282309,
124.302550900816)) ;
#56787 = CARTESIAN_POINT('Ctrl Pts',(-20.4591503182004,-47.9121216477504,
124.525228377064)) ;
#56788 = CARTESIAN_POINT('Ctrl Pts',(-20.5020771655509,-48.1119871908466,
123.963916176458)) ;
#56789 = CARTESIAN_POINT('Ctrl Pts',(-20.775283647874,-47.9319981103661,124.101934449859)) ;
#56790 = CARTESIAN_POINT('Ctrl Pts',(-20.6250718690425,-48.1319644194519,
123.557348462164)) ;
#56791 = CARTESIAN_POINT('Ctrl Pts',(-20.9290246640745,-47.9519753389714,
123.593724361123)) ;
#56792 = CARTESIAN_POINT('Ctrl Pts',(-20.6016537275589,-48.1518992774256,
123.134089906052)) ;
#56793 = CARTESIAN_POINT('Ctrl Pts',(-20.8997496416068,-47.9719101969451,
123.064652071518)) ;
#56794 = CARTESIAN_POINT('Ctrl Pts',(-20.4359503230159,-48.1717957263564,
122.744874511836)) ;
#56795 = CARTESIAN_POINT('Ctrl Pts',(-20.6926191393825,-47.9918066458759,
122.57813484947)) ;
#56796 = CARTESIAN_POINT('Ctrl Pts',(-20.1473267208655,-48.191717010423,122.434822386439)) ;
#56797 = CARTESIAN_POINT('Ctrl Pts',(-20.3318393280273,-48.0117279299425,
122.190571444716)) ;
#56798 = CARTESIAN_POINT('Ctrl Pts',(-19.7694900246731,-48.2116736600939,
122.241648838417)) ;
#56799 = CARTESIAN_POINT('Ctrl Pts',(-19.8595433797258,-48.0316845796135,
121.949105900236)) ;
#56800 = CARTESIAN_POINT('Ctrl Pts',(-19.3501801167776,-48.2315509532055,
122.189092571805)) ;
#56801 = CARTESIAN_POINT('Ctrl Pts',(-19.3354077539385,-48.0515618727251,
121.883411775771)) ;
#56802 = CARTESIAN_POINT('Ctrl Pts',(-18.9375691670233,-48.251437425434,122.281750555441)) ;
#56803 = CARTESIAN_POINT('Ctrl Pts',(-18.8196458601561,-48.0714483449535,
121.999233714734)) ;
#56804 = CARTESIAN_POINT('Ctrl Pts',(-18.5785832798502,-48.271498991358,122.512179757162)) ;
#56805 = CARTESIAN_POINT('Ctrl Pts',(-18.3709126384581,-48.0915099108775,
122.287270877058)) ;
#56806 = CARTESIAN_POINT('Ctrl Pts',(-18.3229725036018,-48.2913393988987,
122.847760478558)) ;
#56807 = CARTESIAN_POINT('Ctrl Pts',(-18.051400875237,-48.1113503184183,122.706744756722)) ;
#56808 = CARTESIAN_POINT('Ctrl Pts',(-18.1954566816947,-48.3111907228717,
123.250147542051)) ;
#56809 = CARTESIAN_POINT('Ctrl Pts',(-17.8920053837549,-48.1312016423912,
123.209726070938)) ;
#56810 = CARTESIAN_POINT('Ctrl Pts',(-18.2137292660296,-48.3312439928231,
123.676086435332)) ;
#56811 = CARTESIAN_POINT('Ctrl Pts',(-17.9148449515305,-48.1512549123426,
123.742150506238)) ;
#56812 = CARTESIAN_POINT('Ctrl Pts',(-18.3743522701606,-48.3510646502064,
124.065843827562)) ;
#56813 = CARTESIAN_POINT('Ctrl Pts',(-18.1156214421197,-48.171075569726,124.229345578979)) ;
#56814 = CARTESIAN_POINT('Ctrl Pts',(-18.6598163322656,-48.3710360715369,
124.380035479297)) ;
#56815 = CARTESIAN_POINT('Ctrl Pts',(-18.4724496626934,-48.1910469910565,
124.622086302421)) ;
#56816 = CARTESIAN_POINT('Ctrl Pts',(-19.0341051163834,-48.3909295639006,
124.577408934611)) ;
#56817 = CARTESIAN_POINT('Ctrl Pts',(-18.9403084788281,-48.2109404834202,
124.868804641701)) ;
#56818 = CARTESIAN_POINT('Ctrl Pts',(-19.4558297886332,-48.4109536501417,
124.635272002044)) ;
#56819 = CARTESIAN_POINT('Ctrl Pts',(-19.4674642242625,-48.2309645696612,
124.941135895911)) ;
#56820 = CARTESIAN_POINT('Ctrl Pts',(-19.8676091497869,-48.4307585292546,
124.54692460703)) ;
#56821 = CARTESIAN_POINT('Ctrl Pts',(-19.9821868641728,-48.2507694487741,
124.830704772486)) ;
#56822 = CARTESIAN_POINT('Ctrl Pts',(-20.2278594836264,-48.4507175449524,
124.322628489146)) ;
#56823 = CARTESIAN_POINT('Ctrl Pts',(-20.4325013286811,-48.270728464472,124.550337764618)) ;
#56824 = CARTESIAN_POINT('Ctrl Pts',(-20.4895249553124,-48.4707035685815,
123.987793204805)) ;
#56825 = CARTESIAN_POINT('Ctrl Pts',(-20.7595855619426,-48.290714488101,124.131795730285)) ;
#56826 = CARTESIAN_POINT('Ctrl Pts',(-20.620851700236,-48.490512064342,123.587567929602)) ;
#56827 = CARTESIAN_POINT('Ctrl Pts',(-20.9237469671221,-48.3105229838615,
123.631516939114)) ;
#56828 = CARTESIAN_POINT('Ctrl Pts',(-20.6081359744809,-48.5104947034476,
123.162963885691)) ;
#56829 = CARTESIAN_POINT('Ctrl Pts',(-20.9078563779527,-48.3305056229671,
123.100761863387)) ;
#56830 = CARTESIAN_POINT('Ctrl Pts',(-20.4519095426807,-48.5303761512416,
122.770042814153)) ;
#56831 = CARTESIAN_POINT('Ctrl Pts',(-20.712577492358,-48.3503870707611,122.609609792181)) ;
#56832 = CARTESIAN_POINT('Ctrl Pts',(-20.1703007545969,-48.5503326179791,
122.452751245619)) ;
#56833 = CARTESIAN_POINT('Ctrl Pts',(-20.3605699836002,-48.3703435374986,
122.212992650296)) ;
#56834 = CARTESIAN_POINT('Ctrl Pts',(-19.7987956805758,-48.5702100149347,
122.251075325285)) ;
#56835 = CARTESIAN_POINT('Ctrl Pts',(-19.8961915071148,-48.3902209344542,
121.960894036655)) ;
#56836 = CARTESIAN_POINT('Ctrl Pts',(-19.3787174367408,-48.59019196111,122.187732374788)) ;
#56837 = CARTESIAN_POINT('Ctrl Pts',(-19.3710944052831,-48.4102028806295,
121.881710834772)) ;
#56838 = CARTESIAN_POINT('Ctrl Pts',(-18.9632548947561,-48.6101210601467,
122.271556210172)) ;
#56839 = CARTESIAN_POINT('Ctrl Pts',(-18.8517658004596,-48.4301319796663,
121.986485154888)) ;
#56840 = CARTESIAN_POINT('Ctrl Pts',(-18.6014532782387,-48.6300496833594,
122.491970120177)) ;
#56841 = CARTESIAN_POINT('Ctrl Pts',(-18.3995108076249,-48.4500606028789,
122.262000851676)) ;
#56842 = CARTESIAN_POINT('Ctrl Pts',(-18.3371474305036,-48.6498840074658,
122.820662580448)) ;
#56843 = CARTESIAN_POINT('Ctrl Pts',(-18.0691275874109,-48.4698949269853,
122.672852581534)) ;
#56844 = CARTESIAN_POINT('Ctrl Pts',(-18.2224259879656,-48.6665362948492,
123.155533978461)) ;
#56845 = CARTESIAN_POINT('Ctrl Pts',(-17.9257131668265,-48.4865472143687,
123.091471777925)) ;
#56846 = CARTESIAN_POINT('Ctrl Pts',(-18.2035092636524,-48.6797967958714,
123.433741752069)) ;
#56847 = CARTESIAN_POINT('Ctrl Pts',(-17.9020712048987,-48.4998077153909,
123.439203218317)) ;
#56848 = CARTESIAN_POINT('Ctrl Pts',(-18.2254971301078,-48.6897982730727,
123.64284321915)) ;
#56849 = CARTESIAN_POINT('Ctrl Pts',(-17.9295520560355,-48.5098091925922,
123.700586123937)) ;
#56850 = CARTESIAN_POINT('Ctrl Pts',(-18.2839780007626,-48.6998302939322,
123.845485351349)) ;
#56851 = CARTESIAN_POINT('Ctrl Pts',(-18.0026504044852,-48.5198412134517,
123.953887639501)) ;
#56852 = CARTESIAN_POINT('Ctrl Pts',(-18.3749627895114,-48.7096938376577,
124.03181215673)) ;
#56853 = CARTESIAN_POINT('Ctrl Pts',(-18.1163811919581,-48.5297047571772,
124.186799307523)) ;
#56854 = CARTESIAN_POINT('Ctrl Pts',(-18.4977838557843,-48.7196625513279,
124.201640045108)) ;
#56855 = CARTESIAN_POINT('Ctrl Pts',(-18.2698960728996,-48.5396734708474,
124.399078392985)) ;
#56856 = CARTESIAN_POINT('Ctrl Pts',(-18.6994061492759,-48.7330082987316,
124.396656788491)) ;
#56857 = CARTESIAN_POINT('Ctrl Pts',(-18.5219675224637,-48.5530192182511,
124.642888173995)) ;
#56858 = CARTESIAN_POINT('Ctrl Pts',(-18.9435543299916,-48.7461588538042,
124.533062447628)) ;
#56859 = CARTESIAN_POINT('Ctrl Pts',(-18.8271260676445,-48.5661697733238,
124.813370161097)) ;
#56860 = CARTESIAN_POINT('Ctrl Pts',(-19.2163009315313,-48.7595442343541,
124.602291897744)) ;
#56861 = CARTESIAN_POINT('Ctrl Pts',(-19.1680417733394,-48.5795551538736,
124.899907926198)) ;
#56862 = CARTESIAN_POINT('Ctrl Pts',(-19.4236287954365,-48.7694321703469,
124.617669125966)) ;
#56863 = CARTESIAN_POINT('Ctrl Pts',(-19.4272046606702,-48.5894430898665,
124.919132760913)) ;
#56864 = CARTESIAN_POINT('Ctrl Pts',(-19.6326234694383,-48.7794233601596,
124.59695356156)) ;
#56865 = CARTESIAN_POINT('Ctrl Pts',(-19.6884474342912,-48.5994342796791,
124.89324094596)) ;
#56866 = CARTESIAN_POINT('Ctrl Pts',(-19.8341362224527,-48.7893754586979,
124.54055689342)) ;
#56867 = CARTESIAN_POINT('Ctrl Pts',(-19.9403393905852,-48.6093863782174,
124.822747843727)) ;
#56868 = CARTESIAN_POINT('Ctrl Pts',(-20.0244791000905,-48.7994217151483,
124.449067132527)) ;
#56869 = CARTESIAN_POINT('Ctrl Pts',(-20.1782692263093,-48.6194326346679,
124.708388112083)) ;
#56870 = CARTESIAN_POINT('Ctrl Pts',(-20.1927872751713,-48.8092711625425,
124.328441823876)) ;
#56871 = CARTESIAN_POINT('Ctrl Pts',(-20.3886560574849,-48.629282082062,124.557608790027)) ;
#56872 = CARTESIAN_POINT('Ctrl Pts',(-20.3397216534064,-48.8192338150376,
124.179192839321)) ;
#56873 = CARTESIAN_POINT('Ctrl Pts',(-20.572326096074,-48.6392447345572,124.371049479818)) ;
#56874 = CARTESIAN_POINT('Ctrl Pts',(-20.4590010872859,-48.8292569006798,
124.005486486065)) ;
#56875 = CARTESIAN_POINT('Ctrl Pts',(-20.7214277474901,-48.6492678201993,
124.15391807749)) ;
#56876 = CARTESIAN_POINT('Ctrl Pts',(-20.5456810010499,-48.8391820164367,
123.815659921871)) ;
#56877 = CARTESIAN_POINT('Ctrl Pts',(-20.8297802317773,-48.6591929359562,
123.916635975711)) ;
#56878 = CARTESIAN_POINT('Ctrl Pts',(-20.5986636057936,-48.8492344948365,
123.611094978186)) ;
#56879 = CARTESIAN_POINT('Ctrl Pts',(-20.8960112320081,-48.669245414356,123.660930444439)) ;
#56880 = CARTESIAN_POINT('Ctrl Pts',(-20.6151308206564,-48.8590859935392,
123.4046256451)) ;
#56881 = CARTESIAN_POINT('Ctrl Pts',(-20.9165980683453,-48.6790969130588,
123.402843889693)) ;
#56882 = CARTESIAN_POINT('Ctrl Pts',(-20.5958067267319,-48.8690577327418,
123.19590749213)) ;
#56883 = CARTESIAN_POINT('Ctrl Pts',(-20.8924457356937,-48.6890686522613,
123.141945824746)) ;
#56884 = CARTESIAN_POINT('Ctrl Pts',(-20.5403646088462,-48.8790529405074,
122.993187529069)) ;
#56885 = CARTESIAN_POINT('Ctrl Pts',(-20.8231457688336,-48.699063860027,122.888545055515)) ;
#56886 = CARTESIAN_POINT('Ctrl Pts',(-20.4500071936649,-48.8890869419765,
122.802593518848)) ;
#56887 = CARTESIAN_POINT('Ctrl Pts',(-20.7102015281,-48.709097861496,122.650301300747)) ;
#56888 = CARTESIAN_POINT('Ctrl Pts',(-20.3303491214858,-48.8989423000689,
122.633423450339)) ;
#56889 = CARTESIAN_POINT('Ctrl Pts',(-20.5606310890588,-48.7189532195884,
122.438836911221)) ;
#56890 = CARTESIAN_POINT('Ctrl Pts',(-20.1812231910538,-48.9089417756622,
122.485307584382)) ;
#56891 = CARTESIAN_POINT('Ctrl Pts',(-20.3742255769776,-48.7289526951817,
122.253690036729)) ;
#56892 = CARTESIAN_POINT('Ctrl Pts',(-20.0105298951127,-48.9188362241573,
122.366356746529)) ;
#56893 = CARTESIAN_POINT('Ctrl Pts',(-20.1608603227563,-48.7388471436768,
122.104999075597)) ;
#56894 = CARTESIAN_POINT('Ctrl Pts',(-19.8186007680799,-48.928899348385,122.277447738823)) ;
#56895 = CARTESIAN_POINT('Ctrl Pts',(-19.920950110455,-48.7489102679045,121.993860313418)) ;
#56896 = CARTESIAN_POINT('Ctrl Pts',(-19.6186814141664,-48.9387389747136,
122.224180471466)) ;
#56897 = CARTESIAN_POINT('Ctrl Pts',(-19.6710512311664,-48.7587498942331,
121.92727346975)) ;
#56898 = CARTESIAN_POINT('Ctrl Pts',(-19.4079521083204,-48.9488022097566,
122.205769170469)) ;
#56899 = CARTESIAN_POINT('Ctrl Pts',(-19.4076398792596,-48.7688131292761,
121.904256633365)) ;
#56900 = CARTESIAN_POINT('Ctrl Pts',(-19.2007357621224,-48.9586962149906,
122.224096611744)) ;
#56901 = CARTESIAN_POINT('Ctrl Pts',(-19.1486188793578,-48.7787071345101,
121.927163232638)) ;
#56902 = CARTESIAN_POINT('Ctrl Pts',(-18.9987560013201,-48.9686389282064,
122.277825494424)) ;
#56903 = CARTESIAN_POINT('Ctrl Pts',(-18.8961432338449,-48.7886498477259,
121.994321818585)) ;
#56904 = CARTESIAN_POINT('Ctrl Pts',(-18.8079128243991,-48.9786446680046,
122.36634819626)) ;
#56905 = CARTESIAN_POINT('Ctrl Pts',(-18.6575880746054,-48.7986555875241,
122.104972809747)) ;
#56906 = CARTESIAN_POINT('Ctrl Pts',(-18.6352354087058,-48.988665570151,122.48702462515)) ;
#56907 = CARTESIAN_POINT('Ctrl Pts',(-18.4417397384624,-48.8086764896705,
122.25581614595)) ;
#56908 = CARTESIAN_POINT('Ctrl Pts',(-18.4878939976367,-48.9985563401998,
122.633756235366)) ;
#56909 = CARTESIAN_POINT('Ctrl Pts',(-18.2575608010037,-48.8185672597194,
122.439229061336)) ;
#56910 = CARTESIAN_POINT('Ctrl Pts',(-18.366802071252,-49.0085477509796,122.805381393975)) ;
#56911 = CARTESIAN_POINT('Ctrl Pts',(-18.1061936757507,-48.8285586704991,
122.653759103555)) ;
#56912 = CARTESIAN_POINT('Ctrl Pts',(-18.2777961208184,-49.0184960966441,
122.994637884771)) ;
#56913 = CARTESIAN_POINT('Ctrl Pts',(-17.9949337390312,-48.8385070161635,
122.890328842151)) ;
#56914 = CARTESIAN_POINT('Ctrl Pts',(-18.2225909158697,-49.0284409547052,
123.196309162691)) ;
#56915 = CARTESIAN_POINT('Ctrl Pts',(-17.9259246877566,-48.8484518742248,
123.142417551851)) ;
#56916 = CARTESIAN_POINT('Ctrl Pts',(-18.2033401476526,-49.0384957900982,
123.40679518885)) ;
#56917 = CARTESIAN_POINT('Ctrl Pts',(-17.9018586343297,-48.8585067096177,
123.405524737977)) ;
#56918 = CARTESIAN_POINT('Ctrl Pts',(-18.2201677805228,-49.0483181621996,
123.612623482533)) ;
#56919 = CARTESIAN_POINT('Ctrl Pts',(-17.9228907003336,-48.8683290817192,
123.662811089204)) ;
#56920 = CARTESIAN_POINT('Ctrl Pts',(-18.2733451038834,-49.0583740296434,
123.817216281984)) ;
#56921 = CARTESIAN_POINT('Ctrl Pts',(-17.9893599289027,-48.8783849491629,
123.918552606328)) ;
#56922 = CARTESIAN_POINT('Ctrl Pts',(-18.3605807016632,-49.0683147595013,
124.007132559612)) ;
#56923 = CARTESIAN_POINT('Ctrl Pts',(-18.0984022473482,-48.8883256790208,
124.155949320502)) ;
#56924 = CARTESIAN_POINT('Ctrl Pts',(-18.478492080276,-49.0782190980524,124.178754700712)) ;
#56925 = CARTESIAN_POINT('Ctrl Pts',(-18.2457897777088,-48.8982300175719,
124.370478803639)) ;
#56926 = CARTESIAN_POINT('Ctrl Pts',(-18.6265896771452,-49.0882657794809,
124.329321820747)) ;
#56927 = CARTESIAN_POINT('Ctrl Pts',(-18.4309099577425,-48.9082766990004,
124.558689346557)) ;
#56928 = CARTESIAN_POINT('Ctrl Pts',(-18.7959241485075,-49.0981612869501,
124.450228240295)) ;
#56929 = CARTESIAN_POINT('Ctrl Pts',(-18.6425771223677,-48.9181722064697,
124.709824664254)) ;
#56930 = CARTESIAN_POINT('Ctrl Pts',(-18.9867862815912,-49.1082235554488,
124.541375926304)) ;
#56931 = CARTESIAN_POINT('Ctrl Pts',(-18.8811535876287,-48.9282344749683,
124.823761366756)) ;
#56932 = CARTESIAN_POINT('Ctrl Pts',(-19.1861338900622,-49.1180655457194,
124.596897992535)) ;
#56933 = CARTESIAN_POINT('Ctrl Pts',(-19.1303382919264,-48.9380764652389,
124.893166471284)) ;
#56934 = CARTESIAN_POINT('Ctrl Pts',(-19.3951586958825,-49.1280589626003,
124.617736026602)) ;
#56935 = CARTESIAN_POINT('Ctrl Pts',(-19.391619244589,-48.9480698821199,124.919216288672)) ;
#56936 = CARTESIAN_POINT('Ctrl Pts',(-19.6032371853687,-49.1379834504525,
124.602087040925)) ;
#56937 = CARTESIAN_POINT('Ctrl Pts',(-19.6517180268592,-48.957994369972,124.899657271503)) ;
#56938 = CARTESIAN_POINT('Ctrl Pts',(-19.8069854701028,-49.147983084361,124.550380447897)) ;
#56939 = CARTESIAN_POINT('Ctrl Pts',(-19.9064040385698,-48.9679940038805,
124.835026142199)) ;
#56940 = CARTESIAN_POINT('Ctrl Pts',(-19.9984490408071,-49.1579691946177,
124.464185024781)) ;
#56941 = CARTESIAN_POINT('Ctrl Pts',(-20.1457345661112,-48.9779801141373,
124.727283799882)) ;
#56942 = CARTESIAN_POINT('Ctrl Pts',(-20.1727370286862,-49.1680051458049,
124.345311201538)) ;
#56943 = CARTESIAN_POINT('Ctrl Pts',(-20.3635957587597,-48.9880160653244,
124.578693439331)) ;
#56944 = CARTESIAN_POINT('Ctrl Pts',(-20.3212855419175,-49.1778617841397,
124.200809116619)) ;
#56945 = CARTESIAN_POINT('Ctrl Pts',(-20.5492835775736,-48.9978727036592,
124.398066759206)) ;
#56946 = CARTESIAN_POINT('Ctrl Pts',(-20.4444358570333,-49.1878607442177,
124.030495135267)) ;
#56947 = CARTESIAN_POINT('Ctrl Pts',(-20.7032232578313,-49.0078716637372,
124.185175408139)) ;
#56948 = CARTESIAN_POINT('Ctrl Pts',(-20.5354258116152,-49.1977559745315,
123.843382253148)) ;
#56949 = CARTESIAN_POINT('Ctrl Pts',(-20.8169628558538,-49.017766894051,123.951284539038)) ;
#56950 = CARTESIAN_POINT('Ctrl Pts',(-20.5934596272314,-49.2078164870001,
123.640024401084)) ;
#56951 = CARTESIAN_POINT('Ctrl Pts',(-20.8895070312652,-49.0278274065196,
123.697088016947)) ;
#56952 = CARTESIAN_POINT('Ctrl Pts',(-20.614964621342,-49.2176657785463,123.434065207261)) ;
#56953 = CARTESIAN_POINT('Ctrl Pts',(-20.9163903857337,-49.0376766980658,
123.439638200358)) ;
#56954 = CARTESIAN_POINT('Ctrl Pts',(-20.6006524939482,-49.2276929644785,
123.223753772235)) ;
#56955 = CARTESIAN_POINT('Ctrl Pts',(-20.8985020839433,-49.047703883998,123.176748817964)) ;
#56956 = CARTESIAN_POINT('Ctrl Pts',(-20.5494925233518,-49.2377215009378,
123.019212625671)) ;
#56957 = CARTESIAN_POINT('Ctrl Pts',(-20.8345541011954,-49.0577324204573,
122.921071960493)) ;
#56958 = CARTESIAN_POINT('Ctrl Pts',(-20.4655325528851,-49.2475667409028,
122.830041408162)) ;
#56959 = CARTESIAN_POINT('Ctrl Pts',(-20.7296054274978,-49.0675776604223,
122.684606145125)) ;
#56960 = CARTESIAN_POINT('Ctrl Pts',(-20.3487525475356,-49.257557435826,122.655457201128)) ;
#56961 = CARTESIAN_POINT('Ctrl Pts',(-20.5836317517276,-49.0775683553455,
122.466374760866)) ;
#56962 = CARTESIAN_POINT('Ctrl Pts',(-20.2024139642059,-49.2675952565846,
122.503414527449)) ;
#56963 = CARTESIAN_POINT('Ctrl Pts',(-20.4007099670647,-49.0876061761041,
122.276320211535)) ;
#56964 = CARTESIAN_POINT('Ctrl Pts',(-20.0353851635832,-49.2774398503615,
122.381196686235)) ;
#56965 = CARTESIAN_POINT('Ctrl Pts',(-20.1919240684865,-49.097450769881,122.123545794941)) ;
#56966 = CARTESIAN_POINT('Ctrl Pts',(-19.8472610421014,-49.2874238457376,
122.288151641728)) ;
#56967 = CARTESIAN_POINT('Ctrl Pts',(-19.9567693977813,-49.1074347652571,
122.007237918667)) ;
#56968 = CARTESIAN_POINT('Ctrl Pts',(-19.6465098945046,-49.297372894299,122.229404619294)) ;
#56969 = CARTESIAN_POINT('Ctrl Pts',(-19.7058304590878,-49.1173838138185,
121.933802444851)) ;
#56970 = CARTESIAN_POINT('Ctrl Pts',(-19.4375191683223,-49.3073753332735,
122.206058321571)) ;
#56971 = CARTESIAN_POINT('Ctrl Pts',(-19.4445921214465,-49.127386252793,121.904618015454)) ;
#56972 = CARTESIAN_POINT('Ctrl Pts',(-19.2272793153479,-49.3173965745699,
122.219664475617)) ;
#56973 = CARTESIAN_POINT('Ctrl Pts',(-19.1817922312834,-49.1374074940894,
121.921624060184)) ;
#56974 = CARTESIAN_POINT('Ctrl Pts',(-19.0251633000382,-49.3272892530094,
122.268684611015)) ;
#56975 = CARTESIAN_POINT('Ctrl Pts',(-18.9291459750505,-49.1473001725289,
121.982897915506)) ;
#56976 = CARTESIAN_POINT('Ctrl Pts',(-18.8326207757844,-49.337279306957,122.352565184891)) ;
#56977 = CARTESIAN_POINT('Ctrl Pts',(-18.6884670362895,-49.1572902264765,
122.087747388008)) ;
#56978 = CARTESIAN_POINT('Ctrl Pts',(-18.65820968593,-49.3472376681055,122.468356623585)) ;
#56979 = CARTESIAN_POINT('Ctrl Pts',(-18.4704519829065,-49.167248587625,122.232485671663)) ;
#56980 = CARTESIAN_POINT('Ctrl Pts',(-18.5070800115735,-49.3571372949903,
122.611463780261)) ;
#56981 = CARTESIAN_POINT('Ctrl Pts',(-18.2815383414218,-49.1771482145098,
122.411369259759)) ;
#56982 = CARTESIAN_POINT('Ctrl Pts',(-18.3813177298446,-49.3671851917937,
122.781158712775)) ;
#56983 = CARTESIAN_POINT('Ctrl Pts',(-18.1243345329149,-49.1871961113132,
122.623486945878)) ;
#56984 = CARTESIAN_POINT('Ctrl Pts',(-18.2881930918701,-49.3770805494297,
122.96721883373)) ;
#56985 = CARTESIAN_POINT('Ctrl Pts',(-18.0079271715272,-49.1970914689492,
122.856062333911)) ;
#56986 = CARTESIAN_POINT('Ctrl Pts',(-18.2277777790016,-49.3871422018863,
123.169910866014)) ;
#56987 = CARTESIAN_POINT('Ctrl Pts',(-17.9324068929377,-49.2071531214059,
123.109426695854)) ;
#56988 = CARTESIAN_POINT('Ctrl Pts',(-18.2039634409259,-49.3969868061583,
123.375507420365)) ;
#56989 = CARTESIAN_POINT('Ctrl Pts',(-17.9026375539876,-49.2169977256778,
123.366423552928)) ;
#56990 = CARTESIAN_POINT('Ctrl Pts',(-18.21560282813,-49.4069469278563,123.584573029196)) ;
#56991 = CARTESIAN_POINT('Ctrl Pts',(-17.9171858176287,-49.2269578473758,
123.627756075238)) ;
#56992 = CARTESIAN_POINT('Ctrl Pts',(-18.2641366558949,-49.4169849622188,
123.789939361942)) ;
#56993 = CARTESIAN_POINT('Ctrl Pts',(-17.9778519475614,-49.2369958817383,
123.884464098804)) ;
#56994 = CARTESIAN_POINT('Ctrl Pts',(-18.3458936811806,-49.4268592748053,
123.980778500139)) ;
#56995 = CARTESIAN_POINT('Ctrl Pts',(-18.0800477461698,-49.2468701943248,
124.123014445759)) ;
#56996 = CARTESIAN_POINT('Ctrl Pts',(-18.4617697259283,-49.436928755588,124.1579063665)) ;
#56997 = CARTESIAN_POINT('Ctrl Pts',(-18.2248917332059,-49.2569396751075,
124.344424493794)) ;
#56998 = CARTESIAN_POINT('Ctrl Pts',(-18.6032069971224,-49.4467630916051,
124.308729317286)) ;
#56999 = CARTESIAN_POINT('Ctrl Pts',(-18.4016886195746,-49.2667740111246,
124.532954912197)) ;
#57000 = CARTESIAN_POINT('Ctrl Pts',(-18.7716598122527,-49.4567960493333,
124.435654755595)) ;
#57001 = CARTESIAN_POINT('Ctrl Pts',(-18.6122540927978,-49.2768069688528,
124.691612235922)) ;
#57002 = CARTESIAN_POINT('Ctrl Pts',(-18.9596285266735,-49.4668164479085,
124.530768810622)) ;
#57003 = CARTESIAN_POINT('Ctrl Pts',(-18.8472145111849,-49.286827367428,124.810505656996)) ;
#57004 = CARTESIAN_POINT('Ctrl Pts',(-19.1580012266402,-49.4766820216797,
124.591362825177)) ;
#57005 = CARTESIAN_POINT('Ctrl Pts',(-19.0951813190911,-49.2966929411992,
124.886249263638)) ;
#57006 = CARTESIAN_POINT('Ctrl Pts',(-19.3680870984409,-49.4867508963358,
124.617111323159)) ;
#57007 = CARTESIAN_POINT('Ctrl Pts',(-19.3577881565843,-49.3067618158553,
124.918435603033)) ;
#57008 = CARTESIAN_POINT('Ctrl Pts',(-19.5747954024805,-49.4965963272413,
124.606267618942)) ;
#57009 = CARTESIAN_POINT('Ctrl Pts',(-19.6161749842929,-49.3166072467608,
124.904881658668)) ;
#57010 = CARTESIAN_POINT('Ctrl Pts',(-19.7793647307938,-49.506575952112,124.559725510975)) ;
#57011 = CARTESIAN_POINT('Ctrl Pts',(-19.8718870581655,-49.3265868716315,
124.846704437051)) ;
#57012 = CARTESIAN_POINT('Ctrl Pts',(-19.9733472943274,-49.5165946350261,
124.477683630801)) ;
#57013 = CARTESIAN_POINT('Ctrl Pts',(-20.1143655070661,-49.3366055545456,
124.744152692694)) ;
#57014 = CARTESIAN_POINT('Ctrl Pts',(-20.1480134440682,-49.5264779002099,
124.365106465105)) ;
#57015 = CARTESIAN_POINT('Ctrl Pts',(-20.3326993756055,-49.3464888197294,
124.603431043529)) ;
#57016 = CARTESIAN_POINT('Ctrl Pts',(-20.3032270535751,-49.5365461943013,
124.221241519737)) ;
#57017 = CARTESIAN_POINT('Ctrl Pts',(-20.5267164376819,-49.3565571138208,
124.423600519523)) ;
#57018 = CARTESIAN_POINT('Ctrl Pts',(-20.4283133218922,-49.5463763244866,
124.056692970203)) ;
#57019 = CARTESIAN_POINT('Ctrl Pts',(-20.6830755386352,-49.3663872440061,
124.217913860324)) ;
#57020 = CARTESIAN_POINT('Ctrl Pts',(-20.5254162570907,-49.5564428727018,
123.868692053615)) ;
#57021 = CARTESIAN_POINT('Ctrl Pts',(-20.8044543032973,-49.3764537922212,
123.982913211206)) ;
#57022 = CARTESIAN_POINT('Ctrl Pts',(-20.5871922984484,-49.5663331213904,
123.67013049004)) ;
#57023 = CARTESIAN_POINT('Ctrl Pts',(-20.8816750149605,-49.3863440409099,
123.734710364382)) ;
#57024 = CARTESIAN_POINT('Ctrl Pts',(-20.6142760100577,-49.5763253031664,
123.461828924434)) ;
#57025 = CARTESIAN_POINT('Ctrl Pts',(-20.9155298641694,-49.3963362226859,
123.47433321887)) ;
#57026 = CARTESIAN_POINT('Ctrl Pts',(-20.6046113032203,-49.5862880837942,
123.252607087574)) ;
#57027 = CARTESIAN_POINT('Ctrl Pts',(-20.9034492218807,-49.4062990033137,
123.212805454245)) ;
#57028 = CARTESIAN_POINT('Ctrl Pts',(-20.5595393091731,-49.5961924884679,
123.049307305498)) ;
#57029 = CARTESIAN_POINT('Ctrl Pts',(-20.8471090807329,-49.4162034079875,
122.95867980125)) ;
#57030 = CARTESIAN_POINT('Ctrl Pts',(-20.478467374034,-49.606252482947,122.853990633004)) ;
#57031 = CARTESIAN_POINT('Ctrl Pts',(-20.7457693981853,-49.4262634024665,
122.714534227853)) ;
#57032 = CARTESIAN_POINT('Ctrl Pts',(-20.3672356635817,-49.6161011049168,
122.679339657836)) ;
#57033 = CARTESIAN_POINT('Ctrl Pts',(-20.6067290421984,-49.4361120244363,
122.496219298813)) ;
#57034 = CARTESIAN_POINT('Ctrl Pts',(-20.2251544951592,-49.6261315443286,
122.523536505665)) ;
#57035 = CARTESIAN_POINT('Ctrl Pts',(-20.429127558072,-49.4461424638481,122.301465539428)) ;
#57036 = CARTESIAN_POINT('Ctrl Pts',(-20.0582370192232,-49.6361412599634,
122.395350931652)) ;
#57037 = CARTESIAN_POINT('Ctrl Pts',(-20.2204806966358,-49.4561521794829,
122.141233524141)) ;
#57038 = CARTESIAN_POINT('Ctrl Pts',(-19.8735746846781,-49.646052012656,122.298896339654)) ;
#57039 = CARTESIAN_POINT('Ctrl Pts',(-19.9896519590277,-49.4660629321755,
122.020664911434)) ;
#57040 = CARTESIAN_POINT('Ctrl Pts',(-19.6747293616063,-49.6559812856024,
122.23534414131)) ;
#57041 = CARTESIAN_POINT('Ctrl Pts',(-19.7410945155702,-49.4759922051219,
121.941224683029)) ;
#57042 = CARTESIAN_POINT('Ctrl Pts',(-19.4655008779412,-49.666023976995,122.207142648671)) ;
#57043 = CARTESIAN_POINT('Ctrl Pts',(-19.4795590979007,-49.4860348965146,
121.905973034113)) ;
#57044 = CARTESIAN_POINT('Ctrl Pts',(-19.2578087514022,-49.6759105102126,
122.215430584698)) ;
#57045 = CARTESIAN_POINT('Ctrl Pts',(-19.2199428620303,-49.4959214297321,
121.916333239267)) ;
#57046 = CARTESIAN_POINT('Ctrl Pts',(-19.0524672632715,-49.6859036551446,
122.259778671092)) ;
#57047 = CARTESIAN_POINT('Ctrl Pts',(-18.9632658836805,-49.5059145746641,
121.971768765041)) ;
#57048 = CARTESIAN_POINT('Ctrl Pts',(-18.8588885046853,-49.6958493359811,
122.3388088344)) ;
#57049 = CARTESIAN_POINT('Ctrl Pts',(-18.7212920166234,-49.5158602555006,
122.070557018354)) ;
#57050 = CARTESIAN_POINT('Ctrl Pts',(-18.6817080873745,-49.7057965931296,
122.449910909112)) ;
#57051 = CARTESIAN_POINT('Ctrl Pts',(-18.4998162838952,-49.5258075126491,
122.209435357085)) ;
#57052 = CARTESIAN_POINT('Ctrl Pts',(-18.5251114478869,-49.7158444970016,
122.591672777569)) ;
#57053 = CARTESIAN_POINT('Ctrl Pts',(-18.304070955553,-49.5358554165211,122.386637839432)) ;
#57054 = CARTESIAN_POINT('Ctrl Pts',(-18.3979488536748,-49.7256921960996,
122.755046538999)) ;
#57055 = CARTESIAN_POINT('Ctrl Pts',(-18.145117242453,-49.5457031156191,122.590856449649)) ;
#57056 = CARTESIAN_POINT('Ctrl Pts',(-18.2993856740285,-49.7356536870782,
122.939814886333)) ;
#57057 = CARTESIAN_POINT('Ctrl Pts',(-18.0219137174262,-49.5556646065978,
122.821817640605)) ;
#57058 = CARTESIAN_POINT('Ctrl Pts',(-18.2342214042971,-49.7456831494922,
123.140352456418)) ;
#57059 = CARTESIAN_POINT('Ctrl Pts',(-17.9404590217541,-49.5656940690117,
123.072489705592)) ;
#57060 = CARTESIAN_POINT('Ctrl Pts',(-18.2051140091869,-49.7555903805921,
123.346589615801)) ;
#57061 = CARTESIAN_POINT('Ctrl Pts',(-17.904075330187,-49.5756013001116,123.330287135653)) ;
#57062 = CARTESIAN_POINT('Ctrl Pts',(-18.211860951267,-49.7655367592695,123.555572269236)) ;
#57063 = CARTESIAN_POINT('Ctrl Pts',(-17.912509878086,-49.585547678789,123.591516015352)) ;
#57064 = CARTESIAN_POINT('Ctrl Pts',(-18.2549768342654,-49.7755415280784,
123.761455951672)) ;
#57065 = CARTESIAN_POINT('Ctrl Pts',(-17.9664056107729,-49.5955524475979,
123.848870528869)) ;
#57066 = CARTESIAN_POINT('Ctrl Pts',(-18.3335291933488,-49.7855626490986,
123.956934913202)) ;
#57067 = CARTESIAN_POINT('Ctrl Pts',(-18.0645967711896,-49.6055735686181,
124.093218904719)) ;
#57068 = CARTESIAN_POINT('Ctrl Pts',(-18.4431860931502,-49.7954535149512,
124.133615577516)) ;
#57069 = CARTESIAN_POINT('Ctrl Pts',(-18.2016691690772,-49.6154644344707,
124.314070124151)) ;
#57070 = CARTESIAN_POINT('Ctrl Pts',(-18.5830122161219,-49.8054443237105,
124.290330824793)) ;
#57071 = CARTESIAN_POINT('Ctrl Pts',(-18.3764527035837,-49.62545524323,124.509963683078)) ;
#57072 = CARTESIAN_POINT('Ctrl Pts',(-18.747304518671,-49.8153949818908,124.419846948591)) ;
#57073 = CARTESIAN_POINT('Ctrl Pts',(-18.5818191089981,-49.6354059014103,
124.671858407389)) ;
#57074 = CARTESIAN_POINT('Ctrl Pts',(-18.9311656323854,-49.8253311915329,
124.518959631838)) ;
#57075 = CARTESIAN_POINT('Ctrl Pts',(-18.8116465770376,-49.6453421110524,
124.795748611864)) ;
#57076 = CARTESIAN_POINT('Ctrl Pts',(-19.1303351595038,-49.8353143582578,
124.585224682126)) ;
#57077 = CARTESIAN_POINT('Ctrl Pts',(-19.0606091019101,-49.6553252777773,
124.87857888627)) ;
#57078 = CARTESIAN_POINT('Ctrl Pts',(-19.3392535954594,-49.8453581554681,
124.615693199531)) ;
#57079 = CARTESIAN_POINT('Ctrl Pts',(-19.3217571085241,-49.6653690749876,
124.916663479723)) ;
#57080 = CARTESIAN_POINT('Ctrl Pts',(-19.5458273359172,-49.8551863716364,
124.610045735336)) ;
#57081 = CARTESIAN_POINT('Ctrl Pts',(-19.5799756953261,-49.6751972911558,
124.90960289312)) ;
#57082 = CARTESIAN_POINT('Ctrl Pts',(-19.7533454043374,-49.8652629391056,
124.567682590718)) ;
#57083 = CARTESIAN_POINT('Ctrl Pts',(-19.8393726054797,-49.6852738586251,
124.856647819379)) ;
#57084 = CARTESIAN_POINT('Ctrl Pts',(-19.9460859117418,-49.875115024795,124.491728264813)) ;
#57085 = CARTESIAN_POINT('Ctrl Pts',(-20.0802989167655,-49.6951259443145,
124.761703259226)) ;
#57086 = CARTESIAN_POINT('Ctrl Pts',(-20.126701616753,-49.8851882922004,124.381226191815)) ;
#57087 = CARTESIAN_POINT('Ctrl Pts',(-20.3060674977483,-49.7051992117199,
124.623574722153)) ;
#57088 = CARTESIAN_POINT('Ctrl Pts',(-20.2817328321541,-49.895029708624,124.244194431429)) ;
#57089 = CARTESIAN_POINT('Ctrl Pts',(-20.4998566129317,-49.7150406281435,
124.452283158368)) ;
#57090 = CARTESIAN_POINT('Ctrl Pts',(-20.4127836030217,-49.9049909667667,
124.080861209861)) ;
#57091 = CARTESIAN_POINT('Ctrl Pts',(-20.6636690761592,-49.7250018862862,
124.248115309387)) ;
#57092 = CARTESIAN_POINT('Ctrl Pts',(-20.5138903858792,-49.9150276431986,
123.895664527938)) ;
#57093 = CARTESIAN_POINT('Ctrl Pts',(-20.7900512079499,-49.7350385627182,
124.016618869512)) ;
#57094 = CARTESIAN_POINT('Ctrl Pts',(-20.5805838627807,-49.9249062510625,
123.698962304801)) ;
#57095 = CARTESIAN_POINT('Ctrl Pts',(-20.8734168718336,-49.744917170582,123.770739635663)) ;
#57096 = CARTESIAN_POINT('Ctrl Pts',(-20.6127292545574,-49.9349664797013,
123.489949368876)) ;
#57097 = CARTESIAN_POINT('Ctrl Pts',(-20.9135969836862,-49.7549773992208,
123.50947350539)) ;
#57098 = CARTESIAN_POINT('Ctrl Pts',(-20.6082434967595,-49.9448334638621,
123.282536648227)) ;
#57099 = CARTESIAN_POINT('Ctrl Pts',(-20.9079881467094,-49.7648443833816,
123.250206599939)) ;
#57100 = CARTESIAN_POINT('Ctrl Pts',(-20.5676533220387,-49.9548390301148,
123.076169983753)) ;
#57101 = CARTESIAN_POINT('Ctrl Pts',(-20.8572486898122,-49.7748499496343,
122.992248524958)) ;
#57102 = CARTESIAN_POINT('Ctrl Pts',(-20.4919395617635,-49.9648228185294,
122.880371545976)) ;
#57103 = CARTESIAN_POINT('Ctrl Pts',(-20.7626047939458,-49.7848337380489,
122.747500893185)) ;
#57104 = CARTESIAN_POINT('Ctrl Pts',(-20.3825347856944,-49.974868675332,122.699741996269)) ;
#57105 = CARTESIAN_POINT('Ctrl Pts',(-20.6258474890933,-49.7948795948515,
122.521714953315)) ;
#57106 = CARTESIAN_POINT('Ctrl Pts',(-20.246666531369,-49.984694552548,122.544142027715)) ;
#57107 = CARTESIAN_POINT('Ctrl Pts',(-20.4560100050582,-49.8047054720675,
122.327215169929)) ;
#57108 = CARTESIAN_POINT('Ctrl Pts',(-20.0835826601991,-49.9946850283893,
122.411791016735)) ;
#57109 = CARTESIAN_POINT('Ctrl Pts',(-20.252153795509,-49.8146959479088,122.16177782072)) ;
#57110 = CARTESIAN_POINT('Ctrl Pts',(-19.8987503711464,-50.0047286042881,
122.309710132215)) ;
#57111 = CARTESIAN_POINT('Ctrl Pts',(-20.0211126979257,-49.8247395238076,
122.03417835313)) ;
#57112 = CARTESIAN_POINT('Ctrl Pts',(-19.7035546402409,-50.0145503965861,
122.242375343609)) ;
#57113 = CARTESIAN_POINT('Ctrl Pts',(-19.7771162249332,-49.8345613161056,
121.95001127871)) ;
#57114 = CARTESIAN_POINT('Ctrl Pts',(-19.495286249998,-50.024585362212,122.208741496858)) ;
#57115 = CARTESIAN_POINT('Ctrl Pts',(-19.5167805110306,-49.8445962817315,
121.907971037083)) ;
#57116 = CARTESIAN_POINT('Ctrl Pts',(-19.2845564519754,-50.034610279145,122.21236484356)) ;
#57117 = CARTESIAN_POINT('Ctrl Pts',(-19.2533683214096,-49.8546211986646,
121.912502122611)) ;
#57118 = CARTESIAN_POINT('Ctrl Pts',(-19.0811423574655,-50.0444622175212,
122.251384498715)) ;
#57119 = CARTESIAN_POINT('Ctrl Pts',(-18.9991000928775,-49.8644731370407,
121.961278882103)) ;
#57120 = CARTESIAN_POINT('Ctrl Pts',(-18.8847759421629,-50.0544531935459,
122.325861032936)) ;
#57121 = CARTESIAN_POINT('Ctrl Pts',(-18.7536426684467,-49.8744641130654,
122.054376600757)) ;
#57122 = CARTESIAN_POINT('Ctrl Pts',(-18.7055278261908,-50.0643710143496,
122.432422183055)) ;
#57123 = CARTESIAN_POINT('Ctrl Pts',(-18.5295831347982,-49.8843819338691,
122.187580190288)) ;
#57124 = CARTESIAN_POINT('Ctrl Pts',(-18.5457533128135,-50.0743997349142,
122.569951039098)) ;
#57125 = CARTESIAN_POINT('Ctrl Pts',(-18.3298664400282,-49.8944106544337,
122.35949288137)) ;
#57126 = CARTESIAN_POINT('Ctrl Pts',(-18.4140890328722,-50.0842826615234,
122.730702151589)) ;
#57127 = CARTESIAN_POINT('Ctrl Pts',(-18.1652873215396,-49.9042935810429,
122.560433756569)) ;
#57128 = CARTESIAN_POINT('Ctrl Pts',(-18.3108162869546,-50.0942869466428,
122.913895712092)) ;
#57129 = CARTESIAN_POINT('Ctrl Pts',(-18.0361983459777,-49.9142978661624,
122.789426912386)) ;
#57130 = CARTESIAN_POINT('Ctrl Pts',(-18.2410673724431,-50.1042706278507,
123.111893587272)) ;
#57131 = CARTESIAN_POINT('Ctrl Pts',(-17.9490142970122,-49.9242815473702,
123.036925185799)) ;
#57132 = CARTESIAN_POINT('Ctrl Pts',(-18.20680742649,-50.1143116265806,123.320172550146)) ;
#57133 = CARTESIAN_POINT('Ctrl Pts',(-17.9061915787471,-49.9343225461001,
123.29727415585)) ;
#57134 = CARTESIAN_POINT('Ctrl Pts',(-18.2088904962245,-50.1241440714477,
123.52687311072)) ;
#57135 = CARTESIAN_POINT('Ctrl Pts',(-17.908797723189,-49.9441549909672,123.555650792539)) ;
#57136 = CARTESIAN_POINT('Ctrl Pts',(-18.2468487955305,-50.1341390698781,
123.733536628154)) ;
#57137 = CARTESIAN_POINT('Ctrl Pts',(-17.9562480236737,-49.9541499893976,
123.813979871603)) ;
#57138 = CARTESIAN_POINT('Ctrl Pts',(-18.3208110885934,-50.1441706186277,
123.931048389592)) ;
#57139 = CARTESIAN_POINT('Ctrl Pts',(-18.048703067227,-49.9641815381472,124.060868718077)) ;
#57140 = CARTESIAN_POINT('Ctrl Pts',(-18.4259334331203,-50.1540359969332,
124.109821606205)) ;
#57141 = CARTESIAN_POINT('Ctrl Pts',(-18.1801084381385,-49.9740469164527,
124.284334653835)) ;
#57142 = CARTESIAN_POINT('Ctrl Pts',(-18.5613765662075,-50.1639978443934,
124.26956672375)) ;
#57143 = CARTESIAN_POINT('Ctrl Pts',(-18.3494144438133,-49.984008763913,124.484014611013)) ;
#57144 = CARTESIAN_POINT('Ctrl Pts',(-18.7238875342035,-50.1740327852077,
124.404073431431)) ;
#57145 = CARTESIAN_POINT('Ctrl Pts',(-18.5525546908186,-49.9940437047272,
124.65214608364)) ;
#57146 = CARTESIAN_POINT('Ctrl Pts',(-18.9044058295045,-50.1839177462248,
124.507085840432)) ;
#57147 = CARTESIAN_POINT('Ctrl Pts',(-18.7782043026535,-50.0039286657444,
124.780909685997)) ;
#57148 = CARTESIAN_POINT('Ctrl Pts',(-19.103599497382,-50.1939833551437,124.578405574943)) ;
#57149 = CARTESIAN_POINT('Ctrl Pts',(-19.0271970939725,-50.0139942746632,
124.870056934682)) ;
#57150 = CARTESIAN_POINT('Ctrl Pts',(-19.3074891707686,-50.2038225301854,
124.613469337633)) ;
#57151 = CARTESIAN_POINT('Ctrl Pts',(-19.2820603187289,-50.0238334497049,
124.913884244431)) ;
#57152 = CARTESIAN_POINT('Ctrl Pts',(-19.5190104294486,-50.2138850856853,
124.612870871899)) ;
#57153 = CARTESIAN_POINT('Ctrl Pts',(-19.5464617510583,-50.0338960052048,
124.913133557283)) ;
#57154 = CARTESIAN_POINT('Ctrl Pts',(-19.7237883029565,-50.2237822603782,
124.575939416995)) ;
#57155 = CARTESIAN_POINT('Ctrl Pts',(-19.8024340996861,-50.0437931798978,
124.86696663096)) ;
#57156 = CARTESIAN_POINT('Ctrl Pts',(-19.9199318195631,-50.2337129753016,
124.504433105692)) ;
#57157 = CARTESIAN_POINT('Ctrl Pts',(-20.0476128623709,-50.0537238948211,
124.777581121193)) ;
#57158 = CARTESIAN_POINT('Ctrl Pts',(-20.1026202548277,-50.2437570033792,
124.398553787405)) ;
#57159 = CARTESIAN_POINT('Ctrl Pts',(-20.2759720548009,-50.0637679228987,
124.64522970371)) ;
#57160 = CARTESIAN_POINT('Ctrl Pts',(-20.2617301651388,-50.2536432052325,
124.264811495273)) ;
#57161 = CARTESIAN_POINT('Ctrl Pts',(-20.4748580561478,-50.073654124752,124.478049523118)) ;
#57162 = CARTESIAN_POINT('Ctrl Pts',(-20.3968653014659,-50.2636363716993,
124.103982279919)) ;
#57163 = CARTESIAN_POINT('Ctrl Pts',(-20.6437749692228,-50.0836472912189,
124.277011182846)) ;
#57164 = CARTESIAN_POINT('Ctrl Pts',(-20.5015352977048,-50.2735758426865,
123.923098316065)) ;
#57165 = CARTESIAN_POINT('Ctrl Pts',(-20.7746102357307,-50.093586762206,124.050904663447)) ;
#57166 = CARTESIAN_POINT('Ctrl Pts',(-20.5737859343558,-50.2835923570407,
123.725325502378)) ;
#57167 = CARTESIAN_POINT('Ctrl Pts',(-20.8649209947813,-50.1036032765602,
123.803687665032)) ;
#57168 = CARTESIAN_POINT('Ctrl Pts',(-20.6104642438826,-50.2935223835175,
123.519782917965)) ;
#57169 = CARTESIAN_POINT('Ctrl Pts',(-20.9107662309863,-50.113533303037,123.546758707791)) ;
#57170 = CARTESIAN_POINT('Ctrl Pts',(-20.6108086522076,-50.303574919027,123.308465111307)) ;
#57171 = CARTESIAN_POINT('Ctrl Pts',(-20.911194011605,-50.1235858385465,123.282611468897)) ;
#57172 = CARTESIAN_POINT('Ctrl Pts',(-20.5753140283502,-50.3134213222466,
123.104521388382)) ;
#57173 = CARTESIAN_POINT('Ctrl Pts',(-20.8668229608976,-50.1334322417662,
123.02768188532)) ;
#57174 = CARTESIAN_POINT('Ctrl Pts',(-20.5047639569835,-50.3233833651007,
122.907340910753)) ;
#57175 = CARTESIAN_POINT('Ctrl Pts',(-20.7786326900258,-50.1433942846202,
122.781207115368)) ;
#57176 = CARTESIAN_POINT('Ctrl Pts',(-20.4001053609626,-50.3334119158914,
122.724304136021)) ;
#57177 = CARTESIAN_POINT('Ctrl Pts',(-20.6478070137,-50.1534228354109,122.552412487742)) ;
#57178 = CARTESIAN_POINT('Ctrl Pts',(-20.2669138933572,-50.343322241609,122.564103535408)) ;
#57179 = CARTESIAN_POINT('Ctrl Pts',(-20.4813154003933,-50.1633331611285,
122.352163354325)) ;
#57180 = CARTESIAN_POINT('Ctrl Pts',(-20.1078761445415,-50.3532571534386,
122.428702223204)) ;
#57181 = CARTESIAN_POINT('Ctrl Pts',(-20.2825162868525,-50.1732680729581,
122.182913771785)) ;
#57182 = CARTESIAN_POINT('Ctrl Pts',(-19.9257330097845,-50.3632981602067,
122.32201626754)) ;
#57183 = CARTESIAN_POINT('Ctrl Pts',(-20.0548359116665,-50.1833090797262,
122.049558725216)) ;
#57184 = CARTESIAN_POINT('Ctrl Pts',(-19.7308882493759,-50.3731857930389,
122.249563232581)) ;
#57185 = CARTESIAN_POINT('Ctrl Pts',(-19.8112788264832,-50.1931967125584,
121.958995011196)) ;
#57186 = CARTESIAN_POINT('Ctrl Pts',(-19.5243853029293,-50.3831762241369,
122.211289416377)) ;
#57187 = CARTESIAN_POINT('Ctrl Pts',(-19.5531495649875,-50.2031871436564,
121.911155500771)) ;
#57188 = CARTESIAN_POINT('Ctrl Pts',(-19.3150912519442,-50.3931316606941,
122.209571649096)) ;
#57189 = CARTESIAN_POINT('Ctrl Pts',(-19.2915318675942,-50.2131425802137,
121.909011127435)) ;
#57190 = CARTESIAN_POINT('Ctrl Pts',(-19.1095552736864,-50.4030426087935,
122.243685794913)) ;
#57191 = CARTESIAN_POINT('Ctrl Pts',(-19.0346123537931,-50.223053528313,121.951656547133)) ;
#57192 = CARTESIAN_POINT('Ctrl Pts',(-18.9109486179919,-50.4130546848912,
122.313456614259)) ;
#57193 = CARTESIAN_POINT('Ctrl Pts',(-18.786354698485,-50.2330656044107,122.038872975787)) ;
#57194 = CARTESIAN_POINT('Ctrl Pts',(-18.727435602444,-50.4230820069661,122.417161220471)) ;
#57195 = CARTESIAN_POINT('Ctrl Pts',(-18.5569655229776,-50.2430929264857,
122.168505406345)) ;
#57196 = CARTESIAN_POINT('Ctrl Pts',(-18.5670779315736,-50.4329407819203,
122.548532884562)) ;
#57197 = CARTESIAN_POINT('Ctrl Pts',(-18.3565173090446,-50.2529517014398,
122.332725267534)) ;
#57198 = CARTESIAN_POINT('Ctrl Pts',(-18.3833334191599,-50.4463669747327,
122.762717425023)) ;
#57199 = CARTESIAN_POINT('Ctrl Pts',(-18.1268538969004,-50.2663778942522,
122.600443072263)) ;
#57200 = CARTESIAN_POINT('Ctrl Pts',(-18.2623681721055,-50.4594509905141,
123.013391436687)) ;
#57201 = CARTESIAN_POINT('Ctrl Pts',(-17.9756521685596,-50.2794619100337,
122.913754436123)) ;
#57202 = CARTESIAN_POINT('Ctrl Pts',(-18.2092179613212,-50.4729244392694,
123.29151187479)) ;
#57203 = CARTESIAN_POINT('Ctrl Pts',(-17.9092019312809,-50.2929353587889,
123.261460162943)) ;
#57204 = CARTESIAN_POINT('Ctrl Pts',(-18.2065405992436,-50.4827573970752,
123.498250206426)) ;
#57205 = CARTESIAN_POINT('Ctrl Pts',(-17.9058612704974,-50.3027683165947,
123.519872041673)) ;
#57206 = CARTESIAN_POINT('Ctrl Pts',(-18.2393587707171,-50.4927206705259,
123.705106522157)) ;
#57207 = CARTESIAN_POINT('Ctrl Pts',(-17.9468858269984,-50.3127315900454,
123.778444889164)) ;
#57208 = CARTESIAN_POINT('Ctrl Pts',(-18.3085355723821,-50.5027577443438,
123.904453594488)) ;
#57209 = CARTESIAN_POINT('Ctrl Pts',(-18.0333597049391,-50.3227686638634,
124.027627149756)) ;
#57210 = CARTESIAN_POINT('Ctrl Pts',(-18.409286084184,-50.5126327473555,124.085999426355)) ;
#57211 = CARTESIAN_POINT('Ctrl Pts',(-18.1593001784576,-50.332643666875,124.254558222602)) ;
#57212 = CARTESIAN_POINT('Ctrl Pts',(-18.5425517962584,-50.5227004269817,
124.250393752023)) ;
#57213 = CARTESIAN_POINT('Ctrl Pts',(-18.3258841680297,-50.3427113465012,
124.460049112042)) ;
#57214 = CARTESIAN_POINT('Ctrl Pts',(-18.6986982462725,-50.5325412771994,
124.386149557232)) ;
#57215 = CARTESIAN_POINT('Ctrl Pts',(-18.5210703742057,-50.3525521967189,
124.629743115024)) ;
#57216 = CARTESIAN_POINT('Ctrl Pts',(-18.9386955742681,-50.5458774756753,
124.531065619422)) ;
#57217 = CARTESIAN_POINT('Ctrl Pts',(-18.8210606851902,-50.3658883951949,
124.810877501258)) ;
#57218 = CARTESIAN_POINT('Ctrl Pts',(-19.2087059356425,-50.5590949994898,
124.609228100724)) ;
#57219 = CARTESIAN_POINT('Ctrl Pts',(-19.1585310682669,-50.3791059190093,
124.908576997398)) ;
#57220 = CARTESIAN_POINT('Ctrl Pts',(-19.488920896454,-50.572429925981,124.615199991677)) ;
#57221 = CARTESIAN_POINT('Ctrl Pts',(-19.5088595130197,-50.3924408455006,
124.916046148063)) ;
#57222 = CARTESIAN_POINT('Ctrl Pts',(-19.6963926036681,-50.5824130265756,
124.583239687426)) ;
#57223 = CARTESIAN_POINT('Ctrl Pts',(-19.7681867122923,-50.4024239460952,
124.876091752379)) ;
#57224 = CARTESIAN_POINT('Ctrl Pts',(-19.8962274127877,-50.5924578024753,
124.515046658216)) ;
#57225 = CARTESIAN_POINT('Ctrl Pts',(-20.0179829922926,-50.4124687219948,
124.790847910401)) ;
#57226 = CARTESIAN_POINT('Ctrl Pts',(-20.0772393222898,-50.6022757256612,
124.415835187125)) ;
#57227 = CARTESIAN_POINT('Ctrl Pts',(-20.2442444734922,-50.4222866451807,
124.666833014762)) ;
#57228 = CARTESIAN_POINT('Ctrl Pts',(-20.2423226616433,-50.6123250396165,
124.284011355845)) ;
#57229 = CARTESIAN_POINT('Ctrl Pts',(-20.4505999320312,-50.432335959136,124.502045801009)) ;
#57230 = CARTESIAN_POINT('Ctrl Pts',(-20.4268261999454,-50.6256287802391,
124.073810716125)) ;
#57231 = CARTESIAN_POINT('Ctrl Pts',(-20.6812147144193,-50.4456396997586,
124.239319481669)) ;
#57232 = CARTESIAN_POINT('Ctrl Pts',(-20.5831565120962,-50.6421189757157,
123.759929328214)) ;
#57233 = CARTESIAN_POINT('Ctrl Pts',(-20.8766371022421,-50.4621298952353,
123.846918741814)) ;
#57234 = CARTESIAN_POINT('Ctrl Pts',(-20.6233943821416,-50.6588381406404,
123.40675844073)) ;
#57235 = CARTESIAN_POINT('Ctrl Pts',(-20.926926793522,-50.4788490601599,123.405534034858)) ;
#57236 = CARTESIAN_POINT('Ctrl Pts',(-20.5824794471599,-50.6719991343105,
123.133106842893)) ;
#57237 = CARTESIAN_POINT('Ctrl Pts',(-20.8757804023398,-50.49201005383,123.063406602083)) ;
#57238 = CARTESIAN_POINT('Ctrl Pts',(-20.516519250953,-50.6819953564158,122.933581400906)) ;
#57239 = CARTESIAN_POINT('Ctrl Pts',(-20.7933286315983,-50.5020062759353,
122.814013822107)) ;
#57240 = CARTESIAN_POINT('Ctrl Pts',(-20.4162173833348,-50.6920191959495,
122.748251975362)) ;
#57241 = CARTESIAN_POINT('Ctrl Pts',(-20.6679470250345,-50.512030115469,122.582347913081)) ;
#57242 = CARTESIAN_POINT('Ctrl Pts',(-20.2443086428061,-50.7052125179428,
122.530542353315)) ;
#57243 = CARTESIAN_POINT('Ctrl Pts',(-20.4530703197071,-50.5252234374623,
122.310222407797)) ;
#57244 = CARTESIAN_POINT('Ctrl Pts',(-19.9606322188696,-50.7218716897201,
122.318490004045)) ;
#57245 = CARTESIAN_POINT('Ctrl Pts',(-20.0984605250235,-50.5418826092396,
122.045150356451)) ;
#57246 = CARTESIAN_POINT('Ctrl Pts',(-19.5552783088555,-50.7417818652058,
122.196329453374)) ;
#57247 = CARTESIAN_POINT('Ctrl Pts',(-19.5917715292075,-50.5617927847253,
121.892456854642)) ;
#57248 = CARTESIAN_POINT('Ctrl Pts',(-19.1329219062142,-50.7616718530502,
122.218924903769)) ;
#57249 = CARTESIAN_POINT('Ctrl Pts',(-19.0638261203038,-50.5816827725697,
121.920703930721)) ;
#57250 = CARTESIAN_POINT('Ctrl Pts',(-18.7416302883475,-50.781677301065,122.385558421519)) ;
#57251 = CARTESIAN_POINT('Ctrl Pts',(-18.5747132437699,-50.6016882205845,
122.128999458592)) ;
#57252 = CARTESIAN_POINT('Ctrl Pts',(-18.4328824089552,-50.8015136950923,
122.673074672253)) ;
#57253 = CARTESIAN_POINT('Ctrl Pts',(-18.1887817455253,-50.6215246146118,
122.488396022904)) ;
#57254 = CARTESIAN_POINT('Ctrl Pts',(-18.2390777335758,-50.821521488989,123.051656272595)) ;
#57255 = CARTESIAN_POINT('Ctrl Pts',(-17.9465286195624,-50.6415324085085,
122.961624501202)) ;
#57256 = CARTESIAN_POINT('Ctrl Pts',(-18.1864063154851,-50.8413481252829,
123.469998542685)) ;
#57257 = CARTESIAN_POINT('Ctrl Pts',(-17.8806923531252,-50.6613590448024,
123.484550765069)) ;
#57258 = CARTESIAN_POINT('Ctrl Pts',(-18.279598430072,-50.8613270682368,123.884440335655)) ;
#57259 = CARTESIAN_POINT('Ctrl Pts',(-17.99718458044,-50.6813379877563,124.002602226893)) ;
#57260 = CARTESIAN_POINT('Ctrl Pts',(-18.5086965529277,-50.8812588701058,
124.240917370752)) ;
#57261 = CARTESIAN_POINT('Ctrl Pts',(-18.283558724871,-50.7012697896254,124.448196582463)) ;
#57262 = CARTESIAN_POINT('Ctrl Pts',(-18.8431584214289,-50.9010831706034,
124.497674618011)) ;
#57263 = CARTESIAN_POINT('Ctrl Pts',(-18.7016353947099,-50.7210940901229,
124.769140330364)) ;
#57264 = CARTESIAN_POINT('Ctrl Pts',(-19.2506039421692,-50.9211791719433,
124.62581638792)) ;
#57265 = CARTESIAN_POINT('Ctrl Pts',(-19.2109425558623,-50.7411900914627,
124.929317666411)) ;
#57266 = CARTESIAN_POINT('Ctrl Pts',(-19.6705888408136,-50.9409375880472,
124.607973358778)) ;
#57267 = CARTESIAN_POINT('Ctrl Pts',(-19.7359254653455,-50.7609485075667,
124.907008256675)) ;
#57268 = CARTESIAN_POINT('Ctrl Pts',(-20.0654721859542,-50.9610312809313,
124.445475299511)) ;
#57269 = CARTESIAN_POINT('Ctrl Pts',(-20.2295077366867,-50.7810422004508,
124.703903011912)) ;
#57270 = CARTESIAN_POINT('Ctrl Pts',(-20.2716279154534,-50.9741422468379,
124.257625275152)) ;
#57271 = CARTESIAN_POINT('Ctrl Pts',(-20.4872438679816,-50.7941531663575,
124.469055541413)) ;
#57272 = CARTESIAN_POINT('Ctrl Pts',(-20.357892637621,-50.9808556216258,124.146615798218)) ;
#57273 = CARTESIAN_POINT('Ctrl Pts',(-20.5950497968806,-50.8008665411453,
124.330315451521)) ;
#57274 = CARTESIAN_POINT('',(-18.0898543520415,-12.1693713464509,124.125218065099)) ;
#57275 = CARTESIAN_POINT('',(-17.9274924084134,-12.1498929727495,123.644402320537)) ;
#57276 = CARTESIAN_POINT('Ctrl Pts',(-18.0898543518917,-12.1693713463351,
124.125218065234)) ;
#57277 = CARTESIAN_POINT('Ctrl Pts',(-18.1107251988235,-12.1855021497363,
124.106411345451)) ;
#57278 = CARTESIAN_POINT('Ctrl Pts',(-18.1304694810459,-12.2014740553584,
124.085663653832)) ;
#57279 = CARTESIAN_POINT('Ctrl Pts',(-18.1672576147845,-12.2331466325994,
124.038148222986)) ;
#57280 = CARTESIAN_POINT('Ctrl Pts',(-18.1843150887597,-12.2490832455646,
124.010368233214)) ;
#57281 = CARTESIAN_POINT('Ctrl Pts',(-18.2056877954049,-12.2722339064756,
123.958712601024)) ;
#57282 = CARTESIAN_POINT('Ctrl Pts',(-18.2123701677247,-12.2807335431958,
123.935854209123)) ;
#57283 = CARTESIAN_POINT('Ctrl Pts',(-18.2181185876305,-12.291774580405,123.895191373631)) ;
#57284 = CARTESIAN_POINT('Ctrl Pts',(-18.21884719455,-12.2953090478409,123.878001998223)) ;
#57285 = CARTESIAN_POINT('Ctrl Pts',(-18.2166942034222,-12.2989586422489,
123.849069156915)) ;
#57286 = CARTESIAN_POINT('Ctrl Pts',(-18.2149368250641,-12.2998030471561,
123.837528420933)) ;
#57287 = CARTESIAN_POINT('Ctrl Pts',(-18.2110620214478,-12.3000404731419,
123.821269100306)) ;
#57288 = CARTESIAN_POINT('Ctrl Pts',(-18.2097329849641,-12.2999877851218,
123.816451295881)) ;
#57289 = CARTESIAN_POINT('Ctrl Pts',(-18.207972662911,-12.2997790216126,123.810859304896)) ;
#57290 = CARTESIAN_POINT('Ctrl Pts',(-18.2077076065518,-12.2997444373638,
123.810035197199)) ;
#57291 = CARTESIAN_POINT('Ctrl Pts',(-18.2074255071376,-12.299704400868,123.809176454917)) ;
#57292 = CARTESIAN_POINT('Ctrl Pts',(-18.2074135269255,-12.2997026946395,
123.809140019673)) ;
#57293 = CARTESIAN_POINT('Ctrl Pts',(-18.2073953439793,-12.2997000959883,
123.809084771462)) ;
#57294 = CARTESIAN_POINT('Ctrl Pts',(-18.207389148473,-12.2996992089591,123.809065955664)) ;
#57295 = CARTESIAN_POINT('Ctrl Pts',(-18.2073762490693,-12.2996973588126,
123.809026798846)) ;
#57296 = CARTESIAN_POINT('Ctrl Pts',(-18.2073695447124,-12.2996963953616,
123.809006457953)) ;
#57297 = CARTESIAN_POINT('Ctrl Pts',(-18.2073595638262,-12.2996949583005,
123.808976191801)) ;
#57298 = CARTESIAN_POINT('Ctrl Pts',(-18.2073562896495,-12.2996944864394,
123.808966265658)) ;
#57299 = CARTESIAN_POINT('Ctrl Pts',(-18.207350487964,-12.299693649543,123.808948681443)) ;
#57300 = CARTESIAN_POINT('Ctrl Pts',(-18.2073479607712,-12.2996932847316,
123.808941023316)) ;
#57301 = CARTESIAN_POINT('Ctrl Pts',(-18.2073426945459,-12.2996925239825,
123.808925068233)) ;
#57302 = CARTESIAN_POINT('Ctrl Pts',(-18.2073399554604,-12.2996921279915,
123.808916771376)) ;
#57303 = CARTESIAN_POINT('Ctrl Pts',(-18.2073328524603,-12.299691100309,123.808895260494)) ;
#57304 = CARTESIAN_POINT('Ctrl Pts',(-18.2073284877422,-12.2996904680284,
123.808882046723)) ;
#57305 = CARTESIAN_POINT('Ctrl Pts',(-18.2073102435383,-12.2996878218805,
123.808826832669)) ;
#57306 = CARTESIAN_POINT('Ctrl Pts',(-18.2072963521413,-12.299685799183,123.808784836724)) ;
#57307 = CARTESIAN_POINT('Ctrl Pts',(-18.2067002687993,-12.2995986671134,
123.806984700008)) ;
#57308 = CARTESIAN_POINT('Ctrl Pts',(-18.2060950417741,-12.2994964054139,
123.805235382609)) ;
#57309 = CARTESIAN_POINT('Ctrl Pts',(-18.2029100719787,-12.2988910495203,
123.796412826518)) ;
#57310 = CARTESIAN_POINT('Ctrl Pts',(-18.1999823466222,-12.2981229845307,
123.789508567045)) ;
#57311 = CARTESIAN_POINT('Ctrl Pts',(-18.1907776852835,-12.2952052971042,
123.770713859956)) ;
#57312 = CARTESIAN_POINT('Ctrl Pts',(-18.1837783560155,-12.2924682785729,
123.759423255741)) ;
#57313 = CARTESIAN_POINT('Ctrl Pts',(-18.1647286466641,-12.2841136491298,
123.734251409911)) ;
#57314 = CARTESIAN_POINT('Ctrl Pts',(-18.1519831900975,-12.27787160617,123.721427746504)) ;
#57315 = CARTESIAN_POINT('Ctrl Pts',(-18.1183690064087,-12.2604608869746,
123.694387616855)) ;
#57316 = CARTESIAN_POINT('Ctrl Pts',(-18.0964700298874,-12.2483832091272,
123.682080321854)) ;
#57317 = CARTESIAN_POINT('Ctrl Pts',(-18.031885753796,-12.2118235042901,123.655137433837)) ;
#57318 = CARTESIAN_POINT('Ctrl Pts',(-17.9824298926407,-12.1827151160779,
123.645606479208)) ;
#57319 = CARTESIAN_POINT('Ctrl Pts',(-17.9274924082143,-12.1498929726306,
123.644402320532)) ;
#57320 = CARTESIAN_POINT('',(-20.5746457983858,-12.,122.467488525849)) ;
#57321 = CARTESIAN_POINT('Ctrl Pts',(-20.5746457983858,-12.,122.467488525849)) ;
#57322 = CARTESIAN_POINT('Ctrl Pts',(-20.5627382419342,-12.0007217907825,
122.452815451161)) ;
#57323 = CARTESIAN_POINT('Ctrl Pts',(-20.4947798807797,-12.0047464667125,
122.372266602231)) ;
#57324 = CARTESIAN_POINT('Ctrl Pts',(-20.3539293395536,-12.0121810504321,
122.236896566325)) ;
#57325 = CARTESIAN_POINT('Ctrl Pts',(-20.1370409747147,-12.0221110972068,
122.091764368012)) ;
#57326 = CARTESIAN_POINT('Ctrl Pts',(-19.8980237231667,-12.0320625395439,
121.985643564698)) ;
#57327 = CARTESIAN_POINT('Ctrl Pts',(-19.6416983085707,-12.0421093367232,
121.922384338977)) ;
#57328 = CARTESIAN_POINT('Ctrl Pts',(-19.3835093232675,-12.0519572774033,
121.904703348343)) ;
#57329 = CARTESIAN_POINT('Ctrl Pts',(-19.1231275997313,-12.0619189087459,
121.931627958287)) ;
#57330 = CARTESIAN_POINT('Ctrl Pts',(-18.8697470442625,-12.0719475681218,
122.004163670847)) ;
#57331 = CARTESIAN_POINT('Ctrl Pts',(-18.6355935850335,-12.08185787101,122.118142693142)) ;
#57332 = CARTESIAN_POINT('Ctrl Pts',(-18.4238474019827,-12.0917927655722,
122.270883953054)) ;
#57333 = CARTESIAN_POINT('Ctrl Pts',(-18.2400799717895,-12.1018338642391,
122.460231143199)) ;
#57334 = CARTESIAN_POINT('Ctrl Pts',(-18.0940875093298,-12.1117211467435,
122.675182672206)) ;
#57335 = CARTESIAN_POINT('Ctrl Pts',(-17.9861176823212,-12.121712887254,122.914511116819)) ;
#57336 = CARTESIAN_POINT('Ctrl Pts',(-17.921689729601,-12.1316634364894,123.16795292873)) ;
#57337 = CARTESIAN_POINT('Ctrl Pts',(-17.9030108427875,-12.1410363173938,
123.413537993095)) ;
#57338 = CARTESIAN_POINT('Ctrl Pts',(-17.9162454187765,-12.1471236046148,
123.57278095633)) ;
#57339 = CARTESIAN_POINT('Ctrl Pts',(-17.9274924084134,-12.1498929727495,
123.644402320537)) ;
#57340 = CARTESIAN_POINT('',(-20.6888487350626,-11.9999999997025,122.656717008064)) ;
#57341 = CARTESIAN_POINT('Ctrl Pts',(-20.5746457983858,-12.,122.467488525849)) ;
#57342 = CARTESIAN_POINT('Ctrl Pts',(-20.5960286970766,-12.,122.497557942705)) ;
#57343 = CARTESIAN_POINT('Ctrl Pts',(-20.6162418843401,-12.0000000000049,
122.528364603676)) ;
#57344 = CARTESIAN_POINT('Ctrl Pts',(-20.6543685264773,-12.0000000000049,
122.591550197525)) ;
#57345 = CARTESIAN_POINT('Ctrl Pts',(-20.6722191984465,-12.,122.62383024764)) ;
#57346 = CARTESIAN_POINT('Ctrl Pts',(-20.6888487341057,-12.,122.656717008548)) ;
#57347 = CARTESIAN_POINT('Ctrl Pts',(-20.6888487348625,-11.9999999994367,
122.656717007968)) ;
#57348 = CARTESIAN_POINT('Ctrl Pts',(-20.6504013293531,-12.0242010028557,
122.669878337729)) ;
#57349 = CARTESIAN_POINT('Ctrl Pts',(-20.6126735676598,-12.0487776575878,
122.685887455227)) ;
#57350 = CARTESIAN_POINT('Ctrl Pts',(-20.5429100063498,-12.0961255449868,
122.722350893296)) ;
#57351 = CARTESIAN_POINT('Ctrl Pts',(-20.5100459148922,-12.1193501392808,
122.742829239747)) ;
#57352 = CARTESIAN_POINT('Ctrl Pts',(-20.4795958757324,-12.1420202642929,
122.766130796517)) ;
#57353 = CARTESIAN_POINT('Ctrl Pts',(-18.0898543520415,-12.1693713464509,
124.125218065099)) ;
#57354 = CARTESIAN_POINT('Ctrl Pts',(-18.0987410756712,-12.1700845612802,
124.141640469505)) ;
#57355 = CARTESIAN_POINT('Ctrl Pts',(-18.1505706173883,-12.174105036101,124.233279228286)) ;
#57356 = CARTESIAN_POINT('Ctrl Pts',(-18.263117466536,-12.1814863726884,124.391272663474)) ;
#57357 = CARTESIAN_POINT('Ctrl Pts',(-18.4514152853576,-12.1915186409522,
124.575779592005)) ;
#57358 = CARTESIAN_POINT('Ctrl Pts',(-18.6649582254988,-12.2013826029581,
124.722768521293)) ;
#57359 = CARTESIAN_POINT('Ctrl Pts',(-18.9056381213548,-12.211452664303,124.832713751572)) ;
#57360 = CARTESIAN_POINT('Ctrl Pts',(-19.1560012005742,-12.2212950286517,
124.897694900574)) ;
#57361 = CARTESIAN_POINT('Ctrl Pts',(-19.4168488001017,-12.2312557011542,
124.919426126704)) ;
#57362 = CARTESIAN_POINT('Ctrl Pts',(-19.6794781670334,-12.241293772222,124.894826056415)) ;
#57363 = CARTESIAN_POINT('Ctrl Pts',(-19.9298584470305,-12.2511673871824,
124.826609084731)) ;
#57364 = CARTESIAN_POINT('Ctrl Pts',(-20.1692027685541,-12.2612396217637,
124.713703674863)) ;
#57365 = CARTESIAN_POINT('Ctrl Pts',(-20.3802336084559,-12.2710636402125,
124.56490174156)) ;
#57366 = CARTESIAN_POINT('Ctrl Pts',(-20.5668505339034,-12.2811285611885,
124.3775468474)) ;
#57367 = CARTESIAN_POINT('Ctrl Pts',(-20.7654710388387,-12.2943388594833,
124.092731380698)) ;
#57368 = CARTESIAN_POINT('Ctrl Pts',(-20.8864681734945,-12.3076543062152,
123.760293059331)) ;
#57369 = CARTESIAN_POINT('Ctrl Pts',(-20.9168412402485,-12.3209445514825,
123.412248798329)) ;
#57370 = CARTESIAN_POINT('Ctrl Pts',(-20.8936136564304,-12.3309953010896,
123.149204261583)) ;
#57371 = CARTESIAN_POINT('Ctrl Pts',(-20.8271599100472,-12.3408079080718,
122.900008574106)) ;
#57372 = CARTESIAN_POINT('Ctrl Pts',(-20.7159339872492,-12.3508790060661,
122.659895486434)) ;
#57373 = CARTESIAN_POINT('Ctrl Pts',(-20.5671825471141,-12.360768578841,122.446765213332)) ;
#57374 = CARTESIAN_POINT('Ctrl Pts',(-20.3217335957846,-12.3740386856443,
122.199036770175)) ;
#57375 = CARTESIAN_POINT('Ctrl Pts',(-19.9402799223287,-12.3906553725668,
121.976489963183)) ;
#57376 = CARTESIAN_POINT('Ctrl Pts',(-19.5069560654083,-12.407229415883,121.897341845887)) ;
#57377 = CARTESIAN_POINT('Ctrl Pts',(-19.1586250796142,-12.4205259833148,
121.925240968701)) ;
#57378 = CARTESIAN_POINT('Ctrl Pts',(-18.9035497915594,-12.4305560468922,
121.991664800906)) ;
#57379 = CARTESIAN_POINT('Ctrl Pts',(-18.6671468529052,-12.4404499387415,
122.099840645972)) ;
#57380 = CARTESIAN_POINT('Ctrl Pts',(-18.3796682061191,-12.453702694527,122.296549637466)) ;
#57381 = CARTESIAN_POINT('Ctrl Pts',(-18.0908280313655,-12.4704307995195,
122.634462100718)) ;
#57382 = CARTESIAN_POINT('Ctrl Pts',(-17.9056069777788,-12.4902616359979,
123.128014485523)) ;
#57383 = CARTESIAN_POINT('Ctrl Pts',(-17.8986058474029,-12.5101870278881,
123.65743523967)) ;
#57384 = CARTESIAN_POINT('Ctrl Pts',(-18.0728134812496,-12.5301122412401,
124.157630024429)) ;
#57385 = CARTESIAN_POINT('Ctrl Pts',(-18.4070561283902,-12.5500372547252,
124.568319257347)) ;
#57386 = CARTESIAN_POINT('Ctrl Pts',(-18.8599799731256,-12.5699137264252,
124.840308096966)) ;
#57387 = CARTESIAN_POINT('Ctrl Pts',(-19.3811313633293,-12.5898930443341,
124.942158139695)) ;
#57388 = CARTESIAN_POINT('Ctrl Pts',(-19.9045262603243,-12.6098260479101,
124.859844414469)) ;
#57389 = CARTESIAN_POINT('Ctrl Pts',(-20.3677432424192,-12.6297213179378,
124.6048789893)) ;
#57390 = CARTESIAN_POINT('Ctrl Pts',(-20.7170498595964,-12.6496426558436,
124.206944794287)) ;
#57391 = CARTESIAN_POINT('Ctrl Pts',(-20.9098403565593,-12.6696002791098,
123.712751204342)) ;
#57392 = CARTESIAN_POINT('Ctrl Pts',(-20.922485985003,-12.689480111067,123.18461209717)) ;
#57393 = CARTESIAN_POINT('Ctrl Pts',(-20.7554545445051,-12.7093619623639,
122.683172172836)) ;
#57394 = CARTESIAN_POINT('Ctrl Pts',(-20.4235254244291,-12.7294329794677,
122.265649141046)) ;
#57395 = CARTESIAN_POINT('Ctrl Pts',(-19.9749237655201,-12.7492402032208,
121.989968961482)) ;
#57396 = CARTESIAN_POINT('Ctrl Pts',(-19.4550399386783,-12.7692213387896,
121.881799009553)) ;
#57397 = CARTESIAN_POINT('Ctrl Pts',(-18.9310095255677,-12.7891488321288,
121.958350587305)) ;
#57398 = CARTESIAN_POINT('Ctrl Pts',(-18.4660378435683,-12.8089694934866,
122.206286369213)) ;
#57399 = CARTESIAN_POINT('Ctrl Pts',(-18.1095237058469,-12.8290666827084,
122.603786127405)) ;
#57400 = CARTESIAN_POINT('Ctrl Pts',(-17.9128685242105,-12.8488303617167,
123.091145395877)) ;
#57401 = CARTESIAN_POINT('Ctrl Pts',(-17.8934532250119,-12.8688876403898,
123.623648070234)) ;
#57402 = CARTESIAN_POINT('Ctrl Pts',(-18.0551868058747,-12.8886830641372,
124.124451004221)) ;
#57403 = CARTESIAN_POINT('Ctrl Pts',(-18.3794288064129,-12.9086467088648,
124.544379679826)) ;
#57404 = CARTESIAN_POINT('Ctrl Pts',(-18.8287006511552,-12.9286302001389,
124.827680379695)) ;
#57405 = CARTESIAN_POINT('Ctrl Pts',(-19.3429186866301,-12.9484376952882,
124.94073161998)) ;
#57406 = CARTESIAN_POINT('Ctrl Pts',(-19.8693844497185,-12.9684202860083,
124.871533418394)) ;
#57407 = CARTESIAN_POINT('Ctrl Pts',(-20.3384447754671,-12.9883029399996,
124.627871581349)) ;
#57408 = CARTESIAN_POINT('Ctrl Pts',(-20.6976976848122,-13.0082611848626,
124.237731507644)) ;
#57409 = CARTESIAN_POINT('Ctrl Pts',(-20.9017768869257,-13.0281367719042,
123.750397269444)) ;
#57410 = CARTESIAN_POINT('Ctrl Pts',(-20.9278087943981,-13.0481176600395,
123.220011471926)) ;
#57411 = CARTESIAN_POINT('Ctrl Pts',(-20.7712144053819,-13.0680528011505,
122.713763278227)) ;
#57412 = CARTESIAN_POINT('Ctrl Pts',(-20.4520106816014,-13.0879648191615,
122.291696114272)) ;
#57413 = CARTESIAN_POINT('Ctrl Pts',(-20.0087285877316,-13.1078530374051,
122.003722192709)) ;
#57414 = CARTESIAN_POINT('Ctrl Pts',(-19.5791090604564,-13.124451341252,121.903703056221)) ;
#57415 = CARTESIAN_POINT('Ctrl Pts',(-19.2304680801455,-13.1377239311549,
121.914976366624)) ;
#57416 = CARTESIAN_POINT('Ctrl Pts',(-18.9730360739326,-13.1477313461057,
121.968723010403)) ;
#57417 = CARTESIAN_POINT('Ctrl Pts',(-18.7289237747832,-13.1577386928383,
122.066570256317)) ;
#57418 = CARTESIAN_POINT('Ctrl Pts',(-18.4326373531694,-13.1710050526399,
122.250316913842)) ;
#57419 = CARTESIAN_POINT('Ctrl Pts',(-18.1316373287835,-13.1875197102629,
122.569692622284)) ;
#57420 = CARTESIAN_POINT('Ctrl Pts',(-17.9558681007045,-13.2041171435055,
122.974265631492)) ;
#57421 = CARTESIAN_POINT('Ctrl Pts',(-17.9045373896821,-13.2174651406505,
123.321302564893)) ;
#57422 = CARTESIAN_POINT('Ctrl Pts',(-17.9113737957956,-13.2273608950021,
123.581262925382)) ;
#57423 = CARTESIAN_POINT('Ctrl Pts',(-17.9634088821012,-13.2373488489335,
123.838506352538)) ;
#57424 = CARTESIAN_POINT('Ctrl Pts',(-18.0589349739685,-13.2473060726382,
124.082144873651)) ;
#57425 = CARTESIAN_POINT('Ctrl Pts',(-18.1964661586106,-13.2573416191949,
124.307146372465)) ;
#57426 = CARTESIAN_POINT('Ctrl Pts',(-18.3682700533626,-13.267228730471,124.502082982706)) ;
#57427 = CARTESIAN_POINT('Ctrl Pts',(-18.573168600081,-13.2772201355718,124.666246335832)) ;
#57428 = CARTESIAN_POINT('Ctrl Pts',(-18.8024527486924,-13.2871657567866,
124.791696662128)) ;
#57429 = CARTESIAN_POINT('Ctrl Pts',(-19.0499707909463,-13.2971150050549,
124.87596822317)) ;
#57430 = CARTESIAN_POINT('Ctrl Pts',(-19.3109074952385,-13.3071615002235,
124.91606420447)) ;
#57431 = CARTESIAN_POINT('Ctrl Pts',(-19.5697458477253,-13.3170128430151,
124.910614060128)) ;
#57432 = CARTESIAN_POINT('Ctrl Pts',(-19.8268961278364,-13.3269846231424,
124.86034740168)) ;
#57433 = CARTESIAN_POINT('Ctrl Pts',(-20.0720441858723,-13.3369798231201,
124.765921346646)) ;
#57434 = CARTESIAN_POINT('Ctrl Pts',(-20.2977248332106,-13.3470138148161,
124.629595035348)) ;
#57435 = CARTESIAN_POINT('Ctrl Pts',(-20.4930785404264,-13.3568692197887,
124.459519571124)) ;
#57436 = CARTESIAN_POINT('Ctrl Pts',(-20.6585461151986,-13.3668685176344,
124.255447402342)) ;
#57437 = CARTESIAN_POINT('Ctrl Pts',(-20.7850259763668,-13.3767636302396,
124.028196369691)) ;
#57438 = CARTESIAN_POINT('Ctrl Pts',(-20.8714967332555,-13.3868242757746,
123.778389961119)) ;
#57439 = CARTESIAN_POINT('Ctrl Pts',(-20.9125557494614,-13.3966731527638,
123.522828864941)) ;
#57440 = CARTESIAN_POINT('Ctrl Pts',(-20.9092102411542,-13.4067018638574,
123.259309807964)) ;
#57441 = CARTESIAN_POINT('Ctrl Pts',(-20.8594509750379,-13.4167312651135,
123.00048234628)) ;
#57442 = CARTESIAN_POINT('Ctrl Pts',(-20.7678172835609,-13.4265714569095,
122.758667592175)) ;
#57443 = CARTESIAN_POINT('Ctrl Pts',(-20.6338292437046,-13.4365748861025,
122.532528063033)) ;
#57444 = CARTESIAN_POINT('Ctrl Pts',(-20.4628072717642,-13.4465603985687,
122.333446821148)) ;
#57445 = CARTESIAN_POINT('Ctrl Pts',(-20.258572195235,-13.4566014949527,122.16640991458)) ;
#57446 = CARTESIAN_POINT('Ctrl Pts',(-20.0331061121126,-13.4664446909037,
122.03957718795)) ;
#57447 = CARTESIAN_POINT('Ctrl Pts',(-19.7857320971473,-13.4764310019581,
121.952101012445)) ;
#57448 = CARTESIAN_POINT('Ctrl Pts',(-19.5282010411868,-13.4863656872158,
121.908939847016)) ;
#57449 = CARTESIAN_POINT('Ctrl Pts',(-19.2639488168614,-13.4964232484328,
121.911409438826)) ;
#57450 = CARTESIAN_POINT('Ctrl Pts',(-19.0100966675528,-13.5062448900415,
121.958214888149)) ;
#57451 = CARTESIAN_POINT('Ctrl Pts',(-18.7623301682284,-13.5163009536324,
122.050058119956)) ;
#57452 = CARTESIAN_POINT('Ctrl Pts',(-18.5371012425962,-13.5262416293942,
122.182417857288)) ;
#57453 = CARTESIAN_POINT('Ctrl Pts',(-18.338478245611,-13.5361459881825,122.350628473911)) ;
#57454 = CARTESIAN_POINT('Ctrl Pts',(-18.1698329826385,-13.5461926427584,
122.553733855565)) ;
#57455 = CARTESIAN_POINT('Ctrl Pts',(-18.0407519036657,-13.5560882374012,
122.779526388176)) ;
#57456 = CARTESIAN_POINT('Ctrl Pts',(-17.9513576421501,-13.5661501840581,
123.028342279855)) ;
#57457 = CARTESIAN_POINT('Ctrl Pts',(-17.9074152113575,-13.5759998079902,
123.283436990171)) ;
#57458 = CARTESIAN_POINT('Ctrl Pts',(-17.9075794490051,-13.5859630470201,
123.545245160118)) ;
#57459 = CARTESIAN_POINT('Ctrl Pts',(-17.9538438452054,-13.5959876217959,
123.804601716854)) ;
#57460 = CARTESIAN_POINT('Ctrl Pts',(-18.0433151854202,-13.6059061844836,
124.0494068293)) ;
#57461 = CARTESIAN_POINT('Ctrl Pts',(-18.1745142883211,-13.6158983712076,
124.276882942804)) ;
#57462 = CARTESIAN_POINT('Ctrl Pts',(-18.3442843563806,-13.6259331697918,
124.478655912716)) ;
#57463 = CARTESIAN_POINT('Ctrl Pts',(-18.5426287178469,-13.6357883604655,
124.645217964009)) ;
#57464 = CARTESIAN_POINT('Ctrl Pts',(-18.7699291705974,-13.6457877086185,
124.776978497853)) ;
#57465 = CARTESIAN_POINT('Ctrl Pts',(-19.0140681533579,-13.6556828342936,
124.86662328346)) ;
#57466 = CARTESIAN_POINT('Ctrl Pts',(-19.2742712713222,-13.6657433772417,
124.913241817981)) ;
#57467 = CARTESIAN_POINT('Ctrl Pts',(-19.5331191647968,-13.6755926515086,
124.914103544901)) ;
#57468 = CARTESIAN_POINT('Ctrl Pts',(-19.792878148494,-13.6856198760785,124.869872597639)) ;
#57469 = CARTESIAN_POINT('Ctrl Pts',(-20.0408282968694,-13.6956482752663,
124.780544744153)) ;
#57470 = CARTESIAN_POINT('Ctrl Pts',(-20.2655486146661,-13.7054940256798,
124.652339842706)) ;
#57471 = CARTESIAN_POINT('Ctrl Pts',(-20.4679785318478,-13.7154828160805,
124.485209945321)) ;
#57472 = CARTESIAN_POINT('Ctrl Pts',(-20.638747035496,-13.7255277444802,124.283933112254)) ;
#57473 = CARTESIAN_POINT('Ctrl Pts',(-20.7695822850911,-13.7353522292692,
124.061344007578)) ;
#57474 = CARTESIAN_POINT('Ctrl Pts',(-20.8622650301573,-13.7454096268104,
123.813853115559)) ;
#57475 = CARTESIAN_POINT('Ctrl Pts',(-20.9096073544687,-13.7553357183966,
123.557318498504)) ;
#57476 = CARTESIAN_POINT('Ctrl Pts',(-20.9123708210729,-13.7652905035412,
123.295734355723)) ;
#57477 = CARTESIAN_POINT('Ctrl Pts',(-20.8690285856397,-13.7753278731988,
123.035549479101)) ;
#57478 = CARTESIAN_POINT('Ctrl Pts',(-20.7826546061871,-13.7852166833204,
122.790448432935)) ;
#57479 = CARTESIAN_POINT('Ctrl Pts',(-20.6541544832906,-13.7952060423715,
122.561546360115)) ;
#57480 = CARTESIAN_POINT('Ctrl Pts',(-20.4882245281512,-13.8051645898276,
122.359184924028)) ;
#57481 = CARTESIAN_POINT('Ctrl Pts',(-20.2912542115885,-13.8150641663786,
122.189215690163)) ;
#57482 = CARTESIAN_POINT('Ctrl Pts',(-20.0644048944981,-13.8251120782093,
122.054135819925)) ;
#57483 = CARTESIAN_POINT('Ctrl Pts',(-19.8213040212289,-13.8350074260699,
121.961702812424)) ;
#57484 = CARTESIAN_POINT('Ctrl Pts',(-19.5616299165928,-13.8450691026011,
121.912040392459)) ;
#57485 = CARTESIAN_POINT('Ctrl Pts',(-19.302943765994,-13.8549136203502,121.908260248801)) ;
#57486 = CARTESIAN_POINT('Ctrl Pts',(-19.0443926106772,-13.864874064065,121.949016797608)) ;
#57487 = CARTESIAN_POINT('Ctrl Pts',(-18.7951065533296,-13.8749108968832,
122.035163624274)) ;
#57488 = CARTESIAN_POINT('Ctrl Pts',(-18.5679607592808,-13.88478969363,122.160911880469)) ;
#57489 = CARTESIAN_POINT('Ctrl Pts',(-18.3623992980865,-13.8948490097584,
122.327074678705)) ;
#57490 = CARTESIAN_POINT('Ctrl Pts',(-18.1920392191495,-13.9047194565116,
122.522692233472)) ;
#57491 = CARTESIAN_POINT('Ctrl Pts',(-18.0559754687445,-13.9147120947696,
122.747289602296)) ;
#57492 = CARTESIAN_POINT('Ctrl Pts',(-17.9611352243635,-13.9247441103175,
122.993260746216)) ;
#57493 = CARTESIAN_POINT('Ctrl Pts',(-17.9107237978205,-13.9346099666241,
123.247603809028)) ;
#57494 = CARTESIAN_POINT('Ctrl Pts',(-17.9051038745564,-13.9446792560932,
123.512124786768)) ;
#57495 = CARTESIAN_POINT('Ctrl Pts',(-17.9445700338335,-13.9545228136446,
123.767790796992)) ;
#57496 = CARTESIAN_POINT('Ctrl Pts',(-18.0281629110103,-13.9645029404324,
124.016370584098)) ;
#57497 = CARTESIAN_POINT('Ctrl Pts',(-18.1545752563571,-13.9745214890323,
124.247305606012)) ;
#57498 = CARTESIAN_POINT('Ctrl Pts',(-18.3165363213439,-13.9844047895555,
124.450385027953)) ;
#57499 = CARTESIAN_POINT('Ctrl Pts',(-18.4859844039085,-13.9930026771457,
124.599786853217)) ;
#57500 = CARTESIAN_POINT('Ctrl Pts',(-18.5982098542005,-13.9981476377442,
124.674581361741)) ;
#57501 = CARTESIAN_POINT('Ctrl Pts',(-18.6398461652381,-13.9999999999504,
124.699448408814)) ;
#57502 = CARTESIAN_POINT('Ctrl Pts',(-17.9901976317162,-10.,123.897592500161)) ;
#57503 = CARTESIAN_POINT('Ctrl Pts',(-18.2740109056134,-9.82001091963712,
123.800437437226)) ;
#57504 = CARTESIAN_POINT('Ctrl Pts',(-18.0463587734884,-10.0066268508181,
124.061733136808)) ;
#57505 = CARTESIAN_POINT('Ctrl Pts',(-18.318952820002,-9.82663777045524,123.931772257896)) ;
#57506 = CARTESIAN_POINT('Ctrl Pts',(-18.2158202083151,-10.0198574772991,
124.369865791197)) ;
#57507 = CARTESIAN_POINT('Ctrl Pts',(-18.4544999964107,-9.83986839693625,
124.178242269465)) ;
#57508 = CARTESIAN_POINT('Ctrl Pts',(-18.6148367045085,-10.0398330985578,
124.72010058675)) ;
#57509 = CARTESIAN_POINT('Ctrl Pts',(-18.7737259547846,-9.85984401819488,
124.458448709452)) ;
#57510 = CARTESIAN_POINT('Ctrl Pts',(-19.1081207670208,-10.0597504334597,
124.912141899864)) ;
#57511 = CARTESIAN_POINT('Ctrl Pts',(-19.1683517739458,-9.87976135309682,
124.612076728176)) ;
#57512 = CARTESIAN_POINT('Ctrl Pts',(-19.636206114934,-10.0796237101757,124.92549851548)) ;
#57513 = CARTESIAN_POINT('Ctrl Pts',(-19.5908222086086,-9.89963462981282,
124.622761886445)) ;
#57514 = CARTESIAN_POINT('Ctrl Pts',(-20.1407529320189,-10.0996482003397,
124.756244590335)) ;
#57515 = CARTESIAN_POINT('Ctrl Pts',(-19.994458721673,-9.91965911997678,124.487357109044)) ;
#57516 = CARTESIAN_POINT('Ctrl Pts',(-20.5540202995955,-10.1195160414904,
124.427406225433)) ;
#57517 = CARTESIAN_POINT('Ctrl Pts',(-20.3250727353524,-9.9395269611275,124.224284451464)) ;
#57518 = CARTESIAN_POINT('Ctrl Pts',(-20.8319818407582,-10.1394616923699,
123.976064807431)) ;
#57519 = CARTESIAN_POINT('Ctrl Pts',(-20.547440485577,-9.95947261200706,123.863209762279)) ;
#57520 = CARTESIAN_POINT('Ctrl Pts',(-20.9388342400949,-10.1593670929869,
123.457915382835)) ;
#57521 = CARTESIAN_POINT('Ctrl Pts',(-20.6329204948871,-9.97937801262402,
123.448688955287)) ;
#57522 = CARTESIAN_POINT('Ctrl Pts',(-20.8636098402301,-10.1792413208033,
122.935072644727)) ;
#57523 = CARTESIAN_POINT('Ctrl Pts',(-20.5727382379585,-9.99925224044038,
123.03041411648)) ;
#57524 = CARTESIAN_POINT('Ctrl Pts',(-20.6131115834081,-10.1992271116809,
122.466642059227)) ;
#57525 = CARTESIAN_POINT('Ctrl Pts',(-20.3723371633396,-10.019238031318,122.655670872381)) ;
#57526 = CARTESIAN_POINT('Ctrl Pts',(-20.219446657189,-10.2191213543406,122.11369274935)) ;
#57527 = CARTESIAN_POINT('Ctrl Pts',(-20.0574027588299,-10.0391322739778,
122.373312971228)) ;
#57528 = CARTESIAN_POINT('Ctrl Pts',(-19.729780773993,-10.2390000704127,121.915093775378)) ;
#57529 = CARTESIAN_POINT('Ctrl Pts',(-19.6656681100072,-10.0590109900498,
122.21443654672)) ;
#57530 = CARTESIAN_POINT('Ctrl Pts',(-19.1975679684769,-10.2590395202573,
121.895998337816)) ;
#57531 = CARTESIAN_POINT('Ctrl Pts',(-19.2398980466007,-10.0790504398944,
122.199163431724)) ;
#57532 = CARTESIAN_POINT('Ctrl Pts',(-18.6950312339923,-10.2789026817952,
122.058270950238)) ;
#57533 = CARTESIAN_POINT('Ctrl Pts',(-18.837868920824,-10.0989136014323,122.328984924085)) ;
#57534 = CARTESIAN_POINT('Ctrl Pts',(-18.2756669291778,-10.2988820498094,
122.383749835563)) ;
#57535 = CARTESIAN_POINT('Ctrl Pts',(-18.5023795133954,-10.1188929694465,
122.589370885141)) ;
#57536 = CARTESIAN_POINT('Ctrl Pts',(-17.9943038605785,-10.3186926303322,
122.828930487561)) ;
#57537 = CARTESIAN_POINT('Ctrl Pts',(-18.2772917344201,-10.1387035499693,
122.945518187819)) ;
#57538 = CARTESIAN_POINT('Ctrl Pts',(-17.8800540061898,-10.3386735586178,
123.347451469643)) ;
#57539 = CARTESIAN_POINT('Ctrl Pts',(-18.1858955346146,-10.1586844782549,
123.360335798021)) ;
#57540 = CARTESIAN_POINT('Ctrl Pts',(-17.949663613675,-10.3585662304872,123.871624239523)) ;
#57541 = CARTESIAN_POINT('Ctrl Pts',(-18.2415877728661,-10.1785771501243,
123.779674103343)) ;
#57542 = CARTESIAN_POINT('Ctrl Pts',(-18.1935384904851,-10.3784925607743,
124.34174209524)) ;
#57543 = CARTESIAN_POINT('Ctrl Pts',(-18.4366892418074,-10.1985034804115,
124.155765909524)) ;
#57544 = CARTESIAN_POINT('Ctrl Pts',(-18.5843830566034,-10.3984631148666,
124.700856014279)) ;
#57545 = CARTESIAN_POINT('Ctrl Pts',(-18.7493759717748,-10.2184740345037,
124.44305681766)) ;
#57546 = CARTESIAN_POINT('Ctrl Pts',(-18.9897866675992,-10.4149949539542,
124.870306748339)) ;
#57547 = CARTESIAN_POINT('Ctrl Pts',(-19.0736749228579,-10.2350058735914,
124.578605598989)) ;
#57548 = CARTESIAN_POINT('Ctrl Pts',(-19.3371420473607,-10.4283346927818,
124.917711789777)) ;
#57549 = CARTESIAN_POINT('Ctrl Pts',(-19.3515822796175,-10.2483456124189,
124.6165344309)) ;
#57550 = CARTESIAN_POINT('Ctrl Pts',(-19.6005562667331,-10.4383669350004,
124.907063768782)) ;
#57551 = CARTESIAN_POINT('Ctrl Pts',(-19.5623087731277,-10.2583778546375,
124.608012505296)) ;
#57552 = CARTESIAN_POINT('Ctrl Pts',(-19.8537397870735,-10.4482246356439,
124.852203726746)) ;
#57553 = CARTESIAN_POINT('Ctrl Pts',(-19.7648571225557,-10.268235555281,124.564122220758)) ;
#57554 = CARTESIAN_POINT('Ctrl Pts',(-20.0969735539785,-10.4582165002831,
124.753332920083)) ;
#57555 = CARTESIAN_POINT('Ctrl Pts',(-19.9594412734619,-10.2782274199202,
124.485025314983)) ;
#57556 = CARTESIAN_POINT('Ctrl Pts',(-20.3177787346395,-10.4681390500432,
124.614652183365)) ;
#57557 = CARTESIAN_POINT('Ctrl Pts',(-20.1360907041886,-10.2881499696804,
124.374071880139)) ;
#57558 = CARTESIAN_POINT('Ctrl Pts',(-20.5771970981362,-10.4814168235367,
124.381203458891)) ;
#57559 = CARTESIAN_POINT('Ctrl Pts',(-20.3435922192053,-10.3014277431738,
124.18734533642)) ;
#57560 = CARTESIAN_POINT('Ctrl Pts',(-20.7701003708174,-10.4947641624773,
124.083584310457)) ;
#57561 = CARTESIAN_POINT('Ctrl Pts',(-20.4979358992389,-10.3147750821144,
123.949230612993)) ;
#57562 = CARTESIAN_POINT('Ctrl Pts',(-20.8774553693723,-10.5079713942705,
123.753475217054)) ;
#57563 = CARTESIAN_POINT('Ctrl Pts',(-20.5838202404129,-10.3279823139076,
123.685128879657)) ;
#57564 = CARTESIAN_POINT('Ctrl Pts',(-20.9145282391216,-10.5179585103602,
123.493699384276)) ;
#57565 = CARTESIAN_POINT('Ctrl Pts',(-20.6134756829108,-10.3379694299973,
123.477310647391)) ;
#57566 = CARTESIAN_POINT('Ctrl Pts',(-20.9061303769722,-10.52790941594,123.232285620267)) ;
#57567 = CARTESIAN_POINT('Ctrl Pts',(-20.6067552793287,-10.3479203355771,
123.268178977505)) ;
#57568 = CARTESIAN_POINT('Ctrl Pts',(-20.8516285272166,-10.5379645179474,
122.973767430347)) ;
#57569 = CARTESIAN_POINT('Ctrl Pts',(-20.5631517097427,-10.3579754375845,
123.061365248372)) ;
#57570 = CARTESIAN_POINT('Ctrl Pts',(-20.755752145473,-10.5477861912685,122.734100762332)) ;
#57571 = CARTESIAN_POINT('Ctrl Pts',(-20.4864480022253,-10.3677971109056,
122.869632334128)) ;
#57572 = CARTESIAN_POINT('Ctrl Pts',(-20.6168357130529,-10.5578446623434,
122.509252277714)) ;
#57573 = CARTESIAN_POINT('Ctrl Pts',(-20.3753148734437,-10.3778555819805,
122.689756047917)) ;
#57574 = CARTESIAN_POINT('Ctrl Pts',(-20.4430403513938,-10.5677692735199,
122.314768071456)) ;
#57575 = CARTESIAN_POINT('Ctrl Pts',(-20.2362698376991,-10.387780193157,122.534165626482)) ;
#57576 = CARTESIAN_POINT('Ctrl Pts',(-20.1694406712993,-10.5810466124203,
122.098190251904)) ;
#57577 = CARTESIAN_POINT('Ctrl Pts',(-20.0174235370575,-10.4010575320574,
122.360928563111)) ;
#57578 = CARTESIAN_POINT('Ctrl Pts',(-19.8449850134819,-10.5943454916579,
121.958111265335)) ;
#57579 = CARTESIAN_POINT('Ctrl Pts',(-19.7578454755217,-10.414356411295,122.248851541412)) ;
#57580 = CARTESIAN_POINT('Ctrl Pts',(-19.5008057716341,-10.6075843638286,
121.907157355648)) ;
#57581 = CARTESIAN_POINT('Ctrl Pts',(-19.4824812721784,-10.4275952834657,
122.208088431707)) ;
#57582 = CARTESIAN_POINT('Ctrl Pts',(-19.2379220825872,-10.6175909819652,
121.913944971404)) ;
#57583 = CARTESIAN_POINT('Ctrl Pts',(-19.2721785612158,-10.4376019016023,
122.213521362329)) ;
#57584 = CARTESIAN_POINT('Ctrl Pts',(-18.9796997397484,-10.6276219270267,
121.966900411424)) ;
#57585 = CARTESIAN_POINT('Ctrl Pts',(-19.0656000663898,-10.4476328466638,
122.255887759951)) ;
#57586 = CARTESIAN_POINT('Ctrl Pts',(-18.7386663423424,-10.6374781003785,
122.061762842601)) ;
#57587 = CARTESIAN_POINT('Ctrl Pts',(-18.8727746408769,-10.4574890200157,
122.33177976469)) ;
#57588 = CARTESIAN_POINT('Ctrl Pts',(-18.5144394578762,-10.6474773713414,
122.198683103417)) ;
#57589 = CARTESIAN_POINT('Ctrl Pts',(-18.6933942799492,-10.4674882909785,
122.44131783091)) ;
#57590 = CARTESIAN_POINT('Ctrl Pts',(-18.3191873796767,-10.6573718230987,
122.370468477432)) ;
#57591 = CARTESIAN_POINT('Ctrl Pts',(-18.5371942578644,-10.4773827427359,
122.578747654411)) ;
#57592 = CARTESIAN_POINT('Ctrl Pts',(-18.1540827677519,-10.6674351389081,
122.576990252266)) ;
#57593 = CARTESIAN_POINT('Ctrl Pts',(-18.4051122800728,-10.4874460585452,
122.743966484082)) ;
#57594 = CARTESIAN_POINT('Ctrl Pts',(-18.0298636947034,-10.6772739956477,
122.80380319062)) ;
#57595 = CARTESIAN_POINT('Ctrl Pts',(-18.3057391118683,-10.4972849152848,
122.925417599334)) ;
#57596 = CARTESIAN_POINT('Ctrl Pts',(-17.9447485718205,-10.6873401174653,
123.054218033102)) ;
#57597 = CARTESIAN_POINT('Ctrl Pts',(-18.2376490673584,-10.5073510371024,
123.125750218179)) ;
#57598 = CARTESIAN_POINT('Ctrl Pts',(-17.9052474071487,-10.6972233451896,
123.310952604467)) ;
#57599 = CARTESIAN_POINT('Ctrl Pts',(-18.2060503446323,-10.5172342648267,
123.331137917859)) ;
#57600 = CARTESIAN_POINT('Ctrl Pts',(-17.9104088183902,-10.7072128064683,
123.573388107812)) ;
#57601 = CARTESIAN_POINT('Ctrl Pts',(-18.2101816191011,-10.5272237261055,
123.541086174157)) ;
#57602 = CARTESIAN_POINT('Ctrl Pts',(-17.9610292610865,-10.7171765168948,
123.830297049982)) ;
#57603 = CARTESIAN_POINT('Ctrl Pts',(-18.2506800579227,-10.5371874365319,
123.746612765702)) ;
#57604 = CARTESIAN_POINT('Ctrl Pts',(-18.055529675207,-10.7271715196257,124.075387412779)) ;
#57605 = CARTESIAN_POINT('Ctrl Pts',(-18.3262823460712,-10.5471824392628,
123.942684211435)) ;
#57606 = CARTESIAN_POINT('Ctrl Pts',(-18.1920485023394,-10.737207850636,124.30103460394)) ;
#57607 = CARTESIAN_POINT('Ctrl Pts',(-18.4354992728269,-10.5572187702731,
124.12320085702)) ;
#57608 = CARTESIAN_POINT('Ctrl Pts',(-18.3620830674316,-10.7470540799783,
124.496092551227)) ;
#57609 = CARTESIAN_POINT('Ctrl Pts',(-18.5715282310147,-10.5670649996154,
124.279245472498)) ;
#57610 = CARTESIAN_POINT('Ctrl Pts',(-18.5658978745921,-10.7570395782535,
124.661307439936)) ;
#57611 = CARTESIAN_POINT('Ctrl Pts',(-18.7345812884953,-10.5770504978907,
124.411415684018)) ;
#57612 = CARTESIAN_POINT('Ctrl Pts',(-18.7941275674691,-10.7669744812365,
124.788187738228)) ;
#57613 = CARTESIAN_POINT('Ctrl Pts',(-18.9171658133098,-10.5869854008736,
124.51291799715)) ;
#57614 = CARTESIAN_POINT('Ctrl Pts',(-19.0439620659958,-10.7770319843317,
124.874312872399)) ;
#57615 = CARTESIAN_POINT('Ctrl Pts',(-19.1170341816332,-10.5970429039689,
124.58181616074)) ;
#57616 = CARTESIAN_POINT('Ctrl Pts',(-19.2988377714799,-10.7868536407023,
124.915180256188)) ;
#57617 = CARTESIAN_POINT('Ctrl Pts',(-19.3209344474807,-10.6068645603394,
124.614507954235)) ;
#57618 = CARTESIAN_POINT('Ctrl Pts',(-19.5630543230624,-10.7969097033674,
124.911570311771)) ;
#57619 = CARTESIAN_POINT('Ctrl Pts',(-19.5323077507347,-10.6169206230045,
124.611618015563)) ;
#57620 = CARTESIAN_POINT('Ctrl Pts',(-19.819595446342,-10.8068503680706,124.862237558294)) ;
#57621 = CARTESIAN_POINT('Ctrl Pts',(-19.7375400007717,-10.6268612877077,
124.572149858921)) ;
#57622 = CARTESIAN_POINT('Ctrl Pts',(-20.0630665620373,-10.8167547720191,
124.77021482164)) ;
#57623 = CARTESIAN_POINT('Ctrl Pts',(-19.9323158100592,-10.6367656916563,
124.498530010754)) ;
#57624 = CARTESIAN_POINT('Ctrl Pts',(-20.2899670415844,-10.8268012570127,
124.635280761768)) ;
#57625 = CARTESIAN_POINT('Ctrl Pts',(-20.1138352645202,-10.6468121766498,
124.390581038644)) ;
#57626 = CARTESIAN_POINT('Ctrl Pts',(-20.4871895041345,-10.8366974848244,
124.465706330208)) ;
#57627 = CARTESIAN_POINT('Ctrl Pts',(-20.2716116273665,-10.6567084044615,
124.254920337405)) ;
#57628 = CARTESIAN_POINT('Ctrl Pts',(-20.6546848715982,-10.8467570683879,
124.261221540526)) ;
#57629 = CARTESIAN_POINT('Ctrl Pts',(-20.4056065232405,-10.666767988025,124.091331180759)) ;
#57630 = CARTESIAN_POINT('Ctrl Pts',(-20.7815048415044,-10.8566090780567,
124.035494716813)) ;
#57631 = CARTESIAN_POINT('Ctrl Pts',(-20.5070605035221,-10.6766199976938,
123.910749362364)) ;
#57632 = CARTESIAN_POINT('Ctrl Pts',(-20.8689878382938,-10.8665716094963,
123.788751735695)) ;
#57633 = CARTESIAN_POINT('Ctrl Pts',(-20.5770451355397,-10.6865825291334,
123.713354624159)) ;
#57634 = CARTESIAN_POINT('Ctrl Pts',(-20.912200798905,-10.8766031577357,123.528690516731)) ;
#57635 = CARTESIAN_POINT('Ctrl Pts',(-20.6116136920761,-10.6966140773728,
123.505305293071)) ;
#57636 = CARTESIAN_POINT('Ctrl Pts',(-20.9098873495447,-10.8864945689487,
123.268764662041)) ;
#57637 = CARTESIAN_POINT('Ctrl Pts',(-20.6097611319996,-10.7065054885858,
123.297365172637)) ;
#57638 = CARTESIAN_POINT('Ctrl Pts',(-20.8623452479891,-10.8965108226567,
123.009867420401)) ;
#57639 = CARTESIAN_POINT('Ctrl Pts',(-20.5717257539026,-10.7165217422938,
123.090247714627)) ;
#57640 = CARTESIAN_POINT('Ctrl Pts',(-20.7699148713601,-10.9065409255014,
122.763029266333)) ;
#57641 = CARTESIAN_POINT('Ctrl Pts',(-20.4977797294624,-10.7265518451385,
122.89277779572)) ;
#57642 = CARTESIAN_POINT('Ctrl Pts',(-20.6387642261451,-10.9163973744551,
122.539650565094)) ;
#57643 = CARTESIAN_POINT('Ctrl Pts',(-20.3928580826567,-10.7364082940922,
122.714076343171)) ;
#57644 = CARTESIAN_POINT('Ctrl Pts',(-20.4686808693851,-10.9263963852274,
122.339414946397)) ;
#57645 = CARTESIAN_POINT('Ctrl Pts',(-20.2567901831118,-10.7464073048645,
122.553889022845)) ;
#57646 = CARTESIAN_POINT('Ctrl Pts',(-20.2686322562331,-10.9362916021454,
122.17321802605)) ;
#57647 = CARTESIAN_POINT('Ctrl Pts',(-20.0967507033617,-10.7563025217825,
122.420933115589)) ;
#57648 = CARTESIAN_POINT('Ctrl Pts',(-20.0390441621644,-10.9463521175027,
122.042191046987)) ;
#57649 = CARTESIAN_POINT('Ctrl Pts',(-19.9130792483847,-10.7663630371399,
122.316112859812)) ;
#57650 = CARTESIAN_POINT('Ctrl Pts',(-19.7954165502139,-10.9562014108898,
121.954734482504)) ;
#57651 = CARTESIAN_POINT('Ctrl Pts',(-19.7181774003615,-10.7762123305269,
122.246149405366)) ;
#57652 = CARTESIAN_POINT('Ctrl Pts',(-19.5358374377705,-10.9662285865698,
121.909463378996)) ;
#57653 = CARTESIAN_POINT('Ctrl Pts',(-19.5105138249597,-10.7862395062069,
122.209933979971)) ;
#57654 = CARTESIAN_POINT('Ctrl Pts',(-19.2722869357793,-10.976257162197,121.910644966112)) ;
#57655 = CARTESIAN_POINT('Ctrl Pts',(-19.2996733747243,-10.7962680818341,
122.210880867466)) ;
#57656 = CARTESIAN_POINT('Ctrl Pts',(-19.0176264126342,-10.9861022557429,
121.956219772892)) ;
#57657 = CARTESIAN_POINT('Ctrl Pts',(-19.0959461067893,-10.80611317538,122.247342053206)) ;
#57658 = CARTESIAN_POINT('Ctrl Pts',(-18.7708903038592,-10.9960934971746,
122.045998590472)) ;
#57659 = CARTESIAN_POINT('Ctrl Pts',(-18.8985578386737,-10.8161044168118,
122.319166355093)) ;
#57660 = CARTESIAN_POINT('Ctrl Pts',(-18.5427482922778,-11.0061292783179,
122.178316886012)) ;
#57661 = CARTESIAN_POINT('Ctrl Pts',(-18.7160448934344,-10.826140197955,122.425022334904)) ;
#57662 = CARTESIAN_POINT('Ctrl Pts',(-18.3445251559911,-11.0159814840476,
122.344856285624)) ;
#57663 = CARTESIAN_POINT('Ctrl Pts',(-18.5574679962225,-10.8359924036847,
122.558254360555)) ;
#57664 = CARTESIAN_POINT('Ctrl Pts',(-18.1757880512695,-11.0259435781646,
122.545009574833)) ;
#57665 = CARTESIAN_POINT('Ctrl Pts',(-18.422479486084,-10.8459544978017,122.718377561325)) ;
#57666 = CARTESIAN_POINT('Ctrl Pts',(-18.0438458206682,-11.0359661389917,
122.7729601423)) ;
#57667 = CARTESIAN_POINT('Ctrl Pts',(-18.3169268399301,-10.8559770586288,
122.900738711909)) ;
#57668 = CARTESIAN_POINT('Ctrl Pts',(-17.9540915966108,-11.0458939106433,
123.017952668927)) ;
#57669 = CARTESIAN_POINT('Ctrl Pts',(-18.245124831637,-10.8659048302804,123.096732704545)) ;
#57670 = CARTESIAN_POINT('Ctrl Pts',(-17.9077456060715,-11.0559362947681,
123.277734456028)) ;
#57671 = CARTESIAN_POINT('Ctrl Pts',(-18.2080492829974,-10.8759472144052,
123.304558492291)) ;
#57672 = CARTESIAN_POINT('Ctrl Pts',(-17.9071113956414,-11.0658255188387,
123.537627775337)) ;
#57673 = CARTESIAN_POINT('Ctrl Pts',(-18.2075431810581,-10.8858364384758,
123.512472408022)) ;
#57674 = CARTESIAN_POINT('Ctrl Pts',(-17.9515732678051,-11.075814767006,123.796333212552)) ;
#57675 = CARTESIAN_POINT('Ctrl Pts',(-18.2431137880875,-10.8958256866432,
123.719436394321)) ;
#57676 = CARTESIAN_POINT('Ctrl Pts',(-18.0401957307403,-11.085773344048,124.042564530846)) ;
#57677 = CARTESIAN_POINT('Ctrl Pts',(-18.3140127714057,-10.9057842636851,
123.916420715581)) ;
#57678 = CARTESIAN_POINT('Ctrl Pts',(-18.168909061226,-11.0956729131393,124.268660685117)) ;
#57679 = CARTESIAN_POINT('Ctrl Pts',(-18.4169840046767,-10.9156838327764,
124.097296505228)) ;
#57680 = CARTESIAN_POINT('Ctrl Pts',(-18.337456729501,-11.1057208252233,124.471882073783)) ;
#57681 = CARTESIAN_POINT('Ctrl Pts',(-18.5518230802635,-10.9257317448604,
124.259873062704)) ;
#57682 = CARTESIAN_POINT('Ctrl Pts',(-18.5355938114042,-11.1156161795305,
124.640356432155)) ;
#57683 = CARTESIAN_POINT('Ctrl Pts',(-18.7103328563198,-10.9356270991676,
124.394651291218)) ;
#57684 = CARTESIAN_POINT('Ctrl Pts',(-18.7636640136148,-11.1256778300217,
124.774075513825)) ;
#57685 = CARTESIAN_POINT('Ctrl Pts',(-18.8927897608012,-10.9456887496588,
124.50162580593)) ;
#57686 = CARTESIAN_POINT('Ctrl Pts',(-19.006164366436,-11.1355224454842,124.864226909227)) ;
#57687 = CARTESIAN_POINT('Ctrl Pts',(-19.0867894053353,-10.9555333651213,
124.573745602818)) ;
#57688 = CARTESIAN_POINT('Ctrl Pts',(-19.2634346826531,-11.1454825243856,
124.912371167711)) ;
#57689 = CARTESIAN_POINT('Ctrl Pts',(-19.2926054448866,-10.9654934440227,
124.612260162443)) ;
#57690 = CARTESIAN_POINT('Ctrl Pts',(-19.527207804198,-11.1555207187439,124.914621442776)) ;
#57691 = CARTESIAN_POINT('Ctrl Pts',(-19.5036240790433,-10.9755316383811,
124.614059468937)) ;
#57692 = CARTESIAN_POINT('Ctrl Pts',(-19.7832249578582,-11.1653944341435,
124.872221302149)) ;
#57693 = CARTESIAN_POINT('Ctrl Pts',(-19.7084367869545,-10.9854053537807,
124.580138714143)) ;
#57694 = CARTESIAN_POINT('Ctrl Pts',(-20.0328232712046,-11.1754661436778,
124.784280775567)) ;
#57695 = CARTESIAN_POINT('Ctrl Pts',(-19.9081154761896,-10.9954770633149,
124.509785425241)) ;
#57696 = CARTESIAN_POINT('Ctrl Pts',(-20.2580073160466,-11.1852985841303,
124.657525797588)) ;
#57697 = CARTESIAN_POINT('Ctrl Pts',(-20.0882613121544,-11.0053095037674,
124.408381348776)) ;
#57698 = CARTESIAN_POINT('Ctrl Pts',(-20.4622563153842,-11.1953304050557,
124.490859965048)) ;
#57699 = CARTESIAN_POINT('Ctrl Pts',(-20.2516602105671,-11.0153413246928,
124.275048161913)) ;
#57700 = CARTESIAN_POINT('Ctrl Pts',(-20.6337047072471,-11.2053507749413,
124.290992198856)) ;
#57701 = CARTESIAN_POINT('Ctrl Pts',(-20.388818355727,-11.0253616945784,124.115153420591)) ;
#57702 = CARTESIAN_POINT('Ctrl Pts',(-20.7663802888455,-11.215217546075,124.068198059716)) ;
#57703 = CARTESIAN_POINT('Ctrl Pts',(-20.4949578009106,-11.0352284657122,
123.936918629634)) ;
#57704 = CARTESIAN_POINT('Ctrl Pts',(-20.8602333250101,-11.2252883172644,
123.820777914708)) ;
#57705 = CARTESIAN_POINT('Ctrl Pts',(-20.5700397729981,-11.0452992369015,
123.738981987884)) ;
#57706 = CARTESIAN_POINT('Ctrl Pts',(-20.9086197171465,-11.235131477786,123.566660443392)) ;
#57707 = CARTESIAN_POINT('Ctrl Pts',(-20.608748082228,-11.0551423974231,123.535689006923)) ;
#57708 = CARTESIAN_POINT('Ctrl Pts',(-20.9130575837451,-11.2451117109724,
123.304436329207)) ;
#57709 = CARTESIAN_POINT('Ctrl Pts',(-20.6122979803846,-11.0651226306096,
123.325909958137)) ;
#57710 = CARTESIAN_POINT('Ctrl Pts',(-20.871238578832,-11.2551302310076,123.044509679255)) ;
#57711 = CARTESIAN_POINT('Ctrl Pts',(-20.5788422638188,-11.0751411506447,
123.117968711757)) ;
#57712 = CARTESIAN_POINT('Ctrl Pts',(-20.7865977118334,-11.2650135393913,
122.798931493979)) ;
#57713 = CARTESIAN_POINT('Ctrl Pts',(-20.5111294989851,-11.0850244590284,
122.921507117009)) ;
#57714 = CARTESIAN_POINT('Ctrl Pts',(-20.6581795184354,-11.2750818235621,
122.567651782636)) ;
#57715 = CARTESIAN_POINT('Ctrl Pts',(-20.4083944277967,-11.0950927431992,
122.736483258853)) ;
#57716 = CARTESIAN_POINT('Ctrl Pts',(-20.4956768373956,-11.2849119502298,
122.366783576293)) ;
#57717 = CARTESIAN_POINT('Ctrl Pts',(-20.278392801361,-11.1049228698669,122.575789859925)) ;
#57718 = CARTESIAN_POINT('Ctrl Pts',(-20.2963683002106,-11.2949785224363,
122.192903170129)) ;
#57719 = CARTESIAN_POINT('Ctrl Pts',(-20.1189455705143,-11.1149894420734,
122.436685510706)) ;
#57720 = CARTESIAN_POINT('Ctrl Pts',(-20.0737183940731,-11.304868678677,122.058761956782)) ;
#57721 = CARTESIAN_POINT('Ctrl Pts',(-19.9408262162374,-11.1248795983141,
122.329373218762)) ;
#57722 = CARTESIAN_POINT('Ctrl Pts',(-19.8289002832035,-11.3148612062534,
121.963839656321)) ;
#57723 = CARTESIAN_POINT('Ctrl Pts',(-19.7449718346838,-11.1348721258905,
122.253435573056)) ;
#57724 = CARTESIAN_POINT('Ctrl Pts',(-19.5720596012938,-11.3248226961277,
121.913243325035)) ;
#57725 = CARTESIAN_POINT('Ctrl Pts',(-19.53949961243,-11.1448336157648,122.212958778088)) ;
#57726 = CARTESIAN_POINT('Ctrl Pts',(-19.3117087063765,-11.3347319180149,
121.907440658381)) ;
#57727 = CARTESIAN_POINT('Ctrl Pts',(-19.3312196283681,-11.154742837652,122.208316707602)) ;
#57728 = CARTESIAN_POINT('Ctrl Pts',(-19.0507261790839,-11.3447804978252,
121.947576761925)) ;
#57729 = CARTESIAN_POINT('Ctrl Pts',(-19.1224334112309,-11.1647914174624,
122.240425692634)) ;
#57730 = CARTESIAN_POINT('Ctrl Pts',(-18.8047397506185,-11.3546634722953,
122.030941792183)) ;
#57731 = CARTESIAN_POINT('Ctrl Pts',(-18.9256451263576,-11.1746743919324,
122.307117480373)) ;
#57732 = CARTESIAN_POINT('Ctrl Pts',(-18.5741327464813,-11.364658383438,122.156656022076)) ;
#57733 = CARTESIAN_POINT('Ctrl Pts',(-18.7411596022947,-11.1846693030751,
122.407688711713)) ;
#57734 = CARTESIAN_POINT('Ctrl Pts',(-18.3685394795987,-11.3746787700116,
122.321218804861)) ;
#57735 = CARTESIAN_POINT('Ctrl Pts',(-18.5766849675727,-11.1946896896487,
122.539338955783)) ;
#57736 = CARTESIAN_POINT('Ctrl Pts',(-18.1964679003152,-11.3845888738687,
122.516679816547)) ;
#57737 = CARTESIAN_POINT('Ctrl Pts',(-18.4390281618024,-11.2045997935058,
122.69570718939)) ;
#57738 = CARTESIAN_POINT('Ctrl Pts',(-18.0601098924679,-11.3945165860786,
122.739110167226)) ;
#57739 = CARTESIAN_POINT('Ctrl Pts',(-18.3299418822673,-11.2145275057157,
122.873650852243)) ;
#57740 = CARTESIAN_POINT('Ctrl Pts',(-17.9635464111682,-11.4045596958458,
122.984721718142)) ;
#57741 = CARTESIAN_POINT('Ctrl Pts',(-18.2526908895868,-11.2245706154829,
123.070140194401)) ;
#57742 = CARTESIAN_POINT('Ctrl Pts',(-17.9117458665147,-11.4144461163014,
123.239325516368)) ;
#57743 = CARTESIAN_POINT('Ctrl Pts',(-18.2112504325607,-11.2344570359385,
123.273822340803)) ;
#57744 = CARTESIAN_POINT('Ctrl Pts',(-17.9044206322636,-11.424439293907,123.501819128649)) ;
#57745 = CARTESIAN_POINT('Ctrl Pts',(-18.2053899382535,-11.2444502135441,
123.483817059054)) ;
#57746 = CARTESIAN_POINT('Ctrl Pts',(-17.9427031377925,-11.4343849568109,
123.760362733581)) ;
#57747 = CARTESIAN_POINT('Ctrl Pts',(-18.2360155909013,-11.254395876448,123.690651513861)) ;
#57748 = CARTESIAN_POINT('Ctrl Pts',(-18.0248064637638,-11.4443322530161,
124.008552115012)) ;
#57749 = CARTESIAN_POINT('Ctrl Pts',(-18.3016977085877,-11.2643431726532,
123.889202714741)) ;
#57750 = CARTESIAN_POINT('Ctrl Pts',(-18.1502567640289,-11.454380018594,124.240883955143)) ;
#57751 = CARTESIAN_POINT('Ctrl Pts',(-18.402057739547,-11.2743909382311,124.075068526834)) ;
#57752 = CARTESIAN_POINT('Ctrl Pts',(-18.31072897444,-11.4642282318116,124.443923603713)) ;
#57753 = CARTESIAN_POINT('Ctrl Pts',(-18.5304345036023,-11.2842391514487,
124.237499615883)) ;
#57754 = CARTESIAN_POINT('Ctrl Pts',(-18.5056290796381,-11.4741878046057,
124.618608195999)) ;
#57755 = CARTESIAN_POINT('Ctrl Pts',(-18.6863538979281,-11.2941987242428,
124.377247496808)) ;
#57756 = CARTESIAN_POINT('Ctrl Pts',(-18.7298566496538,-11.4842244256382,
124.757470221316)) ;
#57757 = CARTESIAN_POINT('Ctrl Pts',(-18.8657357990191,-11.3042353452753,
124.488337605862)) ;
#57758 = CARTESIAN_POINT('Ctrl Pts',(-18.9708633136617,-11.4941049404486,
124.854157638432)) ;
#57759 = CARTESIAN_POINT('Ctrl Pts',(-19.0585400766373,-11.3141158600857,
124.565687764043)) ;
#57760 = CARTESIAN_POINT('Ctrl Pts',(-19.2293390121453,-11.5041575917556,
124.90854357499)) ;
#57761 = CARTESIAN_POINT('Ctrl Pts',(-19.265320722865,-11.3241685113927,124.609197170298)) ;
#57762 = CARTESIAN_POINT('Ctrl Pts',(-19.4892814880954,-11.5140529900356,
124.917196362515)) ;
#57763 = CARTESIAN_POINT('Ctrl Pts',(-19.4732739141341,-11.3340639096727,
124.61612002099)) ;
#57764 = CARTESIAN_POINT('Ctrl Pts',(-19.7507413265183,-11.5241031117417,
124.880139860388)) ;
#57765 = CARTESIAN_POINT('Ctrl Pts',(-19.6824420883012,-11.3441140313788,
124.586475461409)) ;
#57766 = CARTESIAN_POINT('Ctrl Pts',(-19.9977235238706,-11.5339873912836,
124.799620909315)) ;
#57767 = CARTESIAN_POINT('Ctrl Pts',(-19.8800272541223,-11.3539983109207,
124.522061213482)) ;
#57768 = CARTESIAN_POINT('Ctrl Pts',(-20.2297217101426,-11.5439821725755,
124.676533838734)) ;
#57769 = CARTESIAN_POINT('Ctrl Pts',(-20.0656260392352,-11.3639930922127,
124.423592342302)) ;
#57770 = CARTESIAN_POINT('Ctrl Pts',(-20.4358226950316,-11.5539300177623,
124.515687379052)) ;
#57771 = CARTESIAN_POINT('Ctrl Pts',(-20.2305069652934,-11.3739409373994,
124.294916057216)) ;
#57772 = CARTESIAN_POINT('Ctrl Pts',(-20.6109276227123,-11.5638669811497,
124.321995034894)) ;
#57773 = CARTESIAN_POINT('Ctrl Pts',(-20.37059121164,-11.3838779007868,124.139963144074)) ;
#57774 = CARTESIAN_POINT('Ctrl Pts',(-20.7506923359331,-11.5738499458869,
124.099943607919)) ;
#57775 = CARTESIAN_POINT('Ctrl Pts',(-20.482403674932,-11.3938608655241,123.962322680992)) ;
#57776 = CARTESIAN_POINT('Ctrl Pts',(-20.8499100759965,-11.5838937973026,
123.855392878857)) ;
#57777 = CARTESIAN_POINT('Ctrl Pts',(-20.561778696542,-11.4039047169397,123.766682270914)) ;
#57778 = CARTESIAN_POINT('Ctrl Pts',(-20.9045834153395,-11.5937219986373,
123.60293017781)) ;
#57779 = CARTESIAN_POINT('Ctrl Pts',(-20.6055180794411,-11.4137329182744,
123.5647134447)) ;
#57780 = CARTESIAN_POINT('Ctrl Pts',(-20.9149654649752,-11.6037985712354,
123.338386769837)) ;
#57781 = CARTESIAN_POINT('Ctrl Pts',(-20.6138247398722,-11.4238094908725,
123.353078412637)) ;
#57782 = CARTESIAN_POINT('Ctrl Pts',(-20.8801663077808,-11.6136506512429,
123.081776137432)) ;
#57783 = CARTESIAN_POINT('Ctrl Pts',(-20.5859865727851,-11.43366157088,123.147790745259)) ;
#57784 = CARTESIAN_POINT('Ctrl Pts',(-20.7998144512249,-11.623723936247,122.829596800206)) ;
#57785 = CARTESIAN_POINT('Ctrl Pts',(-20.5217060262302,-11.4437348558841,
122.946046639568)) ;
#57786 = CARTESIAN_POINT('Ctrl Pts',(-20.6796373590905,-11.6335652879575,
122.60057140377)) ;
#57787 = CARTESIAN_POINT('Ctrl Pts',(-20.4255657854105,-11.4535762075946,
122.762826748449)) ;
#57788 = CARTESIAN_POINT('Ctrl Pts',(-20.5203770951846,-11.643526787354,122.39283222261)) ;
#57789 = CARTESIAN_POINT('Ctrl Pts',(-20.2981587895807,-11.4635377069911,
122.59663487523)) ;
#57790 = CARTESIAN_POINT('Ctrl Pts',(-20.3256964580967,-11.653562563484,122.21490632929)) ;
#57791 = CARTESIAN_POINT('Ctrl Pts',(-20.1424150134632,-11.4735734831211,
122.454293226116)) ;
#57792 = CARTESIAN_POINT('Ctrl Pts',(-20.1065035192901,-11.6634509901216,
122.07533899432)) ;
#57793 = CARTESIAN_POINT('Ctrl Pts',(-19.9670619537043,-11.4834619097587,
122.34263870474)) ;
#57794 = CARTESIAN_POINT('Ctrl Pts',(-19.8635046295888,-11.6734663121965,
121.974209274979)) ;
#57795 = CARTESIAN_POINT('Ctrl Pts',(-19.7726633636097,-11.4934772318336,
122.261733686333)) ;
#57796 = CARTESIAN_POINT('Ctrl Pts',(-19.6061275734712,-11.6834966610967,
121.917323321599)) ;
#57797 = CARTESIAN_POINT('Ctrl Pts',(-19.5667619143694,-11.5035075807338,
122.216223718493)) ;
#57798 = CARTESIAN_POINT('Ctrl Pts',(-19.3477206075241,-11.6933400367034,
121.905682077823)) ;
#57799 = CARTESIAN_POINT('Ctrl Pts',(-19.3600373704475,-11.5133509563405,
122.206909440148)) ;
#57800 = CARTESIAN_POINT('Ctrl Pts',(-19.0862848802727,-11.7033694736005,
121.939135039902)) ;
#57801 = CARTESIAN_POINT('Ctrl Pts',(-19.1508885485966,-11.5233803932376,
122.233670378294)) ;
#57802 = CARTESIAN_POINT('Ctrl Pts',(-18.834778258423,-11.7134013515334,122.018183059179)) ;
#57803 = CARTESIAN_POINT('Ctrl Pts',(-18.9496827948867,-11.5334122711706,
122.296907572202)) ;
#57804 = CARTESIAN_POINT('Ctrl Pts',(-18.6053133475109,-11.7232309746389,
122.136772150957)) ;
#57805 = CARTESIAN_POINT('Ctrl Pts',(-18.7661111198526,-11.543241894276,122.391777125529)) ;
#57806 = CARTESIAN_POINT('Ctrl Pts',(-18.3960907645237,-11.733220445792,122.295336373572)) ;
#57807 = CARTESIAN_POINT('Ctrl Pts',(-18.5987322188273,-11.5532313654291,
122.518627168111)) ;
#57808 = CARTESIAN_POINT('Ctrl Pts',(-18.2171052463347,-11.7432642945544,
122.489315908043)) ;
#57809 = CARTESIAN_POINT('Ctrl Pts',(-18.4555426693397,-11.5632752141915,
122.673809908671)) ;
#57810 = CARTESIAN_POINT('Ctrl Pts',(-18.0772224088806,-11.7530860000861,
122.706227559913)) ;
#57811 = CARTESIAN_POINT('Ctrl Pts',(-18.3436356441143,-11.5730969197232,
122.847337557249)) ;
#57812 = CARTESIAN_POINT('Ctrl Pts',(-17.974358275623,-11.7631210399139,122.949047320032)) ;
#57813 = CARTESIAN_POINT('Ctrl Pts',(-18.2613427735164,-11.583131959551,123.041592794472)) ;
#57814 = CARTESIAN_POINT('Ctrl Pts',(-17.9159869176276,-11.7731457468054,
123.205947428722)) ;
#57815 = CARTESIAN_POINT('Ctrl Pts',(-18.2146441954026,-11.5931566664425,
123.247112562016)) ;
#57816 = CARTESIAN_POINT('Ctrl Pts',(-17.9027824760765,-11.7829984511461,
123.464529062484)) ;
#57817 = CARTESIAN_POINT('Ctrl Pts',(-18.2040790568452,-11.6030093707832,
123.453976982937)) ;
#57818 = CARTESIAN_POINT('Ctrl Pts',(-17.9346582755181,-11.7929865733538,
123.72504475189)) ;
#57819 = CARTESIAN_POINT('Ctrl Pts',(-18.2295779793896,-11.6129974929909,
123.662389596345)) ;
#57820 = CARTESIAN_POINT('Ctrl Pts',(-18.0108208430666,-11.8029150434611,
123.974597684985)) ;
#57821 = CARTESIAN_POINT('Ctrl Pts',(-18.290506276576,-11.6229259630982,123.862032045727)) ;
#57822 = CARTESIAN_POINT('Ctrl Pts',(-18.129492517191,-11.8129040206283,124.20875545915)) ;
#57823 = CARTESIAN_POINT('Ctrl Pts',(-18.3854419582014,-11.6329149402654,
124.049358946099)) ;
#57824 = CARTESIAN_POINT('Ctrl Pts',(-18.2881378411285,-11.822941827908,124.419490767607)) ;
#57825 = CARTESIAN_POINT('Ctrl Pts',(-18.5123568914905,-11.6429527475451,
124.217948275703)) ;
#57826 = CARTESIAN_POINT('Ctrl Pts',(-18.4770035096972,-11.8327881287713,
124.596360779214)) ;
#57827 = CARTESIAN_POINT('Ctrl Pts',(-18.6634476664908,-11.6527990484084,
124.359445074232)) ;
#57828 = CARTESIAN_POINT('Ctrl Pts',(-18.6973386411338,-11.8428138721506,
124.740820127041)) ;
#57829 = CARTESIAN_POINT('Ctrl Pts',(-18.8397147708248,-11.6628247917877,
124.47501413786)) ;
#57830 = CARTESIAN_POINT('Ctrl Pts',(-18.9398076657194,-11.8528447385896,
124.844250930531)) ;
#57831 = CARTESIAN_POINT('Ctrl Pts',(-19.0336893273778,-11.6728556582267,
124.557760414888)) ;
#57832 = CARTESIAN_POINT('Ctrl Pts',(-19.1914647637144,-11.8626820973884,
124.903358127309)) ;
#57833 = CARTESIAN_POINT('Ctrl Pts',(-19.2350138511474,-11.6826930170255,
124.605047798239)) ;
#57834 = CARTESIAN_POINT('Ctrl Pts',(-19.4535879451844,-11.8726740583222,
124.918802859843)) ;
#57835 = CARTESIAN_POINT('Ctrl Pts',(-19.4447121787566,-11.6926849779593,
124.617405527106)) ;
#57836 = CARTESIAN_POINT('Ctrl Pts',(-19.7154151681285,-11.8827064208787,
124.887849956679)) ;
#57837 = CARTESIAN_POINT('Ctrl Pts',(-19.6541742063547,-11.7027173405158,
124.592645060716)) ;
#57838 = CARTESIAN_POINT('Ctrl Pts',(-19.9637513981786,-11.8925715814531,
124.813477415096)) ;
#57839 = CARTESIAN_POINT('Ctrl Pts',(-19.8528431830511,-11.7125825010902,
124.533149033972)) ;
#57840 = CARTESIAN_POINT('Ctrl Pts',(-20.1980246864583,-11.9025334860308,
124.696630723348)) ;
#57841 = CARTESIAN_POINT('Ctrl Pts',(-20.0402625347496,-11.7225444056679,
124.439673577518)) ;
#57842 = CARTESIAN_POINT('Ctrl Pts',(-20.4097188088187,-11.9125684161065,
124.539405883131)) ;
#57843 = CARTESIAN_POINT('Ctrl Pts',(-20.2096190243359,-11.7325793357437,
124.313895264542)) ;
#57844 = CARTESIAN_POINT('Ctrl Pts',(-20.5885436050965,-11.9224533629601,
124.350939834724)) ;
#57845 = CARTESIAN_POINT('Ctrl Pts',(-20.3526800140608,-11.7424642825973,
124.163124141174)) ;
#57846 = CARTESIAN_POINT('Ctrl Pts',(-20.7344544461953,-11.9325190392716,
124.130360829596)) ;
#57847 = CARTESIAN_POINT('Ctrl Pts',(-20.4694104306545,-11.7525299589087,
123.986661948345)) ;
#57848 = CARTESIAN_POINT('Ctrl Pts',(-20.8377538535721,-11.9423579589065,
123.89328858742)) ;
#57849 = CARTESIAN_POINT('Ctrl Pts',(-20.5520516016734,-11.7623688785436,
123.797005487303)) ;
#57850 = CARTESIAN_POINT('Ctrl Pts',(-20.9000168313516,-11.9524214686409,
123.636302931589)) ;
#57851 = CARTESIAN_POINT('Ctrl Pts',(-20.6018640323336,-11.7724323882781,
123.591417349548)) ;
#57852 = CARTESIAN_POINT('Ctrl Pts',(-20.9162207081352,-11.9623150818027,
123.376783859036)) ;
#57853 = CARTESIAN_POINT('Ctrl Pts',(-20.6148291614224,-11.7823260014398,
123.383802596767)) ;
#57854 = CARTESIAN_POINT('Ctrl Pts',(-20.8876645643203,-11.9722590886161,
123.117066234101)) ;
#57855 = CARTESIAN_POINT('Ctrl Pts',(-20.5919863882844,-11.7922700082532,
123.176028481019)) ;
#57856 = CARTESIAN_POINT('Ctrl Pts',(-20.8141243155986,-11.9822600429704,
122.8647086418)) ;
#57857 = CARTESIAN_POINT('Ctrl Pts',(-20.5331562591136,-11.8022709626075,
122.974141872013)) ;
#57858 = CARTESIAN_POINT('Ctrl Pts',(-20.6970504996991,-11.9922988006627,
122.628327621003)) ;
#57859 = CARTESIAN_POINT('Ctrl Pts',(-20.4394990793776,-11.8123097202998,
122.78503611631)) ;
#57860 = CARTESIAN_POINT('Ctrl Pts',(-20.5444825751892,-12.0021229848327,
122.420035361004)) ;
#57861 = CARTESIAN_POINT('Ctrl Pts',(-20.3174467467038,-11.8221339044698,
122.618401417283)) ;
#57862 = CARTESIAN_POINT('Ctrl Pts',(-20.3539293395536,-12.0121810504321,
122.236896566325)) ;
#57863 = CARTESIAN_POINT('Ctrl Pts',(-20.1650056265507,-11.8321919700692,
122.471888771544)) ;
#57864 = CARTESIAN_POINT('Ctrl Pts',(-20.1370409747147,-12.0221110972068,
122.091764368012)) ;
#57865 = CARTESIAN_POINT('Ctrl Pts',(-19.9914963147766,-11.8421220168439,
122.355781349936)) ;
#57866 = CARTESIAN_POINT('Ctrl Pts',(-19.8980237231667,-12.0320625395439,
121.985643564698)) ;
#57867 = CARTESIAN_POINT('Ctrl Pts',(-19.8002835442428,-11.8520734591811,
122.270882756195)) ;
#57868 = CARTESIAN_POINT('Ctrl Pts',(-19.6416983085707,-12.0421093367232,
121.922384338977)) ;
#57869 = CARTESIAN_POINT('Ctrl Pts',(-19.5952237285874,-11.8621202563603,
122.220273262082)) ;
#57870 = CARTESIAN_POINT('Ctrl Pts',(-19.3835093232675,-12.0519572774033,
121.904703348343)) ;
#57871 = CARTESIAN_POINT('Ctrl Pts',(-19.3886730067727,-11.8719681970404,
122.206126303218)) ;
#57872 = CARTESIAN_POINT('Ctrl Pts',(-19.1231275997313,-12.0619189087459,
121.931627958287)) ;
#57873 = CARTESIAN_POINT('Ctrl Pts',(-19.1803674964563,-11.881929828383,122.227663754114)) ;
#57874 = CARTESIAN_POINT('Ctrl Pts',(-18.8697470442625,-12.0719475681218,
122.004163670847)) ;
#57875 = CARTESIAN_POINT('Ctrl Pts',(-18.9776624753786,-11.8919584877589,
122.28569018209)) ;
#57876 = CARTESIAN_POINT('Ctrl Pts',(-18.6355935850335,-12.08185787101,122.118142693142)) ;
#57877 = CARTESIAN_POINT('Ctrl Pts',(-18.7903388847647,-11.9018687906471,
122.376871325098)) ;
#57878 = CARTESIAN_POINT('Ctrl Pts',(-18.4238474019827,-12.0917927655722,
122.270883953054)) ;
#57879 = CARTESIAN_POINT('Ctrl Pts',(-18.6209407077585,-11.9118036852093,
122.49906244756)) ;
#57880 = CARTESIAN_POINT('Ctrl Pts',(-18.2400799717895,-12.1018338642391,
122.460231143199)) ;
#57881 = CARTESIAN_POINT('Ctrl Pts',(-18.4739251815215,-11.9218447838762,
122.650538612055)) ;
#57882 = CARTESIAN_POINT('Ctrl Pts',(-18.0940875093298,-12.1117211467435,
122.675182672206)) ;
#57883 = CARTESIAN_POINT('Ctrl Pts',(-18.3571294254557,-11.9317320663806,
122.822498468009)) ;
#57884 = CARTESIAN_POINT('Ctrl Pts',(-17.9861176823212,-12.121712887254,122.914511116819)) ;
#57885 = CARTESIAN_POINT('Ctrl Pts',(-18.2707515313325,-11.9417238068911,
123.013960245955)) ;
#57886 = CARTESIAN_POINT('Ctrl Pts',(-17.921689729601,-12.1316634364894,123.16795292873)) ;
#57887 = CARTESIAN_POINT('Ctrl Pts',(-18.2192070041483,-11.9516743561265,
123.216713069332)) ;
#57888 = CARTESIAN_POINT('Ctrl Pts',(-17.9018892648507,-12.1415991141242,
123.428284203218)) ;
#57889 = CARTESIAN_POINT('Ctrl Pts',(-18.203364387403,-11.9616100337613,123.424977867107)) ;
#57890 = CARTESIAN_POINT('Ctrl Pts',(-17.9274444398076,-12.151584531917,123.689463440879)) ;
#57891 = CARTESIAN_POINT('Ctrl Pts',(-18.2238062820509,-11.9715954515541,
123.633921427947)) ;
#57892 = CARTESIAN_POINT('Ctrl Pts',(-17.9985764205707,-12.1616133247875,
123.943226816736)) ;
#57893 = CARTESIAN_POINT('Ctrl Pts',(-18.2807096769127,-11.9816242444246,
123.836932670854)) ;
#57894 = CARTESIAN_POINT('Ctrl Pts',(-18.1107411250608,-12.1714928360155,
124.177366527378)) ;
#57895 = CARTESIAN_POINT('Ctrl Pts',(-18.3704394042732,-11.9915037556526,
124.024245403531)) ;
#57896 = CARTESIAN_POINT('Ctrl Pts',(-18.263117466536,-12.1814863726884,124.391272663474)) ;
#57897 = CARTESIAN_POINT('Ctrl Pts',(-18.4923386313118,-12.0014972923255,
124.195371583237)) ;
#57898 = CARTESIAN_POINT('Ctrl Pts',(-18.4514152853576,-12.1915186409522,
124.575779592005)) ;
#57899 = CARTESIAN_POINT('Ctrl Pts',(-18.6429752478029,-12.0115295605894,
124.342978676221)) ;
#57900 = CARTESIAN_POINT('Ctrl Pts',(-18.6649582254987,-12.2013826029581,
124.722768521293)) ;
#57901 = CARTESIAN_POINT('Ctrl Pts',(-18.813808386405,-12.0213935225952,124.460571699597)) ;
#57902 = CARTESIAN_POINT('Ctrl Pts',(-18.9056381213548,-12.211452664303,124.832713751572)) ;
#57903 = CARTESIAN_POINT('Ctrl Pts',(-19.0063512619196,-12.0314635839401,
124.548529868389)) ;
#57904 = CARTESIAN_POINT('Ctrl Pts',(-19.1560012005742,-12.2212950286517,
124.897694900574)) ;
#57905 = CARTESIAN_POINT('Ctrl Pts',(-19.2066412928752,-12.0413059482889,
124.600516988053)) ;
#57906 = CARTESIAN_POINT('Ctrl Pts',(-19.4168488001017,-12.2312557011542,
124.919426126704)) ;
#57907 = CARTESIAN_POINT('Ctrl Pts',(-19.4153192326186,-12.0512666207913,
124.617904150398)) ;
#57908 = CARTESIAN_POINT('Ctrl Pts',(-19.6794781670334,-12.241293772222,124.894826056415)) ;
#57909 = CARTESIAN_POINT('Ctrl Pts',(-19.6254228033852,-12.0613046918591,
124.598226319022)) ;
#57910 = CARTESIAN_POINT('Ctrl Pts',(-19.9298584470305,-12.2511673871824,
124.826609084731)) ;
#57911 = CARTESIAN_POINT('Ctrl Pts',(-19.82572781557,-12.0711783068196,124.543654773306)) ;
#57912 = CARTESIAN_POINT('Ctrl Pts',(-20.1692027685541,-12.2612396217637,
124.713703674863)) ;
#57913 = CARTESIAN_POINT('Ctrl Pts',(-20.0172039403952,-12.0812505414008,
124.45333259084)) ;
#57914 = CARTESIAN_POINT('Ctrl Pts',(-20.3802336084559,-12.2710636402125,
124.56490174156)) ;
#57915 = CARTESIAN_POINT('Ctrl Pts',(-20.1860304834579,-12.0910745598496,
124.334292311524)) ;
#57916 = CARTESIAN_POINT('Ctrl Pts',(-20.5668505339034,-12.2811285611885,
124.3775468474)) ;
#57917 = CARTESIAN_POINT('Ctrl Pts',(-20.3353241585353,-12.1011394808256,
124.184411132778)) ;
#57918 = CARTESIAN_POINT('Ctrl Pts',(-20.7654710388387,-12.2943388594833,
124.092731380698)) ;
#57919 = CARTESIAN_POINT('Ctrl Pts',(-20.4942292379436,-12.1143497791204,
123.9565547192)) ;
#57920 = CARTESIAN_POINT('Ctrl Pts',(-20.8864681734945,-12.3076543062152,
123.760293059331)) ;
#57921 = CARTESIAN_POINT('Ctrl Pts',(-20.5910323501045,-12.1276652258523,
123.690569694297)) ;
#57922 = CARTESIAN_POINT('Ctrl Pts',(-20.9168412402485,-12.3209445514825,
123.412248798329)) ;
#57923 = CARTESIAN_POINT('Ctrl Pts',(-20.6153241110925,-12.1409554711196,
123.412181858016)) ;
#57924 = CARTESIAN_POINT('Ctrl Pts',(-20.8936136564304,-12.3309953010896,
123.149204261583)) ;
#57925 = CARTESIAN_POINT('Ctrl Pts',(-20.5967459980804,-12.1510062207267,
123.20173670269)) ;
#57926 = CARTESIAN_POINT('Ctrl Pts',(-20.8271599100472,-12.3408079080718,
122.900008574106)) ;
#57927 = CARTESIAN_POINT('Ctrl Pts',(-20.5435845615401,-12.160818827709,123.002381693859)) ;
#57928 = CARTESIAN_POINT('Ctrl Pts',(-20.7159339872492,-12.3508790060661,
122.659895486434)) ;
#57929 = CARTESIAN_POINT('Ctrl Pts',(-20.4546048866285,-12.1708899257032,
122.810289464688)) ;
#57930 = CARTESIAN_POINT('Ctrl Pts',(-20.5671825471141,-12.360768578841,122.446765213332)) ;
#57931 = CARTESIAN_POINT('Ctrl Pts',(-20.3356088789073,-12.1807794984781,
122.639785845869)) ;
#57932 = CARTESIAN_POINT('Ctrl Pts',(-20.3217335957846,-12.3740386856443,
122.199036770175)) ;
#57933 = CARTESIAN_POINT('Ctrl Pts',(-20.1392327070889,-12.1940496052814,
122.441591581826)) ;
#57934 = CARTESIAN_POINT('Ctrl Pts',(-19.9402799223287,-12.3906553725668,
121.976489963183)) ;
#57935 = CARTESIAN_POINT('Ctrl Pts',(-19.8341061887492,-12.2106662922039,
122.263562894215)) ;
#57936 = CARTESIAN_POINT('Ctrl Pts',(-19.5069560654083,-12.407229415883,121.897341845887)) ;
#57937 = CARTESIAN_POINT('Ctrl Pts',(-19.4873858330109,-12.2272403355201,
122.200234744545)) ;
#57938 = CARTESIAN_POINT('Ctrl Pts',(-19.1586250796142,-12.4205259833148,
121.925240968701)) ;
#57939 = CARTESIAN_POINT('Ctrl Pts',(-19.2087707820573,-12.2405369029519,
122.222555129474)) ;
#57940 = CARTESIAN_POINT('Ctrl Pts',(-18.9035497915594,-12.4305560468922,
121.991664800906)) ;
#57941 = CARTESIAN_POINT('Ctrl Pts',(-19.0046999503751,-12.2505669665293,
122.275692101065)) ;
#57942 = CARTESIAN_POINT('Ctrl Pts',(-18.6671468529052,-12.4404499387414,
122.099840645972)) ;
#57943 = CARTESIAN_POINT('Ctrl Pts',(-18.8155801630729,-12.2604608583786,
122.362230133135)) ;
#57944 = CARTESIAN_POINT('Ctrl Pts',(-18.3796682061191,-12.453702694527,122.296549637466)) ;
#57945 = CARTESIAN_POINT('Ctrl Pts',(-18.5855889437377,-12.2737136141641,
122.519603145883)) ;
#57946 = CARTESIAN_POINT('Ctrl Pts',(-18.0908280313655,-12.4704307995194,
122.634462100718)) ;
#57947 = CARTESIAN_POINT('Ctrl Pts',(-18.3545219823308,-12.2904417191566,
122.789922698833)) ;
#57948 = CARTESIAN_POINT('Ctrl Pts',(-17.9056069777788,-12.4902616359979,
123.128014485523)) ;
#57949 = CARTESIAN_POINT('Ctrl Pts',(-18.2063394436304,-12.3102725556351,
123.184767136768)) ;
#57950 = CARTESIAN_POINT('Ctrl Pts',(-17.8986058474029,-12.5101870278881,
123.65743523967)) ;
#57951 = CARTESIAN_POINT('Ctrl Pts',(-18.2007363231524,-12.3301979475252,
123.608303576448)) ;
#57952 = CARTESIAN_POINT('Ctrl Pts',(-18.0728134812496,-12.5301122412401,
124.157630024429)) ;
#57953 = CARTESIAN_POINT('Ctrl Pts',(-18.3400999156776,-12.3501231608772,
124.00846101179)) ;
#57954 = CARTESIAN_POINT('Ctrl Pts',(-18.4070561283902,-12.5500372547252,
124.568319257347)) ;
#57955 = CARTESIAN_POINT('Ctrl Pts',(-18.6074925126866,-12.3700481743623,
124.337014427016)) ;
#57956 = CARTESIAN_POINT('Ctrl Pts',(-18.8599799731256,-12.5699137264252,
124.840308096966)) ;
#57957 = CARTESIAN_POINT('Ctrl Pts',(-18.9698314340081,-12.3899246460623,
124.554607919997)) ;
#57958 = CARTESIAN_POINT('Ctrl Pts',(-19.3811313633293,-12.5898930443341,
124.942158139695)) ;
#57959 = CARTESIAN_POINT('Ctrl Pts',(-19.3867523851537,-12.4099039639712,
124.636089848104)) ;
#57960 = CARTESIAN_POINT('Ctrl Pts',(-19.9045262603243,-12.6098260479101,
124.859844414469)) ;
#57961 = CARTESIAN_POINT('Ctrl Pts',(-19.8054692095567,-12.4298369675472,
124.570240637955)) ;
#57962 = CARTESIAN_POINT('Ctrl Pts',(-20.3677432424192,-12.6297213179378,
124.6048789893)) ;
#57963 = CARTESIAN_POINT('Ctrl Pts',(-20.1760444928505,-12.4497322375749,
124.366269105617)) ;
#57964 = CARTESIAN_POINT('Ctrl Pts',(-20.7170498595964,-12.6496426558436,
124.206944794287)) ;
#57965 = CARTESIAN_POINT('Ctrl Pts',(-20.4554911883008,-12.4696535754807,
124.047921837557)) ;
#57966 = CARTESIAN_POINT('Ctrl Pts',(-20.9098403565593,-12.6696002791098,
123.712751204342)) ;
#57967 = CARTESIAN_POINT('Ctrl Pts',(-20.6097246738742,-12.4896111987469,
123.652566906432)) ;
#57968 = CARTESIAN_POINT('Ctrl Pts',(-20.922485985003,-12.689480111067,123.18461209717)) ;
#57969 = CARTESIAN_POINT('Ctrl Pts',(-20.6198419805455,-12.5094910307041,
123.230054122359)) ;
#57970 = CARTESIAN_POINT('Ctrl Pts',(-20.7554545445051,-12.7093619623639,
122.683172172836)) ;
#57971 = CARTESIAN_POINT('Ctrl Pts',(-20.4862161995466,-12.529372882001,122.828900805559)) ;
#57972 = CARTESIAN_POINT('Ctrl Pts',(-20.4235254244291,-12.7294329794677,
122.265649141046)) ;
#57973 = CARTESIAN_POINT('Ctrl Pts',(-20.2206735911977,-12.5494438991048,
122.494883034392)) ;
#57974 = CARTESIAN_POINT('Ctrl Pts',(-19.9749237655201,-12.7492402032208,
121.989968961482)) ;
#57975 = CARTESIAN_POINT('Ctrl Pts',(-19.8617900839095,-12.5692511228579,
122.274337697005)) ;
#57976 = CARTESIAN_POINT('Ctrl Pts',(-19.4550399386783,-12.7692213387896,
121.881799009553)) ;
#57977 = CARTESIAN_POINT('Ctrl Pts',(-19.4458826423283,-12.5892322584267,
122.18780260183)) ;
#57978 = CARTESIAN_POINT('Ctrl Pts',(-18.9310095255676,-12.7891488321288,
121.958350587305)) ;
#57979 = CARTESIAN_POINT('Ctrl Pts',(-19.0266575304228,-12.6091597517659,
122.24904461452)) ;
#57980 = CARTESIAN_POINT('Ctrl Pts',(-18.4660378435683,-12.8089694934866,
122.206286369213)) ;
#57981 = CARTESIAN_POINT('Ctrl Pts',(-18.6546792788745,-12.6289804131237,
122.447395528075)) ;
#57982 = CARTESIAN_POINT('Ctrl Pts',(-18.1095237058468,-12.8290666827084,
122.603786127405)) ;
#57983 = CARTESIAN_POINT('Ctrl Pts',(-18.3694696834846,-12.6490776023455,
122.765395547961)) ;
#57984 = CARTESIAN_POINT('Ctrl Pts',(-17.9128685242105,-12.8488303617167,
123.091145395877)) ;
#57985 = CARTESIAN_POINT('Ctrl Pts',(-18.212146236786,-12.6688412813539,123.155285756016)) ;
#57986 = CARTESIAN_POINT('Ctrl Pts',(-17.8934532250118,-12.8688876403898,
123.623648070234)) ;
#57987 = CARTESIAN_POINT('Ctrl Pts',(-18.1966161448372,-12.6888985600269,
123.581287459871)) ;
#57988 = CARTESIAN_POINT('Ctrl Pts',(-18.0551868058746,-12.8886830641372,
124.124451004221)) ;
#57989 = CARTESIAN_POINT('Ctrl Pts',(-18.3260055893083,-12.7086939837743,
123.981930874229)) ;
#57990 = CARTESIAN_POINT('Ctrl Pts',(-18.3794288064129,-12.9086467088648,
124.544379679826)) ;
#57991 = CARTESIAN_POINT('Ctrl Pts',(-18.5854015952883,-12.7286576285019,
124.317872293328)) ;
#57992 = CARTESIAN_POINT('Ctrl Pts',(-18.8287006511552,-12.9286302001389,
124.827680379695)) ;
#57993 = CARTESIAN_POINT('Ctrl Pts',(-18.9448205353017,-12.748641119776,124.544510768176)) ;
#57994 = CARTESIAN_POINT('Ctrl Pts',(-19.3429186866301,-12.9484376952882,
124.94073161998)) ;
#57995 = CARTESIAN_POINT('Ctrl Pts',(-19.3561969576373,-12.7684486149253,
124.634949144309)) ;
#57996 = CARTESIAN_POINT('Ctrl Pts',(-19.8693844497185,-12.9684202860083,
124.871533418394)) ;
#57997 = CARTESIAN_POINT('Ctrl Pts',(-19.7773692207012,-12.7884312056454,
124.579587326227)) ;
#57998 = CARTESIAN_POINT('Ctrl Pts',(-20.3384447754671,-12.9883029399995,
124.627871581349)) ;
#57999 = CARTESIAN_POINT('Ctrl Pts',(-20.1526165530644,-12.8083138596367,
124.384654591439)) ;
#58000 = CARTESIAN_POINT('Ctrl Pts',(-20.6976976848122,-13.0082611848626,
124.237731507644)) ;
#58001 = CARTESIAN_POINT('Ctrl Pts',(-20.4400164509615,-12.8282721044997,
124.072539967842)) ;
#58002 = CARTESIAN_POINT('Ctrl Pts',(-20.9017768869257,-13.0281367719042,
123.750397269444)) ;
#58003 = CARTESIAN_POINT('Ctrl Pts',(-20.6032766081325,-12.8481476915413,
123.682670590867)) ;
#58004 = CARTESIAN_POINT('Ctrl Pts',(-20.9278087943981,-13.0481176600395,
123.220011471926)) ;
#58005 = CARTESIAN_POINT('Ctrl Pts',(-20.6240984650254,-12.8681285796766,
123.258361753543)) ;
#58006 = CARTESIAN_POINT('Ctrl Pts',(-20.7712144053819,-13.0680528011505,
122.713763278227)) ;
#58007 = CARTESIAN_POINT('Ctrl Pts',(-20.4988186174616,-12.8880637207876,
122.853363994619)) ;
#58008 = CARTESIAN_POINT('Ctrl Pts',(-20.4520106816014,-13.0879648191615,
122.291696114272)) ;
#58009 = CARTESIAN_POINT('Ctrl Pts',(-20.2434545045575,-12.9079757387987,
122.515712746724)) ;
#58010 = CARTESIAN_POINT('Ctrl Pts',(-20.0087285877316,-13.1078530374051,
122.003722192709)) ;
#58011 = CARTESIAN_POINT('Ctrl Pts',(-19.8888179313836,-12.9278639570422,
122.285335578687)) ;
#58012 = CARTESIAN_POINT('Ctrl Pts',(-19.5791090604564,-13.124451341252,121.903703056221)) ;
#58013 = CARTESIAN_POINT('Ctrl Pts',(-19.5451473403849,-12.9444622608891,
122.20532771232)) ;
#58014 = CARTESIAN_POINT('Ctrl Pts',(-19.2304680801455,-13.1377239311548,
121.914976366624)) ;
#58015 = CARTESIAN_POINT('Ctrl Pts',(-19.2662110826215,-12.957734850792,122.214345972793)) ;
#58016 = CARTESIAN_POINT('Ctrl Pts',(-18.9730360739325,-13.1477313461057,
121.968723010403)) ;
#58017 = CARTESIAN_POINT('Ctrl Pts',(-19.0602727214037,-12.9677422657428,
122.25734421058)) ;
#58018 = CARTESIAN_POINT('Ctrl Pts',(-18.7289237747832,-13.1577386928383,
122.066570256317)) ;
#58019 = CARTESIAN_POINT('Ctrl Pts',(-18.8649743141328,-12.9777496124754,
122.335631001214)) ;
#58020 = CARTESIAN_POINT('Ctrl Pts',(-18.4326373531694,-13.1710050526399,
122.250316913842)) ;
#58021 = CARTESIAN_POINT('Ctrl Pts',(-18.6279877739114,-12.991015972277,122.482594753417)) ;
#58022 = CARTESIAN_POINT('Ctrl Pts',(-18.1316373287835,-13.1875197102629,
122.569692622284)) ;
#58023 = CARTESIAN_POINT('Ctrl Pts',(-18.3871406493088,-13.0075306299,122.738147077933)) ;
#58024 = CARTESIAN_POINT('Ctrl Pts',(-17.9558681007045,-13.2041171435055,
122.974265631492)) ;
#58025 = CARTESIAN_POINT('Ctrl Pts',(-18.2465546550527,-13.0241280631426,
123.061762709622)) ;
#58026 = CARTESIAN_POINT('Ctrl Pts',(-17.9045373896821,-13.2174651406505,
123.321302564893)) ;
#58027 = CARTESIAN_POINT('Ctrl Pts',(-18.20548016203,-13.0374760602876,123.339423056025)) ;
#58028 = CARTESIAN_POINT('Ctrl Pts',(-17.9113737957956,-13.2273608950021,
123.581262925382)) ;
#58029 = CARTESIAN_POINT('Ctrl Pts',(-18.2109541050246,-13.0473718146392,
123.547385244145)) ;
#58030 = CARTESIAN_POINT('Ctrl Pts',(-17.9634088821012,-13.2373488489335,
123.838506352538)) ;
#58031 = CARTESIAN_POINT('Ctrl Pts',(-18.2525836755494,-13.0573597685706,
123.753181135679)) ;
#58032 = CARTESIAN_POINT('Ctrl Pts',(-18.0589349739684,-13.2473060726382,
124.082144873651)) ;
#58033 = CARTESIAN_POINT('Ctrl Pts',(-18.3290068212281,-13.0673169922753,
123.948090676495)) ;
#58034 = CARTESIAN_POINT('Ctrl Pts',(-18.1964661586106,-13.2573416191949,
124.307146372465)) ;
#58035 = CARTESIAN_POINT('Ctrl Pts',(-18.4390335973166,-13.077352538832,124.128090758229)) ;
#58036 = CARTESIAN_POINT('Ctrl Pts',(-18.3682700533626,-13.267228730471,124.502082982706)) ;
#58037 = CARTESIAN_POINT('Ctrl Pts',(-18.576478424902,-13.0872396501081,124.284038539208)) ;
#58038 = CARTESIAN_POINT('Ctrl Pts',(-18.573168600081,-13.2772201355718,124.666246335832)) ;
#58039 = CARTESIAN_POINT('Ctrl Pts',(-18.7403986257916,-13.0972310552089,
124.415367430382)) ;
#58040 = CARTESIAN_POINT('Ctrl Pts',(-18.8024527486924,-13.2871657567866,
124.791696662128)) ;
#58041 = CARTESIAN_POINT('Ctrl Pts',(-18.9238269941468,-13.1071766764237,
124.515725689855)) ;
#58042 = CARTESIAN_POINT('Ctrl Pts',(-19.0499707909462,-13.2971150050549,
124.87596822317)) ;
#58043 = CARTESIAN_POINT('Ctrl Pts',(-19.1218420945713,-13.117125924692,124.58314078008)) ;
#58044 = CARTESIAN_POINT('Ctrl Pts',(-19.3109074952385,-13.3071615002235,
124.91606420447)) ;
#58045 = CARTESIAN_POINT('Ctrl Pts',(-19.3305917563602,-13.1271724198607,
124.615215324585)) ;
#58046 = CARTESIAN_POINT('Ctrl Pts',(-19.5697458477253,-13.3170128430151,
124.910614060128)) ;
#58047 = CARTESIAN_POINT('Ctrl Pts',(-19.5376622956873,-13.1370237626522,
124.610852953311)) ;
#58048 = CARTESIAN_POINT('Ctrl Pts',(-19.8268961278364,-13.3269846231424,
124.86034740168)) ;
#58049 = CARTESIAN_POINT('Ctrl Pts',(-19.7433819968767,-13.1469955427795,
124.570637436565)) ;
#58050 = CARTESIAN_POINT('Ctrl Pts',(-20.0720441858723,-13.3369798231201,
124.765921346646)) ;
#58051 = CARTESIAN_POINT('Ctrl Pts',(-19.9394995773028,-13.1569907427572,
124.495094521128)) ;
#58052 = CARTESIAN_POINT('Ctrl Pts',(-20.2977248332106,-13.3470138148161,
124.629595035348)) ;
#58053 = CARTESIAN_POINT('Ctrl Pts',(-20.1200429020722,-13.1670247344533,
124.386031555564)) ;
#58054 = CARTESIAN_POINT('Ctrl Pts',(-20.4930785404264,-13.3568692197886,
124.459519571124)) ;
#58055 = CARTESIAN_POINT('Ctrl Pts',(-20.2763242533844,-13.1768801394258,
124.2499696171)) ;
#58056 = CARTESIAN_POINT('Ctrl Pts',(-20.6585461151986,-13.3668685176344,
124.255447402342)) ;
#58057 = CARTESIAN_POINT('Ctrl Pts',(-20.4086965325383,-13.1868794372715,
124.086710531574)) ;
#58058 = CARTESIAN_POINT('Ctrl Pts',(-20.7850259763668,-13.3767636302396,
124.028196369691)) ;
#58059 = CARTESIAN_POINT('Ctrl Pts',(-20.509878386038,-13.1967745498767,123.904908812571)) ;
#58060 = CARTESIAN_POINT('Ctrl Pts',(-20.8714967332555,-13.3868242757746,
123.778389961119)) ;
#58061 = CARTESIAN_POINT('Ctrl Pts',(-20.5790529024792,-13.2068351954117,
123.705062936695)) ;
#58062 = CARTESIAN_POINT('Ctrl Pts',(-20.9125557494614,-13.3966731527638,
123.522828864941)) ;
#58063 = CARTESIAN_POINT('Ctrl Pts',(-20.6118978858686,-13.2166840724009,
123.500614018673)) ;
#58064 = CARTESIAN_POINT('Ctrl Pts',(-20.9092102411542,-13.4067018638574,
123.259309807964)) ;
#58065 = CARTESIAN_POINT('Ctrl Pts',(-20.60921931471,-13.2267127834945,123.289798833326)) ;
#58066 = CARTESIAN_POINT('Ctrl Pts',(-20.8594509750379,-13.4167312651135,
123.00048234628)) ;
#58067 = CARTESIAN_POINT('Ctrl Pts',(-20.5694097280133,-13.2367421847506,
123.082737285215)) ;
#58068 = CARTESIAN_POINT('Ctrl Pts',(-20.7678172835609,-13.4265714569095,
122.758667592175)) ;
#58069 = CARTESIAN_POINT('Ctrl Pts',(-20.4961008807738,-13.2465823765466,
122.889286615854)) ;
#58070 = CARTESIAN_POINT('Ctrl Pts',(-20.6338292437046,-13.4365748861025,
122.532528063033)) ;
#58071 = CARTESIAN_POINT('Ctrl Pts',(-20.3889086516706,-13.2565858057396,
122.708376145626)) ;
#58072 = CARTESIAN_POINT('Ctrl Pts',(-20.4628072717642,-13.4465603985687,
122.333446821148)) ;
#58073 = CARTESIAN_POINT('Ctrl Pts',(-20.2520895182278,-13.2665713182058,
122.549112622993)) ;
#58074 = CARTESIAN_POINT('Ctrl Pts',(-20.258572195235,-13.4566014949527,122.16640991458)) ;
#58075 = CARTESIAN_POINT('Ctrl Pts',(-20.0887000684384,-13.2766124145898,
122.415484760473)) ;
#58076 = CARTESIAN_POINT('Ctrl Pts',(-20.0331061121126,-13.4664446909037,
122.03957718795)) ;
#58077 = CARTESIAN_POINT('Ctrl Pts',(-19.9083265551085,-13.2864556105408,
122.314020659262)) ;
#58078 = CARTESIAN_POINT('Ctrl Pts',(-19.7857320971472,-13.4764310019581,
121.952101012445)) ;
#58079 = CARTESIAN_POINT('Ctrl Pts',(-19.7104267699532,-13.2964419215952,
122.2440417256)) ;
#58080 = CARTESIAN_POINT('Ctrl Pts',(-19.5282010411868,-13.4863656872158,
121.908939847016)) ;
#58081 = CARTESIAN_POINT('Ctrl Pts',(-19.5044018436985,-13.3063766068529,
122.209514865674)) ;
#58082 = CARTESIAN_POINT('Ctrl Pts',(-19.2639488168614,-13.4964232484328,
121.911409438826)) ;
#58083 = CARTESIAN_POINT('Ctrl Pts',(-19.2929999897462,-13.31643416807,122.211492628297)) ;
#58084 = CARTESIAN_POINT('Ctrl Pts',(-19.0100966675528,-13.5062448900414,
121.958214888149)) ;
#58085 = CARTESIAN_POINT('Ctrl Pts',(-19.0899192590891,-13.3262558096786,
122.248938879444)) ;
#58086 = CARTESIAN_POINT('Ctrl Pts',(-18.7623301682284,-13.5163009536324,
122.050058119956)) ;
#58087 = CARTESIAN_POINT('Ctrl Pts',(-18.8917066650352,-13.3363118732695,
122.322415354375)) ;
#58088 = CARTESIAN_POINT('Ctrl Pts',(-18.5371012425962,-13.5262416293942,
122.182417857288)) ;
#58089 = CARTESIAN_POINT('Ctrl Pts',(-18.7115247897244,-13.3462525490313,
122.428304768289)) ;
#58090 = CARTESIAN_POINT('Ctrl Pts',(-18.338478245611,-13.5361459881825,122.350628473911)) ;
#58091 = CARTESIAN_POINT('Ctrl Pts',(-18.5526279681694,-13.3561569078197,
122.562874462125)) ;
#58092 = CARTESIAN_POINT('Ctrl Pts',(-18.1698329826385,-13.5461926427583,
122.553733855565)) ;
#58093 = CARTESIAN_POINT('Ctrl Pts',(-18.4177132105659,-13.3662035623955,
122.725360081205)) ;
#58094 = CARTESIAN_POINT('Ctrl Pts',(-18.0407519036657,-13.5560882374012,
122.779526388176)) ;
#58095 = CARTESIAN_POINT('Ctrl Pts',(-18.314450248629,-13.3760991570383,122.905994658498)) ;
#58096 = CARTESIAN_POINT('Ctrl Pts',(-17.9513576421501,-13.5661501840581,
123.028342279855)) ;
#58097 = CARTESIAN_POINT('Ctrl Pts',(-18.2429366010411,-13.3861611036952,
123.105048152778)) ;
#58098 = CARTESIAN_POINT('Ctrl Pts',(-17.9074152113575,-13.5759998079902,
123.283436990171)) ;
#58099 = CARTESIAN_POINT('Ctrl Pts',(-18.2077846559609,-13.3960107276274,
123.30912358981)) ;
#58100 = CARTESIAN_POINT('Ctrl Pts',(-17.9075794490051,-13.5859630470201,
123.545245160118)) ;
#58101 = CARTESIAN_POINT('Ctrl Pts',(-18.2079178311045,-13.4059739666572,
123.518569875125)) ;
#58102 = CARTESIAN_POINT('Ctrl Pts',(-17.9538438452054,-13.5959876217959,
123.804601716854)) ;
#58103 = CARTESIAN_POINT('Ctrl Pts',(-18.2449311618866,-13.415998541433,123.726054822038)) ;
#58104 = CARTESIAN_POINT('Ctrl Pts',(-18.0433151854202,-13.6059061844836,
124.0494068293)) ;
#58105 = CARTESIAN_POINT('Ctrl Pts',(-18.3165097898856,-13.4259171041207,
123.921897880132)) ;
#58106 = CARTESIAN_POINT('Ctrl Pts',(-18.1745142883211,-13.6158983712076,
124.276882942804)) ;
#58107 = CARTESIAN_POINT('Ctrl Pts',(-18.4214705117975,-13.4359092908447,
124.103877785203)) ;
#58108 = CARTESIAN_POINT('Ctrl Pts',(-18.3442843563806,-13.6259331697918,
124.478655912716)) ;
#58109 = CARTESIAN_POINT('Ctrl Pts',(-18.5572880000568,-13.4459440894289,
124.265295042287)) ;
#58110 = CARTESIAN_POINT('Ctrl Pts',(-18.5426287178468,-13.6357883604655,
124.645217964009)) ;
#58111 = CARTESIAN_POINT('Ctrl Pts',(-18.7159640464026,-13.4557992801026,
124.398542876088)) ;
#58112 = CARTESIAN_POINT('Ctrl Pts',(-18.7699291705974,-13.6457877086185,
124.776978497853)) ;
#58113 = CARTESIAN_POINT('Ctrl Pts',(-18.8978051604027,-13.4657986282556,
124.503949791851)) ;
#58114 = CARTESIAN_POINT('Ctrl Pts',(-19.0140681533579,-13.6556828342936,
124.86662328346)) ;
#58115 = CARTESIAN_POINT('Ctrl Pts',(-19.0931163563245,-13.4756937539307,
124.57566388753)) ;
#58116 = CARTESIAN_POINT('Ctrl Pts',(-19.2742712713222,-13.6657433772417,
124.913241817981)) ;
#58117 = CARTESIAN_POINT('Ctrl Pts',(-19.3012793296211,-13.4857542968788,
124.612957136434)) ;
#58118 = CARTESIAN_POINT('Ctrl Pts',(-19.5331191647968,-13.6755926515086,
124.914103544901)) ;
#58119 = CARTESIAN_POINT('Ctrl Pts',(-19.5083568152058,-13.4956035711457,
124.613644905364)) ;
#58120 = CARTESIAN_POINT('Ctrl Pts',(-19.792878148494,-13.6856198760785,124.869872597639)) ;
#58121 = CARTESIAN_POINT('Ctrl Pts',(-19.7161637833577,-13.5056307957156,
124.578258678487)) ;
#58122 = CARTESIAN_POINT('Ctrl Pts',(-20.0408282968694,-13.6956482752663,
124.780544744153)) ;
#58123 = CARTESIAN_POINT('Ctrl Pts',(-19.9145234061736,-13.5156591949034,
124.506794855646)) ;
#58124 = CARTESIAN_POINT('Ctrl Pts',(-20.2655486146661,-13.7054940256798,
124.652339842706)) ;
#58125 = CARTESIAN_POINT('Ctrl Pts',(-20.0942981282645,-13.5255049453169,
124.404230053982)) ;
#58126 = CARTESIAN_POINT('Ctrl Pts',(-20.4679785318478,-13.7154828160805,
124.485209945321)) ;
#58127 = CARTESIAN_POINT('Ctrl Pts',(-20.2562410584806,-13.5354937357177,
124.270525177274)) ;
#58128 = CARTESIAN_POINT('Ctrl Pts',(-20.6387470354959,-13.7255277444802,
124.283933112254)) ;
#58129 = CARTESIAN_POINT('Ctrl Pts',(-20.3928547958644,-13.5455386641174,
124.109502630356)) ;
#58130 = CARTESIAN_POINT('Ctrl Pts',(-20.7695822850911,-13.7353522292692,
124.061344007578)) ;
#58131 = CARTESIAN_POINT('Ctrl Pts',(-20.4975212694255,-13.5553631489063,
123.931431547031)) ;
#58132 = CARTESIAN_POINT('Ctrl Pts',(-20.8622650301573,-13.7454096268104,
123.813853115559)) ;
#58133 = CARTESIAN_POINT('Ctrl Pts',(-20.5716663117887,-13.5654205464475,
123.733438175729)) ;
#58134 = CARTESIAN_POINT('Ctrl Pts',(-20.9096073544687,-13.7553357183966,
123.557318498504)) ;
#58135 = CARTESIAN_POINT('Ctrl Pts',(-20.6095387227254,-13.5753466380337,
123.528210720789)) ;
#58136 = CARTESIAN_POINT('Ctrl Pts',(-20.9123708210729,-13.7652905035412,
123.295734355723)) ;
#58137 = CARTESIAN_POINT('Ctrl Pts',(-20.6117482517937,-13.5853014231783,
123.318943754624)) ;
#58138 = CARTESIAN_POINT('Ctrl Pts',(-20.8690285856397,-13.7753278731988,
123.035549479101)) ;
#58139 = CARTESIAN_POINT('Ctrl Pts',(-20.5770731610732,-13.5953387928359,
123.110795969221)) ;
#58140 = CARTESIAN_POINT('Ctrl Pts',(-20.7826546061871,-13.7852166833204,
122.790448432935)) ;
#58141 = CARTESIAN_POINT('Ctrl Pts',(-20.5079730348007,-13.6052276029575,
122.914716243319)) ;
#58142 = CARTESIAN_POINT('Ctrl Pts',(-20.6541544832906,-13.7952060423715,
122.561546360115)) ;
#58143 = CARTESIAN_POINT('Ctrl Pts',(-20.4051720120301,-13.6152169620086,
122.731595301545)) ;
#58144 = CARTESIAN_POINT('Ctrl Pts',(-20.4882245281512,-13.8051645898276,
122.359184924028)) ;
#58145 = CARTESIAN_POINT('Ctrl Pts',(-20.2724273390847,-13.6251755094647,
122.569707182105)) ;
#58146 = CARTESIAN_POINT('Ctrl Pts',(-20.2912542115885,-13.8150641663786,
122.189215690163)) ;
#58147 = CARTESIAN_POINT('Ctrl Pts',(-20.1148509292206,-13.6350750860157,
122.433733053993)) ;
#58148 = CARTESIAN_POINT('Ctrl Pts',(-20.0644048944981,-13.8251120782093,
122.054135819925)) ;
#58149 = CARTESIAN_POINT('Ctrl Pts',(-19.9333707741338,-13.6451229978464,
122.325669994257)) ;
#58150 = CARTESIAN_POINT('Ctrl Pts',(-19.8213040212289,-13.8350074260699,
121.961702812424)) ;
#58151 = CARTESIAN_POINT('Ctrl Pts',(-19.7388903925254,-13.655018345707,122.251724810852)) ;
#58152 = CARTESIAN_POINT('Ctrl Pts',(-19.5616299165928,-13.845069102601,121.912040392459)) ;
#58153 = CARTESIAN_POINT('Ctrl Pts',(-19.5311506601532,-13.6650800222382,
122.211995830886)) ;
#58154 = CARTESIAN_POINT('Ctrl Pts',(-19.302943765994,-13.8549136203502,121.908260248801)) ;
#58155 = CARTESIAN_POINT('Ctrl Pts',(-19.3242027824673,-13.6749245399873,
122.208972745531)) ;
#58156 = CARTESIAN_POINT('Ctrl Pts',(-19.0443926106772,-13.864874064065,121.949016797608)) ;
#58157 = CARTESIAN_POINT('Ctrl Pts',(-19.1173623421421,-13.6848849837021,
122.241578712485)) ;
#58158 = CARTESIAN_POINT('Ctrl Pts',(-18.7951065533296,-13.8749108968832,
122.035163624274)) ;
#58159 = CARTESIAN_POINT('Ctrl Pts',(-18.9179336758563,-13.6949218165203,
122.310497076572)) ;
#58160 = CARTESIAN_POINT('Ctrl Pts',(-18.5679607592807,-13.88478969363,122.160911880469)) ;
#58161 = CARTESIAN_POINT('Ctrl Pts',(-18.7362182015604,-13.7048006132671,
122.411095961693)) ;
#58162 = CARTESIAN_POINT('Ctrl Pts',(-18.3623992980865,-13.8948490097584,
122.327074678705)) ;
#58163 = CARTESIAN_POINT('Ctrl Pts',(-18.5717693261378,-13.7148599293955,
122.544026976484)) ;
#58164 = CARTESIAN_POINT('Ctrl Pts',(-18.1920392191495,-13.9047194565116,
122.522692233472)) ;
#58165 = CARTESIAN_POINT('Ctrl Pts',(-18.4354824658003,-13.7247303761487,
122.700520842774)) ;
#58166 = CARTESIAN_POINT('Ctrl Pts',(-18.0559754687445,-13.9147120947696,
122.747289602296)) ;
#58167 = CARTESIAN_POINT('Ctrl Pts',(-18.3266320713964,-13.7347230144067,
122.880198925302)) ;
#58168 = CARTESIAN_POINT('Ctrl Pts',(-17.9611352243635,-13.9247441103175,
122.993260746216)) ;
#58169 = CARTESIAN_POINT('Ctrl Pts',(-18.2507605487093,-13.7447550299547,
123.076976202334)) ;
#58170 = CARTESIAN_POINT('Ctrl Pts',(-17.9107237978205,-13.9346099666241,
123.247603809028)) ;
#58171 = CARTESIAN_POINT('Ctrl Pts',(-18.210432205314,-13.7546208862612,123.280449806178)) ;
#58172 = CARTESIAN_POINT('Ctrl Pts',(-17.9051038745564,-13.9446792560932,
123.512124786768)) ;
#58173 = CARTESIAN_POINT('Ctrl Pts',(-18.2059368701527,-13.7646901757304,
123.492066934925)) ;
#58174 = CARTESIAN_POINT('Ctrl Pts',(-17.9445700338335,-13.9545228136445,
123.767790796992)) ;
#58175 = CARTESIAN_POINT('Ctrl Pts',(-18.2375102230327,-13.7745337332817,
123.696598534101)) ;
#58176 = CARTESIAN_POINT('Ctrl Pts',(-18.0281629110103,-13.9645029404324,
124.016370584098)) ;
#58177 = CARTESIAN_POINT('Ctrl Pts',(-18.3043848156925,-13.7845138600695,
123.895462003248)) ;
#58178 = CARTESIAN_POINT('Ctrl Pts',(-18.1545752563571,-13.9745214890323,
124.247305606012)) ;
#58179 = CARTESIAN_POINT('Ctrl Pts',(-18.4055151504625,-13.7945324086694,
124.080209779767)) ;
#58180 = CARTESIAN_POINT('Ctrl Pts',(-18.3165363213439,-13.9844047895555,
124.450385027953)) ;
#58181 = CARTESIAN_POINT('Ctrl Pts',(-18.535083750399,-13.8044157091926,124.242672395031)) ;
#58182 = CARTESIAN_POINT('Ctrl Pts',(-18.5149631927261,-13.9944730766036,
124.625337357405)) ;
#58183 = CARTESIAN_POINT('Ctrl Pts',(-18.6938257640231,-13.8144839962408,
124.382634169633)) ;
#58184 = CARTESIAN_POINT('Ctrl Pts',(-18.7353286473751,-14.0043031996223,
124.760223493667)) ;
#58185 = CARTESIAN_POINT('Ctrl Pts',(-18.8701172488312,-13.8243141192594,
124.49054215336)) ;
#58186 = CARTESIAN_POINT('Ctrl Pts',(-18.9813430292803,-14.0143697835476,
124.857357794633)) ;
#58187 = CARTESIAN_POINT('Ctrl Pts',(-19.0669291407156,-13.8343807031847,
124.568249482507)) ;
#58188 = CARTESIAN_POINT('Ctrl Pts',(-19.2360505050157,-14.0242598965621,
124.909235187301)) ;
#58189 = CARTESIAN_POINT('Ctrl Pts',(-19.2706943553894,-13.8442708161992,
124.60975094901)) ;
#58190 = CARTESIAN_POINT('Ctrl Pts',(-19.4985188781141,-14.0342525853247,
124.916724579482)) ;
#58191 = CARTESIAN_POINT('Ctrl Pts',(-19.4806688914999,-13.8542635049618,
124.615742311681)) ;
#58192 = CARTESIAN_POINT('Ctrl Pts',(-19.7574815058424,-14.0442134736805,
124.878462065094)) ;
#58193 = CARTESIAN_POINT('Ctrl Pts',(-19.6878385846522,-13.8642243933176,
124.585132166976)) ;
#58194 = CARTESIAN_POINT('Ctrl Pts',(-20.0049101277491,-14.0541314185605,
124.796606975513)) ;
#58195 = CARTESIAN_POINT('Ctrl Pts',(-19.8857808233358,-13.8741423381976,
124.519648232361)) ;
#58196 = CARTESIAN_POINT('Ctrl Pts',(-20.2366270328514,-14.0641391716567,
124.672163407092)) ;
#58197 = CARTESIAN_POINT('Ctrl Pts',(-20.0711543039772,-13.8841500912938,
124.420093397815)) ;
#58198 = CARTESIAN_POINT('Ctrl Pts',(-20.4433359395377,-14.0741702656157,
124.508602153767)) ;
#58199 = CARTESIAN_POINT('Ctrl Pts',(-20.2365214217928,-13.8941811852529,
124.289244226254)) ;
#58200 = CARTESIAN_POINT('Ctrl Pts',(-20.6157637308144,-14.0840182336437,
124.315591986878)) ;
#58201 = CARTESIAN_POINT('Ctrl Pts',(-20.3744629095565,-13.9040291532808,
124.134836941808)) ;
#58202 = CARTESIAN_POINT('Ctrl Pts',(-20.7551952257147,-14.0940801897696,
124.090948556963)) ;
#58203 = CARTESIAN_POINT('Ctrl Pts',(-20.4860083127366,-13.9140911094067,
123.955121992217)) ;
#58204 = CARTESIAN_POINT('Ctrl Pts',(-20.8516795936219,-14.1039774013707,
123.849406694872)) ;
#58205 = CARTESIAN_POINT('Ctrl Pts',(-20.5631955167448,-13.9239883210078,
123.761889246969)) ;
#58206 = CARTESIAN_POINT('Ctrl Pts',(-20.9057797422551,-14.1139085680353,
123.594099508417)) ;
#58207 = CARTESIAN_POINT('Ctrl Pts',(-20.6064757368551,-13.9339194876725,
123.557644109238)) ;
#58208 = CARTESIAN_POINT('Ctrl Pts',(-20.9145419978762,-14.1239507522395,
123.330350913867)) ;
#58209 = CARTESIAN_POINT('Ctrl Pts',(-20.6134856993466,-13.9439616718766,
123.346645072015)) ;
#58210 = CARTESIAN_POINT('Ctrl Pts',(-20.878134852128,-14.1338374204927,123.073090399106)) ;
#58211 = CARTESIAN_POINT('Ctrl Pts',(-20.5843603024591,-13.9538483401298,
123.140837492851)) ;
#58212 = CARTESIAN_POINT('Ctrl Pts',(-20.797171317607,-14.1438305324709,122.823288399636)) ;
#58213 = CARTESIAN_POINT('Ctrl Pts',(-20.5195898212087,-13.963841452108,122.940995952471)) ;
#58214 = CARTESIAN_POINT('Ctrl Pts',(-20.6745548235997,-14.1537762100867,
122.592473334251)) ;
#58215 = CARTESIAN_POINT('Ctrl Pts',(-20.4214971012033,-13.9737871297239,
122.756344186729)) ;
#58216 = CARTESIAN_POINT('Ctrl Pts',(-20.5141104749864,-14.1637235130717,
122.386083823547)) ;
#58217 = CARTESIAN_POINT('Ctrl Pts',(-20.2931422359031,-13.9837344327088,
122.591232683106)) ;
#58218 = CARTESIAN_POINT('Ctrl Pts',(-20.3181292651246,-14.1737712368185,
122.209146648077)) ;
#58219 = CARTESIAN_POINT('Ctrl Pts',(-20.1363573513922,-13.9937821564556,
122.449682552309)) ;
#58220 = CARTESIAN_POINT('Ctrl Pts',(-20.098946063385,-14.183619610581,122.071534647514)) ;
#58221 = CARTESIAN_POINT('Ctrl Pts',(-19.961011947168,-14.0036305302181,122.339593209163)) ;
#58222 = CARTESIAN_POINT('Ctrl Pts',(-19.8568324061559,-14.1935785830267,
121.972166958928)) ;
#58223 = CARTESIAN_POINT('Ctrl Pts',(-19.767321602057,-14.0135895026638,122.260098632269)) ;
#58224 = CARTESIAN_POINT('Ctrl Pts',(-19.5989991593622,-14.2036174449079,
121.916368996619)) ;
#58225 = CARTESIAN_POINT('Ctrl Pts',(-19.5610549871586,-14.023628364545,122.215459749838)) ;
#58226 = CARTESIAN_POINT('Ctrl Pts',(-19.339581937027,-14.2134960490797,121.905934350721)) ;
#58227 = CARTESIAN_POINT('Ctrl Pts',(-19.3535221269257,-14.0335069687168,
122.207111469005)) ;
#58228 = CARTESIAN_POINT('Ctrl Pts',(-19.0778376414756,-14.223547590283,121.941189793871)) ;
#58229 = CARTESIAN_POINT('Ctrl Pts',(-19.1441263879232,-14.0435585099201,
122.235315233814)) ;
#58230 = CARTESIAN_POINT('Ctrl Pts',(-18.8299973984445,-14.2334429882633,
122.020057862292)) ;
#58231 = CARTESIAN_POINT('Ctrl Pts',(-18.9458547296678,-14.0534539079004,
122.298408839437)) ;
#58232 = CARTESIAN_POINT('Ctrl Pts',(-18.5959941772312,-14.2434942208086,
122.142497343035)) ;
#58233 = CARTESIAN_POINT('Ctrl Pts',(-18.7586516520923,-14.0635051404457,
122.396359920337)) ;
#58234 = CARTESIAN_POINT('Ctrl Pts',(-18.3901717062413,-14.2533804114329,
122.301075810793)) ;
#58235 = CARTESIAN_POINT('Ctrl Pts',(-18.5939939275408,-14.07339133107,122.523221635957)) ;
#58236 = CARTESIAN_POINT('Ctrl Pts',(-18.2128046217201,-14.2633729507487,
122.494683384681)) ;
#58237 = CARTESIAN_POINT('Ctrl Pts',(-18.4520997745653,-14.0833838703858,
122.678107034334)) ;
#58238 = CARTESIAN_POINT('Ctrl Pts',(-18.0724208014174,-14.2733213966434,
122.715249428786)) ;
#58239 = CARTESIAN_POINT('Ctrl Pts',(-18.339792292697,-14.0933323162805,122.854559084059)) ;
#58240 = CARTESIAN_POINT('Ctrl Pts',(-17.9722554347127,-14.2832581991753,
122.956378922665)) ;
#58241 = CARTESIAN_POINT('Ctrl Pts',(-18.2596593906044,-14.1032691188124,
123.047461874324)) ;
#58242 = CARTESIAN_POINT('Ctrl Pts',(-17.9148800450432,-14.2932412066266,
123.212405357803)) ;
#58243 = CARTESIAN_POINT('Ctrl Pts',(-18.2137581989984,-14.1132521262637,
123.252282614946)) ;
#58244 = CARTESIAN_POINT('Ctrl Pts',(-17.9032450354326,-14.3032850480414,
123.476059954926)) ;
#58245 = CARTESIAN_POINT('Ctrl Pts',(-18.2044493516429,-14.1232959676785,
123.463206407145)) ;
#58246 = CARTESIAN_POINT('Ctrl Pts',(-17.9362327116183,-14.3131132466653,
123.732259863028)) ;
#58247 = CARTESIAN_POINT('Ctrl Pts',(-18.2308383754507,-14.1331241663024,
123.668165314127)) ;
#58248 = CARTESIAN_POINT('Ctrl Pts',(-18.0150012319065,-14.3231898401075,
123.985018013429)) ;
#58249 = CARTESIAN_POINT('Ctrl Pts',(-18.2938523322178,-14.1432007597447,
123.870372464175)) ;
#58250 = CARTESIAN_POINT('Ctrl Pts',(-18.1336866675862,-14.3330418394491,
124.215176688599)) ;
#58251 = CARTESIAN_POINT('Ctrl Pts',(-18.3887993080397,-14.1530527590862,
124.054499001948)) ;
#58252 = CARTESIAN_POINT('Ctrl Pts',(-18.2938233161721,-14.343115426273,124.425914520946)) ;
#58253 = CARTESIAN_POINT('Ctrl Pts',(-18.5169079559941,-14.1631263459101,
124.223090181388)) ;
#58254 = CARTESIAN_POINT('Ctrl Pts',(-18.4837016929012,-14.3529556513705,
124.601492972209)) ;
#58255 = CARTESIAN_POINT('Ctrl Pts',(-18.6688091616826,-14.1729665710076,
124.363553020106)) ;
#58256 = CARTESIAN_POINT('Ctrl Pts',(-18.703416961841,-14.3629213553991,124.743969337012)) ;
#58257 = CARTESIAN_POINT('Ctrl Pts',(-18.844580419153,-14.1829322750362,124.47753501832)) ;
#58258 = CARTESIAN_POINT('Ctrl Pts',(-18.946190326884,-14.3729479887057,124.846418837597)) ;
#58259 = CARTESIAN_POINT('Ctrl Pts',(-19.0387986926441,-14.1929589083428,
124.559495739056)) ;
#58260 = CARTESIAN_POINT('Ctrl Pts',(-19.2001264119849,-14.3828622844175,
124.904667897107)) ;
#58261 = CARTESIAN_POINT('Ctrl Pts',(-19.2419467128813,-14.2028732040546,
124.60609605546)) ;
#58262 = CARTESIAN_POINT('Ctrl Pts',(-19.4622585243968,-14.39285057311,124.918515058784)) ;
#58263 = CARTESIAN_POINT('Ctrl Pts',(-19.4516521770258,-14.2128614927471,
124.617175109609)) ;
#58264 = CARTESIAN_POINT('Ctrl Pts',(-19.7240472766002,-14.4028893062683,
124.886002641431)) ;
#58265 = CARTESIAN_POINT('Ctrl Pts',(-19.6610834379714,-14.2229002259054,
124.591166382665)) ;
#58266 = CARTESIAN_POINT('Ctrl Pts',(-19.9714422784701,-14.4127326380959,
124.810452799983)) ;
#58267 = CARTESIAN_POINT('Ctrl Pts',(-19.8589988887457,-14.232743557733,124.530728061937)) ;
#58268 = CARTESIAN_POINT('Ctrl Pts',(-20.2065561510804,-14.4227603639755,
124.691438006509)) ;
#58269 = CARTESIAN_POINT('Ctrl Pts',(-20.0470906952005,-14.2427712836126,
124.435517495806)) ;
#58270 = CARTESIAN_POINT('Ctrl Pts',(-20.4171057819061,-14.432792700364,124.532757562362)) ;
#58271 = CARTESIAN_POINT('Ctrl Pts',(-20.2155312378511,-14.2528036200011,
124.308574138805)) ;
#58272 = CARTESIAN_POINT('Ctrl Pts',(-20.5936350310893,-14.4426222006646,
124.34420163555)) ;
#58273 = CARTESIAN_POINT('Ctrl Pts',(-20.3567549741227,-14.2626331203018,
124.15773110315)) ;
#58274 = CARTESIAN_POINT('Ctrl Pts',(-20.7377126082824,-14.4526117045814,
124.124750610571)) ;
#58275 = CARTESIAN_POINT('Ctrl Pts',(-20.4720182693449,-14.2726226242185,
123.982171262254)) ;
#58276 = CARTESIAN_POINT('Ctrl Pts',(-20.8414417058682,-14.4626555450938,
123.882049023559)) ;
#58277 = CARTESIAN_POINT('Ctrl Pts',(-20.5550029138087,-14.2826664647309,
123.788010448594)) ;
#58278 = CARTESIAN_POINT('Ctrl Pts',(-20.900648035962,-14.4724772508619,123.63082704311)) ;
#58279 = CARTESIAN_POINT('Ctrl Pts',(-20.602369249548,-14.292488170499,123.587034187836)) ;
#58280 = CARTESIAN_POINT('Ctrl Pts',(-20.9162986354435,-14.4825122979942,
123.367582647658)) ;
#58281 = CARTESIAN_POINT('Ctrl Pts',(-20.6148913940102,-14.3025232176314,
123.376438685901)) ;
#58282 = CARTESIAN_POINT('Ctrl Pts',(-20.8853105895479,-14.4925369754311,
123.105964149167)) ;
#58283 = CARTESIAN_POINT('Ctrl Pts',(-20.5901024698145,-14.3125478950683,
123.167143688753)) ;
#58284 = CARTESIAN_POINT('Ctrl Pts',(-20.8111959911623,-14.5023897902856,
122.85787673168)) ;
#58285 = CARTESIAN_POINT('Ctrl Pts',(-20.5308125817991,-14.3224007099227,
122.96867405913)) ;
#58286 = CARTESIAN_POINT('Ctrl Pts',(-20.6939628548545,-14.5123774998931,
122.623068574786)) ;
#58287 = CARTESIAN_POINT('Ctrl Pts',(-20.4370276691554,-14.3323884195303,
122.780826900379)) ;
#58288 = CARTESIAN_POINT('Ctrl Pts',(-20.5386353139162,-14.5223075098872,
122.413370344863)) ;
#58289 = CARTESIAN_POINT('Ctrl Pts',(-20.3127672606121,-14.3423184295243,
122.613067632083)) ;
#58290 = CARTESIAN_POINT('Ctrl Pts',(-20.3483991859879,-14.5322972651064,
122.232456679631)) ;
#58291 = CARTESIAN_POINT('Ctrl Pts',(-20.1605796814699,-14.3523081847435,
122.468335499922)) ;
#58292 = CARTESIAN_POINT('Ctrl Pts',(-20.1286457021689,-14.5423238737893,
122.087070807904)) ;
#58293 = CARTESIAN_POINT('Ctrl Pts',(-19.9847778210034,-14.3623347934264,
122.352025351931)) ;
#58294 = CARTESIAN_POINT('Ctrl Pts',(-19.8905327192245,-14.5522078138111,
121.983318872916)) ;
#58295 = CARTESIAN_POINT('Ctrl Pts',(-19.7942886798817,-14.3722187334482,
122.269022420981)) ;
#58296 = CARTESIAN_POINT('Ctrl Pts',(-19.635462587809,-14.5621970413496,121.921242080345)) ;
#58297 = CARTESIAN_POINT('Ctrl Pts',(-19.5902331362649,-14.3822079609867,
122.219359208042)) ;
#58298 = CARTESIAN_POINT('Ctrl Pts',(-19.3720577988296,-14.5722399118733,
121.904853033029)) ;
#58299 = CARTESIAN_POINT('Ctrl Pts',(-19.3795093430328,-14.3922508315104,
122.206246194466)) ;
#58300 = CARTESIAN_POINT('Ctrl Pts',(-19.1152596800331,-14.5820722986287,
121.933419317847)) ;
#58301 = CARTESIAN_POINT('Ctrl Pts',(-19.1740714024378,-14.4020832182658,
122.229097307701)) ;
#58302 = CARTESIAN_POINT('Ctrl Pts',(-18.8630536665113,-14.5920655918003,
122.006599511882)) ;
#58303 = CARTESIAN_POINT('Ctrl Pts',(-18.9723061434464,-14.4120765114374,
122.287639558264)) ;
#58304 = CARTESIAN_POINT('Ctrl Pts',(-18.6267003875226,-14.6020975974487,
122.123410637976)) ;
#58305 = CARTESIAN_POINT('Ctrl Pts',(-18.7832226648472,-14.4221085170859,
122.38108679379)) ;
#58306 = CARTESIAN_POINT('Ctrl Pts',(-18.4175822404663,-14.6119628534177,
122.276618419926)) ;
#58307 = CARTESIAN_POINT('Ctrl Pts',(-18.61592748227,-14.4319737730548,122.503651126042)) ;
#58308 = CARTESIAN_POINT('Ctrl Pts',(-18.2359363520061,-14.6219247333252,
122.465143513999)) ;
#58309 = CARTESIAN_POINT('Ctrl Pts',(-18.4706094571108,-14.4419356529623,
122.654469655171)) ;
#58310 = CARTESIAN_POINT('Ctrl Pts',(-18.0890820796082,-14.6319596666871,
122.684159241081)) ;
#58311 = CARTESIAN_POINT('Ctrl Pts',(-18.3531243943116,-14.4519705863242,
122.829681166478)) ;
#58312 = CARTESIAN_POINT('Ctrl Pts',(-17.9836588830903,-14.6418446250664,
122.921611991648)) ;
#58313 = CARTESIAN_POINT('Ctrl Pts',(-18.2687841767101,-14.4618555447035,
123.019642136378)) ;
#58314 = CARTESIAN_POINT('Ctrl Pts',(-17.91999930049,-14.6519102519891,123.178306439075)) ;
#58315 = CARTESIAN_POINT('Ctrl Pts',(-18.217854528994,-14.4719211716262,123.224997325049)) ;
#58316 = CARTESIAN_POINT('Ctrl Pts',(-17.9020169238166,-14.6617493576534,
123.43628455332)) ;
#58317 = CARTESIAN_POINT('Ctrl Pts',(-18.2034666313559,-14.4817602772905,
123.431379111336)) ;
#58318 = CARTESIAN_POINT('Ctrl Pts',(-17.9293579840825,-14.6718121726588,
123.699271479237)) ;
#58319 = CARTESIAN_POINT('Ctrl Pts',(-18.2253374197392,-14.4918230922959,
123.641768973016)) ;
#58320 = CARTESIAN_POINT('Ctrl Pts',(-18.0009916819233,-14.6817083787074,
123.949301617982)) ;
#58321 = CARTESIAN_POINT('Ctrl Pts',(-18.2826422983745,-14.5017192983446,
123.841793287146)) ;
#58322 = CARTESIAN_POINT('Ctrl Pts',(-18.1147854788541,-14.6916492017327,
124.184415931245)) ;
#58323 = CARTESIAN_POINT('Ctrl Pts',(-18.3736753208548,-14.5116601213698,
124.029885468125)) ;
#58324 = CARTESIAN_POINT('Ctrl Pts',(-18.2686378473878,-14.7016537847114,
124.397645063482)) ;
#58325 = CARTESIAN_POINT('Ctrl Pts',(-18.4967554534644,-14.5216647043485,
124.200469975829)) ;
#58326 = CARTESIAN_POINT('Ctrl Pts',(-18.4576820792314,-14.7116746791561,
124.580965224182)) ;
#58327 = CARTESIAN_POINT('Ctrl Pts',(-18.6479893550732,-14.5316855987932,
124.347127597631)) ;
#58328 = CARTESIAN_POINT('Ctrl Pts',(-18.6727084410143,-14.7215665997455,
124.72705053099)) ;
#58329 = CARTESIAN_POINT('Ctrl Pts',(-18.8200089755962,-14.5415775193826,
124.463997424165)) ;
#58330 = CARTESIAN_POINT('Ctrl Pts',(-18.9120984381462,-14.7315600320909,
124.835009694246)) ;
#58331 = CARTESIAN_POINT('Ctrl Pts',(-19.0115200042416,-14.551570951728,124.55036669427)) ;
#58332 = CARTESIAN_POINT('Ctrl Pts',(-19.1654082297074,-14.7415056369908,
124.899373825222)) ;
#58333 = CARTESIAN_POINT('Ctrl Pts',(-19.2141671271123,-14.5615165566279,
124.601860046211)) ;
#58334 = CARTESIAN_POINT('Ctrl Pts',(-19.4260649276626,-14.7514529104723,
124.919311654018)) ;
#58335 = CARTESIAN_POINT('Ctrl Pts',(-19.4226921583559,-14.5714638301094,
124.617812487927)) ;
#58336 = CARTESIAN_POINT('Ctrl Pts',(-19.6888039980346,-14.7615008249487,
124.893135998467)) ;
#58337 = CARTESIAN_POINT('Ctrl Pts',(-19.6328836382695,-14.5815117445858,
124.596874129132)) ;
#58338 = CARTESIAN_POINT('Ctrl Pts',(-19.9380105597305,-14.771348465296,124.823369065413)) ;
#58339 = CARTESIAN_POINT('Ctrl Pts',(-19.8322491726103,-14.5913593849331,
124.541062779856)) ;
#58340 = CARTESIAN_POINT('Ctrl Pts',(-20.1743610165879,-14.7813101806726,
124.710840541122)) ;
#58341 = CARTESIAN_POINT('Ctrl Pts',(-20.0213304109851,-14.6013211003097,
124.451042024514)) ;
#58342 = CARTESIAN_POINT('Ctrl Pts',(-20.3888445239229,-14.7913388042454,
124.557674697892)) ;
#58343 = CARTESIAN_POINT('Ctrl Pts',(-20.1929184772654,-14.6113497238825,
124.32851117537)) ;
#58344 = CARTESIAN_POINT('Ctrl Pts',(-20.5713377846761,-14.8012491663118,
124.371890859621)) ;
#58345 = CARTESIAN_POINT('Ctrl Pts',(-20.3389145561169,-14.6212600859489,
124.179885784323)) ;
#58346 = CARTESIAN_POINT('Ctrl Pts',(-20.7197431781313,-14.8111838599642,
124.157087470465)) ;
#58347 = CARTESIAN_POINT('Ctrl Pts',(-20.457640661641,-14.6311947796013,124.008044437838)) ;
#58348 = CARTESIAN_POINT('Ctrl Pts',(-20.8295234845104,-14.8212257030921,
123.917131743842)) ;
#58349 = CARTESIAN_POINT('Ctrl Pts',(-20.5454669287708,-14.6412366227292,
123.816080822821)) ;
#58350 = CARTESIAN_POINT('Ctrl Pts',(-20.8951642259537,-14.8311102086625,
123.665780824477)) ;
#58351 = CARTESIAN_POINT('Ctrl Pts',(-20.5979816634709,-14.6511211282996,
123.615000778527)) ;
#58352 = CARTESIAN_POINT('Ctrl Pts',(-20.9167156314067,-14.8411123124477,
123.40385951735)) ;
#58353 = CARTESIAN_POINT('Ctrl Pts',(-20.6152250273271,-14.6611232320848,
123.405463971272)) ;
#58354 = CARTESIAN_POINT('Ctrl Pts',(-20.8928717590869,-14.8510306638627,
123.144264974598)) ;
#58355 = CARTESIAN_POINT('Ctrl Pts',(-20.5961521920614,-14.6710415834998,
123.197788211826)) ;
#58356 = CARTESIAN_POINT('Ctrl Pts',(-20.8233784416685,-14.8610783198836,
122.889574983756)) ;
#58357 = CARTESIAN_POINT('Ctrl Pts',(-20.5405596778779,-14.6810892395207,
122.994035641784)) ;
#58358 = CARTESIAN_POINT('Ctrl Pts',(-20.7129195792152,-14.8709495129118,
122.65480303298)) ;
#58359 = CARTESIAN_POINT('Ctrl Pts',(-20.4521948362717,-14.6909604325489,
122.806217311393)) ;
#58360 = CARTESIAN_POINT('Ctrl Pts',(-20.5605298604237,-14.8810152260553,
122.438669790613)) ;
#58361 = CARTESIAN_POINT('Ctrl Pts',(-20.330284230218,-14.7010261456924,122.633308925959)) ;
#58362 = CARTESIAN_POINT('Ctrl Pts',(-20.3770184511198,-14.890867686628,122.255919659017)) ;
#58363 = CARTESIAN_POINT('Ctrl Pts',(-20.1834793625096,-14.7108786062651,
122.487109277975)) ;
#58364 = CARTESIAN_POINT('Ctrl Pts',(-20.087542768723,-14.9042961493505,122.054287114174)) ;
#58365 = CARTESIAN_POINT('Ctrl Pts',(-19.9518873140162,-14.7243070689876,
122.325790630287)) ;
#58366 = CARTESIAN_POINT('Ctrl Pts',(-19.7606733441546,-14.9173770968676,
121.935403530529)) ;
#58367 = CARTESIAN_POINT('Ctrl Pts',(-19.6903664132712,-14.7373880165047,
122.230682365548)) ;
#58368 = CARTESIAN_POINT('Ctrl Pts',(-19.4080294143569,-14.9308515951022,
121.904239538084)) ;
#58369 = CARTESIAN_POINT('Ctrl Pts',(-19.408296278235,-14.7508625147393,122.205756669958)) ;
#58370 = CARTESIAN_POINT('Ctrl Pts',(-19.1506048230124,-14.9406836987116,
121.926886772641)) ;
#58371 = CARTESIAN_POINT('Ctrl Pts',(-19.2023472618255,-14.7606946183488,
122.223870633588)) ;
#58372 = CARTESIAN_POINT('Ctrl Pts',(-18.8974267387151,-14.9506496018383,
121.993755117999)) ;
#58373 = CARTESIAN_POINT('Ctrl Pts',(-18.9998068131851,-14.7706605214754,
122.277363288063)) ;
#58374 = CARTESIAN_POINT('Ctrl Pts',(-18.6583498545096,-14.9606770111485,
122.104643278367)) ;
#58375 = CARTESIAN_POINT('Ctrl Pts',(-18.8085430338256,-14.7806879307857,
122.366073028994)) ;
#58376 = CARTESIAN_POINT('Ctrl Pts',(-18.4446798401524,-14.9705880425151,
122.253516252991)) ;
#58377 = CARTESIAN_POINT('Ctrl Pts',(-18.6376088003778,-14.7905989621522,
122.485164544284)) ;
#58378 = CARTESIAN_POINT('Ctrl Pts',(-18.1971580268326,-14.9838323501362,
122.498300087744)) ;
#58379 = CARTESIAN_POINT('Ctrl Pts',(-18.4395744217537,-14.8038432697733,
122.681015310389)) ;
#58380 = CARTESIAN_POINT('Ctrl Pts',(-17.9735883960073,-15.0005328328073,
122.881645823256)) ;
#58381 = CARTESIAN_POINT('Ctrl Pts',(-18.2607334713096,-14.8205437524445,
122.987646040595)) ;
#58382 = CARTESIAN_POINT('Ctrl Pts',(-17.8949212635065,-15.0170396619631,
123.313331293313)) ;
#58383 = CARTESIAN_POINT('Ctrl Pts',(-18.197786980337,-14.8370505816002,123.333061833224)) ;
#58384 = CARTESIAN_POINT('Ctrl Pts',(-17.9226408363166,-15.0303502902007,
123.661981974254)) ;
#58385 = CARTESIAN_POINT('Ctrl Pts',(-18.2199642568686,-14.8503612098378,
123.611928568434)) ;
#58386 = CARTESIAN_POINT('Ctrl Pts',(-17.9885443792014,-15.0403428537408,
123.916213406476)) ;
#58387 = CARTESIAN_POINT('Ctrl Pts',(-18.2726848749169,-14.8603537733779,
123.815325758311)) ;
#58388 = CARTESIAN_POINT('Ctrl Pts',(-18.0982567045418,-15.0503729367423,
124.155839488556)) ;
#58389 = CARTESIAN_POINT('Ctrl Pts',(-18.3604503472436,-14.8703838563795,
124.007021726878)) ;
#58390 = CARTESIAN_POINT('Ctrl Pts',(-18.294281628791,-15.0635465407401,124.441261777876)) ;
#58391 = CARTESIAN_POINT('Ctrl Pts',(-18.5172815099474,-14.8835574603772,
124.235376257215)) ;
#58392 = CARTESIAN_POINT('Ctrl Pts',(-18.6299004804778,-15.0801842459715,
124.72893753815)) ;
#58393 = CARTESIAN_POINT('Ctrl Pts',(-18.785763290496,-14.9001951656086,124.465502997211)) ;
#58394 = CARTESIAN_POINT('Ctrl Pts',(-19.1244402677115,-15.1000660085389,
124.915683237853)) ;
#58395 = CARTESIAN_POINT('Ctrl Pts',(-19.1813811513845,-14.9200769281761,
124.614910725455)) ;
#58396 = CARTESIAN_POINT('Ctrl Pts',(-19.5680268436857,-15.1167623607554,
124.921075710828)) ;
#58397 = CARTESIAN_POINT('Ctrl Pts',(-19.5363048231766,-14.9367732803926,
124.619219761806)) ;
#58398 = CARTESIAN_POINT('Ctrl Pts',(-19.9032277012158,-15.1299193885445,
124.836006276955)) ;
#58399 = CARTESIAN_POINT('Ctrl Pts',(-19.804416663056,-14.9499303081817,124.551173733196)) ;
#58400 = CARTESIAN_POINT('Ctrl Pts',(-20.2240299227746,-15.1432967431881,
124.692326184051)) ;
#58401 = CARTESIAN_POINT('Ctrl Pts',(-20.0610789329257,-14.9633076628252,
124.436222806107)) ;
#58402 = CARTESIAN_POINT('Ctrl Pts',(-20.5648835408221,-15.1598275774469,
124.415004995461)) ;
#58403 = CARTESIAN_POINT('Ctrl Pts',(-20.33374952369,-14.979838497084,124.214377150155)) ;
#58404 = CARTESIAN_POINT('Ctrl Pts',(-20.8382356610329,-15.17979226719,123.960261264776)) ;
#58405 = CARTESIAN_POINT('Ctrl Pts',(-20.5524388724161,-14.9998031868271,
123.850580630537)) ;
#58406 = CARTESIAN_POINT('Ctrl Pts',(-20.9392779039823,-15.1997087606136,
123.440635012867)) ;
#58407 = CARTESIAN_POINT('Ctrl Pts',(-20.6332747129782,-15.0197196802507,
123.434880576487)) ;
#58408 = CARTESIAN_POINT('Ctrl Pts',(-20.8580805309166,-15.2195984799632,
122.918218801443)) ;
#58409 = CARTESIAN_POINT('Ctrl Pts',(-20.5683198928512,-15.0396093996003,
123.016946176903)) ;
#58410 = CARTESIAN_POINT('Ctrl Pts',(-20.6016712396196,-15.239605209611,122.45246543698)) ;
#58411 = CARTESIAN_POINT('Ctrl Pts',(-20.363194945236,-15.0596161292481,122.644342199294)) ;
#58412 = CARTESIAN_POINT('Ctrl Pts',(-20.2052118909962,-15.2594432632579,
122.104699832134)) ;
#58413 = CARTESIAN_POINT('Ctrl Pts',(-20.0460282780659,-15.079454182895,122.366126875178)) ;
#58414 = CARTESIAN_POINT('Ctrl Pts',(-19.7104197648505,-15.2794366014715,
121.911172706133)) ;
#58415 = CARTESIAN_POINT('Ctrl Pts',(-19.6501953671741,-15.0994475211086,
122.211302958785)) ;
#58416 = CARTESIAN_POINT('Ctrl Pts',(-19.1820210308814,-15.2993194008781,
121.898505004141)) ;
#58417 = CARTESIAN_POINT('Ctrl Pts',(-19.2274754164287,-15.1193303205152,
122.201166461084)) ;
#58418 = CARTESIAN_POINT('Ctrl Pts',(-18.6807320925926,-15.3192115817968,
122.06605896947)) ;
#58419 = CARTESIAN_POINT('Ctrl Pts',(-18.8264426177306,-15.1392225014339,
122.335208221256)) ;
#58420 = CARTESIAN_POINT('Ctrl Pts',(-18.2657076846686,-15.3391137602919,
122.394277865644)) ;
#58421 = CARTESIAN_POINT('Ctrl Pts',(-18.494421510302,-15.159124679929,122.597782896425)) ;
#58422 = CARTESIAN_POINT('Ctrl Pts',(-17.9866547281374,-15.3591510714956,
122.847707709371)) ;
#58423 = CARTESIAN_POINT('Ctrl Pts',(-18.2711780423566,-15.1791619911328,
122.960525608524)) ;
#58424 = CARTESIAN_POINT('Ctrl Pts',(-17.8794922157529,-15.3789635130365,
123.363506708324)) ;
#58425 = CARTESIAN_POINT('Ctrl Pts',(-18.1854465971545,-15.1989744326736,
123.373166586324)) ;
#58426 = CARTESIAN_POINT('Ctrl Pts',(-17.955834597053,-15.3990287537714,123.891058298143)) ;
#58427 = CARTESIAN_POINT('Ctrl Pts',(-18.2465194339574,-15.2190396734085,
123.795207317988)) ;
#58428 = CARTESIAN_POINT('Ctrl Pts',(-18.2036257717715,-15.4187859586272,
124.35431729337)) ;
#58429 = CARTESIAN_POINT('Ctrl Pts',(-18.444753257949,-15.2387968782644,124.165817334642)) ;
#58430 = CARTESIAN_POINT('Ctrl Pts',(-18.5991767273495,-15.4388192312729,
124.710349085039)) ;
#58431 = CARTESIAN_POINT('Ctrl Pts',(-18.7611938046602,-15.2588301509101,
124.450642577608)) ;
#58432 = CARTESIAN_POINT('Ctrl Pts',(-19.0875441524019,-15.4586321397268,
124.907957059452)) ;
#58433 = CARTESIAN_POINT('Ctrl Pts',(-19.1518899723408,-15.2786430593639,
124.608729644721)) ;
#58434 = CARTESIAN_POINT('Ctrl Pts',(-19.6183970906308,-15.4786282858542,
124.927914166445)) ;
#58435 = CARTESIAN_POINT('Ctrl Pts',(-19.576572466702,-15.2986392054913,124.62469458261)) ;
#58436 = CARTESIAN_POINT('Ctrl Pts',(-20.1213238855666,-15.4984900390767,
124.766723103207)) ;
#58437 = CARTESIAN_POINT('Ctrl Pts',(-19.9789150179613,-15.3185009587138,
124.495740310664)) ;
#58438 = CARTESIAN_POINT('Ctrl Pts',(-20.5429196526182,-15.5185585562048,
124.440174246411)) ;
#58439 = CARTESIAN_POINT('Ctrl Pts',(-20.3161903555175,-15.3385694758419,
124.234500854143)) ;
#58440 = CARTESIAN_POINT('Ctrl Pts',(-20.8242320696034,-15.5383894292016,
123.994315885912)) ;
#58441 = CARTESIAN_POINT('Ctrl Pts',(-20.5412403549953,-15.3584003488387,
123.877812029321)) ;
#58442 = CARTESIAN_POINT('Ctrl Pts',(-20.9383743235662,-15.5583113400183,
123.477399544044)) ;
#58443 = CARTESIAN_POINT('Ctrl Pts',(-20.6325525210197,-15.3783222596554,
123.464277746288)) ;
#58444 = CARTESIAN_POINT('Ctrl Pts',(-20.8690610707405,-15.5782407834536,
122.952175132017)) ;
#58445 = CARTESIAN_POINT('Ctrl Pts',(-20.5770999180587,-15.3982517030907,
123.044097841455)) ;
#58446 = CARTESIAN_POINT('Ctrl Pts',(-20.6251692263084,-15.59815045357,122.482655310939)) ;
#58447 = CARTESIAN_POINT('Ctrl Pts',(-20.3819841289406,-15.4181613732071,
122.668482232618)) ;
#58448 = CARTESIAN_POINT('Ctrl Pts',(-20.2369405024036,-15.6180238108329,
122.124408327086)) ;
#58449 = CARTESIAN_POINT('Ctrl Pts',(-20.0713986144983,-15.43803473047,122.381885868014)) ;
#58450 = CARTESIAN_POINT('Ctrl Pts',(-19.7469529682357,-15.6380153454508,
121.919076471871)) ;
#58451 = CARTESIAN_POINT('Ctrl Pts',(-19.6794074858345,-15.4580262650879,
122.217622870441)) ;
#58452 = CARTESIAN_POINT('Ctrl Pts',(-19.2195107524883,-15.6578809628615,
121.893213319316)) ;
#58453 = CARTESIAN_POINT('Ctrl Pts',(-19.257452611772,-15.4778918824987,122.196935186946)) ;
#58454 = CARTESIAN_POINT('Ctrl Pts',(-18.7119132760314,-15.6778618926898,
122.049260143643)) ;
#58455 = CARTESIAN_POINT('Ctrl Pts',(-18.8513754816871,-15.4978728123269,
122.321775691797)) ;
#58456 = CARTESIAN_POINT('Ctrl Pts',(-18.2892684219833,-15.6978003547729,
122.368964780256)) ;
#58457 = CARTESIAN_POINT('Ctrl Pts',(-18.513261161945,-15.51781127441,122.577542114275)) ;
#58458 = CARTESIAN_POINT('Ctrl Pts',(-18.0010412603232,-15.7176925479946,
122.812265657401)) ;
#58459 = CARTESIAN_POINT('Ctrl Pts',(-18.2826819358055,-15.5377034676318,
122.932185207393)) ;
#58460 = CARTESIAN_POINT('Ctrl Pts',(-17.8812058283193,-15.73766326303,123.329230583634)) ;
#58461 = CARTESIAN_POINT('Ctrl Pts',(-18.1868169736697,-15.5576741826671,
123.345758094485)) ;
#58462 = CARTESIAN_POINT('Ctrl Pts',(-17.9435942352086,-15.7574729346961,
123.852155946774)) ;
#58463 = CARTESIAN_POINT('Ctrl Pts',(-18.236731360586,-15.5774838543332,123.764098868335)) ;
#58464 = CARTESIAN_POINT('Ctrl Pts',(-18.1823832687672,-15.7774661513873,
124.326648974509)) ;
#58465 = CARTESIAN_POINT('Ctrl Pts',(-18.4277666392234,-15.5974770710244,
124.143691534973)) ;
#58466 = CARTESIAN_POINT('Ctrl Pts',(-18.5660086878683,-15.7973170635836,
124.689180060652)) ;
#58467 = CARTESIAN_POINT('Ctrl Pts',(-18.7346680390251,-15.6173279832208,
124.433713872996)) ;
#58468 = CARTESIAN_POINT('Ctrl Pts',(-19.0555605460036,-15.8173916699027,
124.900980308244)) ;
#58469 = CARTESIAN_POINT('Ctrl Pts',(-19.126318602416,-15.6374025895398,124.603150145415)) ;
#58470 = CARTESIAN_POINT('Ctrl Pts',(-19.493934124633,-15.833908301786,124.927054796924)) ;
#58471 = CARTESIAN_POINT('Ctrl Pts',(-19.4769939508857,-15.6539192214231,
124.62400662122)) ;
#58472 = CARTESIAN_POINT('Ctrl Pts',(-19.837342147255,-15.8472470094801,124.8571673599)) ;
#58473 = CARTESIAN_POINT('Ctrl Pts',(-19.7517415685983,-15.6672579291172,
124.568093350014)) ;
#58474 = CARTESIAN_POINT('Ctrl Pts',(-20.0781804979122,-15.8570893837884,
124.762739875852)) ;
#58475 = CARTESIAN_POINT('Ctrl Pts',(-19.9444057990373,-15.6771003034255,
124.492551480651)) ;
#58476 = CARTESIAN_POINT('Ctrl Pts',(-20.303796053823,-15.8671444037711,124.625272793233)) ;
#58477 = CARTESIAN_POINT('Ctrl Pts',(-20.1249049700663,-15.6871553234083,
124.38256759213)) ;
#58478 = CARTESIAN_POINT('Ctrl Pts',(-20.5648469001253,-15.8803765604287,
124.395495442102)) ;
#58479 = CARTESIAN_POINT('Ctrl Pts',(-20.333709310747,-15.7003874800658,124.198785755722)) ;
#58480 = CARTESIAN_POINT('Ctrl Pts',(-20.8101326079248,-15.8969915277738,
124.02832371329)) ;
#58481 = CARTESIAN_POINT('Ctrl Pts',(-20.5299755608498,-15.717002447411,123.904990049025)) ;
#58482 = CARTESIAN_POINT('Ctrl Pts',(-20.9150857051299,-15.913586114785,123.599951810518)) ;
#58483 = CARTESIAN_POINT('Ctrl Pts',(-20.6139164049773,-15.7335970344222,
123.562338490809)) ;
#58484 = CARTESIAN_POINT('Ctrl Pts',(-20.9083137993507,-15.9268196831404,
123.252228775196)) ;
#58485 = CARTESIAN_POINT('Ctrl Pts',(-20.6085033810929,-15.7468306027775,
123.28412879026)) ;
#58486 = CARTESIAN_POINT('Ctrl Pts',(-20.8574915953394,-15.9368633009491,
122.993254896173)) ;
#58487 = CARTESIAN_POINT('Ctrl Pts',(-20.5678420886449,-15.7568742205862,
123.076956586024)) ;
#58488 = CARTESIAN_POINT('Ctrl Pts',(-20.7640240610611,-15.9467502251839,
122.750807958911)) ;
#58489 = CARTESIAN_POINT('Ctrl Pts',(-20.4930658151328,-15.766761144821,122.88299771998)) ;
#58490 = CARTESIAN_POINT('Ctrl Pts',(-20.6288932481491,-15.9567408796307,
122.525730668388)) ;
#58491 = CARTESIAN_POINT('Ctrl Pts',(-20.3849611673798,-15.7767517992678,
122.702938858516)) ;
#58492 = CARTESIAN_POINT('Ctrl Pts',(-20.4571800169588,-15.9667026380847,
122.328129169805)) ;
#58493 = CARTESIAN_POINT('Ctrl Pts',(-20.2475814010665,-15.7867135577218,
122.544854090362)) ;
#58494 = CARTESIAN_POINT('Ctrl Pts',(-20.1849716448928,-15.9800425031519,
122.107130949398)) ;
#58495 = CARTESIAN_POINT('Ctrl Pts',(-20.0298503330428,-15.800053422789,122.368082503893)) ;
#58496 = CARTESIAN_POINT('Ctrl Pts',(-19.8618390549407,-15.9933512860652,
121.963354376013)) ;
#58497 = CARTESIAN_POINT('Ctrl Pts',(-19.7713258119905,-15.8133622057023,
122.25304504801)) ;
#58498 = CARTESIAN_POINT('Ctrl Pts',(-19.5194352459976,-16.0065470435093,
121.908483591951)) ;
#58499 = CARTESIAN_POINT('Ctrl Pts',(-19.4973853555819,-15.8265579631464,
122.209149363533)) ;
#58500 = CARTESIAN_POINT('Ctrl Pts',(-19.2576646411518,-16.0165089271858,
121.911843868139)) ;
#58501 = CARTESIAN_POINT('Ctrl Pts',(-19.2879723775728,-15.8365198468229,
122.211840251455)) ;
#58502 = CARTESIAN_POINT('Ctrl Pts',(-18.9984455353945,-16.0265520367004,
121.961426597411)) ;
#58503 = CARTESIAN_POINT('Ctrl Pts',(-19.0805966476983,-15.8465629563375,
122.251508536236)) ;
#58504 = CARTESIAN_POINT('Ctrl Pts',(-18.7563398527303,-16.0364042866996,
122.053197919852)) ;
#58505 = CARTESIAN_POINT('Ctrl Pts',(-18.8869132360213,-15.8564152063368,
122.324927701526)) ;
#58506 = CARTESIAN_POINT('Ctrl Pts',(-18.5308557513542,-16.0463758236501,
122.186642824529)) ;
#58507 = CARTESIAN_POINT('Ctrl Pts',(-18.7065271150843,-15.8663867432872,
122.431685506008)) ;
#58508 = CARTESIAN_POINT('Ctrl Pts',(-18.331455189681,-16.0563710891276,122.357680218404)) ;
#58509 = CARTESIAN_POINT('Ctrl Pts',(-18.5470081927436,-15.8763820087648,
122.568517085258)) ;
#58510 = CARTESIAN_POINT('Ctrl Pts',(-18.164426495201,-16.0664050620013,122.561684900348)) ;
#58511 = CARTESIAN_POINT('Ctrl Pts',(-18.4133869982469,-15.8864159816384,
122.731722236848)) ;
#58512 = CARTESIAN_POINT('Ctrl Pts',(-18.037271614364,-16.0762604767636,122.787340539645)) ;
#58513 = CARTESIAN_POINT('Ctrl Pts',(-18.3116651407134,-15.8962713964007,
122.912247684701)) ;
#58514 = CARTESIAN_POINT('Ctrl Pts',(-17.9496588451974,-16.0862597542724,
123.035027131255)) ;
#58515 = CARTESIAN_POINT('Ctrl Pts',(-18.2415770550694,-15.9062706739096,
123.110397634539)) ;
#58516 = CARTESIAN_POINT('Ctrl Pts',(-17.9065430994945,-16.0961549384354,
123.291508010341)) ;
#58517 = CARTESIAN_POINT('Ctrl Pts',(-18.2070866753849,-15.9161658580725,
123.315582497717)) ;
#58518 = CARTESIAN_POINT('Ctrl Pts',(-17.908679550301,-16.1062153180762,123.555839709386)) ;
#58519 = CARTESIAN_POINT('Ctrl Pts',(-18.2087980556812,-15.9262262377133,
123.527047864045)) ;
#58520 = CARTESIAN_POINT('Ctrl Pts',(-17.9555303866204,-16.1160651870843,
123.810434776852)) ;
#58521 = CARTESIAN_POINT('Ctrl Pts',(-18.246280837973,-15.9360761067214,123.730723208321)) ;
#58522 = CARTESIAN_POINT('Ctrl Pts',(-18.0469625663343,-16.1260967482922,
124.057672087697)) ;
#58523 = CARTESIAN_POINT('Ctrl Pts',(-18.3194286080762,-15.9461076679293,
123.928512283029)) ;
#58524 = CARTESIAN_POINT('Ctrl Pts',(-18.1801329408613,-16.1361071971745,
124.284566442434)) ;
#58525 = CARTESIAN_POINT('Ctrl Pts',(-18.4259667878995,-15.9561181168116,
124.110026615654)) ;
#58526 = CARTESIAN_POINT('Ctrl Pts',(-18.3486698658472,-16.1460139365915,
124.482977937529)) ;
#58527 = CARTESIAN_POINT('Ctrl Pts',(-18.560797834217,-15.9660248562286,124.26875420935)) ;
#58528 = CARTESIAN_POINT('Ctrl Pts',(-18.5494006644894,-16.1559519526599,
124.65002353466)) ;
#58529 = CARTESIAN_POINT('Ctrl Pts',(-18.7213836797502,-15.9759628722971,
124.402388898548)) ;
#58530 = CARTESIAN_POINT('Ctrl Pts',(-18.7775718601343,-16.1659571991111,
124.780727182674)) ;
#58531 = CARTESIAN_POINT('Ctrl Pts',(-18.9039216373305,-15.9859681187482,
124.506949936595)) ;
#58532 = CARTESIAN_POINT('Ctrl Pts',(-19.0257972538791,-16.1759912601674,
124.869646856981)) ;
#58533 = CARTESIAN_POINT('Ctrl Pts',(-19.1025026967416,-15.9960021798045,
124.578083637669)) ;
#58534 = CARTESIAN_POINT('Ctrl Pts',(-19.2807496064641,-16.1858363412255,
124.913723831211)) ;
#58535 = CARTESIAN_POINT('Ctrl Pts',(-19.3064644940587,-16.0058472608626,
124.613343042249)) ;
#58536 = CARTESIAN_POINT('Ctrl Pts',(-19.5431244270057,-16.195822147179,124.913341409534)) ;
#58537 = CARTESIAN_POINT('Ctrl Pts',(-19.5163642183528,-16.0158330668161,
124.61303502158)) ;
#58538 = CARTESIAN_POINT('Ctrl Pts',(-19.8002495182117,-16.2057569677332,
124.86781116894)) ;
#58539 = CARTESIAN_POINT('Ctrl Pts',(-19.7220636745429,-16.0257678873703,
124.576608849091)) ;
#58540 = CARTESIAN_POINT('Ctrl Pts',(-20.0484305675557,-16.2158144928654,
124.777029790826)) ;
#58541 = CARTESIAN_POINT('Ctrl Pts',(-19.9206078848616,-16.0358254125025,
124.503981752975)) ;
#58542 = CARTESIAN_POINT('Ctrl Pts',(-20.2719717473046,-16.2256361435168,
124.647952173762)) ;
#58543 = CARTESIAN_POINT('Ctrl Pts',(-20.0994392637093,-16.0456470631539,
124.40071820774)) ;
#58544 = CARTESIAN_POINT('Ctrl Pts',(-20.4747026404309,-16.2356922070215,
124.478471590715)) ;
#58545 = CARTESIAN_POINT('Ctrl Pts',(-20.2616227752683,-16.0557031266586,
124.265132163495)) ;
#58546 = CARTESIAN_POINT('Ctrl Pts',(-20.6426334922787,-16.2456328740854,
124.278356285801)) ;
#58547 = CARTESIAN_POINT('Ctrl Pts',(-20.395965720866,-16.0656437937226,124.105038812576)) ;
#58548 = CARTESIAN_POINT('Ctrl Pts',(-20.7734945781979,-16.2555372677514,
124.053362462488)) ;
#58549 = CARTESIAN_POINT('Ctrl Pts',(-20.5006527028132,-16.0755481873885,
123.925043150666)) ;
#58550 = CARTESIAN_POINT('Ctrl Pts',(-20.8644201156856,-16.2655837915144,
123.805527276489)) ;
#58551 = CARTESIAN_POINT('Ctrl Pts',(-20.5733913233788,-16.0855947111516,
123.726774248411)) ;
#58552 = CARTESIAN_POINT('Ctrl Pts',(-20.9104948421842,-16.2754798745308,
123.549534920301)) ;
#58553 = CARTESIAN_POINT('Ctrl Pts',(-20.6102491311177,-16.0954907941679,
123.521980487086)) ;
#58554 = CARTESIAN_POINT('Ctrl Pts',(-20.9113721563004,-16.2855465737608,
123.285041710437)) ;
#58555 = CARTESIAN_POINT('Ctrl Pts',(-20.6109490499967,-16.105557493398,123.310385748136)) ;
#58556 = CARTESIAN_POINT('Ctrl Pts',(-20.8676796982969,-16.2953701841619,
123.030571216678)) ;
#58557 = CARTESIAN_POINT('Ctrl Pts',(-20.5759933528988,-16.115381103799,123.106810427065)) ;
#58558 = CARTESIAN_POINT('Ctrl Pts',(-20.7788672822299,-16.3054260443394,
122.78172092023)) ;
#58559 = CARTESIAN_POINT('Ctrl Pts',(-20.5049416634882,-16.1254369639765,
122.907730678547)) ;
#58560 = CARTESIAN_POINT('Ctrl Pts',(-20.6494650621371,-16.3153591906443,
122.554983567681)) ;
#58561 = CARTESIAN_POINT('Ctrl Pts',(-20.4014184363261,-16.1353701102815,
122.726342029914)) ;
#58562 = CARTESIAN_POINT('Ctrl Pts',(-20.482907205734,-16.3253044464149,122.353620794924)) ;
#58563 = CARTESIAN_POINT('Ctrl Pts',(-20.2681709878727,-16.1453153660521,
122.565253212726)) ;
#58564 = CARTESIAN_POINT('Ctrl Pts',(-20.2832435137654,-16.3352877448534,
122.183387066587)) ;
#58565 = CARTESIAN_POINT('Ctrl Pts',(-20.1084390193321,-16.1552986644905,
122.42906766522)) ;
#58566 = CARTESIAN_POINT('Ctrl Pts',(-20.0556974557247,-16.345324925,122.050026596419)) ;
#58567 = CARTESIAN_POINT('Ctrl Pts',(-19.9264011931984,-16.1653358446372,
122.322380816789)) ;
#58568 = CARTESIAN_POINT('Ctrl Pts',(-19.8130492090875,-16.3551794777095,
121.959479734219)) ;
#58569 = CARTESIAN_POINT('Ctrl Pts',(-19.7322826766303,-16.1751903973466,
122.249945218267)) ;
#58570 = CARTESIAN_POINT('Ctrl Pts',(-19.5547543717417,-16.3651789961568,
121.911400782604)) ;
#58571 = CARTESIAN_POINT('Ctrl Pts',(-19.5256466039838,-16.185189915794,122.211483732283)) ;
#58572 = CARTESIAN_POINT('Ctrl Pts',(-19.2946925229401,-16.3750740786189,
121.908649507765)) ;
#58573 = CARTESIAN_POINT('Ctrl Pts',(-19.3175976958741,-16.195084998256,122.209284348646)) ;
#58574 = CARTESIAN_POINT('Ctrl Pts',(-19.0338948184868,-16.385134624125,121.951817978904)) ;
#58575 = CARTESIAN_POINT('Ctrl Pts',(-19.1089596094464,-16.2051455437621,
122.243820773441)) ;
#58576 = CARTESIAN_POINT('Ctrl Pts',(-18.7896903909749,-16.394983931373,122.037651600435)) ;
#58577 = CARTESIAN_POINT('Ctrl Pts',(-18.9135973885813,-16.2149948510101,
122.312488912832)) ;
#58578 = CARTESIAN_POINT('Ctrl Pts',(-18.5597221685601,-16.4050110214604,
122.166277137884)) ;
#58579 = CARTESIAN_POINT('Ctrl Pts',(-18.729623508621,-16.2250219410975,122.415390653368)) ;
#58580 = CARTESIAN_POINT('Ctrl Pts',(-18.3559738383633,-16.4150399255973,
122.333461717457)) ;
#58581 = CARTESIAN_POINT('Ctrl Pts',(-18.5666258270769,-16.2350508452344,
122.549139604119)) ;
#58582 = CARTESIAN_POINT('Ctrl Pts',(-18.1871403035161,-16.4248837906966,
122.529443722511)) ;
#58583 = CARTESIAN_POINT('Ctrl Pts',(-18.4315607383292,-16.2448947103337,
122.705925518047)) ;
#58584 = CARTESIAN_POINT('Ctrl Pts',(-18.0522973396058,-16.434879617405,122.754872248908)) ;
#58585 = CARTESIAN_POINT('Ctrl Pts',(-18.3236876314131,-16.2548905370421,
122.886268932754)) ;
#58586 = CARTESIAN_POINT('Ctrl Pts',(-17.9588203685943,-16.444904834054,123.001188739217)) ;
#58587 = CARTESIAN_POINT('Ctrl Pts',(-18.2489074300727,-16.2649157536911,
123.083322689755)) ;
#58588 = CARTESIAN_POINT('Ctrl Pts',(-17.909853990901,-16.4547946662116,123.256433493462)) ;
#58589 = CARTESIAN_POINT('Ctrl Pts',(-18.2097358498301,-16.2748055858487,
123.287518087541)) ;
#58590 = CARTESIAN_POINT('Ctrl Pts',(-17.9055514641145,-16.4647855222963,
123.518938743175)) ;
#58591 = CARTESIAN_POINT('Ctrl Pts',(-18.2062951731,-16.2847964419335,123.497522159626)) ;
#58592 = CARTESIAN_POINT('Ctrl Pts',(-17.9467544397181,-16.4747306168892,
123.777016725455)) ;
#58593 = CARTESIAN_POINT('Ctrl Pts',(-18.2392588287559,-16.2947415365263,
123.70398393257)) ;
#58594 = CARTESIAN_POINT('Ctrl Pts',(-18.0317409622789,-16.4846825206573,
124.02435926062)) ;
#58595 = CARTESIAN_POINT('Ctrl Pts',(-18.3072491056377,-16.3046934402944,
123.901857190127)) ;
#58596 = CARTESIAN_POINT('Ctrl Pts',(-18.1596521832206,-16.4947189201267,
124.255004193986)) ;
#58597 = CARTESIAN_POINT('Ctrl Pts',(-18.4095792698802,-16.3147298397639,
124.086372598792)) ;
#58598 = CARTESIAN_POINT('Ctrl Pts',(-18.3230928107259,-16.5046079902154,
124.45706017088)) ;
#58599 = CARTESIAN_POINT('Ctrl Pts',(-18.5403322885734,-16.3246189098525,
124.248016015903)) ;
#58600 = CARTESIAN_POINT('Ctrl Pts',(-18.5207993714946,-16.5145972795863,
124.62974295052)) ;
#58601 = CARTESIAN_POINT('Ctrl Pts',(-18.6984981684148,-16.3346081992234,
124.386161255533)) ;
#58602 = CARTESIAN_POINT('Ctrl Pts',(-18.7448946531672,-16.524555845796,124.764889240736)) ;
#58603 = CARTESIAN_POINT('Ctrl Pts',(-18.8777747171326,-16.3445667654331,
124.494277080252)) ;
#58604 = CARTESIAN_POINT('Ctrl Pts',(-18.9873964306672,-16.5344554170128,
124.859121187844)) ;
#58605 = CARTESIAN_POINT('Ctrl Pts',(-19.0717758652844,-16.3544663366499,
124.569661399205)) ;
#58606 = CARTESIAN_POINT('Ctrl Pts',(-19.2463751321028,-16.5445033314271,
124.910475054052)) ;
#58607 = CARTESIAN_POINT('Ctrl Pts',(-19.2789592074066,-16.3645142510642,
124.610743469147)) ;
#58608 = CARTESIAN_POINT('Ctrl Pts',(-19.5063926931676,-16.5543986742876,
124.916202482167)) ;
#58609 = CARTESIAN_POINT('Ctrl Pts',(-19.4869725482659,-16.3744095939248,
124.615324365784)) ;
#58610 = CARTESIAN_POINT('Ctrl Pts',(-19.7677103786567,-16.5644603682351,
124.876078188685)) ;
#58611 = CARTESIAN_POINT('Ctrl Pts',(-19.696026799547,-16.3844712878722,124.583223879591)) ;
#58612 = CARTESIAN_POINT('Ctrl Pts',(-20.0127402827111,-16.5743048213192,
124.793052261125)) ;
#58613 = CARTESIAN_POINT('Ctrl Pts',(-19.8920493950965,-16.3943157409564,
124.516802517793)) ;
#58614 = CARTESIAN_POINT('Ctrl Pts',(-20.2427297441495,-16.5842655062777,
124.668092227822)) ;
#58615 = CARTESIAN_POINT('Ctrl Pts',(-20.0760402661694,-16.4042764259148,
124.416833962095)) ;
#58616 = CARTESIAN_POINT('Ctrl Pts',(-20.4488151079738,-16.5943014387862,
124.503505578167)) ;
#58617 = CARTESIAN_POINT('Ctrl Pts',(-20.2409080798894,-16.4143123584233,
124.285163870932)) ;
#58618 = CARTESIAN_POINT('Ctrl Pts',(-20.6208188759846,-16.6041900544743,
124.308721850935)) ;
#58619 = CARTESIAN_POINT('Ctrl Pts',(-20.3785099279013,-16.4242009741114,
124.129336942414)) ;
#58620 = CARTESIAN_POINT('Ctrl Pts',(-20.7585722335098,-16.6142044636167,
124.084465548632)) ;
#58621 = CARTESIAN_POINT('Ctrl Pts',(-20.4887119985352,-16.4342153832538,
123.949931533889)) ;
#58622 = CARTESIAN_POINT('Ctrl Pts',(-20.8548321532337,-16.6242382725745,
123.839003471637)) ;
#58623 = CARTESIAN_POINT('Ctrl Pts',(-20.5657191556869,-16.4442491922116,
123.753561447325)) ;
#58624 = CARTESIAN_POINT('Ctrl Pts',(-20.9066678159083,-16.6340687268307,
123.585891332046)) ;
#58625 = CARTESIAN_POINT('Ctrl Pts',(-20.6071867566373,-16.4540796464678,
123.551072756513)) ;
#58626 = CARTESIAN_POINT('Ctrl Pts',(-20.9140293672991,-16.6441463944089,
123.321214560583)) ;
#58627 = CARTESIAN_POINT('Ctrl Pts',(-20.6130753215692,-16.464157314046,123.33933095717)) ;
#58628 = CARTESIAN_POINT('Ctrl Pts',(-20.8763072380744,-16.6539982625311,
123.065023312876)) ;
#58629 = CARTESIAN_POINT('Ctrl Pts',(-20.5828971286681,-16.4740091821683,
123.134379095039)) ;
#58630 = CARTESIAN_POINT('Ctrl Pts',(-20.7930831562176,-16.6640713000965,
122.81378563807)) ;
#58631 = CARTESIAN_POINT('Ctrl Pts',(-20.5163171841745,-16.4840822197336,
122.933388811495)) ;
#58632 = CARTESIAN_POINT('Ctrl Pts',(-20.6703077317123,-16.6739138534474,
122.586104119148)) ;
#58633 = CARTESIAN_POINT('Ctrl Pts',(-20.4180968468373,-16.4939247730845,
122.751244883158)) ;
#58634 = CARTESIAN_POINT('Ctrl Pts',(-20.5083311850613,-16.6838942489408,
122.3798384328)) ;
#58635 = CARTESIAN_POINT('Ctrl Pts',(-20.288515456469,-16.5039051685779,122.586232769824)) ;
#58636 = CARTESIAN_POINT('Ctrl Pts',(-20.3119093379596,-16.6939127269186,
122.204541346776)) ;
#58637 = CARTESIAN_POINT('Ctrl Pts',(-20.1313776273068,-16.5139236465557,
122.445995481957)) ;
#58638 = CARTESIAN_POINT('Ctrl Pts',(-20.0913143430655,-16.7037960412247,
122.067389838621)) ;
#58639 = CARTESIAN_POINT('Ctrl Pts',(-19.9549021776647,-16.5238069608618,
122.336275060039)) ;
#58640 = CARTESIAN_POINT('Ctrl Pts',(-19.8457714437164,-16.7138643437634,
121.968950139572)) ;
#58641 = CARTESIAN_POINT('Ctrl Pts',(-19.7584674011895,-16.5338752634005,
122.25752355759)) ;
#58642 = CARTESIAN_POINT('Ctrl Pts',(-19.5929691002655,-16.7236943910368,
121.915607289983)) ;
#58643 = CARTESIAN_POINT('Ctrl Pts',(-19.5562266645258,-16.543705310674,122.214849855465)) ;
#58644 = CARTESIAN_POINT('Ctrl Pts',(-19.3286263043383,-16.7337612624523,
121.906429428325)) ;
#58645 = CARTESIAN_POINT('Ctrl Pts',(-19.3447521004645,-16.5537721820895,
122.207507801228)) ;
#58646 = CARTESIAN_POINT('Ctrl Pts',(-19.0712701351498,-16.7436503012514,
121.942787563624)) ;
#58647 = CARTESIAN_POINT('Ctrl Pts',(-19.1388680389634,-16.5636612208885,
122.236594472759)) ;
#58648 = CARTESIAN_POINT('Ctrl Pts',(-18.8213494437771,-16.7536469993855,
122.023645715726)) ;
#58649 = CARTESIAN_POINT('Ctrl Pts',(-18.9389316809213,-16.5736579190226,
122.301281090436)) ;
#58650 = CARTESIAN_POINT('Ctrl Pts',(-18.5903042632975,-16.7635994250975,
122.146243992672)) ;
#58651 = CARTESIAN_POINT('Ctrl Pts',(-18.7540959986369,-16.5836103447346,
122.399359670759)) ;
#58652 = CARTESIAN_POINT('Ctrl Pts',(-18.3840928904313,-16.7735407273304,
122.306608387421)) ;
#58653 = CARTESIAN_POINT('Ctrl Pts',(-18.5891273551198,-16.5935516469676,
122.52765094837)) ;
#58654 = CARTESIAN_POINT('Ctrl Pts',(-18.2078769998902,-16.7835239664143,
122.501007316772)) ;
#58655 = CARTESIAN_POINT('Ctrl Pts',(-18.4481547970743,-16.6035348860515,
122.683169946801)) ;
#58656 = CARTESIAN_POINT('Ctrl Pts',(-18.0676897405683,-16.7935627679829,
122.724459360897)) ;
#58657 = CARTESIAN_POINT('Ctrl Pts',(-18.3360050210743,-16.6135736876201,
122.861931768501)) ;
#58658 = CARTESIAN_POINT('Ctrl Pts',(-17.9698306083083,-16.8034108741046,
122.964068373402)) ;
#58659 = CARTESIAN_POINT('Ctrl Pts',(-18.2577181420015,-16.6234217937417,
123.053617920861)) ;
#58660 = CARTESIAN_POINT('Ctrl Pts',(-17.91365079712,-16.8134710696799,123.222378870925)) ;
#58661 = CARTESIAN_POINT('Ctrl Pts',(-18.2127741641893,-16.633481989317,123.260266584404)) ;
#58662 = CARTESIAN_POINT('Ctrl Pts',(-17.9035805406861,-16.8233687529913,
123.482295776231)) ;
#58663 = CARTESIAN_POINT('Ctrl Pts',(-18.2047179840723,-16.6433796726285,
123.468199309359)) ;
#58664 = CARTESIAN_POINT('Ctrl Pts',(-17.938061631521,-16.8332997933653,123.740980891344)) ;
#58665 = CARTESIAN_POINT('Ctrl Pts',(-18.2323025565366,-16.6533107130024,
123.675146859333)) ;
#58666 = CARTESIAN_POINT('Ctrl Pts',(-18.018089634645,-16.8433420110219,123.992448629415)) ;
#58667 = CARTESIAN_POINT('Ctrl Pts',(-18.2963248642871,-16.6633529306591,
123.876321254892)) ;
#58668 = CARTESIAN_POINT('Ctrl Pts',(-18.1385099721154,-16.8532286717559,
124.222681786331)) ;
#58669 = CARTESIAN_POINT('Ctrl Pts',(-18.3926605542748,-16.673239591393,124.06050710284)) ;
#58670 = CARTESIAN_POINT('Ctrl Pts',(-18.2984195187527,-16.8632217803584,
124.430972590157)) ;
#58671 = CARTESIAN_POINT('Ctrl Pts',(-18.5205878453715,-16.6832326999955,
124.227139806063)) ;
#58672 = CARTESIAN_POINT('Ctrl Pts',(-18.4912243940808,-16.8731674789966,
124.607428923697)) ;
#58673 = CARTESIAN_POINT('Ctrl Pts',(-18.6748312019824,-16.6931783986337,
124.368304761902)) ;
#58674 = CARTESIAN_POINT('Ctrl Pts',(-18.7114963548054,-16.8831147012677,
124.748207213336)) ;
#58675 = CARTESIAN_POINT('Ctrl Pts',(-18.8510481570175,-16.7031256209048,
124.480927500203)) ;
#58676 = CARTESIAN_POINT('Ctrl Pts',(-18.9554062189626,-16.8931627268478,
124.849334419905)) ;
#58677 = CARTESIAN_POINT('Ctrl Pts',(-19.0461761012947,-16.7131736464849,
124.561829660936)) ;
#58678 = CARTESIAN_POINT('Ctrl Pts',(-19.2079801341472,-16.9030099739907,
124.905647599935)) ;
#58679 = CARTESIAN_POINT('Ctrl Pts',(-19.2482340537887,-16.7230208936278,
124.606880351078)) ;
#58680 = CARTESIAN_POINT('Ctrl Pts',(-19.4694948938835,-16.9129731510814,
124.918213293)) ;
#58681 = CARTESIAN_POINT('Ctrl Pts',(-19.4574454686167,-16.7329840707186,
124.616933496724)) ;
#58682 = CARTESIAN_POINT('Ctrl Pts',(-19.7309060814548,-16.9230028721148,
124.884564981777)) ;
#58683 = CARTESIAN_POINT('Ctrl Pts',(-19.6665745634729,-16.743013791752,124.590015342495)) ;
#58684 = CARTESIAN_POINT('Ctrl Pts',(-19.9794823375165,-16.9329073396477,
124.807315146919)) ;
#58685 = CARTESIAN_POINT('Ctrl Pts',(-19.8654350540059,-16.7529182592849,
124.528216247189)) ;
#58686 = CARTESIAN_POINT('Ctrl Pts',(-20.2136657521584,-16.9429318254775,
124.686737651366)) ;
#58687 = CARTESIAN_POINT('Ctrl Pts',(-20.0527821064406,-16.7629427451146,
124.431754771356)) ;
#58688 = CARTESIAN_POINT('Ctrl Pts',(-20.421015963903,-16.9528356606014,124.529379524787)) ;
#58689 = CARTESIAN_POINT('Ctrl Pts',(-20.2186620983548,-16.7728465802385,
124.305869231909)) ;
#58690 = CARTESIAN_POINT('Ctrl Pts',(-20.6005228715144,-16.9628868513114,
124.335656354932)) ;
#58691 = CARTESIAN_POINT('Ctrl Pts',(-20.3622682531827,-16.7828977709485,
124.150891007985)) ;
#58692 = CARTESIAN_POINT('Ctrl Pts',(-20.7413629698391,-16.9727712939697,
124.117369250282)) ;
#58693 = CARTESIAN_POINT('Ctrl Pts',(-20.4749404514896,-16.7927822136068,
123.976262404854)) ;
#58694 = CARTESIAN_POINT('Ctrl Pts',(-20.8436992076654,-16.9827643018216,
123.875549411217)) ;
#58695 = CARTESIAN_POINT('Ctrl Pts',(-20.5568101194757,-16.8027752214587,
123.782806994121)) ;
#58696 = CARTESIAN_POINT('Ctrl Pts',(-20.9021522987122,-16.9927126215379,
123.62071892228)) ;
#58697 = CARTESIAN_POINT('Ctrl Pts',(-20.6035732565573,-16.812723541175,123.578943200647)) ;
#58698 = CARTESIAN_POINT('Ctrl Pts',(-20.9158262169464,-17.0026494602473,
123.359970070186)) ;
#58699 = CARTESIAN_POINT('Ctrl Pts',(-20.6145132340894,-16.8226603798844,
123.370344673644)) ;
#58700 = CARTESIAN_POINT('Ctrl Pts',(-20.884191716522,-17.0126324491669,123.099507780396)) ;
#58701 = CARTESIAN_POINT('Ctrl Pts',(-20.5892065993372,-16.832643368804,123.161974931273)) ;
#58702 = CARTESIAN_POINT('Ctrl Pts',(-20.8069010684721,-17.022676328531,122.84716775239)) ;
#58703 = CARTESIAN_POINT('Ctrl Pts',(-20.5273748335759,-16.8426872481681,
122.960102519886)) ;
#58704 = CARTESIAN_POINT('Ctrl Pts',(-20.6900614936507,-17.0325043938894,
122.616789554295)) ;
#58705 = CARTESIAN_POINT('Ctrl Pts',(-20.4339045684967,-16.8525153135265,
122.775800548252)) ;
#58706 = CARTESIAN_POINT('Ctrl Pts',(-20.5312178370155,-17.0425814824443,
122.404977090048)) ;
#58707 = CARTESIAN_POINT('Ctrl Pts',(-20.306830239219,-16.8625924020815,122.606349695402)) ;
#58708 = CARTESIAN_POINT('Ctrl Pts',(-20.3423853676555,-17.0524316346006,
122.227828485222)) ;
#58709 = CARTESIAN_POINT('Ctrl Pts',(-20.1557657033809,-16.8724425542378,
122.464630732549)) ;
#58710 = CARTESIAN_POINT('Ctrl Pts',(-20.1207672096215,-17.062512115053,122.082830799905)) ;
#58711 = CARTESIAN_POINT('Ctrl Pts',(-19.9784714607027,-16.8825230346901,
122.348631493821)) ;
#58712 = CARTESIAN_POINT('Ctrl Pts',(-19.883737034747,-17.0723266128218,121.981011738217)) ;
#58713 = CARTESIAN_POINT('Ctrl Pts',(-19.7888488634291,-16.8923375324589,
122.267175689381)) ;
#58714 = CARTESIAN_POINT('Ctrl Pts',(-19.6263495978592,-17.0823949088419,
121.919989507403)) ;
#58715 = CARTESIAN_POINT('Ctrl Pts',(-19.5829389187349,-16.9024058284791,
122.218356659132)) ;
#58716 = CARTESIAN_POINT('Ctrl Pts',(-19.3665898868783,-17.0922937413247,
121.904909547411)) ;
#58717 = CARTESIAN_POINT('Ctrl Pts',(-19.3751318865944,-16.9123046609618,
122.206291541471)) ;
#58718 = CARTESIAN_POINT('Ctrl Pts',(-19.1042454569356,-17.1023466213392,
121.935528536243)) ;
#58719 = CARTESIAN_POINT('Ctrl Pts',(-19.1652560101051,-16.9223575409764,
122.230785548798)) ;
#58720 = CARTESIAN_POINT('Ctrl Pts',(-18.855638307516,-17.1122164368354,122.009652399298)) ;
#58721 = CARTESIAN_POINT('Ctrl Pts',(-18.9663707255866,-16.9322273564725,
122.29008319219)) ;
#58722 = CARTESIAN_POINT('Ctrl Pts',(-18.6189668205951,-17.1222891179182,
122.128093849741)) ;
#58723 = CARTESIAN_POINT('Ctrl Pts',(-18.7770327094499,-16.9423000375553,
122.384835334691)) ;
#58724 = CARTESIAN_POINT('Ctrl Pts',(-18.4114058096886,-17.1321215964892,
122.282028735497)) ;
#58725 = CARTESIAN_POINT('Ctrl Pts',(-18.6109839479363,-16.9521325161263,
122.507981587497)) ;
#58726 = CARTESIAN_POINT('Ctrl Pts',(-18.2296195608768,-17.1421522304753,
122.472896223419)) ;
#58727 = CARTESIAN_POINT('Ctrl Pts',(-18.4655538438899,-16.9621631501124,
122.660674621782)) ;
#58728 = CARTESIAN_POINT('Ctrl Pts',(-18.0843508674256,-17.1521837876944,
122.692895741896)) ;
#58729 = CARTESIAN_POINT('Ctrl Pts',(-18.3493377687508,-16.9721947073315,
122.836673575722)) ;
#58730 = CARTESIAN_POINT('Ctrl Pts',(-17.9811153912308,-17.1620134965661,
122.92966578504)) ;
#58731 = CARTESIAN_POINT('Ctrl Pts',(-18.2667484984008,-16.9820244162032,
123.026088115789)) ;
#58732 = CARTESIAN_POINT('Ctrl Pts',(-17.9188078334472,-17.1720029453682,
123.184684449035)) ;
#58733 = CARTESIAN_POINT('Ctrl Pts',(-18.2169009623757,-16.9920138650053,
123.230102537214)) ;
#58734 = CARTESIAN_POINT('Ctrl Pts',(-17.9023020185663,-17.1820467977682,
123.44810689289)) ;
#58735 = CARTESIAN_POINT('Ctrl Pts',(-18.2036948702119,-17.0020577174053,
123.440840520039)) ;
#58736 = CARTESIAN_POINT('Ctrl Pts',(-17.9306034522518,-17.1918685111003,
123.704655127921)) ;
#58737 = CARTESIAN_POINT('Ctrl Pts',(-18.2263343758186,-17.0118794307374,
123.646078286481)) ;
#58738 = CARTESIAN_POINT('Ctrl Pts',(-18.0039709952741,-17.201903516089,123.957951976954)) ;
#58739 = CARTESIAN_POINT('Ctrl Pts',(-18.2850268365724,-17.0219144357261,
123.848716309395)) ;
#58740 = CARTESIAN_POINT('Ctrl Pts',(-18.1207470223198,-17.2119283545366,
124.194108297233)) ;
#58741 = CARTESIAN_POINT('Ctrl Pts',(-18.3784462993163,-17.0319392741737,
124.03764205884)) ;
#58742 = CARTESIAN_POINT('Ctrl Pts',(-18.2736158124755,-17.2217805674918,
124.40306698223)) ;
#58743 = CARTESIAN_POINT('Ctrl Pts',(-18.5007395422443,-17.0417914871289,
124.204809319358)) ;
#58744 = CARTESIAN_POINT('Ctrl Pts',(-18.4627330156681,-17.2317705236856,
124.585121418507)) ;
#58745 = CARTESIAN_POINT('Ctrl Pts',(-18.6520320121567,-17.0517814433227,
124.350453999726)) ;
#58746 = CARTESIAN_POINT('Ctrl Pts',(-18.6792511906987,-17.2416986339689,
124.730700896654)) ;
#58747 = CARTESIAN_POINT('Ctrl Pts',(-18.8252452509934,-17.061709553606,124.466918770551)) ;
#58748 = CARTESIAN_POINT('Ctrl Pts',(-18.9190395513556,-17.2516872340484,
124.837500135833)) ;
#58749 = CARTESIAN_POINT('Ctrl Pts',(-19.0170750943207,-17.0716981536855,
124.552359735373)) ;
#58750 = CARTESIAN_POINT('Ctrl Pts',(-19.174783750514,-17.2617138259759,124.900929840425)) ;
#58751 = CARTESIAN_POINT('Ctrl Pts',(-19.2216700660752,-17.081724745613,124.603105176145)) ;
#58752 = CARTESIAN_POINT('Ctrl Pts',(-19.4339184087845,-17.2715989540401,
124.919007255833)) ;
#58753 = CARTESIAN_POINT('Ctrl Pts',(-19.4289770822547,-17.0916098736772,
124.617568828664)) ;
#58754 = CARTESIAN_POINT('Ctrl Pts',(-19.6951036459662,-17.2815900715136,
124.892117022616)) ;
#58755 = CARTESIAN_POINT('Ctrl Pts',(-19.6379253382598,-17.1016009911507,
124.596058506662)) ;
#58756 = CARTESIAN_POINT('Ctrl Pts',(-19.9487403100385,-17.2916306873654,
124.819396962872)) ;
#58757 = CARTESIAN_POINT('Ctrl Pts',(-19.8408352281527,-17.1116416070025,
124.537884144439)) ;
#58758 = CARTESIAN_POINT('Ctrl Pts',(-20.1811784262085,-17.3014636782191,
124.706518373388)) ;
#58759 = CARTESIAN_POINT('Ctrl Pts',(-20.0267858395131,-17.1214745978562,
124.447583262725)) ;
#58760 = CARTESIAN_POINT('Ctrl Pts',(-20.3943355471498,-17.3114568096694,
124.553138757061)) ;
#58761 = CARTESIAN_POINT('Ctrl Pts',(-20.1973125961385,-17.1314677293065,
124.324881214405)) ;
#58762 = CARTESIAN_POINT('Ctrl Pts',(-20.5779551582987,-17.3214888581048,
124.36395098382)) ;
#58763 = CARTESIAN_POINT('Ctrl Pts',(-20.3442096485662,-17.1414997777419,
124.17353227877)) ;
#58764 = CARTESIAN_POINT('Ctrl Pts',(-20.7237261254064,-17.3313541046472,
124.149582721403)) ;
#58765 = CARTESIAN_POINT('Ctrl Pts',(-20.4608276825751,-17.1513650242843,
124.002039230348)) ;
#58766 = CARTESIAN_POINT('Ctrl Pts',(-20.831788362086,-17.341315979474,123.911130472896)) ;
#58767 = CARTESIAN_POINT('Ctrl Pts',(-20.5472792280348,-17.1613268991111,
123.811278448521)) ;
#58768 = CARTESIAN_POINT('Ctrl Pts',(-20.8968589917748,-17.3513509425853,
123.655591647109)) ;
#58769 = CARTESIAN_POINT('Ctrl Pts',(-20.5993376400282,-17.1713618622224,
123.606847845879)) ;
#58770 = CARTESIAN_POINT('Ctrl Pts',(-20.9167197829666,-17.3612357870477,
123.396550342786)) ;
#58771 = CARTESIAN_POINT('Ctrl Pts',(-20.6152282496205,-17.1812467066848,
123.399615406321)) ;
#58772 = CARTESIAN_POINT('Ctrl Pts',(-20.8907754476135,-17.3713018398884,
123.133346946234)) ;
#58773 = CARTESIAN_POINT('Ctrl Pts',(-20.5944747717883,-17.1913127595256,
123.189052373295)) ;
#58774 = CARTESIAN_POINT('Ctrl Pts',(-20.8213961192781,-17.3811393557974,
122.88426085308)) ;
#58775 = CARTESIAN_POINT('Ctrl Pts',(-20.5389734280671,-17.2011502754345,
122.989783496606)) ;
#58776 = CARTESIAN_POINT('Ctrl Pts',(-20.7074934610674,-17.3912081039063,
122.645486865945)) ;
#58777 = CARTESIAN_POINT('Ctrl Pts',(-20.4478531284103,-17.2112190235434,
122.798763308908)) ;
#58778 = CARTESIAN_POINT('Ctrl Pts',(-20.5566061673441,-17.4010886209373,
122.434129920283)) ;
#58779 = CARTESIAN_POINT('Ctrl Pts',(-20.3271452112243,-17.2210995405744,
122.629676886925)) ;
#58780 = CARTESIAN_POINT('Ctrl Pts',(-20.3696663136538,-17.4110798078718,
122.249820531952)) ;
#58781 = CARTESIAN_POINT('Ctrl Pts',(-20.1775948836073,-17.2310907275089,
122.482227931951)) ;
#58782 = CARTESIAN_POINT('Ctrl Pts',(-20.1543475643769,-17.4210328741467,
122.101259878823)) ;
#58783 = CARTESIAN_POINT('Ctrl Pts',(-20.0053412412653,-17.2410437937838,
122.363377768744)) ;
#58784 = CARTESIAN_POINT('Ctrl Pts',(-19.9145466995836,-17.4310687116793,
121.991540433781)) ;
#58785 = CARTESIAN_POINT('Ctrl Pts',(-19.8135014215866,-17.2510796313164,
122.275600286841)) ;
#58786 = CARTESIAN_POINT('Ctrl Pts',(-19.6630503154042,-17.4409588378907,
121.925907930665)) ;
#58787 = CARTESIAN_POINT('Ctrl Pts',(-19.6123051763993,-17.2609697575279,
122.223092308256)) ;
#58788 = CARTESIAN_POINT('Ctrl Pts',(-19.4013697921715,-17.4509510197987,
121.904306259386)) ;
#58789 = CARTESIAN_POINT('Ctrl Pts',(-19.4029610196723,-17.2709619394358,
122.205808818119)) ;
#58790 = CARTESIAN_POINT('Ctrl Pts',(-19.1411178680801,-17.4608969597373,
121.928446401877)) ;
#58791 = CARTESIAN_POINT('Ctrl Pts',(-19.1947594651076,-17.2809078793744,
122.22511876556)) ;
#58792 = CARTESIAN_POINT('Ctrl Pts',(-18.88882641169,-17.4708441435014,121.996908692805)) ;
#58793 = CARTESIAN_POINT('Ctrl Pts',(-18.9929258788226,-17.2908550631385,
122.279886435726)) ;
#58794 = CARTESIAN_POINT('Ctrl Pts',(-18.6500049664529,-17.4808920818088,
122.109521528359)) ;
#58795 = CARTESIAN_POINT('Ctrl Pts',(-18.8018677870459,-17.300903001446,122.369974738324)) ;
#58796 = CARTESIAN_POINT('Ctrl Pts',(-18.4385276907917,-17.4907397165491,
122.258681232222)) ;
#58797 = CARTESIAN_POINT('Ctrl Pts',(-18.6326849625005,-17.3107506361862,
122.489300526383)) ;
#58798 = CARTESIAN_POINT('Ctrl Pts',(-18.2534782916843,-17.5007014305229,
122.443832320291)) ;
#58799 = CARTESIAN_POINT('Ctrl Pts',(-18.4846439297647,-17.3207123501601,
122.637419744003)) ;
#58800 = CARTESIAN_POINT('Ctrl Pts',(-18.1026371828242,-17.5107300653138,
122.659957308441)) ;
#58801 = CARTESIAN_POINT('Ctrl Pts',(-18.3639692439427,-17.3307409849509,
122.810318436287)) ;
#58802 = CARTESIAN_POINT('Ctrl Pts',(-17.9928588043532,-17.5206403839109,
122.896109111999)) ;
#58803 = CARTESIAN_POINT('Ctrl Pts',(-18.2761445935121,-17.340651303548,122.999238788582)) ;
#58804 = CARTESIAN_POINT('Ctrl Pts',(-17.9249170447996,-17.5305752402224,
123.148201377917)) ;
#58805 = CARTESIAN_POINT('Ctrl Pts',(-18.2217890416061,-17.3505861598595,
123.200911914671)) ;
#58806 = CARTESIAN_POINT('Ctrl Pts',(-17.9017863181592,-17.5406164761831,
123.41104640664)) ;
#58807 = CARTESIAN_POINT('Ctrl Pts',(-18.2032822312824,-17.3606273958202,
123.411187703811)) ;
#58808 = CARTESIAN_POINT('Ctrl Pts',(-17.9240826085059,-17.5505032477631,
123.669927416836)) ;
#58809 = CARTESIAN_POINT('Ctrl Pts',(-18.221117014871,-17.3705141674002,123.618292577988)) ;
#58810 = CARTESIAN_POINT('Ctrl Pts',(-17.991434789336,-17.5605034264693,123.923904177985)) ;
#58811 = CARTESIAN_POINT('Ctrl Pts',(-18.274996565428,-17.3805143461064,123.821474510317)) ;
#58812 = CARTESIAN_POINT('Ctrl Pts',(-18.1007768933539,-17.5704207046789,
124.160520976212)) ;
#58813 = CARTESIAN_POINT('Ctrl Pts',(-18.3624681751621,-17.390431624316,124.010768829435)) ;
#58814 = CARTESIAN_POINT('Ctrl Pts',(-18.2515125585857,-17.5804679510926,
124.377250917313)) ;
#58815 = CARTESIAN_POINT('Ctrl Pts',(-18.4830548228013,-17.4004788707297,
124.184154022707)) ;
#58816 = CARTESIAN_POINT('Ctrl Pts',(-18.4342365122274,-17.5903418400739,
124.561534748343)) ;
#58817 = CARTESIAN_POINT('Ctrl Pts',(-18.6292323540018,-17.410352759711,124.331582640151)) ;
#58818 = CARTESIAN_POINT('Ctrl Pts',(-18.6500768441802,-17.6004038576544,
124.714221581004)) ;
#58819 = CARTESIAN_POINT('Ctrl Pts',(-18.8019032612626,-17.4204147772915,
124.453733907963)) ;
#58820 = CARTESIAN_POINT('Ctrl Pts',(-18.8846741125319,-17.6102749193887,
124.82495821564)) ;
#58821 = CARTESIAN_POINT('Ctrl Pts',(-18.9895801047362,-17.4302858390258,
124.542325248395)) ;
#58822 = CARTESIAN_POINT('Ctrl Pts',(-19.1378416764729,-17.620268982749,124.894832090563)) ;
#58823 = CARTESIAN_POINT('Ctrl Pts',(-19.1921135246435,-17.4402799023861,
124.598226499213)) ;
#58824 = CARTESIAN_POINT('Ctrl Pts',(-19.4003404043878,-17.6303011407824,
124.919197850728)) ;
#58825 = CARTESIAN_POINT('Ctrl Pts',(-19.4021122156701,-17.4503120604195,
124.617721341599)) ;
#58826 = CARTESIAN_POINT('Ctrl Pts',(-19.6587556166457,-17.6401650170226,
124.898540308878)) ;
#58827 = CARTESIAN_POINT('Ctrl Pts',(-19.6088446217045,-17.4601759366597,
124.601197540958)) ;
#58828 = CARTESIAN_POINT('Ctrl Pts',(-19.9148657636072,-17.6502355316608,
124.832005118292)) ;
#58829 = CARTESIAN_POINT('Ctrl Pts',(-19.8137332138143,-17.470246451298,124.54797155282)) ;
#58830 = CARTESIAN_POINT('Ctrl Pts',(-20.150095477634,-17.6600761686018,124.724523892798)) ;
#58831 = CARTESIAN_POINT('Ctrl Pts',(-20.0019179240621,-17.4800870882389,
124.461988673264)) ;
#58832 = CARTESIAN_POINT('Ctrl Pts',(-20.3662817216806,-17.670043297442,124.576684081866)) ;
#58833 = CARTESIAN_POINT('Ctrl Pts',(-20.1748686108959,-17.4900542170791,
124.343718154926)) ;
#58834 = CARTESIAN_POINT('Ctrl Pts',(-20.5542290543161,-17.6800572705665,
124.392466662647)) ;
#58835 = CARTESIAN_POINT('Ctrl Pts',(-20.3252263581462,-17.5000681902037,
124.196347578167)) ;
#58836 = CARTESIAN_POINT('Ctrl Pts',(-20.7574242465171,-17.6933420044298,
124.108563216833)) ;
#58837 = CARTESIAN_POINT('Ctrl Pts',(-20.487792909875,-17.5133529240669,123.969217895372)) ;
#58838 = CARTESIAN_POINT('Ctrl Pts',(-20.8815792327918,-17.7065672691446,
123.779776387227)) ;
#58839 = CARTESIAN_POINT('Ctrl Pts',(-20.5871211385938,-17.5265781887817,
123.706157444669)) ;
#58840 = CARTESIAN_POINT('Ctrl Pts',(-20.9167156267444,-17.7198777916994,
123.431719811702)) ;
#58841 = CARTESIAN_POINT('Ctrl Pts',(-20.6152233992077,-17.5398887113366,
123.427758937628)) ;
#58842 = CARTESIAN_POINT('Ctrl Pts',(-20.8970403045933,-17.7299064366016,
123.168922156233)) ;
#58843 = CARTESIAN_POINT('Ctrl Pts',(-20.599487173877,-17.5499173562387,123.217511388876)) ;
#58844 = CARTESIAN_POINT('Ctrl Pts',(-20.833211337434,-17.7397874689555,122.917220164191)) ;
#58845 = CARTESIAN_POINT('Ctrl Pts',(-20.5484257925112,-17.5597983885926,
123.016151680332)) ;
#58846 = CARTESIAN_POINT('Ctrl Pts',(-20.7260717926928,-17.7497684416356,
122.677813694401)) ;
#58847 = CARTESIAN_POINT('Ctrl Pts',(-20.4627150058846,-17.5697793612727,
122.824624299976)) ;
#58848 = CARTESIAN_POINT('Ctrl Pts',(-20.5788081877206,-17.7597495692216,
122.460780265078)) ;
#58849 = CARTESIAN_POINT('Ctrl Pts',(-20.3449101987234,-17.5797604888587,
122.650998991699)) ;
#58850 = CARTESIAN_POINT('Ctrl Pts',(-20.3368568947388,-17.772992759483,122.21053545582)) ;
#58851 = CARTESIAN_POINT('Ctrl Pts',(-20.1513291199415,-17.5930036791201,
122.450788794857)) ;
#58852 = CARTESIAN_POINT('Ctrl Pts',(-19.9569936985326,-17.7896607548438,
121.982786748505)) ;
#58853 = CARTESIAN_POINT('Ctrl Pts',(-19.8474794990023,-17.6096716744809,
122.26860190868)) ;
#58854 = CARTESIAN_POINT('Ctrl Pts',(-19.5259606159641,-17.8061812548558,
121.898720902141)) ;
#58855 = CARTESIAN_POINT('Ctrl Pts',(-19.5025885463891,-17.626192174493,122.201337274905)) ;
#58856 = CARTESIAN_POINT('Ctrl Pts',(-19.1769501917683,-17.8194942711718,
121.922374301912)) ;
#58857 = CARTESIAN_POINT('Ctrl Pts',(-19.2234321602598,-17.639505190809,122.220261939682)) ;
#58858 = CARTESIAN_POINT('Ctrl Pts',(-18.9238414463951,-17.8294108294048,
121.984571342196)) ;
#58859 = CARTESIAN_POINT('Ctrl Pts',(-19.0209334397387,-17.649421749042,122.270017435273)) ;
#58860 = CARTESIAN_POINT('Ctrl Pts',(-18.6828367951169,-17.8394384977077,
122.090994480729)) ;
#58861 = CARTESIAN_POINT('Ctrl Pts',(-18.8281336451652,-17.6594494173448,
122.355152451845)) ;
#58862 = CARTESIAN_POINT('Ctrl Pts',(-18.394515897223,-17.8526190874524,122.283176068422)) ;
#58863 = CARTESIAN_POINT('Ctrl Pts',(-18.5974653676165,-17.6726300070895,
122.50890583314)) ;
#58864 = CARTESIAN_POINT('Ctrl Pts',(-18.1010163558912,-17.8693672265717,
122.617564692546)) ;
#58865 = CARTESIAN_POINT('Ctrl Pts',(-18.3626740164398,-17.6893781462089,
122.776403445059)) ;
#58866 = CARTESIAN_POINT('Ctrl Pts',(-17.909361184572,-17.8891619690823,123.107788785577)) ;
#58867 = CARTESIAN_POINT('Ctrl Pts',(-18.2093429356618,-17.7091728887194,
123.168586034307)) ;
#58868 = CARTESIAN_POINT('Ctrl Pts',(-17.8958042831171,-17.9092063618911,
123.640179567808)) ;
#58869 = CARTESIAN_POINT('Ctrl Pts',(-18.198495043607,-17.7292172815282,123.594497346099)) ;
#58870 = CARTESIAN_POINT('Ctrl Pts',(-18.0635490482974,-17.9290455441898,
124.140228438831)) ;
#58871 = CARTESIAN_POINT('Ctrl Pts',(-18.3326878464618,-17.7490564638269,
123.994538700796)) ;
#58872 = CARTESIAN_POINT('Ctrl Pts',(-18.3920994920008,-17.9489708678827,
124.555410464658)) ;
#58873 = CARTESIAN_POINT('Ctrl Pts',(-18.5955264281991,-17.7689817875198,
124.3266864764)) ;
#58874 = CARTESIAN_POINT('Ctrl Pts',(-18.842788696369,-17.9688945059342,124.833584548175)) ;
#58875 = CARTESIAN_POINT('Ctrl Pts',(-18.9560768416233,-17.7889054255713,
124.549228339882)) ;
#58876 = CARTESIAN_POINT('Ctrl Pts',(-19.3612051307133,-17.9888193793997,
124.941403037166)) ;
#58877 = CARTESIAN_POINT('Ctrl Pts',(-19.3708100925674,-17.8088302990368,
124.635485728076)) ;
#58878 = CARTESIAN_POINT('Ctrl Pts',(-19.8842672961237,-18.0086979864787,
124.866686275026)) ;
#58879 = CARTESIAN_POINT('Ctrl Pts',(-19.7892612316858,-17.8287089061158,
124.575714277679)) ;
#58880 = CARTESIAN_POINT('Ctrl Pts',(-20.3528378762813,-18.0286754293106,
124.616972672775)) ;
#58881 = CARTESIAN_POINT('Ctrl Pts',(-20.1641187657695,-17.8486863489478,
124.375944971353)) ;
#58882 = CARTESIAN_POINT('Ctrl Pts',(-20.7070199751766,-18.0486072773953,
124.222957551387)) ;
#58883 = CARTESIAN_POINT('Ctrl Pts',(-20.4474662649599,-17.8686181970324,
124.060733674475)) ;
#58884 = CARTESIAN_POINT('Ctrl Pts',(-20.9055702118375,-18.0685025457379,
123.732901280458)) ;
#58885 = CARTESIAN_POINT('Ctrl Pts',(-20.6063082810486,-17.888513465375,123.668688213802)) ;
#58886 = CARTESIAN_POINT('Ctrl Pts',(-20.9255908588565,-18.08842504415,123.203759760806)) ;
#58887 = CARTESIAN_POINT('Ctrl Pts',(-20.622325941902,-17.9084359637871,123.245374181992)) ;
#58888 = CARTESIAN_POINT('Ctrl Pts',(-20.7634037510858,-18.108384526026,122.69863823452)) ;
#58889 = CARTESIAN_POINT('Ctrl Pts',(-20.4925770626071,-17.9283954456631,
122.84127622867)) ;
#58890 = CARTESIAN_POINT('Ctrl Pts',(-20.4400561873198,-18.1282622784854,
122.280931726728)) ;
#58891 = CARTESIAN_POINT('Ctrl Pts',(-20.2338986900793,-17.9482731981225,
122.507109352624)) ;
#58892 = CARTESIAN_POINT('Ctrl Pts',(-19.9941357017279,-18.1481440692199,
121.997211525704)) ;
#58893 = CARTESIAN_POINT('Ctrl Pts',(-19.8771609449229,-17.9681549888571,
122.280132520306)) ;
#58894 = CARTESIAN_POINT('Ctrl Pts',(-19.473136676439,-18.1682174080709,121.882665391242)) ;
#58895 = CARTESIAN_POINT('Ctrl Pts',(-19.4603626713499,-17.988228327708,122.188495684092)) ;
#58896 = CARTESIAN_POINT('Ctrl Pts',(-18.9512092802025,-18.1880218753067,
121.951729931367)) ;
#58897 = CARTESIAN_POINT('Ctrl Pts',(-19.0428183076886,-18.0080327949438,
122.243747774639)) ;
#58898 = CARTESIAN_POINT('Ctrl Pts',(-18.4795781028299,-18.2080052157145,
122.195819043251)) ;
#58899 = CARTESIAN_POINT('Ctrl Pts',(-18.665513625463,-18.0280161353516,122.43901994105)) ;
#58900 = CARTESIAN_POINT('Ctrl Pts',(-18.1213593079001,-18.2279201803125,
122.585493056781)) ;
#58901 = CARTESIAN_POINT('Ctrl Pts',(-18.3789384269809,-18.0479310999496,
122.750760357878)) ;
#58902 = CARTESIAN_POINT('Ctrl Pts',(-17.9166900271828,-18.2477887150289,
123.072398846961)) ;
#58903 = CARTESIAN_POINT('Ctrl Pts',(-18.2152038535447,-18.067799634666,123.140286849332)) ;
#58904 = CARTESIAN_POINT('Ctrl Pts',(-17.891096129626,-18.2678410992406,123.604588275985)) ;
#58905 = CARTESIAN_POINT('Ctrl Pts',(-18.1947300898754,-18.0878520188777,
123.566037963837)) ;
#58906 = CARTESIAN_POINT('Ctrl Pts',(-18.0458895721995,-18.2876150630298,
124.107054946119)) ;
#58907 = CARTESIAN_POINT('Ctrl Pts',(-18.3185671783008,-18.1076259826669,
123.968012895512)) ;
#58908 = CARTESIAN_POINT('Ctrl Pts',(-18.3667637788578,-18.3076694420512,
124.53239666562)) ;
#58909 = CARTESIAN_POINT('Ctrl Pts',(-18.5752679245152,-18.1276803616883,
124.308284615384)) ;
#58910 = CARTESIAN_POINT('Ctrl Pts',(-18.8082021318572,-18.3274661796244,
124.819004328744)) ;
#58911 = CARTESIAN_POINT('Ctrl Pts',(-18.9284212935939,-18.1474770992615,
124.537569929665)) ;
#58912 = CARTESIAN_POINT('Ctrl Pts',(-19.3247749684746,-18.3474339919759,
124.940168786496)) ;
#58913 = CARTESIAN_POINT('Ctrl Pts',(-19.3416804332519,-18.167444911613,124.634498827263)) ;
#58914 = CARTESIAN_POINT('Ctrl Pts',(-19.8515753099783,-18.3673929680409,
124.876958419446)) ;
#58915 = CARTESIAN_POINT('Ctrl Pts',(-19.7631206608013,-18.187403887678,124.583927892231)) ;
#58916 = CARTESIAN_POINT('Ctrl Pts',(-20.323705737491,-18.3872878863183,124.638896796326)) ;
#58917 = CARTESIAN_POINT('Ctrl Pts',(-20.140824401647,-18.2072988059554,124.393475677266)) ;
#58918 = CARTESIAN_POINT('Ctrl Pts',(-20.6867396805035,-18.4071841987686,
124.254454112951)) ;
#58919 = CARTESIAN_POINT('Ctrl Pts',(-20.4312497270068,-18.2271951184057,
124.085918852288)) ;
#58920 = CARTESIAN_POINT('Ctrl Pts',(-20.8974889909594,-18.4270921321427,
123.769075405427)) ;
#58921 = CARTESIAN_POINT('Ctrl Pts',(-20.5998462757639,-18.2471030517799,
123.697614033343)) ;
#58922 = CARTESIAN_POINT('Ctrl Pts',(-20.9299591274622,-18.4470420224312,
123.239880881336)) ;
#58923 = CARTESIAN_POINT('Ctrl Pts',(-20.6258188645366,-18.2670529420683,
123.274257946613)) ;
#58924 = CARTESIAN_POINT('Ctrl Pts',(-20.7809301918273,-18.4669192529325,
122.732978965387)) ;
#58925 = CARTESIAN_POINT('Ctrl Pts',(-20.5065921666265,-18.2869301725696,
122.868736840689)) ;
#58926 = CARTESIAN_POINT('Ctrl Pts',(-20.4664719534886,-18.4869019218035,
122.305004321908)) ;
#58927 = CARTESIAN_POINT('Ctrl Pts',(-20.2550218602243,-18.3069128414406,
122.526359509871)) ;
#58928 = CARTESIAN_POINT('Ctrl Pts',(-20.0256670326121,-18.5068348083839,
122.011010324086)) ;
#58929 = CARTESIAN_POINT('Ctrl Pts',(-19.9023778434081,-18.326845728021,122.291166823134)) ;
#58930 = CARTESIAN_POINT('Ctrl Pts',(-19.5117084694408,-18.5267475544018,
121.884894904274)) ;
#58931 = CARTESIAN_POINT('Ctrl Pts',(-19.4912012916676,-18.3467584740389,
122.190280271835)) ;
#58932 = CARTESIAN_POINT('Ctrl Pts',(-19.0738118336098,-18.5433172757436,
121.93169130508)) ;
#58933 = CARTESIAN_POINT('Ctrl Pts',(-19.140910274212,-18.3633281953808,122.227714621675)) ;
#58934 = CARTESIAN_POINT('Ctrl Pts',(-18.7476501460358,-18.5566172870486,
122.057314468906)) ;
#58935 = CARTESIAN_POINT('Ctrl Pts',(-18.8799531105504,-18.3766282066857,
122.32822609425)) ;
#58936 = CARTESIAN_POINT('Ctrl Pts',(-18.4486656986035,-18.5698874747985,
122.23684236878)) ;
#58937 = CARTESIAN_POINT('Ctrl Pts',(-18.6408115504094,-18.3898983944356,
122.471815668889)) ;
#58938 = CARTESIAN_POINT('Ctrl Pts',(-18.1413722273347,-18.5865148571639,
122.554451895096)) ;
#58939 = CARTESIAN_POINT('Ctrl Pts',(-18.3949285205775,-18.406525776801,122.72595265338)) ;
#58940 = CARTESIAN_POINT('Ctrl Pts',(-17.9611265356219,-18.6031371469091,
122.957810899862)) ;
#58941 = CARTESIAN_POINT('Ctrl Pts',(-18.2507608262965,-18.4231480665462,
123.048601618741)) ;
#58942 = CARTESIAN_POINT('Ctrl Pts',(-17.9059528961361,-18.6163823613036,
123.301475150408)) ;
#58943 = CARTESIAN_POINT('Ctrl Pts',(-18.2066124741129,-18.4363932809408,
123.323560293853)) ;
#58944 = CARTESIAN_POINT('Ctrl Pts',(-17.9091768534027,-18.6262943262643,
123.561948497621)) ;
#58945 = CARTESIAN_POINT('Ctrl Pts',(-18.2091963170387,-18.4463052459014,
123.53193369723)) ;
#58946 = CARTESIAN_POINT('Ctrl Pts',(-17.9585883655337,-18.6363529494288,
123.821589557109)) ;
#58947 = CARTESIAN_POINT('Ctrl Pts',(-18.2487269958253,-18.4563638690659,
123.739647432984)) ;
#58948 = CARTESIAN_POINT('Ctrl Pts',(-18.0499609717764,-18.6461930635446,
124.06353698501)) ;
#58949 = CARTESIAN_POINT('Ctrl Pts',(-18.3218274009337,-18.4662039831817,
123.933204397028)) ;
#58950 = CARTESIAN_POINT('Ctrl Pts',(-18.1847150492908,-18.6562588485022,
124.291112489594)) ;
#58951 = CARTESIAN_POINT('Ctrl Pts',(-18.4296324649852,-18.4762697681393,
124.11526364337)) ;
#58952 = CARTESIAN_POINT('Ctrl Pts',(-18.3539469883158,-18.6661421662901,
124.488176476276)) ;
#58953 = CARTESIAN_POINT('Ctrl Pts',(-18.5650197804419,-18.4861530859272,
124.272913430482)) ;
#58954 = CARTESIAN_POINT('Ctrl Pts',(-18.5565725704209,-18.6761316041487,
124.655035297587)) ;
#58955 = CARTESIAN_POINT('Ctrl Pts',(-18.7271216359093,-18.4961425237858,
124.406398725453)) ;
#58956 = CARTESIAN_POINT('Ctrl Pts',(-18.7845837390266,-18.6860953182014,
124.783781642268)) ;
#58957 = CARTESIAN_POINT('Ctrl Pts',(-18.9095316568693,-18.5061062378385,
124.509393835218)) ;
#58958 = CARTESIAN_POINT('Ctrl Pts',(-19.0321760408685,-18.6960903298606,
124.871518685265)) ;
#58959 = CARTESIAN_POINT('Ctrl Pts',(-19.1076061994151,-18.5161012494978,
124.579581328801)) ;
#58960 = CARTESIAN_POINT('Ctrl Pts',(-19.2923475774158,-18.7061266215549,
124.914699798494)) ;
#58961 = CARTESIAN_POINT('Ctrl Pts',(-19.3157437283926,-18.526137541192,124.614123995732)) ;
#58962 = CARTESIAN_POINT('Ctrl Pts',(-19.5511061455371,-18.7159729992483,
124.912522869748)) ;
#58963 = CARTESIAN_POINT('Ctrl Pts',(-19.5227505956409,-18.5359839188854,
124.612380200103)) ;
#58964 = CARTESIAN_POINT('Ctrl Pts',(-19.8091754394204,-18.725957943399,124.865290742735)) ;
#58965 = CARTESIAN_POINT('Ctrl Pts',(-19.7292055595761,-18.5459688630361,
124.574592283995)) ;
#58966 = CARTESIAN_POINT('Ctrl Pts',(-20.0540693302501,-18.735894914529,124.774521245313)) ;
#58967 = CARTESIAN_POINT('Ctrl Pts',(-19.9251198339151,-18.5559058341661,
124.50197459087)) ;
#58968 = CARTESIAN_POINT('Ctrl Pts',(-20.2819125648932,-18.7459446991607,
124.64102455522)) ;
#58969 = CARTESIAN_POINT('Ctrl Pts',(-20.1073932380398,-18.5659556187978,
124.395175312067)) ;
#58970 = CARTESIAN_POINT('Ctrl Pts',(-20.4792864441643,-18.7557951612382,
124.473508135846)) ;
#58971 = CARTESIAN_POINT('Ctrl Pts',(-20.2652908081466,-18.5758060808753,
124.261160516284)) ;
#58972 = CARTESIAN_POINT('Ctrl Pts',(-20.6471074503595,-18.7657671747586,
124.272284173853)) ;
#58973 = CARTESIAN_POINT('Ctrl Pts',(-20.3995458257233,-18.5857780943957,
124.100179977328)) ;
#58974 = CARTESIAN_POINT('Ctrl Pts',(-20.7777500986428,-18.775762321878,124.044367513356)) ;
#58975 = CARTESIAN_POINT('Ctrl Pts',(-20.5040579656922,-18.5957732415151,
123.917845587999)) ;
#58976 = CARTESIAN_POINT('Ctrl Pts',(-20.86685809816,-18.7857962916141,123.796222100934)) ;
#58977 = CARTESIAN_POINT('Ctrl Pts',(-20.5753422305749,-18.6058072112512,
123.719328523745)) ;
#58978 = CARTESIAN_POINT('Ctrl Pts',(-20.9111412970602,-18.7956518372847,
123.541018035015)) ;
#58979 = CARTESIAN_POINT('Ctrl Pts',(-20.6107665482665,-18.6156627569218,
123.515165073301)) ;
#58980 = CARTESIAN_POINT('Ctrl Pts',(-20.9107995971931,-18.8056505942979,
123.278303845419)) ;
#58981 = CARTESIAN_POINT('Ctrl Pts',(-20.6104909554121,-18.6256615139351,
123.304993798075)) ;
#58982 = CARTESIAN_POINT('Ctrl Pts',(-20.8655454311932,-18.8155477295351,
123.022145216685)) ;
#58983 = CARTESIAN_POINT('Ctrl Pts',(-20.5742854776814,-18.6355586491722,
123.100067482626)) ;
#58984 = CARTESIAN_POINT('Ctrl Pts',(-20.7751653502272,-18.8256008253747,
122.773930212868)) ;
#58985 = CARTESIAN_POINT('Ctrl Pts',(-20.5019793282326,-18.6456117450119,
122.901496230122)) ;
#58986 = CARTESIAN_POINT('Ctrl Pts',(-20.6452882013384,-18.8354843341053,
122.54898577994)) ;
#58987 = CARTESIAN_POINT('Ctrl Pts',(-20.3980758193706,-18.6554952537425,
122.72154200763)) ;
#58988 = CARTESIAN_POINT('Ctrl Pts',(-20.4769328739096,-18.8454792067514,
122.347392525977)) ;
#58989 = CARTESIAN_POINT('Ctrl Pts',(-20.2633899435099,-18.6654901263886,
122.56026886385)) ;
#58990 = CARTESIAN_POINT('Ctrl Pts',(-20.2753461930725,-18.8554991683871,
122.177967546874)) ;
#58991 = CARTESIAN_POINT('Ctrl Pts',(-20.1021192027833,-18.6755100880243,
122.424730580812)) ;
#58992 = CARTESIAN_POINT('Ctrl Pts',(-20.0501362495513,-18.865404532187,122.047445707246)) ;
#58993 = CARTESIAN_POINT('Ctrl Pts',(-19.9219503672684,-18.6854154518241,
122.320315127144)) ;
#58994 = CARTESIAN_POINT('Ctrl Pts',(-19.8050116122211,-18.8753451197945,
121.957195984845)) ;
#58995 = CARTESIAN_POINT('Ctrl Pts',(-19.7258501182768,-18.6953560394316,
122.248117437871)) ;
#58996 = CARTESIAN_POINT('Ctrl Pts',(-19.5463105434524,-18.8853479378952,
121.910432554943)) ;
#58997 = CARTESIAN_POINT('Ctrl Pts',(-19.5188889496675,-18.7053588575323,
122.21070880072)) ;
#58998 = CARTESIAN_POINT('Ctrl Pts',(-19.2826245313416,-18.8953826496193,
121.909724812354)) ;
#58999 = CARTESIAN_POINT('Ctrl Pts',(-19.307940120733,-18.7153935692564,122.21014477667)) ;
#59000 = CARTESIAN_POINT('Ctrl Pts',(-19.0276297317745,-18.9052275563566,
121.953532899944)) ;
#59001 = CARTESIAN_POINT('Ctrl Pts',(-19.1039450889391,-18.7252384759937,
122.245193267705)) ;
#59002 = CARTESIAN_POINT('Ctrl Pts',(-18.7805173029334,-18.9152134089256,
122.041718002023)) ;
#59003 = CARTESIAN_POINT('Ctrl Pts',(-18.906255967733,-18.7352243285627,122.315743268288)) ;
#59004 = CARTESIAN_POINT('Ctrl Pts',(-18.5534655977386,-18.9251482173387,
122.170689853634)) ;
#59005 = CARTESIAN_POINT('Ctrl Pts',(-18.7246158475465,-18.7451591369758,
122.418922408914)) ;
#59006 = CARTESIAN_POINT('Ctrl Pts',(-18.3499886138001,-18.9352057444197,
122.33930838977)) ;
#59007 = CARTESIAN_POINT('Ctrl Pts',(-18.5618355205911,-18.7552166640568,
122.553818905849)) ;
#59008 = CARTESIAN_POINT('Ctrl Pts',(-18.1825491267777,-18.9450273994168,
122.535766487528)) ;
#59009 = CARTESIAN_POINT('Ctrl Pts',(-18.4278858915271,-18.7650383190539,
122.710986228041)) ;
#59010 = CARTESIAN_POINT('Ctrl Pts',(-18.0482437942149,-18.9550834435898,
122.76333018742)) ;
#59011 = CARTESIAN_POINT('Ctrl Pts',(-18.3204432872126,-18.775094363227,122.893038272163)) ;
#59012 = CARTESIAN_POINT('Ctrl Pts',(-17.9569846493071,-18.965024183635,123.008115620737)) ;
#59013 = CARTESIAN_POINT('Ctrl Pts',(-18.2474379774065,-18.7850351032721,
123.08886708059)) ;
#59014 = CARTESIAN_POINT('Ctrl Pts',(-17.9089873948513,-18.9749283047079,
123.26392514927)) ;
#59015 = CARTESIAN_POINT('Ctrl Pts',(-18.2090421543443,-18.794939224345,123.293514641434)) ;
#59016 = CARTESIAN_POINT('Ctrl Pts',(-17.9062567714271,-18.9849758458621,
123.527931134947)) ;
#59017 = CARTESIAN_POINT('Ctrl Pts',(-18.2068596105166,-18.8049867654992,
123.504719530089)) ;
#59018 = CARTESIAN_POINT('Ctrl Pts',(-17.9485884795945,-18.9948745974625,
123.784627499312)) ;
#59019 = CARTESIAN_POINT('Ctrl Pts',(-18.2407268052107,-18.8148855170996,
123.710075859708)) ;
#59020 = CARTESIAN_POINT('Ctrl Pts',(-18.0360231031298,-19.0049230764283,
124.033764662916)) ;
#59021 = CARTESIAN_POINT('Ctrl Pts',(-18.3106763436582,-18.8249339960654,
123.909385048735)) ;
#59022 = CARTESIAN_POINT('Ctrl Pts',(-18.163325670764,-19.014810573512,124.260307326459)) ;
#59023 = CARTESIAN_POINT('Ctrl Pts',(-18.4125198128121,-18.8348214931492,
124.09061779922)) ;
#59024 = CARTESIAN_POINT('Ctrl Pts',(-18.3293793931802,-19.0248036638101,
124.463720725707)) ;
#59025 = CARTESIAN_POINT('Ctrl Pts',(-18.5453641388487,-18.8448145834472,
124.253347258974)) ;
#59026 = CARTESIAN_POINT('Ctrl Pts',(-18.5275042406602,-19.0347558338704,
124.634466519872)) ;
#59027 = CARTESIAN_POINT('Ctrl Pts',(-18.7038650100524,-18.8547667535075,
124.389942302569)) ;
#59028 = CARTESIAN_POINT('Ctrl Pts',(-18.7517438317463,-19.0446942537849,
124.768323296831)) ;
#59029 = CARTESIAN_POINT('Ctrl Pts',(-18.8832572996416,-18.864705173422,124.497025999753)) ;
#59030 = CARTESIAN_POINT('Ctrl Pts',(-18.9969024435329,-19.0546793838705,
124.861939962815)) ;
#59031 = CARTESIAN_POINT('Ctrl Pts',(-19.079384667915,-18.8746903035076,124.571917644386)) ;
#59032 = CARTESIAN_POINT('Ctrl Pts',(-19.2559540582378,-19.0647160732846,
124.91143051181)) ;
#59033 = CARTESIAN_POINT('Ctrl Pts',(-19.286626370737,-18.8847269929217,124.611508315008)) ;
#59034 = CARTESIAN_POINT('Ctrl Pts',(-19.5149158429124,-19.0745707572771,
124.915534595951)) ;
#59035 = CARTESIAN_POINT('Ctrl Pts',(-19.4937950895379,-18.8945816769142,
124.614789827494)) ;
#59036 = CARTESIAN_POINT('Ctrl Pts',(-19.774403515448,-19.0845702413249,124.874379795706)) ;
#59037 = CARTESIAN_POINT('Ctrl Pts',(-19.7013848578054,-18.9045811609621,
124.581864340682)) ;
#59038 = CARTESIAN_POINT('Ctrl Pts',(-20.0203843648563,-19.0944653301018,
124.789921645643)) ;
#59039 = CARTESIAN_POINT('Ctrl Pts',(-19.898168451651,-18.914476249739,124.514296469915)) ;
#59040 = CARTESIAN_POINT('Ctrl Pts',(-20.2516876994953,-19.104525884748,124.66194576436)) ;
#59041 = CARTESIAN_POINT('Ctrl Pts',(-20.0832104950723,-18.9245368043851,
124.41191423788)) ;
#59042 = CARTESIAN_POINT('Ctrl Pts',(-20.4530733453116,-19.1143751491209,
124.499321729623)) ;
#59043 = CARTESIAN_POINT('Ctrl Pts',(-20.2443173510078,-18.934386068758,124.281814281811)) ;
#59044 = CARTESIAN_POINT('Ctrl Pts',(-20.6267212720183,-19.1244024015687,
124.301134264892)) ;
#59045 = CARTESIAN_POINT('Ctrl Pts',(-20.3832345959501,-18.9444133212059,
124.123263308682)) ;
#59046 = CARTESIAN_POINT('Ctrl Pts',(-20.7627508777503,-19.1344306991389,
124.075408616383)) ;
#59047 = CARTESIAN_POINT('Ctrl Pts',(-20.4920569238612,-18.954441618776,123.942681905956)) ;
#59048 = CARTESIAN_POINT('Ctrl Pts',(-20.8562554221649,-19.1442768281449,
123.834159661665)) ;
#59049 = CARTESIAN_POINT('Ctrl Pts',(-20.5668588165386,-18.964287747782,123.749683032266)) ;
#59050 = CARTESIAN_POINT('Ctrl Pts',(-20.9078510940648,-19.154270733507,123.576649296537)) ;
#59051 = CARTESIAN_POINT('Ctrl Pts',(-20.6081339643689,-18.9742816531441,
123.543674604084)) ;
#59052 = CARTESIAN_POINT('Ctrl Pts',(-20.9134974107354,-19.16429483119,123.313280162661)) ;
#59053 = CARTESIAN_POINT('Ctrl Pts',(-20.6126495326501,-18.9843057508271,
123.332979224958)) ;
#59054 = CARTESIAN_POINT('Ctrl Pts',(-20.8741896282484,-19.174184659044,123.056370784505)) ;
#59055 = CARTESIAN_POINT('Ctrl Pts',(-20.5812020083466,-18.9941955786812,
123.127452614158)) ;
#59056 = CARTESIAN_POINT('Ctrl Pts',(-20.7903778747057,-19.1841766404745,
122.807538053505)) ;
#59057 = CARTESIAN_POINT('Ctrl Pts',(-20.5141513809669,-19.0041875601116,
122.928386999942)) ;
#59058 = CARTESIAN_POINT('Ctrl Pts',(-20.665139925686,-19.1941236452403,122.578095153288)) ;
#59059 = CARTESIAN_POINT('Ctrl Pts',(-20.41396002509,-19.0141345648774,122.744833684279)) ;
#59060 = CARTESIAN_POINT('Ctrl Pts',(-20.5022911487532,-19.2040732966301,
122.373520731289)) ;
#59061 = CARTESIAN_POINT('Ctrl Pts',(-20.2836802639546,-19.0240842162672,
122.581175227014)) ;
#59062 = CARTESIAN_POINT('Ctrl Pts',(-20.3045468222314,-19.2141102996075,
122.198982921485)) ;
#59063 = CARTESIAN_POINT('Ctrl Pts',(-20.125483863784,-19.0341212192446,122.441545883708)) ;
#59064 = CARTESIAN_POINT('Ctrl Pts',(-20.0829020053588,-19.2239992080425,
122.063295386373)) ;
#59065 = CARTESIAN_POINT('Ctrl Pts',(-19.9481679801292,-19.0440101276797,
122.332997314253)) ;
#59066 = CARTESIAN_POINT('Ctrl Pts',(-19.8387974857453,-19.23398854052,121.96675176185)) ;
#59067 = CARTESIAN_POINT('Ctrl Pts',(-19.7528840990243,-19.0539994601571,
122.255763553244)) ;
#59068 = CARTESIAN_POINT('Ctrl Pts',(-19.5823918613755,-19.2439470959571,
121.91441371455)) ;
#59069 = CARTESIAN_POINT('Ctrl Pts',(-19.547759698978,-19.0639580155942,122.213894361448)) ;
#59070 = CARTESIAN_POINT('Ctrl Pts',(-19.3223367513905,-19.2538466671576,
121.906790613366)) ;
#59071 = CARTESIAN_POINT('Ctrl Pts',(-19.3397162836837,-19.0738575867947,
122.20779695611)) ;
#59072 = CARTESIAN_POINT('Ctrl Pts',(-19.0611077173987,-19.2638945924096,
121.945087876798)) ;
#59073 = CARTESIAN_POINT('Ctrl Pts',(-19.1307330399337,-19.0839055120467,
122.23843585839)) ;
#59074 = CARTESIAN_POINT('Ctrl Pts',(-18.814173133126,-19.2737898919356,122.026726025059)) ;
#59075 = CARTESIAN_POINT('Ctrl Pts',(-18.9331863897438,-19.0938008115727,
122.303747125533)) ;
#59076 = CARTESIAN_POINT('Ctrl Pts',(-18.5813585770366,-19.2838517483836,
122.152010675439)) ;
#59077 = CARTESIAN_POINT('Ctrl Pts',(-18.7469349998699,-19.1038626680207,
122.403975871039)) ;
#59078 = CARTESIAN_POINT('Ctrl Pts',(-18.3782635159342,-19.2936955948002,
122.312252866463)) ;
#59079 = CARTESIAN_POINT('Ctrl Pts',(-18.5844604094953,-19.1137065144373,
122.53216976341)) ;
#59080 = CARTESIAN_POINT('Ctrl Pts',(-18.203337799749,-19.3036585439283,122.507039819624)) ;
#59081 = CARTESIAN_POINT('Ctrl Pts',(-18.4445206716217,-19.1236694635654,
122.687999590902)) ;
#59082 = CARTESIAN_POINT('Ctrl Pts',(-18.0642605165968,-19.3136925803563,
122.731072713085)) ;
#59083 = CARTESIAN_POINT('Ctrl Pts',(-18.3332595529383,-19.1337034999934,
122.867226472839)) ;
#59084 = CARTESIAN_POINT('Ctrl Pts',(-17.9673787966871,-19.3235800073143,
122.972163161456)) ;
#59085 = CARTESIAN_POINT('Ctrl Pts',(-18.2557552582931,-19.1435909269514,
123.060098390728)) ;
#59086 = CARTESIAN_POINT('Ctrl Pts',(-17.9126484521056,-19.3335944416507,
123.229596243496)) ;
#59087 = CARTESIAN_POINT('Ctrl Pts',(-18.2119716852264,-19.1536053612878,
123.266044996015)) ;
#59088 = CARTESIAN_POINT('Ctrl Pts',(-17.9040917216401,-19.3436293862856,
123.493147352358)) ;
#59089 = CARTESIAN_POINT('Ctrl Pts',(-18.2051271768608,-19.1636403059227,
123.476886022838)) ;
#59090 = CARTESIAN_POINT('Ctrl Pts',(-17.9399787131204,-19.3534617363166,
123.749059430674)) ;
#59091 = CARTESIAN_POINT('Ctrl Pts',(-18.2338373040545,-19.1734726559537,
123.681614412356)) ;
#59092 = CARTESIAN_POINT('Ctrl Pts',(-18.0216292180747,-19.3635371754338,
124.000873856143)) ;
#59093 = CARTESIAN_POINT('Ctrl Pts',(-18.2991584729874,-19.183548095071,123.883066086777)) ;
#59094 = CARTESIAN_POINT('Ctrl Pts',(-18.1429328956799,-19.3733896406684,
124.229675102606)) ;
#59095 = CARTESIAN_POINT('Ctrl Pts',(-18.396201496122,-19.1934005603056,124.066105849519)) ;
#59096 = CARTESIAN_POINT('Ctrl Pts',(-18.3054527184388,-19.3834625182453,
124.438557806816)) ;
#59097 = CARTESIAN_POINT('Ctrl Pts',(-18.5262180422587,-19.2034734378824,
124.23321192103)) ;
#59098 = CARTESIAN_POINT('Ctrl Pts',(-18.497358063962,-19.3933051144378,124.61200943149)) ;
#59099 = CARTESIAN_POINT('Ctrl Pts',(-18.6797418858111,-19.2133160340749,
124.371972008953)) ;
#59100 = CARTESIAN_POINT('Ctrl Pts',(-18.7190343990807,-19.4032854985531,
124.75215735034)) ;
#59101 = CARTESIAN_POINT('Ctrl Pts',(-18.8570829522641,-19.2232964181902,
124.4840898822)) ;
#59102 = CARTESIAN_POINT('Ctrl Pts',(-18.9628028394866,-19.4133039792019,
124.851593565958)) ;
#59103 = CARTESIAN_POINT('Ctrl Pts',(-19.0520979082859,-19.233314898839,124.56363837805)) ;
#59104 = CARTESIAN_POINT('Ctrl Pts',(-19.2165815610938,-19.4231872942023,
124.906993128951)) ;
#59105 = CARTESIAN_POINT('Ctrl Pts',(-19.2551201081469,-19.2431982138394,
124.607957472016)) ;
#59106 = CARTESIAN_POINT('Ctrl Pts',(-19.48091038097,-19.4332555912927,124.917562972667)) ;
#59107 = CARTESIAN_POINT('Ctrl Pts',(-19.4665835088432,-19.2532665109298,
124.616412951815)) ;
#59108 = CARTESIAN_POINT('Ctrl Pts',(-19.7369866664886,-19.443085659665,124.883208337292)) ;
#59109 = CARTESIAN_POINT('Ctrl Pts',(-19.6714432710506,-19.2630965793021,
124.588929081079)) ;
#59110 = CARTESIAN_POINT('Ctrl Pts',(-19.9891462344239,-19.4531524521334,
124.803370268973)) ;
#59111 = CARTESIAN_POINT('Ctrl Pts',(-19.8731711567886,-19.2731633717705,
124.525058292213)) ;
#59112 = CARTESIAN_POINT('Ctrl Pts',(-20.2195097660386,-19.4630417856219,
124.682973671205)) ;
#59113 = CARTESIAN_POINT('Ctrl Pts',(-20.0574610978455,-19.2830527052591,
124.428741164273)) ;
#59114 = CARTESIAN_POINT('Ctrl Pts',(-20.4279957455821,-19.473043917038,124.522983695097)) ;
#59115 = CARTESIAN_POINT('Ctrl Pts',(-20.2242496883146,-19.2930548366751,
124.300749114728)) ;
#59116 = CARTESIAN_POINT('Ctrl Pts',(-20.6043330327823,-19.482967786659,124.330784900546)) ;
#59117 = CARTESIAN_POINT('Ctrl Pts',(-20.3653190116598,-19.3029787062961,
124.146990434962)) ;
#59118 = CARTESIAN_POINT('Ctrl Pts',(-20.7461987470963,-19.4930113021762,
124.108267757242)) ;
#59119 = CARTESIAN_POINT('Ctrl Pts',(-20.4788115505222,-19.3130222218133,
123.968976491356)) ;
#59120 = CARTESIAN_POINT('Ctrl Pts',(-20.8459623353145,-19.5028935150645,
123.868447779189)) ;
#59121 = CARTESIAN_POINT('Ctrl Pts',(-20.5586220080263,-19.3229044347016,
123.77712130273)) ;
#59122 = CARTESIAN_POINT('Ctrl Pts',(-20.9036081809755,-19.5129615922839,
123.610275746684)) ;
#59123 = CARTESIAN_POINT('Ctrl Pts',(-20.6047386771519,-19.332972511921,123.570583349477)) ;
#59124 = CARTESIAN_POINT('Ctrl Pts',(-20.9155157124554,-19.5228000970181,
123.351961006778)) ;
#59125 = CARTESIAN_POINT('Ctrl Pts',(-20.6142646315837,-19.3428110166552,
123.363932740499)) ;
#59126 = CARTESIAN_POINT('Ctrl Pts',(-20.8820171905211,-19.5328628654475,
123.089685129375)) ;
#59127 = CARTESIAN_POINT('Ctrl Pts',(-20.5874658526555,-19.3528737850846,
123.154111733586)) ;
#59128 = CARTESIAN_POINT('Ctrl Pts',(-20.8044967773862,-19.5427598587302,
122.841407511896)) ;
#59129 = CARTESIAN_POINT('Ctrl Pts',(-20.5254497644867,-19.3627707783674,
122.955490404283)) ;
#59130 = CARTESIAN_POINT('Ctrl Pts',(-20.6854165300552,-19.552691086365,122.609182603989)) ;
#59131 = CARTESIAN_POINT('Ctrl Pts',(-20.4301860313907,-19.3727020060021,
122.769710887484)) ;
#59132 = CARTESIAN_POINT('Ctrl Pts',(-20.5258305091892,-19.5627332450072,
122.399010178353)) ;
#59133 = CARTESIAN_POINT('Ctrl Pts',(-20.3025172352716,-19.3827441646443,
122.601572722186)) ;
#59134 = CARTESIAN_POINT('Ctrl Pts',(-20.3352897321001,-19.5726199545382,
122.222366967696)) ;
#59135 = CARTESIAN_POINT('Ctrl Pts',(-20.1500853867411,-19.3926308741753,
122.460258598056)) ;
#59136 = CARTESIAN_POINT('Ctrl Pts',(-20.1148863727174,-19.5826129269668,
122.079617245507)) ;
#59137 = CARTESIAN_POINT('Ctrl Pts',(-19.9737630061899,-19.4026238466039,
122.346058647369)) ;
#59138 = CARTESIAN_POINT('Ctrl Pts',(-19.8741264226561,-19.5925591215034,
121.977883229186)) ;
#59139 = CARTESIAN_POINT('Ctrl Pts',(-19.7811555923769,-19.4125700411405,
122.264671358312)) ;
#59140 = CARTESIAN_POINT('Ctrl Pts',(-19.6194821905471,-19.6025044963549,
121.918938430882)) ;
#59141 = CARTESIAN_POINT('Ctrl Pts',(-19.5774407611386,-19.422515415992,122.217515208665)) ;
#59142 = CARTESIAN_POINT('Ctrl Pts',(-19.3556280435181,-19.6125594157148,
121.905362356848)) ;
#59143 = CARTESIAN_POINT('Ctrl Pts',(-19.3663572165396,-19.4325703353519,
122.206654013868)) ;
#59144 = CARTESIAN_POINT('Ctrl Pts',(-19.0993869105069,-19.6223809351583,
121.936569596424)) ;
#59145 = CARTESIAN_POINT('Ctrl Pts',(-19.1613655396477,-19.4423918547954,
122.231619200685)) ;
#59146 = CARTESIAN_POINT('Ctrl Pts',(-18.8463008166757,-19.6324467039252,
122.013333704317)) ;
#59147 = CARTESIAN_POINT('Ctrl Pts',(-18.9588962140942,-19.4524576235623,
122.29303006788)) ;
#59148 = CARTESIAN_POINT('Ctrl Pts',(-18.6141847413824,-19.6423486255803,
122.131051371132)) ;
#59149 = CARTESIAN_POINT('Ctrl Pts',(-18.7732037818426,-19.4623595452174,
122.387203418498)) ;
#59150 = CARTESIAN_POINT('Ctrl Pts',(-18.4029852173609,-19.6523916844013,
122.289280682628)) ;
#59151 = CARTESIAN_POINT('Ctrl Pts',(-18.604243687009,-19.4724026040384,122.513786518166)) ;
#59152 = CARTESIAN_POINT('Ctrl Pts',(-18.2250106932067,-19.662297678444,122.479267826305)) ;
#59153 = CARTESIAN_POINT('Ctrl Pts',(-18.4618641781161,-19.4823085980811,
122.665775345268)) ;
#59154 = CARTESIAN_POINT('Ctrl Pts',(-18.0816334128682,-19.6722354515258,
122.697543077663)) ;
#59155 = CARTESIAN_POINT('Ctrl Pts',(-18.3471620419146,-19.4922463711629,
122.840394715573)) ;
#59156 = CARTESIAN_POINT('Ctrl Pts',(-17.9775290976188,-19.6822758152581,
122.939982086318)) ;
#59157 = CARTESIAN_POINT('Ctrl Pts',(-18.2638779349782,-19.5022867348952,
123.034345802999)) ;
#59158 = CARTESIAN_POINT('Ctrl Pts',(-17.9178270664722,-19.6921631589816,
123.192873036797)) ;
#59159 = CARTESIAN_POINT('Ctrl Pts',(-18.2161158243129,-19.5121740786187,
123.236657594822)) ;
#59160 = CARTESIAN_POINT('Ctrl Pts',(-17.9023535730957,-19.7021553895503,
123.454984271159)) ;
#59161 = CARTESIAN_POINT('Ctrl Pts',(-18.2037362398585,-19.5221663091874,
123.446346372631)) ;
#59162 = CARTESIAN_POINT('Ctrl Pts',(-17.9325684280021,-19.7121039173339,
123.714684335697)) ;
#59163 = CARTESIAN_POINT('Ctrl Pts',(-18.2279072969856,-19.532114836971,123.654106084101)) ;
#59164 = CARTESIAN_POINT('Ctrl Pts',(-18.0069653213655,-19.7220407010572,
123.964967568088)) ;
#59165 = CARTESIAN_POINT('Ctrl Pts',(-18.2874238319089,-19.5420516206943,
123.854332429313)) ;
#59166 = CARTESIAN_POINT('Ctrl Pts',(-18.1239596004005,-19.7320237018542,
124.199815869688)) ;
#59167 = CARTESIAN_POINT('Ctrl Pts',(-18.3810183152476,-19.5520346214913,
124.042211309555)) ;
#59168 = CARTESIAN_POINT('Ctrl Pts',(-18.2812582377019,-19.7420675886949,
124.411727571249)) ;
#59169 = CARTESIAN_POINT('Ctrl Pts',(-18.5068566460487,-19.562078508332,124.21174128928)) ;
#59170 = CARTESIAN_POINT('Ctrl Pts',(-18.4684715103472,-19.7518956122695,
124.589706055916)) ;
#59171 = CARTESIAN_POINT('Ctrl Pts',(-18.6566257534126,-19.5719065319066,
124.3541239909)) ;
#59172 = CARTESIAN_POINT('Ctrl Pts',(-18.6890566141087,-19.7619728604831,
124.736130030075)) ;
#59173 = CARTESIAN_POINT('Ctrl Pts',(-18.8330935698082,-19.5819837801202,
124.471264200358)) ;
#59174 = CARTESIAN_POINT('Ctrl Pts',(-18.9262775519246,-19.7718224157884,
124.839850242289)) ;
#59175 = CARTESIAN_POINT('Ctrl Pts',(-19.0228689899652,-19.5918333354255,
124.554240926399)) ;
#59176 = CARTESIAN_POINT('Ctrl Pts',(-19.1837052991682,-19.7819051239861,
124.902304787671)) ;
#59177 = CARTESIAN_POINT('Ctrl Pts',(-19.2288112851542,-19.6019160436232,
124.604205685487)) ;
#59178 = CARTESIAN_POINT('Ctrl Pts',(-19.4410933758794,-19.7917177169126,
124.918904855256)) ;
#59179 = CARTESIAN_POINT('Ctrl Pts',(-19.434720478767,-19.6117286365497,124.61748677879)) ;
#59180 = CARTESIAN_POINT('Ctrl Pts',(-19.7040333399795,-19.8017849091705,
124.890266579354)) ;
#59181 = CARTESIAN_POINT('Ctrl Pts',(-19.6450728626718,-19.6217958288076,
124.594577333264)) ;
#59182 = CARTESIAN_POINT('Ctrl Pts',(-19.9538529269052,-19.8116837386331,
124.817515981026)) ;
#59183 = CARTESIAN_POINT('Ctrl Pts',(-19.8449282229179,-19.6316946582702,
124.536378184494)) ;
#59184 = CARTESIAN_POINT('Ctrl Pts',(-20.1908446168851,-19.8217377298233,
124.700847328328)) ;
#59185 = CARTESIAN_POINT('Ctrl Pts',(-20.0345222842642,-19.6417486494604,
124.443044266715)) ;
#59186 = CARTESIAN_POINT('Ctrl Pts',(-20.4003396792968,-19.8316094546065,
124.547752149574)) ;
#59187 = CARTESIAN_POINT('Ctrl Pts',(-20.2021184087781,-19.6516203742436,
124.32056963313)) ;
#59188 = CARTESIAN_POINT('Ctrl Pts',(-20.5836646742585,-19.8416798967367,
124.356956666456)) ;
#59189 = CARTESIAN_POINT('Ctrl Pts',(-20.3487795243232,-19.6616908163738,
124.167933928758)) ;
#59190 = CARTESIAN_POINT('Ctrl Pts',(-20.7277380468266,-19.851512975167,124.142415105616)) ;
#59191 = CARTESIAN_POINT('Ctrl Pts',(-20.4640387321514,-19.6715238948041,
123.996302256258)) ;
#59192 = CARTESIAN_POINT('Ctrl Pts',(-20.8351448171807,-19.8615434486684,
123.901710971158)) ;
#59193 = CARTESIAN_POINT('Ctrl Pts',(-20.5499655097051,-19.6815543683055,
123.803739479692)) ;
#59194 = CARTESIAN_POINT('Ctrl Pts',(-20.8983935514118,-19.8715750479671,
123.645775745948)) ;
#59195 = CARTESIAN_POINT('Ctrl Pts',(-20.6005657740463,-19.6915859676042,
123.598991547224)) ;
#59196 = CARTESIAN_POINT('Ctrl Pts',(-20.9164189115037,-19.8814047490052,
123.388108112838)) ;
#59197 = CARTESIAN_POINT('Ctrl Pts',(-20.6149874004344,-19.7014156686424,
123.392858551262)) ;
#59198 = CARTESIAN_POINT('Ctrl Pts',(-20.889769707107,-19.8913941870617,123.126944309975)) ;
#59199 = CARTESIAN_POINT('Ctrl Pts',(-20.5936696114577,-19.7114051066988,
123.183927490661)) ;
#59200 = CARTESIAN_POINT('Ctrl Pts',(-20.817146145048,-19.9014380902778,122.873192498264)) ;
#59201 = CARTESIAN_POINT('Ctrl Pts',(-20.5355721095239,-19.7214490099149,
122.980925533021)) ;
#59202 = CARTESIAN_POINT('Ctrl Pts',(-20.7046073617645,-19.9112596110913,
122.640918152662)) ;
#59203 = CARTESIAN_POINT('Ctrl Pts',(-20.4455429052235,-19.7312705307284,
122.795106281435)) ;
#59204 = CARTESIAN_POINT('Ctrl Pts',(-20.5506673334166,-19.9212953353384,
122.426787436432)) ;
#59205 = CARTESIAN_POINT('Ctrl Pts',(-20.3223921809841,-19.7413062549755,
122.623800668938)) ;
#59206 = CARTESIAN_POINT('Ctrl Pts',(-20.3616469061169,-19.9313174892709,
122.243358309574)) ;
#59207 = CARTESIAN_POINT('Ctrl Pts',(-20.1711768967696,-19.751328408908,122.477056260967)) ;
#59208 = CARTESIAN_POINT('Ctrl Pts',(-20.1473968172802,-19.9411797210282,
122.097565987472)) ;
#59209 = CARTESIAN_POINT('Ctrl Pts',(-19.9997783728668,-19.7611906406653,
122.360421503876)) ;
#59210 = CARTESIAN_POINT('Ctrl Pts',(-19.9090443945828,-19.9511387914861,
121.989462309799)) ;
#59211 = CARTESIAN_POINT('Ctrl Pts',(-19.8090974023785,-19.7711497111232,
122.273937084454)) ;
#59212 = CARTESIAN_POINT('Ctrl Pts',(-19.653521817539,-19.9611739638623,121.924289992094)) ;
#59213 = CARTESIAN_POINT('Ctrl Pts',(-19.6046796893941,-19.7811848834994,
122.221797596013)) ;
#59214 = CARTESIAN_POINT('Ctrl Pts',(-19.3946113132475,-19.9710543490205,
121.904388967509)) ;
#59215 = CARTESIAN_POINT('Ctrl Pts',(-19.397552035366,-19.7910652686577,122.205875089908)) ;
#59216 = CARTESIAN_POINT('Ctrl Pts',(-19.1316102592397,-19.9811110636145,
121.930090607281)) ;
#59217 = CARTESIAN_POINT('Ctrl Pts',(-19.1871508676461,-19.8011219832516,
122.226434670213)) ;
#59218 = CARTESIAN_POINT('Ctrl Pts',(-18.8815248170591,-19.9909903321865,
121.999843996043)) ;
#59219 = CARTESIAN_POINT('Ctrl Pts',(-18.9870826419165,-19.8110012518237,
122.282235527794)) ;
#59220 = CARTESIAN_POINT('Ctrl Pts',(-18.6444106249268,-20.0009812896722,
122.112585153845)) ;
#59221 = CARTESIAN_POINT('Ctrl Pts',(-18.7973905924176,-19.8209922093093,
122.372426718099)) ;
#59222 = CARTESIAN_POINT('Ctrl Pts',(-18.4297462676032,-20.0110219483074,
122.266017180346)) ;
#59223 = CARTESIAN_POINT('Ctrl Pts',(-18.6256580184065,-19.8310328679445,
122.495170938252)) ;
#59224 = CARTESIAN_POINT('Ctrl Pts',(-18.2485010034738,-20.0208549280154,
122.450186849546)) ;
#59225 = CARTESIAN_POINT('Ctrl Pts',(-18.4806610287741,-19.8408658476525,
122.642504838089)) ;
#59226 = CARTESIAN_POINT('Ctrl Pts',(-18.0989811418267,-20.0308480612651,
122.666069459646)) ;
#59227 = CARTESIAN_POINT('Ctrl Pts',(-18.361043590352,-19.8508589809022,122.815209731099)) ;
#59228 = CARTESIAN_POINT('Ctrl Pts',(-17.9892812124725,-20.0408801136485,
122.905806909259)) ;
#59229 = CARTESIAN_POINT('Ctrl Pts',(-18.2732819325311,-19.8608910332856,
123.006998938251)) ;
#59230 = CARTESIAN_POINT('Ctrl Pts',(-17.9236747635864,-20.0507453425998,
123.15660297018)) ;
#59231 = CARTESIAN_POINT('Ctrl Pts',(-18.2207950630936,-19.8707562622369,
123.207634737405)) ;
#59232 = CARTESIAN_POINT('Ctrl Pts',(-17.9016652917606,-20.060707283843,123.417472522822)) ;
#59233 = CARTESIAN_POINT('Ctrl Pts',(-18.2031854905323,-19.8807182034801,
123.416330009112)) ;
#59234 = CARTESIAN_POINT('Ctrl Pts',(-17.9258798988399,-20.0707419988798,
123.680047914976)) ;
#59235 = CARTESIAN_POINT('Ctrl Pts',(-18.2225552242478,-19.8907529185169,
123.626390529728)) ;
#59236 = CARTESIAN_POINT('Ctrl Pts',(-17.9938945221677,-20.0806277692238,
123.930807070481)) ;
#59237 = CARTESIAN_POINT('Ctrl Pts',(-18.2769648599555,-19.9006386888609,
123.82699794779)) ;
#59238 = CARTESIAN_POINT('Ctrl Pts',(-18.1063688771636,-20.0906903666126,
124.17009418255)) ;
#59239 = CARTESIAN_POINT('Ctrl Pts',(-18.3669425672961,-19.9107012862497,
124.018428597259)) ;
#59240 = CARTESIAN_POINT('Ctrl Pts',(-18.2554062654784,-20.1005407784478,
124.381769206372)) ;
#59241 = CARTESIAN_POINT('Ctrl Pts',(-18.4861705070814,-19.9205516980849,
124.187769342642)) ;
#59242 = CARTESIAN_POINT('Ctrl Pts',(-18.4417280629167,-20.1105679477337,
124.568087270912)) ;
#59243 = CARTESIAN_POINT('Ctrl Pts',(-18.635226462847,-19.9305788673709,124.336825291195)) ;
#59244 = CARTESIAN_POINT('Ctrl Pts',(-18.6579883240975,-20.1205954284479,
124.71867494309)) ;
#59245 = CARTESIAN_POINT('Ctrl Pts',(-18.808233509183,-19.940606348085,124.457297090605)) ;
#59246 = CARTESIAN_POINT('Ctrl Pts',(-18.8924830333248,-20.1304384810272,
124.827831022184)) ;
#59247 = CARTESIAN_POINT('Ctrl Pts',(-18.9958279396515,-19.9504494006643,
124.544623631068)) ;
#59248 = CARTESIAN_POINT('Ctrl Pts',(-19.1460332396166,-20.1404323844658,
124.896285825858)) ;
#59249 = CARTESIAN_POINT('Ctrl Pts',(-19.1986674699778,-19.9604433041029,
124.599389529279)) ;
#59250 = CARTESIAN_POINT('Ctrl Pts',(-19.408537282864,-20.1504595072422,124.919271899717)) ;
#59251 = CARTESIAN_POINT('Ctrl Pts',(-19.408670501884,-19.9704704268793,124.617780480819)) ;
#59252 = CARTESIAN_POINT('Ctrl Pts',(-19.6674999586504,-20.1603502121343,
124.896966576094)) ;
#59253 = CARTESIAN_POINT('Ctrl Pts',(-19.6158404984156,-19.9803611317714,
124.599938376062)) ;
#59254 = CARTESIAN_POINT('Ctrl Pts',(-19.9213144643627,-20.1703422389846,
124.829720703187)) ;
#59255 = CARTESIAN_POINT('Ctrl Pts',(-19.8188925751091,-19.9903531586217,
124.546143793371)) ;
#59256 = CARTESIAN_POINT('Ctrl Pts',(-20.158473228304,-20.1802882204731,124.719860821045)) ;
#59257 = CARTESIAN_POINT('Ctrl Pts',(-20.0086203263769,-20.0002991401102,
124.458257924358)) ;
#59258 = CARTESIAN_POINT('Ctrl Pts',(-20.3732942470927,-20.190235393095,124.570897282398)) ;
#59259 = CARTESIAN_POINT('Ctrl Pts',(-20.1804782620418,-20.0102463127322,
124.339088990223)) ;
#59260 = CARTESIAN_POINT('Ctrl Pts',(-20.5606438303885,-20.2002833344212,
124.384839709342)) ;
#59261 = CARTESIAN_POINT('Ctrl Pts',(-20.3303594683394,-20.0202942540583,
124.19024447105)) ;
#59262 = CARTESIAN_POINT('Ctrl Pts',(-20.7099931677264,-20.210130968229,124.17349632098)) ;
#59263 = CARTESIAN_POINT('Ctrl Pts',(-20.4498405454841,-20.0301418878661,
124.021171285439)) ;
#59264 = CARTESIAN_POINT('Ctrl Pts',(-20.8223918370586,-20.220092682914,123.937083946774)) ;
#59265 = CARTESIAN_POINT('Ctrl Pts',(-20.5397614600564,-20.0401036025511,
123.832042436741)) ;
#59266 = CARTESIAN_POINT('Ctrl Pts',(-20.8921871412405,-20.2301213157925,
123.682935524378)) ;
#59267 = CARTESIAN_POINT('Ctrl Pts',(-20.5955998340411,-20.0501322354297,
123.628724320913)) ;
#59268 = CARTESIAN_POINT('Ctrl Pts',(-20.9165866653184,-20.2400316413277,
123.423658765384)) ;
#59269 = CARTESIAN_POINT('Ctrl Pts',(-20.6151216495105,-20.0600425609648,
123.421303286286)) ;
#59270 = CARTESIAN_POINT('Ctrl Pts',(-20.8962205046669,-20.2499664717994,
123.163371888268)) ;
#59271 = CARTESIAN_POINT('Ctrl Pts',(-20.5988309868347,-20.0699773914365,
123.213073725564)) ;
#59272 = CARTESIAN_POINT('Ctrl Pts',(-20.8300540056933,-20.2600078041814,
122.907927043714)) ;
#59273 = CARTESIAN_POINT('Ctrl Pts',(-20.545899908751,-20.0800187238185,123.008717280529)) ;
#59274 = CARTESIAN_POINT('Ctrl Pts',(-20.7222442141385,-20.2699006776202,
122.671362855132)) ;
#59275 = CARTESIAN_POINT('Ctrl Pts',(-20.4596543888742,-20.0899115972573,
122.819465277106)) ;
#59276 = CARTESIAN_POINT('Ctrl Pts',(-20.574403392537,-20.2798698434381,122.45507183945)) ;
#59277 = CARTESIAN_POINT('Ctrl Pts',(-20.3413828139098,-20.0998807630752,
122.646430631496)) ;
#59278 = CARTESIAN_POINT('Ctrl Pts',(-20.389867415721,-20.2898985771546,122.266945763663)) ;
#59279 = CARTESIAN_POINT('Ctrl Pts',(-20.1937587117748,-20.1099094967917,
122.495930505573)) ;
#59280 = CARTESIAN_POINT('Ctrl Pts',(-20.108189935514,-20.3030910959258,122.064717611353)) ;
#59281 = CARTESIAN_POINT('Ctrl Pts',(-19.9684034754264,-20.1231020155629,
122.334134312511)) ;
#59282 = CARTESIAN_POINT('Ctrl Pts',(-19.776200429425,-20.3164509639684,121.939098030054)) ;
#59283 = CARTESIAN_POINT('Ctrl Pts',(-19.70278986189,-20.1364618836056,122.233638111856)) ;
#59284 = CARTESIAN_POINT('Ctrl Pts',(-19.4302944299176,-20.3296763011173,
121.904585070859)) ;
#59285 = CARTESIAN_POINT('Ctrl Pts',(-19.4261079855339,-20.1496872207544,
122.206033326473)) ;
#59286 = CARTESIAN_POINT('Ctrl Pts',(-19.1686900557449,-20.3396575269579,
121.923502397448)) ;
#59287 = CARTESIAN_POINT('Ctrl Pts',(-19.2168157977084,-20.1596684465951,
122.221163228254)) ;
#59288 = CARTESIAN_POINT('Ctrl Pts',(-18.9130849261984,-20.3496930939408,
121.988403504327)) ;
#59289 = CARTESIAN_POINT('Ctrl Pts',(-19.0123335164269,-20.1697040135779,
122.273082369404)) ;
#59290 = CARTESIAN_POINT('Ctrl Pts',(-18.6765159440695,-20.3595561719029,
122.094373600289)) ;
#59291 = CARTESIAN_POINT('Ctrl Pts',(-18.8230767411481,-20.17956709154,122.357856308508)) ;
#59292 = CARTESIAN_POINT('Ctrl Pts',(-18.4574468061617,-20.369626470704,122.2427865665)) ;
#59293 = CARTESIAN_POINT('Ctrl Pts',(-18.6478204417451,-20.1896373903411,
122.476584793139)) ;
#59294 = CARTESIAN_POINT('Ctrl Pts',(-18.2717579005638,-20.3794687692718,
122.422851075719)) ;
#59295 = CARTESIAN_POINT('Ctrl Pts',(-18.4992676185254,-20.1994796889089,
122.620634878705)) ;
#59296 = CARTESIAN_POINT('Ctrl Pts',(-18.1175586647282,-20.3894294674416,
122.634360678073)) ;
#59297 = CARTESIAN_POINT('Ctrl Pts',(-18.3759064506187,-20.2094403870787,
122.78984130679)) ;
#59298 = CARTESIAN_POINT('Ctrl Pts',(-18.0020059072157,-20.3994675016211,
122.871483585782)) ;
#59299 = CARTESIAN_POINT('Ctrl Pts',(-18.2834623026179,-20.2194784212582,
122.97953855026)) ;
#59300 = CARTESIAN_POINT('Ctrl Pts',(-17.9300887193781,-20.4093412384676,
123.12082468391)) ;
#59301 = CARTESIAN_POINT('Ctrl Pts',(-18.2259264014613,-20.2293521581047,
123.179011012652)) ;
#59302 = CARTESIAN_POINT('Ctrl Pts',(-17.9020448474058,-20.4194130223928,
123.383973224126)) ;
#59303 = CARTESIAN_POINT('Ctrl Pts',(-18.2034891482727,-20.2394239420299,
123.389529423009)) ;
#59304 = CARTESIAN_POINT('Ctrl Pts',(-17.9195350319781,-20.429245143594,123.641783391188)) ;
#59305 = CARTESIAN_POINT('Ctrl Pts',(-18.2174791482912,-20.2492560632311,
123.595778035105)) ;
#59306 = CARTESIAN_POINT('Ctrl Pts',(-17.9820931576725,-20.4392781676194,
123.897898640785)) ;
#59307 = CARTESIAN_POINT('Ctrl Pts',(-18.2675235858112,-20.2592890872566,
123.8006706467)) ;
#59308 = CARTESIAN_POINT('Ctrl Pts',(-18.0886185614509,-20.4492940478161,
124.138604141846)) ;
#59309 = CARTESIAN_POINT('Ctrl Pts',(-18.3527418295689,-20.2693049674532,
123.993235758513)) ;
#59310 = CARTESIAN_POINT('Ctrl Pts',(-18.2329706508674,-20.4591775669103,
124.354523331879)) ;
#59311 = CARTESIAN_POINT('Ctrl Pts',(-18.4682220840992,-20.2791884865474,
124.165972815499)) ;
#59312 = CARTESIAN_POINT('Ctrl Pts',(-18.4143074091382,-20.469167979274,124.54434899152)) ;
#59313 = CARTESIAN_POINT('Ctrl Pts',(-18.6132892508366,-20.2891788989111,
124.31783370646)) ;
#59314 = CARTESIAN_POINT('Ctrl Pts',(-18.6951170310066,-20.4824311424774,
124.750853866765)) ;
#59315 = CARTESIAN_POINT('Ctrl Pts',(-18.8379390825619,-20.3024420621145,
124.483045334698)) ;
#59316 = CARTESIAN_POINT('Ctrl Pts',(-19.0235816254603,-20.4957087127286,
124.879780338446)) ;
#59317 = CARTESIAN_POINT('Ctrl Pts',(-19.1007466138958,-20.3157196323657,
124.586193622694)) ;
#59318 = CARTESIAN_POINT('Ctrl Pts',(-19.3717460245778,-20.5090390152352,
124.918788838269)) ;
#59319 = CARTESIAN_POINT('Ctrl Pts',(-19.3792305302181,-20.3290499348723,
124.617392368579)) ;
#59320 = CARTESIAN_POINT('Ctrl Pts',(-19.631378352144,-20.5189376970516,124.902811153565)) ;
#59321 = CARTESIAN_POINT('Ctrl Pts',(-19.586946416879,-20.3389486166887,124.604614298726)) ;
#59322 = CARTESIAN_POINT('Ctrl Pts',(-19.886681931356,-20.5289272120991,124.841743662503)) ;
#59323 = CARTESIAN_POINT('Ctrl Pts',(-19.7911870921237,-20.3489381317363,
124.555761778186)) ;
#59324 = CARTESIAN_POINT('Ctrl Pts',(-20.1265183759964,-20.5388752638742,
124.737689396078)) ;
#59325 = CARTESIAN_POINT('Ctrl Pts',(-19.9830583085483,-20.3588861835113,
124.472519572636)) ;
#59326 = CARTESIAN_POINT('Ctrl Pts',(-20.3446556457236,-20.5488166671527,
124.593959705977)) ;
#59327 = CARTESIAN_POINT('Ctrl Pts',(-20.1575676024382,-20.3688275867898,
124.357539619825)) ;
#59328 = CARTESIAN_POINT('Ctrl Pts',(-20.5987445476078,-20.5621033319336,
124.354427857962)) ;
#59329 = CARTESIAN_POINT('Ctrl Pts',(-20.3608485152388,-20.3821142515707,
124.165903776339)) ;
#59330 = CARTESIAN_POINT('Ctrl Pts',(-20.8307521720102,-20.5787137535884,
123.97887050718)) ;
#59331 = CARTESIAN_POINT('Ctrl Pts',(-20.5464484061325,-20.3987246732255,
123.865472812429)) ;
#59332 = CARTESIAN_POINT('Ctrl Pts',(-20.9389514260489,-20.5986250158392,
123.460821316337)) ;
#59333 = CARTESIAN_POINT('Ctrl Pts',(-20.6330141894971,-20.4186359354763,
123.451029346131)) ;
#59334 = CARTESIAN_POINT('Ctrl Pts',(-20.8639502681966,-20.6185691450041,
122.93604284961)) ;
#59335 = CARTESIAN_POINT('Ctrl Pts',(-20.5730157436839,-20.4385800646412,
123.031206971255)) ;
#59336 = CARTESIAN_POINT('Ctrl Pts',(-20.614611211859,-20.6384923076093,122.468951374548)) ;
#59337 = CARTESIAN_POINT('Ctrl Pts',(-20.373547351219,-20.4585032272464,122.657531515704)) ;
#59338 = CARTESIAN_POINT('Ctrl Pts',(-20.2219924331107,-20.6583824300158,
122.114827126927)) ;
#59339 = CARTESIAN_POINT('Ctrl Pts',(-20.0594536357031,-20.4783933496529,
122.374229525961)) ;
#59340 = CARTESIAN_POINT('Ctrl Pts',(-19.7292685932625,-20.6783873836159,
121.915230361568)) ;
#59341 = CARTESIAN_POINT('Ctrl Pts',(-19.6652757291056,-20.498398303253,122.2145494258)) ;
#59342 = CARTESIAN_POINT('Ctrl Pts',(-19.2022698837694,-20.6982256406315,
121.895490958203)) ;
#59343 = CARTESIAN_POINT('Ctrl Pts',(-19.2436755852947,-20.5182365602686,
122.198755216504)) ;
#59344 = CARTESIAN_POINT('Ctrl Pts',(-18.6962108824023,-20.718219941418,122.057473862947)) ;
#59345 = CARTESIAN_POINT('Ctrl Pts',(-18.8388276085648,-20.5382308610552,
122.328339327978)) ;
#59346 = CARTESIAN_POINT('Ctrl Pts',(-18.2783285952611,-20.7381051834625,
122.381075560874)) ;
#59347 = CARTESIAN_POINT('Ctrl Pts',(-18.5045195347661,-20.5581161030996,
122.587219431288)) ;
#59348 = CARTESIAN_POINT('Ctrl Pts',(-17.994854669319,-20.7579801299384,122.826813664133)) ;
#59349 = CARTESIAN_POINT('Ctrl Pts',(-18.2777383070033,-20.5779910495756,
122.943810054151)) ;
#59350 = CARTESIAN_POINT('Ctrl Pts',(-17.8799919148202,-20.7780131998795,
123.346775629798)) ;
#59351 = CARTESIAN_POINT('Ctrl Pts',(-18.1858465680844,-20.5980241195166,
123.359778876185)) ;
#59352 = CARTESIAN_POINT('Ctrl Pts',(-17.9496011378404,-20.7979017067799,
123.870729922687)) ;
#59353 = CARTESIAN_POINT('Ctrl Pts',(-18.2415323136978,-20.617912626417,123.778943688252)) ;
#59354 = CARTESIAN_POINT('Ctrl Pts',(-18.1918462219095,-20.8177565665612,
124.3396421318)) ;
#59355 = CARTESIAN_POINT('Ctrl Pts',(-18.4353283966454,-20.6377674861983,
124.15407531908)) ;
#59356 = CARTESIAN_POINT('Ctrl Pts',(-18.5838321068267,-20.8378074003489,
124.700496054133)) ;
#59357 = CARTESIAN_POINT('Ctrl Pts',(-18.7489159490425,-20.657818319986,124.442758816039)) ;
#59358 = CARTESIAN_POINT('Ctrl Pts',(-19.068464276831,-20.8575733422382,124.903648311882)) ;
#59359 = CARTESIAN_POINT('Ctrl Pts',(-19.1366240867067,-20.6775842618753,
124.605282256728)) ;
#59360 = CARTESIAN_POINT('Ctrl Pts',(-19.5995315082648,-20.8775860736975,
124.930591112169)) ;
#59361 = CARTESIAN_POINT('Ctrl Pts',(-19.5614778234741,-20.6975969933346,
124.626836366824)) ;
#59362 = CARTESIAN_POINT('Ctrl Pts',(-20.1049415619315,-20.8974789086411,
124.774856355301)) ;
#59363 = CARTESIAN_POINT('Ctrl Pts',(-19.9658071300402,-20.7174898282782,
124.502248164714)) ;
#59364 = CARTESIAN_POINT('Ctrl Pts',(-20.5274834956155,-20.9173859319806,
124.456638371314)) ;
#59365 = CARTESIAN_POINT('Ctrl Pts',(-20.3038412440261,-20.7373968516177,
124.247672563111)) ;
#59366 = CARTESIAN_POINT('Ctrl Pts',(-20.816830578431,-20.9373011968813,124.013259477076)) ;
#59367 = CARTESIAN_POINT('Ctrl Pts',(-20.5353184953281,-20.7573121165184,
123.892968103574)) ;
#59368 = CARTESIAN_POINT('Ctrl Pts',(-20.9375148304315,-20.957332889041,123.494752291647)) ;
#59369 = CARTESIAN_POINT('Ctrl Pts',(-20.6318648818766,-20.7773438086781,
123.47816249865)) ;
#59370 = CARTESIAN_POINT('Ctrl Pts',(-20.8746353856575,-20.977175935614,122.971063764451)) ;
#59371 = CARTESIAN_POINT('Ctrl Pts',(-20.5815599743237,-20.7971868552511,
123.059210077434)) ;
#59372 = CARTESIAN_POINT('Ctrl Pts',(-20.6370889547164,-20.9970924835138,
122.498095047724)) ;
#59373 = CARTESIAN_POINT('Ctrl Pts',(-20.3915208071778,-20.8171034031509,
122.680835172587)) ;
#59374 = CARTESIAN_POINT('Ctrl Pts',(-20.2519449229263,-21.0170247265051,
122.134274226715)) ;
#59375 = CARTESIAN_POINT('Ctrl Pts',(-20.0834038045587,-20.8370356461422,
122.389779490593)) ;
#59376 = CARTESIAN_POINT('Ctrl Pts',(-19.7666424548644,-21.0369285613144,
121.923791010191)) ;
#59377 = CARTESIAN_POINT('Ctrl Pts',(-19.6951601330397,-20.8569394809515,
122.221394579836)) ;
#59378 = CARTESIAN_POINT('Ctrl Pts',(-19.2387517746297,-21.0568289615019,
121.890890792397)) ;
#59379 = CARTESIAN_POINT('Ctrl Pts',(-19.2728466143262,-20.876839881139,122.195076908479)) ;
#59380 = CARTESIAN_POINT('Ctrl Pts',(-18.7299794806847,-21.0767786378812,
122.040270945825)) ;
#59381 = CARTESIAN_POINT('Ctrl Pts',(-18.8658292110054,-20.8967895575183,
122.314583763135)) ;
#59382 = CARTESIAN_POINT('Ctrl Pts',(-18.303166710287,-21.0967111621016,122.354115893689)) ;
#59383 = CARTESIAN_POINT('Ctrl Pts',(-18.5243802930808,-20.9167220817387,
122.565662292929)) ;
#59384 = CARTESIAN_POINT('Ctrl Pts',(-18.0088633209534,-21.1166311710878,
122.794268679534)) ;
#59385 = CARTESIAN_POINT('Ctrl Pts',(-18.2889398325272,-20.9366420907249,
122.917786669233)) ;
#59386 = CARTESIAN_POINT('Ctrl Pts',(-17.8822937308164,-21.136588077264,123.309313272766)) ;
#59387 = CARTESIAN_POINT('Ctrl Pts',(-18.1876872095001,-20.9565989969011,
123.329823376665)) ;
#59388 = CARTESIAN_POINT('Ctrl Pts',(-17.9384143246764,-21.1564739167655,
123.834958994811)) ;
#59389 = CARTESIAN_POINT('Ctrl Pts',(-18.2325869694415,-20.9764848364026,
123.750340253762)) ;
#59390 = CARTESIAN_POINT('Ctrl Pts',(-18.1714993859742,-21.1764450889013,
124.31171484266)) ;
#59391 = CARTESIAN_POINT('Ctrl Pts',(-18.4190587792687,-20.9964560085384,
124.131743525052)) ;
#59392 = CARTESIAN_POINT('Ctrl Pts',(-18.5499193847217,-21.1962592858857,
124.678080171936)) ;
#59393 = CARTESIAN_POINT('Ctrl Pts',(-18.7217959353721,-21.0162702055228,
124.424833857205)) ;
#59394 = CARTESIAN_POINT('Ctrl Pts',(-19.0342352621923,-21.2162404718539,
124.89571496393)) ;
#59395 = CARTESIAN_POINT('Ctrl Pts',(-19.1092580929924,-21.0362513914911,
124.598937764021)) ;
#59396 = CARTESIAN_POINT('Ctrl Pts',(-19.4736619237772,-21.2328159772432,
124.928069751188)) ;
#59397 = CARTESIAN_POINT('Ctrl Pts',(-19.4607756982869,-21.0528268968803,
124.624819424069)) ;
#59398 = CARTESIAN_POINT('Ctrl Pts',(-19.8173383619088,-21.2461254251068,
124.863112509641)) ;
#59399 = CARTESIAN_POINT('Ctrl Pts',(-19.7357439277155,-21.0661363447439,
124.572846691441)) ;
#59400 = CARTESIAN_POINT('Ctrl Pts',(-20.1458733462935,-21.2594931228834,
124.738714343657)) ;
#59401 = CARTESIAN_POINT('Ctrl Pts',(-19.998523136109,-21.0795040425205,124.473349266923)) ;
#59402 = CARTESIAN_POINT('Ctrl Pts',(-20.5018728442166,-21.2759836945493,
124.483060829662)) ;
#59403 = CARTESIAN_POINT('Ctrl Pts',(-20.2833722640373,-21.0959946141864,
124.268798320229)) ;
#59404 = CARTESIAN_POINT('Ctrl Pts',(-20.8018337601815,-21.2959039668821,
124.04687473534)) ;
#59405 = CARTESIAN_POINT('Ctrl Pts',(-20.5233223409627,-21.1159148865192,
123.919846740881)) ;
#59406 = CARTESIAN_POINT('Ctrl Pts',(-20.9126872837308,-21.3125210026031,
123.619326861712)) ;
#59407 = CARTESIAN_POINT('Ctrl Pts',(-20.6120012338397,-21.1325319222402,
123.57783290666)) ;
#59408 = CARTESIAN_POINT('Ctrl Pts',(-20.9100801364126,-21.3258118528842,
123.270041130568)) ;
#59409 = CARTESIAN_POINT('Ctrl Pts',(-20.6099160373388,-21.1458227725213,
123.298380131864)) ;
#59410 = CARTESIAN_POINT('Ctrl Pts',(-20.8627908877047,-21.3357808980387,
123.01239695694)) ;
#59411 = CARTESIAN_POINT('Ctrl Pts',(-20.572081952972,-21.1557918176758,123.092270099761)) ;
#59412 = CARTESIAN_POINT('Ctrl Pts',(-20.7725483587208,-21.3456842886722,
122.768260657611)) ;
#59413 = CARTESIAN_POINT('Ctrl Pts',(-20.499885452573,-21.1656952083094,122.896960032138)) ;
#59414 = CARTESIAN_POINT('Ctrl Pts',(-20.6391462593297,-21.355742074785,122.540122041422)) ;
#59415 = CARTESIAN_POINT('Ctrl Pts',(-20.3931639432043,-21.1757529944221,
122.714452096665)) ;
#59416 = CARTESIAN_POINT('Ctrl Pts',(-20.471796281269,-21.3655941114347,122.342544854426)) ;
#59417 = CARTESIAN_POINT('Ctrl Pts',(-20.2592745302504,-21.1856050310718,
122.556386398767)) ;
#59418 = CARTESIAN_POINT('Ctrl Pts',(-20.202086568455,-21.3789592355779,122.117585029651)) ;
#59419 = CARTESIAN_POINT('Ctrl Pts',(-20.0435429434541,-21.198970155215,122.376446523523)) ;
#59420 = CARTESIAN_POINT('Ctrl Pts',(-19.8829746642869,-21.3921852985409,
121.970083356066)) ;
#59421 = CARTESIAN_POINT('Ctrl Pts',(-19.7882331633885,-21.2121962181781,
122.25842782825)) ;
#59422 = CARTESIAN_POINT('Ctrl Pts',(-19.5386166648269,-21.4054889468232,
121.909867161857)) ;
#59423 = CARTESIAN_POINT('Ctrl Pts',(-19.5127307955836,-21.2254998664603,
122.210256068313)) ;
#59424 = CARTESIAN_POINT('Ctrl Pts',(-19.2760167649195,-21.4154804779862,
121.910107183642)) ;
#59425 = CARTESIAN_POINT('Ctrl Pts',(-19.302654042271,-21.2354913976233,122.210450691306)) ;
#59426 = CARTESIAN_POINT('Ctrl Pts',(-19.0163207496462,-21.4255199257855,
121.956500605478)) ;
#59427 = CARTESIAN_POINT('Ctrl Pts',(-19.0948968590476,-21.2455308454226,
122.247567530299)) ;
#59428 = CARTESIAN_POINT('Ctrl Pts',(-18.7732843139319,-21.4353637012994,
122.045159677628)) ;
#59429 = CARTESIAN_POINT('Ctrl Pts',(-18.9004686755779,-21.2553746209365,
122.318496939825)) ;
#59430 = CARTESIAN_POINT('Ctrl Pts',(-18.5458944197202,-21.445349342687,122.176053036341)) ;
#59431 = CARTESIAN_POINT('Ctrl Pts',(-18.7185578856858,-21.2653602623241,
122.42321354917)) ;
#59432 = CARTESIAN_POINT('Ctrl Pts',(-18.3455158402902,-21.4552861270488,
122.343559635745)) ;
#59433 = CARTESIAN_POINT('Ctrl Pts',(-18.5582565294496,-21.2752970466859,
122.557220524187)) ;
#59434 = CARTESIAN_POINT('Ctrl Pts',(-18.1755004123989,-21.4653359615162,
122.545621877111)) ;
#59435 = CARTESIAN_POINT('Ctrl Pts',(-18.4222459430947,-21.2853468811533,
122.718871736199)) ;
#59436 = CARTESIAN_POINT('Ctrl Pts',(-18.0455857951863,-21.4751864110193,
122.769542152888)) ;
#59437 = CARTESIAN_POINT('Ctrl Pts',(-18.3183162510833,-21.2951973306564,
122.898009008209)) ;
#59438 = CARTESIAN_POINT('Ctrl Pts',(-17.9548017337126,-21.4851584250014,
123.015333175436)) ;
#59439 = CARTESIAN_POINT('Ctrl Pts',(-18.2456911442363,-21.3051693446385,
123.094642518288)) ;
#59440 = CARTESIAN_POINT('Ctrl Pts',(-17.9079865989931,-21.4951535828485,
123.273832595304)) ;
#59441 = CARTESIAN_POINT('Ctrl Pts',(-18.2082412561885,-21.3151645024856,
123.3014423916)) ;
#59442 = CARTESIAN_POINT('Ctrl Pts',(-17.9070803718407,-21.5051875092122,
123.537489745388)) ;
#59443 = CARTESIAN_POINT('Ctrl Pts',(-18.2075185318219,-21.3251984288494,
123.512368089065)) ;
#59444 = CARTESIAN_POINT('Ctrl Pts',(-17.9507793758627,-21.5150432176446,
123.792798278233)) ;
#59445 = CARTESIAN_POINT('Ctrl Pts',(-18.2424799133806,-21.3350541372817,
123.716614351345)) ;
#59446 = CARTESIAN_POINT('Ctrl Pts',(-18.0390300008137,-21.5250413669833,
124.040230621142)) ;
#59447 = CARTESIAN_POINT('Ctrl Pts',(-18.3130824917955,-21.3450522866204,
123.914559406275)) ;
#59448 = CARTESIAN_POINT('Ctrl Pts',(-18.1674560178269,-21.5349407701568,
124.266510551616)) ;
#59449 = CARTESIAN_POINT('Ctrl Pts',(-18.4158251303191,-21.354951689794,124.095582078707)) ;
#59450 = CARTESIAN_POINT('Ctrl Pts',(-18.3356760700349,-21.5449919670453,
124.470114254987)) ;
#59451 = CARTESIAN_POINT('Ctrl Pts',(-18.5504028849582,-21.3650028866824,
124.258463636638)) ;
#59452 = CARTESIAN_POINT('Ctrl Pts',(-18.5333267197165,-21.5548742908582,
124.63859875685)) ;
#59453 = CARTESIAN_POINT('Ctrl Pts',(-18.7085246479764,-21.3748852104953,
124.393249391773)) ;
#59454 = CARTESIAN_POINT('Ctrl Pts',(-18.7594560018533,-21.5648691865148,
124.772199667984)) ;
#59455 = CARTESIAN_POINT('Ctrl Pts',(-18.8894291059458,-21.3848801061519,
124.500128205226)) ;
#59456 = CARTESIAN_POINT('Ctrl Pts',(-19.0061476935566,-21.5748902858973,
124.864395292257)) ;
#59457 = CARTESIAN_POINT('Ctrl Pts',(-19.0867832058502,-21.3949012055344,
124.573882634977)) ;
#59458 = CARTESIAN_POINT('Ctrl Pts',(-19.2621059878606,-21.5847975537594,
124.912011501582)) ;
#59459 = CARTESIAN_POINT('Ctrl Pts',(-19.2915499957338,-21.4048084733965,
124.611973405595)) ;
#59460 = CARTESIAN_POINT('Ctrl Pts',(-19.523241461829,-21.5947358975846,124.914993347183)) ;
#59461 = CARTESIAN_POINT('Ctrl Pts',(-19.5004581837589,-21.4147468172218,
124.61435673395)) ;
#59462 = CARTESIAN_POINT('Ctrl Pts',(-19.7826877608653,-21.6047393168851,
124.872466522298)) ;
#59463 = CARTESIAN_POINT('Ctrl Pts',(-19.7080148132996,-21.4247502365222,
124.580333183701)) ;
#59464 = CARTESIAN_POINT('Ctrl Pts',(-20.0313953526163,-21.6147738675922,
124.784868563439)) ;
#59465 = CARTESIAN_POINT('Ctrl Pts',(-19.9069801784579,-21.4347847872293,
124.510252765367)) ;
#59466 = CARTESIAN_POINT('Ctrl Pts',(-20.2570175361055,-21.6246188171978,
124.658232944476)) ;
#59467 = CARTESIAN_POINT('Ctrl Pts',(-20.0874764875126,-21.4446297368349,
124.408942636223)) ;
#59468 = CARTESIAN_POINT('Ctrl Pts',(-20.4603562191612,-21.6346046593107,
124.492418457877)) ;
#59469 = CARTESIAN_POINT('Ctrl Pts',(-20.2501460171759,-21.4546155789478,
124.276289513827)) ;
#59470 = CARTESIAN_POINT('Ctrl Pts',(-20.6311392301702,-21.6445394666798,
124.294885221514)) ;
#59471 = CARTESIAN_POINT('Ctrl Pts',(-20.3867706983452,-21.4645503863169,
124.118261777518)) ;
#59472 = CARTESIAN_POINT('Ctrl Pts',(-20.7664361277187,-21.6545970083931,
124.067883129677)) ;
#59473 = CARTESIAN_POINT('Ctrl Pts',(-20.4950064705292,-21.4746079280302,
123.936658954064)) ;
#59474 = CARTESIAN_POINT('Ctrl Pts',(-20.8584564948569,-21.6644186059052,
123.826712005177)) ;
#59475 = CARTESIAN_POINT('Ctrl Pts',(-20.5686206343265,-21.4844295255424,
123.743721915454)) ;
#59476 = CARTESIAN_POINT('Ctrl Pts',(-20.9088388978743,-21.6744748653857,
123.567314526484)) ;
#59477 = CARTESIAN_POINT('Ctrl Pts',(-20.6089246277522,-21.4944857850228,
123.536203466964)) ;
#59478 = CARTESIAN_POINT('Ctrl Pts',(-20.912905442173,-21.6844148016861,123.306120784318)) ;
#59479 = CARTESIAN_POINT('Ctrl Pts',(-20.61217581895,-21.5044257213232,123.327248710015)) ;
#59480 = CARTESIAN_POINT('Ctrl Pts',(-20.8724715625939,-21.6943219224305,
123.048933898916)) ;
#59481 = CARTESIAN_POINT('Ctrl Pts',(-20.5798268670816,-21.5143328420676,
123.121499921516)) ;
#59482 = CARTESIAN_POINT('Ctrl Pts',(-20.7867471086995,-21.7043648283558,
122.799333949718)) ;
#59483 = CARTESIAN_POINT('Ctrl Pts',(-20.5112454371669,-21.5243757479929,
122.921820528242)) ;
#59484 = CARTESIAN_POINT('Ctrl Pts',(-20.6607421010669,-21.714272609455,122.571477249608)) ;
#59485 = CARTESIAN_POINT('Ctrl Pts',(-20.4104399317555,-21.5342835290921,
122.739536474708)) ;
#59486 = CARTESIAN_POINT('Ctrl Pts',(-20.4957543255686,-21.7242829784574,
122.366574426333)) ;
#59487 = CARTESIAN_POINT('Ctrl Pts',(-20.2784482779818,-21.5442938980945,
122.575615429182)) ;
#59488 = CARTESIAN_POINT('Ctrl Pts',(-20.2969450012254,-21.7343138170262,
122.19348877084)) ;
#59489 = CARTESIAN_POINT('Ctrl Pts',(-20.1193995041773,-21.5543247366633,
122.437148355907)) ;
#59490 = CARTESIAN_POINT('Ctrl Pts',(-20.0753430040453,-21.7441666566659,
122.059562188914)) ;
#59491 = CARTESIAN_POINT('Ctrl Pts',(-19.9421175002561,-21.564177576303,122.330009052223)) ;
#59492 = CARTESIAN_POINT('Ctrl Pts',(-19.8307389892015,-21.7541546578309,
121.964427436421)) ;
#59493 = CARTESIAN_POINT('Ctrl Pts',(-19.7464337668386,-21.574165577468,122.253902995604)) ;
#59494 = CARTESIAN_POINT('Ctrl Pts',(-19.5748309877734,-21.76408347681,121.913501885889)) ;
#59495 = CARTESIAN_POINT('Ctrl Pts',(-19.5417073934896,-21.5840943964472,
122.213164409837)) ;
#59496 = CARTESIAN_POINT('Ctrl Pts',(-19.3124241042443,-21.7740711795323,
121.907308024055)) ;
#59497 = CARTESIAN_POINT('Ctrl Pts',(-19.3317819920219,-21.5940820991695,
122.208211065179)) ;
#59498 = CARTESIAN_POINT('Ctrl Pts',(-19.0517647367421,-21.784107179335,121.947395958042)) ;
#59499 = CARTESIAN_POINT('Ctrl Pts',(-19.1232547049505,-21.6041180989721,
122.240283218186)) ;
#59500 = CARTESIAN_POINT('Ctrl Pts',(-18.8063639187183,-21.7939620491364,
122.030208537148)) ;
#59501 = CARTESIAN_POINT('Ctrl Pts',(-18.9269353053611,-21.6139729687736,
122.306534697317)) ;
#59502 = CARTESIAN_POINT('Ctrl Pts',(-18.5756220536227,-21.80396147956,122.155848712853)) ;
#59503 = CARTESIAN_POINT('Ctrl Pts',(-18.7423427130502,-21.6239723991971,
122.407048265854)) ;
#59504 = CARTESIAN_POINT('Ctrl Pts',(-18.3721015982493,-21.8138565970253,
122.317772569663)) ;
#59505 = CARTESIAN_POINT('Ctrl Pts',(-18.5795278239004,-21.6338675166624,
122.536588260672)) ;
#59506 = CARTESIAN_POINT('Ctrl Pts',(-18.1969788650756,-21.8239170905422,
122.515789157084)) ;
#59507 = CARTESIAN_POINT('Ctrl Pts',(-18.4394307367387,-21.6439280101794,
122.695002760507)) ;
#59508 = CARTESIAN_POINT('Ctrl Pts',(-18.0616465449145,-21.8337665707434,
122.736447563643)) ;
#59509 = CARTESIAN_POINT('Ctrl Pts',(-18.3311666894869,-21.6537774903805,
122.871529616356)) ;
#59510 = CARTESIAN_POINT('Ctrl Pts',(-17.9643529997641,-21.8437930210072,
122.981307539562)) ;
#59511 = CARTESIAN_POINT('Ctrl Pts',(-18.2533332210301,-21.6638039406443,
123.067418172796)) ;
#59512 = CARTESIAN_POINT('Ctrl Pts',(-17.911737129383,-21.8538243114853,123.239620782822)) ;
#59513 = CARTESIAN_POINT('Ctrl Pts',(-18.2112421016013,-21.6738352311224,
123.274069149451)) ;
#59514 = CARTESIAN_POINT('Ctrl Pts',(-17.9043414975955,-21.8636656991371,
123.498138969836)) ;
#59515 = CARTESIAN_POINT('Ctrl Pts',(-18.2053271327317,-21.6836766187742,
123.480882829659)) ;
#59516 = CARTESIAN_POINT('Ctrl Pts',(-17.9420552180239,-21.8736691000283,
123.758271923707)) ;
#59517 = CARTESIAN_POINT('Ctrl Pts',(-18.2354994952421,-21.6936800196655,
123.688988903637)) ;
#59518 = CARTESIAN_POINT('Ctrl Pts',(-18.0243333212748,-21.8836534828195,
124.007465107845)) ;
#59519 = CARTESIAN_POINT('Ctrl Pts',(-18.3013232846925,-21.7036644024566,
123.888342843706)) ;
#59520 = CARTESIAN_POINT('Ctrl Pts',(-18.1494974495607,-21.8936925728329,
124.239670692868)) ;
#59521 = CARTESIAN_POINT('Ctrl Pts',(-18.4014559474029,-21.71370349247,124.074106700481)) ;
#59522 = CARTESIAN_POINT('Ctrl Pts',(-18.3096733742783,-21.9035383817421,
124.442892027175)) ;
#59523 = CARTESIAN_POINT('Ctrl Pts',(-18.5295972153698,-21.7235493013792,
124.236682156643)) ;
#59524 = CARTESIAN_POINT('Ctrl Pts',(-18.5050211085327,-21.9135228045611,
124.618000034142)) ;
#59525 = CARTESIAN_POINT('Ctrl Pts',(-18.6858761220133,-21.7335337241982,
124.376767460048)) ;
#59526 = CARTESIAN_POINT('Ctrl Pts',(-18.7268105926817,-21.9234624298023,
124.756042327652)) ;
#59527 = CARTESIAN_POINT('Ctrl Pts',(-18.8633080134688,-21.7434733494394,
124.487199981582)) ;
#59528 = CARTESIAN_POINT('Ctrl Pts',(-18.9716093217471,-21.9335021193209,
124.854379340595)) ;
#59529 = CARTESIAN_POINT('Ctrl Pts',(-19.0591475870826,-21.7535130389581,
124.565868438061)) ;
#59530 = CARTESIAN_POINT('Ctrl Pts',(-19.2258769015638,-21.9433903077395,
124.908032136323)) ;
#59531 = CARTESIAN_POINT('Ctrl Pts',(-19.2625611888641,-21.7634012273766,
124.608789286634)) ;
#59532 = CARTESIAN_POINT('Ctrl Pts',(-19.4882188467763,-21.9533798337416,
124.917301153433)) ;
#59533 = CARTESIAN_POINT('Ctrl Pts',(-19.4724346146083,-21.7733907533787,
124.616203339472)) ;
#59534 = CARTESIAN_POINT('Ctrl Pts',(-19.7473517520323,-21.9633383350968,
124.88079179001)) ;
#59535 = CARTESIAN_POINT('Ctrl Pts',(-19.679740427849,-21.7833492547339,124.586994707607)) ;
#59536 = CARTESIAN_POINT('Ctrl Pts',(-19.9949571853173,-21.9732379291004,
124.800926502595)) ;
#59537 = CARTESIAN_POINT('Ctrl Pts',(-19.8778237805908,-21.7932488487375,
124.523101689369)) ;
#59538 = CARTESIAN_POINT('Ctrl Pts',(-20.2282969934944,-21.9832858172217,
124.67739751358)) ;
#59539 = CARTESIAN_POINT('Ctrl Pts',(-20.0644952773521,-21.8032967368588,
124.424277463967)) ;
#59540 = CARTESIAN_POINT('Ctrl Pts',(-20.4336615725465,-21.9931812424672,
124.51780896921)) ;
#59541 = CARTESIAN_POINT('Ctrl Pts',(-20.2287857314875,-21.8131921621044,
124.296606263855)) ;
#59542 = CARTESIAN_POINT('Ctrl Pts',(-20.6111028161255,-22.0032426331678,
124.321832200981)) ;
#59543 = CARTESIAN_POINT('Ctrl Pts',(-20.3707381429069,-21.8232535528049,
124.139823967692)) ;
#59544 = CARTESIAN_POINT('Ctrl Pts',(-20.7488672563639,-22.0130882168545,
124.102810049072)) ;
#59545 = CARTESIAN_POINT('Ctrl Pts',(-20.4809482739668,-21.8330991364916,
123.964606606129)) ;
#59546 = CARTESIAN_POINT('Ctrl Pts',(-20.8484784322108,-22.0230511901637,
123.860702848364)) ;
#59547 = CARTESIAN_POINT('Ctrl Pts',(-20.5606363386565,-21.8430621098008,
123.770920863267)) ;
#59548 = CARTESIAN_POINT('Ctrl Pts',(-20.9045567467684,-22.0330768569895,
123.603259320304)) ;
#59549 = CARTESIAN_POINT('Ctrl Pts',(-20.6054981356393,-21.8530877766266,
123.564965788728)) ;
#59550 = CARTESIAN_POINT('Ctrl Pts',(-20.9151055478435,-22.0429913348558,
123.342939247587)) ;
#59551 = CARTESIAN_POINT('Ctrl Pts',(-20.6139362973576,-21.8630022544929,
123.356710337489)) ;
#59552 = CARTESIAN_POINT('Ctrl Pts',(-20.8805485313156,-22.0529798495308,
123.082714706942)) ;
#59553 = CARTESIAN_POINT('Ctrl Pts',(-20.586289982988,-21.8729907691679,123.148530979108)) ;
#59554 = CARTESIAN_POINT('Ctrl Pts',(-20.8003679518013,-22.0630239604462,
122.831264561867)) ;
#59555 = CARTESIAN_POINT('Ctrl Pts',(-20.5221446448977,-21.8830348800833,
122.947370978964)) ;
#59556 = CARTESIAN_POINT('Ctrl Pts',(-20.6809098953037,-22.0728520980408,
122.602235481647)) ;
#59557 = CARTESIAN_POINT('Ctrl Pts',(-20.4265781234052,-21.8928630176779,
122.76414910543)) ;
#59558 = CARTESIAN_POINT('Ctrl Pts',(-20.5196736795458,-22.0829286660997,
122.392249516455)) ;
#59559 = CARTESIAN_POINT('Ctrl Pts',(-20.2975883848863,-21.9029395857368,
122.596160459755)) ;
#59560 = CARTESIAN_POINT('Ctrl Pts',(-20.328782028387,-22.0927808280039,122.217258955797)) ;
#59561 = CARTESIAN_POINT('Ctrl Pts',(-20.1448754008448,-21.912791747641,122.456169202449)) ;
#59562 = CARTESIAN_POINT('Ctrl Pts',(-20.1057172725599,-22.1028537899607,
122.074824536988)) ;
#59563 = CARTESIAN_POINT('Ctrl Pts',(-19.9664229786563,-21.9228647095978,
122.342221984015)) ;
#59564 = CARTESIAN_POINT('Ctrl Pts',(-19.8668228113398,-22.1126963519636,
121.975615871429)) ;
#59565 = CARTESIAN_POINT('Ctrl Pts',(-19.7753082232677,-21.9327072716007,
122.262856048578)) ;
#59566 = CARTESIAN_POINT('Ctrl Pts',(-19.6110214816132,-22.1226767884574,
121.917755554155)) ;
#59567 = CARTESIAN_POINT('Ctrl Pts',(-19.5706673154193,-21.9426877080945,
122.216568229645)) ;
#59568 = CARTESIAN_POINT('Ctrl Pts',(-19.3480335183811,-22.1326950937818,
121.905648968687)) ;
#59569 = CARTESIAN_POINT('Ctrl Pts',(-19.3602769131939,-21.9527060134189,
122.206883477632)) ;
#59570 = CARTESIAN_POINT('Ctrl Pts',(-19.090340079734,-22.1425790577013,121.938406487101)) ;
#59571 = CARTESIAN_POINT('Ctrl Pts',(-19.1541230782783,-21.9625899773384,
122.233089760099)) ;
#59572 = CARTESIAN_POINT('Ctrl Pts',(-18.8377600204759,-22.1526449344398,
122.016875429429)) ;
#59573 = CARTESIAN_POINT('Ctrl Pts',(-18.9520588488056,-21.9726558540769,
122.295865388187)) ;
#59574 = CARTESIAN_POINT('Ctrl Pts',(-18.6078114382176,-22.1624840353007,
122.135152615212)) ;
#59575 = CARTESIAN_POINT('Ctrl Pts',(-18.7681011911182,-21.9824949549378,
122.390486916667)) ;
#59576 = CARTESIAN_POINT('Ctrl Pts',(-18.3974600457705,-22.1725171181664,
122.294091316826)) ;
#59577 = CARTESIAN_POINT('Ctrl Pts',(-18.5998201180981,-21.9925280378036,
122.517638081399)) ;
#59578 = CARTESIAN_POINT('Ctrl Pts',(-18.2185627413665,-22.1825388034419,
122.487389938133)) ;
#59579 = CARTESIAN_POINT('Ctrl Pts',(-18.4567025086376,-22.002549723079,122.67227724618)) ;
#59580 = CARTESIAN_POINT('Ctrl Pts',(-18.0778211454052,-22.1924054985404,
122.70513209668)) ;
#59581 = CARTESIAN_POINT('Ctrl Pts',(-18.3441099857594,-22.0124164181775,
122.846470267623)) ;
#59582 = CARTESIAN_POINT('Ctrl Pts',(-17.9754225074273,-22.2023653882749,
122.946017980769)) ;
#59583 = CARTESIAN_POINT('Ctrl Pts',(-18.2621912862455,-22.0223763079121,
123.039178659271)) ;
#59584 = CARTESIAN_POINT('Ctrl Pts',(-17.9163607642041,-22.2124003761004,
123.203010659034)) ;
#59585 = CARTESIAN_POINT('Ctrl Pts',(-18.2149420385229,-22.0324112957375,
123.244772955829)) ;
#59586 = CARTESIAN_POINT('Ctrl Pts',(-17.9025839574836,-22.2222870801747,
123.462494584695)) ;
#59587 = CARTESIAN_POINT('Ctrl Pts',(-18.2039207061201,-22.0422979998118,
123.452359223595)) ;
#59588 = CARTESIAN_POINT('Ctrl Pts',(-17.9346959980839,-22.2323522244076,
123.724996117154)) ;
#59589 = CARTESIAN_POINT('Ctrl Pts',(-18.2296104579225,-22.0523631440447,
123.662360751984)) ;
#59590 = CARTESIAN_POINT('Ctrl Pts',(-18.0099377691919,-22.2421915151362,
123.972415043862)) ;
#59591 = CARTESIAN_POINT('Ctrl Pts',(-18.2898035447589,-22.0622024347733,
123.860294755891)) ;
#59592 = CARTESIAN_POINT('Ctrl Pts',(-18.1292969690806,-22.2522540725746,
124.208342841471)) ;
#59593 = CARTESIAN_POINT('Ctrl Pts',(-18.3852909705668,-22.0722649922117,
124.049037294054)) ;
#59594 = CARTESIAN_POINT('Ctrl Pts',(-18.2854516849338,-22.2621511238267,
124.416351010826)) ;
#59595 = CARTESIAN_POINT('Ctrl Pts',(-18.5102142588833,-22.0821620434638,
124.215443190149)) ;
#59596 = CARTESIAN_POINT('Ctrl Pts',(-18.4753956190122,-22.272082330575,124.595319409224)) ;
#59597 = CARTESIAN_POINT('Ctrl Pts',(-18.6621688310842,-22.0920932502121,
124.358617678543)) ;
#59598 = CARTESIAN_POINT('Ctrl Pts',(-18.6961275311406,-22.2821245147938,
124.739948983585)) ;
#59599 = CARTESIAN_POINT('Ctrl Pts',(-18.8387544167778,-22.1021354344309,
124.47432155666)) ;
#59600 = CARTESIAN_POINT('Ctrl Pts',(-18.9348029986765,-22.2920111429047,
124.842623278117)) ;
#59601 = CARTESIAN_POINT('Ctrl Pts',(-19.0296939129993,-22.1120220625418,
124.556460832634)) ;
#59602 = CARTESIAN_POINT('Ctrl Pts',(-19.190281558459,-22.3020044154371,124.903358057767)) ;
#59603 = CARTESIAN_POINT('Ctrl Pts',(-19.2340765313827,-22.1220153350742,
124.605048920887)) ;
#59604 = CARTESIAN_POINT('Ctrl Pts',(-19.4511817330596,-22.3119494909786,
124.918648968524)) ;
#59605 = CARTESIAN_POINT('Ctrl Pts',(-19.442796174619,-22.1319604106157,124.61728190834)) ;
#59606 = CARTESIAN_POINT('Ctrl Pts',(-19.7109595708651,-22.3218990417068,
124.888897659172)) ;
#59607 = CARTESIAN_POINT('Ctrl Pts',(-19.6506180532169,-22.141909961344,124.593481323135)) ;
#59608 = CARTESIAN_POINT('Ctrl Pts',(-19.963792160214,-22.3319383765548,124.813587576149)) ;
#59609 = CARTESIAN_POINT('Ctrl Pts',(-19.8528843512006,-22.1519492961919,
124.533233558072)) ;
#59610 = CARTESIAN_POINT('Ctrl Pts',(-20.196245173065,-22.3418245154987,124.697521392829)) ;
#59611 = CARTESIAN_POINT('Ctrl Pts',(-20.0388461770694,-22.1618354351359,
124.440381365318)) ;
#59612 = CARTESIAN_POINT('Ctrl Pts',(-20.4075357060316,-22.3518226284724,
124.541405526169)) ;
#59613 = CARTESIAN_POINT('Ctrl Pts',(-20.2078787966008,-22.1718335481096,
124.315489143515)) ;
#59614 = CARTESIAN_POINT('Ctrl Pts',(-20.5872481934702,-22.3617423908249,
124.352530361773)) ;
#59615 = CARTESIAN_POINT('Ctrl Pts',(-20.3516487449868,-22.181753310462,124.164389831893)) ;
#59616 = CARTESIAN_POINT('Ctrl Pts',(-20.7332188476262,-22.3717817864375,
124.132782767646)) ;
#59617 = CARTESIAN_POINT('Ctrl Pts',(-20.4684258066509,-22.1917927060747,
123.988591943343)) ;
#59618 = CARTESIAN_POINT('Ctrl Pts',(-20.8373803848515,-22.3816909722258,
123.894117096644)) ;
#59619 = CARTESIAN_POINT('Ctrl Pts',(-20.5517552368214,-22.2017018918629,
123.797660275818)) ;
#59620 = CARTESIAN_POINT('Ctrl Pts',(-20.8993918232317,-22.3916261563833,
123.640499494821)) ;
#59621 = CARTESIAN_POINT('Ctrl Pts',(-20.6013649575712,-22.2116370760204,
123.594766873805)) ;
#59622 = CARTESIAN_POINT('Ctrl Pts',(-20.9163470243233,-22.4016672137692,
123.377183112359)) ;
#59623 = CARTESIAN_POINT('Ctrl Pts',(-20.6149297759424,-22.2216781334063,
123.38411366101)) ;
#59624 = CARTESIAN_POINT('Ctrl Pts',(-20.8879521472035,-22.4115543718025,
123.118900643946)) ;
#59625 = CARTESIAN_POINT('Ctrl Pts',(-20.5922146560384,-22.2315652914396,
123.177488436444)) ;
#59626 = CARTESIAN_POINT('Ctrl Pts',(-20.8147966666412,-22.4215466514784,
122.866729097642)) ;
#59627 = CARTESIAN_POINT('Ctrl Pts',(-20.5336910860111,-22.2415575711155,
122.97575113261)) ;
#59628 = CARTESIAN_POINT('Ctrl Pts',(-20.6993946933195,-22.4314951685235,
122.632124438289)) ;
#59629 = CARTESIAN_POINT('Ctrl Pts',(-20.4413704002996,-22.2515060881606,
122.788067448919)) ;
#59630 = CARTESIAN_POINT('Ctrl Pts',(-20.5455120187168,-22.4414319460939,
122.421182047729)) ;
#59631 = CARTESIAN_POINT('Ctrl Pts',(-20.3182652644741,-22.261442865731,122.619313435312)) ;
#59632 = CARTESIAN_POINT('Ctrl Pts',(-20.3566546113368,-22.4514149822408,
122.239043334206)) ;
#59633 = CARTESIAN_POINT('Ctrl Pts',(-20.1671801441174,-22.2714259018779,
122.473601924756)) ;
#59634 = CARTESIAN_POINT('Ctrl Pts',(-20.1374997937318,-22.4614587338345,
122.092007982459)) ;
#59635 = CARTESIAN_POINT('Ctrl Pts',(-19.9918566291476,-22.2814696534717,
122.355972866551)) ;
#59636 = CARTESIAN_POINT('Ctrl Pts',(-19.9014984819869,-22.4712872630471,
121.986966332369)) ;
#59637 = CARTESIAN_POINT('Ctrl Pts',(-19.803057030311,-22.2912981826842,122.27193912262)) ;
#59638 = CARTESIAN_POINT('Ctrl Pts',(-19.644672669795,-22.4813626239558,121.922812414429)) ;
#59639 = CARTESIAN_POINT('Ctrl Pts',(-19.5975962939444,-22.3013735435929,
122.220614925738)) ;
#59640 = CARTESIAN_POINT('Ctrl Pts',(-19.3862413607618,-22.491219222843,121.904531259593)) ;
#59641 = CARTESIAN_POINT('Ctrl Pts',(-19.3908522878681,-22.3112301424801,
122.205989042091)) ;
#59642 = CARTESIAN_POINT('Ctrl Pts',(-19.1232446773172,-22.5012822168609,
121.931678446646)) ;
#59643 = CARTESIAN_POINT('Ctrl Pts',(-19.1804545703553,-22.321293136498,122.227705729695)) ;
#59644 = CARTESIAN_POINT('Ctrl Pts',(-18.8735448281778,-22.5111601511503,
122.002791143889)) ;
#59645 = CARTESIAN_POINT('Ctrl Pts',(-18.9806951761436,-22.3311710707875,
122.284594621574)) ;
#59646 = CARTESIAN_POINT('Ctrl Pts',(-18.6369922199882,-22.5211607987084,
122.117182286071)) ;
#59647 = CARTESIAN_POINT('Ctrl Pts',(-18.7914526693458,-22.3411717183456,
122.376106428338)) ;
#59648 = CARTESIAN_POINT('Ctrl Pts',(-18.4254683343915,-22.5310786451465,
122.269531684477)) ;
#59649 = CARTESIAN_POINT('Ctrl Pts',(-18.6222333099972,-22.3510895647836,
122.497984627214)) ;
#59650 = CARTESIAN_POINT('Ctrl Pts',(-18.2412825269459,-22.5411297621521,
122.45879123557)) ;
#59651 = CARTESIAN_POINT('Ctrl Pts',(-18.4748836852717,-22.3611406817893,
122.649391549011)) ;
#59652 = CARTESIAN_POINT('Ctrl Pts',(-18.0951286476762,-22.5510004974627,
122.673148447113)) ;
#59653 = CARTESIAN_POINT('Ctrl Pts',(-18.3579599995673,-22.3710114170999,
122.820875923692)) ;
#59654 = CARTESIAN_POINT('Ctrl Pts',(-17.986241610246,-22.5610712047057,122.914310640418)) ;
#59655 = CARTESIAN_POINT('Ctrl Pts',(-18.270849088114,-22.3810821243429,123.013805409563)) ;
#59656 = CARTESIAN_POINT('Ctrl Pts',(-17.9222939724761,-22.5709042121576,
123.164699747312)) ;
#59657 = CARTESIAN_POINT('Ctrl Pts',(-18.2196899694515,-22.3909151317947,
123.214115380671)) ;
#59658 = CARTESIAN_POINT('Ctrl Pts',(-17.9016542679233,-22.5809347044599,
123.427471548306)) ;
#59659 = CARTESIAN_POINT('Ctrl Pts',(-18.2031767454531,-22.400945624097,123.424332776703)) ;
#59660 = CARTESIAN_POINT('Ctrl Pts',(-17.927723884169,-22.5909662995333,123.689813957202)) ;
#59661 = CARTESIAN_POINT('Ctrl Pts',(-18.2240311522087,-22.4109772191704,
123.634206897862)) ;
#59662 = CARTESIAN_POINT('Ctrl Pts',(-17.9969878123147,-22.6007959986715,
123.93865131243)) ;
#59663 = CARTESIAN_POINT('Ctrl Pts',(-18.2794406618939,-22.4208069183087,
123.833276183553)) ;
#59664 = CARTESIAN_POINT('Ctrl Pts',(-18.1095198729244,-22.6107854485531,
124.175829191989)) ;
#59665 = CARTESIAN_POINT('Ctrl Pts',(-18.3694648327991,-22.4307963681902,
124.023019031505)) ;
#59666 = CARTESIAN_POINT('Ctrl Pts',(-18.2628916857644,-22.6208293063688,
124.390633246382)) ;
#59667 = CARTESIAN_POINT('Ctrl Pts',(-18.4921611832323,-22.4408402260059,
124.194863205091)) ;
#59668 = CARTESIAN_POINT('Ctrl Pts',(-18.446692434265,-22.630650996959,124.571839161793)) ;
#59669 = CARTESIAN_POINT('Ctrl Pts',(-18.6391999895716,-22.4506619165961,
124.339828335497)) ;
#59670 = CARTESIAN_POINT('Ctrl Pts',(-18.6634124377873,-22.6406860874994,
124.722085054435)) ;
#59671 = CARTESIAN_POINT('Ctrl Pts',(-18.8125751167322,-22.4606970071365,
124.460026463756)) ;
#59672 = CARTESIAN_POINT('Ctrl Pts',(-18.9029886662497,-22.6507106064821,
124.831675526016)) ;
#59673 = CARTESIAN_POINT('Ctrl Pts',(-19.0042354735576,-22.4707215261192,
124.547700237809)) ;
#59674 = CARTESIAN_POINT('Ctrl Pts',(-19.1536198777574,-22.6605704518923,
124.897332264122)) ;
#59675 = CARTESIAN_POINT('Ctrl Pts',(-19.204739284053,-22.4805813715294,124.600226994176)) ;
#59676 = CARTESIAN_POINT('Ctrl Pts',(-19.4144244913002,-22.670530228208,124.919409092967)) ;
#59677 = CARTESIAN_POINT('Ctrl Pts',(-19.4133825651792,-22.4905411478451,
124.617890170222)) ;
#59678 = CARTESIAN_POINT('Ctrl Pts',(-19.6768496651292,-22.6805584255226,
124.895342097645)) ;
#59679 = CARTESIAN_POINT('Ctrl Pts',(-19.6233228939347,-22.5005693451597,
124.598638241263)) ;
#59680 = CARTESIAN_POINT('Ctrl Pts',(-19.9281559636117,-22.6904659678129,
124.827199646983)) ;
#59681 = CARTESIAN_POINT('Ctrl Pts',(-19.8243678986999,-22.51047688745,124.544126081424)) ;
#59682 = CARTESIAN_POINT('Ctrl Pts',(-20.1667897461997,-22.7004986183768,
124.715157775083)) ;
#59683 = CARTESIAN_POINT('Ctrl Pts',(-20.0152757027157,-22.5205095380139,
124.454494146685)) ;
#59684 = CARTESIAN_POINT('Ctrl Pts',(-20.3792168210052,-22.7103825748034,
124.56567950925)) ;
#59685 = CARTESIAN_POINT('Ctrl Pts',(-20.1852178909652,-22.5303934944406,
124.334913312455)) ;
#59686 = CARTESIAN_POINT('Ctrl Pts',(-20.5648833309736,-22.7203722761653,
124.380082284069)) ;
#59687 = CARTESIAN_POINT('Ctrl Pts',(-20.333752327996,-22.5403831958024,124.18643693813)) ;
#59688 = CARTESIAN_POINT('Ctrl Pts',(-20.7158142403492,-22.7304132714413,
124.163643559951)) ;
#59689 = CARTESIAN_POINT('Ctrl Pts',(-20.454498551908,-22.5504241910784,124.013286914038)) ;
#59690 = CARTESIAN_POINT('Ctrl Pts',(-20.8249543879318,-22.7402461607097,
123.929430163563)) ;
#59691 = CARTESIAN_POINT('Ctrl Pts',(-20.5418120172613,-22.5602570803468,
123.825917666245)) ;
#59692 = CARTESIAN_POINT('Ctrl Pts',(-20.8935867559205,-22.7502393190771,
123.675951817842)) ;
#59693 = CARTESIAN_POINT('Ctrl Pts',(-20.5967197715693,-22.5702502387142,
123.623135597207)) ;
#59694 = CARTESIAN_POINT('Ctrl Pts',(-20.9167106283028,-22.7602713614292,
123.413324039136)) ;
#59695 = CARTESIAN_POINT('Ctrl Pts',(-20.6152207367782,-22.5802822810663,
123.413033509542)) ;
#59696 = CARTESIAN_POINT('Ctrl Pts',(-20.8945827853963,-22.7701366053876,
123.155034786092)) ;
#59697 = CARTESIAN_POINT('Ctrl Pts',(-20.5975204254551,-22.5901475250248,
123.206402523635)) ;
#59698 = CARTESIAN_POINT('Ctrl Pts',(-20.82800234089,-22.7800984966336,122.901847296241)) ;
#59699 = CARTESIAN_POINT('Ctrl Pts',(-20.5442580738547,-22.6001094162708,
123.003852212977)) ;
#59700 = CARTESIAN_POINT('Ctrl Pts',(-20.7172881603951,-22.7901333966521,
122.662521920387)) ;
#59701 = CARTESIAN_POINT('Ctrl Pts',(-20.4556884995148,-22.6101443162892,
122.812391063934)) ;
#59702 = CARTESIAN_POINT('Ctrl Pts',(-20.5692752424808,-22.8000184770667,
122.449004039222)) ;
#59703 = CARTESIAN_POINT('Ctrl Pts',(-20.3372800779245,-22.6200293967038,
122.641575980296)) ;
#59704 = CARTESIAN_POINT('Ctrl Pts',(-20.3831352080727,-22.8100836491915,
122.261135086256)) ;
#59705 = CARTESIAN_POINT('Ctrl Pts',(-20.1883694027549,-22.6300945688287,
122.491279318454)) ;
#59706 = CARTESIAN_POINT('Ctrl Pts',(-20.1719153765991,-22.819930883915,122.111588554488)) ;
#59707 = CARTESIAN_POINT('Ctrl Pts',(-20.0193951546591,-22.6399418035521,
122.37164074922)) ;
#59708 = CARTESIAN_POINT('Ctrl Pts',(-19.9338810019722,-22.8299616952328,
121.998385955222)) ;
#59709 = CARTESIAN_POINT('Ctrl Pts',(-19.8289685381442,-22.6499726148699,
122.281076763213)) ;
#59710 = CARTESIAN_POINT('Ctrl Pts',(-19.6801542546242,-22.8399713111463,
121.928888950712)) ;
#59711 = CARTESIAN_POINT('Ctrl Pts',(-19.6259877257716,-22.6599822307834,
122.225477204985)) ;
#59712 = CARTESIAN_POINT('Ctrl Pts',(-19.4208786354196,-22.84988209055,121.904493618432)) ;
#59713 = CARTESIAN_POINT('Ctrl Pts',(-19.4185677565269,-22.6698930101871,
122.20595890965)) ;
#59714 = CARTESIAN_POINT('Ctrl Pts',(-19.1607322268354,-22.859811356339,121.924877430898)) ;
#59715 = CARTESIAN_POINT('Ctrl Pts',(-19.2104507120868,-22.6798222759761,
122.222263811396)) ;
#59716 = CARTESIAN_POINT('Ctrl Pts',(-18.9052696006217,-22.8698540496516,
121.991077325652)) ;
#59717 = CARTESIAN_POINT('Ctrl Pts',(-19.0060800555527,-22.6898649692887,
122.275221687729)) ;
#59718 = CARTESIAN_POINT('Ctrl Pts',(-18.6688210508467,-22.8797405823464,
122.098781259546)) ;
#59719 = CARTESIAN_POINT('Ctrl Pts',(-18.8169206428243,-22.6997515019835,
122.361382756701)) ;
#59720 = CARTESIAN_POINT('Ctrl Pts',(-18.4521283292672,-22.8897337274496,
122.247107144986)) ;
#59721 = CARTESIAN_POINT('Ctrl Pts',(-18.6435653091888,-22.7097446470868,
122.480041629506)) ;
#59722 = CARTESIAN_POINT('Ctrl Pts',(-18.2654318576276,-22.8996794081237,
122.430014319229)) ;
#59723 = CARTESIAN_POINT('Ctrl Pts',(-18.4942067535944,-22.7196903277608,
122.626365697427)) ;
#59724 = CARTESIAN_POINT('Ctrl Pts',(-18.1128639588266,-22.9096266657504,
122.642292140986)) ;
#59725 = CARTESIAN_POINT('Ctrl Pts',(-18.372150743422,-22.7296375853876,122.796186542585)) ;
#59726 = CARTESIAN_POINT('Ctrl Pts',(-17.9986015572507,-22.9196745678719,
122.880328253833)) ;
#59727 = CARTESIAN_POINT('Ctrl Pts',(-18.280738856107,-22.739685487509,122.986614497746)) ;
#59728 = CARTESIAN_POINT('Ctrl Pts',(-17.9286121291567,-22.9295222734936,
123.129473138919)) ;
#59729 = CARTESIAN_POINT('Ctrl Pts',(-18.2247452886835,-22.7495331931307,
123.18592950677)) ;
#59730 = CARTESIAN_POINT('Ctrl Pts',(-17.9018275042711,-22.9394837401277,
123.389866644002)) ;
#59731 = CARTESIAN_POINT('Ctrl Pts',(-18.2033153717119,-22.7594946597648,
123.394243983057)) ;
#59732 = CARTESIAN_POINT('Ctrl Pts',(-17.9211473399048,-22.9495132933959,
123.652733485376)) ;
#59733 = CARTESIAN_POINT('Ctrl Pts',(-18.2187690258878,-22.769524213033,123.604537583863)) ;
#59734 = CARTESIAN_POINT('Ctrl Pts',(-17.9848788717473,-22.9594201854233,
123.905158576402)) ;
#59735 = CARTESIAN_POINT('Ctrl Pts',(-18.2697520510413,-22.7794311050604,
123.806478038071)) ;
#59736 = CARTESIAN_POINT('Ctrl Pts',(-18.0914378078134,-22.9693678295363,
124.143845240036)) ;
#59737 = CARTESIAN_POINT('Ctrl Pts',(-18.3549971072633,-22.7893787491735,
123.997428193049)) ;
#59738 = CARTESIAN_POINT('Ctrl Pts',(-18.2384883382395,-22.9793678725652,
124.361682579422)) ;
#59739 = CARTESIAN_POINT('Ctrl Pts',(-18.4726356373326,-22.7993787922023,
124.17169927459)) ;
#59740 = CARTESIAN_POINT('Ctrl Pts',(-18.4221353271476,-22.9894066385592,
124.551044334108)) ;
#59741 = CARTESIAN_POINT('Ctrl Pts',(-18.6195515901072,-22.8094175581963,
124.323190202852)) ;
#59742 = CARTESIAN_POINT('Ctrl Pts',(-18.6310313255418,-22.9992317005814,
124.702816918751)) ;
#59743 = CARTESIAN_POINT('Ctrl Pts',(-18.7866669492004,-22.8192426202186,
124.444610004211)) ;
#59744 = CARTESIAN_POINT('Ctrl Pts',(-18.8683046803637,-23.0092862479078,
124.81903454041)) ;
#59745 = CARTESIAN_POINT('Ctrl Pts',(-18.9764846127344,-22.8292971675449,
124.537586113637)) ;
#59746 = CARTESIAN_POINT('Ctrl Pts',(-19.1194917233323,-23.019229491357,124.891049871198)) ;
#59747 = CARTESIAN_POINT('Ctrl Pts',(-19.1774335457929,-22.8392404109942,
124.59520052088)) ;
#59748 = CARTESIAN_POINT('Ctrl Pts',(-19.3782034066478,-23.0291316629649,
124.919048155738)) ;
#59749 = CARTESIAN_POINT('Ctrl Pts',(-19.3844026140547,-22.849142582602,124.617601382244)) ;
#59750 = CARTESIAN_POINT('Ctrl Pts',(-19.6417720055539,-23.0391844985751,
124.9012746228)) ;
#59751 = CARTESIAN_POINT('Ctrl Pts',(-19.5952575647132,-22.8591954182122,
124.603384820688)) ;
#59752 = CARTESIAN_POINT('Ctrl Pts',(-19.8937094829923,-23.0490575562606,
124.839234191459)) ;
#59753 = CARTESIAN_POINT('Ctrl Pts',(-19.7968081119254,-22.8690684758978,
124.553754624461)) ;
#59754 = CARTESIAN_POINT('Ctrl Pts',(-20.1342348698061,-23.0590528177863,
124.733693798384)) ;
#59755 = CARTESIAN_POINT('Ctrl Pts',(-19.9892291535961,-22.8790637374234,
124.469324531308)) ;
#59756 = CARTESIAN_POINT('Ctrl Pts',(-20.3531841875638,-23.0690781872068,
124.587158170132)) ;
#59757 = CARTESIAN_POINT('Ctrl Pts',(-20.1643902941915,-22.8890891068439,
124.352097370289)) ;
#59758 = CARTESIAN_POINT('Ctrl Pts',(-20.5410358788454,-23.0789680197334,
124.407538039965)) ;
#59759 = CARTESIAN_POINT('Ctrl Pts',(-20.3146713621505,-22.8989789393705,
124.208404998467)) ;
#59760 = CARTESIAN_POINT('Ctrl Pts',(-20.74814931711,-23.0922659905428,124.126127329763)) ;
#59761 = CARTESIAN_POINT('Ctrl Pts',(-20.4803737638767,-22.9122769101799,
123.98326757738)) ;
#59762 = CARTESIAN_POINT('Ctrl Pts',(-20.87663678955,-23.105464385652,123.799667857733)) ;
#59763 = CARTESIAN_POINT('Ctrl Pts',(-20.58316718686,-22.9254753052891,123.722071594726)) ;
#59764 = CARTESIAN_POINT('Ctrl Pts',(-20.9162580761209,-23.1188598279314,
123.449902418922)) ;
#59765 = CARTESIAN_POINT('Ctrl Pts',(-20.6148571213026,-22.9388707475686,
123.442305273441)) ;
#59766 = CARTESIAN_POINT('Ctrl Pts',(-20.9004717403109,-23.1287356661704,
123.190816756868)) ;
#59767 = CARTESIAN_POINT('Ctrl Pts',(-20.6022321474832,-22.9487465858075,
123.235027218103)) ;
#59768 = CARTESIAN_POINT('Ctrl Pts',(-20.8389416666321,-23.1387970687681,
122.933714939038)) ;
#59769 = CARTESIAN_POINT('Ctrl Pts',(-20.5530100608366,-22.9588079884053,
123.029348080478)) ;
#59770 = CARTESIAN_POINT('Ctrl Pts',(-20.7357971607144,-23.1486621257033,
122.69583283738)) ;
#59771 = CARTESIAN_POINT('Ctrl Pts',(-20.4704951899831,-22.9686730453404,
122.839039863601)) ;
#59772 = CARTESIAN_POINT('Ctrl Pts',(-20.5912157870178,-23.1586742216521,
122.476050346887)) ;
#59773 = CARTESIAN_POINT('Ctrl Pts',(-20.3548367390331,-22.9786851412892,
122.663215848403)) ;
#59774 = CARTESIAN_POINT('Ctrl Pts',(-20.3516936594044,-23.1719515307975,
122.222286259416)) ;
#59775 = CARTESIAN_POINT('Ctrl Pts',(-20.1631968596537,-22.9919624504346,
122.460187975031)) ;
#59776 = CARTESIAN_POINT('Ctrl Pts',(-19.9764398067608,-23.1885505563048,
121.990323874655)) ;
#59777 = CARTESIAN_POINT('Ctrl Pts',(-19.8630376390117,-23.0085614759419,
122.27463286839)) ;
#59778 = CARTESIAN_POINT('Ctrl Pts',(-19.5445846288261,-23.2051496043378,
121.900290049291)) ;
#59779 = CARTESIAN_POINT('Ctrl Pts',(-19.5174874237851,-23.025160523975,122.202591932357)) ;
#59780 = CARTESIAN_POINT('Ctrl Pts',(-19.197050432373,-23.2183930163688,121.919316506906)) ;
#59781 = CARTESIAN_POINT('Ctrl Pts',(-19.2395130687559,-23.0384039360059,
122.217815974426)) ;
#59782 = CARTESIAN_POINT('Ctrl Pts',(-18.9401631491161,-23.2284304440572,
121.979134289703)) ;
#59783 = CARTESIAN_POINT('Ctrl Pts',(-19.0339916375281,-23.0484413636943,
122.26566763804)) ;
#59784 = CARTESIAN_POINT('Ctrl Pts',(-18.7007825062615,-23.2383347460128,
122.08131781826)) ;
#59785 = CARTESIAN_POINT('Ctrl Pts',(-18.8424912391791,-23.0583456656499,
122.347410849636)) ;
#59786 = CARTESIAN_POINT('Ctrl Pts',(-18.4082618728628,-23.251601585988,122.271030307521)) ;
#59787 = CARTESIAN_POINT('Ctrl Pts',(-18.60846034993,-23.0716125056251,122.499189722715)) ;
#59788 = CARTESIAN_POINT('Ctrl Pts',(-18.1123399887699,-23.2682277840779,
122.599191193754)) ;
#59789 = CARTESIAN_POINT('Ctrl Pts',(-18.37173453001,-23.088238703715,122.761707661206)) ;
#59790 = CARTESIAN_POINT('Ctrl Pts',(-17.9131297581632,-23.2881468994613,
123.089717711788)) ;
#59791 = CARTESIAN_POINT('Ctrl Pts',(-18.2123565653371,-23.1081578190985,
123.154114524712)) ;
#59792 = CARTESIAN_POINT('Ctrl Pts',(-17.8962057487813,-23.3047533225956,
123.530754190466)) ;
#59793 = CARTESIAN_POINT('Ctrl Pts',(-18.1988208182487,-23.1247642422327,
123.506996945006)) ;
#59794 = CARTESIAN_POINT('Ctrl Pts',(-17.9736383080703,-23.3180495430913,
123.871481315084)) ;
#59795 = CARTESIAN_POINT('Ctrl Pts',(-18.260758884604,-23.1380604627284,123.779530840826)) ;
#59796 = CARTESIAN_POINT('Ctrl Pts',(-18.1080876895051,-23.3313183754327,
124.193291225439)) ;
#59797 = CARTESIAN_POINT('Ctrl Pts',(-18.3683238288418,-23.1513292950698,
124.03699746914)) ;
#59798 = CARTESIAN_POINT('Ctrl Pts',(-18.3795904845808,-23.3480096234658,
124.544002089629)) ;
#59799 = CARTESIAN_POINT('Ctrl Pts',(-18.5855160258156,-23.1680205431029,
124.317555357592)) ;
#59800 = CARTESIAN_POINT('Ctrl Pts',(-18.8243580038784,-23.3678193551386,
124.825895671555)) ;
#59801 = CARTESIAN_POINT('Ctrl Pts',(-18.9413318339364,-23.1878302747757,
124.543077599675)) ;
#59802 = CARTESIAN_POINT('Ctrl Pts',(-19.3426692477421,-23.3877969624672,
124.941057197669)) ;
#59803 = CARTESIAN_POINT('Ctrl Pts',(-19.3559797197809,-23.2078078821043,
124.635208534349)) ;
#59804 = CARTESIAN_POINT('Ctrl Pts',(-19.8676443126626,-23.407723271525,124.871649885225)) ;
#59805 = CARTESIAN_POINT('Ctrl Pts',(-19.7759608640312,-23.2277341911621,
124.579685870567)) ;
#59806 = CARTESIAN_POINT('Ctrl Pts',(-20.3358743901566,-23.4275401316897,
124.630155280585)) ;
#59807 = CARTESIAN_POINT('Ctrl Pts',(-20.1505472945724,-23.2475510513268,
124.386491407269)) ;
#59808 = CARTESIAN_POINT('Ctrl Pts',(-20.6978674016167,-23.4476399472837,
124.237525821763)) ;
#59809 = CARTESIAN_POINT('Ctrl Pts',(-20.4401428874829,-23.2676508669208,
124.072390151263)) ;
#59810 = CARTESIAN_POINT('Ctrl Pts',(-20.9010174941863,-23.4673969111663,
123.753071870117)) ;
#59811 = CARTESIAN_POINT('Ctrl Pts',(-20.6026658029561,-23.2874078308034,
123.684825804928)) ;
#59812 = CARTESIAN_POINT('Ctrl Pts',(-20.9280426935608,-23.4874338372357,
123.221391133714)) ;
#59813 = CARTESIAN_POINT('Ctrl Pts',(-20.6242875973045,-23.3074447568728,
123.259481619139)) ;
#59814 = CARTESIAN_POINT('Ctrl Pts',(-20.772426096765,-23.5073034196172,122.716597558778)) ;
#59815 = CARTESIAN_POINT('Ctrl Pts',(-20.4997956703775,-23.3273143392544,
122.855645015619)) ;
#59816 = CARTESIAN_POINT('Ctrl Pts',(-20.4545393933605,-23.5272079913704,
122.293853597091)) ;
#59817 = CARTESIAN_POINT('Ctrl Pts',(-20.245486515064,-23.3472189110075,122.517448272747)) ;
#59818 = CARTESIAN_POINT('Ctrl Pts',(-20.0102149504557,-23.5471605935689,
122.004204373971)) ;
#59819 = CARTESIAN_POINT('Ctrl Pts',(-19.8900270498159,-23.367171513206,122.28572785493)) ;
#59820 = CARTESIAN_POINT('Ctrl Pts',(-19.4949902616942,-23.5670700845392,
121.884042017214)) ;
#59821 = CARTESIAN_POINT('Ctrl Pts',(-19.477846400596,-23.3870810041763,122.189596888272)) ;
#59822 = CARTESIAN_POINT('Ctrl Pts',(-18.9708122647659,-23.5869214532386,
121.94527950064)) ;
#59823 = CARTESIAN_POINT('Ctrl Pts',(-19.0585021151188,-23.4069323728757,
122.23858718962)) ;
#59824 = CARTESIAN_POINT('Ctrl Pts',(-18.4941229340544,-23.6070016493746,
122.185035924344)) ;
#59825 = CARTESIAN_POINT('Ctrl Pts',(-18.6771515404996,-23.4270125690117,
122.43039179208)) ;
#59826 = CARTESIAN_POINT('Ctrl Pts',(-18.1327837985555,-23.62680259295,122.567847534588)) ;
#59827 = CARTESIAN_POINT('Ctrl Pts',(-18.3880785930256,-23.4468135125871,
122.736642978161)) ;
#59828 = CARTESIAN_POINT('Ctrl Pts',(-17.9208269264055,-23.6467865694595,
123.054772698368)) ;
#59829 = CARTESIAN_POINT('Ctrl Pts',(-18.2185138580659,-23.4667974890966,
123.126183626084)) ;
#59830 = CARTESIAN_POINT('Ctrl Pts',(-17.8886839110732,-23.6667025324351,
123.583127051767)) ;
#59831 = CARTESIAN_POINT('Ctrl Pts',(-18.1928000784033,-23.4867134520722,
123.548868146991)) ;
#59832 = CARTESIAN_POINT('Ctrl Pts',(-18.0370543006657,-23.686572967257,124.090087584522)) ;
#59833 = CARTESIAN_POINT('Ctrl Pts',(-18.3114982241245,-23.5065838868942,
123.954437479053)) ;
#59834 = CARTESIAN_POINT('Ctrl Pts',(-18.3529120736301,-23.7066232524901,
124.519105466772)) ;
#59835 = CARTESIAN_POINT('Ctrl Pts',(-18.5641852225777,-23.5266341721272,
124.297650597675)) ;
#59836 = CARTESIAN_POINT('Ctrl Pts',(-18.789984541274,-23.7263972212494,124.811340607854)) ;
#59837 = CARTESIAN_POINT('Ctrl Pts',(-18.9138460145566,-23.5464081408865,
124.531438476037)) ;
#59838 = CARTESIAN_POINT('Ctrl Pts',(-19.3073372095614,-23.746453679369,124.93893490729)) ;
#59839 = CARTESIAN_POINT('Ctrl Pts',(-19.3277281762554,-23.5664645990061,
124.633511759487)) ;
#59840 = CARTESIAN_POINT('Ctrl Pts',(-19.8306051755044,-23.76624856236,124.882843707526)) ;
#59841 = CARTESIAN_POINT('Ctrl Pts',(-19.7463441186502,-23.5862594819971,
124.588636471734)) ;
#59842 = CARTESIAN_POINT('Ctrl Pts',(-20.3078444224997,-23.7862152176623,
124.651011447722)) ;
#59843 = CARTESIAN_POINT('Ctrl Pts',(-20.1281345081567,-23.6062261372994,
124.40316804433)) ;
#59844 = CARTESIAN_POINT('Ctrl Pts',(-20.6767016461882,-23.8061741877388,
124.269621393362)) ;
#59845 = CARTESIAN_POINT('Ctrl Pts',(-20.4232185854534,-23.6261851073759,
124.09805398004)) ;
#59846 = CARTESIAN_POINT('Ctrl Pts',(-20.892884068729,-23.8260702753289,123.787054530312)) ;
#59847 = CARTESIAN_POINT('Ctrl Pts',(-20.5961622166163,-23.6460811949661,
123.711998606436)) ;
#59848 = CARTESIAN_POINT('Ctrl Pts',(-20.9320464014087,-23.8459684452405,
123.259690813219)) ;
#59849 = CARTESIAN_POINT('Ctrl Pts',(-20.6274889756677,-23.6659793648776,
123.290106706066)) ;
#59850 = CARTESIAN_POINT('Ctrl Pts',(-20.7893616368976,-23.8658742806076,
122.750190072207)) ;
#59851 = CARTESIAN_POINT('Ctrl Pts',(-20.5133377383693,-23.6858852002447,
122.882506513553)) ;
#59852 = CARTESIAN_POINT('Ctrl Pts',(-20.4807327588592,-23.8858242055455,
122.319088447684)) ;
#59853 = CARTESIAN_POINT('Ctrl Pts',(-20.2664316366618,-23.7058351251827,
122.537627039628)) ;
#59854 = CARTESIAN_POINT('Ctrl Pts',(-20.0452649316201,-23.9057033954559,
122.019778092239)) ;
#59855 = CARTESIAN_POINT('Ctrl Pts',(-19.9180547884745,-23.725714315093,122.298181446568)) ;
#59856 = CARTESIAN_POINT('Ctrl Pts',(-19.5313379424967,-23.9256847197365,
121.886108846057)) ;
#59857 = CARTESIAN_POINT('Ctrl Pts',(-19.5069121971362,-23.7456956393736,
122.191249793125)) ;
#59858 = CARTESIAN_POINT('Ctrl Pts',(-19.0038793190178,-23.9456145039448,
121.936000230857)) ;
#59859 = CARTESIAN_POINT('Ctrl Pts',(-19.084945405429,-23.765625423582,122.231166579714)) ;
#59860 = CARTESIAN_POINT('Ctrl Pts',(-18.5255093850671,-23.9655344933356,
122.162577000674)) ;
#59861 = CARTESIAN_POINT('Ctrl Pts',(-18.70225086222,-23.7855454129728,122.412432333271)) ;
#59862 = CARTESIAN_POINT('Ctrl Pts',(-18.1533588423712,-23.9853896886896,
122.536910497568)) ;
#59863 = CARTESIAN_POINT('Ctrl Pts',(-18.4045331019949,-23.8054006083268,
122.711900044301)) ;
#59864 = CARTESIAN_POINT('Ctrl Pts',(-17.9297252155865,-24.005435690349,123.020349675099)) ;
#59865 = CARTESIAN_POINT('Ctrl Pts',(-18.225629991919,-23.8254466099861,123.098661705087)) ;
#59866 = CARTESIAN_POINT('Ctrl Pts',(-17.8922881637436,-24.0219354375588,
123.457418896112)) ;
#59867 = CARTESIAN_POINT('Ctrl Pts',(-18.1956840852011,-23.8419463571959,
123.448290621712)) ;
#59868 = CARTESIAN_POINT('Ctrl Pts',(-17.9536182369137,-24.0353240420069,
123.803823185436)) ;
#59869 = CARTESIAN_POINT('Ctrl Pts',(-18.2447511118131,-23.855334961644,123.725437823404)) ;
#59870 = CARTESIAN_POINT('Ctrl Pts',(-18.0424306542549,-24.0451858703418,
124.047300970856)) ;
#59871 = CARTESIAN_POINT('Ctrl Pts',(-18.3158010379649,-23.8651967899789,
123.920212948107)) ;
#59872 = CARTESIAN_POINT('Ctrl Pts',(-18.1728224348044,-24.0551520130994,
124.274441107709)) ;
#59873 = CARTESIAN_POINT('Ctrl Pts',(-18.4201247042669,-23.8751629327365,
124.101932317986)) ;
#59874 = CARTESIAN_POINT('Ctrl Pts',(-18.398315477012,-24.0685137592243,124.543527593381)) ;
#59875 = CARTESIAN_POINT('Ctrl Pts',(-18.600479724246,-23.8885246788614,124.317163946771)) ;
#59876 = CARTESIAN_POINT('Ctrl Pts',(-18.7557534014151,-24.0849680881794,
124.795766078304)) ;
#59877 = CARTESIAN_POINT('Ctrl Pts',(-18.8864880582342,-23.9049790078165,
124.518993913012)) ;
#59878 = CARTESIAN_POINT('Ctrl Pts',(-19.1855079887731,-24.1017353332277,
124.913045707015)) ;
#59879 = CARTESIAN_POINT('Ctrl Pts',(-19.2302449597953,-23.9217462528648,
124.61279458323)) ;
#59880 = CARTESIAN_POINT('Ctrl Pts',(-19.5321625871901,-24.1149218985017,
124.914163508115)) ;
#59881 = CARTESIAN_POINT('Ctrl Pts',(-19.5076007478974,-23.9349328181389,
124.613694249745)) ;
#59882 = CARTESIAN_POINT('Ctrl Pts',(-19.7909027433267,-24.1249113572463,
124.870218955293)) ;
#59883 = CARTESIAN_POINT('Ctrl Pts',(-19.7145860227272,-23.9449222768835,
124.578534711631)) ;
#59884 = CARTESIAN_POINT('Ctrl Pts',(-20.0373293987813,-24.1348651297274,
124.782335916118)) ;
#59885 = CARTESIAN_POINT('Ctrl Pts',(-19.9117282978741,-23.9548760493646,
124.508226619746)) ;
#59886 = CARTESIAN_POINT('Ctrl Pts',(-20.2667248444726,-24.1449129462601,
124.651640371251)) ;
#59887 = CARTESIAN_POINT('Ctrl Pts',(-20.0952430132553,-23.9649238658972,
124.403668150689)) ;
#59888 = CARTESIAN_POINT('Ctrl Pts',(-20.4660081191832,-24.1547544793826,
124.486757064472)) ;
#59889 = CARTESIAN_POINT('Ctrl Pts',(-20.2546683482556,-23.9747653990197,
124.27175978153)) ;
#59890 = CARTESIAN_POINT('Ctrl Pts',(-20.6364815530708,-24.1647407216023,
124.287296273843)) ;
#59891 = CARTESIAN_POINT('Ctrl Pts',(-20.3910452989074,-23.9847516412394,
124.112189719401)) ;
#59892 = CARTESIAN_POINT('Ctrl Pts',(-20.7692271456916,-24.1746773450272,
124.062380424929)) ;
#59893 = CARTESIAN_POINT('Ctrl Pts',(-20.497239809877,-23.9946882646643,123.932255945756)) ;
#59894 = CARTESIAN_POINT('Ctrl Pts',(-20.8617993883025,-24.1847272224102,
123.815064619583)) ;
#59895 = CARTESIAN_POINT('Ctrl Pts',(-20.5712954677108,-24.0047381420473,
123.734402552555)) ;
#59896 = CARTESIAN_POINT('Ctrl Pts',(-20.9092661000716,-24.1945776611878,
123.560575071859)) ;
#59897 = CARTESIAN_POINT('Ctrl Pts',(-20.6092666006814,-24.0145885808249,
123.53081059359)) ;
#59898 = CARTESIAN_POINT('Ctrl Pts',(-20.9125392723098,-24.2045496751565,
123.298574461719)) ;
#59899 = CARTESIAN_POINT('Ctrl Pts',(-20.6118828876205,-24.0245605947936,
123.3212101705)) ;
#59900 = CARTESIAN_POINT('Ctrl Pts',(-20.8701252717379,-24.2145448437826,
123.039316830709)) ;
#59901 = CARTESIAN_POINT('Ctrl Pts',(-20.5779494825875,-24.0345557634197,
123.113804490714)) ;
#59902 = CARTESIAN_POINT('Ctrl Pts',(-20.7827267210347,-24.2245787270438,
122.790564493814)) ;
#59903 = CARTESIAN_POINT('Ctrl Pts',(-20.5080285227167,-24.0445896466809,
122.914803398227)) ;
#59904 = CARTESIAN_POINT('Ctrl Pts',(-20.6560814228119,-24.2344345971071,
122.564616215145)) ;
#59905 = CARTESIAN_POINT('Ctrl Pts',(-20.4067104191487,-24.0544455167443,
122.734046035466)) ;
#59906 = CARTESIAN_POINT('Ctrl Pts',(-20.4901252098502,-24.2444321430243,
122.3609792939)) ;
#59907 = CARTESIAN_POINT('Ctrl Pts',(-20.2739437686294,-24.0644430626614,
122.571137967992)) ;
#59908 = CARTESIAN_POINT('Ctrl Pts',(-20.293135035734,-24.2543402699236,122.190698398529)) ;
#59909 = CARTESIAN_POINT('Ctrl Pts',(-20.1163503191905,-24.0743511895607,
122.434915056073)) ;
#59910 = CARTESIAN_POINT('Ctrl Pts',(-20.0674961654377,-24.2643506414457,
122.055437128195)) ;
#59911 = CARTESIAN_POINT('Ctrl Pts',(-19.9358381408742,-24.0843615610829,
122.326707954225)) ;
#59912 = CARTESIAN_POINT('Ctrl Pts',(-19.8211172047256,-24.2743810841931,
121.961778537735)) ;
#59913 = CARTESIAN_POINT('Ctrl Pts',(-19.7387341883922,-24.0943920038303,
122.251783172163)) ;
#59914 = CARTESIAN_POINT('Ctrl Pts',(-19.5670147878812,-24.2842290367464,
121.912623318456)) ;
#59915 = CARTESIAN_POINT('Ctrl Pts',(-19.5354521536671,-24.1042399563836,
122.212461213181)) ;
#59916 = CARTESIAN_POINT('Ctrl Pts',(-19.3026436245788,-24.2942917057674,
121.908036631008)) ;
#59917 = CARTESIAN_POINT('Ctrl Pts',(-19.3239551506336,-24.1143026254045,
122.208794046212)) ;
#59918 = CARTESIAN_POINT('Ctrl Pts',(-19.0458393133714,-24.3041860812313,
121.948921771872)) ;
#59919 = CARTESIAN_POINT('Ctrl Pts',(-19.1185123080235,-24.1241970008685,
122.24150428493)) ;
#59920 = CARTESIAN_POINT('Ctrl Pts',(-18.7986820358757,-24.3141278795495,
122.033501629842)) ;
#59921 = CARTESIAN_POINT('Ctrl Pts',(-18.9207873807656,-24.1341387991866,
122.309170130401)) ;
#59922 = CARTESIAN_POINT('Ctrl Pts',(-18.5684608876012,-24.3241303732768,
122.160425707919)) ;
#59923 = CARTESIAN_POINT('Ctrl Pts',(-18.7366115490919,-24.1441412929139,
122.410711225786)) ;
#59924 = CARTESIAN_POINT('Ctrl Pts',(-18.3634159135229,-24.3341651717837,
122.326219304177)) ;
#59925 = CARTESIAN_POINT('Ctrl Pts',(-18.572576923515,-24.1541760914208,122.543347798557)) ;
#59926 = CARTESIAN_POINT('Ctrl Pts',(-18.1931997744196,-24.3440100557631,
122.521073096174)) ;
#59927 = CARTESIAN_POINT('Ctrl Pts',(-18.4364059140593,-24.1640209754002,
122.699231890635)) ;
#59928 = CARTESIAN_POINT('Ctrl Pts',(-18.0570939034257,-24.3539959125811,
122.745386068162)) ;
#59929 = CARTESIAN_POINT('Ctrl Pts',(-18.3275230654761,-24.1740068322182,
122.878683238655)) ;
#59930 = CARTESIAN_POINT('Ctrl Pts',(-17.9622837121039,-24.3639307267559,
122.988691099202)) ;
#59931 = CARTESIAN_POINT('Ctrl Pts',(-18.2516769244132,-24.183941646393,123.07332776623)) ;
#59932 = CARTESIAN_POINT('Ctrl Pts',(-17.9107758866694,-24.3739882265412,
123.247885388004)) ;
#59933 = CARTESIAN_POINT('Ctrl Pts',(-18.2104726941361,-24.1939991461783,
123.28068369653)) ;
#59934 = CARTESIAN_POINT('Ctrl Pts',(-17.904793545213,-24.3838099849595,123.505950068629)) ;
#59935 = CARTESIAN_POINT('Ctrl Pts',(-18.2056888745737,-24.2038209045966,
123.487134859051)) ;
#59936 = CARTESIAN_POINT('Ctrl Pts',(-17.9441385895894,-24.3938656427435,
123.767234420915)) ;
#59937 = CARTESIAN_POINT('Ctrl Pts',(-18.2371668835213,-24.2138765623806,
123.696162133941)) ;
#59938 = CARTESIAN_POINT('Ctrl Pts',(-18.0277646258523,-24.4038078249235,
124.014774122479)) ;
#59939 = CARTESIAN_POINT('Ctrl Pts',(-18.3040695599417,-24.2238187445607,
123.894192987516)) ;
#59940 = CARTESIAN_POINT('Ctrl Pts',(-18.1519307759585,-24.4137130336182,
124.243545142332)) ;
#59941 = CARTESIAN_POINT('Ctrl Pts',(-18.4034039803286,-24.2337239532553,
124.077208506641)) ;
#59942 = CARTESIAN_POINT('Ctrl Pts',(-18.3162322484998,-24.4237548245807,
124.450038000876)) ;
#59943 = CARTESIAN_POINT('Ctrl Pts',(-18.5348467279855,-24.2437657442178,
124.242401635478)) ;
#59944 = CARTESIAN_POINT('Ctrl Pts',(-18.5112465951366,-24.4336625990529,
124.622564118162)) ;
#59945 = CARTESIAN_POINT('Ctrl Pts',(-18.6908591806819,-24.25367351869,124.380420796196)) ;
#59946 = CARTESIAN_POINT('Ctrl Pts',(-18.7353216882572,-24.4436740992805,
124.760445262885)) ;
#59947 = CARTESIAN_POINT('Ctrl Pts',(-18.8701201999352,-24.2636850189176,
124.490724088854)) ;
#59948 = CARTESIAN_POINT('Ctrl Pts',(-18.9806475911732,-24.4537068596732,
124.857016709312)) ;
#59949 = CARTESIAN_POINT('Ctrl Pts',(-19.0663816751917,-24.2737177793103,
124.567979438308)) ;
#59950 = CARTESIAN_POINT('Ctrl Pts',(-19.2342398512447,-24.4635574288081,
124.909018469813)) ;
#59951 = CARTESIAN_POINT('Ctrl Pts',(-19.2692552091276,-24.2835683484452,
124.609578862469)) ;
#59952 = CARTESIAN_POINT('Ctrl Pts',(-19.496593073052,-24.473546038338,124.916794312844)) ;
#59953 = CARTESIAN_POINT('Ctrl Pts',(-19.4791376938432,-24.2935569579751,
124.615797717518)) ;
#59954 = CARTESIAN_POINT('Ctrl Pts',(-19.7547810174037,-24.4834746943621,
124.879120015881)) ;
#59955 = CARTESIAN_POINT('Ctrl Pts',(-19.685687402309,-24.3034856139992,124.585656541612)) ;
#59956 = CARTESIAN_POINT('Ctrl Pts',(-20.0041249025158,-24.4934624405399,
124.797121058112)) ;
#59957 = CARTESIAN_POINT('Ctrl Pts',(-19.8851618270809,-24.313473360177,124.520055766498)) ;
#59958 = CARTESIAN_POINT('Ctrl Pts',(-20.2363287243684,-24.5034984294756,
124.672094532501)) ;
#59959 = CARTESIAN_POINT('Ctrl Pts',(-20.0709240851037,-24.3235093491128,
124.42003291363)) ;
#59960 = CARTESIAN_POINT('Ctrl Pts',(-20.4398532893897,-24.5133532992892,
124.511915768883)) ;
#59961 = CARTESIAN_POINT('Ctrl Pts',(-20.23374208075,-24.3333642189264,124.291888988596)) ;
#59962 = CARTESIAN_POINT('Ctrl Pts',(-20.6152286146219,-24.523352740531,124.316286380148)) ;
#59963 = CARTESIAN_POINT('Ctrl Pts',(-20.3740410150847,-24.3433636601681,
124.135384433191)) ;
#59964 = CARTESIAN_POINT('Ctrl Pts',(-20.7528077611867,-24.5332478147111,
124.095579716367)) ;
#59965 = CARTESIAN_POINT('Ctrl Pts',(-20.4841026378956,-24.3532587343482,
123.958818739032)) ;
#59966 = CARTESIAN_POINT('Ctrl Pts',(-20.8515452176625,-24.5433084705508,
123.850362627596)) ;
#59967 = CARTESIAN_POINT('Ctrl Pts',(-20.5630911554068,-24.3633193901879,
123.762644277068)) ;
#59968 = CARTESIAN_POINT('Ctrl Pts',(-20.90521146566,-24.5531573447464,123.597149046186)) ;
#59969 = CARTESIAN_POINT('Ctrl Pts',(-20.6060224056543,-24.3731682643835,
123.560073894341)) ;
#59970 = CARTESIAN_POINT('Ctrl Pts',(-20.9149218984342,-24.5631860567097,
123.333787858284)) ;
#59971 = CARTESIAN_POINT('Ctrl Pts',(-20.6137892700435,-24.3831969763468,
123.349384859398)) ;
#59972 = CARTESIAN_POINT('Ctrl Pts',(-20.8780431867244,-24.5732154572928,
123.072813707619)) ;
#59973 = CARTESIAN_POINT('Ctrl Pts',(-20.5842846871539,-24.3932263769299,
123.140605706527)) ;
#59974 = CARTESIAN_POINT('Ctrl Pts',(-20.7984988600526,-24.5830556509096,
122.826757371458)) ;
#59975 = CARTESIAN_POINT('Ctrl Pts',(-20.5206480690799,-24.4030665705467,
122.943761971265)) ;
#59976 = CARTESIAN_POINT('Ctrl Pts',(-20.675875973219,-24.5930590734848,122.594259198633)) ;
#59977 = CARTESIAN_POINT('Ctrl Pts',(-20.4225485501973,-24.4130699931219,
122.757764169377)) ;
#59978 = CARTESIAN_POINT('Ctrl Pts',(-20.5149236678703,-24.6030446105779,
122.386952011327)) ;
#59979 = CARTESIAN_POINT('Ctrl Pts',(-20.2937856775477,-24.423055530215,122.591919429252)) ;
#59980 = CARTESIAN_POINT('Ctrl Pts',(-20.319214882974,-24.6130856150647,122.210004150072)) ;
#59981 = CARTESIAN_POINT('Ctrl Pts',(-20.1372175724213,-24.4330965347018,
122.450362171703)) ;
#59982 = CARTESIAN_POINT('Ctrl Pts',(-20.100298824301,-24.6229291540059,122.072161974285)) ;
#59983 = CARTESIAN_POINT('Ctrl Pts',(-19.9620847673465,-24.442940073643,122.340090125974)) ;
#59984 = CARTESIAN_POINT('Ctrl Pts',(-19.8575938757749,-24.6329141849967,
121.972533729906)) ;
#59985 = CARTESIAN_POINT('Ctrl Pts',(-19.7679204996431,-24.4529251046338,
122.260388809874)) ;
#59986 = CARTESIAN_POINT('Ctrl Pts',(-19.6023947114749,-24.6428536475187,
121.916697509575)) ;
#59987 = CARTESIAN_POINT('Ctrl Pts',(-19.5637613212233,-24.4628645671558,
122.215721172914)) ;
#59988 = CARTESIAN_POINT('Ctrl Pts',(-19.3388001962216,-24.6528933797425,
121.905974359338)) ;
#59989 = CARTESIAN_POINT('Ctrl Pts',(-19.3528855389491,-24.4729042993796,
122.207143937649)) ;
#59990 = CARTESIAN_POINT('Ctrl Pts',(-19.0812413725031,-24.6627815600597,
121.940528367606)) ;
#59991 = CARTESIAN_POINT('Ctrl Pts',(-19.1468393800042,-24.4827924796968,
122.23478829755)) ;
#59992 = CARTESIAN_POINT('Ctrl Pts',(-18.830930339593,-24.6727710757622,122.019607849904)) ;
#59993 = CARTESIAN_POINT('Ctrl Pts',(-18.9465910651468,-24.4927819953993,
122.298052933552)) ;
#59994 = CARTESIAN_POINT('Ctrl Pts',(-18.5989667873706,-24.6827296264169,
122.140752466296)) ;
#59995 = CARTESIAN_POINT('Ctrl Pts',(-18.7610210868457,-24.502740546054,122.394969531165)) ;
#59996 = CARTESIAN_POINT('Ctrl Pts',(-18.3923783177254,-24.6926290335219,
122.298887165231)) ;
#59997 = CARTESIAN_POINT('Ctrl Pts',(-18.5957515114888,-24.5126399531591,
122.521477699572)) ;
#59998 = CARTESIAN_POINT('Ctrl Pts',(-18.2138481637525,-24.7026776199382,
122.493414575767)) ;
#59999 = CARTESIAN_POINT('Ctrl Pts',(-18.4529280643294,-24.5226885395753,
122.677100488762)) ;
#60000 = CARTESIAN_POINT('Ctrl Pts',(-18.0737497675781,-24.7125704389027,
122.712471449112)) ;
#60001 = CARTESIAN_POINT('Ctrl Pts',(-18.3408506079003,-24.5325813585398,
122.852345913931)) ;
#60002 = CARTESIAN_POINT('Ctrl Pts',(-17.9721440404555,-24.7226415564325,
122.95679058556)) ;
#60003 = CARTESIAN_POINT('Ctrl Pts',(-18.2595668744231,-24.5426524760696,
123.047801904658)) ;
#60004 = CARTESIAN_POINT('Ctrl Pts',(-17.9156039987701,-24.7324572503985,
123.208514840523)) ;
#60005 = CARTESIAN_POINT('Ctrl Pts',(-18.214336048054,-24.5524681700357,123.249180320883)) ;
#60006 = CARTESIAN_POINT('Ctrl Pts',(-17.9029486725744,-24.7425236278958,
123.472689210429)) ;
#60007 = CARTESIAN_POINT('Ctrl Pts',(-18.2042126493569,-24.562534547533,123.460520152789)) ;
#60008 = CARTESIAN_POINT('Ctrl Pts',(-17.935892095498,-24.7524226139777,123.730795685717)) ;
#60009 = CARTESIAN_POINT('Ctrl Pts',(-18.2305681821553,-24.5724335336148,
123.667004510187)) ;
#60010 = CARTESIAN_POINT('Ctrl Pts',(-18.0142279454651,-24.7624767939712,
123.983068491379)) ;
#60011 = CARTESIAN_POINT('Ctrl Pts',(-18.2932377609771,-24.5824877136083,
123.868822703197)) ;
#60012 = CARTESIAN_POINT('Ctrl Pts',(-18.1327982653444,-24.7723476069039,
124.213846997016)) ;
#60013 = CARTESIAN_POINT('Ctrl Pts',(-18.3880943171351,-24.592358526541,124.053444317472)) ;
#60014 = CARTESIAN_POINT('Ctrl Pts',(-18.2927953165878,-24.7824215077577,
124.424680232047)) ;
#60015 = CARTESIAN_POINT('Ctrl Pts',(-18.5160928152564,-24.6024324273948,
124.222110690457)) ;
#60016 = CARTESIAN_POINT('Ctrl Pts',(-18.4819523062821,-24.7922416631444,
124.600316090913)) ;
#60017 = CARTESIAN_POINT('Ctrl Pts',(-18.6674179941489,-24.6122525827815,
124.36261799151)) ;
#60018 = CARTESIAN_POINT('Ctrl Pts',(-18.7041959809352,-24.8023203700966,
124.744270009316)) ;
#60019 = CARTESIAN_POINT('Ctrl Pts',(-18.8452136184264,-24.6223312897337,
124.477780764093)) ;
#60020 = CARTESIAN_POINT('Ctrl Pts',(-18.9426453970189,-24.8121719586354,
124.845254460228)) ;
#60021 = CARTESIAN_POINT('Ctrl Pts',(-19.0359724337194,-24.6321828782725,
124.558567311492)) ;
#60022 = CARTESIAN_POINT('Ctrl Pts',(-19.200521069137,-24.8222450751604,124.904809172551)) ;
#60023 = CARTESIAN_POINT('Ctrl Pts',(-19.2422734477073,-24.6422559947975,
124.606210577257)) ;
#60024 = CARTESIAN_POINT('Ctrl Pts',(-19.4588424041164,-24.8320875922562,
124.91832832477)) ;
#60025 = CARTESIAN_POINT('Ctrl Pts',(-19.4489294152064,-24.6520985118933,
124.617025231616)) ;
#60026 = CARTESIAN_POINT('Ctrl Pts',(-19.7192553917927,-24.8420680538102,
124.887225976131)) ;
#60027 = CARTESIAN_POINT('Ctrl Pts',(-19.6572595128658,-24.6620789734473,
124.592142995155)) ;
#60028 = CARTESIAN_POINT('Ctrl Pts',(-19.9711242826029,-24.8520863038009,
124.810604842072)) ;
#60029 = CARTESIAN_POINT('Ctrl Pts',(-19.8587544824804,-24.6720972234381,
124.530845590783)) ;
#60030 = CARTESIAN_POINT('Ctrl Pts',(-20.2029896410635,-24.8619704639947,
124.693474375189)) ;
#60031 = CARTESIAN_POINT('Ctrl Pts',(-20.0442458164623,-24.6819813836318,
124.437141271385)) ;
#60032 = CARTESIAN_POINT('Ctrl Pts',(-20.4147243951242,-24.8720356109697,
124.535001991824)) ;
#60033 = CARTESIAN_POINT('Ctrl Pts',(-20.2136336325646,-24.6920465306068,
124.310362857701)) ;
#60034 = CARTESIAN_POINT('Ctrl Pts',(-20.5918496186671,-24.8818774346105,
124.346514930548)) ;
#60035 = CARTESIAN_POINT('Ctrl Pts',(-20.3553327465534,-24.7018883542476,
124.159573817455)) ;
#60036 = CARTESIAN_POINT('Ctrl Pts',(-20.7368372685072,-24.8919069070713,
124.126420308641)) ;
#60037 = CARTESIAN_POINT('Ctrl Pts',(-20.4713227600886,-24.7119178267085,
123.983497953276)) ;
#60038 = CARTESIAN_POINT('Ctrl Pts',(-20.8407071584653,-24.9019337623334,
123.884255455993)) ;
#60039 = CARTESIAN_POINT('Ctrl Pts',(-20.5544183607699,-24.7219446819705,
123.789765854984)) ;
#60040 = CARTESIAN_POINT('Ctrl Pts',(-20.9004509562917,-24.9117770124439,
123.632574419147)) ;
#60041 = CARTESIAN_POINT('Ctrl Pts',(-20.6022129291242,-24.731787932081,123.588422099066)) ;
#60042 = CARTESIAN_POINT('Ctrl Pts',(-20.916260611242,-24.9218254520271,123.368993380643)) ;
#60043 = CARTESIAN_POINT('Ctrl Pts',(-20.614860543706,-24.7418363716642,123.377557052921)) ;
#60044 = CARTESIAN_POINT('Ctrl Pts',(-20.8859488523691,-24.931774946275,123.109292637768)) ;
#60045 = CARTESIAN_POINT('Ctrl Pts',(-20.59061096289,-24.7517858659121,123.169796946132)) ;
#60046 = CARTESIAN_POINT('Ctrl Pts',(-20.812063374515,-24.941682802001,122.85961242254)) ;
#60047 = CARTESIAN_POINT('Ctrl Pts',(-20.531502761985,-24.7616937216381,122.970053477872)) ;
#60048 = CARTESIAN_POINT('Ctrl Pts',(-20.6939388264685,-24.9517422786509,
122.623150935641)) ;
#60049 = CARTESIAN_POINT('Ctrl Pts',(-20.4370029110324,-24.771753198288,122.7808840852)) ;
#60050 = CARTESIAN_POINT('Ctrl Pts',(-20.5402177796958,-24.9615830880596,
122.415150839327)) ;
#60051 = CARTESIAN_POINT('Ctrl Pts',(-20.3140267650596,-24.7815940076967,
122.614484958291)) ;
#60052 = CARTESIAN_POINT('Ctrl Pts',(-20.3487716521003,-24.9716452383604,
122.232796879525)) ;
#60053 = CARTESIAN_POINT('Ctrl Pts',(-20.1608697005257,-24.7916561579975,
122.46860153275)) ;
#60054 = CARTESIAN_POINT('Ctrl Pts',(-20.1319979378848,-24.981542399483,122.089055106717)) ;
#60055 = CARTESIAN_POINT('Ctrl Pts',(-19.9874513995793,-24.8015533191201,
122.353608554069)) ;
#60056 = CARTESIAN_POINT('Ctrl Pts',(-19.8931048762682,-24.991473573887,121.983991783669)) ;
#60057 = CARTESIAN_POINT('Ctrl Pts',(-19.7963375692776,-24.8114844935241,
122.269557920393)) ;
#60058 = CARTESIAN_POINT('Ctrl Pts',(-19.6366938542377,-25.001515777612,121.921591372385)) ;
#60059 = CARTESIAN_POINT('Ctrl Pts',(-19.5912086257086,-24.8215266972492,
122.219637404033)) ;
#60060 = CARTESIAN_POINT('Ctrl Pts',(-19.3774193320319,-25.0114023600425,
121.904731667752)) ;
#60061 = CARTESIAN_POINT('Ctrl Pts',(-19.3837898885551,-24.8314132796796,
122.206149496955)) ;
#60062 = CARTESIAN_POINT('Ctrl Pts',(-19.116345118076,-25.0213957957908,121.933019786069)) ;
#60063 = CARTESIAN_POINT('Ctrl Pts',(-19.1749306450464,-24.8414067154279,
122.228779665525)) ;
#60064 = CARTESIAN_POINT('Ctrl Pts',(-18.8653899853733,-25.031340264149,122.0059331557)) ;
#60065 = CARTESIAN_POINT('Ctrl Pts',(-18.9741669200582,-24.8513511837861,
122.287109951159)) ;
#60066 = CARTESIAN_POINT('Ctrl Pts',(-18.6305081904514,-25.0412920803945,
122.120959221121)) ;
#60067 = CARTESIAN_POINT('Ctrl Pts',(-18.7862616983895,-24.8613030000317,
122.379130236719)) ;
#60068 = CARTESIAN_POINT('Ctrl Pts',(-18.4175106984375,-25.051329516509,122.276526693865)) ;
#60069 = CARTESIAN_POINT('Ctrl Pts',(-18.6158633904333,-24.8713404361461,
122.503584006888)) ;
#60070 = CARTESIAN_POINT('Ctrl Pts',(-18.2373294887089,-25.0612144756854,
122.463677159572)) ;
#60071 = CARTESIAN_POINT('Ctrl Pts',(-18.4717187211798,-24.8812253953225,
122.653303473347)) ;
#60072 = CARTESIAN_POINT('Ctrl Pts',(-18.0904935273236,-25.0712125938973,
122.681519130343)) ;
#60073 = CARTESIAN_POINT('Ctrl Pts',(-18.3542496121446,-24.8912235135344,
122.82757667031)) ;
#60074 = CARTESIAN_POINT('Ctrl Pts',(-17.9843474113932,-25.0811335264093,
122.919675638714)) ;
#60075 = CARTESIAN_POINT('Ctrl Pts',(-18.2693324840715,-24.9011444460464,
123.018101090549)) ;
#60076 = CARTESIAN_POINT('Ctrl Pts',(-17.9203421285094,-25.0911748266313,
123.175657289294)) ;
#60077 = CARTESIAN_POINT('Ctrl Pts',(-18.2181276878849,-24.9111857462685,
123.222886415152)) ;
#60078 = CARTESIAN_POINT('Ctrl Pts',(-17.9020926498255,-25.1010817450213,
123.435363279085)) ;
#60079 = CARTESIAN_POINT('Ctrl Pts',(-18.2035276252548,-24.9210926646584,
123.430650454951)) ;
#60080 = CARTESIAN_POINT('Ctrl Pts',(-17.9285484881312,-25.1110175367304,
123.69512331008)) ;
#60081 = CARTESIAN_POINT('Ctrl Pts',(-18.2246915312731,-24.9310284563675,
123.638458030304)) ;
#60082 = CARTESIAN_POINT('Ctrl Pts',(-18.0007127842541,-25.1210584313083,
123.948921149935)) ;
#60083 = CARTESIAN_POINT('Ctrl Pts',(-18.2824223843685,-24.9410693509454,
123.841496622937)) ;
#60084 = CARTESIAN_POINT('Ctrl Pts',(-18.1139247515408,-25.1309456330221,
124.18280063066)) ;
#60085 = CARTESIAN_POINT('Ctrl Pts',(-18.3729909704001,-24.9509565526592,
124.028599762318)) ;
#60086 = CARTESIAN_POINT('Ctrl Pts',(-18.2672700656794,-25.1409379007837,
124.395937506852)) ;
#60087 = CARTESIAN_POINT('Ctrl Pts',(-18.4956664766225,-24.9609488204208,
124.199109598826)) ;
#60088 = CARTESIAN_POINT('Ctrl Pts',(-18.4545445264848,-25.1508864218055,
124.578379945049)) ;
#60089 = CARTESIAN_POINT('Ctrl Pts',(-18.6454851891911,-24.9708973414426,
124.345063807)) ;
#60090 = CARTESIAN_POINT('Ctrl Pts',(-18.6701593794825,-25.1608231953832,
124.72564450551)) ;
#60091 = CARTESIAN_POINT('Ctrl Pts',(-18.8179761594363,-24.9808341150203,
124.462875886773)) ;
#60092 = CARTESIAN_POINT('Ctrl Pts',(-18.9090898746252,-25.1708062435242,
124.834059046402)) ;
#60093 = CARTESIAN_POINT('Ctrl Pts',(-19.0091199773882,-24.9908171631614,
124.549608297516)) ;
#60094 = CARTESIAN_POINT('Ctrl Pts',(-19.1648198261409,-25.1808499511343,
124.899256681723)) ;
#60095 = CARTESIAN_POINT('Ctrl Pts',(-19.2137038781447,-25.0008608707714,
124.601767252083)) ;
#60096 = CARTESIAN_POINT('Ctrl Pts',(-19.4223677819913,-25.1906786442876,
124.919232914373)) ;
#60097 = CARTESIAN_POINT('Ctrl Pts',(-19.4197410212802,-25.0106895639247,
124.617749120168)) ;
#60098 = CARTESIAN_POINT('Ctrl Pts',(-19.6858526790546,-25.200753393417,124.893750955826)) ;
#60099 = CARTESIAN_POINT('Ctrl Pts',(-19.6305293633067,-25.0207643130542,
124.59736453674)) ;
#60100 = CARTESIAN_POINT('Ctrl Pts',(-19.9356579462158,-25.2106187192126,
124.824304856564)) ;
#60101 = CARTESIAN_POINT('Ctrl Pts',(-19.8303729649698,-25.0306296388497,
124.541808869368)) ;
#60102 = CARTESIAN_POINT('Ctrl Pts',(-20.173585469303,-25.2206408935695,124.711387601586)) ;
#60103 = CARTESIAN_POINT('Ctrl Pts',(-20.0207155100975,-25.0406518132067,
124.451476093775)) ;
#60104 = CARTESIAN_POINT('Ctrl Pts',(-20.3880226560733,-25.2306669467765,
124.558270853384)) ;
#60105 = CARTESIAN_POINT('Ctrl Pts',(-20.1922658914238,-25.0506778664136,
124.328983483751)) ;
#60106 = CARTESIAN_POINT('Ctrl Pts',(-20.5697163878782,-25.2405206436227,
124.373799671678)) ;
#60107 = CARTESIAN_POINT('Ctrl Pts',(-20.3376209782561,-25.0605315632599,
124.181408007588)) ;
#60108 = CARTESIAN_POINT('Ctrl Pts',(-20.7188606913848,-25.2504800483757,
124.15871963452)) ;
#60109 = CARTESIAN_POINT('Ctrl Pts',(-20.4569372775264,-25.0704909680128,
124.009344986073)) ;
#60110 = CARTESIAN_POINT('Ctrl Pts',(-20.8288249195141,-25.2605182940806,
123.91895416316)) ;
#60111 = CARTESIAN_POINT('Ctrl Pts',(-20.5449097751489,-25.0805292137177,
123.817532999354)) ;
#60112 = CARTESIAN_POINT('Ctrl Pts',(-20.8948612313139,-25.2703924782426,
123.667978712676)) ;
#60113 = CARTESIAN_POINT('Ctrl Pts',(-20.5977398529196,-25.0904033978798,
123.616753747338)) ;
#60114 = CARTESIAN_POINT('Ctrl Pts',(-20.9167246661195,-25.2804622613806,
123.404296836379)) ;
#60115 = CARTESIAN_POINT('Ctrl Pts',(-20.6152318948764,-25.1004731810177,
123.405808073507)) ;
#60116 = CARTESIAN_POINT('Ctrl Pts',(-20.8931748950452,-25.2902955164013,
123.146942101532)) ;
#60117 = CARTESIAN_POINT('Ctrl Pts',(-20.5963934691841,-25.1103064360384,
123.199925185877)) ;
#60118 = CARTESIAN_POINT('Ctrl Pts',(-20.824664603496,-25.300325942533,122.892421113422)) ;
#60119 = CARTESIAN_POINT('Ctrl Pts',(-20.5415866267975,-25.1203368621701,
122.996307948949)) ;
#60120 = CARTESIAN_POINT('Ctrl Pts',(-20.7122848539056,-25.31035755472,122.653938383803)) ;
#60121 = CARTESIAN_POINT('Ctrl Pts',(-20.4516839742709,-25.1303684743571,
122.805521151809)) ;
#60122 = CARTESIAN_POINT('Ctrl Pts',(-20.5637225648046,-25.3201872515746,
122.442640422475)) ;
#60123 = CARTESIAN_POINT('Ctrl Pts',(-20.3328358819854,-25.1401981712117,
122.636482800151)) ;
#60124 = CARTESIAN_POINT('Ctrl Pts',(-20.3782914259255,-25.3301766934771,
122.2568129731)) ;
#60125 = CARTESIAN_POINT('Ctrl Pts',(-20.1844921808869,-25.1501876131142,
122.487819833207)) ;
#60126 = CARTESIAN_POINT('Ctrl Pts',(-20.1618642262399,-25.3402205854928,
122.105737145019)) ;
#60127 = CARTESIAN_POINT('Ctrl Pts',(-20.0113511467643,-25.1602315051299,
122.366957925949)) ;
#60128 = CARTESIAN_POINT('Ctrl Pts',(-19.9280150892264,-25.350042147262,121.996514020556)) ;
#60129 = CARTESIAN_POINT('Ctrl Pts',(-19.8242733908789,-25.1700530668991,
122.279578452109)) ;
#60130 = CARTESIAN_POINT('Ctrl Pts',(-19.6734892886853,-25.3600777188862,
121.927457195706)) ;
#60131 = CARTESIAN_POINT('Ctrl Pts',(-19.6206531100156,-25.1800886385233,
122.224331363423)) ;
#60132 = CARTESIAN_POINT('Ctrl Pts',(-19.4109364974854,-25.370106993168,121.904446478748)) ;
#60133 = CARTESIAN_POINT('Ctrl Pts',(-19.410610970347,-25.1901179128051,122.205921274802)) ;
#60134 = CARTESIAN_POINT('Ctrl Pts',(-19.153425698316,-25.3799408302867,121.92623667871)) ;
#60135 = CARTESIAN_POINT('Ctrl Pts',(-19.2046030736676,-25.1999517499238,
122.223351721254)) ;
#60136 = CARTESIAN_POINT('Ctrl Pts',(-18.8979973838901,-25.3899932263748,
121.99356443242)) ;
#60137 = CARTESIAN_POINT('Ctrl Pts',(-19.0002598327071,-25.2100041460119,
122.277212317537)) ;
#60138 = CARTESIAN_POINT('Ctrl Pts',(-18.6610161340933,-25.3999299933253,
122.103265136597)) ;
#60139 = CARTESIAN_POINT('Ctrl Pts',(-18.8106744978957,-25.2199409129625,
122.364971228474)) ;
#60140 = CARTESIAN_POINT('Ctrl Pts',(-18.4463642084405,-25.4098642283046,
122.251846102408)) ;
#60141 = CARTESIAN_POINT('Ctrl Pts',(-18.6389522789307,-25.2298751479417,
122.483834331329)) ;
#60142 = CARTESIAN_POINT('Ctrl Pts',(-18.2592125481551,-25.4198879916314,
122.437210228712)) ;
#60143 = CARTESIAN_POINT('Ctrl Pts',(-18.4892297234926,-25.2398989112685,
122.632124410148)) ;
#60144 = CARTESIAN_POINT('Ctrl Pts',(-18.1090179641426,-25.429774333016,122.649196677396)) ;
#60145 = CARTESIAN_POINT('Ctrl Pts',(-18.3690729553001,-25.2497852526532,
122.801712072819)) ;
#60146 = CARTESIAN_POINT('Ctrl Pts',(-17.9962023976865,-25.439763381783,122.886228834323)) ;
#60147 = CARTESIAN_POINT('Ctrl Pts',(-18.2788188754758,-25.2597743014202,
122.991336884264)) ;
#60148 = CARTESIAN_POINT('Ctrl Pts',(-17.92642324804,-25.4498046024804,123.140706746069)) ;
#60149 = CARTESIAN_POINT('Ctrl Pts',(-18.2229938254166,-25.2698155221175,
123.194918814878)) ;
#60150 = CARTESIAN_POINT('Ctrl Pts',(-17.9019779830715,-25.4596372426583,
123.397935296118)) ;
#60151 = CARTESIAN_POINT('Ctrl Pts',(-18.2034358520446,-25.2796481622954,
123.400700720434)) ;
#60152 = CARTESIAN_POINT('Ctrl Pts',(-17.9221548130397,-25.4696311719663,
123.659787613403)) ;
#60153 = CARTESIAN_POINT('Ctrl Pts',(-18.2195753605606,-25.2896420916034,
123.610182627543)) ;
#60154 = CARTESIAN_POINT('Ctrl Pts',(-17.9882634627547,-25.4796603796468,
123.914920831953)) ;
#60155 = CARTESIAN_POINT('Ctrl Pts',(-18.2724604733462,-25.2996712992839,
123.814289688043)) ;
#60156 = CARTESIAN_POINT('Ctrl Pts',(-18.095614902813,-25.4895361913509,124.151219574805)) ;
#60157 = CARTESIAN_POINT('Ctrl Pts',(-18.3583396441264,-25.309547110988,124.003328991269)) ;
#60158 = CARTESIAN_POINT('Ctrl Pts',(-18.243932354423,-25.4995354183223,124.368086107195)) ;
#60159 = CARTESIAN_POINT('Ctrl Pts',(-18.4769919264261,-25.3195463379594,
124.176823257669)) ;
#60160 = CARTESIAN_POINT('Ctrl Pts',(-18.4258762775159,-25.509444899478,124.554446462771)) ;
#60161 = CARTESIAN_POINT('Ctrl Pts',(-18.6225453691918,-25.3294558191151,
124.325912669467)) ;
#60162 = CARTESIAN_POINT('Ctrl Pts',(-18.6404489287507,-25.5194981297789,
124.708521879958)) ;
#60163 = CARTESIAN_POINT('Ctrl Pts',(-18.7942023889779,-25.339509049416,124.449174675351)) ;
#60164 = CARTESIAN_POINT('Ctrl Pts',(-18.8741769469546,-25.52936874633,124.821053391255)) ;
#60165 = CARTESIAN_POINT('Ctrl Pts',(-18.981183490012,-25.3493796659671,124.539201487123)) ;
#60166 = CARTESIAN_POINT('Ctrl Pts',(-19.127535526737,-25.539390408062,124.892923586668)) ;
#60167 = CARTESIAN_POINT('Ctrl Pts',(-19.1838697832088,-25.3594013276991,
124.596699645032)) ;
#60168 = CARTESIAN_POINT('Ctrl Pts',(-19.3896325300281,-25.5494132212431,
124.919115026202)) ;
#60169 = CARTESIAN_POINT('Ctrl Pts',(-19.3935471728134,-25.3694241408802,
124.617654797419)) ;
#60170 = CARTESIAN_POINT('Ctrl Pts',(-19.6482244565105,-25.5592803857031,
124.900141299359)) ;
#60171 = CARTESIAN_POINT('Ctrl Pts',(-19.6004204014471,-25.3792913053402,
124.602477906034)) ;
#60172 = CARTESIAN_POINT('Ctrl Pts',(-19.902976585568,-25.569273827923,124.83632140457)) ;
#60173 = CARTESIAN_POINT('Ctrl Pts',(-19.8042225357259,-25.3892847475601,
124.551424072953)) ;
#60174 = CARTESIAN_POINT('Ctrl Pts',(-20.1434775002714,-25.5793055015233,
124.728362358273)) ;
#60175 = CARTESIAN_POINT('Ctrl Pts',(-19.9966241166619,-25.3993164211604,
124.465058726285)) ;
#60176 = CARTESIAN_POINT('Ctrl Pts',(-20.3582214202011,-25.5891719366363,
124.583046155646)) ;
#60177 = CARTESIAN_POINT('Ctrl Pts',(-20.1684200947875,-25.4091828562734,
124.348807744366)) ;
#60178 = CARTESIAN_POINT('Ctrl Pts',(-20.5470220993217,-25.5991593871694,
124.400775187836)) ;
#60179 = CARTESIAN_POINT('Ctrl Pts',(-20.3194620631275,-25.4191703068065,
124.202992587349)) ;
#60180 = CARTESIAN_POINT('Ctrl Pts',(-20.7008042109663,-25.6091043169973,
124.189419968421)) ;
#60181 = CARTESIAN_POINT('Ctrl Pts',(-20.4424893892085,-25.4291152366345,
124.033909833955)) ;
#60182 = CARTESIAN_POINT('Ctrl Pts',(-20.8165443609091,-25.6191492120525,
123.952204828847)) ;
#60183 = CARTESIAN_POINT('Ctrl Pts',(-20.535083449004,-25.4391601316896,123.844138651969)) ;
#60184 = CARTESIAN_POINT('Ctrl Pts',(-20.8882445301737,-25.6290112737383,
123.70313575114)) ;
#60185 = CARTESIAN_POINT('Ctrl Pts',(-20.5924455729224,-25.4490221933754,
123.644884316791)) ;
#60186 = CARTESIAN_POINT('Ctrl Pts',(-20.9164870894924,-25.6390029965252,
123.442107956851)) ;
#60187 = CARTESIAN_POINT('Ctrl Pts',(-20.6150418055074,-25.4590139161623,
123.436062394398)) ;
#60188 = CARTESIAN_POINT('Ctrl Pts',(-20.8989852870473,-25.6489352107651,
123.181683998695)) ;
#60189 = CARTESIAN_POINT('Ctrl Pts',(-20.6010425682798,-25.4689461304023,
123.227723257091)) ;
#60190 = CARTESIAN_POINT('Ctrl Pts',(-20.8370703423436,-25.6588745293309,
122.927926047669)) ;
#60191 = CARTESIAN_POINT('Ctrl Pts',(-20.5515128122733,-25.478885448968,123.024716500619)) ;
#60192 = CARTESIAN_POINT('Ctrl Pts',(-20.7307098426691,-25.6689187041067,
122.686357803622)) ;
#60193 = CARTESIAN_POINT('Ctrl Pts',(-20.4664264490109,-25.4889296237439,
122.831461026835)) ;
#60194 = CARTESIAN_POINT('Ctrl Pts',(-20.5866715410215,-25.6787892581717,
122.47063867262)) ;
#60195 = CARTESIAN_POINT('Ctrl Pts',(-20.351197775471,-25.4988001778088,122.658884659411)) ;
#60196 = CARTESIAN_POINT('Ctrl Pts',(-20.4061979028758,-25.6887542405259,
122.280888722177)) ;
#60197 = CARTESIAN_POINT('Ctrl Pts',(-20.2068205491805,-25.508765160163,122.507083201106)) ;
#60198 = CARTESIAN_POINT('Ctrl Pts',(-20.1938959519348,-25.6987849434157,
122.124661424676)) ;
#60199 = CARTESIAN_POINT('Ctrl Pts',(-20.0369803529524,-25.5187958630528,
122.382099587623)) ;
#60200 = CARTESIAN_POINT('Ctrl Pts',(-19.9610841220414,-25.7086772834409,
122.008927766554)) ;
#60201 = CARTESIAN_POINT('Ctrl Pts',(-19.8507319966017,-25.528688203078,122.289510701505)) ;
#60202 = CARTESIAN_POINT('Ctrl Pts',(-19.7077317559287,-25.7187305166009,
121.934171888619)) ;
#60203 = CARTESIAN_POINT('Ctrl Pts',(-19.6480507770561,-25.538741436238,122.229703850899)) ;
#60204 = CARTESIAN_POINT('Ctrl Pts',(-19.4496748815431,-25.7286117610776,
121.904882259363)) ;
#60205 = CARTESIAN_POINT('Ctrl Pts',(-19.4416056279945,-25.5486226807147,
122.206269922949)) ;
#60206 = CARTESIAN_POINT('Ctrl Pts',(-19.1865495494831,-25.7386448819486,
121.920889891667)) ;
#60207 = CARTESIAN_POINT('Ctrl Pts',(-19.2311052788292,-25.5586558015858,
122.219073772921)) ;
#60208 = CARTESIAN_POINT('Ctrl Pts',(-18.933934095788,-25.7485260922237,121.981208015015)) ;
#60209 = CARTESIAN_POINT('Ctrl Pts',(-19.029012442334,-25.5685370118608,122.26732607008)) ;
#60210 = CARTESIAN_POINT('Ctrl Pts',(-18.6913224502721,-25.758588167993,122.086259918764)) ;
#60211 = CARTESIAN_POINT('Ctrl Pts',(-18.8349222926242,-25.5785990876302,
122.351365495269)) ;
#60212 = CARTESIAN_POINT('Ctrl Pts',(-18.4750177696445,-25.7684452263748,
122.228841554689)) ;
#60213 = CARTESIAN_POINT('Ctrl Pts',(-18.6618773148377,-25.5884561460119,
122.465428920654)) ;
#60214 = CARTESIAN_POINT('Ctrl Pts',(-18.2838238477272,-25.7784397816638,
122.408857735709)) ;
#60215 = CARTESIAN_POINT('Ctrl Pts',(-18.5089206655225,-25.5984507013009,
122.60944020259)) ;
#60216 = CARTESIAN_POINT('Ctrl Pts',(-18.1277492566093,-25.7883656691993,
122.617897877619)) ;
#60217 = CARTESIAN_POINT('Ctrl Pts',(-18.3840591928632,-25.6083765888364,
122.77667098702)) ;
#60218 = CARTESIAN_POINT('Ctrl Pts',(-18.0091260993972,-25.7983906891946,
122.853105228335)) ;
#60219 = CARTESIAN_POINT('Ctrl Pts',(-18.2891587030672,-25.6184016088317,
122.964835791046)) ;
#60220 = CARTESIAN_POINT('Ctrl Pts',(-17.9340157762588,-25.8082880662982,
123.102124235181)) ;
#60221 = CARTESIAN_POINT('Ctrl Pts',(-18.2290682857916,-25.6282989859354,
123.164050416227)) ;
#60222 = CARTESIAN_POINT('Ctrl Pts',(-17.9024264992633,-25.8182783033791,
123.362756958186)) ;
#60223 = CARTESIAN_POINT('Ctrl Pts',(-18.2037946795891,-25.6382892230162,
123.372556307197)) ;
#60224 = CARTESIAN_POINT('Ctrl Pts',(-17.9171433202812,-25.8283149161879,
123.62609402293)) ;
#60225 = CARTESIAN_POINT('Ctrl Pts',(-18.2155658929526,-25.648325835825,123.583225962692)) ;
#60226 = CARTESIAN_POINT('Ctrl Pts',(-17.9758333009536,-25.8381647996059,
123.878206838358)) ;
#60227 = CARTESIAN_POINT('Ctrl Pts',(-18.2625157992265,-25.658175719243,123.784916942111)) ;
#60228 = CARTESIAN_POINT('Ctrl Pts',(-18.0784917995666,-25.8481684165084,
124.120189945079)) ;
#60229 = CARTESIAN_POINT('Ctrl Pts',(-18.3446404819217,-25.6681793361455,
123.978504135792)) ;
#60230 = CARTESIAN_POINT('Ctrl Pts',(-18.2215613397651,-25.8581578282735,
124.340338256903)) ;
#60231 = CARTESIAN_POINT('Ctrl Pts',(-18.4590946437798,-25.6781687479106,
124.154624345632)) ;
#60232 = CARTESIAN_POINT('Ctrl Pts',(-18.4012825635189,-25.8681765896183,
124.532704279284)) ;
#60233 = CARTESIAN_POINT('Ctrl Pts',(-18.6028685580281,-25.6881875092555,
124.308517112761)) ;
#60234 = CARTESIAN_POINT('Ctrl Pts',(-18.6786331146531,-25.8813952649994,
124.7419424)) ;
#60235 = CARTESIAN_POINT('Ctrl Pts',(-18.8247543705837,-25.7014061846365,
124.475917413394)) ;
#60236 = CARTESIAN_POINT('Ctrl Pts',(-19.0063037436624,-25.8947055722441,
124.875037990649)) ;
#60237 = CARTESIAN_POINT('Ctrl Pts',(-19.0869232033359,-25.7147164918812,
124.582399636663)) ;
#60238 = CARTESIAN_POINT('Ctrl Pts',(-19.3515492793032,-25.9079432384701,
124.918059062423)) ;
#60239 = CARTESIAN_POINT('Ctrl Pts',(-19.3630728386149,-25.7279541581072,
124.616808324183)) ;
#60240 = CARTESIAN_POINT('Ctrl Pts',(-19.6119358669547,-25.9178629338808,
124.905712873478)) ;
#60241 = CARTESIAN_POINT('Ctrl Pts',(-19.5713918638856,-25.7378738535179,
124.606935541768)) ;
#60242 = CARTESIAN_POINT('Ctrl Pts',(-19.8695568706956,-25.9279158008794,
124.847282646854)) ;
#60243 = CARTESIAN_POINT('Ctrl Pts',(-19.7774862246626,-25.7479267205165,
124.560193132552)) ;
#60244 = CARTESIAN_POINT('Ctrl Pts',(-20.1084811470634,-25.9377712092086,
124.747272818571)) ;
#60245 = CARTESIAN_POINT('Ctrl Pts',(-19.9686281873536,-25.7577821288458,
124.480186034087)) ;
#60246 = CARTESIAN_POINT('Ctrl Pts',(-20.3306652047621,-25.9478098408852,
124.60508116567)) ;
#60247 = CARTESIAN_POINT('Ctrl Pts',(-20.1463738336963,-25.7678207605223,
124.366438470224)) ;
#60248 = CARTESIAN_POINT('Ctrl Pts',(-20.5876341488702,-25.9611120231522,
124.368071353018)) ;
#60249 = CARTESIAN_POINT('Ctrl Pts',(-20.3519625615486,-25.7811229427894,
124.176812457001)) ;
#60250 = CARTESIAN_POINT('Ctrl Pts',(-20.8234715239028,-25.9776570362351,
123.996893725382)) ;
#60251 = CARTESIAN_POINT('Ctrl Pts',(-20.5406208335467,-25.7976679558722,
123.87990862136)) ;
#60252 = CARTESIAN_POINT('Ctrl Pts',(-20.9191905979447,-25.9943090523113,
123.56485434143)) ;
#60253 = CARTESIAN_POINT('Ctrl Pts',(-20.6172087980807,-25.8143199719484,
123.534214776845)) ;
#60254 = CARTESIAN_POINT('Ctrl Pts',(-20.9040855806235,-26.0075321432166,
123.217655815596)) ;
#60255 = CARTESIAN_POINT('Ctrl Pts',(-20.6051216995438,-25.8275430628537,
123.256506511511)) ;
#60256 = CARTESIAN_POINT('Ctrl Pts',(-20.8481710288913,-26.0174931027759,
122.961938491828)) ;
#60257 = CARTESIAN_POINT('Ctrl Pts',(-20.5603924152172,-25.837504022413,123.051921427646)) ;
#60258 = CARTESIAN_POINT('Ctrl Pts',(-20.7477672743641,-26.027517899527,122.718386742879)) ;
#60259 = CARTESIAN_POINT('Ctrl Pts',(-20.4800725252395,-25.8475288191641,
122.857083778402)) ;
#60260 = CARTESIAN_POINT('Ctrl Pts',(-20.561933381812,-26.0407423469228,122.424679164752)) ;
#60261 = CARTESIAN_POINT('Ctrl Pts',(-20.3313987756676,-25.8607532665599,
122.622107468328)) ;
#60262 = CARTESIAN_POINT('Ctrl Pts',(-20.2373134506599,-26.0573761316219,
122.124643357412)) ;
#60263 = CARTESIAN_POINT('Ctrl Pts',(-20.0717139940136,-25.877387051259,122.382085646915)) ;
#60264 = CARTESIAN_POINT('Ctrl Pts',(-19.7495611853889,-26.0772787983468,
121.919792632271)) ;
#60265 = CARTESIAN_POINT('Ctrl Pts',(-19.6815098776299,-25.897289717984,122.218198920366)) ;
#60266 = CARTESIAN_POINT('Ctrl Pts',(-19.22136228124,-26.0971790261287,121.892991857284)) ;
#60267 = CARTESIAN_POINT('Ctrl Pts',(-19.2589510054893,-25.9171899457658,
122.196756056214)) ;
#60268 = CARTESIAN_POINT('Ctrl Pts',(-18.715147674176,-26.1170965136602,122.047840068895)) ;
#60269 = CARTESIAN_POINT('Ctrl Pts',(-18.8539776981445,-25.9371074332973,
122.320631958508)) ;
#60270 = CARTESIAN_POINT('Ctrl Pts',(-18.2916834899083,-26.1370260394771,
122.366086543322)) ;
#60271 = CARTESIAN_POINT('Ctrl Pts',(-18.5152044325254,-25.9570369591142,
122.575227523537)) ;
#60272 = CARTESIAN_POINT('Ctrl Pts',(-18.0018457091614,-26.1569883073634,
122.810521281011)) ;
#60273 = CARTESIAN_POINT('Ctrl Pts',(-18.283332009678,-25.9769992270005,122.930774214087)) ;
#60274 = CARTESIAN_POINT('Ctrl Pts',(-17.8814876928622,-26.1768785023156,
123.325213587121)) ;
#60275 = CARTESIAN_POINT('Ctrl Pts',(-18.1870431423497,-25.9968894219527,
123.342528513262)) ;
#60276 = CARTESIAN_POINT('Ctrl Pts',(-17.942686360803,-26.1967687470618,123.850425839036)) ;
#60277 = CARTESIAN_POINT('Ctrl Pts',(-18.2360005788665,-26.016779666699,123.762699536368)) ;
#60278 = CARTESIAN_POINT('Ctrl Pts',(-18.182532872639,-26.2168431196243,124.326942241085)) ;
#60279 = CARTESIAN_POINT('Ctrl Pts',(-18.4278757324527,-26.0368540392614,
124.143912810045)) ;
#60280 = CARTESIAN_POINT('Ctrl Pts',(-18.5649877790472,-26.2366284969846,
124.687956672163)) ;
#60281 = CARTESIAN_POINT('Ctrl Pts',(-18.7338401401723,-26.0566394166217,
124.432727122548)) ;
#60282 = CARTESIAN_POINT('Ctrl Pts',(-19.0512197803277,-26.2565903710517,
124.900124064153)) ;
#60283 = CARTESIAN_POINT('Ctrl Pts',(-19.1228258509435,-26.0766012906889,
124.602461970491)) ;
#60284 = CARTESIAN_POINT('Ctrl Pts',(-19.5812880978387,-26.2765703465422,
124.932395779744)) ;
#60285 = CARTESIAN_POINT('Ctrl Pts',(-19.5468805975335,-26.0965812661794,
124.628280541388)) ;
#60286 = CARTESIAN_POINT('Ctrl Pts',(-20.0865875254388,-26.2963827764202,
124.784090581285)) ;
#60287 = CARTESIAN_POINT('Ctrl Pts',(-19.9511225306785,-26.1163936960573,
124.50963622777)) ;
#60288 = CARTESIAN_POINT('Ctrl Pts',(-20.5148410357087,-26.3163628845105,
124.470248873448)) ;
#60289 = CARTESIAN_POINT('Ctrl Pts',(-20.2937255891069,-26.1363738041476,
124.258562667596)) ;
#60290 = CARTESIAN_POINT('Ctrl Pts',(-20.8089496480924,-26.3362572681077,
124.030690459046)) ;
#60291 = CARTESIAN_POINT('Ctrl Pts',(-20.5290131148898,-26.1562681877448,
123.906914797705)) ;
#60292 = CARTESIAN_POINT('Ctrl Pts',(-20.9360216455939,-26.3561841960849,
123.516657893152)) ;
#60293 = CARTESIAN_POINT('Ctrl Pts',(-20.6306703947907,-26.1761951157221,
123.495687702575)) ;
#60294 = CARTESIAN_POINT('Ctrl Pts',(-20.8808211228342,-26.3760790533862,
122.990653193015)) ;
#60295 = CARTESIAN_POINT('Ctrl Pts',(-20.5865088182755,-26.1960899730233,
123.074882896028)) ;
#60296 = CARTESIAN_POINT('Ctrl Pts',(-20.647350202661,-26.3961182469898,122.512000068605)) ;
#60297 = CARTESIAN_POINT('Ctrl Pts',(-20.3997313810415,-26.2161291666269,
122.691961220065)) ;
#60298 = CARTESIAN_POINT('Ctrl Pts',(-20.2682064549475,-26.4159582149006,
122.145440895336)) ;
#60299 = CARTESIAN_POINT('Ctrl Pts',(-20.0964143290626,-26.2359691345377,
122.398713470548)) ;
#60300 = CARTESIAN_POINT('Ctrl Pts',(-19.7855675978371,-26.4358730318646,
121.928243360252)) ;
#60301 = CARTESIAN_POINT('Ctrl Pts',(-19.7103017055272,-26.2558839515018,
122.224956789686)) ;
#60302 = CARTESIAN_POINT('Ctrl Pts',(-19.2570238059739,-26.4558152772609,
121.889095738746)) ;
#60303 = CARTESIAN_POINT('Ctrl Pts',(-19.2874659515853,-26.275826196898,122.193640519728)) ;
#60304 = CARTESIAN_POINT('Ctrl Pts',(-18.748249738879,-26.4756873253754,122.031335489932)) ;
#60305 = CARTESIAN_POINT('Ctrl Pts',(-18.8804462675257,-26.2956982450125,
122.307434864793)) ;
#60306 = CARTESIAN_POINT('Ctrl Pts',(-18.3160101803626,-26.4956983903295,
122.340952921604)) ;
#60307 = CARTESIAN_POINT('Ctrl Pts',(-18.5346560494726,-26.3157093099666,
122.555130681776)) ;
#60308 = CARTESIAN_POINT('Ctrl Pts',(-18.0174531568864,-26.5155099146331,
122.774978345867)) ;
#60309 = CARTESIAN_POINT('Ctrl Pts',(-18.2958118673303,-26.3355208342703,
122.902353753564)) ;
#60310 = CARTESIAN_POINT('Ctrl Pts',(-17.883457283048,-26.5356051265965,123.29177843999)) ;
#60311 = CARTESIAN_POINT('Ctrl Pts',(-18.188618039186,-26.3556160462336,123.315793821141)) ;
#60312 = CARTESIAN_POINT('Ctrl Pts',(-17.9332038026506,-26.5553858505163,
123.815368387734)) ;
#60313 = CARTESIAN_POINT('Ctrl Pts',(-18.2284182371962,-26.3753967701534,
123.734667085211)) ;
#60314 = CARTESIAN_POINT('Ctrl Pts',(-18.1597535329976,-26.5753769261591,
124.295760856938)) ;
#60315 = CARTESIAN_POINT('Ctrl Pts',(-18.409661050836,-26.3953878457962,124.118979676145)) ;
#60316 = CARTESIAN_POINT('Ctrl Pts',(-18.5350790245251,-26.5952588652021,
124.667951356014)) ;
#60317 = CARTESIAN_POINT('Ctrl Pts',(-18.7099242517618,-26.4152697848392,
124.416730225271)) ;
#60318 = CARTESIAN_POINT('Ctrl Pts',(-19.0161267182173,-26.6152114697054,
124.89094908574)) ;
#60319 = CARTESIAN_POINT('Ctrl Pts',(-19.0947641449975,-26.4352223893425,
124.595125248235)) ;
#60320 = CARTESIAN_POINT('Ctrl Pts',(-19.5431138580635,-26.635110338436,124.936289536443)) ;
#60321 = CARTESIAN_POINT('Ctrl Pts',(-19.5163546351924,-26.4551212580731,
124.631394176078)) ;
#60322 = CARTESIAN_POINT('Ctrl Pts',(-20.0538241489415,-26.6550037382456,
124.799784245693)) ;
#60323 = CARTESIAN_POINT('Ctrl Pts',(-19.9249224379141,-26.4750146578827,
124.522185551533)) ;
#60324 = CARTESIAN_POINT('Ctrl Pts',(-20.4882718449817,-26.6749128690856,
124.497507103209)) ;
#60325 = CARTESIAN_POINT('Ctrl Pts',(-20.2724781151579,-26.4949237887228,
124.280362392057)) ;
#60326 = CARTESIAN_POINT('Ctrl Pts',(-20.7946862216762,-26.6949449688492,
124.062171882771)) ;
#60327 = CARTESIAN_POINT('Ctrl Pts',(-20.5176077611612,-26.5149558884863,
123.932084425509)) ;
#60328 = CARTESIAN_POINT('Ctrl Pts',(-20.9099487231253,-26.7114770420187,
123.638071483004)) ;
#60329 = CARTESIAN_POINT('Ctrl Pts',(-20.6098098769218,-26.5314879616558,
123.592826514406)) ;
#60330 = CARTESIAN_POINT('Ctrl Pts',(-20.9115489477632,-26.7248123826246,
123.287684923675)) ;
#60331 = CARTESIAN_POINT('Ctrl Pts',(-20.6110911397521,-26.5448233022617,
123.312495827901)) ;
#60332 = CARTESIAN_POINT('Ctrl Pts',(-20.8682561091955,-26.7346549411643,
123.032650001442)) ;
#60333 = CARTESIAN_POINT('Ctrl Pts',(-20.5764556671409,-26.5546658608015,
123.108474233604)) ;
#60334 = CARTESIAN_POINT('Ctrl Pts',(-20.77977083026,-26.7447068480142,122.78379500435)) ;
#60335 = CARTESIAN_POINT('Ctrl Pts',(-20.5056588060069,-26.5647177676514,
122.909381558418)) ;
#60336 = CARTESIAN_POINT('Ctrl Pts',(-20.6078481493321,-26.7579553624051,
122.480989791618)) ;
#60337 = CARTESIAN_POINT('Ctrl Pts',(-20.368152466766,-26.5779662820423,122.667181160605)) ;
#60338 = CARTESIAN_POINT('Ctrl Pts',(-20.2986718809481,-26.7745545373529,
122.166348506659)) ;
#60339 = CARTESIAN_POINT('Ctrl Pts',(-20.120762032831,-26.59456545699,122.415419305003)) ;
#60340 = CARTESIAN_POINT('Ctrl Pts',(-19.9009478345017,-26.7911433231479,
121.976048097058)) ;
#60341 = CARTESIAN_POINT('Ctrl Pts',(-19.8026233502208,-26.6111542427851,
122.263209553901)) ;
#60342 = CARTESIAN_POINT('Ctrl Pts',(-19.5580496300445,-26.8044191394899,
121.911724128209)) ;
#60343 = CARTESIAN_POINT('Ctrl Pts',(-19.5282751818262,-26.624430059127,122.211739560136)) ;
#60344 = CARTESIAN_POINT('Ctrl Pts',(-19.2959531359205,-26.8143929902837,
121.908486613091)) ;
#60345 = CARTESIAN_POINT('Ctrl Pts',(-19.3186038165586,-26.6344039099208,
122.209154538032)) ;
#60346 = CARTESIAN_POINT('Ctrl Pts',(-19.0359115386452,-26.8244220223761,
121.951317775132)) ;
#60347 = CARTESIAN_POINT('Ctrl Pts',(-19.1105694160277,-26.6444329420132,
122.243420903689)) ;
#60348 = CARTESIAN_POINT('Ctrl Pts',(-18.7905877643252,-26.834312147878,122.037189062032)) ;
#60349 = CARTESIAN_POINT('Ctrl Pts',(-18.9143114743061,-26.6543230675151,
122.312120264419)) ;
#60350 = CARTESIAN_POINT('Ctrl Pts',(-18.5614228030226,-26.8443046261495,
122.165337470072)) ;
#60351 = CARTESIAN_POINT('Ctrl Pts',(-18.7309805312086,-26.6643155457866,
122.414640877474)) ;
#60352 = CARTESIAN_POINT('Ctrl Pts',(-18.3586851596353,-26.8542558412469,
122.330580371171)) ;
#60353 = CARTESIAN_POINT('Ctrl Pts',(-18.5687918791563,-26.674266760884,122.546836944886)) ;
#60354 = CARTESIAN_POINT('Ctrl Pts',(-18.1862556413636,-26.8643043430019,
122.530537857795)) ;
#60355 = CARTESIAN_POINT('Ctrl Pts',(-18.4308500085545,-26.6843152626391,
122.706804337278)) ;
#60356 = CARTESIAN_POINT('Ctrl Pts',(-18.0536640724743,-26.8741456926187,
122.752611956706)) ;
#60357 = CARTESIAN_POINT('Ctrl Pts',(-18.3247786705187,-26.6941566122558,
122.884464800855)) ;
#60358 = CARTESIAN_POINT('Ctrl Pts',(-17.9597894559771,-26.8841319836389,
122.997630523713)) ;
#60359 = CARTESIAN_POINT('Ctrl Pts',(-18.2496811140076,-26.7041429032761,
123.080480402911)) ;
#60360 = CARTESIAN_POINT('Ctrl Pts',(-17.9099883261813,-26.8940685953675,
123.254005646133)) ;
#60361 = CARTESIAN_POINT('Ctrl Pts',(-18.2098424357147,-26.7140795150047,
123.285580874397)) ;
#60362 = CARTESIAN_POINT('Ctrl Pts',(-17.9055405282516,-26.9041184707351,
123.518041545854)) ;
#60363 = CARTESIAN_POINT('Ctrl Pts',(-18.2062864585873,-26.7241293903722,
123.496809585011)) ;
#60364 = CARTESIAN_POINT('Ctrl Pts',(-17.9459982769325,-26.9139689292705,
123.7737392886)) ;
#60365 = CARTESIAN_POINT('Ctrl Pts',(-18.2386548730221,-26.7339798489077,
123.70136733283)) ;
#60366 = CARTESIAN_POINT('Ctrl Pts',(-18.0306120394359,-26.9239408662233,
124.021720774531)) ;
#60367 = CARTESIAN_POINT('Ctrl Pts',(-18.3063479820366,-26.7439517858604,
123.89975170688)) ;
#60368 = CARTESIAN_POINT('Ctrl Pts',(-18.1573679303231,-26.9339363231554,
124.251828560722)) ;
#60369 = CARTESIAN_POINT('Ctrl Pts',(-18.4077546301214,-26.7539472427925,
124.083836797404)) ;
#60370 = CARTESIAN_POINT('Ctrl Pts',(-18.3229646348335,-26.9439691302085,
124.456964358552)) ;
#60371 = CARTESIAN_POINT('Ctrl Pts',(-18.540233729948,-26.7639800498456,124.24794399399)) ;
#60372 = CARTESIAN_POINT('Ctrl Pts',(-18.5180312778613,-26.9538290167985,
124.627530238962)) ;
#60373 = CARTESIAN_POINT('Ctrl Pts',(-18.6962883826648,-26.7738399364356,
124.384394886845)) ;
#60374 = CARTESIAN_POINT('Ctrl Pts',(-18.7423698226788,-26.9638180973637,
124.763794005457)) ;
#60375 = CARTESIAN_POINT('Ctrl Pts',(-18.8757603004552,-26.7838290170008,
124.493403950581)) ;
#60376 = CARTESIAN_POINT('Ctrl Pts',(-18.9855793301611,-26.9737495765729,
124.858494603905)) ;
#60377 = CARTESIAN_POINT('Ctrl Pts',(-19.07032857135,-26.79376049621,124.569162300801)) ;
#60378 = CARTESIAN_POINT('Ctrl Pts',(-19.2428644372235,-26.9837354360188,
124.910233267454)) ;
#60379 = CARTESIAN_POINT('Ctrl Pts',(-19.2761570014402,-26.8037463556559,
124.610551055388)) ;
#60380 = CARTESIAN_POINT('Ctrl Pts',(-19.5065740592286,-26.993773586666,124.916079842677)) ;
#60381 = CARTESIAN_POINT('Ctrl Pts',(-19.4871247473151,-26.8137845063031,
124.615226085904)) ;
#60382 = CARTESIAN_POINT('Ctrl Pts',(-19.7624778086568,-27.0036216771704,
124.877322071397)) ;
#60383 = CARTESIAN_POINT('Ctrl Pts',(-19.691847097787,-26.8236325968075,124.584217745267)) ;
#60384 = CARTESIAN_POINT('Ctrl Pts',(-20.0130872707028,-27.0136825856884,
124.793163184846)) ;
#60385 = CARTESIAN_POINT('Ctrl Pts',(-19.892334005724,-26.8336935053255,124.51688855541)) ;
#60386 = CARTESIAN_POINT('Ctrl Pts',(-20.2414042796906,-27.0235774328464,
124.668672645301)) ;
#60387 = CARTESIAN_POINT('Ctrl Pts',(-20.0749863296734,-26.8435883524835,
124.417294323175)) ;
#60388 = CARTESIAN_POINT('Ctrl Pts',(-20.4459889974729,-27.0335191048914,
124.506241389245)) ;
#60389 = CARTESIAN_POINT('Ctrl Pts',(-20.238652605061,-26.8535300245285,124.287347771796)) ;
#60390 = CARTESIAN_POINT('Ctrl Pts',(-20.6204448444618,-27.0435216320169,
124.309576543544)) ;
#60391 = CARTESIAN_POINT('Ctrl Pts',(-20.3782156448559,-26.863532551654,124.130014531869)) ;
#60392 = CARTESIAN_POINT('Ctrl Pts',(-20.758164805552,-27.0535564232043,124.084711962413)) ;
#60393 = CARTESIAN_POINT('Ctrl Pts',(-20.4883897705064,-26.8735673428414,
123.950121722146)) ;
#60394 = CARTESIAN_POINT('Ctrl Pts',(-20.8533381771542,-27.0634013030634,
123.8441219504)) ;
#60395 = CARTESIAN_POINT('Ctrl Pts',(-20.5645263213738,-26.8834122227005,
123.757649351723)) ;
#60396 = CARTESIAN_POINT('Ctrl Pts',(-20.9065073830601,-27.0733871836819,
123.587189440378)) ;
#60397 = CARTESIAN_POINT('Ctrl Pts',(-20.6070596196296,-26.893398103319,123.552103047888)) ;
#60398 = CARTESIAN_POINT('Ctrl Pts',(-20.9144081114304,-27.0833219067751,
123.326185418482)) ;
#60399 = CARTESIAN_POINT('Ctrl Pts',(-20.6133781382632,-26.9033328264122,
123.343300030194)) ;
#60400 = CARTESIAN_POINT('Ctrl Pts',(-20.8761775034525,-27.0933797470863,
123.064696003703)) ;
#60401 = CARTESIAN_POINT('Ctrl Pts',(-20.5827915712378,-26.9133906667234,
123.134108707124)) ;
#60402 = CARTESIAN_POINT('Ctrl Pts',(-20.7954566740253,-27.1032002344828,
122.819537535272)) ;
#60403 = CARTESIAN_POINT('Ctrl Pts',(-20.5182131694661,-26.9232111541199,
122.937983169382)) ;
#60404 = CARTESIAN_POINT('Ctrl Pts',(-20.6708300595228,-27.1132606358279,
122.586414372848)) ;
#60405 = CARTESIAN_POINT('Ctrl Pts',(-20.418510079688,-26.9332715554651,122.751485490579)) ;
#60406 = CARTESIAN_POINT('Ctrl Pts',(-20.5094030853154,-27.1231916013808,
122.381316698631)) ;
#60407 = CARTESIAN_POINT('Ctrl Pts',(-20.2893670916496,-26.943202521018,122.587408842451)) ;
#60408 = CARTESIAN_POINT('Ctrl Pts',(-20.3150919759397,-27.1331304637173,
122.206830149708)) ;
#60409 = CARTESIAN_POINT('Ctrl Pts',(-20.133917119692,-26.9531413833544,122.44782126066)) ;
#60410 = CARTESIAN_POINT('Ctrl Pts',(-20.0924353593602,-27.1431161946435,
122.067902692524)) ;
#60411 = CARTESIAN_POINT('Ctrl Pts',(-19.9557909146957,-26.9631271142806,
122.336681000983)) ;
#60412 = CARTESIAN_POINT('Ctrl Pts',(-19.8480377025175,-27.1531405800709,
121.969643385179)) ;
#60413 = CARTESIAN_POINT('Ctrl Pts',(-19.7602720483066,-26.9731514997081,
122.258075383028)) ;
#60414 = CARTESIAN_POINT('Ctrl Pts',(-19.59343508194,-27.1630438644242,121.915568323419)) ;
#60415 = CARTESIAN_POINT('Ctrl Pts',(-19.5565899913194,-26.9830547840613,
122.214817300124)) ;
#60416 = CARTESIAN_POINT('Ctrl Pts',(-19.3292573389903,-27.1731038690022,
121.90646877428)) ;
#60417 = CARTESIAN_POINT('Ctrl Pts',(-19.3452475890792,-26.9931147886393,
122.207539583563)) ;
#60418 = CARTESIAN_POINT('Ctrl Pts',(-19.0730690560541,-27.1829471380713,
121.942410469089)) ;
#60419 = CARTESIAN_POINT('Ctrl Pts',(-19.1402979129544,-27.0029580577084,
122.236294726187)) ;
#60420 = CARTESIAN_POINT('Ctrl Pts',(-18.8231985706705,-27.192937703679,122.02288556215)) ;
#60421 = CARTESIAN_POINT('Ctrl Pts',(-18.9404022136018,-27.0129486233161,
122.300676481672)) ;
#60422 = CARTESIAN_POINT('Ctrl Pts',(-18.5925284415636,-27.2028658354578,
122.144814465017)) ;
#60423 = CARTESIAN_POINT('Ctrl Pts',(-18.7558673038755,-27.022876755095,122.398221026076)) ;
#60424 = CARTESIAN_POINT('Ctrl Pts',(-18.3850125185332,-27.2128537225387,
122.305545417301)) ;
#60425 = CARTESIAN_POINT('Ctrl Pts',(-18.5898557473657,-27.0328646421759,
122.526807075092)) ;
#60426 = CARTESIAN_POINT('Ctrl Pts',(-18.2080550368114,-27.2228896721074,
122.501085855653)) ;
#60427 = CARTESIAN_POINT('Ctrl Pts',(-18.4482910618857,-27.0429005917445,
122.683240696432)) ;
#60428 = CARTESIAN_POINT('Ctrl Pts',(-18.0698877945043,-27.2327445584862,
122.720150718132)) ;
#60429 = CARTESIAN_POINT('Ctrl Pts',(-18.3377591347981,-27.0527554781234,
122.858492893348)) ;
#60430 = CARTESIAN_POINT('Ctrl Pts',(-17.9701127120356,-27.2427439728341,
122.963197940076)) ;
#60431 = CARTESIAN_POINT('Ctrl Pts',(-18.2579406678591,-27.0627548924712,
123.05293121135)) ;
#60432 = CARTESIAN_POINT('Ctrl Pts',(-17.9143476221429,-27.2526391380246,
123.217227543753)) ;
#60433 = CARTESIAN_POINT('Ctrl Pts',(-18.2133303139703,-27.0726500576617,
123.256154668995)) ;
#60434 = CARTESIAN_POINT('Ctrl Pts',(-17.9033877648429,-27.2626994567166,
123.481339637183)) ;
#60435 = CARTESIAN_POINT('Ctrl Pts',(-18.2045640578609,-27.0827103763537,
123.467444605589)) ;
#60436 = CARTESIAN_POINT('Ctrl Pts',(-17.937576742963,-27.2725495884926,123.737946697359)) ;
#60437 = CARTESIAN_POINT('Ctrl Pts',(-18.2319167231407,-27.0925605081298,
123.672729209851)) ;
#60438 = CARTESIAN_POINT('Ctrl Pts',(-18.0166306722375,-27.2825801589429,
123.989393136718)) ;
#60439 = CARTESIAN_POINT('Ctrl Pts',(-18.2951613035429,-27.10259107858,123.873885960265)) ;
#60440 = CARTESIAN_POINT('Ctrl Pts',(-18.1384764760697,-27.2925943096157,
124.222663794495)) ;
#60441 = CARTESIAN_POINT('Ctrl Pts',(-18.3926393637792,-27.1126052292528,
124.060501732075)) ;
#60442 = CARTESIAN_POINT('Ctrl Pts',(-18.2966929164752,-27.3024872431611,
124.428958569241)) ;
#60443 = CARTESIAN_POINT('Ctrl Pts',(-18.5192133357134,-27.1224981627982,
124.225536119169)) ;
#60444 = CARTESIAN_POINT('Ctrl Pts',(-18.4899718704159,-27.3124767571514,
124.60656373873)) ;
#60445 = CARTESIAN_POINT('Ctrl Pts',(-18.673837373234,-27.1324876767885,124.367619065612)) ;
#60446 = CARTESIAN_POINT('Ctrl Pts',(-18.7103215045909,-27.3224305278038,
124.74758509881)) ;
#60447 = CARTESIAN_POINT('Ctrl Pts',(-18.8501175596139,-27.1424414474409,
124.480434760865)) ;
#60448 = CARTESIAN_POINT('Ctrl Pts',(-18.9541222140896,-27.3324782964644,
124.848911596832)) ;
#60449 = CARTESIAN_POINT('Ctrl Pts',(-19.0451588376447,-27.1524892161015,
124.561494652999)) ;
#60450 = CARTESIAN_POINT('Ctrl Pts',(-19.2065092981465,-27.3423200229042,
124.905498197986)) ;
#60451 = CARTESIAN_POINT('Ctrl Pts',(-19.2470678872194,-27.1623309425413,
124.606762343776)) ;
#60452 = CARTESIAN_POINT('Ctrl Pts',(-19.4685730601993,-27.3523055397269,
124.918145048951)) ;
#60453 = CARTESIAN_POINT('Ctrl Pts',(-19.456718762585,-27.172316459364,124.616878517439)) ;
#60454 = CARTESIAN_POINT('Ctrl Pts',(-19.727737905255,-27.3622448714225,124.885335148688)) ;
#60455 = CARTESIAN_POINT('Ctrl Pts',(-19.6640500453479,-27.1822557910596,
124.590629385903)) ;
#60456 = CARTESIAN_POINT('Ctrl Pts',(-19.9797167083431,-27.37228464112,124.807206664709)) ;
#60457 = CARTESIAN_POINT('Ctrl Pts',(-19.8656328181808,-27.1922955607571,
124.528125331113)) ;
#60458 = CARTESIAN_POINT('Ctrl Pts',(-20.210851339288,-27.3821728023688,124.688432935281)) ;
#60459 = CARTESIAN_POINT('Ctrl Pts',(-20.0505392887375,-27.2021837220059,
124.433105562087)) ;
#60460 = CARTESIAN_POINT('Ctrl Pts',(-20.4202523049205,-27.3921623568712,
124.530127299133)) ;
#60461 = CARTESIAN_POINT('Ctrl Pts',(-20.2180592277372,-27.2121732765083,
124.306460234651)) ;
#60462 = CARTESIAN_POINT('Ctrl Pts',(-20.5982841261054,-27.4021207713948,
124.338329003495)) ;
#60463 = CARTESIAN_POINT('Ctrl Pts',(-20.360483568371,-27.222131691032,124.153021035403)) ;
#60464 = CARTESIAN_POINT('Ctrl Pts',(-20.7400208952278,-27.4120206842242,
124.120151747141)) ;
#60465 = CARTESIAN_POINT('Ctrl Pts',(-20.473871715113,-27.2320316038613,123.9784792444)) ;
#60466 = CARTESIAN_POINT('Ctrl Pts',(-20.8431437130591,-27.4220673838741,
123.877134998684)) ;
#60467 = CARTESIAN_POINT('Ctrl Pts',(-20.5563690459131,-27.2420783035112,
123.784065268537)) ;
#60468 = CARTESIAN_POINT('Ctrl Pts',(-20.9018126855217,-27.4319672441797,
123.623637353348)) ;
#60469 = CARTESIAN_POINT('Ctrl Pts',(-20.6033030544183,-27.2519781638168,
123.581267614642)) ;
#60470 = CARTESIAN_POINT('Ctrl Pts',(-20.9158681861848,-27.4420186483852,
123.359908517845)) ;
#60471 = CARTESIAN_POINT('Ctrl Pts',(-20.614546450276,-27.2620295680223,123.370284295332)) ;
#60472 = CARTESIAN_POINT('Ctrl Pts',(-20.8845444215458,-27.4518996853063,
123.102102763115)) ;
#60473 = CARTESIAN_POINT('Ctrl Pts',(-20.5894865476393,-27.2719106049434,
123.164040624998)) ;
#60474 = CARTESIAN_POINT('Ctrl Pts',(-20.8083897017697,-27.4618995174838,
122.850639705419)) ;
#60475 = CARTESIAN_POINT('Ctrl Pts',(-20.5285619312095,-27.2819104371209,
122.962870552448)) ;
#60476 = CARTESIAN_POINT('Ctrl Pts',(-20.6908521995959,-27.4718175204687,
122.61796100732)) ;
#60477 = CARTESIAN_POINT('Ctrl Pts',(-20.43453143348,-27.2918284401058,122.776728527516)) ;
#60478 = CARTESIAN_POINT('Ctrl Pts',(-20.5325862276468,-27.4818688263432,
122.406544566139)) ;
#60479 = CARTESIAN_POINT('Ctrl Pts',(-20.3079178321186,-27.3018797459804,
122.607595752983)) ;
#60480 = CARTESIAN_POINT('Ctrl Pts',(-20.3436360267876,-27.4917386497348,
122.228783160696)) ;
#60481 = CARTESIAN_POINT('Ctrl Pts',(-20.1567577854576,-27.3117495693719,
122.465387842878)) ;
#60482 = CARTESIAN_POINT('Ctrl Pts',(-20.1222882553386,-27.5018128157851,
122.083664260692)) ;
#60483 = CARTESIAN_POINT('Ctrl Pts',(-19.9796788329855,-27.3218237354222,
122.349293214515)) ;
#60484 = CARTESIAN_POINT('Ctrl Pts',(-19.8852542608473,-27.5116328999267,
121.981478176074)) ;
#60485 = CARTESIAN_POINT('Ctrl Pts',(-19.7900524902871,-27.3316438195639,
122.267545514143)) ;
#60486 = CARTESIAN_POINT('Ctrl Pts',(-19.6276445348726,-27.5217116266626,
121.920220233275)) ;
#60487 = CARTESIAN_POINT('Ctrl Pts',(-19.5839641856869,-27.3417225462997,
122.218539730451)) ;
#60488 = CARTESIAN_POINT('Ctrl Pts',(-19.3691479103184,-27.5315632073121,
121.904877852358)) ;
#60489 = CARTESIAN_POINT('Ctrl Pts',(-19.3771679014181,-27.3515741269492,
122.206266540335)) ;
#60490 = CARTESIAN_POINT('Ctrl Pts',(-19.1062132173581,-27.5416363356105,
121.935078088023)) ;
#60491 = CARTESIAN_POINT('Ctrl Pts',(-19.1668198669398,-27.3616472552476,
122.230427363407)) ;
#60492 = CARTESIAN_POINT('Ctrl Pts',(-18.8582685980059,-27.5514788135019,
122.008806224884)) ;
#60493 = CARTESIAN_POINT('Ctrl Pts',(-18.9684654319779,-27.3714897331391,
122.289410133124)) ;
#60494 = CARTESIAN_POINT('Ctrl Pts',(-18.6232876861483,-27.5614594201,122.125286522871)) ;
#60495 = CARTESIAN_POINT('Ctrl Pts',(-18.7804810973601,-27.3814703397371,
122.382594611719)) ;
#60496 = CARTESIAN_POINT('Ctrl Pts',(-18.4116002704639,-27.5714771291188,
122.281782687979)) ;
#60497 = CARTESIAN_POINT('Ctrl Pts',(-18.6111314675826,-27.3914880487559,
122.507791959957)) ;
#60498 = CARTESIAN_POINT('Ctrl Pts',(-18.2323009870814,-27.5813633081562,
122.469819398542)) ;
#60499 = CARTESIAN_POINT('Ctrl Pts',(-18.4676929146779,-27.4013742277934,
122.65822097498)) ;
#60500 = CARTESIAN_POINT('Ctrl Pts',(-18.0858887221731,-27.5914209207286,
122.689836404072)) ;
#60501 = CARTESIAN_POINT('Ctrl Pts',(-18.3505632824027,-27.4114318403657,
122.834234999918)) ;
#60502 = CARTESIAN_POINT('Ctrl Pts',(-17.981772680714,-27.6012973141007,122.927596725681)) ;
#60503 = CARTESIAN_POINT('Ctrl Pts',(-18.2672711670262,-27.4213082337378,
123.024442556299)) ;
#60504 = CARTESIAN_POINT('Ctrl Pts',(-17.9191542665853,-27.6112923422511,
123.182674524743)) ;
#60505 = CARTESIAN_POINT('Ctrl Pts',(-18.2171766775005,-27.4313032618883,
123.228504708676)) ;
#60506 = CARTESIAN_POINT('Ctrl Pts',(-17.9021807329972,-27.6213130890971,
123.445473162291)) ;
#60507 = CARTESIAN_POINT('Ctrl Pts',(-18.2035981738734,-27.4413240087343,
123.4387436757)) ;
#60508 = CARTESIAN_POINT('Ctrl Pts',(-17.930448869701,-27.6312151577635,123.704146901839)) ;
#60509 = CARTESIAN_POINT('Ctrl Pts',(-18.2262128505501,-27.4512260774006,
123.645681876394)) ;
#60510 = CARTESIAN_POINT('Ctrl Pts',(-18.0034825912362,-27.6412058975832,
123.956332064129)) ;
#60511 = CARTESIAN_POINT('Ctrl Pts',(-18.2846399233845,-27.4612168172203,
123.847429782292)) ;
#60512 = CARTESIAN_POINT('Ctrl Pts',(-18.1190427862629,-27.6511690937935,
124.191258163438)) ;
#60513 = CARTESIAN_POINT('Ctrl Pts',(-18.3770881012001,-27.4711800134306,
124.035370248739)) ;
#60514 = CARTESIAN_POINT('Ctrl Pts',(-18.2722240570765,-27.6610732780936,
124.401708795378)) ;
#60515 = CARTESIAN_POINT('Ctrl Pts',(-18.4996327056077,-27.4810841977308,
124.203730123677)) ;
#60516 = CARTESIAN_POINT('Ctrl Pts',(-18.4626904000373,-27.6711337384845,
124.585014918484)) ;
#60517 = CARTESIAN_POINT('Ctrl Pts',(-18.6520060497622,-27.4911446581216,
124.350375149966)) ;
#60518 = CARTESIAN_POINT('Ctrl Pts',(-18.6771667745688,-27.6809742843553,
124.729554078274)) ;
#60519 = CARTESIAN_POINT('Ctrl Pts',(-18.8235861793774,-27.5009852039924,
124.466005811902)) ;
#60520 = CARTESIAN_POINT('Ctrl Pts',(-18.9186090603338,-27.6910365050671,
124.83730737481)) ;
#60521 = CARTESIAN_POINT('Ctrl Pts',(-19.016740247443,-27.5110474247042,124.552208638131)) ;
#60522 = CARTESIAN_POINT('Ctrl Pts',(-19.1709926750529,-27.7009336480836,
124.900195583727)) ;
#60523 = CARTESIAN_POINT('Ctrl Pts',(-19.2186463603094,-27.5209445677207,
124.602519015299)) ;
#60524 = CARTESIAN_POINT('Ctrl Pts',(-19.4312729665485,-27.7108648245008,
124.919233320648)) ;
#60525 = CARTESIAN_POINT('Ctrl Pts',(-19.4268700019089,-27.5308757441379,
124.617749388828)) ;
#60526 = CARTESIAN_POINT('Ctrl Pts',(-19.6937795868889,-27.7209070382794,
124.892204557255)) ;
#60527 = CARTESIAN_POINT('Ctrl Pts',(-19.636875479684,-27.5409179579165,124.59612651213)) ;
#60528 = CARTESIAN_POINT('Ctrl Pts',(-19.9437421483585,-27.7307935784821,
124.821306255689)) ;
#60529 = CARTESIAN_POINT('Ctrl Pts',(-19.836844746594,-27.5508044981193,124.539408302028)) ;
#60530 = CARTESIAN_POINT('Ctrl Pts',(-20.180282407611,-27.7407871730876,124.707252644134)) ;
#60531 = CARTESIAN_POINT('Ctrl Pts',(-20.0260769445174,-27.5607980927247,
124.448165758018)) ;
#60532 = CARTESIAN_POINT('Ctrl Pts',(-20.3923713220577,-27.7507310482451,
124.554570637425)) ;
#60533 = CARTESIAN_POINT('Ctrl Pts',(-20.1957478479467,-27.5707419678822,
124.326020684454)) ;
#60534 = CARTESIAN_POINT('Ctrl Pts',(-20.5752568933734,-27.7606915843599,
124.367331130021)) ;
#60535 = CARTESIAN_POINT('Ctrl Pts',(-20.3420563159796,-27.5807025039971,
124.176229618266)) ;
#60536 = CARTESIAN_POINT('Ctrl Pts',(-20.7235437790341,-27.7706881876827,
124.150451479886)) ;
#60537 = CARTESIAN_POINT('Ctrl Pts',(-20.4606861037265,-27.5906991073198,
124.002726235317)) ;
#60538 = CARTESIAN_POINT('Ctrl Pts',(-20.8319614750394,-27.7807212706372,
123.910121632712)) ;
#60539 = CARTESIAN_POINT('Ctrl Pts',(-20.5474206058342,-27.6007321902743,
123.810462391625)) ;
#60540 = CARTESIAN_POINT('Ctrl Pts',(-20.8961417940296,-27.7905724393387,
123.65932892789)) ;
#60541 = CARTESIAN_POINT('Ctrl Pts',(-20.5987649851893,-27.6105833589758,
123.609829391344)) ;
#60542 = CARTESIAN_POINT('Ctrl Pts',(-20.9167937428057,-27.8005349300376,
123.398350225034)) ;
#60543 = CARTESIAN_POINT('Ctrl Pts',(-20.6152871158748,-27.6205458496747,
123.401046845239)) ;
#60544 = CARTESIAN_POINT('Ctrl Pts',(-20.8913248727649,-27.8105633584554,
123.136032193867)) ;
#60545 = CARTESIAN_POINT('Ctrl Pts',(-20.5949125321571,-27.6305742780925,
123.191192291486)) ;
#60546 = CARTESIAN_POINT('Ctrl Pts',(-20.8216156440544,-27.8204737258199,
122.885112920422)) ;
#60547 = CARTESIAN_POINT('Ctrl Pts',(-20.5391458591745,-27.640484645457,122.990457403175)) ;
#60548 = CARTESIAN_POINT('Ctrl Pts',(-20.7097290522174,-27.830408593435,122.649216253135)) ;
#60549 = CARTESIAN_POINT('Ctrl Pts',(-20.4496374549925,-27.6504195130721,
122.801740241644)) ;
#60550 = CARTESIAN_POINT('Ctrl Pts',(-20.5567753117552,-27.840449735414,122.434208642636)) ;
#60551 = CARTESIAN_POINT('Ctrl Pts',(-20.3272749058312,-27.6604606550512,
122.629733654314)) ;
#60552 = CARTESIAN_POINT('Ctrl Pts',(-20.371806724897,-27.8503368716172,122.251718186914)) ;
#60553 = CARTESIAN_POINT('Ctrl Pts',(-20.1793011160621,-27.6703477912543,
122.483741378946)) ;
#60554 = CARTESIAN_POINT('Ctrl Pts',(-20.1559638841929,-27.8603291540206,
122.102205529793)) ;
#60555 = CARTESIAN_POINT('Ctrl Pts',(-20.006627433317,-27.6803400736577,122.364130687556)) ;
#60556 = CARTESIAN_POINT('Ctrl Pts',(-19.9184230348256,-27.8702776819858,
121.99297454764)) ;
#60557 = CARTESIAN_POINT('Ctrl Pts',(-19.816595474273,-27.6902886016229,122.276745372545)) ;
#60558 = CARTESIAN_POINT('Ctrl Pts',(-19.665953180287,-27.8802144131479,121.926377817828)) ;
#60559 = CARTESIAN_POINT('Ctrl Pts',(-19.6146203057764,-27.7002253327851,
122.223467276849)) ;
#60560 = CARTESIAN_POINT('Ctrl Pts',(-19.4045120642448,-27.8901976240079,
121.904196807196)) ;
#60561 = CARTESIAN_POINT('Ctrl Pts',(-19.4054676973117,-27.710208543645,122.205721541653)) ;
#60562 = CARTESIAN_POINT('Ctrl Pts',(-19.1417251311674,-27.9002407231578,
121.92835440127)) ;
#60563 = CARTESIAN_POINT('Ctrl Pts',(-19.1952379245654,-27.7202516427949,
122.225046799241)) ;
#60564 = CARTESIAN_POINT('Ctrl Pts',(-18.892293224786,-27.9100716874327,121.995765252508)) ;
#60565 = CARTESIAN_POINT('Ctrl Pts',(-18.9956932551907,-27.7300826070698,
122.278974240053)) ;
#60566 = CARTESIAN_POINT('Ctrl Pts',(-18.6525836805033,-27.9201445398186,
122.107953193368)) ;
#60567 = CARTESIAN_POINT('Ctrl Pts',(-18.8039248906843,-27.7401554594558,
122.368723808351)) ;
#60568 = CARTESIAN_POINT('Ctrl Pts',(-18.4404518362338,-27.9300086675304,
122.256983728471)) ;
#60569 = CARTESIAN_POINT('Ctrl Pts',(-18.6342195866533,-27.7500195871675,
122.487946889381)) ;
#60570 = CARTESIAN_POINT('Ctrl Pts',(-18.2540538810711,-27.9400308696653,
122.44303741669)) ;
#60571 = CARTESIAN_POINT('Ctrl Pts',(-18.4851003818533,-27.7600417893024,
122.636789047312)) ;
#60572 = CARTESIAN_POINT('Ctrl Pts',(-18.1032133230383,-27.9500580626337,
122.659116134907)) ;
#60573 = CARTESIAN_POINT('Ctrl Pts',(-18.3644270759834,-27.7700689822708,
122.809651490149)) ;
#60574 = CARTESIAN_POINT('Ctrl Pts',(-17.9937284543403,-27.9599136566007,
122.893810711294)) ;
#60575 = CARTESIAN_POINT('Ctrl Pts',(-18.2768385935525,-27.7799245762378,
122.997405800576)) ;
#60576 = CARTESIAN_POINT('Ctrl Pts',(-17.9252066477856,-27.969870828466,123.146353412769)) ;
#60577 = CARTESIAN_POINT('Ctrl Pts',(-18.2220200039114,-27.7898817481031,
123.199439298674)) ;
#60578 = CARTESIAN_POINT('Ctrl Pts',(-17.9018363926086,-27.9799096724644,
123.409110487333)) ;
#60579 = CARTESIAN_POINT('Ctrl Pts',(-18.2033226182715,-27.7999205921015,
123.409644963665)) ;
#60580 = CARTESIAN_POINT('Ctrl Pts',(-17.9236207437678,-27.98978369634,123.667708642615)) ;
#60581 = CARTESIAN_POINT('Ctrl Pts',(-18.2207487591916,-27.8097946159771,
123.616522787693)) ;
#60582 = CARTESIAN_POINT('Ctrl Pts',(-17.9912807797275,-27.9998535223304,
123.923499029241)) ;
#60583 = CARTESIAN_POINT('Ctrl Pts',(-18.2748756263371,-27.8198644419675,
123.821155692994)) ;
#60584 = CARTESIAN_POINT('Ctrl Pts',(-18.0996170115864,-28.0096867662276,
124.158124720439)) ;
#60585 = CARTESIAN_POINT('Ctrl Pts',(-18.3615429995661,-27.8296976858648,
124.008855863308)) ;
#60586 = CARTESIAN_POINT('Ctrl Pts',(-18.249371382821,-28.0197171940007,124.375030745284)) ;
#60587 = CARTESIAN_POINT('Ctrl Pts',(-18.481345335379,-27.8397281136378,124.182381569428)) ;
#60588 = CARTESIAN_POINT('Ctrl Pts',(-18.4350962680924,-28.0297488107458,
124.562139179243)) ;
#60589 = CARTESIAN_POINT('Ctrl Pts',(-18.6299243679393,-27.8497597303829,
124.332069278655)) ;
#60590 = CARTESIAN_POINT('Ctrl Pts',(-18.6458160519967,-28.0395784877265,
124.711519341739)) ;
#60591 = CARTESIAN_POINT('Ctrl Pts',(-18.798498550654,-27.8595894073637,124.451573974288)) ;
#60592 = CARTESIAN_POINT('Ctrl Pts',(-18.8827549500496,-28.0495680045665,
124.824558143869)) ;
#60593 = CARTESIAN_POINT('Ctrl Pts',(-18.9880488657586,-27.8695789242036,
124.542006370576)) ;
#60594 = CARTESIAN_POINT('Ctrl Pts',(-19.1372585887124,-28.0596116167062,
124.894470815532)) ;
#60595 = CARTESIAN_POINT('Ctrl Pts',(-19.1916515109275,-27.8796225363434,
124.597937922925)) ;
#60596 = CARTESIAN_POINT('Ctrl Pts',(-19.3942099817878,-28.0694342230415,
124.91912779169)) ;
#60597 = CARTESIAN_POINT('Ctrl Pts',(-19.3972114824336,-27.8894451426787,
124.617664945199)) ;
#60598 = CARTESIAN_POINT('Ctrl Pts',(-19.6572218646034,-28.0794724529408,
124.898947663021)) ;
#60599 = CARTESIAN_POINT('Ctrl Pts',(-19.6076212137935,-27.8994833725779,
124.601522486604)) ;
#60600 = CARTESIAN_POINT('Ctrl Pts',(-19.9119170104515,-28.0894834877327,
124.832984826371)) ;
#60601 = CARTESIAN_POINT('Ctrl Pts',(-19.8113776795567,-27.9094944073698,
124.548753715423)) ;
#60602 = CARTESIAN_POINT('Ctrl Pts',(-20.1487320477206,-28.0993812186998,
124.725423875281)) ;
#60603 = CARTESIAN_POINT('Ctrl Pts',(-20.000829845105,-27.919392138337,124.462706670356)) ;
#60604 = CARTESIAN_POINT('Ctrl Pts',(-20.3654611748462,-28.1093708465503,
124.5772951408)) ;
#60605 = CARTESIAN_POINT('Ctrl Pts',(-20.1742139780183,-27.9293817661874,
124.344205147162)) ;
#60606 = CARTESIAN_POINT('Ctrl Pts',(-20.5524779416027,-28.1193266369963,
124.394341663434)) ;
#60607 = CARTESIAN_POINT('Ctrl Pts',(-20.3238283305594,-27.9393375566334,
124.197843770989)) ;
#60608 = CARTESIAN_POINT('Ctrl Pts',(-20.7048656204767,-28.1292540355584,
124.182581520283)) ;
#60609 = CARTESIAN_POINT('Ctrl Pts',(-20.4457396528893,-27.9492649551955,
124.028437013102)) ;
#60610 = CARTESIAN_POINT('Ctrl Pts',(-20.8192132351186,-28.1392796306682,
123.945237856592)) ;
#60611 = CARTESIAN_POINT('Ctrl Pts',(-20.5372193152296,-27.9592905503054,
123.838562820331)) ;
#60612 = CARTESIAN_POINT('Ctrl Pts',(-20.8897744387993,-28.1491654813378,
123.695212486568)) ;
#60613 = CARTESIAN_POINT('Ctrl Pts',(-20.5936698151312,-27.9691764009749,
123.638543566476)) ;
#60614 = CARTESIAN_POINT('Ctrl Pts',(-20.9167426862714,-28.159154661182,123.434089007642)) ;
#60615 = CARTESIAN_POINT('Ctrl Pts',(-20.6152462522755,-27.9791655808191,
123.429645100009)) ;
#60616 = CARTESIAN_POINT('Ctrl Pts',(-20.8973138529512,-28.1691958482856,
123.170934263122)) ;
#60617 = CARTESIAN_POINT('Ctrl Pts',(-20.5997049495287,-27.9892067679227,
123.219121101024)) ;
#60618 = CARTESIAN_POINT('Ctrl Pts',(-20.8342467261708,-28.1790284917615,
122.920361624849)) ;
#60619 = CARTESIAN_POINT('Ctrl Pts',(-20.5492532207289,-27.9990394113987,
123.018663281372)) ;
#60620 = CARTESIAN_POINT('Ctrl Pts',(-20.7275828726051,-28.189022441471,122.680368443651)) ;
#60621 = CARTESIAN_POINT('Ctrl Pts',(-20.463923962656,-28.0090333611081,122.826668031653)) ;
#60622 = CARTESIAN_POINT('Ctrl Pts',(-20.5798888066981,-28.1990515642475,
122.462081994114)) ;
#60623 = CARTESIAN_POINT('Ctrl Pts',(-20.3457702502389,-28.0190624838847,
122.652037809533)) ;
#60624 = CARTESIAN_POINT('Ctrl Pts',(-20.3996251641318,-28.2089276951662,
122.275347174546)) ;
#60625 = CARTESIAN_POINT('Ctrl Pts',(-20.2015610992789,-28.0289386148033,
122.502648999522)) ;
#60626 = CARTESIAN_POINT('Ctrl Pts',(-20.1873021799441,-28.2189257301832,
122.120642324747)) ;
#60627 = CARTESIAN_POINT('Ctrl Pts',(-20.0317039475205,-28.0389366498204,
122.37888357736)) ;
#60628 = CARTESIAN_POINT('Ctrl Pts',(-19.9533587455655,-28.2288396599419,
122.005916898594)) ;
#60629 = CARTESIAN_POINT('Ctrl Pts',(-19.8445504140462,-28.0488505795791,
122.287101605949)) ;
#60630 = CARTESIAN_POINT('Ctrl Pts',(-19.6998517913933,-28.2388828476797,
121.932573093305)) ;
#60631 = CARTESIAN_POINT('Ctrl Pts',(-19.6417453532736,-28.0588937673169,
122.228424618319)) ;
#60632 = CARTESIAN_POINT('Ctrl Pts',(-19.4411734358199,-28.2487826898201,
121.904743447238)) ;
#60633 = CARTESIAN_POINT('Ctrl Pts',(-19.4348032777468,-28.0687936094572,
122.206158949824)) ;
#60634 = CARTESIAN_POINT('Ctrl Pts',(-19.1791693222562,-28.2587739566281,
121.921854204058)) ;
#60635 = CARTESIAN_POINT('Ctrl Pts',(-19.2251999469823,-28.0787848762652,
122.219845480099)) ;
#60636 = CARTESIAN_POINT('Ctrl Pts',(-18.923180998322,-28.2688060587601,121.984895781452)) ;
#60637 = CARTESIAN_POINT('Ctrl Pts',(-19.0204087941554,-28.0888169783972,
122.270276784581)) ;
#60638 = CARTESIAN_POINT('Ctrl Pts',(-18.6858684267657,-28.2786729397148,
122.08935619064)) ;
#60639 = CARTESIAN_POINT('Ctrl Pts',(-18.830558338332,-28.098683859352,122.353843037551)) ;
#60640 = CARTESIAN_POINT('Ctrl Pts',(-18.4672132264588,-28.288664731003,122.234743944374)) ;
#60641 = CARTESIAN_POINT('Ctrl Pts',(-18.6556330730798,-28.1086756506401,
122.470151422643)) ;
#60642 = CARTESIAN_POINT('Ctrl Pts',(-18.276712974157,-28.2986968469145,122.416985014583)) ;
#60643 = CARTESIAN_POINT('Ctrl Pts',(-18.5032314387329,-28.1187077665516,
122.615942781619)) ;
#60644 = CARTESIAN_POINT('Ctrl Pts',(-18.1230016340979,-28.3085631637145,
122.625798315029)) ;
#60645 = CARTESIAN_POINT('Ctrl Pts',(-18.380260910136,-28.1285740833517,122.782991837959)) ;
#60646 = CARTESIAN_POINT('Ctrl Pts',(-18.0061033569078,-28.3185506451881,
122.86075275285)) ;
#60647 = CARTESIAN_POINT('Ctrl Pts',(-18.2867404042396,-28.1385615648253,
122.970954341277)) ;
#60648 = CARTESIAN_POINT('Ctrl Pts',(-17.931940003922,-28.328495569567,123.111391293711)) ;
#60649 = CARTESIAN_POINT('Ctrl Pts',(-18.2274077034628,-28.1485064892042,
123.171464381746)) ;
#60650 = CARTESIAN_POINT('Ctrl Pts',(-17.902279648867,-28.3385404554777,123.373664123611)) ;
#60651 = CARTESIAN_POINT('Ctrl Pts',(-18.2036772802856,-28.1585513751149,
123.381282418945)) ;
#60652 = CARTESIAN_POINT('Ctrl Pts',(-17.9180879856087,-28.3484025591903,
123.632366059909)) ;
#60653 = CARTESIAN_POINT('Ctrl Pts',(-18.2163217656105,-28.1684134788274,
123.588243760099)) ;
#60654 = CARTESIAN_POINT('Ctrl Pts',(-17.978845222314,-28.3583941230148,123.887787950721)) ;
#60655 = CARTESIAN_POINT('Ctrl Pts',(-18.2649253910361,-28.1784050426519,
123.792581709161)) ;
#60656 = CARTESIAN_POINT('Ctrl Pts',(-18.0825235360191,-28.3683269310777,
124.127337211337)) ;
#60657 = CARTESIAN_POINT('Ctrl Pts',(-18.3478659549648,-28.1883378507148,
123.984221828264)) ;
#60658 = CARTESIAN_POINT('Ctrl Pts',(-18.2257556811439,-28.378264033314,124.345706898237)) ;
#60659 = CARTESIAN_POINT('Ctrl Pts',(-18.4624497295589,-28.1982749529511,
124.158918686381)) ;
#60660 = CARTESIAN_POINT('Ctrl Pts',(-18.4070352870554,-28.3883164795844,
124.537830699298)) ;
#60661 = CARTESIAN_POINT('Ctrl Pts',(-18.6074717934068,-28.2083273992215,
124.312619238854)) ;
#60662 = CARTESIAN_POINT('Ctrl Pts',(-18.6143836431893,-28.398162595166,124.692645379455)) ;
#60663 = CARTESIAN_POINT('Ctrl Pts',(-18.7733489636727,-28.2181735148031,
124.436472636285)) ;
#60664 = CARTESIAN_POINT('Ctrl Pts',(-18.8499799673712,-28.4082106148809,
124.811841582492)) ;
#60665 = CARTESIAN_POINT('Ctrl Pts',(-18.9618249984737,-28.228221534518,124.531831597543)) ;
#60666 = CARTESIAN_POINT('Ctrl Pts',(-19.1001636769322,-28.4181525665098,
124.887173703346)) ;
#60667 = CARTESIAN_POINT('Ctrl Pts',(-19.1619712108279,-28.238163486147,124.592099400923)) ;
#60668 = CARTESIAN_POINT('Ctrl Pts',(-19.3594558684256,-28.4280913475089,
124.91855224253)) ;
#60669 = CARTESIAN_POINT('Ctrl Pts',(-19.3694046064628,-28.248102267146,124.61720445296)) ;
#60670 = CARTESIAN_POINT('Ctrl Pts',(-19.6225169288426,-28.438117396235,124.904110048364)) ;
#60671 = CARTESIAN_POINT('Ctrl Pts',(-19.5798535127197,-28.2581283158721,
124.60565295931)) ;
#60672 = CARTESIAN_POINT('Ctrl Pts',(-19.8756354818284,-28.4480042566432,
124.845353062354)) ;
#60673 = CARTESIAN_POINT('Ctrl Pts',(-19.7823488152932,-28.2680151762803,
124.55864953328)) ;
#60674 = CARTESIAN_POINT('Ctrl Pts',(-20.1181752200281,-28.458035531775,124.742190925089)) ;
#60675 = CARTESIAN_POINT('Ctrl Pts',(-19.9763812831176,-28.2780464514121,
124.476122110811)) ;
#60676 = CARTESIAN_POINT('Ctrl Pts',(-20.3360779496977,-28.4679185090754,
124.600777052286)) ;
#60677 = CARTESIAN_POINT('Ctrl Pts',(-20.1507052303913,-28.2879294287125,
124.362992221081)) ;
#60678 = CARTESIAN_POINT('Ctrl Pts',(-20.5293776948737,-28.4779753624826,
124.420644314917)) ;
#60679 = CARTESIAN_POINT('Ctrl Pts',(-20.3053443489214,-28.2979862821197,
124.218890369488)) ;
#60680 = CARTESIAN_POINT('Ctrl Pts',(-20.7382563360483,-28.4911436035585,
124.144618303968)) ;
#60681 = CARTESIAN_POINT('Ctrl Pts',(-20.4724604249661,-28.3111545231956,
123.998058237581)) ;
#60682 = CARTESIAN_POINT('Ctrl Pts',(-20.8725696183407,-28.504544632785,123.814898572995)) ;
#60683 = CARTESIAN_POINT('Ctrl Pts',(-20.5799131718557,-28.3245555524222,
123.734258095252)) ;
#60684 = CARTESIAN_POINT('Ctrl Pts',(-20.9154664864313,-28.5177575495159,
123.470229804426)) ;
#60685 = CARTESIAN_POINT('Ctrl Pts',(-20.6142236339119,-28.337768469153,123.458566993245)) ;
#60686 = CARTESIAN_POINT('Ctrl Pts',(-20.9031228604222,-28.5276859439691,
123.209668872578)) ;
#60687 = CARTESIAN_POINT('Ctrl Pts',(-20.6043529645336,-28.3476968636062,
123.250109340891)) ;
#60688 = CARTESIAN_POINT('Ctrl Pts',(-20.8455899283561,-28.5376674440972,
122.953713451803)) ;
#60689 = CARTESIAN_POINT('Ctrl Pts',(-20.5583282472634,-28.3576783637344,
123.045346890605)) ;
#60690 = CARTESIAN_POINT('Ctrl Pts',(-20.7435726949857,-28.5477079873673,
122.710393832338)) ;
#60691 = CARTESIAN_POINT('Ctrl Pts',(-20.4767166760668,-28.3677189070045,
122.850689784726)) ;
#60692 = CARTESIAN_POINT('Ctrl Pts',(-20.6038530329981,-28.5575573191504,
122.492510433972)) ;
#60693 = CARTESIAN_POINT('Ctrl Pts',(-20.3649427782715,-28.3775682387876,
122.676381961247)) ;
#60694 = CARTESIAN_POINT('Ctrl Pts',(-20.4263234254277,-28.5675527236221,
122.298921849287)) ;
#60695 = CARTESIAN_POINT('Ctrl Pts',(-20.2229202780013,-28.3875636432592,
122.521509270193)) ;
#60696 = CARTESIAN_POINT('Ctrl Pts',(-20.2171504397288,-28.5775690510707,
122.139134607576)) ;
#60697 = CARTESIAN_POINT('Ctrl Pts',(-20.0555849188895,-28.3975799707078,
122.393679028551)) ;
#60698 = CARTESIAN_POINT('Ctrl Pts',(-19.9087920777924,-28.5907927082372,
121.978832990271)) ;
#60699 = CARTESIAN_POINT('Ctrl Pts',(-19.8088913174118,-28.4108036278744,
122.265428956437)) ;
#60700 = CARTESIAN_POINT('Ctrl Pts',(-19.5639959876032,-28.6040869996266,
121.90200706357)) ;
#60701 = CARTESIAN_POINT('Ctrl Pts',(-19.5330215630254,-28.4240979192637,
122.203967911005)) ;
#60702 = CARTESIAN_POINT('Ctrl Pts',(-19.2151418343695,-28.6173713505581,
121.916882629654)) ;
#60703 = CARTESIAN_POINT('Ctrl Pts',(-19.2539858779433,-28.4373822701952,
122.215868656955)) ;
#60704 = CARTESIAN_POINT('Ctrl Pts',(-18.9592277477311,-28.6273437316199,
121.973142750752)) ;
#60705 = CARTESIAN_POINT('Ctrl Pts',(-19.0492444708714,-28.447354651257,122.260874150028)) ;
#60706 = CARTESIAN_POINT('Ctrl Pts',(-18.7182849243588,-28.6372521112455,
122.071948770313)) ;
#60707 = CARTESIAN_POINT('Ctrl Pts',(-18.8564918768448,-28.4572630308826,
122.33991702492)) ;
#60708 = CARTESIAN_POINT('Ctrl Pts',(-18.4950390577731,-28.6473061099936,
122.213201780035)) ;
#60709 = CARTESIAN_POINT('Ctrl Pts',(-18.6778931410017,-28.4673170296307,
122.452918687146)) ;
#60710 = CARTESIAN_POINT('Ctrl Pts',(-18.3032620688519,-28.6571683071099,
122.38756772639)) ;
#60711 = CARTESIAN_POINT('Ctrl Pts',(-18.5244716495436,-28.477179226747,122.592405885585)) ;
#60712 = CARTESIAN_POINT('Ctrl Pts',(-18.0882237967221,-28.670515433484,122.664637872146)) ;
#60713 = CARTESIAN_POINT('Ctrl Pts',(-18.352430803744,-28.4905263531211,122.814082073788)) ;
#60714 = CARTESIAN_POINT('Ctrl Pts',(-17.9176634712148,-28.6870523991254,
123.069772556873)) ;
#60715 = CARTESIAN_POINT('Ctrl Pts',(-18.2159875992731,-28.5070633187626,
123.138150149593)) ;
#60716 = CARTESIAN_POINT('Ctrl Pts',(-17.8947632869084,-28.7036870032994,
123.511208297081)) ;
#60717 = CARTESIAN_POINT('Ctrl Pts',(-18.1976653221791,-28.5236979229365,
123.491362432851)) ;
#60718 = CARTESIAN_POINT('Ctrl Pts',(-17.9677541226804,-28.716976796542,123.852806493769)) ;
#60719 = CARTESIAN_POINT('Ctrl Pts',(-18.256052534024,-28.5369877161791,123.764590263567)) ;
#60720 = CARTESIAN_POINT('Ctrl Pts',(-18.0656567609654,-28.7269294278014,
124.095304375433)) ;
#60721 = CARTESIAN_POINT('Ctrl Pts',(-18.3343741827955,-28.5469403474385,
123.9586001496)) ;
#60722 = CARTESIAN_POINT('Ctrl Pts',(-18.2039394803118,-28.7368813951061,
124.317317362258)) ;
#60723 = CARTESIAN_POINT('Ctrl Pts',(-18.444996651739,-28.5568923147432,124.136207458359)) ;
#60724 = CARTESIAN_POINT('Ctrl Pts',(-18.4387363200913,-28.7502486535699,
124.578542730155)) ;
#60725 = CARTESIAN_POINT('Ctrl Pts',(-18.6328430825618,-28.570259573207,124.345197322045)) ;
#60726 = CARTESIAN_POINT('Ctrl Pts',(-18.8064292376097,-28.7667654655191,
124.818587725884)) ;
#60727 = CARTESIAN_POINT('Ctrl Pts',(-18.9269842710425,-28.5867763851562,
124.537227610055)) ;
#60728 = CARTESIAN_POINT('Ctrl Pts',(-19.3245222155934,-28.7867913605254,
124.939922033055)) ;
#60729 = CARTESIAN_POINT('Ctrl Pts',(-19.3414616488824,-28.6068022801626,
124.634301067543)) ;
#60730 = CARTESIAN_POINT('Ctrl Pts',(-19.8475073460439,-28.8066020906556,
124.877979440127)) ;
#60731 = CARTESIAN_POINT('Ctrl Pts',(-19.7598502986681,-28.6266130102927,
124.58474931514)) ;
#60732 = CARTESIAN_POINT('Ctrl Pts',(-20.3222930272887,-28.8265793067854,
124.640387404646)) ;
#60733 = CARTESIAN_POINT('Ctrl Pts',(-20.1396805393653,-28.6465902264226,
124.39467832848)) ;
#60734 = CARTESIAN_POINT('Ctrl Pts',(-20.6858890813368,-28.8465061821807,
124.255335344324)) ;
#60735 = CARTESIAN_POINT('Ctrl Pts',(-20.4305598381238,-28.6665171018178,
124.086638285115)) ;
#60736 = CARTESIAN_POINT('Ctrl Pts',(-20.896748937638,-28.866327643657,123.772474684031)) ;
#60737 = CARTESIAN_POINT('Ctrl Pts',(-20.5992504644692,-28.6863385632941,
123.700349310091)) ;
#60738 = CARTESIAN_POINT('Ctrl Pts',(-20.930240651337,-28.8864019614663,123.240064582413)) ;
#60739 = CARTESIAN_POINT('Ctrl Pts',(-20.6260460784137,-28.7064128811034,
123.27442205142)) ;
#60740 = CARTESIAN_POINT('Ctrl Pts',(-20.7811745275789,-28.9062499304742,
122.733886817119)) ;
#60741 = CARTESIAN_POINT('Ctrl Pts',(-20.5067950359757,-28.7262608501113,
122.869477923346)) ;
#60742 = CARTESIAN_POINT('Ctrl Pts',(-20.4677973260097,-28.9261969645374,
122.306404432572)) ;
#60743 = CARTESIAN_POINT('Ctrl Pts',(-20.2560944036663,-28.7462078841745,
122.527490503496)) ;
#60744 = CARTESIAN_POINT('Ctrl Pts',(-20.0282780332881,-28.9460929155096,
122.012300463532)) ;
#60745 = CARTESIAN_POINT('Ctrl Pts',(-19.9044790239162,-28.7661038351467,
122.292205334614)) ;
#60746 = CARTESIAN_POINT('Ctrl Pts',(-19.5150711784553,-28.9659883951278,
121.885006525189)) ;
#60747 = CARTESIAN_POINT('Ctrl Pts',(-19.4939126765269,-28.7859993147649,
122.190368780619)) ;
#60748 = CARTESIAN_POINT('Ctrl Pts',(-18.987543756163,-28.9859445060926,121.940541079356)) ;
#60749 = CARTESIAN_POINT('Ctrl Pts',(-19.0718901729245,-28.8059554257297,
122.234795557163)) ;
#60750 = CARTESIAN_POINT('Ctrl Pts',(-18.5120357100849,-29.0058490541326,
122.172247469475)) ;
#60751 = CARTESIAN_POINT('Ctrl Pts',(-18.6914823057681,-28.8258599737697,
122.420160465214)) ;
#60752 = CARTESIAN_POINT('Ctrl Pts',(-18.1436273509991,-29.0257231784517,
122.550925494824)) ;
#60753 = CARTESIAN_POINT('Ctrl Pts',(-18.3967545360288,-28.8457340980888,
122.723104052043)) ;
#60754 = CARTESIAN_POINT('Ctrl Pts',(-17.9253569901024,-29.0457777084507,
123.037111210492)) ;
#60755 = CARTESIAN_POINT('Ctrl Pts',(-18.2221384159378,-28.8657886280878,
123.112051915873)) ;
#60756 = CARTESIAN_POINT('Ctrl Pts',(-17.8864107136343,-29.0655852222107,
123.562230606204)) ;
#60757 = CARTESIAN_POINT('Ctrl Pts',(-18.1909813694771,-28.8855961418478,
123.532149866875)) ;
#60758 = CARTESIAN_POINT('Ctrl Pts',(-18.0291344865639,-29.0855685779784,
124.073742812752)) ;
#60759 = CARTESIAN_POINT('Ctrl Pts',(-18.3051612924804,-28.9055794976156,
123.941359571674)) ;
#60760 = CARTESIAN_POINT('Ctrl Pts',(-18.3375275327191,-29.1054868805624,
124.504029337498)) ;
#60761 = CARTESIAN_POINT('Ctrl Pts',(-18.5518768788528,-28.9254978001995,
124.285589192693)) ;
#60762 = CARTESIAN_POINT('Ctrl Pts',(-18.7724331767996,-29.1253550960081,
124.803732067651)) ;
#60763 = CARTESIAN_POINT('Ctrl Pts',(-18.8998033875348,-28.9453660156452,
124.525350924034)) ;
#60764 = CARTESIAN_POINT('Ctrl Pts',(-19.2881479519155,-29.1454054128044,
124.937374691163)) ;
#60765 = CARTESIAN_POINT('Ctrl Pts',(-19.3123750642973,-28.9654163324415,
124.632263609282)) ;
#60766 = CARTESIAN_POINT('Ctrl Pts',(-19.8116842876558,-29.1651814746869,
124.888368150055)) ;
#60767 = CARTESIAN_POINT('Ctrl Pts',(-19.7312061711631,-28.985192394324,124.59305641669)) ;
#60768 = CARTESIAN_POINT('Ctrl Pts',(-20.2935470559368,-29.1852360803793,
124.661024000669)) ;
#60769 = CARTESIAN_POINT('Ctrl Pts',(-20.1166950466578,-29.0052470000165,
124.411179407397)) ;
#60770 = CARTESIAN_POINT('Ctrl Pts',(-20.6641709204212,-29.2050297695352,
124.287435707295)) ;
#60771 = CARTESIAN_POINT('Ctrl Pts',(-20.413193887911,-29.0250406891723,124.112305976162)) ;
#60772 = CARTESIAN_POINT('Ctrl Pts',(-20.8881946382118,-29.2249964611296,
123.806481690324)) ;
#60773 = CARTESIAN_POINT('Ctrl Pts',(-20.592410427374,-29.0450073807667,123.727541366071)) ;
#60774 = CARTESIAN_POINT('Ctrl Pts',(-20.9338249693073,-29.2449565068806,
123.277844260743)) ;
#60775 = CARTESIAN_POINT('Ctrl Pts',(-20.62891209658,-29.0649674265177,123.304630928054)) ;
#60776 = CARTESIAN_POINT('Ctrl Pts',(-20.7971171356574,-29.2648547670308,
122.766988876807)) ;
#60777 = CARTESIAN_POINT('Ctrl Pts',(-20.5195428530867,-29.084865686668,122.895946613903)) ;
#60778 = CARTESIAN_POINT('Ctrl Pts',(-20.4948597929885,-29.28474968258,122.33314837501)) ;
#60779 = CARTESIAN_POINT('Ctrl Pts',(-20.2777339778196,-29.1047606022171,
122.548875457773)) ;
#60780 = CARTESIAN_POINT('Ctrl Pts',(-20.0626359964947,-29.3046598629936,
122.027845909722)) ;
#60781 = CARTESIAN_POINT('Ctrl Pts',(-19.9319525576066,-29.1246707826307,
122.304635941344)) ;
#60782 = CARTESIAN_POINT('Ctrl Pts',(-19.5515593327172,-29.3245956621079,
121.887948224382)) ;
#60783 = CARTESIAN_POINT('Ctrl Pts',(-19.5230899669336,-29.144606581745,122.19272116096)) ;
#60784 = CARTESIAN_POINT('Ctrl Pts',(-19.0233846938744,-29.344533523762,121.930820617086)) ;
#60785 = CARTESIAN_POINT('Ctrl Pts',(-19.1005502612154,-29.1645444433991,
122.227022574999)) ;
#60786 = CARTESIAN_POINT('Ctrl Pts',(-18.5418309889796,-29.3644525703997,
122.150865733304)) ;
#60787 = CARTESIAN_POINT('Ctrl Pts',(-18.7153085362879,-29.1844634900368,
122.403062807844)) ;
#60788 = CARTESIAN_POINT('Ctrl Pts',(-18.1636813294162,-29.3844014684538,
122.522511403366)) ;
#60789 = CARTESIAN_POINT('Ctrl Pts',(-18.4127914568634,-29.2044123880909,
122.700380148177)) ;
#60790 = CARTESIAN_POINT('Ctrl Pts',(-17.9354075384507,-29.4043072958969,
122.999821271264)) ;
#60791 = CARTESIAN_POINT('Ctrl Pts',(-18.2301756194061,-29.224318215534,123.082237846385)) ;
#60792 = CARTESIAN_POINT('Ctrl Pts',(-17.8918934979895,-29.4208899912622,
123.438338526591)) ;
#60793 = CARTESIAN_POINT('Ctrl Pts',(-18.195368494416,-29.2409009108993,123.4330280738)) ;
#60794 = CARTESIAN_POINT('Ctrl Pts',(-17.9480247352152,-29.4341642049858,
123.782679410161)) ;
#60795 = CARTESIAN_POINT('Ctrl Pts',(-18.2402760241612,-29.2541751246229,
123.708522277928)) ;
#60796 = CARTESIAN_POINT('Ctrl Pts',(-18.0352295821613,-29.4442109241851,
124.031850013628)) ;
#60797 = CARTESIAN_POINT('Ctrl Pts',(-18.3100397891959,-29.2642218438223,
123.907851739695)) ;
#60798 = CARTESIAN_POINT('Ctrl Pts',(-18.1615379687603,-29.4540549588308,
124.257627504343)) ;
#60799 = CARTESIAN_POINT('Ctrl Pts',(-18.4110966944545,-29.2740658784679,
124.088481420666)) ;
#60800 = CARTESIAN_POINT('Ctrl Pts',(-18.3825117400926,-29.4673893437353,
124.529570908532)) ;
#60801 = CARTESIAN_POINT('Ctrl Pts',(-18.587837079466,-29.2874002633725,124.305998087073)) ;
#60802 = CARTESIAN_POINT('Ctrl Pts',(-18.7397290349317,-29.4839765610351,
124.788022651488)) ;
#60803 = CARTESIAN_POINT('Ctrl Pts',(-18.8736672821377,-29.3039874806722,
124.512799388885)) ;
#60804 = CARTESIAN_POINT('Ctrl Pts',(-19.1646822605817,-29.500609773073,124.90971077457)) ;
#60805 = CARTESIAN_POINT('Ctrl Pts',(-19.2135860980992,-29.3206206927101,
124.610126710635)) ;
#60806 = CARTESIAN_POINT('Ctrl Pts',(-19.5137203885275,-29.5138922153452,
124.915596996125)) ;
#60807 = CARTESIAN_POINT('Ctrl Pts',(-19.4928464224192,-29.3339031349823,
124.614841247233)) ;
#60808 = CARTESIAN_POINT('Ctrl Pts',(-19.7708729287446,-29.5237981032594,
124.875254844356)) ;
#60809 = CARTESIAN_POINT('Ctrl Pts',(-19.6985621395063,-29.3438090228965,
124.582563747932)) ;
#60810 = CARTESIAN_POINT('Ctrl Pts',(-20.0193014854552,-29.5337865213645,
124.790472867222)) ;
#60811 = CARTESIAN_POINT('Ctrl Pts',(-19.8973061999821,-29.3537974410017,
124.51473599808)) ;
#60812 = CARTESIAN_POINT('Ctrl Pts',(-20.2499022751864,-29.5438099486033,
124.663153811252)) ;
#60813 = CARTESIAN_POINT('Ctrl Pts',(-20.0817838661683,-29.3638208682404,
124.412880687566)) ;
#60814 = CARTESIAN_POINT('Ctrl Pts',(-20.4525327560064,-29.5537143797203,
124.499823981593)) ;
#60815 = CARTESIAN_POINT('Ctrl Pts',(-20.2438922431529,-29.3737252993574,
124.282207749836)) ;
#60816 = CARTESIAN_POINT('Ctrl Pts',(-20.6825120254526,-29.5669775323307,
124.237867726831)) ;
#60817 = CARTESIAN_POINT('Ctrl Pts',(-20.4278473773578,-29.3869884519678,
124.072677218546)) ;
#60818 = CARTESIAN_POINT('Ctrl Pts',(-20.8392151516731,-29.5803024302346,
123.9203381995)) ;
#60819 = CARTESIAN_POINT('Ctrl Pts',(-20.553226732279,-29.4003133498717,123.818635845126)) ;
#60820 = CARTESIAN_POINT('Ctrl Pts',(-20.9074394904579,-29.5935581738502,
123.578684401647)) ;
#60821 = CARTESIAN_POINT('Ctrl Pts',(-20.6078059447763,-29.4135690934873,
123.545295374543)) ;
#60822 = CARTESIAN_POINT('Ctrl Pts',(-20.9137330388378,-29.6035175472975,
123.317072430943)) ;
#60823 = CARTESIAN_POINT('Ctrl Pts',(-20.6128379811963,-29.4235284669346,
123.336009184031)) ;
#60824 = CARTESIAN_POINT('Ctrl Pts',(-20.8748846541773,-29.6134613712245,
123.058630457453)) ;
#60825 = CARTESIAN_POINT('Ctrl Pts',(-20.5817571955094,-29.4334722908616,
123.129255093572)) ;
#60826 = CARTESIAN_POINT('Ctrl Pts',(-20.7906838438031,-29.6235093153718,
122.808386846984)) ;
#60827 = CARTESIAN_POINT('Ctrl Pts',(-20.5143943808657,-29.4435202350089,
122.929061213128)) ;
#60828 = CARTESIAN_POINT('Ctrl Pts',(-20.666972739531,-29.6333602865899,122.580969032646)) ;
#60829 = CARTESIAN_POINT('Ctrl Pts',(-20.4154235694875,-29.4533712062271,
122.747128058925)) ;
#60830 = CARTESIAN_POINT('Ctrl Pts',(-20.504231739043,-29.643332104032,122.37561747521)) ;
#60831 = CARTESIAN_POINT('Ctrl Pts',(-20.285229061277,-29.4633430236691,122.582848300707)) ;
#60832 = CARTESIAN_POINT('Ctrl Pts',(-20.3077646577954,-29.6533275263241,
122.20121873475)) ;
#60833 = CARTESIAN_POINT('Ctrl Pts',(-20.1280539536979,-29.4733384459612,
122.443331024174)) ;
#60834 = CARTESIAN_POINT('Ctrl Pts',(-20.0830517816903,-29.6633605914478,
122.063322483088)) ;
#60835 = CARTESIAN_POINT('Ctrl Pts',(-19.9482825016034,-29.4833715110849,
122.333015964112)) ;
#60836 = CARTESIAN_POINT('Ctrl Pts',(-19.8419990547799,-29.673225924113,121.967921099706)) ;
#60837 = CARTESIAN_POINT('Ctrl Pts',(-19.7554396557229,-29.4932368437501,
122.256697012164)) ;
#60838 = CARTESIAN_POINT('Ctrl Pts',(-19.5857362753535,-29.6831864667106,
121.914563791572)) ;
#60839 = CARTESIAN_POINT('Ctrl Pts',(-19.5504291017455,-29.5031973863477,
122.214013362556)) ;
#60840 = CARTESIAN_POINT('Ctrl Pts',(-19.3221856204255,-29.6932201522123,
121.906899471747)) ;
#60841 = CARTESIAN_POINT('Ctrl Pts',(-19.3395885271886,-29.5132310718494,
122.207884142788)) ;
#60842 = CARTESIAN_POINT('Ctrl Pts',(-19.0650645565921,-29.7031049842026,
121.944106565339)) ;
#60843 = CARTESIAN_POINT('Ctrl Pts',(-19.1338922165619,-29.5231159038397,
122.237651976139)) ;
#60844 = CARTESIAN_POINT('Ctrl Pts',(-18.8138468784926,-29.7131724109624,
122.026926609439)) ;
#60845 = CARTESIAN_POINT('Ctrl Pts',(-18.9329187385003,-29.5331833305995,
122.303910131109)) ;
#60846 = CARTESIAN_POINT('Ctrl Pts',(-18.5859272208204,-29.7230109001213,
122.149077864787)) ;
#60847 = CARTESIAN_POINT('Ctrl Pts',(-18.7505843444716,-29.5430218197584,
122.401632918194)) ;
#60848 = CARTESIAN_POINT('Ctrl Pts',(-18.3778786570836,-29.7330743813114,
122.312276880641)) ;
#60849 = CARTESIAN_POINT('Ctrl Pts',(-18.5841468108762,-29.5530853009485,
122.532193870255)) ;
#60850 = CARTESIAN_POINT('Ctrl Pts',(-18.2044212593036,-29.7429685391265,
122.506008820073)) ;
#60851 = CARTESIAN_POINT('Ctrl Pts',(-18.4453827052769,-29.5629794587636,
122.687180688913)) ;
#60852 = CARTESIAN_POINT('Ctrl Pts',(-18.0660044708574,-29.7529103958708,
122.727551566468)) ;
#60853 = CARTESIAN_POINT('Ctrl Pts',(-18.334651204385,-29.5729213155079,122.864415841661)) ;
#60854 = CARTESIAN_POINT('Ctrl Pts',(-17.9674436496093,-29.7629128735422,
122.971267274101)) ;
#60855 = CARTESIAN_POINT('Ctrl Pts',(-18.255804547113,-29.5829237931793,123.059389144256)) ;
#60856 = CARTESIAN_POINT('Ctrl Pts',(-17.9129372902024,-29.7729476778465,
123.229259453664)) ;
#60857 = CARTESIAN_POINT('Ctrl Pts',(-18.2122015796833,-29.5929585974836,
123.265783349704)) ;
#60858 = CARTESIAN_POINT('Ctrl Pts',(-17.9037873257415,-29.7827925546922,
123.487828320676)) ;
#60859 = CARTESIAN_POINT('Ctrl Pts',(-18.2048837514533,-29.6028034743293,
123.472638064826)) ;
#60860 = CARTESIAN_POINT('Ctrl Pts',(-17.9396889314393,-29.7927784342477,
123.747736250522)) ;
#60861 = CARTESIAN_POINT('Ctrl Pts',(-18.2336070824238,-29.6127893538848,
123.680563995791)) ;
#60862 = CARTESIAN_POINT('Ctrl Pts',(-18.0196096204046,-29.8027131646062,
123.996330158484)) ;
#60863 = CARTESIAN_POINT('Ctrl Pts',(-18.2975455112086,-29.6227240842433,
123.879438242773)) ;
#60864 = CARTESIAN_POINT('Ctrl Pts',(-18.1431663387283,-29.8127709769191,
124.229931834435)) ;
#60865 = CARTESIAN_POINT('Ctrl Pts',(-18.3963927784555,-29.6327818965562,
124.066318691056)) ;
#60866 = CARTESIAN_POINT('Ctrl Pts',(-18.3012830487912,-29.8225915690435,
124.433951656902)) ;
#60867 = CARTESIAN_POINT('Ctrl Pts',(-18.5228873635076,-29.6426024886806,
124.229532798967)) ;
#60868 = CARTESIAN_POINT('Ctrl Pts',(-18.4969190824133,-29.8326581546532,
124.611938648179)) ;
#60869 = CARTESIAN_POINT('Ctrl Pts',(-18.679397626606,-29.6526690742904,124.37192099675)) ;
#60870 = CARTESIAN_POINT('Ctrl Pts',(-18.7169004533599,-29.8425577352351,
124.750929340355)) ;
#60871 = CARTESIAN_POINT('Ctrl Pts',(-18.8553834510956,-29.6625686548722,
124.483111642557)) ;
#60872 = CARTESIAN_POINT('Ctrl Pts',(-18.9612300162177,-29.8526093349133,
124.851178041536)) ;
#60873 = CARTESIAN_POINT('Ctrl Pts',(-19.050847943237,-29.6726202545505,124.563308795822)) ;
#60874 = CARTESIAN_POINT('Ctrl Pts',(-19.2147547487882,-29.8624835213303,
124.90669960071)) ;
#60875 = CARTESIAN_POINT('Ctrl Pts',(-19.2536676428027,-29.6824944409674,
124.607724013081)) ;
#60876 = CARTESIAN_POINT('Ctrl Pts',(-19.4787496446823,-29.8725399972112,
124.917720031893)) ;
#60877 = CARTESIAN_POINT('Ctrl Pts',(-19.4648637461611,-29.6925509168483,
124.616538418507)) ;
#60878 = CARTESIAN_POINT('Ctrl Pts',(-19.7365039466463,-29.8824329285138,
124.883386677831)) ;
#60879 = CARTESIAN_POINT('Ctrl Pts',(-19.6710664653841,-29.7024438481509,
124.589069887457)) ;
#60880 = CARTESIAN_POINT('Ctrl Pts',(-19.9885582400929,-29.8924957072264,
124.803550123632)) ;
#60881 = CARTESIAN_POINT('Ctrl Pts',(-19.8727094596313,-29.7125066268636,
124.52519876481)) ;
#60882 = CARTESIAN_POINT('Ctrl Pts',(-20.2179182729383,-29.9023382328076,
124.683922711731)) ;
#60883 = CARTESIAN_POINT('Ctrl Pts',(-20.0561959904771,-29.7223491524447,
124.429495469086)) ;
#60884 = CARTESIAN_POINT('Ctrl Pts',(-20.4264420362186,-29.9123289982325,
124.524451584241)) ;
#60885 = CARTESIAN_POINT('Ctrl Pts',(-20.2230137897094,-29.7323399178696,
124.301917213795)) ;
#60886 = CARTESIAN_POINT('Ctrl Pts',(-20.6029907905239,-29.9222570742305,
124.332343420825)) ;
#60887 = CARTESIAN_POINT('Ctrl Pts',(-20.3642511922906,-29.7422679938676,
124.148229742484)) ;
#60888 = CARTESIAN_POINT('Ctrl Pts',(-20.7447343008597,-29.9322449846175,
124.11142218186)) ;
#60889 = CARTESIAN_POINT('Ctrl Pts',(-20.4776444559696,-29.7522559042547,
123.971491933959)) ;
#60890 = CARTESIAN_POINT('Ctrl Pts',(-20.8460304545597,-29.9422808967425,
123.867929241378)) ;
#60891 = CARTESIAN_POINT('Ctrl Pts',(-20.5586797287902,-29.7622918163796,
123.776696819529)) ;
#60892 = CARTESIAN_POINT('Ctrl Pts',(-20.9028976475888,-29.9521359095901,
123.61524963978)) ;
#60893 = CARTESIAN_POINT('Ctrl Pts',(-20.6041716209895,-29.7721468292273,
123.574553473142)) ;
#60894 = CARTESIAN_POINT('Ctrl Pts',(-20.9155677101948,-29.9621348555064,
123.352835793816)) ;
#60895 = CARTESIAN_POINT('Ctrl Pts',(-20.6143059849255,-29.7821457751435,
123.364622425134)) ;
#60896 = CARTESIAN_POINT('Ctrl Pts',(-20.8830605294398,-29.9720317679544,
123.094753953415)) ;
#60897 = CARTESIAN_POINT('Ctrl Pts',(-20.5882986910333,-29.7920426875915,
123.158157729796)) ;
#60898 = CARTESIAN_POINT('Ctrl Pts',(-20.805069403928,-29.9820855660479,122.84235819033)) ;
#60899 = CARTESIAN_POINT('Ctrl Pts',(-20.5259041888426,-29.802096485685,122.956241456897)) ;
#60900 = CARTESIAN_POINT('Ctrl Pts',(-20.6865523391872,-29.9919664868746,
122.611290225832)) ;
#60901 = CARTESIAN_POINT('Ctrl Pts',(-20.4310894079275,-29.8119774065117,
122.771388421395)) ;
#60902 = CARTESIAN_POINT('Ctrl Pts',(-20.5281670015566,-30.0019710128723,
122.40148341337)) ;
#60903 = CARTESIAN_POINT('Ctrl Pts',(-20.3043799645414,-29.8219819325095,
122.603543955252)) ;
#60904 = CARTESIAN_POINT('Ctrl Pts',(-20.3360451640396,-30.0119549764898,
122.222739387201)) ;
#60905 = CARTESIAN_POINT('Ctrl Pts',(-20.1506815650826,-29.8319658961269,
122.460549974152)) ;
#60906 = CARTESIAN_POINT('Ctrl Pts',(-20.1144958155581,-30.0219946170411,
122.079517699187)) ;
#60907 = CARTESIAN_POINT('Ctrl Pts',(-19.9734411337302,-29.8420055366782,
122.345973905275)) ;
#60908 = CARTESIAN_POINT('Ctrl Pts',(-19.8762838854574,-30.0318386426558,
121.978637774701)) ;
#60909 = CARTESIAN_POINT('Ctrl Pts',(-19.7828718281963,-29.8518495622929,
122.265271730029)) ;
#60910 = CARTESIAN_POINT('Ctrl Pts',(-19.6205810796489,-30.0418296484732,
121.919049659348)) ;
#60911 = CARTESIAN_POINT('Ctrl Pts',(-19.5783094204032,-29.8618405681103,
122.217602616233)) ;
#60912 = CARTESIAN_POINT('Ctrl Pts',(-19.3571576412147,-30.0518674400053,
121.905299416152)) ;
#60913 = CARTESIAN_POINT('Ctrl Pts',(-19.3675704851451,-29.8718783596425,
122.206603915684)) ;
#60914 = CARTESIAN_POINT('Ctrl Pts',(-19.1003268169004,-30.0617118397937,
121.936426083733)) ;
#60915 = CARTESIAN_POINT('Ctrl Pts',(-19.1621069272286,-29.8817227594309,
122.231506534638)) ;
#60916 = CARTESIAN_POINT('Ctrl Pts',(-18.8491638611297,-30.0716966403505,
122.012238721689)) ;
#60917 = CARTESIAN_POINT('Ctrl Pts',(-18.9611771300981,-29.8917075599876,
122.292157833579)) ;
#60918 = CARTESIAN_POINT('Ctrl Pts',(-18.6159274223169,-30.0816361637616,
122.129904287764)) ;
#60919 = CARTESIAN_POINT('Ctrl Pts',(-18.774588942654,-29.9016470833988,122.386291228805)) ;
#60920 = CARTESIAN_POINT('Ctrl Pts',(-18.4046377386934,-30.0916758828626,
122.287871780247)) ;
#60921 = CARTESIAN_POINT('Ctrl Pts',(-18.6055578744043,-29.9116868024998,
122.512666327168)) ;
#60922 = CARTESIAN_POINT('Ctrl Pts',(-18.2265933390173,-30.1015640547819,
122.477161788335)) ;
#60923 = CARTESIAN_POINT('Ctrl Pts',(-18.4631237804811,-29.921574974419,122.664098660573)) ;
#60924 = CARTESIAN_POINT('Ctrl Pts',(-18.0822626446461,-30.1115536171989,
122.696428624441)) ;
#60925 = CARTESIAN_POINT('Ctrl Pts',(-18.3476602845798,-29.931564536836,122.839512622054)) ;
#60926 = CARTESIAN_POINT('Ctrl Pts',(-17.9786995241896,-30.1215119893936,
122.936755300708)) ;
#60927 = CARTESIAN_POINT('Ctrl Pts',(-18.2648110278588,-29.9415229090307,
123.031774118599)) ;
#60928 = CARTESIAN_POINT('Ctrl Pts',(-17.9181786121953,-30.1314120636243,
123.189791746356)) ;
#60929 = CARTESIAN_POINT('Ctrl Pts',(-18.2163954912986,-29.9514229832614,
123.234202841237)) ;
#60930 = CARTESIAN_POINT('Ctrl Pts',(-17.9023177046355,-30.1414581599979,
123.453303427384)) ;
#60931 = CARTESIAN_POINT('Ctrl Pts',(-18.2037078197734,-29.961469079635,123.445012405779)) ;
#60932 = CARTESIAN_POINT('Ctrl Pts',(-17.9320269697077,-30.151366743995,123.712002752069)) ;
#60933 = CARTESIAN_POINT('Ctrl Pts',(-18.2274762127078,-29.9713776636321,
123.651971093748)) ;
#60934 = CARTESIAN_POINT('Ctrl Pts',(-18.0064982865296,-30.1613773225859,
123.964313150607)) ;
#60935 = CARTESIAN_POINT('Ctrl Pts',(-18.2870541704328,-29.981388242223,123.853819106392)) ;
#60936 = CARTESIAN_POINT('Ctrl Pts',(-18.1243449648106,-30.1714064806987,
124.200064581345)) ;
#60937 = CARTESIAN_POINT('Ctrl Pts',(-18.3813325117191,-29.9914174003359,
124.042419843847)) ;
#60938 = CARTESIAN_POINT('Ctrl Pts',(-18.2782623863857,-30.1812593625368,
124.408253321648)) ;
#60939 = CARTESIAN_POINT('Ctrl Pts',(-18.5044666446186,-30.0012702821739,
124.208969431975)) ;
#60940 = CARTESIAN_POINT('Ctrl Pts',(-18.4674836005063,-30.1912189236878,
124.589086196399)) ;
#60941 = CARTESIAN_POINT('Ctrl Pts',(-18.6558438971189,-30.0112298433249,
124.35363489223)) ;
#60942 = CARTESIAN_POINT('Ctrl Pts',(-18.687199388826,-30.2012573582769,124.735052040734)) ;
#60943 = CARTESIAN_POINT('Ctrl Pts',(-18.8316171435154,-30.021268277914,124.470406880302)) ;
#60944 = CARTESIAN_POINT('Ctrl Pts',(-18.9248025261078,-30.211130630504,124.839385850343)) ;
#60945 = CARTESIAN_POINT('Ctrl Pts',(-19.0216991485207,-30.0311415501411,
124.553872836708)) ;
#60946 = CARTESIAN_POINT('Ctrl Pts',(-19.1819439103011,-30.2212038724976,
124.902021223868)) ;
#60947 = CARTESIAN_POINT('Ctrl Pts',(-19.2274127817706,-30.0412147921347,
124.603980422162)) ;
#60948 = CARTESIAN_POINT('Ctrl Pts',(-19.4395127810917,-30.2310242040306,
124.918975069592)) ;
#60949 = CARTESIAN_POINT('Ctrl Pts',(-19.433466684621,-30.0510351236678,124.617542685309)) ;
#60950 = CARTESIAN_POINT('Ctrl Pts',(-19.7027659038404,-30.2411028652574,
124.890467615748)) ;
#60951 = CARTESIAN_POINT('Ctrl Pts',(-19.6440694852678,-30.0611137848945,
124.594736008976)) ;
#60952 = CARTESIAN_POINT('Ctrl Pts',(-19.9514865660436,-30.2509544605516,
124.818398357271)) ;
#60953 = CARTESIAN_POINT('Ctrl Pts',(-19.8430448190709,-30.0709653801888,
124.537080268754)) ;
#60954 = CARTESIAN_POINT('Ctrl Pts',(-20.1891444820223,-30.2610275957804,
124.701927251076)) ;
#60955 = CARTESIAN_POINT('Ctrl Pts',(-20.0331712033916,-30.0810385154176,
124.44390269208)) ;
#60956 = CARTESIAN_POINT('Ctrl Pts',(-20.398106604193,-30.2708700313055,124.549458419366)) ;
#60957 = CARTESIAN_POINT('Ctrl Pts',(-20.2003396262217,-30.0908809509426,
124.321927803439)) ;
#60958 = CARTESIAN_POINT('Ctrl Pts',(-20.5805436587888,-30.2808508004389,
124.361037704408)) ;
#60959 = CARTESIAN_POINT('Ctrl Pts',(-20.3462888173977,-30.100861720076,124.171191137294)) ;
#60960 = CARTESIAN_POINT('Ctrl Pts',(-20.7276313527105,-30.2908679016827,
124.142726286126)) ;
#60961 = CARTESIAN_POINT('Ctrl Pts',(-20.4639585479526,-30.1108788213199,
123.99654171188)) ;
#60962 = CARTESIAN_POINT('Ctrl Pts',(-20.8336603363903,-30.3007563492846,
123.905461600815)) ;
#60963 = CARTESIAN_POINT('Ctrl Pts',(-20.5487810297276,-30.1207672689217,
123.806730589124)) ;
#60964 = CARTESIAN_POINT('Ctrl Pts',(-20.897966874934,-30.3108120634654,123.649176787978)) ;
#60965 = CARTESIAN_POINT('Ctrl Pts',(-20.6002259506018,-30.1308229831026,
123.601702402648)) ;
#60966 = CARTESIAN_POINT('Ctrl Pts',(-20.916501105489,-30.3206872698793,123.390311340077)) ;
#60967 = CARTESIAN_POINT('Ctrl Pts',(-20.6150528932545,-30.1406981895164,
123.39461094526)) ;
#60968 = CARTESIAN_POINT('Ctrl Pts',(-20.8901135577961,-30.330682322352,123.128988240062)) ;
#60969 = CARTESIAN_POINT('Ctrl Pts',(-20.5939426563615,-30.1506932419891,
123.185552627896)) ;
#60970 = CARTESIAN_POINT('Ctrl Pts',(-20.8181453544106,-30.3407042063141,
122.87563748445)) ;
#60971 = CARTESIAN_POINT('Ctrl Pts',(-20.5363677699957,-30.1607151259512,
122.982872078019)) ;
#60972 = CARTESIAN_POINT('Ctrl Pts',(-20.7048988527743,-30.3506081788434,
122.641302484579)) ;
#60973 = CARTESIAN_POINT('Ctrl Pts',(-20.4457706757612,-30.1706190984805,
122.795404879528)) ;
#60974 = CARTESIAN_POINT('Ctrl Pts',(-20.5516896929561,-30.3605966755043,
122.428164932682)) ;
#60975 = CARTESIAN_POINT('Ctrl Pts',(-20.3232033327596,-30.1806075951414,
122.624895080866)) ;
#60976 = CARTESIAN_POINT('Ctrl Pts',(-20.3641515811051,-30.3705604727523,
122.245458339291)) ;
#60977 = CARTESIAN_POINT('Ctrl Pts',(-20.17317296099,-30.1905713923894,122.478730202668)) ;
#60978 = CARTESIAN_POINT('Ctrl Pts',(-20.1493641423966,-30.3804644960603,
122.098426355358)) ;
#60979 = CARTESIAN_POINT('Ctrl Pts',(-20.0013436095708,-30.2004754156974,
122.361105071754)) ;
#60980 = CARTESIAN_POINT('Ctrl Pts',(-19.9085262576648,-30.3905249993819,
121.989448658708)) ;
#60981 = CARTESIAN_POINT('Ctrl Pts',(-19.8086730047828,-30.2105359190191,
122.273922884312)) ;
#60982 = CARTESIAN_POINT('Ctrl Pts',(-19.6580405512922,-30.4003655345218,
121.925039834791)) ;
#60983 = CARTESIAN_POINT('Ctrl Pts',(-19.6082855766348,-30.2203764541589,
122.222396127967)) ;
#60984 = CARTESIAN_POINT('Ctrl Pts',(-19.3944577950573,-30.4104277552264,
121.904320740095)) ;
#60985 = CARTESIAN_POINT('Ctrl Pts',(-19.3974190827422,-30.2304386748635,
122.205820754266)) ;
#60986 = CARTESIAN_POINT('Ctrl Pts',(-19.1355824753204,-30.4203249090026,
121.929541442186)) ;
#60987 = CARTESIAN_POINT('Ctrl Pts',(-19.1903196245163,-30.2403358286398,
122.225997234219)) ;
#60988 = CARTESIAN_POINT('Ctrl Pts',(-18.8839449757999,-30.4302560423881,
121.998725090014)) ;
#60989 = CARTESIAN_POINT('Ctrl Pts',(-18.9890101207813,-30.2502669620252,
122.281343781079)) ;
#60990 = CARTESIAN_POINT('Ctrl Pts',(-18.6456264180008,-30.4402984175338,
122.112067478881)) ;
#60991 = CARTESIAN_POINT('Ctrl Pts',(-18.7983550586508,-30.260309337171,122.372017626633)) ;
#60992 = CARTESIAN_POINT('Ctrl Pts',(-18.4338243469554,-30.4501843553,122.26253329312)) ;
#60993 = CARTESIAN_POINT('Ctrl Pts',(-18.6289139946321,-30.2701952749371,
122.492389609933)) ;
#60994 = CARTESIAN_POINT('Ctrl Pts',(-18.2490727524169,-30.4601801982848,
122.449233759781)) ;
#60995 = CARTESIAN_POINT('Ctrl Pts',(-18.4811126123803,-30.2801911179219,
122.641749654634)) ;
#60996 = CARTESIAN_POINT('Ctrl Pts',(-18.1003554686225,-30.4701221761634,
122.664059702261)) ;
#60997 = CARTESIAN_POINT('Ctrl Pts',(-18.3621388222961,-30.2901330958005,
122.813609831262)) ;
#60998 = CARTESIAN_POINT('Ctrl Pts',(-17.9906956060769,-30.4800815506444,
122.901684237793)) ;
#60999 = CARTESIAN_POINT('Ctrl Pts',(-18.2744107413088,-30.3000924702815,
123.003708954726)) ;
#61000 = CARTESIAN_POINT('Ctrl Pts',(-17.9235701573867,-30.4900781664782,
123.15569235127)) ;
#61001 = CARTESIAN_POINT('Ctrl Pts',(-18.2207100063737,-30.3100890861153,
123.206915221358)) ;
#61002 = CARTESIAN_POINT('Ctrl Pts',(-17.9018377987369,-30.5001123850517,
123.418476175523)) ;
#61003 = CARTESIAN_POINT('Ctrl Pts',(-18.203323782619,-30.3201233046888,123.417142364106)) ;
#61004 = CARTESIAN_POINT('Ctrl Pts',(-17.9253133851979,-30.5099654522623,
123.676335153502)) ;
#61005 = CARTESIAN_POINT('Ctrl Pts',(-18.2221037452179,-30.3299763718994,
123.623428491503)) ;
#61006 = CARTESIAN_POINT('Ctrl Pts',(-17.9932051454583,-30.5199257101399,
123.929113114964)) ;
#61007 = CARTESIAN_POINT('Ctrl Pts',(-18.2764164755412,-30.339936629777,123.825650660064)) ;
#61008 = CARTESIAN_POINT('Ctrl Pts',(-18.1050124820995,-30.5299547368455,
124.167789386581)) ;
#61009 = CARTESIAN_POINT('Ctrl Pts',(-18.3658619051834,-30.3499656564826,
124.016591970179)) ;
#61010 = CARTESIAN_POINT('Ctrl Pts',(-18.2546907015098,-30.5398649438799,
124.380895877564)) ;
#61011 = CARTESIAN_POINT('Ctrl Pts',(-18.4856036341333,-30.3598758635171,
124.18707690079)) ;
#61012 = CARTESIAN_POINT('Ctrl Pts',(-18.4390851726062,-30.5497998545275,
124.565733591977)) ;
#61013 = CARTESIAN_POINT('Ctrl Pts',(-18.633118334194,-30.3698107741647,124.334947200933)) ;
#61014 = CARTESIAN_POINT('Ctrl Pts',(-18.6551854058701,-30.5598409847068,
124.71713937099)) ;
#61015 = CARTESIAN_POINT('Ctrl Pts',(-18.805998270169,-30.3798519043439,124.456072442656)) ;
#61016 = CARTESIAN_POINT('Ctrl Pts',(-18.8905691522215,-30.5697281250767,
124.827187732175)) ;
#61017 = CARTESIAN_POINT('Ctrl Pts',(-18.994304219969,-30.3897390447139,124.544111408934)) ;
#61018 = CARTESIAN_POINT('Ctrl Pts',(-19.1440074490238,-30.5797204026127,
124.895826199179)) ;
#61019 = CARTESIAN_POINT('Ctrl Pts',(-19.1970544909255,-30.3997313222498,
124.599022913111)) ;
#61020 = CARTESIAN_POINT('Ctrl Pts',(-19.4044083048242,-30.589668945881,124.919242868932)) ;
#61021 = CARTESIAN_POINT('Ctrl Pts',(-19.405374674023,-30.4096798655181,124.61775698852)) ;
#61022 = CARTESIAN_POINT('Ctrl Pts',(-19.6646066985077,-30.5996056206982,
124.897490650973)) ;
#61023 = CARTESIAN_POINT('Ctrl Pts',(-19.6135329527055,-30.4196165403353,
124.600356125457)) ;
#61024 = CARTESIAN_POINT('Ctrl Pts',(-19.9183885696594,-30.6095890416346,
124.830870140857)) ;
#61025 = CARTESIAN_POINT('Ctrl Pts',(-19.816558494324,-30.4295999612717,124.547060681517)) ;
#61026 = CARTESIAN_POINT('Ctrl Pts',(-20.1579384638186,-30.6196313568238,
124.720177686834)) ;
#61027 = CARTESIAN_POINT('Ctrl Pts',(-20.0081988873676,-30.4396422764609,
124.458507428981)) ;
#61028 = CARTESIAN_POINT('Ctrl Pts',(-20.3705238609549,-30.629471674263,124.572936951925)) ;
#61029 = CARTESIAN_POINT('Ctrl Pts',(-20.1782668479969,-30.4494825939001,
124.340716237617)) ;
#61030 = CARTESIAN_POINT('Ctrl Pts',(-20.5582851075911,-30.6395013783205,
124.387959911787)) ;
#61031 = CARTESIAN_POINT('Ctrl Pts',(-20.3284766672307,-30.4595122979576,
124.192735318187)) ;
#61032 = CARTESIAN_POINT('Ctrl Pts',(-20.7103623023063,-30.649522335043,124.172970910553)) ;
#61033 = CARTESIAN_POINT('Ctrl Pts',(-20.450139188978,-30.4695332546801,124.020744631255)) ;
#61034 = CARTESIAN_POINT('Ctrl Pts',(-20.8216762306296,-30.6593888773466,
123.938777584491)) ;
#61035 = CARTESIAN_POINT('Ctrl Pts',(-20.5391909126625,-30.4793997969837,
123.833391248542)) ;
#61036 = CARTESIAN_POINT('Ctrl Pts',(-20.8920560097773,-30.6694599772918,
123.683674797178)) ;
#61037 = CARTESIAN_POINT('Ctrl Pts',(-20.5954958516475,-30.4894708969289,
123.629309014543)) ;
#61038 = CARTESIAN_POINT('Ctrl Pts',(-20.9165006065021,-30.6793020514693,
123.426182698946)) ;
#61039 = CARTESIAN_POINT('Ctrl Pts',(-20.6150525003073,-30.4993129711065,
123.423316470327)) ;
#61040 = CARTESIAN_POINT('Ctrl Pts',(-20.8965796706122,-30.6892628460564,
123.165188338066)) ;
#61041 = CARTESIAN_POINT('Ctrl Pts',(-20.5991170611532,-30.5092737656935,
123.214521207781)) ;
#61042 = CARTESIAN_POINT('Ctrl Pts',(-20.8306367978976,-30.6993007189572,
122.909788435439)) ;
#61043 = CARTESIAN_POINT('Ctrl Pts',(-20.5463638720667,-30.5193116385943,
123.010200889343)) ;
#61044 = CARTESIAN_POINT('Ctrl Pts',(-20.7235512011237,-30.7091750045013,
122.673393853135)) ;
#61045 = CARTESIAN_POINT('Ctrl Pts',(-20.4606968923866,-30.5291859241384,
122.821085433644)) ;
#61046 = CARTESIAN_POINT('Ctrl Pts',(-20.5741723489282,-30.7192447549152,
122.45500866596)) ;
#61047 = CARTESIAN_POINT('Ctrl Pts',(-20.3411947055965,-30.5392556745523,
122.646376333744)) ;
#61048 = CARTESIAN_POINT('Ctrl Pts',(-20.3935486500737,-30.7290780394499,
122.270181067719)) ;
#61049 = CARTESIAN_POINT('Ctrl Pts',(-20.1966973937778,-30.549088959087,122.498514076006)) ;
#61050 = CARTESIAN_POINT('Ctrl Pts',(-20.1798297267143,-30.7391083802499,
122.115914599699)) ;
#61051 = CARTESIAN_POINT('Ctrl Pts',(-20.0257230530562,-30.559119299887,122.375099677665)) ;
#61052 = CARTESIAN_POINT('Ctrl Pts',(-19.9421798972545,-30.7491403042495,
122.001770363478)) ;
#61053 = CARTESIAN_POINT('Ctrl Pts',(-19.8356036909516,-30.5691512238866,
122.28378308955)) ;
#61054 = CARTESIAN_POINT('Ctrl Pts',(-19.6936420289257,-30.7589688391854,
121.931532551847)) ;
#61055 = CARTESIAN_POINT('Ctrl Pts',(-19.6367747626622,-30.5789797588226,
122.227591754788)) ;
#61056 = CARTESIAN_POINT('Ctrl Pts',(-19.4324272173847,-30.7689626169501,
121.904361062443)) ;
#61057 = CARTESIAN_POINT('Ctrl Pts',(-19.4278031940052,-30.5889735365872,
122.205853025448)) ;
#61058 = CARTESIAN_POINT('Ctrl Pts',(-19.1696001927807,-30.7789903274356,
121.923539411999)) ;
#61059 = CARTESIAN_POINT('Ctrl Pts',(-19.2175414369296,-30.5990012470728,
122.221194254643)) ;
#61060 = CARTESIAN_POINT('Ctrl Pts',(-18.9175710994844,-30.7888787382696,
121.986850390428)) ;
#61061 = CARTESIAN_POINT('Ctrl Pts',(-19.0159184367103,-30.6088896579067,
122.271841400405)) ;
#61062 = CARTESIAN_POINT('Ctrl Pts',(-18.6780751168425,-30.7988555888051,
122.09348195838)) ;
#61063 = CARTESIAN_POINT('Ctrl Pts',(-18.8243211846636,-30.6188665084423,
122.357145104466)) ;
#61064 = CARTESIAN_POINT('Ctrl Pts',(-18.4603462228554,-30.8088473853556,
122.240311680779)) ;
#61065 = CARTESIAN_POINT('Ctrl Pts',(-18.6501372714632,-30.6288583049927,
122.474607479311)) ;
#61066 = CARTESIAN_POINT('Ctrl Pts',(-18.2708493730239,-30.8188833914493,
122.42371347671)) ;
#61067 = CARTESIAN_POINT('Ctrl Pts',(-18.4985386630892,-30.6388943110864,
122.621327853477)) ;
#61068 = CARTESIAN_POINT('Ctrl Pts',(-18.1185854663055,-30.8287341257121,
122.633088418445)) ;
#61069 = CARTESIAN_POINT('Ctrl Pts',(-18.376726707459,-30.6487450453492,122.788826190101)) ;
#61070 = CARTESIAN_POINT('Ctrl Pts',(-18.0029869058182,-30.8387253842403,
122.868789450594)) ;
#61071 = CARTESIAN_POINT('Ctrl Pts',(-18.2842463850415,-30.6587363038774,
122.97738614376)) ;
#61072 = CARTESIAN_POINT('Ctrl Pts',(-17.9304364001845,-30.8486432791435,
123.119155041273)) ;
#61073 = CARTESIAN_POINT('Ctrl Pts',(-18.2262044469805,-30.6686541987806,
123.177677695621)) ;
#61074 = CARTESIAN_POINT('Ctrl Pts',(-17.9020877614499,-30.8586714208065,
123.3811332833)) ;
#61075 = CARTESIAN_POINT('Ctrl Pts',(-18.2035238003672,-30.6786823404437,
123.387260129306)) ;
#61076 = CARTESIAN_POINT('Ctrl Pts',(-17.9193001864898,-30.8685565889224,
123.640341140622)) ;
#61077 = CARTESIAN_POINT('Ctrl Pts',(-18.2172919455385,-30.6885675085595,
123.594625944928)) ;
#61078 = CARTESIAN_POINT('Ctrl Pts',(-17.9812908655851,-30.8785459524284,
123.895432047551)) ;
#61079 = CARTESIAN_POINT('Ctrl Pts',(-18.2668826491316,-30.6985568720655,
123.798698988406)) ;
#61080 = CARTESIAN_POINT('Ctrl Pts',(-18.0876859531419,-30.8885870874385,
124.136901868337)) ;
#61081 = CARTESIAN_POINT('Ctrl Pts',(-18.3519971252596,-30.7085980070756,
123.991875626918)) ;
#61082 = CARTESIAN_POINT('Ctrl Pts',(-18.2309896742768,-30.8984197556265,
124.35190954771)) ;
#61083 = CARTESIAN_POINT('Ctrl Pts',(-18.4666381458969,-30.7184306752636,
124.163882156588)) ;
#61084 = CARTESIAN_POINT('Ctrl Pts',(-18.4118327452605,-30.908413658581,124.542354351649)) ;
#61085 = CARTESIAN_POINT('Ctrl Pts',(-18.6113111190892,-30.7284245782181,
124.316239274634)) ;
#61086 = CARTESIAN_POINT('Ctrl Pts',(-18.6240784848063,-30.9184429436655,
124.698611210536)) ;
#61087 = CARTESIAN_POINT('Ctrl Pts',(-18.78110661491,-30.7384538633026,124.441246278568)) ;
#61088 = CARTESIAN_POINT('Ctrl Pts',(-18.856433654806,-30.9283184721074,124.814232093926)) ;
#61089 = CARTESIAN_POINT('Ctrl Pts',(-18.96698940901,-30.7483293917445,124.533744474627)) ;
#61090 = CARTESIAN_POINT('Ctrl Pts',(-19.1083519713591,-30.9383187547235,
124.888948210804)) ;
#61091 = CARTESIAN_POINT('Ctrl Pts',(-19.168523414082,-30.7583296743606,124.593519235513)) ;
#61092 = CARTESIAN_POINT('Ctrl Pts',(-19.3671515658204,-30.9482307707805,
124.918740815708)) ;
#61093 = CARTESIAN_POINT('Ctrl Pts',(-19.3755624914892,-30.7682416904176,
124.617355261869)) ;
#61094 = CARTESIAN_POINT('Ctrl Pts',(-19.6305583756846,-30.9582728461195,
124.903010863025)) ;
#61095 = CARTESIAN_POINT('Ctrl Pts',(-19.5862881163539,-30.7782837657566,
124.604773299001)) ;
#61096 = CARTESIAN_POINT('Ctrl Pts',(-19.8836271403426,-30.9681726787756,
124.842636496997)) ;
#61097 = CARTESIAN_POINT('Ctrl Pts',(-19.7887432076105,-30.7881835984127,
124.55647584906)) ;
#61098 = CARTESIAN_POINT('Ctrl Pts',(-20.1248202353029,-30.9781650793536,
124.738811837685)) ;
#61099 = CARTESIAN_POINT('Ctrl Pts',(-19.9816984157365,-30.7981759989908,
124.473418063959)) ;
#61100 = CARTESIAN_POINT('Ctrl Pts',(-20.3449819506173,-30.988199101113,124.593690835872)) ;
#61101 = CARTESIAN_POINT('Ctrl Pts',(-20.157828908641,-30.8082100207501,124.357322942106)) ;
#61102 = CARTESIAN_POINT('Ctrl Pts',(-20.5335886314549,-30.9980637119542,
124.415853378407)) ;
#61103 = CARTESIAN_POINT('Ctrl Pts',(-20.3087153229984,-30.8180746315913,
124.215054797051)) ;
#61104 = CARTESIAN_POINT('Ctrl Pts',(-20.6909778265813,-31.0080561114154,
124.205652827145)) ;
#61105 = CARTESIAN_POINT('Ctrl Pts',(-20.4346283289395,-30.8280670310525,
124.046895699291)) ;
#61106 = CARTESIAN_POINT('Ctrl Pts',(-20.8094832862645,-31.0180880647483,
123.970160489407)) ;
#61107 = CARTESIAN_POINT('Ctrl Pts',(-20.5294345476933,-30.8380989843854,
123.85850276039)) ;
#61108 = CARTESIAN_POINT('Ctrl Pts',(-20.8844320812118,-31.0279544236899,
123.721940205726)) ;
#61109 = CARTESIAN_POINT('Ctrl Pts',(-20.5893954864046,-30.8479653433271,
123.659927538539)) ;
#61110 = CARTESIAN_POINT('Ctrl Pts',(-20.9159397608911,-31.0379418991757,
123.461410041658)) ;
#61111 = CARTESIAN_POINT('Ctrl Pts',(-20.6146037560401,-30.8579528188129,
123.451503763144)) ;
#61112 = CARTESIAN_POINT('Ctrl Pts',(-20.9019287886433,-31.0478868053642,
123.200405236579)) ;
#61113 = CARTESIAN_POINT('Ctrl Pts',(-20.6033971453962,-30.8678977250013,
123.242699989987)) ;
#61114 = CARTESIAN_POINT('Ctrl Pts',(-20.8420850390457,-31.0579317700244,
122.943333258433)) ;
#61115 = CARTESIAN_POINT('Ctrl Pts',(-20.5555242372743,-30.8779426896616,
123.037041905058)) ;
#61116 = CARTESIAN_POINT('Ctrl Pts',(-20.7406003647243,-31.0677935769293,
122.704848430439)) ;
#61117 = CARTESIAN_POINT('Ctrl Pts',(-20.4743386257341,-30.8878044965664,
122.846253507543)) ;
#61118 = CARTESIAN_POINT('Ctrl Pts',(-20.597822144092,-31.0777862492351,122.484491140274)) ;
#61119 = CARTESIAN_POINT('Ctrl Pts',(-20.3601179413071,-30.8977971688722,
122.669966539594)) ;
#61120 = CARTESIAN_POINT('Ctrl Pts',(-20.4200444703197,-31.0877149201804,
122.293491951008)) ;
#61121 = CARTESIAN_POINT('Ctrl Pts',(-20.2178975346058,-30.9077258398175,
122.517165820862)) ;
#61122 = CARTESIAN_POINT('Ctrl Pts',(-20.2115893827837,-31.0976674624057,
122.135563380117)) ;
#61123 = CARTESIAN_POINT('Ctrl Pts',(-20.0511349097933,-30.9176783820428,
122.390821266279)) ;
#61124 = CARTESIAN_POINT('Ctrl Pts',(-19.9777608298293,-31.1076688184016,
122.015498299379)) ;
#61125 = CARTESIAN_POINT('Ctrl Pts',(-19.864073138811,-30.9276797380387,122.29476724589)) ;
#61126 = CARTESIAN_POINT('Ctrl Pts',(-19.7258837090503,-31.1176974306763,
121.93800176093)) ;
#61127 = CARTESIAN_POINT('Ctrl Pts',(-19.6625721285863,-30.9377083503134,
122.2327679101)) ;
#61128 = CARTESIAN_POINT('Ctrl Pts',(-19.468678402315,-31.1275617652258,121.905569609794)) ;
#61129 = CARTESIAN_POINT('Ctrl Pts',(-19.4568083670694,-30.9475726848629,
122.206820002847)) ;
#61130 = CARTESIAN_POINT('Ctrl Pts',(-19.2064222623212,-31.1375540893024,
121.918044378445)) ;
#61131 = CARTESIAN_POINT('Ctrl Pts',(-19.2470034110608,-30.9575650089395,
122.21679756988)) ;
#61132 = CARTESIAN_POINT('Ctrl Pts',(-18.9518724580088,-31.1474815816683,
121.975353810798)) ;
#61133 = CARTESIAN_POINT('Ctrl Pts',(-19.043363176175,-30.9674925013054,122.262642901527)) ;
#61134 = CARTESIAN_POINT('Ctrl Pts',(-18.7087875925179,-31.1575089402191,
122.076985697164)) ;
#61135 = CARTESIAN_POINT('Ctrl Pts',(-18.8488944626726,-30.9775198598562,
122.343946315082)) ;
#61136 = CARTESIAN_POINT('Ctrl Pts',(-18.4899494031481,-31.1673953582702,
122.217086576)) ;
#61137 = CARTESIAN_POINT('Ctrl Pts',(-18.6738227767691,-30.9874062779074,
122.456025072437)) ;
#61138 = CARTESIAN_POINT('Ctrl Pts',(-18.2959218218459,-31.1774270930056,
122.395489361766)) ;
#61139 = CARTESIAN_POINT('Ctrl Pts',(-18.5185992246313,-30.9974380126427,
122.59874560302)) ;
#61140 = CARTESIAN_POINT('Ctrl Pts',(-18.1379570317836,-31.1873086742489,
122.601654224087)) ;
#61141 = CARTESIAN_POINT('Ctrl Pts',(-18.3922256360828,-31.007319593886,122.763676083483)) ;
#61142 = CARTESIAN_POINT('Ctrl Pts',(-18.0159864387997,-31.1973706522812,
122.836214609579)) ;
#61143 = CARTESIAN_POINT('Ctrl Pts',(-18.2946471919646,-31.0173815719183,
122.951323289987)) ;
#61144 = CARTESIAN_POINT('Ctrl Pts',(-17.9380997062694,-31.2072277306429,
123.083299705092)) ;
#61145 = CARTESIAN_POINT('Ctrl Pts',(-18.2323356602816,-31.02723865028,123.148990682481)) ;
#61146 = CARTESIAN_POINT('Ctrl Pts',(-17.9033134792368,-31.2172223037489,
123.343589981846)) ;
#61147 = CARTESIAN_POINT('Ctrl Pts',(-18.204504458958,-31.037233223386,123.357222569661)) ;
#61148 = CARTESIAN_POINT('Ctrl Pts',(-17.9140838363557,-31.2271481000365,
123.604243273479)) ;
#61149 = CARTESIAN_POINT('Ctrl Pts',(-18.2131185010766,-31.0471590196736,
123.565745298409)) ;
#61150 = CARTESIAN_POINT('Ctrl Pts',(-17.9704288396952,-31.2371734672062,
123.861581949243)) ;
#61151 = CARTESIAN_POINT('Ctrl Pts',(-18.2581923330531,-31.0571843868434,
123.77161667508)) ;
#61152 = CARTESIAN_POINT('Ctrl Pts',(-18.0692181290173,-31.2470695468601,
124.102157307068)) ;
#61153 = CARTESIAN_POINT('Ctrl Pts',(-18.3372216027186,-31.0670804664972,
123.964077752132)) ;
#61154 = CARTESIAN_POINT('Ctrl Pts',(-18.2092168773112,-31.2570646265657,
124.324401074987)) ;
#61155 = CARTESIAN_POINT('Ctrl Pts',(-18.4492191754673,-31.0770755462028,
124.141874372406)) ;
#61156 = CARTESIAN_POINT('Ctrl Pts',(-18.3865390046239,-31.2670897143815,
124.519239586884)) ;
#61157 = CARTESIAN_POINT('Ctrl Pts',(-18.5910734554309,-31.0871006340186,
124.297744917431)) ;
#61158 = CARTESIAN_POINT('Ctrl Pts',(-18.6602990640863,-31.2802735367488,
124.731576473087)) ;
#61159 = CARTESIAN_POINT('Ctrl Pts',(-18.8100883440291,-31.1002844563859,
124.46762529973)) ;
#61160 = CARTESIAN_POINT('Ctrl Pts',(-18.9862948594309,-31.2935956548947,
124.869711357312)) ;
#61161 = CARTESIAN_POINT('Ctrl Pts',(-19.0709153826081,-31.1136065745318,
124.578138411476)) ;
#61162 = CARTESIAN_POINT('Ctrl Pts',(-19.3347015527575,-31.3069748645223,
124.917347223178)) ;
#61163 = CARTESIAN_POINT('Ctrl Pts',(-19.3495941692662,-31.1269857841594,
124.616238563571)) ;
#61164 = CARTESIAN_POINT('Ctrl Pts',(-19.5930836021212,-31.3168131017665,
124.908057132309)) ;
#61165 = CARTESIAN_POINT('Ctrl Pts',(-19.5563095018621,-31.1368240214036,
124.608810852484)) ;
#61166 = CARTESIAN_POINT('Ctrl Pts',(-19.8519437779237,-31.3268860250252,
124.852876717695)) ;
#61167 = CARTESIAN_POINT('Ctrl Pts',(-19.7633952063794,-31.1468969446624,
124.564668365869)) ;
#61168 = CARTESIAN_POINT('Ctrl Pts',(-20.0920602272961,-31.3367426664803,
124.755670606679)) ;
#61169 = CARTESIAN_POINT('Ctrl Pts',(-19.9554908730702,-31.1567535861175,
124.486904328256)) ;
#61170 = CARTESIAN_POINT('Ctrl Pts',(-20.3148623984286,-31.3467280419864,
124.617067390045)) ;
#61171 = CARTESIAN_POINT('Ctrl Pts',(-20.1337308377886,-31.1667389616235,
124.376027861451)) ;
#61172 = CARTESIAN_POINT('Ctrl Pts',(-20.5745088879433,-31.3600120734468,
124.383813942974)) ;
#61173 = CARTESIAN_POINT('Ctrl Pts',(-20.3414635227013,-31.180022993084,124.18940523939)) ;
#61174 = CARTESIAN_POINT('Ctrl Pts',(-20.8154916492515,-31.3765308653172,
124.016626072661)) ;
#61175 = CARTESIAN_POINT('Ctrl Pts',(-20.5342357532926,-31.1965417849543,
123.895695702942)) ;
#61176 = CARTESIAN_POINT('Ctrl Pts',(-20.9173070492714,-31.3933165823238,
123.582394229583)) ;
#61177 = CARTESIAN_POINT('Ctrl Pts',(-20.6157025962168,-31.2133275019609,
123.548246263072)) ;
#61178 = CARTESIAN_POINT('Ctrl Pts',(-20.906515294897,-31.4064297308328,123.237879258058)) ;
#61179 = CARTESIAN_POINT('Ctrl Pts',(-20.6070652302265,-31.2264406504699,
123.272686121829)) ;
#61180 = CARTESIAN_POINT('Ctrl Pts',(-20.8536524123544,-31.416465279913,122.97954630541)) ;
#61181 = CARTESIAN_POINT('Ctrl Pts',(-20.56477758318,-31.2364761995501,123.066008431127)) ;
#61182 = CARTESIAN_POINT('Ctrl Pts',(-20.7561932613821,-31.4264813360924,
122.73500867879)) ;
#61183 = CARTESIAN_POINT('Ctrl Pts',(-20.4868138633641,-31.2464922557295,
122.870382595949)) ;
#61184 = CARTESIAN_POINT('Ctrl Pts',(-20.5747356330736,-31.4396593719584,
122.440107128178)) ;
#61185 = CARTESIAN_POINT('Ctrl Pts',(-20.3416392942912,-31.2596702915955,
122.634448243853)) ;
#61186 = CARTESIAN_POINT('Ctrl Pts',(-20.2550642401252,-31.4562612491455,
122.135837120638)) ;
#61187 = CARTESIAN_POINT('Ctrl Pts',(-20.0859155602014,-31.2762721687826,
122.391041933051)) ;
#61188 = CARTESIAN_POINT('Ctrl Pts',(-19.7659328719897,-31.4763243937614,
121.923514400748)) ;
#61189 = CARTESIAN_POINT('Ctrl Pts',(-19.6946085896363,-31.2963353133985,
122.221176679855)) ;
#61190 = CARTESIAN_POINT('Ctrl Pts',(-19.2406043647874,-31.4961252838451,
121.89094955361)) ;
#61191 = CARTESIAN_POINT('Ctrl Pts',(-19.2743458623151,-31.3161362034822,
122.195122232715)) ;
#61192 = CARTESIAN_POINT('Ctrl Pts',(-18.731841866447,-31.5160684091238,122.039356586224)) ;
#61193 = CARTESIAN_POINT('Ctrl Pts',(-18.8673343450499,-31.3360793287609,
122.313844690629)) ;
#61194 = CARTESIAN_POINT('Ctrl Pts',(-18.3053752399663,-31.5359664542434,
122.352092202936)) ;
#61195 = CARTESIAN_POINT('Ctrl Pts',(-18.5261587181132,-31.3559773738805,
122.564031167843)) ;
#61196 = CARTESIAN_POINT('Ctrl Pts',(-18.0102664114479,-31.5558522138702,
122.790649876929)) ;
#61197 = CARTESIAN_POINT('Ctrl Pts',(-18.2900689875788,-31.3758631335073,
122.914876579139)) ;
#61198 = CARTESIAN_POINT('Ctrl Pts',(-17.8822137797069,-31.57591738905,123.30830329177)) ;
#61199 = CARTESIAN_POINT('Ctrl Pts',(-18.1876243873306,-31.3959283086872,
123.328998110787)) ;
#61200 = CARTESIAN_POINT('Ctrl Pts',(-17.9380242803409,-31.5957440321528,
123.832388879101)) ;
#61201 = CARTESIAN_POINT('Ctrl Pts',(-18.2322702877505,-31.41575495179,123.748268249303)) ;
#61202 = CARTESIAN_POINT('Ctrl Pts',(-18.1688732800194,-31.6156527416012,
124.308361931682)) ;
#61203 = CARTESIAN_POINT('Ctrl Pts',(-18.4169480416883,-31.4356636612383,
124.129048386258)) ;
#61204 = CARTESIAN_POINT('Ctrl Pts',(-18.5492284834963,-31.635604578633,124.678079899656)) ;
#61205 = CARTESIAN_POINT('Ctrl Pts',(-18.7212312265001,-31.4556154982701,
124.424824341634)) ;
#61206 = CARTESIAN_POINT('Ctrl Pts',(-19.0344540490019,-31.6556130533361,
124.895564294001)) ;
#61207 = CARTESIAN_POINT('Ctrl Pts',(-19.1094107625724,-31.4756239729733,
124.598813645085)) ;
#61208 = CARTESIAN_POINT('Ctrl Pts',(-19.5593044714881,-31.6754145120976,
124.934638681105)) ;
#61209 = CARTESIAN_POINT('Ctrl Pts',(-19.529293065133,-31.4954254317348,124.630074897987)) ;
#61210 = CARTESIAN_POINT('Ctrl Pts',(-20.0703188207212,-31.6953714003336,
124.792477849082)) ;
#61211 = CARTESIAN_POINT('Ctrl Pts',(-19.9381052599703,-31.5153823199707,
124.516346913691)) ;
#61212 = CARTESIAN_POINT('Ctrl Pts',(-20.502014723073,-31.7153552377477,124.483083841928)) ;
#61213 = CARTESIAN_POINT('Ctrl Pts',(-20.2834628020649,-31.5353661573848,
124.268832576871)) ;
#61214 = CARTESIAN_POINT('Ctrl Pts',(-20.8005129693209,-31.7351636769686,
124.049324638335)) ;
#61215 = CARTESIAN_POINT('Ctrl Pts',(-20.5222631468944,-31.5551745966057,
123.921823569577)) ;
#61216 = CARTESIAN_POINT('Ctrl Pts',(-20.9347328465596,-31.7551493863488,
123.535538119656)) ;
#61217 = CARTESIAN_POINT('Ctrl Pts',(-20.629639166781,-31.5751603059859,123.510794112745)) ;
#61218 = CARTESIAN_POINT('Ctrl Pts',(-20.8859933951321,-31.7750189093641,
123.009476827453)) ;
#61219 = CARTESIAN_POINT('Ctrl Pts',(-20.5906472054233,-31.5950298290012,
123.089943545706)) ;
#61220 = CARTESIAN_POINT('Ctrl Pts',(-20.6589290212962,-31.7950396484813,
122.528458277174)) ;
#61221 = CARTESIAN_POINT('Ctrl Pts',(-20.4089954572022,-31.6150505681184,
122.705129026127)) ;
#61222 = CARTESIAN_POINT('Ctrl Pts',(-20.2856318116993,-31.8148437134583,
122.157092625036)) ;
#61223 = CARTESIAN_POINT('Ctrl Pts',(-20.1103554752544,-31.6348546330954,
122.408035494353)) ;
#61224 = CARTESIAN_POINT('Ctrl Pts',(-19.8021889396994,-31.834905677189,121.932500294498)) ;
#61225 = CARTESIAN_POINT('Ctrl Pts',(-19.7236013288936,-31.6549165968261,
122.228362959859)) ;
#61226 = CARTESIAN_POINT('Ctrl Pts',(-19.2768672597706,-31.8547388574775,
121.88738259078)) ;
#61227 = CARTESIAN_POINT('Ctrl Pts',(-19.3033420853306,-31.6747497771146,
122.192269707988)) ;
#61228 = CARTESIAN_POINT('Ctrl Pts',(-18.7652950498868,-31.8746580548036,
122.02333953517)) ;
#61229 = CARTESIAN_POINT('Ctrl Pts',(-18.894083985732,-31.6946689744407,122.301037293139)) ;
#61230 = CARTESIAN_POINT('Ctrl Pts',(-18.3305352276764,-31.8945960799169,
122.32632493169)) ;
#61231 = CARTESIAN_POINT('Ctrl Pts',(-18.5462767220526,-31.714606999554,122.543427492195)) ;
#61232 = CARTESIAN_POINT('Ctrl Pts',(-18.0255423060835,-31.914474125973,122.757789608184)) ;
#61233 = CARTESIAN_POINT('Ctrl Pts',(-18.3022836422757,-31.7344850456101,
122.888601425754)) ;
#61234 = CARTESIAN_POINT('Ctrl Pts',(-17.8853325731395,-31.934458860261,123.270040998411)) ;
#61235 = CARTESIAN_POINT('Ctrl Pts',(-18.190118198044,-31.7544697798982,123.298403291928)) ;
#61236 = CARTESIAN_POINT('Ctrl Pts',(-17.928106557493,-31.9543696769395,123.797659471924)) ;
#61237 = CARTESIAN_POINT('Ctrl Pts',(-18.2243400264694,-31.7743805965766,
123.720498525304)) ;
#61238 = CARTESIAN_POINT('Ctrl Pts',(-18.1495333782431,-31.9743686524582,
124.280744001209)) ;
#61239 = CARTESIAN_POINT('Ctrl Pts',(-18.4014839037645,-31.7943795720954,
124.106965091444)) ;
#61240 = CARTESIAN_POINT('Ctrl Pts',(-18.5185878611027,-31.9941735731034,
124.656228575391)) ;
#61241 = CARTESIAN_POINT('Ctrl Pts',(-18.6967305737938,-31.8141844927406,
124.407351675959)) ;
#61242 = CARTESIAN_POINT('Ctrl Pts',(-18.9973682960231,-32.0141575333947,
124.885894562646)) ;
#61243 = CARTESIAN_POINT('Ctrl Pts',(-19.0797564164797,-31.8341684530318,
124.59108154804)) ;
#61244 = CARTESIAN_POINT('Ctrl Pts',(-19.5234477413584,-32.0340437371186,
124.937928873616)) ;
#61245 = CARTESIAN_POINT('Ctrl Pts',(-19.5006209678039,-31.8540546567557,
124.632705726637)) ;
#61246 = CARTESIAN_POINT('Ctrl Pts',(-20.0373301585634,-32.0539929154418,
124.807521706156)) ;
#61247 = CARTESIAN_POINT('Ctrl Pts',(-19.9117263038171,-31.8740038350789,
124.528376628622)) ;
#61248 = CARTESIAN_POINT('Ctrl Pts',(-20.4747803851015,-32.0738947146813,
124.510171457429)) ;
#61249 = CARTESIAN_POINT('Ctrl Pts',(-20.261684750146,-31.8939056343185,124.290492599356)) ;
#61250 = CARTESIAN_POINT('Ctrl Pts',(-20.7850691732621,-32.0937733197337,
124.082510674293)) ;
#61251 = CARTESIAN_POINT('Ctrl Pts',(-20.5099133229686,-31.9137842393708,
123.948363354658)) ;
#61252 = CARTESIAN_POINT('Ctrl Pts',(-20.9316880819048,-32.1138056794594,
123.570639458984)) ;
#61253 = CARTESIAN_POINT('Ctrl Pts',(-20.6272030682315,-31.9338165990965,
123.538857703905)) ;
#61254 = CARTESIAN_POINT('Ctrl Pts',(-20.9004840928426,-32.1303874054155,
123.13101387148)) ;
#61255 = CARTESIAN_POINT('Ctrl Pts',(-20.6022414356194,-31.9503983250526,
123.18718139994)) ;
#61256 = CARTESIAN_POINT('Ctrl Pts',(-20.7882628387208,-32.1435815757134,
122.802971043195)) ;
#61257 = CARTESIAN_POINT('Ctrl Pts',(-20.5124528334552,-31.9635924953505,
122.924720353763)) ;
#61258 = CARTESIAN_POINT('Ctrl Pts',(-20.6197762199004,-32.1568937538066,
122.496386987847)) ;
#61259 = CARTESIAN_POINT('Ctrl Pts',(-20.3776944292789,-31.9769046734437,
122.679499995801)) ;
#61260 = CARTESIAN_POINT('Ctrl Pts',(-20.3152084467147,-32.1734599333999,
122.178383590941)) ;
#61261 = CARTESIAN_POINT('Ctrl Pts',(-20.1339927311637,-31.9934708530371,
122.425047213569)) ;
#61262 = CARTESIAN_POINT('Ctrl Pts',(-19.9191951145893,-32.1900881282601,
121.982318684066)) ;
#61263 = CARTESIAN_POINT('Ctrl Pts',(-19.8172191413778,-32.0100990478972,
122.268225564694)) ;
#61264 = CARTESIAN_POINT('Ctrl Pts',(-19.5767420543761,-32.2033767099699,
121.913670003331)) ;
#61265 = CARTESIAN_POINT('Ctrl Pts',(-19.5432298830773,-32.023387629607,122.21329620248)) ;
#61266 = CARTESIAN_POINT('Ctrl Pts',(-19.3148866166845,-32.2133449580735,
121.907334290486)) ;
#61267 = CARTESIAN_POINT('Ctrl Pts',(-19.3337508380696,-32.0333558777106,
122.208232314246)) ;
#61268 = CARTESIAN_POINT('Ctrl Pts',(-19.0572238635977,-32.2232597143296,
121.946033185605)) ;
#61269 = CARTESIAN_POINT('Ctrl Pts',(-19.1276189170704,-32.0432706339667,
122.239193494291)) ;
#61270 = CARTESIAN_POINT('Ctrl Pts',(-18.8076409322538,-32.2332728649808,
122.029433371392)) ;
#61271 = CARTESIAN_POINT('Ctrl Pts',(-18.9279556714256,-32.0532837846179,
122.305913714308)) ;
#61272 = CARTESIAN_POINT('Ctrl Pts',(-18.5765593857256,-32.2432855721828,
122.155251712162)) ;
#61273 = CARTESIAN_POINT('Ctrl Pts',(-18.7430841787746,-32.0632964918199,
122.406578419691)) ;
#61274 = CARTESIAN_POINT('Ctrl Pts',(-18.3044914721772,-32.2565048608741,
122.371339808174)) ;
#61275 = CARTESIAN_POINT('Ctrl Pts',(-18.5254677230784,-32.0765157805112,
122.579410561966)) ;
#61276 = CARTESIAN_POINT('Ctrl Pts',(-18.0412520385267,-32.2731235418722,
122.725865756024)) ;
#61277 = CARTESIAN_POINT('Ctrl Pts',(-18.3148360322381,-32.0931344615093,
122.863088795251)) ;
#61278 = CARTESIAN_POINT('Ctrl Pts',(-17.9146049570504,-32.2896884496456,
123.147620680735)) ;
#61279 = CARTESIAN_POINT('Ctrl Pts',(-18.2135427847506,-32.1096993692827,
123.200444214174)) ;
#61280 = CARTESIAN_POINT('Ctrl Pts',(-17.904363104532,-32.3030869212564,123.499558748901)) ;
#61281 = CARTESIAN_POINT('Ctrl Pts',(-18.2053428096442,-32.1230978408936,
123.482028671522)) ;
#61282 = CARTESIAN_POINT('Ctrl Pts',(-17.9415874189062,-32.3129281767434,
123.755505137551)) ;
#61283 = CARTESIAN_POINT('Ctrl Pts',(-18.2351264004454,-32.1329390963805,
123.686778655729)) ;
#61284 = CARTESIAN_POINT('Ctrl Pts',(-18.0233154440135,-32.3229144923316,
124.004839610842)) ;
#61285 = CARTESIAN_POINT('Ctrl Pts',(-18.3005104402209,-32.1429254119687,
123.886247298971)) ;
#61286 = CARTESIAN_POINT('Ctrl Pts',(-18.1464078763225,-32.332851099918,124.2351797327)) ;
#61287 = CARTESIAN_POINT('Ctrl Pts',(-18.3989864852805,-32.1528620195551,
124.070517791497)) ;
#61288 = CARTESIAN_POINT('Ctrl Pts',(-18.3095220075479,-32.3429009672863,
124.44285330986)) ;
#61289 = CARTESIAN_POINT('Ctrl Pts',(-18.5294795023595,-32.1629118869234,
124.23665535116)) ;
#61290 = CARTESIAN_POINT('Ctrl Pts',(-18.5022200305885,-32.3527514619611,
124.615730119443)) ;
#61291 = CARTESIAN_POINT('Ctrl Pts',(-18.6836393679515,-32.1727623815982,
124.374955019593)) ;
#61292 = CARTESIAN_POINT('Ctrl Pts',(-18.7243070867326,-32.3627232623556,
124.754758703636)) ;
#61293 = CARTESIAN_POINT('Ctrl Pts',(-18.8613101252405,-32.1827341819927,
124.486175940165)) ;
#61294 = CARTESIAN_POINT('Ctrl Pts',(-18.9678327868554,-32.3727192293814,
124.853354582418)) ;
#61295 = CARTESIAN_POINT('Ctrl Pts',(-19.0561314683988,-32.1927301490186,
124.565050536217)) ;
#61296 = CARTESIAN_POINT('Ctrl Pts',(-19.225851948996,-32.3827566887626,124.90802999486)) ;
#61297 = CARTESIAN_POINT('Ctrl Pts',(-19.2625472401696,-32.2027676083997,
124.608788652274)) ;
#61298 = CARTESIAN_POINT('Ctrl Pts',(-19.4843048557896,-32.3925973896634,
124.917387851395)) ;
#61299 = CARTESIAN_POINT('Ctrl Pts',(-19.4693094439586,-32.2126083093005,
124.616272690437)) ;
#61300 = CARTESIAN_POINT('Ctrl Pts',(-19.7458762676805,-32.4026454109307,
124.881367125265)) ;
#61301 = CARTESIAN_POINT('Ctrl Pts',(-19.6785662481788,-32.2226563305678,
124.587453906341)) ;
#61302 = CARTESIAN_POINT('Ctrl Pts',(-19.9945882738061,-32.4125928040134,
124.800883482138)) ;
#61303 = CARTESIAN_POINT('Ctrl Pts',(-19.8775350535338,-32.2326037236505,
124.523064890071)) ;
#61304 = CARTESIAN_POINT('Ctrl Pts',(-20.2250646863654,-32.4225029500598,
124.679595400653)) ;
#61305 = CARTESIAN_POINT('Ctrl Pts',(-20.0619149780218,-32.2425138696969,
124.426032565424)) ;
#61306 = CARTESIAN_POINT('Ctrl Pts',(-20.4338556734805,-32.4325618639094,
124.517526668951)) ;
#61307 = CARTESIAN_POINT('Ctrl Pts',(-20.2289464252875,-32.2525727835465,
124.296375807091)) ;
#61308 = CARTESIAN_POINT('Ctrl Pts',(-20.6077963923764,-32.4424026341987,
124.326112710777)) ;
#61309 = CARTESIAN_POINT('Ctrl Pts',(-20.3680971502017,-32.2624135538358,
124.143243405943)) ;
#61310 = CARTESIAN_POINT('Ctrl Pts',(-20.749200205045,-32.4524655037773,124.102692225348)) ;
#61311 = CARTESIAN_POINT('Ctrl Pts',(-20.4812183762259,-32.2724764234145,
123.964505819681)) ;
#61312 = CARTESIAN_POINT('Ctrl Pts',(-20.8478072363101,-32.4623598269078,
123.862073047581)) ;
#61313 = CARTESIAN_POINT('Ctrl Pts',(-20.5601018691605,-32.2823707465449,
123.772009890152)) ;
#61314 = CARTESIAN_POINT('Ctrl Pts',(-20.9040808602051,-32.4723016340023,
123.606978235594)) ;
#61315 = CARTESIAN_POINT('Ctrl Pts',(-20.6051186298419,-32.2923125536394,
123.567933786065)) ;
#61316 = CARTESIAN_POINT('Ctrl Pts',(-20.9153764258059,-32.4823041449576,
123.34432986247)) ;
#61317 = CARTESIAN_POINT('Ctrl Pts',(-20.6141529513669,-32.3023150645948,
123.357815062894)) ;
#61318 = CARTESIAN_POINT('Ctrl Pts',(-20.8803820948059,-32.492338865776,123.082976331004)) ;
#61319 = CARTESIAN_POINT('Ctrl Pts',(-20.5861553344511,-32.3123497854131,
123.148732512367)) ;
#61320 = CARTESIAN_POINT('Ctrl Pts',(-20.8024460213099,-32.5021840432817,
122.836257068615)) ;
#61321 = CARTESIAN_POINT('Ctrl Pts',(-20.5238045816804,-32.3221949629189,
122.951358176035)) ;
#61322 = CARTESIAN_POINT('Ctrl Pts',(-20.6816420858177,-32.5121688036828,
122.603373026614)) ;
#61323 = CARTESIAN_POINT('Ctrl Pts',(-20.427159646758,-32.3321797233199,122.765052018463)) ;
#61324 = CARTESIAN_POINT('Ctrl Pts',(-20.523022050828,-32.5221077099992,122.395822102444)) ;
#61325 = CARTESIAN_POINT('Ctrl Pts',(-20.3002621303212,-32.3421186296363,
122.59901272905)) ;
#61326 = CARTESIAN_POINT('Ctrl Pts',(-20.3287624729339,-32.5321499376349,
122.217239391601)) ;
#61327 = CARTESIAN_POINT('Ctrl Pts',(-20.1448530337361,-32.3521608572721,
122.456148061873)) ;
#61328 = CARTESIAN_POINT('Ctrl Pts',(-20.1099755420916,-32.5420351492193,
122.077133850417)) ;
#61329 = CARTESIAN_POINT('Ctrl Pts',(-19.9698227394801,-32.3620460688564,
122.344065585937)) ;
#61330 = CARTESIAN_POINT('Ctrl Pts',(-19.8676198087422,-32.5520340794212,
121.975708802829)) ;
#61331 = CARTESIAN_POINT('Ctrl Pts',(-19.7759374551782,-32.3720449990584,
122.262927442215)) ;
#61332 = CARTESIAN_POINT('Ctrl Pts',(-19.6133877400118,-32.5619515023317,
121.918164610241)) ;
#61333 = CARTESIAN_POINT('Ctrl Pts',(-19.5725517025332,-32.3819624219688,
122.216894103057)) ;
#61334 = CARTESIAN_POINT('Ctrl Pts',(-19.3496802081964,-32.5719994344104,
121.905528177764)) ;
#61335 = CARTESIAN_POINT('Ctrl Pts',(-19.3615855024817,-32.3920103540475,
122.206786949623)) ;
#61336 = CARTESIAN_POINT('Ctrl Pts',(-19.0921154350541,-32.5818768102198,
121.938063647421)) ;
#61337 = CARTESIAN_POINT('Ctrl Pts',(-19.1555344414447,-32.4018877298569,
122.232817207828)) ;
#61338 = CARTESIAN_POINT('Ctrl Pts',(-18.8397271603765,-32.5919307033877,
122.016043063102)) ;
#61339 = CARTESIAN_POINT('Ctrl Pts',(-18.9536242958656,-32.4119416230248,
122.295202630568)) ;
#61340 = CARTESIAN_POINT('Ctrl Pts',(-18.6083164557563,-32.601824326641,122.134675324029)) ;
#61341 = CARTESIAN_POINT('Ctrl Pts',(-18.7684970311458,-32.4218352462781,
122.390109938702)) ;
#61342 = CARTESIAN_POINT('Ctrl Pts',(-18.3975309341739,-32.611886920264,122.29427674415)) ;
#61343 = CARTESIAN_POINT('Ctrl Pts',(-18.5998696580958,-32.4318978399011,
122.517792698231)) ;
#61344 = CARTESIAN_POINT('Ctrl Pts',(-18.221443696393,-32.6217294942531,122.483777412127)) ;
#61345 = CARTESIAN_POINT('Ctrl Pts',(-18.4590017343272,-32.4417404138902,
122.669394019431)) ;
#61346 = CARTESIAN_POINT('Ctrl Pts',(-18.0783294582589,-32.631720251136,122.703848805901)) ;
#61347 = CARTESIAN_POINT('Ctrl Pts',(-18.3445119383423,-32.4517311707731,
122.845452004202)) ;
#61348 = CARTESIAN_POINT('Ctrl Pts',(-17.9762694762357,-32.6416483128939,
122.943971098664)) ;
#61349 = CARTESIAN_POINT('Ctrl Pts',(-18.2628657760219,-32.4616592325311,
123.037550188827)) ;
#61350 = CARTESIAN_POINT('Ctrl Pts',(-17.9166533727178,-32.6516362887831,
123.19959535074)) ;
#61351 = CARTESIAN_POINT('Ctrl Pts',(-18.2151746225017,-32.4716472084202,
123.242049843833)) ;
#61352 = CARTESIAN_POINT('Ctrl Pts',(-17.9027006002209,-32.6616719531395,
123.462944824449)) ;
#61353 = CARTESIAN_POINT('Ctrl Pts',(-18.2040142137418,-32.4816828727767,
123.452729587914)) ;
#61354 = CARTESIAN_POINT('Ctrl Pts',(-17.9337120201421,-32.6715278915592,
123.720099296854)) ;
#61355 = CARTESIAN_POINT('Ctrl Pts',(-18.2288249953322,-32.4915388111963,
123.658452229222)) ;
#61356 = CARTESIAN_POINT('Ctrl Pts',(-18.0095431011939,-32.6815233829561,
123.971557376319)) ;
#61357 = CARTESIAN_POINT('Ctrl Pts',(-18.2894914284038,-32.5015343025932,
123.859618092693)) ;
#61358 = CARTESIAN_POINT('Ctrl Pts',(-18.1268171255641,-32.6914331879096,
124.20409067232)) ;
#61359 = CARTESIAN_POINT('Ctrl Pts',(-18.3833118888715,-32.5114441075467,
124.045643510793)) ;
#61360 = CARTESIAN_POINT('Ctrl Pts',(-18.2839493311189,-32.7014454101763,
124.41513539528)) ;
#61361 = CARTESIAN_POINT('Ctrl Pts',(-18.509018896985,-32.5214563298134,124.214478314619)) ;
#61362 = CARTESIAN_POINT('Ctrl Pts',(-18.4759885042275,-32.7114732908691,
124.595595889866)) ;
#61363 = CARTESIAN_POINT('Ctrl Pts',(-18.6626514215253,-32.5314842105063,
124.358845523371)) ;
#61364 = CARTESIAN_POINT('Ctrl Pts',(-18.6924294796709,-32.7213296868517,
124.737869480862)) ;
#61365 = CARTESIAN_POINT('Ctrl Pts',(-18.8358044087005,-32.5413406064889,
124.472662626393)) ;
#61366 = CARTESIAN_POINT('Ctrl Pts',(-18.9341360919731,-32.7313544840317,
124.842659911602)) ;
#61367 = CARTESIAN_POINT('Ctrl Pts',(-19.0291703120113,-32.5513654036688,
124.556493611938)) ;
#61368 = CARTESIAN_POINT('Ctrl Pts',(-19.1906775296738,-32.7413854140155,
124.903298738838)) ;
#61369 = CARTESIAN_POINT('Ctrl Pts',(-19.2344038900453,-32.5613963336526,
124.605003114696)) ;
#61370 = CARTESIAN_POINT('Ctrl Pts',(-19.4489157332629,-32.7512300165242,
124.918654695543)) ;
#61371 = CARTESIAN_POINT('Ctrl Pts',(-19.4409936483921,-32.5712409361613,
124.617286306339)) ;
#61372 = CARTESIAN_POINT('Ctrl Pts',(-19.7098139114528,-32.7612208677483,
124.889204775659)) ;
#61373 = CARTESIAN_POINT('Ctrl Pts',(-19.6497118803502,-32.5812317873854,
124.593725014445)) ;
#61374 = CARTESIAN_POINT('Ctrl Pts',(-19.962644010255,-32.7712587007595,124.813987935703)) ;
#61375 = CARTESIAN_POINT('Ctrl Pts',(-19.8519756339455,-32.5912696203966,
124.533550073541)) ;
#61376 = CARTESIAN_POINT('Ctrl Pts',(-20.1942400544308,-32.7811030892249,
124.698686780465)) ;
#61377 = CARTESIAN_POINT('Ctrl Pts',(-20.037251000993,-32.6011140088621,124.441308307128)) ;
#61378 = CARTESIAN_POINT('Ctrl Pts',(-20.4055373690367,-32.7910878935945,
124.543175419173)) ;
#61379 = CARTESIAN_POINT('Ctrl Pts',(-20.2062879201296,-32.6110988132316,
124.316898288086)) ;
#61380 = CARTESIAN_POINT('Ctrl Pts',(-20.5859328054878,-32.8010274130773,
124.354225945988)) ;
#61381 = CARTESIAN_POINT('Ctrl Pts',(-20.3506030458168,-32.6210383327145,
124.16573814407)) ;
#61382 = CARTESIAN_POINT('Ctrl Pts',(-20.7321570744506,-32.8110671440787,
124.134645385839)) ;
#61383 = CARTESIAN_POINT('Ctrl Pts',(-20.4675814518196,-32.6310780637158,
123.990072882451)) ;
#61384 = CARTESIAN_POINT('Ctrl Pts',(-20.8365696228075,-32.820955272325,123.896678841576)) ;
#61385 = CARTESIAN_POINT('Ctrl Pts',(-20.551110037506,-32.6409661919621,123.79969981623)) ;
#61386 = CARTESIAN_POINT('Ctrl Pts',(-20.8991776003898,-32.8309449975335,
123.641744550588)) ;
#61387 = CARTESIAN_POINT('Ctrl Pts',(-20.6011952561969,-32.6509559171706,
123.595752273945)) ;
#61388 = CARTESIAN_POINT('Ctrl Pts',(-20.9163259243604,-32.840902762235,123.380631029218)) ;
#61389 = CARTESIAN_POINT('Ctrl Pts',(-20.6149126952404,-32.6609136818721,
123.386861725222)) ;
#61390 = CARTESIAN_POINT('Ctrl Pts',(-20.8886398161754,-32.850805103647,123.121875613575)) ;
#61391 = CARTESIAN_POINT('Ctrl Pts',(-20.5927628294816,-32.6708160232841,
123.179858200967)) ;
#61392 = CARTESIAN_POINT('Ctrl Pts',(-20.8153934381563,-32.8608492993534,
122.868304834852)) ;
#61393 = CARTESIAN_POINT('Ctrl Pts',(-20.5341646599949,-32.6808602189905,
122.977001723796)) ;
#61394 = CARTESIAN_POINT('Ctrl Pts',(-20.7008271858602,-32.8707567001127,
122.634494488512)) ;
#61395 = CARTESIAN_POINT('Ctrl Pts',(-20.4425109923345,-32.6907676197498,
122.789954502378)) ;
#61396 = CARTESIAN_POINT('Ctrl Pts',(-20.5461862319884,-32.880767299987,122.421673048565)) ;
#61397 = CARTESIAN_POINT('Ctrl Pts',(-20.3187974795829,-32.7007782196241,
122.619697941561)) ;
#61398 = CARTESIAN_POINT('Ctrl Pts',(-20.356212767659,-32.8907975958992,122.238939688487)) ;
#61399 = CARTESIAN_POINT('Ctrl Pts',(-20.1668179033373,-32.7108085155363,
122.473511971535)) ;
#61400 = CARTESIAN_POINT('Ctrl Pts',(-20.1414444851523,-32.9006523755489,
122.094253937587)) ;
#61401 = CARTESIAN_POINT('Ctrl Pts',(-19.9950035629509,-32.720663295186,122.35776475964)) ;
#61402 = CARTESIAN_POINT('Ctrl Pts',(-19.9026572208542,-32.9106097037664,
121.987223818498)) ;
#61403 = CARTESIAN_POINT('Ctrl Pts',(-19.8039737675108,-32.7306206234035,
122.272141549309)) ;
#61404 = CARTESIAN_POINT('Ctrl Pts',(-19.6467435512146,-32.9206487366733,
121.923215339529)) ;
#61405 = CARTESIAN_POINT('Ctrl Pts',(-19.5992424816828,-32.7406596563104,
122.220935620064)) ;
#61406 = CARTESIAN_POINT('Ctrl Pts',(-19.3879265897767,-32.9305218485626,
121.90443588022)) ;
#61407 = CARTESIAN_POINT('Ctrl Pts',(-19.3921897535148,-32.7505327681997,
122.205912911945)) ;
#61408 = CARTESIAN_POINT('Ctrl Pts',(-19.1246518188088,-32.9405951335897,
121.93148651026)) ;
#61409 = CARTESIAN_POINT('Ctrl Pts',(-19.18156967997,-32.7606060532268,122.227554264233)) ;
#61410 = CARTESIAN_POINT('Ctrl Pts',(-18.8762664627294,-32.9504154533265,
122.001727342518)) ;
#61411 = CARTESIAN_POINT('Ctrl Pts',(-18.9828627923026,-32.7704263729636,
122.283747296942)) ;
#61412 = CARTESIAN_POINT('Ctrl Pts',(-18.6377418415184,-32.9604941187049,
122.116709479966)) ;
#61413 = CARTESIAN_POINT('Ctrl Pts',(-18.7920430490926,-32.780505038342,122.375733780278)) ;
#61414 = CARTESIAN_POINT('Ctrl Pts',(-18.4274927507125,-32.9703457091887,
122.267875972372)) ;
#61415 = CARTESIAN_POINT('Ctrl Pts',(-18.623845014994,-32.7903566288258,122.496666887985)) ;
#61416 = CARTESIAN_POINT('Ctrl Pts',(-18.2425317134073,-32.9804188595076,
122.457180219424)) ;
#61417 = CARTESIAN_POINT('Ctrl Pts',(-18.4758763682574,-32.8004297791447,
122.648110955056)) ;
#61418 = CARTESIAN_POINT('Ctrl Pts',(-18.0966577530102,-32.9902612394826,
122.670798846665)) ;
#61419 = CARTESIAN_POINT('Ctrl Pts',(-18.3591783416525,-32.8102721591198,
122.819005262211)) ;
#61420 = CARTESIAN_POINT('Ctrl Pts',(-17.987823954365,-33.0002422157257,122.90942173405)) ;
#61421 = CARTESIAN_POINT('Ctrl Pts',(-18.272111762497,-32.8202531353628,123.009903514452)) ;
#61422 = CARTESIAN_POINT('Ctrl Pts',(-17.9222646672302,-33.010258544081,123.164359426917)) ;
#61423 = CARTESIAN_POINT('Ctrl Pts',(-18.2196648233517,-32.8302694637181,
123.213853781775)) ;
#61424 = CARTESIAN_POINT('Ctrl Pts',(-17.9018796513175,-33.0201563410721,
123.423653833823)) ;
#61425 = CARTESIAN_POINT('Ctrl Pts',(-18.2033572916693,-32.8401672607093,
123.421288551752)) ;
#61426 = CARTESIAN_POINT('Ctrl Pts',(-17.9266701886612,-33.0301688978042,
123.685622214838)) ;
#61427 = CARTESIAN_POINT('Ctrl Pts',(-18.2231900289858,-32.8501798174413,
123.630863208958)) ;
#61428 = CARTESIAN_POINT('Ctrl Pts',(-17.9972994489001,-33.0402009326507,
123.939603199681)) ;
#61429 = CARTESIAN_POINT('Ctrl Pts',(-18.2796939144183,-32.8602118522878,
123.834047973384)) ;
#61430 = CARTESIAN_POINT('Ctrl Pts',(-18.1082062116321,-33.0500403334661,
124.173202825564)) ;
#61431 = CARTESIAN_POINT('Ctrl Pts',(-18.3684190950603,-32.8700512531033,
124.020926481006)) ;
#61432 = CARTESIAN_POINT('Ctrl Pts',(-18.2612411137015,-33.0601061191177,
124.388920029464)) ;
#61433 = CARTESIAN_POINT('Ctrl Pts',(-18.4908474005065,-32.8801170387548,
124.193500344908)) ;
#61434 = CARTESIAN_POINT('Ctrl Pts',(-18.4462566311347,-33.0699965742323,
124.571505176903)) ;
#61435 = CARTESIAN_POINT('Ctrl Pts',(-18.6388594192354,-32.8900074938694,
124.339567673731)) ;
#61436 = CARTESIAN_POINT('Ctrl Pts',(-18.6620084681289,-33.0799886928681,
124.721150558715)) ;
#61437 = CARTESIAN_POINT('Ctrl Pts',(-18.8114608287963,-32.8999996125052,
124.459283763965)) ;
#61438 = CARTESIAN_POINT('Ctrl Pts',(-18.8998759883332,-33.0899515196311,
124.830519144683)) ;
#61439 = CARTESIAN_POINT('Ctrl Pts',(-19.0017545994413,-32.9099624392683,
124.546778293489)) ;
#61440 = CARTESIAN_POINT('Ctrl Pts',(-19.1514920073142,-33.099855802904,124.897179406725)) ;
#61441 = CARTESIAN_POINT('Ctrl Pts',(-19.2030466974503,-32.9198667225411,
124.600106275238)) ;
#61442 = CARTESIAN_POINT('Ctrl Pts',(-19.4149143853563,-33.1099162368511,
124.919252762117)) ;
#61443 = CARTESIAN_POINT('Ctrl Pts',(-19.4137848897019,-32.9299271564882,
124.617764888164)) ;
#61444 = CARTESIAN_POINT('Ctrl Pts',(-19.6725102686655,-33.1197567895243,
124.896100987741)) ;
#61445 = CARTESIAN_POINT('Ctrl Pts',(-19.6198604236689,-32.9397677091614,
124.599243563997)) ;
#61446 = CARTESIAN_POINT('Ctrl Pts',(-19.9278232585217,-33.12981900947,124.827395120368)) ;
#61447 = CARTESIAN_POINT('Ctrl Pts',(-19.824111120568,-32.9498299291071,124.544278865711)) ;
#61448 = CARTESIAN_POINT('Ctrl Pts',(-20.1633223010035,-33.1397161487486,
124.716975844118)) ;
#61449 = CARTESIAN_POINT('Ctrl Pts',(-20.0125096303553,-32.9597270683857,
124.455943788509)) ;
#61450 = CARTESIAN_POINT('Ctrl Pts',(-20.377287539303,-33.1496473408836,124.567550900585)) ;
#61451 = CARTESIAN_POINT('Ctrl Pts',(-20.1836814780393,-32.9696582605208,
124.336404350332)) ;
#61452 = CARTESIAN_POINT('Ctrl Pts',(-20.5639122193513,-33.1596894955287,
124.380978396875)) ;
#61453 = CARTESIAN_POINT('Ctrl Pts',(-20.3329814474512,-32.9797004151658,
124.187146334296)) ;
#61454 = CARTESIAN_POINT('Ctrl Pts',(-20.7131557897439,-33.169576256548,124.168279265478)) ;
#61455 = CARTESIAN_POINT('Ctrl Pts',(-20.4523759687857,-32.9895871761851,
124.016987866727)) ;
#61456 = CARTESIAN_POINT('Ctrl Pts',(-20.8247334245669,-33.1795755582652,
123.930412036511)) ;
#61457 = CARTESIAN_POINT('Ctrl Pts',(-20.5416382872207,-32.9995864779024,
123.826694322003)) ;
#61458 = CARTESIAN_POINT('Ctrl Pts',(-20.8929652906654,-33.189496356432,123.678753341723)) ;
#61459 = CARTESIAN_POINT('Ctrl Pts',(-20.5962239379931,-33.0095072760691,
123.625368054938)) ;
#61460 = CARTESIAN_POINT('Ctrl Pts',(-20.9167545830113,-33.1995304100287,
123.416173818305)) ;
#61461 = CARTESIAN_POINT('Ctrl Pts',(-20.6152557226043,-33.0195413296658,
123.415304354511)) ;
#61462 = CARTESIAN_POINT('Ctrl Pts',(-20.894986412613,-33.2094535275951,123.156274431571)) ;
#61463 = CARTESIAN_POINT('Ctrl Pts',(-20.5978416138883,-33.0294644472322,
123.207385423938)) ;
#61464 = CARTESIAN_POINT('Ctrl Pts',(-20.8274911534907,-33.2195096510942,
122.900802570426)) ;
#61465 = CARTESIAN_POINT('Ctrl Pts',(-20.5438456966334,-33.0395205707314,
123.003007611585)) ;
#61466 = CARTESIAN_POINT('Ctrl Pts',(-20.7190711618733,-33.2293550927491,
122.665874666496)) ;
#61467 = CARTESIAN_POINT('Ctrl Pts',(-20.4571105336298,-33.0493660123862,
122.815066148446)) ;
#61468 = CARTESIAN_POINT('Ctrl Pts',(-20.5704789953411,-33.2393173938732,
122.450351068691)) ;
#61469 = CARTESIAN_POINT('Ctrl Pts',(-20.3382375063864,-33.0593283135103,
122.64264722283)) ;
#61470 = CARTESIAN_POINT('Ctrl Pts',(-20.3852299651721,-33.2493458731483,
122.262882911342)) ;
#61471 = CARTESIAN_POINT('Ctrl Pts',(-20.1900385985285,-33.0693567927855,
122.492672276396)) ;
#61472 = CARTESIAN_POINT('Ctrl Pts',(-20.172852355375,-33.259256226658,122.112168058019)) ;
#61473 = CARTESIAN_POINT('Ctrl Pts',(-20.020137396195,-33.0792671462951,122.37210035673)) ;
#61474 = CARTESIAN_POINT('Ctrl Pts',(-19.9372239609423,-33.2691910988352,
121.999716737927)) ;
#61475 = CARTESIAN_POINT('Ctrl Pts',(-19.8316354638329,-33.0892020184723,
122.282138886147)) ;
#61476 = CARTESIAN_POINT('Ctrl Pts',(-19.6829095119979,-33.2792322364209,
121.92938034057)) ;
#61477 = CARTESIAN_POINT('Ctrl Pts',(-19.6281839338197,-33.099243156058,122.225869101484)) ;
#61478 = CARTESIAN_POINT('Ctrl Pts',(-19.4242673412634,-33.2891193856355,
121.904471017884)) ;
#61479 = CARTESIAN_POINT('Ctrl Pts',(-19.4212710912674,-33.1091303052726,
122.205941031457)) ;
#61480 = CARTESIAN_POINT('Ctrl Pts',(-19.1624743734912,-33.2991116203865,
121.924625120071)) ;
#61481 = CARTESIAN_POINT('Ctrl Pts',(-19.2118368178498,-33.1191225400237,
122.222063502103)) ;
#61482 = CARTESIAN_POINT('Ctrl Pts',(-18.9092537722081,-33.3090603259495,
121.989726729914)) ;
#61483 = CARTESIAN_POINT('Ctrl Pts',(-19.009260561855,-33.1290712455866,122.274143925144)) ;
#61484 = CARTESIAN_POINT('Ctrl Pts',(-18.6713579683458,-33.3189963943732,
122.097309682469)) ;
#61485 = CARTESIAN_POINT('Ctrl Pts',(-18.8189440248541,-33.1390073140103,
122.360209282463)) ;
#61486 = CARTESIAN_POINT('Ctrl Pts',(-18.454473086345,-33.328982078589,122.245077547478)) ;
#61487 = CARTESIAN_POINT('Ctrl Pts',(-18.6454357542757,-33.1489929982261,
122.478422680742)) ;
#61488 = CARTESIAN_POINT('Ctrl Pts',(-18.2658309062383,-33.3390225051576,
122.429534786724)) ;
#61489 = CARTESIAN_POINT('Ctrl Pts',(-18.494521322166,-33.1590334247948,122.625987962609)) ;
#61490 = CARTESIAN_POINT('Ctrl Pts',(-18.1148023371037,-33.3488616186214,
122.639409270607)) ;
#61491 = CARTESIAN_POINT('Ctrl Pts',(-18.3736983361703,-33.1688725382585,
122.793886113984)) ;
#61492 = CARTESIAN_POINT('Ctrl Pts',(-17.9997997485683,-33.3588913527972,
122.876570796198)) ;
#61493 = CARTESIAN_POINT('Ctrl Pts',(-18.2816952521632,-33.1789022724343,
122.983614938204)) ;
#61494 = CARTESIAN_POINT('Ctrl Pts',(-17.9284390777351,-33.3689134523031,
123.130086625313)) ;
#61495 = CARTESIAN_POINT('Ctrl Pts',(-18.2246058215283,-33.1889243719402,
123.186427373328)) ;
#61496 = CARTESIAN_POINT('Ctrl Pts',(-17.9019339658882,-33.3787818921965,
123.388080969439)) ;
#61497 = CARTESIAN_POINT('Ctrl Pts',(-18.2034007565293,-33.1987928118337,
123.3928218386)) ;
#61498 = CARTESIAN_POINT('Ctrl Pts',(-17.9210110195692,-33.3888507568821,
123.651967424913)) ;
#61499 = CARTESIAN_POINT('Ctrl Pts',(-18.2186613497739,-33.2088616765193,
123.603931380545)) ;
#61500 = CARTESIAN_POINT('Ctrl Pts',(-17.9841657910811,-33.3986934299808,
123.902803793652)) ;
#61501 = CARTESIAN_POINT('Ctrl Pts',(-18.2691838719648,-33.2187043496179,
123.804599731666)) ;
#61502 = CARTESIAN_POINT('Ctrl Pts',(-18.0903011027806,-33.4086540641432,
124.142069897794)) ;
#61503 = CARTESIAN_POINT('Ctrl Pts',(-18.3540908116242,-33.2286649837803,
123.996012840234)) ;
#61504 = CARTESIAN_POINT('Ctrl Pts',(-18.237930321801,-33.4186919798213,124.360664605472)) ;
#61505 = CARTESIAN_POINT('Ctrl Pts',(-18.4721932743968,-33.2387028994585,
124.170889351092)) ;
#61506 = CARTESIAN_POINT('Ctrl Pts',(-18.4179673638906,-33.4285662546808,
124.547577121921)) ;
#61507 = CARTESIAN_POINT('Ctrl Pts',(-18.6162214263879,-33.2485771743179,
124.320419667571)) ;
#61508 = CARTESIAN_POINT('Ctrl Pts',(-18.6318294560732,-33.4386360050559,
124.703362669157)) ;
#61509 = CARTESIAN_POINT('Ctrl Pts',(-18.7873105748439,-33.258646924693,124.445049300282)) ;
#61510 = CARTESIAN_POINT('Ctrl Pts',(-18.8639015606415,-33.4484693004304,
124.817067545813)) ;
#61511 = CARTESIAN_POINT('Ctrl Pts',(-18.9729667662246,-33.2684802200675,
124.536013921811)) ;
#61512 = CARTESIAN_POINT('Ctrl Pts',(-19.116928618104,-33.45849959791,124.890896842844)) ;
#61513 = CARTESIAN_POINT('Ctrl Pts',(-19.1753880699453,-33.2785105175472,
124.595078779856)) ;
#61514 = CARTESIAN_POINT('Ctrl Pts',(-19.3790808832761,-33.4685316843515,
124.918905806779)) ;
#61515 = CARTESIAN_POINT('Ctrl Pts',(-19.3851098109455,-33.2885426039886,
124.617487248845)) ;
#61516 = CARTESIAN_POINT('Ctrl Pts',(-19.6367776217658,-33.4783596128404,
124.901904690569)) ;
#61517 = CARTESIAN_POINT('Ctrl Pts',(-19.5912662774906,-33.2983705324775,
124.603887836004)) ;
#61518 = CARTESIAN_POINT('Ctrl Pts',(-19.8920737335198,-33.4883556539512,
124.840047977085)) ;
#61519 = CARTESIAN_POINT('Ctrl Pts',(-19.7955034173776,-33.3083665735883,
124.554404008552)) ;
#61520 = CARTESIAN_POINT('Ctrl Pts',(-20.133272867296,-33.4983814660524,124.734019156174)) ;
#61521 = CARTESIAN_POINT('Ctrl Pts',(-19.9884633393389,-33.3183923856895,
124.469582272309)) ;
#61522 = CARTESIAN_POINT('Ctrl Pts',(-20.3495536621585,-33.5082687009472,
124.590024685913)) ;
#61523 = CARTESIAN_POINT('Ctrl Pts',(-20.1614882643308,-33.3282796205843,
124.35438833044)) ;
#61524 = CARTESIAN_POINT('Ctrl Pts',(-20.5395336848334,-33.5182455671582,
124.409369154937)) ;
#61525 = CARTESIAN_POINT('Ctrl Pts',(-20.3134732405899,-33.3382564867954,
124.209865210489)) ;
#61526 = CARTESIAN_POINT('Ctrl Pts',(-20.6955808166486,-33.52823851103,124.198113299847)) ;
#61527 = CARTESIAN_POINT('Ctrl Pts',(-20.4383121677193,-33.3482494306672,
124.040861581618)) ;
#61528 = CARTESIAN_POINT('Ctrl Pts',(-20.8127780411408,-33.5382764337014,
123.961814580438)) ;
#61529 = CARTESIAN_POINT('Ctrl Pts',(-20.5320713666861,-33.3582873533385,
123.851823229752)) ;
#61530 = CARTESIAN_POINT('Ctrl Pts',(-20.8861474399005,-33.5481248979631,
123.713603887042)) ;
#61531 = CARTESIAN_POINT('Ctrl Pts',(-20.5907682089124,-33.3681358176002,
123.653255920477)) ;
#61532 = CARTESIAN_POINT('Ctrl Pts',(-20.9161879631416,-33.5581167647071,
123.452790730188)) ;
#61533 = CARTESIAN_POINT('Ctrl Pts',(-20.6148023084948,-33.3781276843442,
123.444605723383)) ;
#61534 = CARTESIAN_POINT('Ctrl Pts',(-20.9007460375611,-33.5680344967483,
123.192586764787)) ;
#61535 = CARTESIAN_POINT('Ctrl Pts',(-20.6024505212769,-33.3880454163854,
123.236442905293)) ;
#61536 = CARTESIAN_POINT('Ctrl Pts',(-20.8397673980302,-33.5780626816436,
122.936230922789)) ;
#61537 = CARTESIAN_POINT('Ctrl Pts',(-20.5536692986984,-33.3980736012807,
123.031357801439)) ;
#61538 = CARTESIAN_POINT('Ctrl Pts',(-20.7367825952507,-33.5879478396924,
122.697737712798)) ;
#61539 = CARTESIAN_POINT('Ctrl Pts',(-20.4712833051947,-33.4079587593295,
122.840563075759)) ;
#61540 = CARTESIAN_POINT('Ctrl Pts',(-20.5929810834346,-33.5979372002341,
122.478112272451)) ;
#61541 = CARTESIAN_POINT('Ctrl Pts',(-20.3562437228865,-33.4179481198712,
122.664861808084)) ;
#61542 = CARTESIAN_POINT('Ctrl Pts',(-20.4118953447041,-33.6079783571685,
122.28618599598)) ;
#61543 = CARTESIAN_POINT('Ctrl Pts',(-20.211376372118,-33.4279892768056,122.511319516605)) ;
#61544 = CARTESIAN_POINT('Ctrl Pts',(-20.2048905331621,-33.6178109406236,
122.131549195167)) ;
#61545 = CARTESIAN_POINT('Ctrl Pts',(-20.0457742371618,-33.4378218602607,
122.387609057188)) ;
#61546 = CARTESIAN_POINT('Ctrl Pts',(-19.9707238077735,-33.6278051605856,
122.012626278824)) ;
#61547 = CARTESIAN_POINT('Ctrl Pts',(-19.8584418276612,-33.4478160802227,
122.292469026325)) ;
#61548 = CARTESIAN_POINT('Ctrl Pts',(-19.718447243707,-33.6378332623729,121.936421881646)) ;
#61549 = CARTESIAN_POINT('Ctrl Pts',(-19.6566211029712,-33.45784418201,122.231503711827)) ;
#61550 = CARTESIAN_POINT('Ctrl Pts',(-19.4606834132683,-33.647713206996,121.905273090565)) ;
#61551 = CARTESIAN_POINT('Ctrl Pts',(-19.450410798269,-33.4677241266331,122.206582828695)) ;
#61552 = CARTESIAN_POINT('Ctrl Pts',(-19.1985284829144,-33.657703533553,121.919105510909)) ;
#61553 = CARTESIAN_POINT('Ctrl Pts',(-19.2406868632452,-33.4777144531901,
122.217646778312)) ;
#61554 = CARTESIAN_POINT('Ctrl Pts',(-18.9440006247662,-33.6676444652073,
121.977957452937)) ;
#61555 = CARTESIAN_POINT('Ctrl Pts',(-19.037064402286,-33.4876553848444,122.264726340451)) ;
#61556 = CARTESIAN_POINT('Ctrl Pts',(-18.7022824096691,-33.6776315837102,
122.080244334494)) ;
#61557 = CARTESIAN_POINT('Ctrl Pts',(-18.8436891442797,-33.4976425033473,
122.346553933699)) ;
#61558 = CARTESIAN_POINT('Ctrl Pts',(-18.481234424871,-33.6876649166074,122.223936502288)) ;
#61559 = CARTESIAN_POINT('Ctrl Pts',(-18.6668496639801,-33.5076758362445,
122.461506021483)) ;
#61560 = CARTESIAN_POINT('Ctrl Pts',(-18.2913247035046,-33.6975310210521,
122.400490262853)) ;
#61561 = CARTESIAN_POINT('Ctrl Pts',(-18.514920867317,-33.5175419406893,122.602747196414)) ;
#61562 = CARTESIAN_POINT('Ctrl Pts',(-18.1317726324715,-33.7075971349325,
122.611443969021)) ;
#61563 = CARTESIAN_POINT('Ctrl Pts',(-18.3872775066212,-33.5276080545696,
122.771509020567)) ;
#61564 = CARTESIAN_POINT('Ctrl Pts',(-18.0137527035476,-33.7174531467009,
122.84201884311)) ;
#61565 = CARTESIAN_POINT('Ctrl Pts',(-18.2928599689319,-33.537464066338,122.955967544122)) ;
#61566 = CARTESIAN_POINT('Ctrl Pts',(-17.9357556600526,-33.7274478503322,
123.0928133731)) ;
#61567 = CARTESIAN_POINT('Ctrl Pts',(-18.2304603236921,-33.5474587699693,
123.156602459403)) ;
#61568 = CARTESIAN_POINT('Ctrl Pts',(-17.9029259941155,-33.7374791860571,
123.354378720209)) ;
#61569 = CARTESIAN_POINT('Ctrl Pts',(-18.2041945366287,-33.5574901056942,
123.365854477829)) ;
#61570 = CARTESIAN_POINT('Ctrl Pts',(-17.9153845549704,-33.7473457112607,
123.613370405302)) ;
#61571 = CARTESIAN_POINT('Ctrl Pts',(-18.2141592554439,-33.5673566308979,
123.573047516046)) ;
#61572 = CARTESIAN_POINT('Ctrl Pts',(-17.9729030336068,-33.7573331393065,
123.869417371802)) ;
#61573 = CARTESIAN_POINT('Ctrl Pts',(-18.2601719160976,-33.5773440589437,
123.777885465428)) ;
#61574 = CARTESIAN_POINT('Ctrl Pts',(-18.0734724275908,-33.767278068993,124.110676065872)) ;
#61575 = CARTESIAN_POINT('Ctrl Pts',(-18.3406253653803,-33.5872889886301,
123.970893079309)) ;
#61576 = CARTESIAN_POINT('Ctrl Pts',(-18.2159131529908,-33.7773229871015,
124.332886434286)) ;
#61577 = CARTESIAN_POINT('Ctrl Pts',(-18.4545761429792,-33.5973339067386,
124.14866254757)) ;
#61578 = CARTESIAN_POINT('Ctrl Pts',(-18.3913760380472,-33.7871849567154,
124.523645046325)) ;
#61579 = CARTESIAN_POINT('Ctrl Pts',(-18.5949446249841,-33.6071958763525,
124.301270653746)) ;
#61580 = CARTESIAN_POINT('Ctrl Pts',(-18.5996633149286,-33.7971770247366,
124.683493416082)) ;
#61581 = CARTESIAN_POINT('Ctrl Pts',(-18.7615730437336,-33.6171879443737,
124.429151053145)) ;
#61582 = CARTESIAN_POINT('Ctrl Pts',(-18.8311757134717,-33.8071079501112,
124.803984732102)) ;
#61583 = CARTESIAN_POINT('Ctrl Pts',(-18.9467817879391,-33.6271188697483,
124.525545974419)) ;
#61584 = CARTESIAN_POINT('Ctrl Pts',(-19.0804210325099,-33.8170585783346,
124.883010582507)) ;
#61585 = CARTESIAN_POINT('Ctrl Pts',(-19.1461772488705,-33.6370694979717,
124.588768739218)) ;
#61586 = CARTESIAN_POINT('Ctrl Pts',(-19.3409209971923,-33.8270588173937,
124.917887617961)) ;
#61587 = CARTESIAN_POINT('Ctrl Pts',(-19.3545768691479,-33.6470697370308,
124.616672564472)) ;
#61588 = CARTESIAN_POINT('Ctrl Pts',(-19.6042058083092,-33.8370872727629,
124.906594290871)) ;
#61589 = CARTESIAN_POINT('Ctrl Pts',(-19.5652047628629,-33.6570981924,124.607640132786)) ;
#61590 = CARTESIAN_POINT('Ctrl Pts',(-19.8574687091397,-33.8469533073462,
124.851055548244)) ;
#61591 = CARTESIAN_POINT('Ctrl Pts',(-19.767815408138,-33.6669642269833,124.563211299104)) ;
#61592 = CARTESIAN_POINT('Ctrl Pts',(-20.1004399415462,-33.8569456290936,
124.751536396934)) ;
#61593 = CARTESIAN_POINT('Ctrl Pts',(-19.9621930061691,-33.6769565487307,
124.483598313414)) ;
#61594 = CARTESIAN_POINT('Ctrl Pts',(-20.3211678423663,-33.8668779187706,
124.612195664073)) ;
#61595 = CARTESIAN_POINT('Ctrl Pts',(-20.1387771157398,-33.6868888384077,
124.372126818241)) ;
#61596 = CARTESIAN_POINT('Ctrl Pts',(-20.5158504184365,-33.8768795637414,
124.435627299884)) ;
#61597 = CARTESIAN_POINT('Ctrl Pts',(-20.2945221175348,-33.6968904833785,
124.230877050889)) ;
#61598 = CARTESIAN_POINT('Ctrl Pts',(-20.730134344151,-33.8901921971574,124.159073181011)) ;
#61599 = CARTESIAN_POINT('Ctrl Pts',(-20.4659641625927,-33.7102031167945,
124.009619650892)) ;
#61600 = CARTESIAN_POINT('Ctrl Pts',(-20.8667466130496,-33.903423946539,123.835025634149)) ;
#61601 = CARTESIAN_POINT('Ctrl Pts',(-20.5752544036822,-33.7234348661761,
123.750361646045)) ;
#61602 = CARTESIAN_POINT('Ctrl Pts',(-20.9147529608524,-33.916747211356,123.488209575824)) ;
#61603 = CARTESIAN_POINT('Ctrl Pts',(-20.613652637114,-33.7367581309931,123.47295053957)) ;
#61604 = CARTESIAN_POINT('Ctrl Pts',(-20.9055507233818,-33.9266229175737,
123.228839180932)) ;
#61605 = CARTESIAN_POINT('Ctrl Pts',(-20.6062950688991,-33.7466338372108,
123.265445862905)) ;
#61606 = CARTESIAN_POINT('Ctrl Pts',(-20.8511725357474,-33.9366125086737,
122.972045792766)) ;
#61607 = CARTESIAN_POINT('Ctrl Pts',(-20.5627941970681,-33.7566234283109,
123.060012946144)) ;
#61608 = CARTESIAN_POINT('Ctrl Pts',(-20.7537843023225,-33.9465396051291,
122.72999873487)) ;
#61609 = CARTESIAN_POINT('Ctrl Pts',(-20.4848858225803,-33.7665505247663,
122.866373858558)) ;
#61610 = CARTESIAN_POINT('Ctrl Pts',(-20.6145413556846,-33.9565647536337,
122.506380398598)) ;
#61611 = CARTESIAN_POINT('Ctrl Pts',(-20.3734933698443,-33.7765756732709,
122.687478231554)) ;
#61612 = CARTESIAN_POINT('Ctrl Pts',(-20.4409482369391,-33.9664604077804,
122.312726536766)) ;
#61613 = CARTESIAN_POINT('Ctrl Pts',(-20.2346204969347,-33.7864713274175,
122.532553555553)) ;
#61614 = CARTESIAN_POINT('Ctrl Pts',(-20.234405044289,-33.9764639421586,122.150141791109)) ;
#61615 = CARTESIAN_POINT('Ctrl Pts',(-20.0693873459231,-33.7964748617957,
122.402484058768)) ;
#61616 = CARTESIAN_POINT('Ctrl Pts',(-20.0031251936759,-33.9864490805987,
122.026110363717)) ;
#61617 = CARTESIAN_POINT('Ctrl Pts',(-19.8843645383385,-33.8064600002358,
122.303256977614)) ;
#61618 = CARTESIAN_POINT('Ctrl Pts',(-19.7525232072214,-33.996485005194,121.943972168262)) ;
#61619 = CARTESIAN_POINT('Ctrl Pts',(-19.6838837485256,-33.8164959248312,
122.237544337022)) ;
#61620 = CARTESIAN_POINT('Ctrl Pts',(-19.4963012262117,-34.0063362806217,
121.906976170342)) ;
#61621 = CARTESIAN_POINT('Ctrl Pts',(-19.4789062849549,-33.8263472002588,
122.207945321101)) ;
#61622 = CARTESIAN_POINT('Ctrl Pts',(-19.2338112579742,-34.0163285417831,
121.914396519971)) ;
#61623 = CARTESIAN_POINT('Ctrl Pts',(-19.2689142641197,-33.8363394614202,
122.213879435451)) ;
#61624 = CARTESIAN_POINT('Ctrl Pts',(-18.9755284714672,-34.0263684258007,
121.968182550343)) ;
#61625 = CARTESIAN_POINT('Ctrl Pts',(-19.0622876995497,-33.8463793454378,
122.256906084154)) ;
#61626 = CARTESIAN_POINT('Ctrl Pts',(-18.7352293588995,-34.0362032003031,
122.063406918151)) ;
#61627 = CARTESIAN_POINT('Ctrl Pts',(-18.8700473962123,-33.8562141199402,
122.333083630202)) ;
#61628 = CARTESIAN_POINT('Ctrl Pts',(-18.5097194264488,-34.0462795813234,
122.202115742426)) ;
#61629 = CARTESIAN_POINT('Ctrl Pts',(-18.6896381792612,-33.8662905009605,
122.444048990142)) ;
#61630 = CARTESIAN_POINT('Ctrl Pts',(-18.3161370097982,-34.056125854474,122.37385617066)) ;
#61631 = CARTESIAN_POINT('Ctrl Pts',(-18.534771813737,-33.8761367741112,122.581439034222)) ;
#61632 = CARTESIAN_POINT('Ctrl Pts',(-18.0973641720853,-34.0694903757593,
122.648596301571)) ;
#61633 = CARTESIAN_POINT('Ctrl Pts',(-18.3597451619224,-33.8895012953964,
122.801233992996)) ;
#61634 = CARTESIAN_POINT('Ctrl Pts',(-17.9574233667404,-34.0826966201937,
122.97048578706)) ;
#61635 = CARTESIAN_POINT('Ctrl Pts',(-18.2477846414627,-33.9027075398308,
123.058779978968)) ;
#61636 = CARTESIAN_POINT('Ctrl Pts',(-17.9048166903989,-34.0959615748709,
123.315069758424)) ;
#61637 = CARTESIAN_POINT('Ctrl Pts',(-18.2057090036201,-33.9159724945081,
123.334400438449)) ;
#61638 = CARTESIAN_POINT('Ctrl Pts',(-17.9110068532374,-34.1059938554226,
123.57864144408)) ;
#61639 = CARTESIAN_POINT('Ctrl Pts',(-18.2106566732483,-33.9260047750597,
123.545267055076)) ;
#61640 = CARTESIAN_POINT('Ctrl Pts',(-17.9622064695877,-34.1159025889405,
123.833943902984)) ;
#61641 = CARTESIAN_POINT('Ctrl Pts',(-18.2516149524503,-33.9359135085776,
123.749507096678)) ;
#61642 = CARTESIAN_POINT('Ctrl Pts',(-18.0566040745096,-34.125840139808,124.077443630493)) ;
#61643 = CARTESIAN_POINT('Ctrl Pts',(-18.3271318142154,-33.9458510594451,
123.944309004323)) ;
#61644 = CARTESIAN_POINT('Ctrl Pts',(-18.1932746081133,-34.1358699874019,
124.302786499422)) ;
#61645 = CARTESIAN_POINT('Ctrl Pts',(-18.4364641738599,-33.9558809070391,
124.124582034141)) ;
#61646 = CARTESIAN_POINT('Ctrl Pts',(-18.4222258929034,-34.1491051273224,
124.564718290271)) ;
#61647 = CARTESIAN_POINT('Ctrl Pts',(-18.6196353445962,-33.9691160469595,
124.334139139703)) ;
#61648 = CARTESIAN_POINT('Ctrl Pts',(-18.7900532730984,-34.1657735916935,
124.811391878838)) ;
#61649 = CARTESIAN_POINT('Ctrl Pts',(-18.9138856664441,-33.9857845113307,
124.531468849858)) ;
#61650 = CARTESIAN_POINT('Ctrl Pts',(-19.3028100031656,-34.1856446035674,
124.938674734945)) ;
#61651 = CARTESIAN_POINT('Ctrl Pts',(-19.3240782602018,-34.0056555232046,
124.633306456755)) ;
#61652 = CARTESIAN_POINT('Ctrl Pts',(-19.7442781237528,-34.2023516879504,
124.8920557054)) ;
#61653 = CARTESIAN_POINT('Ctrl Pts',(-19.6773043553831,-34.0223626075875,
124.596000463399)) ;
#61654 = CARTESIAN_POINT('Ctrl Pts',(-20.0675644892654,-34.215528969261,124.767792583565)) ;
#61655 = CARTESIAN_POINT('Ctrl Pts',(-19.935888328374,-34.0355398888981,124.496604100906)) ;
#61656 = CARTESIAN_POINT('Ctrl Pts',(-20.3669683527793,-34.2287964297751,
124.589169379259)) ;
#61657 = CARTESIAN_POINT('Ctrl Pts',(-20.1754272032707,-34.0488073494122,
124.353698951168)) ;
#61658 = CARTESIAN_POINT('Ctrl Pts',(-20.6747925423891,-34.2454103204623,
124.272577564532)) ;
#61659 = CARTESIAN_POINT('Ctrl Pts',(-20.4216796479605,-34.0654212400994,
124.100434565729)) ;
#61660 = CARTESIAN_POINT('Ctrl Pts',(-20.8925501699724,-34.2653591198897,
123.789095141607)) ;
#61661 = CARTESIAN_POINT('Ctrl Pts',(-20.5958914715679,-34.0853700395268,
123.713647108598)) ;
#61662 = CARTESIAN_POINT('Ctrl Pts',(-20.9320934628038,-34.2852802314206,
123.26117694893)) ;
#61663 = CARTESIAN_POINT('Ctrl Pts',(-20.627528243359,-34.1052911510577,123.29131282389)) ;
#61664 = CARTESIAN_POINT('Ctrl Pts',(-20.7905220573564,-34.3051466795934,
122.752407298956)) ;
#61665 = CARTESIAN_POINT('Ctrl Pts',(-20.5142733449368,-34.1251575992306,
122.884295234101)) ;
#61666 = CARTESIAN_POINT('Ctrl Pts',(-20.4811847888518,-34.3251730262106,
122.319328242786)) ;
#61667 = CARTESIAN_POINT('Ctrl Pts',(-20.2668055516656,-34.1451839458477,
122.537830873447)) ;
#61668 = CARTESIAN_POINT('Ctrl Pts',(-20.0460469289995,-34.3450350706001,
122.020279911706)) ;
#61669 = CARTESIAN_POINT('Ctrl Pts',(-19.9186955596424,-34.1650459902372,
122.298589641338)) ;
#61670 = CARTESIAN_POINT('Ctrl Pts',(-19.5332082975654,-34.3649803732812,
121.886348768634)) ;
#61671 = CARTESIAN_POINT('Ctrl Pts',(-19.5084245595147,-34.1849912929184,
122.191442818576)) ;
#61672 = CARTESIAN_POINT('Ctrl Pts',(-19.0066946739163,-34.3848756803401,
121.93543015809)) ;
#61673 = CARTESIAN_POINT('Ctrl Pts',(-19.0872124491375,-34.2048865999772,
122.230706348824)) ;
#61674 = CARTESIAN_POINT('Ctrl Pts',(-18.528179666335,-34.4047689505077,122.160351280735)) ;
#61675 = CARTESIAN_POINT('Ctrl Pts',(-18.7043988887934,-34.2247798701449,
122.410642726589)) ;
#61676 = CARTESIAN_POINT('Ctrl Pts',(-18.1538942485171,-34.4247345431882,
122.53647446393)) ;
#61677 = CARTESIAN_POINT('Ctrl Pts',(-18.404969560696,-34.2447454628253,122.711540862601)) ;
#61678 = CARTESIAN_POINT('Ctrl Pts',(-17.9310744457826,-34.444609866873,123.015467619857)) ;
#61679 = CARTESIAN_POINT('Ctrl Pts',(-18.2267125107953,-34.2646207865101,
123.094736487549)) ;
#61680 = CARTESIAN_POINT('Ctrl Pts',(-17.8843177630335,-34.464584929448,123.544333074597)) ;
#61681 = CARTESIAN_POINT('Ctrl Pts',(-18.1893069457108,-34.2845958490851,
123.517829108664)) ;
#61682 = CARTESIAN_POINT('Ctrl Pts',(-18.0214586110986,-34.4845373390791,
124.056594429955)) ;
#61683 = CARTESIAN_POINT('Ctrl Pts',(-18.2990194229785,-34.3045482587162,
123.927638867659)) ;
#61684 = CARTESIAN_POINT('Ctrl Pts',(-18.3225640751946,-34.5043733933152,
124.489356119812)) ;
#61685 = CARTESIAN_POINT('Ctrl Pts',(-18.5399052793811,-34.3243843129523,
124.27384976748)) ;
#61686 = CARTESIAN_POINT('Ctrl Pts',(-18.7560161142767,-34.5243513047327,
124.796045846229)) ;
#61687 = CARTESIAN_POINT('Ctrl Pts',(-18.8866675828867,-34.3443622243698,
124.519201026929)) ;
#61688 = CARTESIAN_POINT('Ctrl Pts',(-19.2667030759239,-34.5442693542362,
124.935377333597)) ;
#61689 = CARTESIAN_POINT('Ctrl Pts',(-19.2952182947917,-34.3642802738733,
124.630665776378)) ;
#61690 = CARTESIAN_POINT('Ctrl Pts',(-19.7932159078448,-34.5641374980043,
124.893556756045)) ;
#61691 = CARTESIAN_POINT('Ctrl Pts',(-19.7164298223103,-34.3841484176414,
124.597207716313)) ;
#61692 = CARTESIAN_POINT('Ctrl Pts',(-20.2777146690572,-34.5841883545916,
124.671918199537)) ;
#61693 = CARTESIAN_POINT('Ctrl Pts',(-20.1040278270987,-34.4041992742287,
124.419895848041)) ;
#61694 = CARTESIAN_POINT('Ctrl Pts',(-20.6529658815064,-34.6039687910475,
124.303496686845)) ;
#61695 = CARTESIAN_POINT('Ctrl Pts',(-20.4042291464414,-34.4239797106846,
124.125155886527)) ;
#61696 = CARTESIAN_POINT('Ctrl Pts',(-20.8834863290637,-34.6239988467253,
123.823760909331)) ;
#61697 = CARTESIAN_POINT('Ctrl Pts',(-20.5886433844177,-34.4440097663624,
123.74136659525)) ;
#61698 = CARTESIAN_POINT('Ctrl Pts',(-20.9351889705778,-34.6438799519001,
123.297798988631)) ;
#61699 = CARTESIAN_POINT('Ctrl Pts',(-20.6300035954088,-34.4638908715372,
123.32059580445)) ;
#61700 = CARTESIAN_POINT('Ctrl Pts',(-20.805790334357,-34.6637604142679,122.785553366895)) ;
#61701 = CARTESIAN_POINT('Ctrl Pts',(-20.5264818601808,-34.483771333905,122.910799001557)) ;
#61702 = CARTESIAN_POINT('Ctrl Pts',(-20.5076352220214,-34.6837455614122,
122.345932910046)) ;
#61703 = CARTESIAN_POINT('Ctrl Pts',(-20.2879554585398,-34.5037564810494,
122.559104093687)) ;
#61704 = CARTESIAN_POINT('Ctrl Pts',(-20.0793236955457,-34.7036361399486,
122.036027427117)) ;
#61705 = CARTESIAN_POINT('Ctrl Pts',(-19.9453039222835,-34.5236470595857,
122.311181522728)) ;
#61706 = CARTESIAN_POINT('Ctrl Pts',(-19.5711560383436,-34.723530159823,121.889965636303)) ;
#61707 = CARTESIAN_POINT('Ctrl Pts',(-19.5387682446119,-34.5435410794601,
122.1943349732)) ;
#61708 = CARTESIAN_POINT('Ctrl Pts',(-19.0429893283783,-34.7434516045494,
121.925987779891)) ;
#61709 = CARTESIAN_POINT('Ctrl Pts',(-19.1162346135711,-34.5634625241865,
122.223156059284)) ;
#61710 = CARTESIAN_POINT('Ctrl Pts',(-18.5587933443279,-34.7633497426048,
122.139065599401)) ;
#61711 = CARTESIAN_POINT('Ctrl Pts',(-18.7288788359676,-34.583360662242,122.393621850554)) ;
#61712 = CARTESIAN_POINT('Ctrl Pts',(-18.1739396124289,-34.7834204978209,
122.508326536902)) ;
#61713 = CARTESIAN_POINT('Ctrl Pts',(-18.4209985757421,-34.603431417458,122.689032837873)) ;
#61714 = CARTESIAN_POINT('Ctrl Pts',(-17.9412291317738,-34.8032060478722,
122.980030562384)) ;
#61715 = CARTESIAN_POINT('Ctrl Pts',(-18.234833032526,-34.6232169675093,123.066398644646)) ;
#61716 = CARTESIAN_POINT('Ctrl Pts',(-17.8816194222905,-34.8231891227495,
123.507694573191)) ;
#61717 = CARTESIAN_POINT('Ctrl Pts',(-18.1871490553495,-34.6432000423866,
123.488530272471)) ;
#61718 = CARTESIAN_POINT('Ctrl Pts',(-18.0060182323476,-34.8430982053954,
124.022021160858)) ;
#61719 = CARTESIAN_POINT('Ctrl Pts',(-18.2866725880628,-34.6631091250326,
123.899991117196)) ;
#61720 = CARTESIAN_POINT('Ctrl Pts',(-18.2964865246401,-34.8629567645182,
124.462795926968)) ;
#61721 = CARTESIAN_POINT('Ctrl Pts',(-18.5190486895846,-34.6829676841553,
124.252608470384)) ;
#61722 = CARTESIAN_POINT('Ctrl Pts',(-18.7241036774144,-34.8830002083569,
124.780319588221)) ;
#61723 = CARTESIAN_POINT('Ctrl Pts',(-18.8611532239642,-34.703011127994,124.506625843281)) ;
#61724 = CARTESIAN_POINT('Ctrl Pts',(-19.1443314362236,-34.8995002730861,
124.906184977463)) ;
#61725 = CARTESIAN_POINT('Ctrl Pts',(-19.1973104768277,-34.7195111927232,
124.607308957452)) ;
#61726 = CARTESIAN_POINT('Ctrl Pts',(-19.4959856145689,-34.912890012935,124.916808895163)) ;
#61727 = CARTESIAN_POINT('Ctrl Pts',(-19.4786571226114,-34.7329009325721,
124.615810467763)) ;
#61728 = CARTESIAN_POINT('Ctrl Pts',(-19.7523697501484,-34.9227469141434,
124.879642738554)) ;
#61729 = CARTESIAN_POINT('Ctrl Pts',(-19.6837596469558,-34.7427578337805,
124.586074466439)) ;
#61730 = CARTESIAN_POINT('Ctrl Pts',(-20.0018598351797,-34.9327384399899,
124.79795143579)) ;
#61731 = CARTESIAN_POINT('Ctrl Pts',(-19.8833526563097,-34.752749359627,124.520719090591)) ;
#61732 = CARTESIAN_POINT('Ctrl Pts',(-20.2319445660988,-34.9426631204409,
124.675054574799)) ;
#61733 = CARTESIAN_POINT('Ctrl Pts',(-20.0674176841992,-34.762674040078,124.4224015819)) ;
#61734 = CARTESIAN_POINT('Ctrl Pts',(-20.438971803788,-34.9526737104853,124.512809926613)) ;
#61735 = CARTESIAN_POINT('Ctrl Pts',(-20.2330436587693,-34.7726846301224,
124.292596602303)) ;
#61736 = CARTESIAN_POINT('Ctrl Pts',(-20.6720998991134,-34.9659329711889,
124.253723717875)) ;
#61737 = CARTESIAN_POINT('Ctrl Pts',(-20.4195165683706,-34.7859438908261,
124.085363349355)) ;
#61738 = CARTESIAN_POINT('Ctrl Pts',(-20.8329350805989,-34.9792840463392,
123.937545082256)) ;
#61739 = CARTESIAN_POINT('Ctrl Pts',(-20.5482036204118,-34.7992949659763,
123.832398938157)) ;
#61740 = CARTESIAN_POINT('Ctrl Pts',(-20.9051329385635,-34.992490355574,123.598017654249)) ;
#61741 = CARTESIAN_POINT('Ctrl Pts',(-20.605960739995,-34.8125012752111,123.56076258238)) ;
#61742 = CARTESIAN_POINT('Ctrl Pts',(-20.914842890768,-35.0024771891643,123.335798885094)) ;
#61743 = CARTESIAN_POINT('Ctrl Pts',(-20.6137261079857,-34.8224881088014,
123.350990280824)) ;
#61744 = CARTESIAN_POINT('Ctrl Pts',(-20.8791149640092,-35.0124299166604,
123.076657694403)) ;
#61745 = CARTESIAN_POINT('Ctrl Pts',(-20.5851416344258,-34.8324408362975,
123.143676914264)) ;
#61746 = CARTESIAN_POINT('Ctrl Pts',(-20.7979778136165,-35.022478013502,122.825409407708)) ;
#61747 = CARTESIAN_POINT('Ctrl Pts',(-20.5202297765397,-34.8424889331391,
122.942679247368)) ;
#61748 = CARTESIAN_POINT('Ctrl Pts',(-20.6772333062096,-35.0323194703738,
122.596674503416)) ;
#61749 = CARTESIAN_POINT('Ctrl Pts',(-20.4236321706692,-34.8523303900109,
122.759692291335)) ;
#61750 = CARTESIAN_POINT('Ctrl Pts',(-20.5167579761239,-35.0423057372873,
122.389083764502)) ;
#61751 = CARTESIAN_POINT('Ctrl Pts',(-20.2952501539374,-34.8623166569244,
122.593621150654)) ;
#61752 = CARTESIAN_POINT('Ctrl Pts',(-20.3236651757576,-35.0522423381877,
122.213233449278)) ;
#61753 = CARTESIAN_POINT('Ctrl Pts',(-20.1407744379203,-34.8722532578248,
122.452942601343)) ;
#61754 = CARTESIAN_POINT('Ctrl Pts',(-20.1004431975683,-35.0622922809748,
122.072138574706)) ;
#61755 = CARTESIAN_POINT('Ctrl Pts',(-19.9621956872849,-34.8823032006119,
122.340068638975)) ;
#61756 = CARTESIAN_POINT('Ctrl Pts',(-19.861002389051,-35.0721424806605,121.973740369883)) ;
#61757 = CARTESIAN_POINT('Ctrl Pts',(-19.7706422695711,-34.8921534002976,
122.261352199334)) ;
#61758 = CARTESIAN_POINT('Ctrl Pts',(-19.6051578614204,-35.0821153855926,
121.917057183094)) ;
#61759 = CARTESIAN_POINT('Ctrl Pts',(-19.5659662526582,-34.9021263052297,
122.216007866642)) ;
#61760 = CARTESIAN_POINT('Ctrl Pts',(-19.3426236375317,-35.0921137600722,
121.905710783946)) ;
#61761 = CARTESIAN_POINT('Ctrl Pts',(-19.3559388367088,-34.9121246797094,
122.206932993469)) ;
#61762 = CARTESIAN_POINT('Ctrl Pts',(-19.0816040718578,-35.1021339339422,
121.940379135869)) ;
#61763 = CARTESIAN_POINT('Ctrl Pts',(-19.1471235237251,-34.9221448535794,
122.234669903381)) ;
#61764 = CARTESIAN_POINT('Ctrl Pts',(-18.8334713868321,-35.1120349778842,
122.018687487834)) ;
#61765 = CARTESIAN_POINT('Ctrl Pts',(-18.9486181859309,-34.9320458975213,
122.297318684873)) ;
#61766 = CARTESIAN_POINT('Ctrl Pts',(-18.600476033389,-35.1220237816085,122.139585076272)) ;
#61767 = CARTESIAN_POINT('Ctrl Pts',(-18.7622230038763,-34.9420347012456,
122.394038699726)) ;
#61768 = CARTESIAN_POINT('Ctrl Pts',(-18.3926205883172,-35.1319892484403,
122.298870811014)) ;
#61769 = CARTESIAN_POINT('Ctrl Pts',(-18.5959400898762,-34.9520001680775,
122.521469007001)) ;
#61770 = CARTESIAN_POINT('Ctrl Pts',(-18.2161904041538,-35.1418928107133,
122.490230413735)) ;
#61771 = CARTESIAN_POINT('Ctrl Pts',(-18.4547977047164,-34.9619037303504,
122.674558035766)) ;
#61772 = CARTESIAN_POINT('Ctrl Pts',(-18.0736527312663,-35.1519534885913,
122.712860272288)) ;
#61773 = CARTESIAN_POINT('Ctrl Pts',(-18.3407694238614,-34.9719644082284,
122.852663144503)) ;
#61774 = CARTESIAN_POINT('Ctrl Pts',(-17.9738293172813,-35.1617937865408,
122.951450001417)) ;
#61775 = CARTESIAN_POINT('Ctrl Pts',(-18.2609128496764,-34.9818047061779,
123.043535471726)) ;
#61776 = CARTESIAN_POINT('Ctrl Pts',(-17.9153656043643,-35.1718567814502,
123.209316008984)) ;
#61777 = CARTESIAN_POINT('Ctrl Pts',(-18.2141439991331,-34.9918677010873,
123.249828796046)) ;
#61778 = CARTESIAN_POINT('Ctrl Pts',(-17.9029906881241,-35.1817510755973,
123.469061216247)) ;
#61779 = CARTESIAN_POINT('Ctrl Pts',(-18.2042462718512,-35.0017619952345,
123.457624801608)) ;
#61780 = CARTESIAN_POINT('Ctrl Pts',(-17.9353509724904,-35.1916928732942,
123.728277083016)) ;
#61781 = CARTESIAN_POINT('Ctrl Pts',(-18.230136599556,-35.0117037929313,123.664997019035)) ;
#61782 = CARTESIAN_POINT('Ctrl Pts',(-18.0126256104855,-35.2016954508233,
123.979555436209)) ;
#61783 = CARTESIAN_POINT('Ctrl Pts',(-18.2919583264141,-35.0217063704604,
123.866019011557)) ;
#61784 = CARTESIAN_POINT('Ctrl Pts',(-18.1330779756745,-35.2117299147444,
124.214117512253)) ;
#61785 = CARTESIAN_POINT('Ctrl Pts',(-18.3883221539504,-35.0317408343815,
124.053667693136)) ;
#61786 = CARTESIAN_POINT('Ctrl Pts',(-18.2891276130123,-35.2215760532655,
124.420521008391)) ;
#61787 = CARTESIAN_POINT('Ctrl Pts',(-18.5131632916011,-35.0415869729026,
124.218788844697)) ;
#61788 = CARTESIAN_POINT('Ctrl Pts',(-18.4808245709193,-35.2315572265025,
124.59951775017)) ;
#61789 = CARTESIAN_POINT('Ctrl Pts',(-18.6665221721677,-35.0515681461396,
124.361984625144)) ;
#61790 = CARTESIAN_POINT('Ctrl Pts',(-18.7001113066703,-35.2415095204597,
124.742060651056)) ;
#61791 = CARTESIAN_POINT('Ctrl Pts',(-18.8419525117809,-35.0615204400968,
124.476017085114)) ;
#61792 = CARTESIAN_POINT('Ctrl Pts',(-18.9418196622479,-35.2515083155943,
124.845159871712)) ;
#61793 = CARTESIAN_POINT('Ctrl Pts',(-19.0353199196314,-35.0715192352314,
124.558494551332)) ;
#61794 = CARTESIAN_POINT('Ctrl Pts',(-19.1988694220206,-35.2615474238551,
124.904462676824)) ;
#61795 = CARTESIAN_POINT('Ctrl Pts',(-19.2409602470283,-35.0815583434922,
124.605934759269)) ;
#61796 = CARTESIAN_POINT('Ctrl Pts',(-19.4566932433114,-35.2713723652943,
124.918494235156)) ;
#61797 = CARTESIAN_POINT('Ctrl Pts',(-19.4472187973089,-35.0913832849314,
124.617157941595)) ;
#61798 = CARTESIAN_POINT('Ctrl Pts',(-19.7190507496054,-35.2814270523687,
124.887257605285)) ;
#61799 = CARTESIAN_POINT('Ctrl Pts',(-19.6571046535086,-35.1014379720058,
124.592166657345)) ;
#61800 = CARTESIAN_POINT('Ctrl Pts',(-19.9690783925131,-35.2913698573088,
124.811356103697)) ;
#61801 = CARTESIAN_POINT('Ctrl Pts',(-19.8571259192075,-35.1113807769459,
124.531443580824)) ;
#61802 = CARTESIAN_POINT('Ctrl Pts',(-20.2015729912878,-35.3012736433053,
124.694371844272)) ;
#61803 = CARTESIAN_POINT('Ctrl Pts',(-20.0431203471688,-35.1212845629424,
124.437854636998)) ;
#61804 = CARTESIAN_POINT('Ctrl Pts',(-20.4131178490129,-35.3113204598701,
124.536438012286)) ;
#61805 = CARTESIAN_POINT('Ctrl Pts',(-20.2123551289518,-35.1313313795072,
124.311505953245)) ;
#61806 = CARTESIAN_POINT('Ctrl Pts',(-20.5915179796175,-35.3212159793488,
124.347180770753)) ;
#61807 = CARTESIAN_POINT('Ctrl Pts',(-20.3550735141645,-35.1412268989859,
124.160099180785)) ;
#61808 = CARTESIAN_POINT('Ctrl Pts',(-20.7367072779153,-35.3312780646732,
124.126231712253)) ;
#61809 = CARTESIAN_POINT('Ctrl Pts',(-20.4712234236235,-35.1512889843104,
123.983338754042)) ;
#61810 = CARTESIAN_POINT('Ctrl Pts',(-20.8392082177454,-35.3411207756312,
123.888720096976)) ;
#61811 = CARTESIAN_POINT('Ctrl Pts',(-20.5532221538063,-35.1611316952683,
123.793329345071)) ;
#61812 = CARTESIAN_POINT('Ctrl Pts',(-20.9004009016988,-35.3511114929372,
123.633439183849)) ;
#61813 = CARTESIAN_POINT('Ctrl Pts',(-20.6021745071673,-35.1711224125743,
123.589104328749)) ;
#61814 = CARTESIAN_POINT('Ctrl Pts',(-20.9161968438839,-35.3610395760338,
123.373005745111)) ;
#61815 = CARTESIAN_POINT('Ctrl Pts',(-20.6148094255355,-35.1810504956709,
123.38075785787)) ;
#61816 = CARTESIAN_POINT('Ctrl Pts',(-20.8868090725257,-35.3710275061455,
123.112172972253)) ;
#61817 = CARTESIAN_POINT('Ctrl Pts',(-20.5912974941036,-35.1910384257827,
123.172091979698)) ;
#61818 = CARTESIAN_POINT('Ctrl Pts',(-20.8118024544747,-35.3810633322728,
122.859341843818)) ;
#61819 = CARTESIAN_POINT('Ctrl Pts',(-20.5312904395145,-35.20107425191,122.969827526995)) ;
#61820 = CARTESIAN_POINT('Ctrl Pts',(-20.6965136129544,-35.3909186693864,
122.627413231324)) ;
#61821 = CARTESIAN_POINT('Ctrl Pts',(-20.4390581291398,-35.2109295890236,
122.784286070346)) ;
#61822 = CARTESIAN_POINT('Ctrl Pts',(-20.5408432692029,-35.4009164042366,
122.415802979033)) ;
#61823 = CARTESIAN_POINT('Ctrl Pts',(-20.3145205770678,-35.2209273238737,
122.614998959278)) ;
#61824 = CARTESIAN_POINT('Ctrl Pts',(-20.3525343320192,-35.4108243082211,
122.235974665639)) ;
#61825 = CARTESIAN_POINT('Ctrl Pts',(-20.1638726660472,-35.2308352278582,
122.471137872087)) ;
#61826 = CARTESIAN_POINT('Ctrl Pts',(-20.1338538119606,-35.4208353827695,
122.089706748638)) ;
#61827 = CARTESIAN_POINT('Ctrl Pts',(-19.9889274042967,-35.2408463024066,
122.354124872877)) ;
#61828 = CARTESIAN_POINT('Ctrl Pts',(-19.8924829761476,-35.4308632383051,
121.983948431218)) ;
#61829 = CARTESIAN_POINT('Ctrl Pts',(-19.7958300154897,-35.2508741579423,
122.26951973446)) ;
#61830 = CARTESIAN_POINT('Ctrl Pts',(-19.6408783355081,-35.4407208322104,
121.922312589415)) ;
#61831 = CARTESIAN_POINT('Ctrl Pts',(-19.5945467001667,-35.2607317518475,
122.220212798044)) ;
#61832 = CARTESIAN_POINT('Ctrl Pts',(-19.3779878358377,-35.4507475190485,
121.904471410872)) ;
#61833 = CARTESIAN_POINT('Ctrl Pts',(-19.3842341773709,-35.2707584386856,
122.205941341526)) ;
#61834 = CARTESIAN_POINT('Ctrl Pts',(-19.116007159778,-35.4607761882022,121.933207053321)) ;
#61835 = CARTESIAN_POINT('Ctrl Pts',(-19.1746497551832,-35.2807871078393,
122.228931467457)) ;
#61836 = CARTESIAN_POINT('Ctrl Pts',(-18.8675097602884,-35.4706213964836,
122.005176454278)) ;
#61837 = CARTESIAN_POINT('Ctrl Pts',(-18.975853120482,-35.2906323161207,122.286508201954)) ;
#61838 = CARTESIAN_POINT('Ctrl Pts',(-18.6315240046396,-35.4806120854467,
122.120258716243)) ;
#61839 = CARTESIAN_POINT('Ctrl Pts',(-18.787065262531,-35.3006230050839,122.3785751853)) ;
#61840 = CARTESIAN_POINT('Ctrl Pts',(-18.4184551336644,-35.490649961729,122.275766762544)) ;
#61841 = CARTESIAN_POINT('Ctrl Pts',(-18.6166109641243,-35.3106608813661,
122.502982897611)) ;
#61842 = CARTESIAN_POINT('Ctrl Pts',(-18.2388143581137,-35.5004943393712,
122.461939201288)) ;
#61843 = CARTESIAN_POINT('Ctrl Pts',(-18.472900009195,-35.3205052590084,122.651921150758)) ;
#61844 = CARTESIAN_POINT('Ctrl Pts',(-18.0917605510307,-35.5104791437627,
122.679207506938)) ;
#61845 = CARTESIAN_POINT('Ctrl Pts',(-18.3552581535845,-35.3304900633998,
122.825736359485)) ;
#61846 = CARTESIAN_POINT('Ctrl Pts',(-17.9850190706446,-35.5204186739812,
122.917641507292)) ;
#61847 = CARTESIAN_POINT('Ctrl Pts',(-18.2698663114521,-35.3404295936183,
123.016483683079)) ;
#61848 = CARTESIAN_POINT('Ctrl Pts',(-17.9207300902949,-35.5304583620181,
123.173500108613)) ;
#61849 = CARTESIAN_POINT('Ctrl Pts',(-18.2184363504254,-35.3504692816552,
123.221170992911)) ;
#61850 = CARTESIAN_POINT('Ctrl Pts',(-17.9019975600655,-35.5403466513864,
123.43269321979)) ;
#61851 = CARTESIAN_POINT('Ctrl Pts',(-18.2034516388014,-35.3603575710235,
123.428524836043)) ;
#61852 = CARTESIAN_POINT('Ctrl Pts',(-17.928329013415,-35.5503357750712,123.693863790479)) ;
#61853 = CARTESIAN_POINT('Ctrl Pts',(-18.2245179343512,-35.3703466947083,
123.637461006412)) ;
#61854 = CARTESIAN_POINT('Ctrl Pts',(-17.9995984433313,-35.5602957847458,
123.945708092075)) ;
#61855 = CARTESIAN_POINT('Ctrl Pts',(-18.2815345383664,-35.3803067043829,
123.83893578616)) ;
#61856 = CARTESIAN_POINT('Ctrl Pts',(-18.1122794989603,-35.57019621445,124.180223126085)) ;
#61857 = CARTESIAN_POINT('Ctrl Pts',(-18.3716800348444,-35.3902071340872,
124.026546724073)) ;
#61858 = CARTESIAN_POINT('Ctrl Pts',(-18.2661525939819,-35.5802392958568,
124.394633262475)) ;
#61859 = CARTESIAN_POINT('Ctrl Pts',(-18.4947794676731,-35.4002502154939,
124.198074338897)) ;
#61860 = CARTESIAN_POINT('Ctrl Pts',(-18.4523813317248,-35.5901466897644,
124.576598857662)) ;
#61861 = CARTESIAN_POINT('Ctrl Pts',(-18.6437627318548,-35.4101576094016,
124.343645597368)) ;
#61862 = CARTESIAN_POINT('Ctrl Pts',(-18.6693558214365,-35.6001584207536,
124.725406064343)) ;
#61863 = CARTESIAN_POINT('Ctrl Pts',(-18.817342832175,-35.4201693403907,124.462690554545)) ;
#61864 = CARTESIAN_POINT('Ctrl Pts',(-18.9095840015776,-35.6101906384684,
124.834028669225)) ;
#61865 = CARTESIAN_POINT('Ctrl Pts',(-19.0095258944054,-35.4302015581055,
124.549587692303)) ;
#61866 = CARTESIAN_POINT('Ctrl Pts',(-19.1603393482666,-35.6200431477146,
124.898453661677)) ;
#61867 = CARTESIAN_POINT('Ctrl Pts',(-19.2101294376099,-35.4400540673517,
124.601126473367)) ;
#61868 = CARTESIAN_POINT('Ctrl Pts',(-19.4211928177086,-35.6300010842576,
124.919386454323)) ;
#61869 = CARTESIAN_POINT('Ctrl Pts',(-19.4188119019026,-35.4500120038947,
124.617871878894)) ;
#61870 = CARTESIAN_POINT('Ctrl Pts',(-19.6837654584528,-35.6400399542659,
124.894038281209)) ;
#61871 = CARTESIAN_POINT('Ctrl Pts',(-19.6288700585704,-35.460050873903,124.59759241855)) ;
#61872 = CARTESIAN_POINT('Ctrl Pts',(-19.9339392913664,-35.6499131094241,
124.825100619419)) ;
#61873 = CARTESIAN_POINT('Ctrl Pts',(-19.8290080447909,-35.4699240290612,
124.542441760864)) ;
#61874 = CARTESIAN_POINT('Ctrl Pts',(-20.1729716447795,-35.6599863842738,
124.711483830272)) ;
#61875 = CARTESIAN_POINT('Ctrl Pts',(-20.0202338855392,-35.4799973039109,
124.451547444271)) ;
#61876 = CARTESIAN_POINT('Ctrl Pts',(-20.3835167615202,-35.6698067014512,
124.562152640001)) ;
#61877 = CARTESIAN_POINT('Ctrl Pts',(-20.1886685395271,-35.4898176210883,
124.332082614018)) ;
#61878 = CARTESIAN_POINT('Ctrl Pts',(-20.5697933970036,-35.6798853872447,
124.373961088606)) ;
#61879 = CARTESIAN_POINT('Ctrl Pts',(-20.337689632591,-35.4998963068818,124.1815286286)) ;
#61880 = CARTESIAN_POINT('Ctrl Pts',(-20.7173141230226,-35.6897368986278,
124.161139832778)) ;
#61881 = CARTESIAN_POINT('Ctrl Pts',(-20.4557050752507,-35.5097478182649,
124.011272119984)) ;
#61882 = CARTESIAN_POINT('Ctrl Pts',(-20.8282376597634,-35.6998103449344,
123.920835993557)) ;
#61883 = CARTESIAN_POINT('Ctrl Pts',(-20.5444435077093,-35.5198212645716,
123.81902847826)) ;
#61884 = CARTESIAN_POINT('Ctrl Pts',(-20.8941975462152,-35.7096516200591,
123.670739828049)) ;
#61885 = CARTESIAN_POINT('Ctrl Pts',(-20.5972105412205,-35.5296625396963,
123.618952491442)) ;
#61886 = CARTESIAN_POINT('Ctrl Pts',(-20.9168565666188,-35.7196367197159,
123.409346913405)) ;
#61887 = CARTESIAN_POINT('Ctrl Pts',(-20.6153373392901,-35.539647639353,123.409838356451)) ;
#61888 = CARTESIAN_POINT('Ctrl Pts',(-20.8933643885283,-35.7296441958502,
123.147392528966)) ;
#61889 = CARTESIAN_POINT('Ctrl Pts',(-20.5965431125166,-35.5496551154873,
123.200274949627)) ;
#61890 = CARTESIAN_POINT('Ctrl Pts',(-20.8255661487373,-35.7395667835592,
122.89561863727)) ;
#61891 = CARTESIAN_POINT('Ctrl Pts',(-20.5423042616246,-35.5595777031963,
122.998856548276)) ;
#61892 = CARTESIAN_POINT('Ctrl Pts',(-20.7147391058567,-35.7495533878325,
122.657703592569)) ;
#61893 = CARTESIAN_POINT('Ctrl Pts',(-20.4536424122356,-35.5695643074696,
122.80852482131)) ;
#61894 = CARTESIAN_POINT('Ctrl Pts',(-20.5631005957844,-35.7595935161666,
122.44181432373)) ;
#61895 = CARTESIAN_POINT('Ctrl Pts',(-20.3323311466458,-35.5796044358037,
122.635813545013)) ;
#61896 = CARTESIAN_POINT('Ctrl Pts',(-20.380378834698,-35.7694329507,122.258824742576)) ;
#61897 = CARTESIAN_POINT('Ctrl Pts',(-20.1861543576817,-35.5894438703371,
122.489422939203)) ;
#61898 = CARTESIAN_POINT('Ctrl Pts',(-20.1640017994239,-35.779497005191,122.106806406757)) ;
#61899 = CARTESIAN_POINT('Ctrl Pts',(-20.0130523328328,-35.5995079248281,
122.36780830073)) ;
#61900 = CARTESIAN_POINT('Ctrl Pts',(-19.9285321533398,-35.7893879244282,
121.996676734452)) ;
#61901 = CARTESIAN_POINT('Ctrl Pts',(-19.8246772528639,-35.6093988440653,
122.279705175091)) ;
#61902 = CARTESIAN_POINT('Ctrl Pts',(-19.67513790255,-35.7993799177342,121.927884966154)) ;
#61903 = CARTESIAN_POINT('Ctrl Pts',(-19.6219619807546,-35.6193908373713,
122.224671942912)) ;
#61904 = CARTESIAN_POINT('Ctrl Pts',(-19.4143822634357,-35.8093427816935,
121.904446853395)) ;
#61905 = CARTESIAN_POINT('Ctrl Pts',(-19.4133578143958,-35.6293537013306,
122.205921690293)) ;
#61906 = CARTESIAN_POINT('Ctrl Pts',(-19.1549680514992,-35.8192470415113,
121.925855666197)) ;
#61907 = CARTESIAN_POINT('Ctrl Pts',(-19.2058271969419,-35.6392579611484,
122.223048715094)) ;
#61908 = CARTESIAN_POINT('Ctrl Pts',(-18.8993526736226,-35.8293075320827,
121.993232864711)) ;
#61909 = CARTESIAN_POINT('Ctrl Pts',(-19.001334645375,-35.6493184517198,122.276950638567)) ;
#61910 = CARTESIAN_POINT('Ctrl Pts',(-18.6643671184913,-35.8391478817137,
122.101269435871)) ;
#61911 = CARTESIAN_POINT('Ctrl Pts',(-18.8133472746285,-35.6591588013508,
122.363379411723)) ;
#61912 = CARTESIAN_POINT('Ctrl Pts',(-18.4467771153745,-35.8492108572037,
122.251492745729)) ;
#61913 = CARTESIAN_POINT('Ctrl Pts',(-18.6392749852965,-35.6692217768408,
122.483558171074)) ;
#61914 = CARTESIAN_POINT('Ctrl Pts',(-18.2618359407232,-35.8591051773471,
122.434298711921)) ;
#61915 = CARTESIAN_POINT('Ctrl Pts',(-18.491322616233,-35.6791160969842,122.629802358124)) ;
#61916 = CARTESIAN_POINT('Ctrl Pts',(-18.1101865601334,-35.8690468904787,
122.646995887001)) ;
#61917 = CARTESIAN_POINT('Ctrl Pts',(-18.3700032496171,-35.6890578101158,
122.799959569415)) ;
#61918 = CARTESIAN_POINT('Ctrl Pts',(-17.9969449047293,-35.8790497802728,
122.884263259516)) ;
#61919 = CARTESIAN_POINT('Ctrl Pts',(-18.2794097634867,-35.69906069991,122.989773283224)) ;
#61920 = CARTESIAN_POINT('Ctrl Pts',(-17.9268443214871,-35.8890896374333,
123.138590645404)) ;
#61921 = CARTESIAN_POINT('Ctrl Pts',(-18.2233291597186,-35.7091005570704,
123.193235305604)) ;
#61922 = CARTESIAN_POINT('Ctrl Pts',(-17.9019122829128,-35.8989138182709,
123.395574782342)) ;
#61923 = CARTESIAN_POINT('Ctrl Pts',(-18.2033834027197,-35.7189247379081,
123.398821321961)) ;
#61924 = CARTESIAN_POINT('Ctrl Pts',(-17.9220883778628,-35.9089707917741,
123.659068393619)) ;
#61925 = CARTESIAN_POINT('Ctrl Pts',(-18.2195239554329,-35.7289817114113,
123.609616505664)) ;
#61926 = CARTESIAN_POINT('Ctrl Pts',(-17.9871986049093,-35.9188989159612,
123.911729558089)) ;
#61927 = CARTESIAN_POINT('Ctrl Pts',(-18.271611742449,-35.7389098355983,123.811744931268)) ;
#61928 = CARTESIAN_POINT('Ctrl Pts',(-18.0948259751119,-35.9288526110346,
124.150136156797)) ;
#61929 = CARTESIAN_POINT('Ctrl Pts',(-18.3577130663129,-35.7488635306717,
124.002469995443)) ;
#61930 = CARTESIAN_POINT('Ctrl Pts',(-18.2438917115577,-35.9388988046099,
124.368025599995)) ;
#61931 = CARTESIAN_POINT('Ctrl Pts',(-18.4769654839936,-35.758909724247,124.176781901697)) ;
#61932 = CARTESIAN_POINT('Ctrl Pts',(-18.4247087145349,-35.9487469069698,
124.553177298368)) ;
#61933 = CARTESIAN_POINT('Ctrl Pts',(-18.6216180178333,-35.7687578266069,
124.324902741368)) ;
#61934 = CARTESIAN_POINT('Ctrl Pts',(-18.6368680943373,-35.9587084951974,
124.706511430656)) ;
#61935 = CARTESIAN_POINT('Ctrl Pts',(-18.7913448718134,-35.7787194148345,
124.44757032455)) ;
#61936 = CARTESIAN_POINT('Ctrl Pts',(-18.8741832744797,-35.9687371653537,
124.821161297278)) ;
#61937 = CARTESIAN_POINT('Ctrl Pts',(-18.9811968587923,-35.7887480849908,
124.539290720976)) ;
#61938 = CARTESIAN_POINT('Ctrl Pts',(-19.1247583602108,-35.9786474682354,
124.892091064519)) ;
#61939 = CARTESIAN_POINT('Ctrl Pts',(-19.1816561053087,-35.7986583878725,
124.59603486579)) ;
#61940 = CARTESIAN_POINT('Ctrl Pts',(-19.3844352240823,-35.9885823520433,
124.919183512007)) ;
#61941 = CARTESIAN_POINT('Ctrl Pts',(-19.3893969971606,-35.8085932716804,
124.617709476599)) ;
#61942 = CARTESIAN_POINT('Ctrl Pts',(-19.6476231191508,-35.9986234937339,
124.900335055066)) ;
#61943 = CARTESIAN_POINT('Ctrl Pts',(-19.5999475089394,-35.8186344133711,
124.602631349119)) ;
#61944 = CARTESIAN_POINT('Ctrl Pts',(-19.8996824512963,-36.0085106148979,
124.837232249301)) ;
#61945 = CARTESIAN_POINT('Ctrl Pts',(-19.8015943370243,-35.828521534535,124.552149980266)) ;
#61946 = CARTESIAN_POINT('Ctrl Pts',(-20.1396295182809,-36.0185029577464,
124.730608252142)) ;
#61947 = CARTESIAN_POINT('Ctrl Pts',(-19.9935521670757,-35.8385138773836,
124.466851580924)) ;
#61948 = CARTESIAN_POINT('Ctrl Pts',(-20.3564426703236,-36.0284512589704,
124.584508836111)) ;
#61949 = CARTESIAN_POINT('Ctrl Pts',(-20.1670027663451,-35.8484621786075,
124.34997293713)) ;
#61950 = CARTESIAN_POINT('Ctrl Pts',(-20.5446351269655,-36.0383888366525,
124.403471920414)) ;
#61951 = CARTESIAN_POINT('Ctrl Pts',(-20.3175569672634,-35.8583997562896,
124.205144391475)) ;
#61952 = CARTESIAN_POINT('Ctrl Pts',(-20.6995297067376,-36.0483754111031,
124.191598913458)) ;
#61953 = CARTESIAN_POINT('Ctrl Pts',(-20.4414732773456,-35.8683863307402,
124.035646689111)) ;
#61954 = CARTESIAN_POINT('Ctrl Pts',(-20.8154914356218,-36.0584042210115,
123.954937669147)) ;
#61955 = CARTESIAN_POINT('Ctrl Pts',(-20.5342434668736,-35.8784151406487,
123.846318005785)) ;
#61956 = CARTESIAN_POINT('Ctrl Pts',(-20.887745257479,-36.0682825423183,123.705606150759)) ;
#61957 = CARTESIAN_POINT('Ctrl Pts',(-20.5920471744882,-35.8882934619554,
123.646853866704)) ;
#61958 = CARTESIAN_POINT('Ctrl Pts',(-20.9165435264159,-36.0782741896657,
123.444611225449)) ;
#61959 = CARTESIAN_POINT('Ctrl Pts',(-20.6150868306485,-35.8982851093029,
123.438058194467)) ;
#61960 = CARTESIAN_POINT('Ctrl Pts',(-20.8989774525734,-36.0883087131035,
123.181512331536)) ;
#61961 = CARTESIAN_POINT('Ctrl Pts',(-20.6010349029805,-35.9083196327406,
123.227578932499)) ;
#61962 = CARTESIAN_POINT('Ctrl Pts',(-20.8375844347476,-36.0981720699821,
122.929660650926)) ;
#61963 = CARTESIAN_POINT('Ctrl Pts',(-20.55192174251,-35.9181829896192,123.026098230027)) ;
#61964 = CARTESIAN_POINT('Ctrl Pts',(-20.7312794061574,-36.1082422966624,
122.687347241547)) ;
#61965 = CARTESIAN_POINT('Ctrl Pts',(-20.4668785833512,-35.9282532162995,
122.832246790872)) ;
#61966 = CARTESIAN_POINT('Ctrl Pts',(-20.5878041611143,-36.1180846047971,
122.472130151302)) ;
#61967 = CARTESIAN_POINT('Ctrl Pts',(-20.3520998563727,-35.9380955244342,
122.660073387355)) ;
#61968 = CARTESIAN_POINT('Ctrl Pts',(-20.4077016432791,-36.1280453368205,
122.282190824122)) ;
#61969 = CARTESIAN_POINT('Ctrl Pts',(-20.2080190009201,-35.9480562564576,
122.50812127463)) ;
#61970 = CARTESIAN_POINT('Ctrl Pts',(-20.1954179813049,-36.1380832260186,
122.125622966376)) ;
#61971 = CARTESIAN_POINT('Ctrl Pts',(-20.0381926818535,-35.9580941456557,
122.382865981336)) ;
#61972 = CARTESIAN_POINT('Ctrl Pts',(-19.9632011127719,-36.1479575089374,
122.009756791366)) ;
#61973 = CARTESIAN_POINT('Ctrl Pts',(-19.852420481698,-35.9679684285746,122.290172259536)) ;
#61974 = CARTESIAN_POINT('Ctrl Pts',(-19.7095295605332,-36.1580272535549,
121.93454430428)) ;
#61975 = CARTESIAN_POINT('Ctrl Pts',(-19.6494833349554,-35.978038173192,122.230000967982)) ;
#61976 = CARTESIAN_POINT('Ctrl Pts',(-19.4527844206973,-36.1678605639005,
121.90508124975)) ;
#61977 = CARTESIAN_POINT('Ctrl Pts',(-19.4440883880503,-35.9878714835377,
122.206429346442)) ;
#61978 = CARTESIAN_POINT('Ctrl Pts',(-19.1896400044963,-36.1778908072532,
121.920204651437)) ;
#61979 = CARTESIAN_POINT('Ctrl Pts',(-19.2335727027001,-35.9979017268903,
122.218526613797)) ;
#61980 = CARTESIAN_POINT('Ctrl Pts',(-18.9332371754208,-36.1879230952316,
121.981571396722)) ;
#61981 = CARTESIAN_POINT('Ctrl Pts',(-19.0284500699383,-36.0079340148687,
122.267618766793)) ;
#61982 = CARTESIAN_POINT('Ctrl Pts',(-18.6960884547325,-36.1977502716997,
122.083816541885)) ;
#61983 = CARTESIAN_POINT('Ctrl Pts',(-18.838731476733,-36.0177611913368,122.349413165543)) ;
#61984 = CARTESIAN_POINT('Ctrl Pts',(-18.4761127317123,-36.2077556545666,
122.22778364051)) ;
#61985 = CARTESIAN_POINT('Ctrl Pts',(-18.6627501158308,-36.0277665742037,
122.464585522614)) ;
#61986 = CARTESIAN_POINT('Ctrl Pts',(-18.2849106465945,-36.2177382935593,
122.407469430057)) ;
#61987 = CARTESIAN_POINT('Ctrl Pts',(-18.5097875384203,-36.0377492131964,
122.60833293523)) ;
#61988 = CARTESIAN_POINT('Ctrl Pts',(-18.127151161634,-36.2277823606959,122.619049599079)) ;
#61989 = CARTESIAN_POINT('Ctrl Pts',(-18.3835787128746,-36.047793280333,122.777596301397)) ;
#61990 = CARTESIAN_POINT('Ctrl Pts',(-18.0107408057579,-36.2376035794999,
122.849407145954)) ;
#61991 = CARTESIAN_POINT('Ctrl Pts',(-18.2904495064269,-36.057614499137,122.961880755855)) ;
#61992 = CARTESIAN_POINT('Ctrl Pts',(-17.9338160941293,-36.247640418438,123.101693464145)) ;
#61993 = CARTESIAN_POINT('Ctrl Pts',(-18.2289081204975,-36.0676513380751,
123.163709405385)) ;
#61994 = CARTESIAN_POINT('Ctrl Pts',(-17.902648663204,-36.2576648305357,123.363283148383)) ;
#61995 = CARTESIAN_POINT('Ctrl Pts',(-18.2039726598348,-36.0776757501728,
123.372980991972)) ;
#61996 = CARTESIAN_POINT('Ctrl Pts',(-17.9165495303506,-36.267516914941,123.621816862721)) ;
#61997 = CARTESIAN_POINT('Ctrl Pts',(-18.2150916816491,-36.0875278345781,
123.579807245692)) ;
#61998 = CARTESIAN_POINT('Ctrl Pts',(-17.9755567901383,-36.2775078116842,
123.877618050233)) ;
#61999 = CARTESIAN_POINT('Ctrl Pts',(-18.2622957977157,-36.0975187313213,
123.784448445474)) ;
#62000 = CARTESIAN_POINT('Ctrl Pts',(-18.0772031608818,-36.2874258035851,
124.117648747743)) ;
#62001 = CARTESIAN_POINT('Ctrl Pts',(-18.3436111230473,-36.1074367232222,
123.976473257481)) ;
#62002 = CARTESIAN_POINT('Ctrl Pts',(-18.2204755143682,-36.2974539190421,
124.338803226218)) ;
#62003 = CARTESIAN_POINT('Ctrl Pts',(-18.4582275584006,-36.1174648386792,
124.153397810827)) ;
#62004 = CARTESIAN_POINT('Ctrl Pts',(-18.3973504809565,-36.3073390949842,
124.529066690562)) ;
#62005 = CARTESIAN_POINT('Ctrl Pts',(-18.5997258423448,-36.1273500146213,
124.30560934978)) ;
#62006 = CARTESIAN_POINT('Ctrl Pts',(-18.6063723872479,-36.3173284533911,
124.687887703223)) ;
#62007 = CARTESIAN_POINT('Ctrl Pts',(-18.7669421404985,-36.1373393730282,
124.43266756716)) ;
#62008 = CARTESIAN_POINT('Ctrl Pts',(-18.8412552934419,-36.3273696009714,
124.808127004772)) ;
#62009 = CARTESIAN_POINT('Ctrl Pts',(-18.9548477220754,-36.1473805206085,
124.528860620491)) ;
#62010 = CARTESIAN_POINT('Ctrl Pts',(-19.088082204701,-36.3372022239778,124.884553235414)) ;
#62011 = CARTESIAN_POINT('Ctrl Pts',(-19.1523079763883,-36.157213143615,124.590003139103)) ;
#62012 = CARTESIAN_POINT('Ctrl Pts',(-19.3485418518654,-36.3471962950886,
124.918229067231)) ;
#62013 = CARTESIAN_POINT('Ctrl Pts',(-19.3606753488184,-36.1672072147257,
124.616945728324)) ;
#62014 = CARTESIAN_POINT('Ctrl Pts',(-19.6117962054243,-36.3572249527295,
124.905606556835)) ;
#62015 = CARTESIAN_POINT('Ctrl Pts',(-19.571278932422,-36.1772358723666,124.606849593265)) ;
#62016 = CARTESIAN_POINT('Ctrl Pts',(-19.8651977309864,-36.3671092789223,
124.848586979554)) ;
#62017 = CARTESIAN_POINT('Ctrl Pts',(-19.7740000730835,-36.1871201985594,
124.561235916018)) ;
#62018 = CARTESIAN_POINT('Ctrl Pts',(-20.1070919688669,-36.3770750224129,
124.748197481995)) ;
#62019 = CARTESIAN_POINT('Ctrl Pts',(-19.9675160571563,-36.19708594205,124.480926240918)) ;
#62020 = CARTESIAN_POINT('Ctrl Pts',(-20.3290461476334,-36.3871034015441,
124.606136879299)) ;
#62021 = CARTESIAN_POINT('Ctrl Pts',(-20.1450804639494,-36.2071143211812,
124.367279397955)) ;
#62022 = CARTESIAN_POINT('Ctrl Pts',(-20.5207969131445,-36.397004247751,124.430224963369)) ;
#62023 = CARTESIAN_POINT('Ctrl Pts',(-20.2984821301222,-36.2170151673881,
124.226551616459)) ;
#62024 = CARTESIAN_POINT('Ctrl Pts',(-20.6815114754316,-36.4070629051681,
124.220415524595)) ;
#62025 = CARTESIAN_POINT('Ctrl Pts',(-20.4270554231223,-36.2270738248052,
124.058705203557)) ;
#62026 = CARTESIAN_POINT('Ctrl Pts',(-20.8012013743605,-36.41692046795,123.990625446808)) ;
#62027 = CARTESIAN_POINT('Ctrl Pts',(-20.5228088997045,-36.2369313875871,
123.874874540363)) ;
#62028 = CARTESIAN_POINT('Ctrl Pts',(-20.8809810994181,-36.4269888705032,
123.738394192383)) ;
#62029 = CARTESIAN_POINT('Ctrl Pts',(-20.5866346717548,-36.2469997901403,
123.673090038089)) ;
#62030 = CARTESIAN_POINT('Ctrl Pts',(-20.9150001537344,-36.4368442692428,
123.481625971228)) ;
#62031 = CARTESIAN_POINT('Ctrl Pts',(-20.6138518770455,-36.2568551888799,
123.467676224677)) ;
#62032 = CARTESIAN_POINT('Ctrl Pts',(-20.9045521214138,-36.4468391363167,
123.219187981031)) ;
#62033 = CARTESIAN_POINT('Ctrl Pts',(-20.6054955832144,-36.2668500559538,
123.257725827146)) ;
#62034 = CARTESIAN_POINT('Ctrl Pts',(-20.8479327596291,-36.4568704313002,
122.961723074886)) ;
#62035 = CARTESIAN_POINT('Ctrl Pts',(-20.5602021162859,-36.2768813509373,
123.051753458956)) ;
#62036 = CARTESIAN_POINT('Ctrl Pts',(-20.7495006730971,-36.4667369560267,
122.721841789066)) ;
#62037 = CARTESIAN_POINT('Ctrl Pts',(-20.4814585578185,-36.2867478756638,
122.859848009329)) ;
#62038 = CARTESIAN_POINT('Ctrl Pts',(-20.609591909687,-36.4767244267224,122.499818683266)) ;
#62039 = CARTESIAN_POINT('Ctrl Pts',(-20.36953342095,-36.2967353463596,122.68222845983)) ;
#62040 = CARTESIAN_POINT('Ctrl Pts',(-20.4340715146542,-36.4866691862863,
122.306140896146)) ;
#62041 = CARTESIAN_POINT('Ctrl Pts',(-20.2291188313566,-36.3066801059234,
122.527284917964)) ;
#62042 = CARTESIAN_POINT('Ctrl Pts',(-20.2254502142119,-36.4967147422351,
122.144429454285)) ;
#62043 = CARTESIAN_POINT('Ctrl Pts',(-20.0622230962988,-36.3167256618723,
122.397914055264)) ;
#62044 = CARTESIAN_POINT('Ctrl Pts',(-19.9963181527322,-36.5065743306102,
122.023404639029)) ;
#62045 = CARTESIAN_POINT('Ctrl Pts',(-19.8789187628921,-36.3265852502474,
122.301092445277)) ;
#62046 = CARTESIAN_POINT('Ctrl Pts',(-19.7463087037596,-36.5165752857463,
121.942510562632)) ;
#62047 = CARTESIAN_POINT('Ctrl Pts',(-19.6789119467519,-36.3365862053834,
122.236375109967)) ;
#62048 = CARTESIAN_POINT('Ctrl Pts',(-19.4885136890261,-36.5264795130239,
121.906393185174)) ;
#62049 = CARTESIAN_POINT('Ctrl Pts',(-19.472676448649,-36.346490432661,122.207479050223)) ;
#62050 = CARTESIAN_POINT('Ctrl Pts',(-19.2248160077214,-36.536521589919,121.915638023373)) ;
#62051 = CARTESIAN_POINT('Ctrl Pts',(-19.2617182336787,-36.3565325095561,
122.214872707114)) ;
#62052 = CARTESIAN_POINT('Ctrl Pts',(-18.9700774883834,-36.5464292026052,
121.969685726458)) ;
#62053 = CARTESIAN_POINT('Ctrl Pts',(-19.0579271360362,-36.3664401222423,
122.258108661664)) ;
#62054 = CARTESIAN_POINT('Ctrl Pts',(-18.7250847627801,-36.5564837332209,
122.068538595468)) ;
#62055 = CARTESIAN_POINT('Ctrl Pts',(-18.8619321279312,-36.376494652858,122.337188894249)) ;
#62056 = CARTESIAN_POINT('Ctrl Pts',(-18.5051552713082,-36.5663445197698,
122.205642071035)) ;
#62057 = CARTESIAN_POINT('Ctrl Pts',(-18.6859875392954,-36.3863554394069,
122.446869671373)) ;
#62058 = CARTESIAN_POINT('Ctrl Pts',(-18.309504624998,-36.5763382748409,122.380772756738)) ;
#62059 = CARTESIAN_POINT('Ctrl Pts',(-18.5294655677005,-36.396349194478,122.586972503952)) ;
#62060 = CARTESIAN_POINT('Ctrl Pts',(-18.1481936177485,-36.5862636350808,
122.585788118924)) ;
#62061 = CARTESIAN_POINT('Ctrl Pts',(-18.4004150621657,-36.406274554718,122.750983322731)) ;
#62062 = CARTESIAN_POINT('Ctrl Pts',(-18.0236841922653,-36.5962915644761,
122.818002834881)) ;
#62063 = CARTESIAN_POINT('Ctrl Pts',(-18.300805562702,-36.4163024841132,122.936753987693)) ;
#62064 = CARTESIAN_POINT('Ctrl Pts',(-17.9422706636189,-36.6061778312754,
123.064758942346)) ;
#62065 = CARTESIAN_POINT('Ctrl Pts',(-18.2356726313687,-36.4261887509125,
123.134158078855)) ;
#62066 = CARTESIAN_POINT('Ctrl Pts',(-17.9042663342486,-36.6162096001737,
123.325585129761)) ;
#62067 = CARTESIAN_POINT('Ctrl Pts',(-18.2052669459445,-36.4362205198108,
123.342818652238)) ;
#62068 = CARTESIAN_POINT('Ctrl Pts',(-17.9117588182437,-36.6260911960173,
123.585201643652)) ;
#62069 = CARTESIAN_POINT('Ctrl Pts',(-18.2112586694567,-36.4461021156544,
123.55051186725)) ;
#62070 = CARTESIAN_POINT('Ctrl Pts',(-17.9650896020763,-36.6361530814852,
123.844142860244)) ;
#62071 = CARTESIAN_POINT('Ctrl Pts',(-18.2539211167218,-36.4561640011224,
123.757665267779)) ;
#62072 = CARTESIAN_POINT('Ctrl Pts',(-18.0605371633806,-36.6460105155041,
124.084996144572)) ;
#62073 = CARTESIAN_POINT('Ctrl Pts',(-18.3302769065666,-36.4660214351412,
123.950348570272)) ;
#62074 = CARTESIAN_POINT('Ctrl Pts',(-18.1977180729179,-36.6560037585461,
124.308890236601)) ;
#62075 = CARTESIAN_POINT('Ctrl Pts',(-18.4400203090856,-36.4760146781832,
124.129465536782)) ;
#62076 = CARTESIAN_POINT('Ctrl Pts',(-18.3706217888367,-36.6659345194324,
124.504384734692)) ;
#62077 = CARTESIAN_POINT('Ctrl Pts',(-18.5783393320726,-36.4859454390695,
124.285860564829)) ;
#62078 = CARTESIAN_POINT('Ctrl Pts',(-18.6449288885869,-36.6792835116296,
124.7231001116)) ;
#62079 = CARTESIAN_POINT('Ctrl Pts',(-18.797794429001,-36.4992944312667,124.46084539929)) ;
#62080 = CARTESIAN_POINT('Ctrl Pts',(-18.9682246085567,-36.692551884446,124.863897618014)) ;
#62081 = CARTESIAN_POINT('Ctrl Pts',(-19.0564576791259,-36.5125628040832,
124.573487208325)) ;
#62082 = CARTESIAN_POINT('Ctrl Pts',(-19.3133563776516,-36.7058348258304,
124.916340475203)) ;
#62083 = CARTESIAN_POINT('Ctrl Pts',(-19.3325181777442,-36.5258457454675,
124.615432945298)) ;
#62084 = CARTESIAN_POINT('Ctrl Pts',(-19.5771730601609,-36.7158776116726,
124.9098870958)) ;
#62085 = CARTESIAN_POINT('Ctrl Pts',(-19.5435804546175,-36.5358885313097,
124.610274688818)) ;
#62086 = CARTESIAN_POINT('Ctrl Pts',(-19.8309776235917,-36.7257275542247,
124.858999538569)) ;
#62087 = CARTESIAN_POINT('Ctrl Pts',(-19.7466221103153,-36.5457384738618,
124.569566509396)) ;
#62088 = CARTESIAN_POINT('Ctrl Pts',(-20.0759163398289,-36.7357247871437,
124.764028514352)) ;
#62089 = CARTESIAN_POINT('Ctrl Pts',(-19.9425753637021,-36.5557357067808,
124.493590557892)) ;
#62090 = CARTESIAN_POINT('Ctrl Pts',(-20.3008516831836,-36.7457396824782,
124.627366616209)) ;
#62091 = CARTESIAN_POINT('Ctrl Pts',(-20.1225212573089,-36.5657506021153,
124.384267868071)) ;
#62092 = CARTESIAN_POINT('Ctrl Pts',(-20.5625371625823,-36.7589793591164,
124.398087289449)) ;
#62093 = CARTESIAN_POINT('Ctrl Pts',(-20.3318880358835,-36.5789902787535,
124.200821860388)) ;
#62094 = CARTESIAN_POINT('Ctrl Pts',(-20.8079029753691,-36.7755265835217,
124.033128787356)) ;
#62095 = CARTESIAN_POINT('Ctrl Pts',(-20.5281632731602,-36.5955375031589,
123.908899479938)) ;
#62096 = CARTESIAN_POINT('Ctrl Pts',(-20.9148689308505,-36.7921740206528,
123.60379676647)) ;
#62097 = CARTESIAN_POINT('Ctrl Pts',(-20.6137528357625,-36.6121849402899,
123.56536784602)) ;
#62098 = CARTESIAN_POINT('Ctrl Pts',(-20.9083945687103,-36.805463518131,123.254597757722)) ;
#62099 = CARTESIAN_POINT('Ctrl Pts',(-20.6085683029633,-36.6254744377682,
123.286061935331)) ;
#62100 = CARTESIAN_POINT('Ctrl Pts',(-20.8593749513475,-36.8153369259534,
122.99980702422)) ;
#62101 = CARTESIAN_POINT('Ctrl Pts',(-20.56935600526,-36.6353478455905,123.082217773299)) ;
#62102 = CARTESIAN_POINT('Ctrl Pts',(-20.7652312032613,-36.8253893035461,
122.752998369539)) ;
#62103 = CARTESIAN_POINT('Ctrl Pts',(-20.4940428185494,-36.6454002231832,
122.884773343294)) ;
#62104 = CARTESIAN_POINT('Ctrl Pts',(-20.6315577727922,-36.835292957087,122.529670136184)) ;
#62105 = CARTESIAN_POINT('Ctrl Pts',(-20.3871046825718,-36.6553038767241,
122.706108244707)) ;
#62106 = CARTESIAN_POINT('Ctrl Pts',(-20.4609498467479,-36.8452372260823,
122.331765024518)) ;
#62107 = CARTESIAN_POINT('Ctrl Pts',(-20.250623548332,-36.6652481457194,122.547784435435)) ;
#62108 = CARTESIAN_POINT('Ctrl Pts',(-20.1896663855523,-36.858568234415,122.109990345323)) ;
#62109 = CARTESIAN_POINT('Ctrl Pts',(-20.0335788518521,-36.6785791540521,
122.3703552458)) ;
#62110 = CARTESIAN_POINT('Ctrl Pts',(-19.7868089891935,-36.8751898149393,
121.928852787723)) ;
#62111 = CARTESIAN_POINT('Ctrl Pts',(-19.7113302438444,-36.6952007345764,
122.22544992753)) ;
#62112 = CARTESIAN_POINT('Ctrl Pts',(-19.3483970122196,-36.8917324856377,
121.895325330693)) ;
#62113 = CARTESIAN_POINT('Ctrl Pts',(-19.3605382150688,-36.7117434052748,
122.198625176032)) ;
#62114 = CARTESIAN_POINT('Ctrl Pts',(-19.0036058959069,-36.9050816452006,
121.959959179237)) ;
#62115 = CARTESIAN_POINT('Ctrl Pts',(-19.084756195026,-36.7250925648377,122.250326885057)) ;
#62116 = CARTESIAN_POINT('Ctrl Pts',(-18.678061892058,-36.9183097953601,122.081981867065)) ;
#62117 = CARTESIAN_POINT('Ctrl Pts',(-18.8243006830399,-36.7383207149972,
122.347949900398)) ;
#62118 = CARTESIAN_POINT('Ctrl Pts',(-18.3181836591371,-36.9349404724976,
122.338513488551)) ;
#62119 = CARTESIAN_POINT('Ctrl Pts',(-18.536409956563,-36.7549513921347,122.553165511551)) ;
#62120 = CARTESIAN_POINT('Ctrl Pts',(-18.0180562107992,-36.9548434117857,
122.774198058464)) ;
#62121 = CARTESIAN_POINT('Ctrl Pts',(-18.2963005856459,-36.7748543314228,
122.901714217013)) ;
#62122 = CARTESIAN_POINT('Ctrl Pts',(-17.884130698863,-36.974746278389,123.285845641894)) ;
#62123 = CARTESIAN_POINT('Ctrl Pts',(-18.1891582490799,-36.7947571980261,
123.311031567695)) ;
#62124 = CARTESIAN_POINT('Ctrl Pts',(-17.9320811341198,-36.9946594434938,
123.813046654327)) ;
#62125 = CARTESIAN_POINT('Ctrl Pts',(-18.2275157048257,-36.8146703631309,
123.732793421951)) ;
#62126 = CARTESIAN_POINT('Ctrl Pts',(-18.159115508631,-37.0146952726351,124.294661831118)) ;
#62127 = CARTESIAN_POINT('Ctrl Pts',(-18.4091406225134,-36.8347061922723,
124.118086406354)) ;
#62128 = CARTESIAN_POINT('Ctrl Pts',(-18.5326928560836,-37.0345138475132,
124.666191700449)) ;
#62129 = CARTESIAN_POINT('Ctrl Pts',(-18.7080017265223,-36.8545247671503,
124.415313158299)) ;
#62130 = CARTESIAN_POINT('Ctrl Pts',(-19.0136563927245,-37.0544841485552,
124.890270639901)) ;
#62131 = CARTESIAN_POINT('Ctrl Pts',(-19.0927719398134,-36.8744950681923,
124.594578398497)) ;
#62132 = CARTESIAN_POINT('Ctrl Pts',(-19.5404829664515,-37.0743756809197,
124.936789595179)) ;
#62133 = CARTESIAN_POINT('Ctrl Pts',(-19.5142340085164,-36.8943866005569,
124.63179555628)) ;
#62134 = CARTESIAN_POINT('Ctrl Pts',(-20.0545360586126,-37.0943987787363,
124.799534983068)) ;
#62135 = CARTESIAN_POINT('Ctrl Pts',(-19.9254767467742,-36.9144096983734,
124.52199379209)) ;
#62136 = CARTESIAN_POINT('Ctrl Pts',(-20.4863256454403,-37.1141955316562,
124.498745537816)) ;
#62137 = CARTESIAN_POINT('Ctrl Pts',(-20.2709110786742,-36.9342064512933,
124.281362358102)) ;
#62138 = CARTESIAN_POINT('Ctrl Pts',(-20.7931678599209,-37.134156620145,124.066005974626)) ;
#62139 = CARTESIAN_POINT('Ctrl Pts',(-20.5163858339727,-36.9541675397821,
123.93517078883)) ;
#62140 = CARTESIAN_POINT('Ctrl Pts',(-20.9329957734479,-37.1541348890772,
123.553712501942)) ;
#62141 = CARTESIAN_POINT('Ctrl Pts',(-20.6282493161937,-36.9741458087143,
123.525336142619)) ;
#62142 = CARTESIAN_POINT('Ctrl Pts',(-20.8907271345775,-37.1739549038682,
123.028678283237)) ;
#62143 = CARTESIAN_POINT('Ctrl Pts',(-20.5944348575025,-36.9939658235053,
123.105306484844)) ;
#62144 = CARTESIAN_POINT('Ctrl Pts',(-20.6717362479,-37.19389331312,122.546084069936)) ;
#62145 = CARTESIAN_POINT('Ctrl Pts',(-20.4192415860018,-37.0139042327571,
122.719230493431)) ;
#62146 = CARTESIAN_POINT('Ctrl Pts',(-20.298300215747,-37.2139404305124,122.165933042875)) ;
#62147 = CARTESIAN_POINT('Ctrl Pts',(-20.1204933529623,-37.0339513501496,
122.415110073134)) ;
#62148 = CARTESIAN_POINT('Ctrl Pts',(-19.8223796112928,-37.2337866763463,
121.938614397227)) ;
#62149 = CARTESIAN_POINT('Ctrl Pts',(-19.7397550078523,-37.0537975959834,
122.233254223609)) ;
#62150 = CARTESIAN_POINT('Ctrl Pts',(-19.2975051439848,-37.2536356448583,
121.885263707638)) ;
#62151 = CARTESIAN_POINT('Ctrl Pts',(-19.3198535804931,-37.0736465644954,
122.190574646049)) ;
#62152 = CARTESIAN_POINT('Ctrl Pts',(-18.7809853427193,-37.2736859471696,
122.01617607887)) ;
#62153 = CARTESIAN_POINT('Ctrl Pts',(-18.9066385592989,-37.0936968668067,
122.295305374503)) ;
#62154 = CARTESIAN_POINT('Ctrl Pts',(-18.3447935795883,-37.2935208696008,
122.312469305322)) ;
#62155 = CARTESIAN_POINT('Ctrl Pts',(-18.5576842939248,-37.113531789238,122.532341920129)) ;
#62156 = CARTESIAN_POINT('Ctrl Pts',(-18.0337656489116,-37.3134512708267,
122.741007439741)) ;
#62157 = CARTESIAN_POINT('Ctrl Pts',(-18.3088629320483,-37.1334621904638,
122.875174080636)) ;
#62158 = CARTESIAN_POINT('Ctrl Pts',(-17.8872187178112,-37.3333362161856,
123.249003693809)) ;
#62159 = CARTESIAN_POINT('Ctrl Pts',(-18.1916271520052,-37.1533471358227,
123.28157263407)) ;
#62160 = CARTESIAN_POINT('Ctrl Pts',(-17.9240043991043,-37.353408824337,123.781130410511)) ;
#62161 = CARTESIAN_POINT('Ctrl Pts',(-18.2210576286058,-37.1734197439741,
123.707273187308)) ;
#62162 = CARTESIAN_POINT('Ctrl Pts',(-18.1371306277917,-37.3732001406651,
124.262126611238)) ;
#62163 = CARTESIAN_POINT('Ctrl Pts',(-18.3915613312149,-37.1932110603022,
124.092070982679)) ;
#62164 = CARTESIAN_POINT('Ctrl Pts',(-18.5035285318798,-37.3931649304323,
124.645891221234)) ;
#62165 = CARTESIAN_POINT('Ctrl Pts',(-18.6846818764584,-37.2131758500695,
124.399080894642)) ;
#62166 = CARTESIAN_POINT('Ctrl Pts',(-18.979960539183,-37.4131478861826,124.8806328502)) ;
#62167 = CARTESIAN_POINT('Ctrl Pts',(-19.0658287233952,-37.2331588058198,
124.586871974143)) ;
#62168 = CARTESIAN_POINT('Ctrl Pts',(-19.5032077670167,-37.4329564081588,
124.93927814081)) ;
#62169 = CARTESIAN_POINT('Ctrl Pts',(-19.4844282141108,-37.2529673277959,
124.633785395356)) ;
#62170 = CARTESIAN_POINT('Ctrl Pts',(-20.0196196742879,-37.4529419828946,
124.815366561225)) ;
#62171 = CARTESIAN_POINT('Ctrl Pts',(-19.8975570540621,-37.2729529025317,
124.534652928844)) ;
#62172 = CARTESIAN_POINT('Ctrl Pts',(-20.4606042546842,-37.472824622963,124.523953283866)) ;
#62173 = CARTESIAN_POINT('Ctrl Pts',(-20.2503434533714,-37.2928355426001,
124.301519156789)) ;
#62174 = CARTESIAN_POINT('Ctrl Pts',(-20.7770251297192,-37.4927799350949,
124.098432867934)) ;
#62175 = CARTESIAN_POINT('Ctrl Pts',(-20.5034774694716,-37.312790854732,123.961100528127)) ;
#62176 = CARTESIAN_POINT('Ctrl Pts',(-20.9290068708027,-37.5126542917027,
123.592447664143)) ;
#62177 = CARTESIAN_POINT('Ctrl Pts',(-20.6250594668182,-37.3326652113398,
123.556310724529)) ;
#62178 = CARTESIAN_POINT('Ctrl Pts',(-20.8993899561854,-37.5326364985638,
123.062239130214)) ;
#62179 = CARTESIAN_POINT('Ctrl Pts',(-20.6013622688047,-37.3526474182009,
123.132144083971)) ;
#62180 = CARTESIAN_POINT('Ctrl Pts',(-20.690825481049,-37.5525675765137,122.575167631245)) ;
#62181 = CARTESIAN_POINT('Ctrl Pts',(-20.4345064463008,-37.3725784961509,
122.742488126059)) ;
#62182 = CARTESIAN_POINT('Ctrl Pts',(-20.3288457045334,-37.5724945513687,
122.188694790906)) ;
#62183 = CARTESIAN_POINT('Ctrl Pts',(-20.1449218052122,-37.3925054710058,
122.433312456316)) ;
#62184 = CARTESIAN_POINT('Ctrl Pts',(-19.8592684233419,-37.5923270103176,
121.94907564169)) ;
#62185 = CARTESIAN_POINT('Ctrl Pts',(-19.7692491705873,-37.4123379299547,
122.241620182198)) ;
#62186 = CARTESIAN_POINT('Ctrl Pts',(-19.4200658004663,-37.6089846944928,
121.894159881209)) ;
#62187 = CARTESIAN_POINT('Ctrl Pts',(-19.4179129229134,-37.4289956141299,
122.197692407191)) ;
#62188 = CARTESIAN_POINT('Ctrl Pts',(-19.0750788995633,-37.6222339183999,
121.941806794377)) ;
#62189 = CARTESIAN_POINT('Ctrl Pts',(-19.1418999521506,-37.442244838037,122.235812007745)) ;
#62190 = CARTESIAN_POINT('Ctrl Pts',(-18.8237258577179,-37.6322829398511,
122.022687580734)) ;
#62191 = CARTESIAN_POINT('Ctrl Pts',(-18.9408249160599,-37.4522938594882,
122.300516750014)) ;
#62192 = CARTESIAN_POINT('Ctrl Pts',(-18.5945663208798,-37.6421429480816,
122.143620577139)) ;
#62193 = CARTESIAN_POINT('Ctrl Pts',(-18.7574893710446,-37.4621538677187,
122.397273180662)) ;
#62194 = CARTESIAN_POINT('Ctrl Pts',(-18.318087679396,-37.6554264613062,122.356789242169)) ;
#62195 = CARTESIAN_POINT('Ctrl Pts',(-18.5363454539202,-37.4754373809433,
122.567770274827)) ;
#62196 = CARTESIAN_POINT('Ctrl Pts',(-18.0500066419728,-37.672072380307,122.708670183428)) ;
#62197 = CARTESIAN_POINT('Ctrl Pts',(-18.3218393587194,-37.4920832999442,
122.849331203031)) ;
#62198 = CARTESIAN_POINT('Ctrl Pts',(-17.9182173116251,-37.6886263581231,
123.1284860917)) ;
#62199 = CARTESIAN_POINT('Ctrl Pts',(-18.2164325852077,-37.5086372777602,
123.185138398988)) ;
#62200 = CARTESIAN_POINT('Ctrl Pts',(-17.9032980831102,-37.7019860870947,
123.479244069035)) ;
#62201 = CARTESIAN_POINT('Ctrl Pts',(-18.2044905709866,-37.5219970067318,
123.465776425923)) ;
#62202 = CARTESIAN_POINT('Ctrl Pts',(-17.9373186787806,-37.7118791388914,
123.737005381468)) ;
#62203 = CARTESIAN_POINT('Ctrl Pts',(-18.2317111977967,-37.5318900585285,
123.671978909914)) ;
#62204 = CARTESIAN_POINT('Ctrl Pts',(-18.0159935017335,-37.7218691041725,
123.987433562175)) ;
#62205 = CARTESIAN_POINT('Ctrl Pts',(-18.2946526703774,-37.5418800238096,
123.872322439341)) ;
#62206 = CARTESIAN_POINT('Ctrl Pts',(-18.1363891804887,-37.7318209850333,
124.219643590471)) ;
#62207 = CARTESIAN_POINT('Ctrl Pts',(-18.3909713400926,-37.5518319046704,
124.058088956669)) ;
#62208 = CARTESIAN_POINT('Ctrl Pts',(-18.2969510924967,-37.7418693367251,
124.42924502608)) ;
#62209 = CARTESIAN_POINT('Ctrl Pts',(-18.5194225674474,-37.5618802563622,
124.225768799345)) ;
#62210 = CARTESIAN_POINT('Ctrl Pts',(-18.4872912316246,-37.7517106208313,
124.60436691775)) ;
#62211 = CARTESIAN_POINT('Ctrl Pts',(-18.6716962379228,-37.5717215404684,
124.365864646808)) ;
#62212 = CARTESIAN_POINT('Ctrl Pts',(-18.7080075972399,-37.761697323957,124.746264446467)) ;
#62213 = CARTESIAN_POINT('Ctrl Pts',(-18.848270497138,-37.5817082435941,124.479380739021)) ;
#62214 = CARTESIAN_POINT('Ctrl Pts',(-18.9487838243805,-37.7716323527744,
124.847344520004)) ;
#62215 = CARTESIAN_POINT('Ctrl Pts',(-19.0408922983168,-37.5916432724115,
124.560242693313)) ;
#62216 = CARTESIAN_POINT('Ctrl Pts',(-19.2065084133453,-37.7816881476813,
124.905549326523)) ;
#62217 = CARTESIAN_POINT('Ctrl Pts',(-19.2470724255386,-37.6016990673184,
124.606804323034)) ;
#62218 = CARTESIAN_POINT('Ctrl Pts',(-19.4645118314012,-37.7915165109706,
124.918239663582)) ;
#62219 = CARTESIAN_POINT('Ctrl Pts',(-19.4534751612069,-37.6115274306077,
124.61695433475)) ;
#62220 = CARTESIAN_POINT('Ctrl Pts',(-19.7268395348764,-37.8015774808685,
124.885556198697)) ;
#62221 = CARTESIAN_POINT('Ctrl Pts',(-19.6633370066296,-37.6215884005056,
124.590805332165)) ;
#62222 = CARTESIAN_POINT('Ctrl Pts',(-19.975820977289,-37.8114917597583,124.808729302256)) ;
#62223 = CARTESIAN_POINT('Ctrl Pts',(-19.8625213953459,-37.6315026793954,
124.529341692583)) ;
#62224 = CARTESIAN_POINT('Ctrl Pts',(-20.2101091148539,-37.8215007542265,
124.689174409311)) ;
#62225 = CARTESIAN_POINT('Ctrl Pts',(-20.0499508319165,-37.6415116738637,
124.433695808887)) ;
#62226 = CARTESIAN_POINT('Ctrl Pts',(-20.4201860704738,-37.8315305887903,
124.529999912084)) ;
#62227 = CARTESIAN_POINT('Ctrl Pts',(-20.2180110082682,-37.6515415084274,
124.306354429914)) ;
#62228 = CARTESIAN_POINT('Ctrl Pts',(-20.596742436033,-37.8413888188625,124.340392518913)) ;
#62229 = CARTESIAN_POINT('Ctrl Pts',(-20.3592543312716,-37.6613997384997,
124.154667125539)) ;
#62230 = CARTESIAN_POINT('Ctrl Pts',(-20.7399359738029,-37.8513875246049,
124.120135025723)) ;
#62231 = CARTESIAN_POINT('Ctrl Pts',(-20.4738072491821,-37.6713984442421,
123.978459973914)) ;
#62232 = CARTESIAN_POINT('Ctrl Pts',(-20.8419611023496,-37.8612821805237,
123.880914135963)) ;
#62233 = CARTESIAN_POINT('Ctrl Pts',(-20.5554252348265,-37.6812931001609,
123.787082588274)) ;
#62234 = CARTESIAN_POINT('Ctrl Pts',(-20.9018013798977,-37.8713452449077,
123.62337316206)) ;
#62235 = CARTESIAN_POINT('Ctrl Pts',(-20.603295299142,-37.6913561645448,123.581049278094)) ;
#62236 = CARTESIAN_POINT('Ctrl Pts',(-20.9159903077687,-37.8811849031876,
123.365144028715)) ;
#62237 = CARTESIAN_POINT('Ctrl Pts',(-20.6146442263728,-37.7011958228247,
123.374466181267)) ;
#62238 = CARTESIAN_POINT('Ctrl Pts',(-20.8847687942713,-37.8912480702694,
123.102580743054)) ;
#62239 = CARTESIAN_POINT('Ctrl Pts',(-20.589664844702,-37.7112589899066,123.16441577383)) ;
#62240 = CARTESIAN_POINT('Ctrl Pts',(-20.809484036126,-37.9011423153965,122.853677895888)) ;
#62241 = CARTESIAN_POINT('Ctrl Pts',(-20.5294350133251,-37.7211532350337,
122.965294385449)) ;
#62242 = CARTESIAN_POINT('Ctrl Pts',(-20.6922226402162,-37.9110841370011,
122.620247034589)) ;
#62243 = CARTESIAN_POINT('Ctrl Pts',(-20.4356240768759,-37.7310950566383,
122.778550847944)) ;
#62244 = CARTESIAN_POINT('Ctrl Pts',(-20.5352958890887,-37.9210866679192,
122.40933067988)) ;
#62245 = CARTESIAN_POINT('Ctrl Pts',(-20.3100810068094,-37.7410975875563,
122.60981908937)) ;
#62246 = CARTESIAN_POINT('Ctrl Pts',(-20.3432724835516,-37.9311212943767,
122.228617908719)) ;
#62247 = CARTESIAN_POINT('Ctrl Pts',(-20.1564607864245,-37.7511322140138,
122.465250443075)) ;
#62248 = CARTESIAN_POINT('Ctrl Pts',(-20.1271504515569,-37.9409668293631,
122.086359667686)) ;
#62249 = CARTESIAN_POINT('Ctrl Pts',(-19.9835623661803,-37.7609777490003,
122.351445878483)) ;
#62250 = CARTESIAN_POINT('Ctrl Pts',(-19.8865382083941,-37.9509502542022,
121.981841696408)) ;
#62251 = CARTESIAN_POINT('Ctrl Pts',(-19.7910718730727,-37.7709611738393,
122.267833461775)) ;
#62252 = CARTESIAN_POINT('Ctrl Pts',(-19.6322370248592,-37.9609006445672,
121.920936388949)) ;
#62253 = CARTESIAN_POINT('Ctrl Pts',(-19.5876306530056,-37.7809115642044,
122.219111287148)) ;
#62254 = CARTESIAN_POINT('Ctrl Pts',(-19.3699906918077,-37.9708982848643,
121.904681189327)) ;
#62255 = CARTESIAN_POINT('Ctrl Pts',(-19.3778335442572,-37.7909092045014,
122.206109169459)) ;
#62256 = CARTESIAN_POINT('Ctrl Pts',(-19.1079206636273,-37.9809373654275,
121.934852971173)) ;
#62257 = CARTESIAN_POINT('Ctrl Pts',(-19.1681777138388,-37.8009482850646,
122.230248687512)) ;
#62258 = CARTESIAN_POINT('Ctrl Pts',(-18.860240682653,-37.9907635161966,122.007929238581)) ;
#62259 = CARTESIAN_POINT('Ctrl Pts',(-18.9700348973941,-37.8107744358337,
122.288711477367)) ;
#62260 = CARTESIAN_POINT('Ctrl Pts',(-18.6234287247367,-38.0008200911257,
122.125206427547)) ;
#62261 = CARTESIAN_POINT('Ctrl Pts',(-18.7805861344579,-37.8208310107629,
122.382535045153)) ;
#62262 = CARTESIAN_POINT('Ctrl Pts',(-18.4132844279037,-38.010760630506,122.280394942276)) ;
#62263 = CARTESIAN_POINT('Ctrl Pts',(-18.6124721241605,-37.8307715501431,
122.506687339545)) ;
#62264 = CARTESIAN_POINT('Ctrl Pts',(-18.2333456791287,-38.0206650234824,
122.468461282899)) ;
#62265 = CARTESIAN_POINT('Ctrl Pts',(-18.4685228183294,-37.8406759431195,
122.657141441045)) ;
#62266 = CARTESIAN_POINT('Ctrl Pts',(-18.0868734496572,-38.0307116776873,
122.68809334047)) ;
#62267 = CARTESIAN_POINT('Ctrl Pts',(-18.3513466170776,-37.8507225973244,
122.832848242214)) ;
#62268 = CARTESIAN_POINT('Ctrl Pts',(-17.9821139835232,-38.0406072396257,
122.926149688474)) ;
#62269 = CARTESIAN_POINT('Ctrl Pts',(-18.2675409920432,-37.8606181592628,
123.023293667874)) ;
#62270 = CARTESIAN_POINT('Ctrl Pts',(-17.9192592235961,-38.0506693174713,
123.182952338498)) ;
#62271 = CARTESIAN_POINT('Ctrl Pts',(-18.2172590200462,-37.8706802371084,
123.228736387907)) ;
#62272 = CARTESIAN_POINT('Ctrl Pts',(-17.9021734628791,-38.060512015885,123.441072933946)) ;
#62273 = CARTESIAN_POINT('Ctrl Pts',(-18.2035923555535,-37.8805229355222,
123.43523229754)) ;
#62274 = CARTESIAN_POINT('Ctrl Pts',(-17.9299628607559,-38.0705027908465,
123.702111270586)) ;
#62275 = CARTESIAN_POINT('Ctrl Pts',(-18.2258256600623,-37.8905137104836,
123.644062635813)) ;
#62276 = CARTESIAN_POINT('Ctrl Pts',(-18.0022482230094,-38.0804306558656,
123.952806457239)) ;
#62277 = CARTESIAN_POINT('Ctrl Pts',(-18.2836555848188,-37.9004415755027,
123.844617906558)) ;
#62278 = CARTESIAN_POINT('Ctrl Pts',(-18.1172694269985,-38.0904194006318,
124.188763665487)) ;
#62279 = CARTESIAN_POINT('Ctrl Pts',(-18.3756740525521,-37.9104303202689,
124.033382779807)) ;
#62280 = CARTESIAN_POINT('Ctrl Pts',(-18.2725063779841,-38.1004521862187,
124.401872836885)) ;
#62281 = CARTESIAN_POINT('Ctrl Pts',(-18.4998651103405,-37.9204631058559,
124.203869099965)) ;
#62282 = CARTESIAN_POINT('Ctrl Pts',(-18.4590525160662,-38.1103188708394,
124.581942987114)) ;
#62283 = CARTESIAN_POINT('Ctrl Pts',(-18.6491027477406,-37.9303297904765,
124.347923469176)) ;
#62284 = CARTESIAN_POINT('Ctrl Pts',(-18.6756943059788,-38.1202807630025,
124.728918023254)) ;
#62285 = CARTESIAN_POINT('Ctrl Pts',(-18.8224168656527,-37.9402916826396,
124.46550199026)) ;
#62286 = CARTESIAN_POINT('Ctrl Pts',(-18.9164378070942,-38.1303142399151,
124.836426983259)) ;
#62287 = CARTESIAN_POINT('Ctrl Pts',(-19.0150124287312,-37.9503251595522,
124.551507627464)) ;
#62288 = CARTESIAN_POINT('Ctrl Pts',(-19.1683321359747,-38.1401985811634,
124.899959302381)) ;
#62289 = CARTESIAN_POINT('Ctrl Pts',(-19.2165276738214,-37.9602095008005,
124.602331745054)) ;
#62290 = CARTESIAN_POINT('Ctrl Pts',(-19.4320465863447,-38.1502615232845,
124.919128358715)) ;
#62291 = CARTESIAN_POINT('Ctrl Pts',(-19.4274995576439,-37.9702724429217,
124.617665373635)) ;
#62292 = CARTESIAN_POINT('Ctrl Pts',(-19.6895940464433,-38.1601119249041,
124.892904733968)) ;
#62293 = CARTESIAN_POINT('Ctrl Pts',(-19.6335365291386,-37.9801228445412,
124.596684955515)) ;
#62294 = CARTESIAN_POINT('Ctrl Pts',(-19.9432929414163,-38.1701388136938,
124.821745925476)) ;
#62295 = CARTESIAN_POINT('Ctrl Pts',(-19.8364952746785,-37.9901497333309,
124.539756471089)) ;
#62296 = CARTESIAN_POINT('Ctrl Pts',(-20.1805416769707,-38.18016742865,124.706967424635)) ;
#62297 = CARTESIAN_POINT('Ctrl Pts',(-20.0262936087495,-38.0001783482871,
124.447932190044)) ;
#62298 = CARTESIAN_POINT('Ctrl Pts',(-20.3906137720793,-38.19001265177,124.555971632204)) ;
#62299 = CARTESIAN_POINT('Ctrl Pts',(-20.1943496685895,-38.0100235714072,
124.327134842774)) ;
#62300 = CARTESIAN_POINT('Ctrl Pts',(-20.574464611682,-38.200003335576,124.368535624673)) ;
#62301 = CARTESIAN_POINT('Ctrl Pts',(-20.3414292436618,-38.0200142552131,
124.177185180511)) ;
#62302 = CARTESIAN_POINT('Ctrl Pts',(-20.7231886883335,-38.2100412176484,
124.1506774248)) ;
#62303 = CARTESIAN_POINT('Ctrl Pts',(-20.4604073258307,-38.0300521372856,
124.002897686156)) ;
#62304 = CARTESIAN_POINT('Ctrl Pts',(-20.8301490996899,-38.2198855772873,
123.915113415464)) ;
#62305 = CARTESIAN_POINT('Ctrl Pts',(-20.5459739843948,-38.0398964969244,
123.814446751513)) ;
#62306 = CARTESIAN_POINT('Ctrl Pts',(-20.8959919668574,-38.229870447902,123.661153850813)) ;
#62307 = CARTESIAN_POINT('Ctrl Pts',(-20.5986469676164,-38.0498813675391,
123.611278966283)) ;
#62308 = CARTESIAN_POINT('Ctrl Pts',(-20.9167692456538,-38.2398097312307,
123.400748772405)) ;
#62309 = CARTESIAN_POINT('Ctrl Pts',(-20.6152674855689,-38.0598206508678,
123.402955237377)) ;
#62310 = CARTESIAN_POINT('Ctrl Pts',(-20.8916876625912,-38.2498503406038,
123.138114322854)) ;
#62311 = CARTESIAN_POINT('Ctrl Pts',(-20.5952009193857,-38.0698612602409,
123.192847680362)) ;
#62312 = CARTESIAN_POINT('Ctrl Pts',(-20.8226462971584,-38.259735191517,122.887662089246)) ;
#62313 = CARTESIAN_POINT('Ctrl Pts',(-20.5399668195097,-38.0797461111542,
122.992486951818)) ;
#62314 = CARTESIAN_POINT('Ctrl Pts',(-20.710161993773,-38.2697371476858,122.650150261944)) ;
#62315 = CARTESIAN_POINT('Ctrl Pts',(-20.44997835604,-38.089748067323,122.802478099931)) ;
#62316 = CARTESIAN_POINT('Ctrl Pts',(-20.5595370994859,-38.2796557444063,
122.437376954978)) ;
#62317 = CARTESIAN_POINT('Ctrl Pts',(-20.3294778457341,-38.0996666640434,
122.632260578575)) ;
#62318 = CARTESIAN_POINT('Ctrl Pts',(-20.3718806509748,-38.2897025664821,
122.251710845181)) ;
#62319 = CARTESIAN_POINT('Ctrl Pts',(-20.1793517557982,-38.1097134861192,
122.483728389381)) ;
#62320 = CARTESIAN_POINT('Ctrl Pts',(-20.1586361996875,-38.2995768475948,
122.103781930093)) ;
#62321 = CARTESIAN_POINT('Ctrl Pts',(-20.0087562603686,-38.1195877672319,
122.365386632677)) ;
#62322 = CARTESIAN_POINT('Ctrl Pts',(-19.9188009996355,-38.3096310476394,
121.993039914093)) ;
#62323 = CARTESIAN_POINT('Ctrl Pts',(-19.8168874663292,-38.1296419672765,
122.276793896463)) ;
#62324 = CARTESIAN_POINT('Ctrl Pts',(-19.6673495935004,-38.3195264772746,
121.926560229075)) ;
#62325 = CARTESIAN_POINT('Ctrl Pts',(-19.615726790868,-38.1395373969118,122.223611339034)) ;
#62326 = CARTESIAN_POINT('Ctrl Pts',(-19.403909575533,-38.329588105592,121.904328761475)) ;
#62327 = CARTESIAN_POINT('Ctrl Pts',(-19.4049744286583,-38.1495990252291,
122.20582716044)) ;
#62328 = CARTESIAN_POINT('Ctrl Pts',(-19.1462446840125,-38.3394327344219,
121.927632920062)) ;
#62329 = CARTESIAN_POINT('Ctrl Pts',(-19.1988436604768,-38.159443654059,122.224471403124)) ;
#62330 = CARTESIAN_POINT('Ctrl Pts',(-18.8933810810859,-38.3493927820275,
121.99520301882)) ;
#62331 = CARTESIAN_POINT('Ctrl Pts',(-18.9965533361364,-38.1694037016646,
122.278528153739)) ;
#62332 = CARTESIAN_POINT('Ctrl Pts',(-18.6544538829586,-38.3594310882016,
122.106985936773)) ;
#62333 = CARTESIAN_POINT('Ctrl Pts',(-18.8054118480748,-38.1794420078387,
122.367955372878)) ;
#62334 = CARTESIAN_POINT('Ctrl Pts',(-18.4417836193016,-38.3693043876342,
122.255686315727)) ;
#62335 = CARTESIAN_POINT('Ctrl Pts',(-18.6352768308471,-38.1893153072714,
122.486915811868)) ;
#62336 = CARTESIAN_POINT('Ctrl Pts',(-18.254572634365,-38.3793776492205,122.442761738888)) ;
#62337 = CARTESIAN_POINT('Ctrl Pts',(-18.4855083791044,-38.1993885688576,
122.636576970832)) ;
#62338 = CARTESIAN_POINT('Ctrl Pts',(-18.1061577776451,-38.3891978751772,
122.653952116024)) ;
#62339 = CARTESIAN_POINT('Ctrl Pts',(-18.3667778089366,-38.2092087948143,
122.805528675082)) ;
#62340 = CARTESIAN_POINT('Ctrl Pts',(-17.9936243510384,-38.3992769391167,
122.893649468812)) ;
#62341 = CARTESIAN_POINT('Ctrl Pts',(-18.2767515207265,-38.2192878587538,
122.997287189187)) ;
#62342 = CARTESIAN_POINT('Ctrl Pts',(-17.9258375544917,-38.4091270291365,
123.143539427592)) ;
#62343 = CARTESIAN_POINT('Ctrl Pts',(-18.2225229861537,-38.2291379487737,
123.197198298179)) ;
#62344 = CARTESIAN_POINT('Ctrl Pts',(-17.9018026838566,-38.4192057827503,
123.40723841002)) ;
#62345 = CARTESIAN_POINT('Ctrl Pts',(-18.2032956687307,-38.2392167023874,
123.408157924605)) ;
#62346 = CARTESIAN_POINT('Ctrl Pts',(-17.923166969544,-38.4290272500098,123.664509279081)) ;
#62347 = CARTESIAN_POINT('Ctrl Pts',(-18.2203875531494,-38.2490381696469,
123.613973301711)) ;
#62348 = CARTESIAN_POINT('Ctrl Pts',(-17.9900867207186,-38.4390928483674,
123.920355248471)) ;
#62349 = CARTESIAN_POINT('Ctrl Pts',(-18.2739238795727,-38.2591037680045,
123.818650252036)) ;
#62350 = CARTESIAN_POINT('Ctrl Pts',(-18.0987428644432,-38.4489955041421,
124.156888509072)) ;
#62351 = CARTESIAN_POINT('Ctrl Pts',(-18.3608489306835,-38.2690064237792,
124.007875995514)) ;
#62352 = CARTESIAN_POINT('Ctrl Pts',(-18.2488988281451,-38.4590463299717,
124.374113939604)) ;
#62353 = CARTESIAN_POINT('Ctrl Pts',(-18.4809742059933,-38.2790572496089,
124.181656254911)) ;
#62354 = CARTESIAN_POINT('Ctrl Pts',(-18.4311282813033,-38.4689205343106,
124.558922029202)) ;
#62355 = CARTESIAN_POINT('Ctrl Pts',(-18.6267574017553,-38.2889314539477,
124.329501781547)) ;
#62356 = CARTESIAN_POINT('Ctrl Pts',(-18.6468226000741,-38.4789929843497,
124.712247945028)) ;
#62357 = CARTESIAN_POINT('Ctrl Pts',(-18.7993133663225,-38.2990039039868,
124.452162386081)) ;
#62358 = CARTESIAN_POINT('Ctrl Pts',(-18.8800743167778,-38.4888220011232,
124.823318123614)) ;
#62359 = CARTESIAN_POINT('Ctrl Pts',(-18.985913767497,-38.3088329207603,124.54101769674)) ;
#62360 = CARTESIAN_POINT('Ctrl Pts',(-19.1349034186575,-38.498888847038,124.894192497804)) ;
#62361 = CARTESIAN_POINT('Ctrl Pts',(-19.18977742163,-38.3188997666751,124.597717046058)) ;
#62362 = CARTESIAN_POINT('Ctrl Pts',(-19.3936404772055,-38.5087790183398,
124.919135574597)) ;
#62363 = CARTESIAN_POINT('Ctrl Pts',(-19.3967662609791,-38.3287899379769,
124.6176711408)) ;
#62364 = CARTESIAN_POINT('Ctrl Pts',(-19.6554475745632,-38.5187712119636,
124.899143715405)) ;
#62365 = CARTESIAN_POINT('Ctrl Pts',(-19.6062117573264,-38.3387821316008,
124.601677525334)) ;
#62366 = CARTESIAN_POINT('Ctrl Pts',(-19.9090056650285,-38.5287340225871,
124.833945501294)) ;
#62367 = CARTESIAN_POINT('Ctrl Pts',(-19.8090578249638,-38.3487449422242,
124.549518845411)) ;
#62368 = CARTESIAN_POINT('Ctrl Pts',(-20.1462891748571,-38.5386382954305,
124.726937805208)) ;
#62369 = CARTESIAN_POINT('Ctrl Pts',(-19.9988839326754,-38.3586492150676,
124.463912964312)) ;
#62370 = CARTESIAN_POINT('Ctrl Pts',(-20.3646057034677,-38.5486987872351,
124.577884540204)) ;
#62371 = CARTESIAN_POINT('Ctrl Pts',(-20.173537335335,-38.3687097068723,124.344670113735)) ;
#62372 = CARTESIAN_POINT('Ctrl Pts',(-20.549872151261,-38.5585391189074,124.397423633048)) ;
#62373 = CARTESIAN_POINT('Ctrl Pts',(-20.3217496440126,-38.3785500385446,
124.200302203012)) ;
#62374 = CARTESIAN_POINT('Ctrl Pts',(-20.7046268368384,-38.5686021649992,
124.183029887266)) ;
#62375 = CARTESIAN_POINT('Ctrl Pts',(-20.4455536256558,-38.3886130846363,
124.028787005913)) ;
#62376 = CARTESIAN_POINT('Ctrl Pts',(-20.8177037943771,-38.5784962206943,
123.948871113631)) ;
#62377 = CARTESIAN_POINT('Ctrl Pts',(-20.5360148493182,-38.3985071403314,
123.841460727974)) ;
#62378 = CARTESIAN_POINT('Ctrl Pts',(-20.889425745872,-38.5884389210173,123.697654055537)) ;
#62379 = CARTESIAN_POINT('Ctrl Pts',(-20.5933924604119,-38.4084498406544,
123.640487633951)) ;
#62380 = CARTESIAN_POINT('Ctrl Pts',(-20.9166674415414,-38.5984446619449,
123.436101061356)) ;
#62381 = CARTESIAN_POINT('Ctrl Pts',(-20.6151860207473,-38.418455581582,123.431245328084)) ;
#62382 = CARTESIAN_POINT('Ctrl Pts',(-20.8977588227754,-38.6084655724604,
123.173448091062)) ;
#62383 = CARTESIAN_POINT('Ctrl Pts',(-20.6000592553857,-38.4284764920975,
123.221122910589)) ;
#62384 = CARTESIAN_POINT('Ctrl Pts',(-20.8346540510326,-38.6183563079104,
122.921298084122)) ;
#62385 = CARTESIAN_POINT('Ctrl Pts',(-20.5495758458622,-38.4383672275475,
123.019403663293)) ;
#62386 = CARTESIAN_POINT('Ctrl Pts',(-20.7280091756525,-38.6283478486392,
122.68137528438)) ;
#62387 = CARTESIAN_POINT('Ctrl Pts',(-20.4642602954684,-38.4483587682763,
122.827465455942)) ;
#62388 = CARTESIAN_POINT('Ctrl Pts',(-20.5819003598894,-38.6382957090609,
122.46460048107)) ;
#62389 = CARTESIAN_POINT('Ctrl Pts',(-20.3473737456245,-38.458306628698,122.654045845982)) ;
#62390 = CARTESIAN_POINT('Ctrl Pts',(-20.400753356158,-38.6482423782472,122.276140396852)) ;
#62391 = CARTESIAN_POINT('Ctrl Pts',(-20.2024567640308,-38.4682532978843,
122.503277819394)) ;
#62392 = CARTESIAN_POINT('Ctrl Pts',(-20.1873323482229,-38.6582904543828,
122.12067245961)) ;
#62393 = CARTESIAN_POINT('Ctrl Pts',(-20.0317199988072,-38.4783013740199,
122.378903072768)) ;
#62394 = CARTESIAN_POINT('Ctrl Pts',(-19.9549752001431,-38.6681380523884,
122.006738756206)) ;
#62395 = CARTESIAN_POINT('Ctrl Pts',(-19.8458354617128,-38.4881489720256,
122.287756243606)) ;
#62396 = CARTESIAN_POINT('Ctrl Pts',(-19.703727329421,-38.6780997754729,121.933263220706)) ;
#62397 = CARTESIAN_POINT('Ctrl Pts',(-19.6448376844739,-38.49811069511,122.228975335749)) ;
#62398 = CARTESIAN_POINT('Ctrl Pts',(-19.4417254602095,-38.6881284105559,
121.904664952716)) ;
#62399 = CARTESIAN_POINT('Ctrl Pts',(-19.435236168815,-38.508139330193,122.206096194811)) ;
#62400 = CARTESIAN_POINT('Ctrl Pts',(-19.181862671313,-38.6980387188739,121.921702009282)) ;
#62401 = CARTESIAN_POINT('Ctrl Pts',(-19.2273466015253,-38.5180496385111,
122.219725252916)) ;
#62402 = CARTESIAN_POINT('Ctrl Pts',(-18.9280968782032,-38.7079736160098,
121.98309499747)) ;
#62403 = CARTESIAN_POINT('Ctrl Pts',(-19.0243343132026,-38.5279845356469,
122.268838827757)) ;
#62404 = CARTESIAN_POINT('Ctrl Pts',(-18.6864010149185,-38.7180146989524,
122.088952068271)) ;
#62405 = CARTESIAN_POINT('Ctrl Pts',(-18.830977224545,-38.5380256185895,122.353523948551)) ;
#62406 = CARTESIAN_POINT('Ctrl Pts',(-18.4700029594323,-38.7279020417806,
122.232792348805)) ;
#62407 = CARTESIAN_POINT('Ctrl Pts',(-18.6578590879055,-38.5479129614178,
122.468595134658)) ;
#62408 = CARTESIAN_POINT('Ctrl Pts',(-18.2795943518185,-38.73789355672,122.413563464237)) ;
#62409 = CARTESIAN_POINT('Ctrl Pts',(-18.5055317681181,-38.5579044763571,
122.613211332423)) ;
#62410 = CARTESIAN_POINT('Ctrl Pts',(-18.1241690742749,-38.7478449479164,
122.623883939098)) ;
#62411 = CARTESIAN_POINT('Ctrl Pts',(-18.3811911759621,-38.5678558675536,
122.781466905472)) ;
#62412 = CARTESIAN_POINT('Ctrl Pts',(-18.0074429397806,-38.7577774812491,
122.857344924824)) ;
#62413 = CARTESIAN_POINT('Ctrl Pts',(-18.2878097133205,-38.5777884008862,
122.968234824021)) ;
#62414 = CARTESIAN_POINT('Ctrl Pts',(-17.9324451631841,-38.7677746391485,
123.109116894518)) ;
#62415 = CARTESIAN_POINT('Ctrl Pts',(-18.2278106582551,-38.5877855587856,
123.1696520247)) ;
#62416 = CARTESIAN_POINT('Ctrl Pts',(-17.9022350151,-38.777759649312,123.369808873099)) ;
#62417 = CARTESIAN_POINT('Ctrl Pts',(-18.2036416362819,-38.5977705689491,
123.378205317584)) ;
#62418 = CARTESIAN_POINT('Ctrl Pts',(-17.918220476194,-38.7878024758818,123.633203162121)) ;
#62419 = CARTESIAN_POINT('Ctrl Pts',(-18.2164291783058,-38.6078133955189,
123.588920944231)) ;
#62420 = CARTESIAN_POINT('Ctrl Pts',(-17.9778363800637,-38.7976327101868,
123.884601181613)) ;
#62421 = CARTESIAN_POINT('Ctrl Pts',(-18.2641206846296,-38.6176436298239,
123.790038464492)) ;
#62422 = CARTESIAN_POINT('Ctrl Pts',(-18.0826097273411,-38.8077087354214,
124.127718361036)) ;
#62423 = CARTESIAN_POINT('Ctrl Pts',(-18.3479385732616,-38.6277196550586,
123.984532923754)) ;
#62424 = CARTESIAN_POINT('Ctrl Pts',(-18.22472296995,-38.8175609719123,124.344203206639)) ;
#62425 = CARTESIAN_POINT('Ctrl Pts',(-18.4616277604428,-38.6375718915494,
124.157720543777)) ;
#62426 = CARTESIAN_POINT('Ctrl Pts',(-18.4060166292549,-38.8276341783464,
124.537031920896)) ;
#62427 = CARTESIAN_POINT('Ctrl Pts',(-18.6066621150346,-38.6476450979836,
124.311984493962)) ;
#62428 = CARTESIAN_POINT('Ctrl Pts',(-18.6132523458117,-38.8374756878536,
124.691787453132)) ;
#62429 = CARTESIAN_POINT('Ctrl Pts',(-18.7724492132766,-38.6574866074907,
124.435789153201)) ;
#62430 = CARTESIAN_POINT('Ctrl Pts',(-18.8465449135048,-38.8474366346334,
124.810489310294)) ;
#62431 = CARTESIAN_POINT('Ctrl Pts',(-18.9590823935704,-38.6674475542705,
124.530751641621)) ;
#62432 = CARTESIAN_POINT('Ctrl Pts',(-19.0989906357663,-38.8574744634334,
124.886965770252)) ;
#62433 = CARTESIAN_POINT('Ctrl Pts',(-19.1610387331382,-38.6774853830706,
124.591933962578)) ;
#62434 = CARTESIAN_POINT('Ctrl Pts',(-19.3565960865171,-38.8673487731879,
124.918417832295)) ;
#62435 = CARTESIAN_POINT('Ctrl Pts',(-19.3671221354591,-38.687359692825,124.617096782375)) ;
#62436 = CARTESIAN_POINT('Ctrl Pts',(-19.620809364879,-38.8774184708611,124.90438027923)) ;
#62437 = CARTESIAN_POINT('Ctrl Pts',(-19.5784931043603,-38.6974293904982,
124.605867998489)) ;
#62438 = CARTESIAN_POINT('Ctrl Pts',(-19.8726090818737,-38.8872519421485,
124.846200103951)) ;
#62439 = CARTESIAN_POINT('Ctrl Pts',(-19.779932174487,-38.7072628617856,124.559325358216)) ;
#62440 = CARTESIAN_POINT('Ctrl Pts',(-20.1154997478902,-38.8972815886784,
124.743876964785)) ;
#62441 = CARTESIAN_POINT('Ctrl Pts',(-19.9742453375795,-38.7172925083155,
124.477468165888)) ;
#62442 = CARTESIAN_POINT('Ctrl Pts',(-20.336613329244,-38.9073161030058,124.600184240686)) ;
#62443 = CARTESIAN_POINT('Ctrl Pts',(-20.1511369670628,-38.7273270226429,
124.362515034824)) ;
#62444 = CARTESIAN_POINT('Ctrl Pts',(-20.525819561072,-38.9171413884767,124.424489904963)) ;
#62445 = CARTESIAN_POINT('Ctrl Pts',(-20.3025021660536,-38.7371523081138,
124.221961312577)) ;
#62446 = CARTESIAN_POINT('Ctrl Pts',(-20.684908264894,-38.9271456300252,124.215225042705)) ;
#62447 = CARTESIAN_POINT('Ctrl Pts',(-20.4297743088031,-38.7471565496623,
124.054550406334)) ;
#62448 = CARTESIAN_POINT('Ctrl Pts',(-20.8049240326916,-38.9371282751043,
123.981897983475)) ;
#62449 = CARTESIAN_POINT('Ctrl Pts',(-20.5257881879668,-38.7571391947414,
123.867889603181)) ;
#62450 = CARTESIAN_POINT('Ctrl Pts',(-20.8827806719574,-38.9471734721958,
123.729693087427)) ;
#62451 = CARTESIAN_POINT('Ctrl Pts',(-20.5880749231069,-38.7671843918329,
123.666125997018)) ;
#62452 = CARTESIAN_POINT('Ctrl Pts',(-20.915373446422,-38.9569965879559,123.473607472964)) ;
#62453 = CARTESIAN_POINT('Ctrl Pts',(-20.6141505414293,-38.7770075075931,
123.461258688752)) ;
#62454 = CARTESIAN_POINT('Ctrl Pts',(-20.9034051256726,-38.9670311997562,
123.210183840102)) ;
#62455 = CARTESIAN_POINT('Ctrl Pts',(-20.6045775434522,-38.7870421193933,
123.250519622744)) ;
#62456 = CARTESIAN_POINT('Ctrl Pts',(-20.8452141569218,-38.9770562085294,
122.953236014192)) ;
#62457 = CARTESIAN_POINT('Ctrl Pts',(-20.5580262508377,-38.7970671281665,
123.044961006179)) ;
#62458 = CARTESIAN_POINT('Ctrl Pts',(-20.7455751866615,-38.9869081333709,
122.714273478739)) ;
#62459 = CARTESIAN_POINT('Ctrl Pts',(-20.4783168903162,-38.8069190530081,
122.853791094508)) ;
#62460 = CARTESIAN_POINT('Ctrl Pts',(-20.6043472152323,-38.9968990716936,
122.492979055733)) ;
#62461 = CARTESIAN_POINT('Ctrl Pts',(-20.3653360237467,-38.8169099913308,
122.676754754454)) ;
#62462 = CARTESIAN_POINT('Ctrl Pts',(-20.4282184151075,-39.0068170568401,
122.300819554238)) ;
#62463 = CARTESIAN_POINT('Ctrl Pts',(-20.2244345676972,-38.8268279764772,
122.523026321021)) ;
#62464 = CARTESIAN_POINT('Ctrl Pts',(-20.2191838999621,-39.0168451577356,
122.140380206335)) ;
#62465 = CARTESIAN_POINT('Ctrl Pts',(-20.0572079946836,-38.8368560773727,
122.394673443587)) ;
#62466 = CARTESIAN_POINT('Ctrl Pts',(-19.988823563365,-39.0267303986782,122.020299045368)) ;
#62467 = CARTESIAN_POINT('Ctrl Pts',(-19.8729210602191,-38.8467413183153,
122.298607226252)) ;
#62468 = CARTESIAN_POINT('Ctrl Pts',(-19.7387023265392,-39.0367195116448,
121.940602617723)) ;
#62469 = CARTESIAN_POINT('Ctrl Pts',(-19.6728247564175,-38.8567304312819,
122.234848346961)) ;
#62470 = CARTESIAN_POINT('Ctrl Pts',(-19.477101074724,-39.0467615759856,121.905935512538)) ;
#62471 = CARTESIAN_POINT('Ctrl Pts',(-19.4635439135823,-38.8667724956227,
122.207112896485)) ;
#62472 = CARTESIAN_POINT('Ctrl Pts',(-19.2190051557775,-39.0565907773901,
121.91648957557)) ;
#62473 = CARTESIAN_POINT('Ctrl Pts',(-19.2570678745084,-38.8766016970272,
122.215554268652)) ;
#62474 = CARTESIAN_POINT('Ctrl Pts',(-18.96201942726,-39.0665976181483,121.972124528539)) ;
#62475 = CARTESIAN_POINT('Ctrl Pts',(-19.0514789416566,-38.8866085377854,
122.260060324957)) ;
#62476 = CARTESIAN_POINT('Ctrl Pts',(-18.7190580246925,-39.0765851423402,
122.071516726106)) ;
#62477 = CARTESIAN_POINT('Ctrl Pts',(-18.8571092146858,-38.8965960619773,
122.339572267112)) ;
#62478 = CARTESIAN_POINT('Ctrl Pts',(-18.4962632862226,-39.0866147881488,
122.21229469891)) ;
#62479 = CARTESIAN_POINT('Ctrl Pts',(-18.6788723982506,-38.9066257077859,
122.452193065279)) ;
#62480 = CARTESIAN_POINT('Ctrl Pts',(-18.3040742602747,-39.0964888188876,
122.386670421096)) ;
#62481 = CARTESIAN_POINT('Ctrl Pts',(-18.5251202815215,-38.9164997385247,
122.591691852851)) ;
#62482 = CARTESIAN_POINT('Ctrl Pts',(-18.142850412755,-39.1064881417517,122.594116058602)) ;
#62483 = CARTESIAN_POINT('Ctrl Pts',(-18.3961396994837,-38.9264990613888,
122.757647081838)) ;
#62484 = CARTESIAN_POINT('Ctrl Pts',(-18.0209136491181,-39.1163989773273,
122.824305926561)) ;
#62485 = CARTESIAN_POINT('Ctrl Pts',(-18.2985886964444,-38.9364098969644,
122.941797703191)) ;
#62486 = CARTESIAN_POINT('Ctrl Pts',(-17.939756418586,-39.1264532253013,123.075703741562)) ;
#62487 = CARTESIAN_POINT('Ctrl Pts',(-18.2336609864209,-38.9464641449384,
123.142915426417)) ;
#62488 = CARTESIAN_POINT('Ctrl Pts',(-17.9038739773889,-39.136311969564,123.332330097261)) ;
#62489 = CARTESIAN_POINT('Ctrl Pts',(-18.2049530965617,-38.9563228892011,
123.348215715669)) ;
#62490 = CARTESIAN_POINT('Ctrl Pts',(-17.9131303556298,-39.146380055637,123.596708290308)) ;
#62491 = CARTESIAN_POINT('Ctrl Pts',(-18.2123561545412,-38.9663909752741,
123.559718464088)) ;
#62492 = CARTESIAN_POINT('Ctrl Pts',(-17.9670211523186,-39.1562355388165,
123.850053708663)) ;
#62493 = CARTESIAN_POINT('Ctrl Pts',(-18.2554666875822,-38.9762464584537,
123.762394736116)) ;
#62494 = CARTESIAN_POINT('Ctrl Pts',(-18.0647131560755,-39.1662303846107,
124.093854715308)) ;
#62495 = CARTESIAN_POINT('Ctrl Pts',(-18.3336182833703,-38.9862413042478,
123.957436260119)) ;
#62496 = CARTESIAN_POINT('Ctrl Pts',(-18.2042478281487,-39.1762616802733,
124.31751521221)) ;
#62497 = CARTESIAN_POINT('Ctrl Pts',(-18.4452442635705,-38.9962725999104,
124.136365752348)) ;
#62498 = CARTESIAN_POINT('Ctrl Pts',(-18.3772981542013,-39.1861282235631,
124.510610102635)) ;
#62499 = CARTESIAN_POINT('Ctrl Pts',(-18.5836826763418,-39.0061391432003,
124.290842767909)) ;
#62500 = CARTESIAN_POINT('Ctrl Pts',(-18.5834523133935,-39.1961156193265,
124.672993813445)) ;
#62501 = CARTESIAN_POINT('Ctrl Pts',(-18.7486045943314,-39.0161265389636,
124.420751367233)) ;
#62502 = CARTESIAN_POINT('Ctrl Pts',(-18.8136849281219,-39.2060606600565,
124.796745724654)) ;
#62503 = CARTESIAN_POINT('Ctrl Pts',(-18.9327894986595,-39.0260715796936,
124.519754710555)) ;
#62504 = CARTESIAN_POINT('Ctrl Pts',(-19.0643744385041,-39.2161051662732,
124.879300115833)) ;
#62505 = CARTESIAN_POINT('Ctrl Pts',(-19.1333404484933,-39.0361160859103,
124.585800271082)) ;
#62506 = CARTESIAN_POINT('Ctrl Pts',(-19.3209006976939,-39.2259686724105,
124.916631731165)) ;
#62507 = CARTESIAN_POINT('Ctrl Pts',(-19.3385608066028,-39.0459795920477,
124.61566765999)) ;
#62508 = CARTESIAN_POINT('Ctrl Pts',(-19.5833595972504,-39.2359615332466,
124.909220187151)) ;
#62509 = CARTESIAN_POINT('Ctrl Pts',(-19.5485279119773,-39.0559724528837,
124.609740630112)) ;
#62510 = CARTESIAN_POINT('Ctrl Pts',(-19.838927622203,-39.2458877269655,124.856807196961)) ;
#62511 = CARTESIAN_POINT('Ctrl Pts',(-19.7529826014343,-39.0658986466027,
124.567812433635)) ;
#62512 = CARTESIAN_POINT('Ctrl Pts',(-20.0837340012441,-39.2559066529981,
124.759990302351)) ;
#62513 = CARTESIAN_POINT('Ctrl Pts',(-19.9488284801805,-39.0759175726352,
124.490360989848)) ;
#62514 = CARTESIAN_POINT('Ctrl Pts',(-20.3058732169499,-39.2658216523657,
124.623740322462)) ;
#62515 = CARTESIAN_POINT('Ctrl Pts',(-20.1265408661882,-39.0858325720028,
124.381362989768)) ;
#62516 = CARTESIAN_POINT('Ctrl Pts',(-20.5036398438425,-39.275876423923,124.448561261991)) ;
#62517 = CARTESIAN_POINT('Ctrl Pts',(-20.2847556360216,-39.0958873435601,
124.241221409002)) ;
#62518 = CARTESIAN_POINT('Ctrl Pts',(-20.6649559413948,-39.2857353862206,
124.245785908657)) ;
#62519 = CARTESIAN_POINT('Ctrl Pts',(-20.4138101229452,-39.1057463058577,
124.079002680325)) ;
#62520 = CARTESIAN_POINT('Ctrl Pts',(-20.7907073337683,-39.2957296300584,
124.015257630016)) ;
#62521 = CARTESIAN_POINT('Ctrl Pts',(-20.5144131818237,-39.1157405496955,
123.894581187682)) ;
#62522 = CARTESIAN_POINT('Ctrl Pts',(-20.8740852786362,-39.3056548594826,
123.76807558954)) ;
#62523 = CARTESIAN_POINT('Ctrl Pts',(-20.5811176317263,-39.1256657791198,
123.696836372389)) ;
#62524 = CARTESIAN_POINT('Ctrl Pts',(-20.9136831801555,-39.3156828233741,
123.507578576389)) ;
#62525 = CARTESIAN_POINT('Ctrl Pts',(-20.6127981700986,-39.1356937430112,
123.488439150127)) ;
#62526 = CARTESIAN_POINT('Ctrl Pts',(-20.9078028794062,-39.3255690830045,
123.247805458002)) ;
#62527 = CARTESIAN_POINT('Ctrl Pts',(-20.6080961812906,-39.1455800026416,
123.280620698185)) ;
#62528 = CARTESIAN_POINT('Ctrl Pts',(-20.8563083055305,-39.3356008460823,
122.989304179214)) ;
#62529 = CARTESIAN_POINT('Ctrl Pts',(-20.5669027458931,-39.1556117657195,
123.07381928786)) ;
#62530 = CARTESIAN_POINT('Ctrl Pts',(-20.7623452754649,-39.3454824723765,
122.747171858518)) ;
#62531 = CARTESIAN_POINT('Ctrl Pts',(-20.4917344390515,-39.1654933920136,
122.880112663831)) ;
#62532 = CARTESIAN_POINT('Ctrl Pts',(-20.6254181998426,-39.3555442418626,
122.521020260046)) ;
#62533 = CARTESIAN_POINT('Ctrl Pts',(-20.3821947440194,-39.1755551614998,
122.699190275451)) ;
#62534 = CARTESIAN_POINT('Ctrl Pts',(-20.4548438165245,-39.3654021093581,
122.326007790114)) ;
#62535 = CARTESIAN_POINT('Ctrl Pts',(-20.2457369371644,-39.1854130289952,
122.543178822639)) ;
#62536 = CARTESIAN_POINT('Ctrl Pts',(-20.2506752048756,-39.3753937344755,
122.160957633342)) ;
#62537 = CARTESIAN_POINT('Ctrl Pts',(-20.0824034879034,-39.1954046541126,
122.41113697398)) ;
#62538 = CARTESIAN_POINT('Ctrl Pts',(-20.0221459359135,-39.3853305335837,
122.034581725534)) ;
#62539 = CARTESIAN_POINT('Ctrl Pts',(-19.8995811564876,-39.2053414532208,
122.310034285515)) ;
#62540 = CARTESIAN_POINT('Ctrl Pts',(-19.7739378812529,-39.3953213631411,
121.948989845805)) ;
#62541 = CARTESIAN_POINT('Ctrl Pts',(-19.7010154745598,-39.2153322827782,
122.241558685224)) ;
#62542 = CARTESIAN_POINT('Ctrl Pts',(-19.5137457792809,-39.4053445988542,
121.90796320333)) ;
#62543 = CARTESIAN_POINT('Ctrl Pts',(-19.4928622206853,-39.2253555184914,
122.208735172086)) ;
#62544 = CARTESIAN_POINT('Ctrl Pts',(-19.2537240353539,-39.4152409468834,
121.912457737756)) ;
#62545 = CARTESIAN_POINT('Ctrl Pts',(-19.284844725392,-39.2352518665205,122.212328561207)) ;
#62546 = CARTESIAN_POINT('Ctrl Pts',(-18.9959028450578,-39.4252305093859,
121.961952758598)) ;
#62547 = CARTESIAN_POINT('Ctrl Pts',(-19.0785873514741,-39.245241429023,122.251922433717)) ;
#62548 = CARTESIAN_POINT('Ctrl Pts',(-18.7495601440801,-39.4352708170704,
122.056425100597)) ;
#62549 = CARTESIAN_POINT('Ctrl Pts',(-18.8815126089877,-39.2552817367076,
122.327498082193)) ;
#62550 = CARTESIAN_POINT('Ctrl Pts',(-18.5275396488835,-39.4451131204176,
122.189149904879)) ;
#62551 = CARTESIAN_POINT('Ctrl Pts',(-18.7038944864329,-39.2651240400548,
122.433676503167)) ;
#62552 = CARTESIAN_POINT('Ctrl Pts',(-18.3281491908963,-39.4551368286967,
122.361220908179)) ;
#62553 = CARTESIAN_POINT('Ctrl Pts',(-18.544382291125,-39.2751477483338,122.571330259957)) ;
#62554 = CARTESIAN_POINT('Ctrl Pts',(-18.1083641388758,-39.4683590061644,
122.630415698339)) ;
#62555 = CARTESIAN_POINT('Ctrl Pts',(-18.3685442466138,-39.2883699258015,
122.786691064912)) ;
#62556 = CARTESIAN_POINT('Ctrl Pts',(-17.9628051141578,-39.4816515912237,
122.952220149241)) ;
#62557 = CARTESIAN_POINT('Ctrl Pts',(-18.2520900201739,-39.3016625108608,
123.0441667538)) ;
#62558 = CARTESIAN_POINT('Ctrl Pts',(-17.9061735340481,-39.4949364471453,
123.296785705772)) ;
#62559 = CARTESIAN_POINT('Ctrl Pts',(-18.2067947639732,-39.3149473667824,
123.319772623799)) ;
#62560 = CARTESIAN_POINT('Ctrl Pts',(-17.9090249687646,-39.5049086743181,
123.558791097656)) ;
#62561 = CARTESIAN_POINT('Ctrl Pts',(-18.2090712941876,-39.3249195939552,
123.529386330433)) ;
#62562 = CARTESIAN_POINT('Ctrl Pts',(-17.956586488933,-39.5148172907571,123.814831513861)) ;
#62563 = CARTESIAN_POINT('Ctrl Pts',(-18.2471189493616,-39.3348282103942,
123.734216637461)) ;
#62564 = CARTESIAN_POINT('Ctrl Pts',(-18.0492936761947,-39.5248704961408,
124.062190998726)) ;
#62565 = CARTESIAN_POINT('Ctrl Pts',(-18.321283555231,-39.3448814157779,123.93210607372)) ;
#62566 = CARTESIAN_POINT('Ctrl Pts',(-18.1809125138042,-39.5347356299011,
124.285566478985)) ;
#62567 = CARTESIAN_POINT('Ctrl Pts',(-18.4265731937417,-39.3547465495382,
124.110805222555)) ;
#62568 = CARTESIAN_POINT('Ctrl Pts',(-18.4080910892468,-39.5480746875274,
124.552496993327)) ;
#62569 = CARTESIAN_POINT('Ctrl Pts',(-18.6083336756882,-39.3680856071645,
124.324363766932)) ;
#62570 = CARTESIAN_POINT('Ctrl Pts',(-18.7706176279161,-39.5646438748606,
124.802631868927)) ;
#62571 = CARTESIAN_POINT('Ctrl Pts',(-18.8983168389849,-39.3846547944977,
124.524458515266)) ;
#62572 = CARTESIAN_POINT('Ctrl Pts',(-19.1984775012585,-39.5812890147116,
124.914837427631)) ;
#62573 = CARTESIAN_POINT('Ctrl Pts',(-19.2406669700555,-39.4012999343487,
124.614238150144)) ;
#62574 = CARTESIAN_POINT('Ctrl Pts',(-19.5473160626107,-39.594561317185,124.912945050677)) ;
#62575 = CARTESIAN_POINT('Ctrl Pts',(-19.5196867817272,-39.4145722368221,
124.6127192198)) ;
#62576 = CARTESIAN_POINT('Ctrl Pts',(-19.8054003621908,-39.6045422806326,
124.866324423649)) ;
#62577 = CARTESIAN_POINT('Ctrl Pts',(-19.7261653890183,-39.4245532002698,
124.575425593905)) ;
#62578 = CARTESIAN_POINT('Ctrl Pts',(-20.0506098849888,-39.6144841127019,
124.776085831053)) ;
#62579 = CARTESIAN_POINT('Ctrl Pts',(-19.9223292887017,-39.4344950323391,
124.503237755022)) ;
#62580 = CARTESIAN_POINT('Ctrl Pts',(-20.3531494019142,-39.6278036819174,
124.600140541929)) ;
#62581 = CARTESIAN_POINT('Ctrl Pts',(-20.1643723390079,-39.4478146015545,
124.362474577121)) ;
#62582 = CARTESIAN_POINT('Ctrl Pts',(-20.6634916788334,-39.6443338368501,
124.289002055755)) ;
#62583 = CARTESIAN_POINT('Ctrl Pts',(-20.4126378083465,-39.4643447564872,
124.11357553459)) ;
#62584 = CARTESIAN_POINT('Ctrl Pts',(-20.8878880488286,-39.6643555623422,
123.80663214029)) ;
#62585 = CARTESIAN_POINT('Ctrl Pts',(-20.5921614310952,-39.4843664819793,
123.727677884978)) ;
#62586 = CARTESIAN_POINT('Ctrl Pts',(-20.9340458411,-39.684166958949,123.281975948021)) ;
#62587 = CARTESIAN_POINT('Ctrl Pts',(-20.6290900257531,-39.5041778785861,
123.307952866676)) ;
#62588 = CARTESIAN_POINT('Ctrl Pts',(-20.7981256340549,-39.7041522076579,
122.768612564933)) ;
#62589 = CARTESIAN_POINT('Ctrl Pts',(-20.5203568572082,-39.524163127295,122.897261068082)) ;
#62590 = CARTESIAN_POINT('Ctrl Pts',(-20.4961474222789,-39.7240462702938,
122.334473379802)) ;
#62591 = CARTESIAN_POINT('Ctrl Pts',(-20.2787761236903,-39.5440571899309,
122.549947532651)) ;
#62592 = CARTESIAN_POINT('Ctrl Pts',(-20.0638627446628,-39.7439779494674,
122.028277249774)) ;
#62593 = CARTESIAN_POINT('Ctrl Pts',(-19.9329493834132,-39.5639888691045,
122.304988270493)) ;
#62594 = CARTESIAN_POINT('Ctrl Pts',(-19.552105313075,-39.7639420039394,121.888081012904)) ;
#62595 = CARTESIAN_POINT('Ctrl Pts',(-19.523543821286,-39.5839529235765,122.192828836387)) ;
#62596 = CARTESIAN_POINT('Ctrl Pts',(-19.0253744540023,-39.7838229057023,
121.930361827111)) ;
#62597 = CARTESIAN_POINT('Ctrl Pts',(-19.1021578729861,-39.6038338253394,
122.226651390255)) ;
#62598 = CARTESIAN_POINT('Ctrl Pts',(-18.5431348409718,-39.8037615673107,
122.150015941344)) ;
#62599 = CARTESIAN_POINT('Ctrl Pts',(-18.7163648705892,-39.6237724869478,
122.402373239355)) ;
#62600 = CARTESIAN_POINT('Ctrl Pts',(-18.1655278033416,-39.823658092566,122.520218221338)) ;
#62601 = CARTESIAN_POINT('Ctrl Pts',(-18.4142773121928,-39.6436690122031,
122.698534606389)) ;
#62602 = CARTESIAN_POINT('Ctrl Pts',(-17.9361396477719,-39.8435531310203,
122.99666905445)) ;
#62603 = CARTESIAN_POINT('Ctrl Pts',(-18.2307652509137,-39.6635640506575,
123.079695848156)) ;
#62604 = CARTESIAN_POINT('Ctrl Pts',(-17.883006132507,-39.8635169543264,123.524568225147)) ;
#62605 = CARTESIAN_POINT('Ctrl Pts',(-18.1882574093228,-39.6835278739635,
123.502015493419)) ;
#62606 = CARTESIAN_POINT('Ctrl Pts',(-18.0122595317287,-39.8833910784555,
124.036771136618)) ;
#62607 = CARTESIAN_POINT('Ctrl Pts',(-18.2916598855057,-39.7034019980926,
123.911779438151)) ;
#62608 = CARTESIAN_POINT('Ctrl Pts',(-18.3096308451413,-39.9033661541827,
124.476606505038)) ;
#62609 = CARTESIAN_POINT('Ctrl Pts',(-18.5295569287949,-39.7233770738199,
124.263648070586)) ;
#62610 = CARTESIAN_POINT('Ctrl Pts',(-18.7392016865621,-39.9233197235393,
124.787593898478)) ;
#62611 = CARTESIAN_POINT('Ctrl Pts',(-18.8732138714757,-39.7433306431764,
124.512438635764)) ;
#62612 = CARTESIAN_POINT('Ctrl Pts',(-19.245888696071,-39.9431576337272,124.933442271979)) ;
#62613 = CARTESIAN_POINT('Ctrl Pts',(-19.278565608068,-39.7631685533643,124.629117598788)) ;
#62614 = CARTESIAN_POINT('Ctrl Pts',(-19.7756254405552,-39.9631334622981,
124.897944226643)) ;
#62615 = CARTESIAN_POINT('Ctrl Pts',(-19.702355195912,-39.7831443819352,124.600718333619)) ;
#62616 = CARTESIAN_POINT('Ctrl Pts',(-20.259776971264,-39.9830515070084,124.68390775287)) ;
#62617 = CARTESIAN_POINT('Ctrl Pts',(-20.0896770292724,-39.8030624266455,
124.429488092088)) ;
#62618 = CARTESIAN_POINT('Ctrl Pts',(-20.6419438140887,-40.002921752796,124.319255201488)) ;
#62619 = CARTESIAN_POINT('Ctrl Pts',(-20.3954104744399,-39.8229326724332,
124.137764014872)) ;
#62620 = CARTESIAN_POINT('Ctrl Pts',(-20.8780281936789,-40.0229707558956,
123.841688417852)) ;
#62621 = CARTESIAN_POINT('Ctrl Pts',(-20.584276553681,-39.8429816755327,123.755710427859)) ;
#62622 = CARTESIAN_POINT('Ctrl Pts',(-20.9367938161444,-40.0427499971364,
123.319128562746)) ;
#62623 = CARTESIAN_POINT('Ctrl Pts',(-20.6312875872331,-39.8627609167736,
123.337660188172)) ;
#62624 = CARTESIAN_POINT('Ctrl Pts',(-20.8129964068986,-40.0627800608453,
122.801479468829)) ;
#62625 = CARTESIAN_POINT('Ctrl Pts',(-20.5322475926192,-39.8827909804824,
122.92354173138)) ;
#62626 = CARTESIAN_POINT('Ctrl Pts',(-20.5213204071413,-40.0826623457473,
122.360731282124)) ;
#62627 = CARTESIAN_POINT('Ctrl Pts',(-20.2989045254631,-39.9026732653844,
122.570943408871)) ;
#62628 = CARTESIAN_POINT('Ctrl Pts',(-20.0977276287473,-40.1025446466403,
122.044872252735)) ;
#62629 = CARTESIAN_POINT('Ctrl Pts',(-19.9600279171563,-39.9225555662774,
122.31825773152)) ;
#62630 = CARTESIAN_POINT('Ctrl Pts',(-19.5891047472004,-40.1225277562586,
121.891899364651)) ;
#62631 = CARTESIAN_POINT('Ctrl Pts',(-19.5531287369363,-39.9425386758957,
122.195882009548)) ;
#62632 = CARTESIAN_POINT('Ctrl Pts',(-19.0612514000338,-40.1424181516365,
121.921603035673)) ;
#62633 = CARTESIAN_POINT('Ctrl Pts',(-19.1308454119986,-39.9624290712736,
122.219647817995)) ;
#62634 = CARTESIAN_POINT('Ctrl Pts',(-18.5748477163413,-40.1623149416708,
122.128947492388)) ;
#62635 = CARTESIAN_POINT('Ctrl Pts',(-18.7417230650517,-39.9823258613079,
122.385526589855)) ;
#62636 = CARTESIAN_POINT('Ctrl Pts',(-18.1875342172556,-40.1822319956124,
122.489841093225)) ;
#62637 = CARTESIAN_POINT('Ctrl Pts',(-18.4318742437841,-40.0022429152495,
122.674244288826)) ;
#62638 = CARTESIAN_POINT('Ctrl Pts',(-17.9457158456868,-40.2022355438159,
122.963405930333)) ;
#62639 = CARTESIAN_POINT('Ctrl Pts',(-18.2384227101736,-40.022246463453,123.05309765344)) ;
#62640 = CARTESIAN_POINT('Ctrl Pts',(-17.8810209349113,-40.2221738374685,
123.489343815251)) ;
#62641 = CARTESIAN_POINT('Ctrl Pts',(-18.1866699625709,-40.0421847571056,
123.473848687239)) ;
#62642 = CARTESIAN_POINT('Ctrl Pts',(-17.9977400537545,-40.2419953249014,
124.003081008329)) ;
#62643 = CARTESIAN_POINT('Ctrl Pts',(-18.2800496556778,-40.0620062445386,
123.884838604969)) ;
#62644 = CARTESIAN_POINT('Ctrl Pts',(-18.2845312148424,-40.2619737178923,
124.449892679348)) ;
#62645 = CARTESIAN_POINT('Ctrl Pts',(-18.5094838885054,-40.0819846375294,
124.242285370891)) ;
#62646 = CARTESIAN_POINT('Ctrl Pts',(-18.7051945465058,-40.281872099506,124.770559205405)) ;
#62647 = CARTESIAN_POINT('Ctrl Pts',(-18.8460248106455,-40.1018830191431,
124.498817503231)) ;
#62648 = CARTESIAN_POINT('Ctrl Pts',(-19.1255703487818,-40.2984550302359,
124.902674539461)) ;
#62649 = CARTESIAN_POINT('Ctrl Pts',(-19.1823032071528,-40.118465949873,124.604500927526)) ;
#62650 = CARTESIAN_POINT('Ctrl Pts',(-19.4741295857763,-40.3117292658247,
124.917986772684)) ;
#62651 = CARTESIAN_POINT('Ctrl Pts',(-19.461172160329,-40.1317401854619,124.616752617202)) ;
#62652 = CARTESIAN_POINT('Ctrl Pts',(-19.7358425463294,-40.3217756832809,
124.883469686194)) ;
#62653 = CARTESIAN_POINT('Ctrl Pts',(-19.6705356336101,-40.1417866029181,
124.589137624141)) ;
#62654 = CARTESIAN_POINT('Ctrl Pts',(-19.9826774778135,-40.3316209085002,
124.805881778584)) ;
#62655 = CARTESIAN_POINT('Ctrl Pts',(-19.8680131815929,-40.1516318281373,
124.527058888594)) ;
#62656 = CARTESIAN_POINT('Ctrl Pts',(-20.293982933582,-40.3449558795396,124.645032731908)) ;
#62657 = CARTESIAN_POINT('Ctrl Pts',(-20.117012406976,-40.1649667991767,124.398409704518)) ;
#62658 = CARTESIAN_POINT('Ctrl Pts',(-20.6198884114383,-40.3615387363322,
124.348182656226)) ;
#62659 = CARTESIAN_POINT('Ctrl Pts',(-20.3777873723934,-40.1815496559694,
124.160882593775)) ;
#62660 = CARTESIAN_POINT('Ctrl Pts',(-20.8256972515988,-40.3781817386816,
123.956743051151)) ;
#62661 = CARTESIAN_POINT('Ctrl Pts',(-20.5424028051594,-40.1981926583188,
123.84776904717)) ;
#62662 = CARTESIAN_POINT('Ctrl Pts',(-20.9027340822747,-40.3914254697133,
123.617264907875)) ;
#62663 = CARTESIAN_POINT('Ctrl Pts',(-20.6040438274232,-40.2114363893504,
123.576158441857)) ;
#62664 = CARTESIAN_POINT('Ctrl Pts',(-20.9155780417739,-40.4014798643879,
123.353409333891)) ;
#62665 = CARTESIAN_POINT('Ctrl Pts',(-20.6143139039399,-40.221490784025,123.365079497654)) ;
#62666 = CARTESIAN_POINT('Ctrl Pts',(-20.8834362366564,-40.4113209257765,
123.096754250363)) ;
#62667 = CARTESIAN_POINT('Ctrl Pts',(-20.5885990123171,-40.2313318454136,
123.159754036855)) ;
#62668 = CARTESIAN_POINT('Ctrl Pts',(-20.805749324976,-40.421387150133,122.843935791926)) ;
#62669 = CARTESIAN_POINT('Ctrl Pts',(-20.5264471820404,-40.2413980697701,
122.957500455723)) ;
#62670 = CARTESIAN_POINT('Ctrl Pts',(-20.6874567828035,-40.4312677630526,
122.61274782886)) ;
#62671 = CARTESIAN_POINT('Ctrl Pts',(-20.431811178883,-40.2512786826897,122.77255090532)) ;
#62672 = CARTESIAN_POINT('Ctrl Pts',(-20.5294818312083,-40.4412610562122,
122.403016184153)) ;
#62673 = CARTESIAN_POINT('Ctrl Pts',(-20.3054294355456,-40.2612719758493,
122.604767012198)) ;
#62674 = CARTESIAN_POINT('Ctrl Pts',(-20.3383061144584,-40.4512120644359,
122.224524733115)) ;
#62675 = CARTESIAN_POINT('Ctrl Pts',(-20.1524873435744,-40.271222984073,122.461975496637)) ;
#62676 = CARTESIAN_POINT('Ctrl Pts',(-20.116847152072,-40.4612605787978,122.080752823443)) ;
#62677 = CARTESIAN_POINT('Ctrl Pts',(-19.9753190159199,-40.281271498435,122.34695989764)) ;
#62678 = CARTESIAN_POINT('Ctrl Pts',(-19.8788615309096,-40.4711020848605,
121.979450513905)) ;
#62679 = CARTESIAN_POINT('Ctrl Pts',(-19.7849296059222,-40.2911130044976,
122.265920106906)) ;
#62680 = CARTESIAN_POINT('Ctrl Pts',(-19.623405666514,-40.4810877374902,121.919608247054)) ;
#62681 = CARTESIAN_POINT('Ctrl Pts',(-19.5805644621411,-40.3010986571273,
122.218048512511)) ;
#62682 = CARTESIAN_POINT('Ctrl Pts',(-19.3625879444289,-40.4910267463351,
121.904994593026)) ;
#62683 = CARTESIAN_POINT('Ctrl Pts',(-19.3719102147239,-40.3110376659722,
122.206359844841)) ;
#62684 = CARTESIAN_POINT('Ctrl Pts',(-19.1006071741867,-40.5010676716281,
121.936267236992)) ;
#62685 = CARTESIAN_POINT('Ctrl Pts',(-19.1623259175616,-40.3210785912652,
122.231380198729)) ;
#62686 = CARTESIAN_POINT('Ctrl Pts',(-18.8517347176778,-40.510957993383,122.011275192603)) ;
#62687 = CARTESIAN_POINT('Ctrl Pts',(-18.9632286807816,-40.3309689130201,
122.291388701103)) ;
#62688 = CARTESIAN_POINT('Ctrl Pts',(-18.6170528304471,-40.5209539667164,
122.129240595666)) ;
#62689 = CARTESIAN_POINT('Ctrl Pts',(-18.775484242593,-40.3409648863536,122.385763008815)) ;
#62690 = CARTESIAN_POINT('Ctrl Pts',(-18.4077408551288,-40.5308853662985,
122.285152304524)) ;
#62691 = CARTESIAN_POINT('Ctrl Pts',(-18.6080360869343,-40.3508962859356,
122.510494122467)) ;
#62692 = CARTESIAN_POINT('Ctrl Pts',(-18.2270702114119,-40.5408909067755,
122.476201697503)) ;
#62693 = CARTESIAN_POINT('Ctrl Pts',(-18.463501244713,-40.3609018264127,122.663335132753)) ;
#62694 = CARTESIAN_POINT('Ctrl Pts',(-18.0823350470843,-40.5509238907068,
122.696568451517)) ;
#62695 = CARTESIAN_POINT('Ctrl Pts',(-18.3477150174073,-40.370934810344,122.839629750178)) ;
#62696 = CARTESIAN_POINT('Ctrl Pts',(-17.9794720037659,-40.5607795215337,
122.934283776559)) ;
#62697 = CARTESIAN_POINT('Ctrl Pts',(-18.2654267150485,-40.3807904411708,
123.029802727258)) ;
#62698 = CARTESIAN_POINT('Ctrl Pts',(-17.9182550889907,-40.5707789237268,
123.189781090327)) ;
#62699 = CARTESIAN_POINT('Ctrl Pts',(-18.2164553726085,-40.390789843364,123.234201028577)) ;
#62700 = CARTESIAN_POINT('Ctrl Pts',(-17.9021932202681,-40.5806733930879,
123.44934937898)) ;
#62701 = CARTESIAN_POINT('Ctrl Pts',(-18.2036080982215,-40.400684312725,123.441855585745)) ;
#62702 = CARTESIAN_POINT('Ctrl Pts',(-17.932011300945,-40.5907365072521,123.712065167649)) ;
#62703 = CARTESIAN_POINT('Ctrl Pts',(-18.2274647737821,-40.4107474268893,
123.65202799485)) ;
#62704 = CARTESIAN_POINT('Ctrl Pts',(-18.0050786320666,-40.6005761529685,
123.960147159055)) ;
#62705 = CARTESIAN_POINT('Ctrl Pts',(-18.2859206557208,-40.4205870726056,
123.850492648776)) ;
#62706 = CARTESIAN_POINT('Ctrl Pts',(-18.122387240134,-40.6106393205242,124.197113300157)) ;
#62707 = CARTESIAN_POINT('Ctrl Pts',(-18.3797695138113,-40.4306502401614,
124.04006462666)) ;
#62708 = CARTESIAN_POINT('Ctrl Pts',(-18.2766451104993,-40.6205335763191,
124.406457589584)) ;
#62709 = CARTESIAN_POINT('Ctrl Pts',(-18.5031774204624,-40.4405444959563,
124.207538542366)) ;
#62710 = CARTESIAN_POINT('Ctrl Pts',(-18.4652776966857,-40.6304753547788,
124.587171422744)) ;
#62711 = CARTESIAN_POINT('Ctrl Pts',(-18.6540848187046,-40.4504862744159,
124.352107914679)) ;
#62712 = CARTESIAN_POINT('Ctrl Pts',(-18.6837565652639,-40.640478047609,124.733392656185)) ;
#62713 = CARTESIAN_POINT('Ctrl Pts',(-18.8288690428585,-40.4604889672461,
124.469083093928)) ;
#62714 = CARTESIAN_POINT('Ctrl Pts',(-18.9251772147638,-40.6505120695628,
124.839403238279)) ;
#62715 = CARTESIAN_POINT('Ctrl Pts',(-19.0220064463768,-40.4705229891999,
124.553889578956)) ;
#62716 = CARTESIAN_POINT('Ctrl Pts',(-19.176509623626,-40.6603598606518,124.901116406676)) ;
#62717 = CARTESIAN_POINT('Ctrl Pts',(-19.2230724433567,-40.480370780289,124.603257935975)) ;
#62718 = CARTESIAN_POINT('Ctrl Pts',(-19.4381766703649,-40.6703413852009,
124.919060383607)) ;
#62719 = CARTESIAN_POINT('Ctrl Pts',(-19.4324060828598,-40.490352304838,124.617611036855)) ;
#62720 = CARTESIAN_POINT('Ctrl Pts',(-19.6981676204706,-40.6802906086918,
124.891345054652)) ;
#62721 = CARTESIAN_POINT('Ctrl Pts',(-19.6403984071711,-40.5003015283289,
124.595436730586)) ;
#62722 = CARTESIAN_POINT('Ctrl Pts',(-19.9507242764533,-40.6902882649084,
124.818869487459)) ;
#62723 = CARTESIAN_POINT('Ctrl Pts',(-19.8424430882566,-40.5102991845455,
124.537454338467)) ;
#62724 = CARTESIAN_POINT('Ctrl Pts',(-20.1876076661773,-40.7003284779634,
124.702714148648)) ;
#62725 = CARTESIAN_POINT('Ctrl Pts',(-20.0319489184708,-40.5203393976006,
124.444528159668)) ;
#62726 = CARTESIAN_POINT('Ctrl Pts',(-20.39657947432,-40.7101565252397,124.550916691026)) ;
#62727 = CARTESIAN_POINT('Ctrl Pts',(-20.1991246693014,-40.5301674448768,
124.323088910881)) ;
#62728 = CARTESIAN_POINT('Ctrl Pts',(-20.5804267072164,-40.7202108722721,
124.361171005036)) ;
#62729 = CARTESIAN_POINT('Ctrl Pts',(-20.346201090862,-40.5402217919092,124.171290919494)) ;
#62730 = CARTESIAN_POINT('Ctrl Pts',(-20.7265146724235,-40.7301520086006,
124.144583500037)) ;
#62731 = CARTESIAN_POINT('Ctrl Pts',(-20.4630696218111,-40.5501629282377,
123.998019996052)) ;
#62732 = CARTESIAN_POINT('Ctrl Pts',(-20.833118168353,-40.7400562416803,123.907137322024)) ;
#62733 = CARTESIAN_POINT('Ctrl Pts',(-20.5483504786271,-40.5600671613174,
123.808062650785)) ;
#62734 = CARTESIAN_POINT('Ctrl Pts',(-20.8976239886845,-40.7501029385239,
123.651145500443)) ;
#62735 = CARTESIAN_POINT('Ctrl Pts',(-20.5999532571857,-40.5701138581611,
123.603268634691)) ;
#62736 = CARTESIAN_POINT('Ctrl Pts',(-20.9166549329738,-40.7599984898042,
123.391755647878)) ;
#62737 = CARTESIAN_POINT('Ctrl Pts',(-20.6151760608745,-40.5800094094413,
123.395757077431)) ;
#62738 = CARTESIAN_POINT('Ctrl Pts',(-20.8899239295474,-40.7700605676437,
123.128727559493)) ;
#62739 = CARTESIAN_POINT('Ctrl Pts',(-20.5937893272539,-40.5900714872808,
123.18533465587)) ;
#62740 = CARTESIAN_POINT('Ctrl Pts',(-20.8196225925667,-40.7799032767398,
122.879777795718)) ;
#62741 = CARTESIAN_POINT('Ctrl Pts',(-20.5375466154367,-40.5999141963769,
122.98617602963)) ;
#62742 = CARTESIAN_POINT('Ctrl Pts',(-20.7060594583057,-40.7898940089782,
122.643100332516)) ;
#62743 = CARTESIAN_POINT('Ctrl Pts',(-20.4466945356706,-40.6099049286153,
122.796834968904)) ;
#62744 = CARTESIAN_POINT('Ctrl Pts',(-20.554024482547,-40.799822034207,122.43106134549)) ;
#62745 = CARTESIAN_POINT('Ctrl Pts',(-20.3250653085112,-40.6198329538441,
122.627205154481)) ;
#62746 = CARTESIAN_POINT('Ctrl Pts',(-20.3666704074435,-40.8098101808575,
122.247223536498)) ;
#62747 = CARTESIAN_POINT('Ctrl Pts',(-20.1751809297172,-40.6298211004947,
122.480136252607)) ;
#62748 = CARTESIAN_POINT('Ctrl Pts',(-20.1490005900659,-40.8198451986975,
122.098346117619)) ;
#62749 = CARTESIAN_POINT('Ctrl Pts',(-20.0010440055564,-40.6398561183346,
122.361035777316)) ;
#62750 = CARTESIAN_POINT('Ctrl Pts',(-19.9129860527782,-40.8297099958027,
121.991128079681)) ;
#62751 = CARTESIAN_POINT('Ctrl Pts',(-19.8122322768596,-40.6497209154398,
122.275263239916)) ;
#62752 = CARTESIAN_POINT('Ctrl Pts',(-19.6596753422036,-40.8396707281588,
121.925143350382)) ;
#62753 = CARTESIAN_POINT('Ctrl Pts',(-19.6095835667024,-40.6596816477959,
122.222477106731)) ;
#62754 = CARTESIAN_POINT('Ctrl Pts',(-19.3968323127543,-40.8497041905558,
121.904431778563)) ;
#62755 = CARTESIAN_POINT('Ctrl Pts',(-19.3993089374676,-40.6697151101929,
122.205909546887)) ;
#62756 = CARTESIAN_POINT('Ctrl Pts',(-19.1381719931737,-40.8595897247672,
121.928871855677)) ;
#62757 = CARTESIAN_POINT('Ctrl Pts',(-19.1923814686727,-40.6796006444043,
122.225463173289)) ;
#62758 = CARTESIAN_POINT('Ctrl Pts',(-18.8832051234913,-40.8696545654472,
121.999096373019)) ;
#62759 = CARTESIAN_POINT('Ctrl Pts',(-18.9884082093164,-40.6896654850843,
122.281644418991)) ;
#62760 = CARTESIAN_POINT('Ctrl Pts',(-18.6493502439054,-40.8795026971761,
122.110000505807)) ;
#62761 = CARTESIAN_POINT('Ctrl Pts',(-18.8013257528878,-40.6995136168132,
122.370368822003)) ;
#62762 = CARTESIAN_POINT('Ctrl Pts',(-18.4340900376583,-40.8895301941662,
122.261979815528)) ;
#62763 = CARTESIAN_POINT('Ctrl Pts',(-18.6291184182037,-40.7095411138033,
122.49195350058)) ;
#62764 = CARTESIAN_POINT('Ctrl Pts',(-18.2489515312442,-40.8995586462113,
122.449550693022)) ;
#62765 = CARTESIAN_POINT('Ctrl Pts',(-18.4810087252179,-40.7195695658484,
122.642011378484)) ;
#62766 = CARTESIAN_POINT('Ctrl Pts',(-18.1015397641077,-40.9094039127754,
122.662154181766)) ;
#62767 = CARTESIAN_POINT('Ctrl Pts',(-18.3630810732943,-40.7294148324125,
122.812094300653)) ;
#62768 = CARTESIAN_POINT('Ctrl Pts',(-17.9910357650172,-40.9193945857163,
122.900318312532)) ;
#62769 = CARTESIAN_POINT('Ctrl Pts',(-18.2746791939818,-40.7394055053534,
123.002626045039)) ;
#62770 = CARTESIAN_POINT('Ctrl Pts',(-17.9238150126673,-40.9294324678048,
123.155391668012)) ;
#62771 = CARTESIAN_POINT('Ctrl Pts',(-18.2209040160254,-40.7494433874419,
123.206685215275)) ;
#62772 = CARTESIAN_POINT('Ctrl Pts',(-17.9018757959936,-40.9392768382444,
123.413170064838)) ;
#62773 = CARTESIAN_POINT('Ctrl Pts',(-18.2033541255179,-40.7592877578816,
123.41290711647)) ;
#62774 = CARTESIAN_POINT('Ctrl Pts',(-17.9248387222201,-40.9492616656398,
123.674518463669)) ;
#62775 = CARTESIAN_POINT('Ctrl Pts',(-18.2217257460994,-40.7692725852769,
123.621985522676)) ;
#62776 = CARTESIAN_POINT('Ctrl Pts',(-17.9924288980122,-40.9592011110451,
123.926859519996)) ;
#62777 = CARTESIAN_POINT('Ctrl Pts',(-18.2757990048026,-40.7792120306822,
123.823857616306)) ;
#62778 = CARTESIAN_POINT('Ctrl Pts',(-18.1039644977268,-40.969241115331,124.165936540769)) ;
#62779 = CARTESIAN_POINT('Ctrl Pts',(-18.3650287084099,-40.7892520349681,
124.015118795446)) ;
#62780 = CARTESIAN_POINT('Ctrl Pts',(-18.2528993475112,-40.9791282245166,
124.378873025714)) ;
#62781 = CARTESIAN_POINT('Ctrl Pts',(-18.4841771835395,-40.7991391441538,
124.185466648641)) ;
#62782 = CARTESIAN_POINT('Ctrl Pts',(-18.4383623409919,-40.9891282844191,
124.564995129704)) ;
#62783 = CARTESIAN_POINT('Ctrl Pts',(-18.6325483359507,-40.8091392040562,
124.334363415602)) ;
#62784 = CARTESIAN_POINT('Ctrl Pts',(-18.6514890497464,-40.9990457003338,
124.715068772833)) ;
#62785 = CARTESIAN_POINT('Ctrl Pts',(-18.8030498870585,-40.8190566199709,
124.454421071669)) ;
#62786 = CARTESIAN_POINT('Ctrl Pts',(-18.8904730960395,-41.0090925150746,
124.827199842309)) ;
#62787 = CARTESIAN_POINT('Ctrl Pts',(-18.9942377675479,-40.8291034347117,
124.54412495723)) ;
#62788 = CARTESIAN_POINT('Ctrl Pts',(-19.1409580665125,-41.0189679922713,
124.895235368087)) ;
#62789 = CARTESIAN_POINT('Ctrl Pts',(-19.1946252220464,-40.8389789119084,
124.59855210373)) ;
#62790 = CARTESIAN_POINT('Ctrl Pts',(-19.4040773768789,-41.0290240879925,
124.919312459321)) ;
#62791 = CARTESIAN_POINT('Ctrl Pts',(-19.4051209742534,-40.8490350076296,
124.617812738242)) ;
#62792 = CARTESIAN_POINT('Ctrl Pts',(-19.6632167072632,-41.0389172500076,
124.897783110469)) ;
#62793 = CARTESIAN_POINT('Ctrl Pts',(-19.612431616485,-40.8589281696447,124.600588287946)) ;
#62794 = CARTESIAN_POINT('Ctrl Pts',(-19.918917313857,-41.0489794860302,124.830551760871)) ;
#62795 = CARTESIAN_POINT('Ctrl Pts',(-19.816992096317,-40.8689904056673,124.546802153709)) ;
#62796 = CARTESIAN_POINT('Ctrl Pts',(-20.1539134835327,-41.0588239516591,
124.722342924619)) ;
#62797 = CARTESIAN_POINT('Ctrl Pts',(-20.0049876465229,-40.8788348712962,
124.460234605023)) ;
#62798 = CARTESIAN_POINT('Ctrl Pts',(-20.3695735130956,-41.0687840443633,
124.574029278927)) ;
#62799 = CARTESIAN_POINT('Ctrl Pts',(-20.1775149195478,-40.8887949640004,
124.34158324237)) ;
#62800 = CARTESIAN_POINT('Ctrl Pts',(-20.5573002807056,-41.0788223333443,
124.388718288801)) ;
#62801 = CARTESIAN_POINT('Ctrl Pts',(-20.3276957826536,-40.8988332529814,
124.193333707095)) ;
#62802 = CARTESIAN_POINT('Ctrl Pts',(-20.7079273846869,-41.0886956564505,
124.177407956231)) ;
#62803 = CARTESIAN_POINT('Ctrl Pts',(-20.4481962954603,-40.9087065760876,
124.024285712482)) ;
#62804 = CARTESIAN_POINT('Ctrl Pts',(-20.8217196875643,-41.0987688405356,
123.938460528923)) ;
#62805 = CARTESIAN_POINT('Ctrl Pts',(-20.5392295466057,-40.9187797601727,
123.833127110571)) ;
#62806 = CARTESIAN_POINT('Ctrl Pts',(-20.8908771120928,-41.1085893528235,
123.689767340494)) ;
#62807 = CARTESIAN_POINT('Ctrl Pts',(-20.5945544458289,-40.9286002724607,
123.634173561183)) ;
#62808 = CARTESIAN_POINT('Ctrl Pts',(-20.9166985130199,-41.1186673489393,
123.426252975594)) ;
#62809 = CARTESIAN_POINT('Ctrl Pts',(-20.615210932042,-40.9386782685765,123.423361632516)) ;
#62810 = CARTESIAN_POINT('Ctrl Pts',(-20.8968766070843,-41.1285214239226,
123.167997632845)) ;
#62811 = CARTESIAN_POINT('Ctrl Pts',(-20.5993528292853,-40.9485323435597,
123.21675844281)) ;
#62812 = CARTESIAN_POINT('Ctrl Pts',(-20.8314512990001,-41.1385853055063,
122.911802236426)) ;
#62813 = CARTESIAN_POINT('Ctrl Pts',(-20.5470119442779,-40.9585962251434,
123.011802002189)) ;
#62814 = CARTESIAN_POINT('Ctrl Pts',(-20.7244059189189,-41.14846873148,122.675111707094)) ;
#62815 = CARTESIAN_POINT('Ctrl Pts',(-20.461375448032,-40.9684796511172,122.822450609287)) ;
#62816 = CARTESIAN_POINT('Ctrl Pts',(-20.5765499860383,-41.1584693354011,
122.457899543958)) ;
#62817 = CARTESIAN_POINT('Ctrl Pts',(-20.3430903518895,-40.9784802550382,
122.648681253808)) ;
#62818 = CARTESIAN_POINT('Ctrl Pts',(-20.3947593959915,-41.168389119739,122.270998373932)) ;
#62819 = CARTESIAN_POINT('Ctrl Pts',(-20.1976579864223,-40.9884000393761,
122.499161080854)) ;
#62820 = CARTESIAN_POINT('Ctrl Pts',(-20.1805968421938,-41.1784364700958,
122.116644490037)) ;
#62821 = CARTESIAN_POINT('Ctrl Pts',(-20.0263275114058,-40.998447389733,122.37567824904)) ;
#62822 = CARTESIAN_POINT('Ctrl Pts',(-19.9469565780985,-41.1883138123301,
122.003445575771)) ;
#62823 = CARTESIAN_POINT('Ctrl Pts',(-19.8394159581554,-41.0083247319672,
122.285119878453)) ;
#62824 = CARTESIAN_POINT('Ctrl Pts',(-19.6924393110652,-41.1983836934047,
121.931197405337)) ;
#62825 = CARTESIAN_POINT('Ctrl Pts',(-19.6358017081943,-41.0183946130419,
122.227321635127)) ;
#62826 = CARTESIAN_POINT('Ctrl Pts',(-19.4354489668085,-41.2082133986064,
121.904602386854)) ;
#62827 = CARTESIAN_POINT('Ctrl Pts',(-19.430210627212,-41.0282243182436,122.206046078659)) ;
#62828 = CARTESIAN_POINT('Ctrl Pts',(-19.1716002965813,-41.2182800597728,
121.923118301563)) ;
#62829 = CARTESIAN_POINT('Ctrl Pts',(-19.2191313901848,-41.03829097941,122.220859076658)) ;
#62830 = CARTESIAN_POINT('Ctrl Pts',(-18.9194385507973,-41.2281702816401,
121.986221032481)) ;
#62831 = CARTESIAN_POINT('Ctrl Pts',(-19.0174028771925,-41.0481812012773,
122.271341336615)) ;
#62832 = CARTESIAN_POINT('Ctrl Pts',(-18.6794263982386,-41.2381624577503,
122.092694865169)) ;
#62833 = CARTESIAN_POINT('Ctrl Pts',(-18.825393369095,-41.0581733773874,122.356520462696)) ;
#62834 = CARTESIAN_POINT('Ctrl Pts',(-18.462319115849,-41.2481252878629,122.239006352315)) ;
#62835 = CARTESIAN_POINT('Ctrl Pts',(-18.6517079609517,-41.0681362075001,
122.473569619426)) ;
#62836 = CARTESIAN_POINT('Ctrl Pts',(-18.2745423237503,-41.2580295002633,
122.419265967195)) ;
#62837 = CARTESIAN_POINT('Ctrl Pts',(-18.5014870946545,-41.0780404199004,
122.617776816636)) ;
#62838 = CARTESIAN_POINT('Ctrl Pts',(-18.1187135739592,-41.2680902143511,
122.632804079682)) ;
#62839 = CARTESIAN_POINT('Ctrl Pts',(-18.3768240055462,-41.0881011339882,
122.788607593364)) ;
#62840 = CARTESIAN_POINT('Ctrl Pts',(-18.0045368875343,-41.2779297173339,
122.864848022296)) ;
#62841 = CARTESIAN_POINT('Ctrl Pts',(-18.2854831831512,-41.097940636971,122.974241688555)) ;
#62842 = CARTESIAN_POINT('Ctrl Pts',(-17.9304874746578,-41.2879958559003,
123.11875522056)) ;
#62843 = CARTESIAN_POINT('Ctrl Pts',(-18.2262435039461,-41.1080067755374,
123.177367738535)) ;
#62844 = CARTESIAN_POINT('Ctrl Pts',(-17.902263224335,-41.2978783703863,123.376958924445)) ;
#62845 = CARTESIAN_POINT('Ctrl Pts',(-18.2036641643928,-41.1178892900235,
123.383929797729)) ;
#62846 = CARTESIAN_POINT('Ctrl Pts',(-17.9189692034043,-41.3078706697419,
123.638973965491)) ;
#62847 = CARTESIAN_POINT('Ctrl Pts',(-18.2170287674167,-41.127881589379,123.593541666519)) ;
#62848 = CARTESIAN_POINT('Ctrl Pts',(-17.9806273077311,-41.3178237366953,
123.893199304568)) ;
#62849 = CARTESIAN_POINT('Ctrl Pts',(-18.2663549772125,-41.1378346563324,
123.796921581805)) ;
#62850 = CARTESIAN_POINT('Ctrl Pts',(-18.0864278200169,-41.3278584449005,
124.134724121174)) ;
#62851 = CARTESIAN_POINT('Ctrl Pts',(-18.3509952924776,-41.1478693645376,
123.990141608418)) ;
#62852 = CARTESIAN_POINT('Ctrl Pts',(-18.2302862077972,-41.3377466658047,
124.351140926558)) ;
#62853 = CARTESIAN_POINT('Ctrl Pts',(-18.4660813609323,-41.1577575854418,
124.163274450491)) ;
#62854 = CARTESIAN_POINT('Ctrl Pts',(-18.411128140004,-41.3477410888351,124.541587743708)) ;
#62855 = CARTESIAN_POINT('Ctrl Pts',(-18.6107545669795,-41.1677520084722,
124.31563199722)) ;
#62856 = CARTESIAN_POINT('Ctrl Pts',(-18.6213277144287,-41.3576864282813,
124.696900401289)) ;
#62857 = CARTESIAN_POINT('Ctrl Pts',(-18.7789136746949,-41.1776973479184,
124.439882070568)) ;
#62858 = CARTESIAN_POINT('Ctrl Pts',(-18.8551198560532,-41.3676337728926,
124.813866561764)) ;
#62859 = CARTESIAN_POINT('Ctrl Pts',(-18.9659467888428,-41.1876446925297,
124.533455168981)) ;
#62860 = CARTESIAN_POINT('Ctrl Pts',(-19.1082663812488,-41.3776816683036,
124.888923688486)) ;
#62861 = CARTESIAN_POINT('Ctrl Pts',(-19.1684641030672,-41.1976925879407,
124.593501257939)) ;
#62862 = CARTESIAN_POINT('Ctrl Pts',(-19.3653576889217,-41.387529313783,124.918508593892)) ;
#62863 = CARTESIAN_POINT('Ctrl Pts',(-19.374135991281,-41.2075402334201,124.617169451887)) ;
#62864 = CARTESIAN_POINT('Ctrl Pts',(-19.6267063239456,-41.397491027697,124.903644555584)) ;
#62865 = CARTESIAN_POINT('Ctrl Pts',(-19.5832145704097,-41.2175019473341,
124.605278846852)) ;
#62866 = CARTESIAN_POINT('Ctrl Pts',(-19.8831669773239,-41.4075196519879,
124.842893155659)) ;
#62867 = CARTESIAN_POINT('Ctrl Pts',(-19.7883832884811,-41.227530571625,124.556678216363)) ;
#62868 = CARTESIAN_POINT('Ctrl Pts',(-20.1223364379903,-41.4174300126446,
124.739853154527)) ;
#62869 = CARTESIAN_POINT('Ctrl Pts',(-19.9797184280272,-41.2374409322817,
124.474246990679)) ;
#62870 = CARTESIAN_POINT('Ctrl Pts',(-20.3409126898904,-41.4273647112179,
124.597063389142)) ;
#62871 = CARTESIAN_POINT('Ctrl Pts',(-20.1545793763586,-41.247375630855,124.360016063863)) ;
#62872 = CARTESIAN_POINT('Ctrl Pts',(-20.5332339905114,-41.4374065360721,
124.416390285309)) ;
#62873 = CARTESIAN_POINT('Ctrl Pts',(-20.3084369714252,-41.2574174557092,
124.215477948896)) ;
#62874 = CARTESIAN_POINT('Ctrl Pts',(-20.6889942202741,-41.4472911098165,
124.208484214558)) ;
#62875 = CARTESIAN_POINT('Ctrl Pts',(-20.4330452122912,-41.2673020294536,
124.049154187181)) ;
#62876 = CARTESIAN_POINT('Ctrl Pts',(-20.8079337346372,-41.4572929591797,
123.974137087454)) ;
#62877 = CARTESIAN_POINT('Ctrl Pts',(-20.5281974668487,-41.2773038788168,
123.861676944645)) ;
#62878 = CARTESIAN_POINT('Ctrl Pts',(-20.8839492756787,-41.4672122607537,
123.724761737193)) ;
#62879 = CARTESIAN_POINT('Ctrl Pts',(-20.5890105118696,-41.2872231803909,
123.662177488703)) ;
#62880 = CARTESIAN_POINT('Ctrl Pts',(-20.9159063783837,-41.477256369099,123.462776779803)) ;
#62881 = CARTESIAN_POINT('Ctrl Pts',(-20.6145770325687,-41.2972672887361,
123.452589454882)) ;
#62882 = CARTESIAN_POINT('Ctrl Pts',(-20.9021882404978,-41.4871407925413,
123.203374700093)) ;
#62883 = CARTESIAN_POINT('Ctrl Pts',(-20.6036034091239,-41.3071517121784,
123.245068567429)) ;
#62884 = CARTESIAN_POINT('Ctrl Pts',(-20.8434269167983,-41.4971571544507,
122.946788139686)) ;
#62885 = CARTESIAN_POINT('Ctrl Pts',(-20.5565953052322,-41.3171680740879,
123.039799101921)) ;
#62886 = CARTESIAN_POINT('Ctrl Pts',(-20.740169246239,-41.5071938099561,122.704103736706)) ;
#62887 = CARTESIAN_POINT('Ctrl Pts',(-20.4739898809288,-41.3272047295932,
122.845651168886)) ;
#62888 = CARTESIAN_POINT('Ctrl Pts',(-20.5998669968465,-41.5170239401454,
122.487161714525)) ;
#62889 = CARTESIAN_POINT('Ctrl Pts',(-20.3617495279934,-41.3370348597826,
122.672097974141)) ;
#62890 = CARTESIAN_POINT('Ctrl Pts',(-20.4197517580595,-41.5270999932353,
122.293140547087)) ;
#62891 = CARTESIAN_POINT('Ctrl Pts',(-20.2176578409717,-41.3471109128724,
122.516880105175)) ;
#62892 = CARTESIAN_POINT('Ctrl Pts',(-20.2133740001492,-41.5369522224211,
122.136713686681)) ;
#62893 = CARTESIAN_POINT('Ctrl Pts',(-20.0525570462563,-41.3569631420582,
122.391738386618)) ;
#62894 = CARTESIAN_POINT('Ctrl Pts',(-19.9779921555952,-41.5470254302204,
122.015693380369)) ;
#62895 = CARTESIAN_POINT('Ctrl Pts',(-19.8642517827859,-41.3670363498575,
122.294921027755)) ;
#62896 = CARTESIAN_POINT('Ctrl Pts',(-19.7309096530658,-41.5568669415718,
121.939233606283)) ;
#62897 = CARTESIAN_POINT('Ctrl Pts',(-19.6665870925325,-41.3768778612089,
122.233752494711)) ;
#62898 = CARTESIAN_POINT('Ctrl Pts',(-19.4713417220652,-41.5668278796093,
121.905469506213)) ;
#62899 = CARTESIAN_POINT('Ctrl Pts',(-19.4589332355636,-41.3868387992465,
122.206739977289)) ;
#62900 = CARTESIAN_POINT('Ctrl Pts',(-19.2078592032353,-41.5768657415343,
121.917907090772)) ;
#62901 = CARTESIAN_POINT('Ctrl Pts',(-19.2481470590052,-41.3968766611714,
122.216688878807)) ;
#62902 = CARTESIAN_POINT('Ctrl Pts',(-18.9545877190135,-41.5867399275314,
121.974495320736)) ;
#62903 = CARTESIAN_POINT('Ctrl Pts',(-19.0455303831215,-41.4067508471685,
122.261958038974)) ;
#62904 = CARTESIAN_POINT('Ctrl Pts',(-18.7103088483806,-41.5968100871093,
122.076174219164)) ;
#62905 = CARTESIAN_POINT('Ctrl Pts',(-18.8501065384056,-41.4168210067464,
122.343300089057)) ;
#62906 = CARTESIAN_POINT('Ctrl Pts',(-18.4925316287136,-41.6066418345351,
122.215244290512)) ;
#62907 = CARTESIAN_POINT('Ctrl Pts',(-18.675884926045,-41.4266527541722,122.454554491954)) ;
#62908 = CARTESIAN_POINT('Ctrl Pts',(-18.2978201733905,-41.6166779146064,
122.393114575387)) ;
#62909 = CARTESIAN_POINT('Ctrl Pts',(-18.5201147167768,-41.4366888342435,
122.596849707631)) ;
#62910 = CARTESIAN_POINT('Ctrl Pts',(-18.1377661291796,-41.6266949614589,
122.602121409424)) ;
#62911 = CARTESIAN_POINT('Ctrl Pts',(-18.3920704452954,-41.446705881096,122.764054368868)) ;
#62912 = CARTESIAN_POINT('Ctrl Pts',(-18.0176363964437,-41.6365772196255,
122.832366722384)) ;
#62913 = CARTESIAN_POINT('Ctrl Pts',(-18.2959657432194,-41.4565881392626,
122.948249322725)) ;
#62914 = CARTESIAN_POINT('Ctrl Pts',(-17.9381960769655,-41.6465649024218,
123.082493245792)) ;
#62915 = CARTESIAN_POINT('Ctrl Pts',(-18.2324121300775,-41.466575822059,123.148349941612)) ;
#62916 = CARTESIAN_POINT('Ctrl Pts',(-17.9033168942799,-41.6565115591386,
123.341584277109)) ;
#62917 = CARTESIAN_POINT('Ctrl Pts',(-18.2045073339234,-41.4765224787757,
123.355622202973)) ;
#62918 = CARTESIAN_POINT('Ctrl Pts',(-17.9143411683041,-41.6665686172188,
123.605613842751)) ;
#62919 = CARTESIAN_POINT('Ctrl Pts',(-18.2133253006572,-41.4865795368559,
123.56684609059)) ;
#62920 = CARTESIAN_POINT('Ctrl Pts',(-17.969355045573,-41.6763867967682,123.857706729659)) ;
#62921 = CARTESIAN_POINT('Ctrl Pts',(-18.2573346904217,-41.4963977164053,
123.768519739504)) ;
#62922 = CARTESIAN_POINT('Ctrl Pts',(-18.0688075005491,-41.6864227312072,
124.101962973962)) ;
#62923 = CARTESIAN_POINT('Ctrl Pts',(-18.3368951443602,-41.5064336508443,
123.963925444336)) ;
#62924 = CARTESIAN_POINT('Ctrl Pts',(-18.2096507194806,-41.6964473856362,
124.324600663781)) ;
#62925 = CARTESIAN_POINT('Ctrl Pts',(-18.4495684418936,-41.5164583052733,
124.142036426713)) ;
#62926 = CARTESIAN_POINT('Ctrl Pts',(-18.3835301012507,-41.7062994052157,
124.51642843277)) ;
#62927 = CARTESIAN_POINT('Ctrl Pts',(-18.5886701972633,-41.5263103248528,
124.295499139978)) ;
#62928 = CARTESIAN_POINT('Ctrl Pts',(-18.5906854588075,-41.7162903189306,
124.677682956406)) ;
#62929 = CARTESIAN_POINT('Ctrl Pts',(-18.7543933282232,-41.5363012385678,
124.424504019859)) ;
#62930 = CARTESIAN_POINT('Ctrl Pts',(-18.8209758181354,-41.7262083077702,
124.799801736939)) ;
#62931 = CARTESIAN_POINT('Ctrl Pts',(-18.9386244015868,-41.5462192274073,
124.522200358764)) ;
#62932 = CARTESIAN_POINT('Ctrl Pts',(-19.0716562721303,-41.736236418501,124.88101516819)) ;
#62933 = CARTESIAN_POINT('Ctrl Pts',(-19.1391682539512,-41.5562473381381,
124.587172769983)) ;
#62934 = CARTESIAN_POINT('Ctrl Pts',(-19.3289219205496,-41.7461216164094,
124.917060930178)) ;
#62935 = CARTESIAN_POINT('Ctrl Pts',(-19.3449799461922,-41.5661325360465,
124.616011040601)) ;
#62936 = CARTESIAN_POINT('Ctrl Pts',(-19.5912951011556,-41.7561108916774,
124.908434150028)) ;
#62937 = CARTESIAN_POINT('Ctrl Pts',(-19.554878426075,-41.5761218113145,124.609111482984)) ;
#62938 = CARTESIAN_POINT('Ctrl Pts',(-19.8493960390687,-41.7661523498469,
124.853543536914)) ;
#62939 = CARTESIAN_POINT('Ctrl Pts',(-19.7613596181265,-41.586163269484,124.565200709918)) ;
#62940 = CARTESIAN_POINT('Ctrl Pts',(-20.089121327571,-41.7759838136352,124.757174104887)) ;
#62941 = CARTESIAN_POINT('Ctrl Pts',(-19.9531398219293,-41.5959947332723,
124.488107167589)) ;
#62942 = CARTESIAN_POINT('Ctrl Pts',(-20.3126159520966,-41.7859887459391,
124.618753527264)) ;
#62943 = CARTESIAN_POINT('Ctrl Pts',(-20.1319364892421,-41.6059996655762,
124.377372384104)) ;
#62944 = CARTESIAN_POINT('Ctrl Pts',(-20.5082790000552,-41.7959751098338,
124.44379651089)) ;
#62945 = CARTESIAN_POINT('Ctrl Pts',(-20.2884681052533,-41.615986029471,124.237408279578)) ;
#62946 = CARTESIAN_POINT('Ctrl Pts',(-20.6710896620277,-41.8060047387197,
124.236556568521)) ;
#62947 = CARTESIAN_POINT('Ctrl Pts',(-20.4187181302531,-41.6260156583568,
124.071617471286)) ;
#62948 = CARTESIAN_POINT('Ctrl Pts',(-20.7938478463196,-41.8158799608281,
124.007888084102)) ;
#62949 = CARTESIAN_POINT('Ctrl Pts',(-20.5169261213944,-41.6358908804652,
123.88868407081)) ;
#62950 = CARTESIAN_POINT('Ctrl Pts',(-20.8763477233689,-41.8258811732252,
123.758394357555)) ;
#62951 = CARTESIAN_POINT('Ctrl Pts',(-20.5829278694143,-41.6458920928623,
123.689089793448)) ;
#62952 = CARTESIAN_POINT('Ctrl Pts',(-20.9141799974451,-41.8357897524607,
123.500723797923)) ;
#62953 = CARTESIAN_POINT('Ctrl Pts',(-20.6131956146695,-41.6558006720979,
123.482954012209)) ;
#62954 = CARTESIAN_POINT('Ctrl Pts',(-20.9065096443018,-41.8458446050167,
123.236647196744)) ;
#62955 = CARTESIAN_POINT('Ctrl Pts',(-20.607061323779,-41.6658555246539,123.271692585024)) ;
#62956 = CARTESIAN_POINT('Ctrl Pts',(-20.8544198064542,-41.8557031872915,
122.982817801589)) ;
#62957 = CARTESIAN_POINT('Ctrl Pts',(-20.5653915448547,-41.6757141069286,
123.068629169974)) ;
#62958 = CARTESIAN_POINT('Ctrl Pts',(-20.7572019522211,-41.8657713167342,
122.736787999825)) ;
#62959 = CARTESIAN_POINT('Ctrl Pts',(-20.4876191232104,-41.6857822363713,
122.871804461378)) ;
#62960 = CARTESIAN_POINT('Ctrl Pts',(-20.6216170476226,-41.8756267884233,
122.516096462903)) ;
#62961 = CARTESIAN_POINT('Ctrl Pts',(-20.3791532034229,-41.6956377080604,
122.695250586501)) ;
#62962 = CARTESIAN_POINT('Ctrl Pts',(-20.4479526497867,-41.8856216368096,
122.319060073039)) ;
#62963 = CARTESIAN_POINT('Ctrl Pts',(-20.2402233360119,-41.7056325564467,
122.537620125504)) ;
#62964 = CARTESIAN_POINT('Ctrl Pts',(-20.2416008599543,-41.895652933594,122.155008415797)) ;
#62965 = CARTESIAN_POINT('Ctrl Pts',(-20.0751431938009,-41.7156638532311,
122.406377179865)) ;
#62966 = CARTESIAN_POINT('Ctrl Pts',(-20.0138985646584,-41.9055194698041,
122.030978291943)) ;
#62967 = CARTESIAN_POINT('Ctrl Pts',(-19.8929827296992,-41.7255303894412,
122.307151422635)) ;
#62968 = CARTESIAN_POINT('Ctrl Pts',(-19.7652803949844,-41.9155068927649,
121.946967065513)) ;
#62969 = CARTESIAN_POINT('Ctrl Pts',(-19.6940889763465,-41.7355178124021,
122.23994043297)) ;
#62970 = CARTESIAN_POINT('Ctrl Pts',(-19.5069103967345,-41.9254518317847,
121.907424800281)) ;
#62971 = CARTESIAN_POINT('Ctrl Pts',(-19.4873934887718,-41.7454627514218,
122.208304514196)) ;
#62972 = CARTESIAN_POINT('Ctrl Pts',(-19.2430300937842,-41.9354967176447,
121.913529165086)) ;
#62973 = CARTESIAN_POINT('Ctrl Pts',(-19.2762891837712,-41.7555076372818,
122.213185853992)) ;
#62974 = CARTESIAN_POINT('Ctrl Pts',(-18.9887092821943,-41.9453652527309,
121.964316287629)) ;
#62975 = CARTESIAN_POINT('Ctrl Pts',(-19.072832435962,-41.7653761723681,122.253813365681)) ;
#62976 = CARTESIAN_POINT('Ctrl Pts',(-18.7444398718667,-41.9553311207376,
122.058732418128)) ;
#62977 = CARTESIAN_POINT('Ctrl Pts',(-18.8774162150229,-41.7753420403747,
122.329344164061)) ;
#62978 = CARTESIAN_POINT('Ctrl Pts',(-18.5191258960405,-41.9653537681901,
122.195167959833)) ;
#62979 = CARTESIAN_POINT('Ctrl Pts',(-18.6971639262968,-41.7853646878272,
122.438490705683)) ;
#62980 = CARTESIAN_POINT('Ctrl Pts',(-18.322858065799,-41.9752774071977,122.366864085304)) ;
#62981 = CARTESIAN_POINT('Ctrl Pts',(-18.5401483567963,-41.7952883268348,
122.575845826025)) ;
#62982 = CARTESIAN_POINT('Ctrl Pts',(-18.1585632397569,-41.9852201322034,
122.570050124167)) ;
#62983 = CARTESIAN_POINT('Ctrl Pts',(-18.4087108446553,-41.8052310518406,
122.738393149906)) ;
#62984 = CARTESIAN_POINT('Ctrl Pts',(-18.0310264117004,-41.9952657382553,
122.80116942064)) ;
#62985 = CARTESIAN_POINT('Ctrl Pts',(-18.3066794495729,-41.8152766578924,
122.923287501502)) ;
#62986 = CARTESIAN_POINT('Ctrl Pts',(-17.9468424318338,-42.0051271607764,
123.046286075553)) ;
#62987 = CARTESIAN_POINT('Ctrl Pts',(-18.2393302260419,-41.8251380804135,
123.119379900334)) ;
#62988 = CARTESIAN_POINT('Ctrl Pts',(-17.9055231594074,-42.0151207292256,
123.305597710692)) ;
#62989 = CARTESIAN_POINT('Ctrl Pts',(-18.2062726013886,-41.8351316488627,
123.326828797274)) ;
#62990 = CARTESIAN_POINT('Ctrl Pts',(-17.9096925519482,-42.0250461999809,
123.56643384868)) ;
#62991 = CARTESIAN_POINT('Ctrl Pts',(-18.2096058544786,-41.845057119618,123.535497626538)) ;
#62992 = CARTESIAN_POINT('Ctrl Pts',(-17.9595713839581,-42.0350738739368,
123.825153894762)) ;
#62993 = CARTESIAN_POINT('Ctrl Pts',(-18.2495067533621,-41.8550847935739,
123.742474085264)) ;
#62994 = CARTESIAN_POINT('Ctrl Pts',(-18.0520856877186,-42.0449610519785,
124.067987197481)) ;
#62995 = CARTESIAN_POINT('Ctrl Pts',(-18.3235158644063,-41.8649719716156,
123.93674127071)) ;
#62996 = CARTESIAN_POINT('Ctrl Pts',(-18.187066988808,-42.0549894313466,124.294288291678)) ;
#62997 = CARTESIAN_POINT('Ctrl Pts',(-18.4314996700195,-41.8750003509838,
124.117783890498)) ;
#62998 = CARTESIAN_POINT('Ctrl Pts',(-18.3569254897191,-42.0648836740681,
124.491191503969)) ;
#62999 = CARTESIAN_POINT('Ctrl Pts',(-18.5673820062169,-41.8848945937052,
124.275305521873)) ;
#63000 = CARTESIAN_POINT('Ctrl Pts',(-18.6285705558117,-42.078236590719,124.71326978042)) ;
#63001 = CARTESIAN_POINT('Ctrl Pts',(-18.7847096513815,-41.8982475103561,
124.452982209414)) ;
#63002 = CARTESIAN_POINT('Ctrl Pts',(-18.948377526286,-42.0914391084657,124.857795814166)) ;
#63003 = CARTESIAN_POINT('Ctrl Pts',(-19.0405786175282,-41.9114500281029,
124.568605567899)) ;
#63004 = CARTESIAN_POINT('Ctrl Pts',(-19.2946442505059,-42.1047950137467,
124.914924015773)) ;
#63005 = CARTESIAN_POINT('Ctrl Pts',(-19.3175485758015,-41.9248059333838,
124.614299551762)) ;
#63006 = CARTESIAN_POINT('Ctrl Pts',(-19.5547381910601,-42.1146916623845,
124.912293117139)) ;
#63007 = CARTESIAN_POINT('Ctrl Pts',(-19.5256324094928,-41.9347025820217,
124.612199382613)) ;
#63008 = CARTESIAN_POINT('Ctrl Pts',(-19.8142993016192,-42.124739800437,124.86390602345)) ;
#63009 = CARTESIAN_POINT('Ctrl Pts',(-19.7332792909241,-41.9447507200741,
124.573491312428)) ;
#63010 = CARTESIAN_POINT('Ctrl Pts',(-20.0576759368903,-42.1346307606148,
124.772616402038)) ;
#63011 = CARTESIAN_POINT('Ctrl Pts',(-19.9279820995287,-41.9546416802519,
124.500461812852)) ;
#63012 = CARTESIAN_POINT('Ctrl Pts',(-20.2841432703349,-42.1446235964915,
124.639664036342)) ;
#63013 = CARTESIAN_POINT('Ctrl Pts',(-20.1091567936653,-41.9646345161287,
124.394101924367)) ;
#63014 = CARTESIAN_POINT('Ctrl Pts',(-20.4846006078538,-42.1546626914931,
124.468172605259)) ;
#63015 = CARTESIAN_POINT('Ctrl Pts',(-20.269524451752,-41.9746736111302,124.256910062148)) ;
#63016 = CARTESIAN_POINT('Ctrl Pts',(-20.6493590677972,-42.1645000473443,
124.268925825602)) ;
#63017 = CARTESIAN_POINT('Ctrl Pts',(-20.4013316292031,-41.9845109669814,
124.097515752566)) ;
#63018 = CARTESIAN_POINT('Ctrl Pts',(-20.8232941424064,-42.177892995275,123.963015567167)) ;
#63019 = CARTESIAN_POINT('Ctrl Pts',(-20.5404892049295,-41.9979039149121,
123.85277973288)) ;
#63020 = CARTESIAN_POINT('Ctrl Pts',(-20.9119427186459,-42.1910596717019,
123.624389608226)) ;
#63021 = CARTESIAN_POINT('Ctrl Pts',(-20.6114090656495,-42.0110705913391,
123.581847590379)) ;
#63022 = CARTESIAN_POINT('Ctrl Pts',(-20.9103198254801,-42.2044444531087,
123.272710611957)) ;
#63023 = CARTESIAN_POINT('Ctrl Pts',(-20.6101088464383,-42.0244553727458,
123.300551791675)) ;
#63024 = CARTESIAN_POINT('Ctrl Pts',(-20.8642332429121,-42.2143062357526,
123.017641919768)) ;
#63025 = CARTESIAN_POINT('Ctrl Pts',(-20.5732425041568,-42.0343171553897,
123.096486611068)) ;
#63026 = CARTESIAN_POINT('Ctrl Pts',(-20.7737441303443,-42.2243053837056,
122.771002649473)) ;
#63027 = CARTESIAN_POINT('Ctrl Pts',(-20.5008532527009,-42.0443163033428,
122.899177173043)) ;
#63028 = CARTESIAN_POINT('Ctrl Pts',(-20.6432311626779,-42.2342081763227,
122.545797674276)) ;
#63029 = CARTESIAN_POINT('Ctrl Pts',(-20.3964433972298,-42.0542190959598,
122.71901073462)) ;
#63030 = CARTESIAN_POINT('Ctrl Pts',(-20.4731343577102,-42.2442577562136,
122.343862138749)) ;
#63031 = CARTESIAN_POINT('Ctrl Pts',(-20.2603721024993,-42.0642686758508,
122.557463185732)) ;
#63032 = CARTESIAN_POINT('Ctrl Pts',(-20.2076003346992,-42.2574448300231,
122.12099560958)) ;
#63033 = CARTESIAN_POINT('Ctrl Pts',(-20.0479240767754,-42.0774557496602,
122.379158188714)) ;
#63034 = CARTESIAN_POINT('Ctrl Pts',(-19.8041265873875,-42.2741976199943,
121.933081385993)) ;
#63035 = CARTESIAN_POINT('Ctrl Pts',(-19.7251863995672,-42.0942085396314,
122.228834129982)) ;
#63036 = CARTESIAN_POINT('Ctrl Pts',(-19.3673812946828,-42.290686272089,121.894819463525)) ;
#63037 = CARTESIAN_POINT('Ctrl Pts',(-19.3757249718531,-42.1106971917261,
122.198219603723)) ;
#63038 = CARTESIAN_POINT('Ctrl Pts',(-19.0216618585074,-42.3040430982724,
121.955010874022)) ;
#63039 = CARTESIAN_POINT('Ctrl Pts',(-19.0992014122385,-42.1240540179095,
122.246369156977)) ;
#63040 = CARTESIAN_POINT('Ctrl Pts',(-18.7769948829387,-42.3139394831503,
122.043336388622)) ;
#63041 = CARTESIAN_POINT('Ctrl Pts',(-18.9034558730959,-42.1339504027875,
122.31702867763)) ;
#63042 = CARTESIAN_POINT('Ctrl Pts',(-18.5489107993243,-42.3239459976708,
122.174062497428)) ;
#63043 = CARTESIAN_POINT('Ctrl Pts',(-18.7209920470431,-42.1439569173079,
122.421605740756)) ;
#63044 = CARTESIAN_POINT('Ctrl Pts',(-18.2820313956166,-42.3371361211872,
122.395439854909)) ;
#63045 = CARTESIAN_POINT('Ctrl Pts',(-18.5074779287399,-42.1571470408243,
122.598716881194)) ;
#63046 = CARTESIAN_POINT('Ctrl Pts',(-18.0248416307128,-42.3539026823368,
122.759167368776)) ;
#63047 = CARTESIAN_POINT('Ctrl Pts',(-18.3017330244153,-42.1739136019739,
122.889684714368)) ;
#63048 = CARTESIAN_POINT('Ctrl Pts',(-17.886048515107,-42.3736871710448,123.266512292216)) ;
#63049 = CARTESIAN_POINT('Ctrl Pts',(-18.190691850351,-42.1936980906819,123.295564709079)) ;
#63050 = CARTESIAN_POINT('Ctrl Pts',(-17.9274046621304,-42.3936326186413,
123.794881011967)) ;
#63051 = CARTESIAN_POINT('Ctrl Pts',(-18.2237744875469,-42.2136435382784,
123.718259302305)) ;
#63052 = CARTESIAN_POINT('Ctrl Pts',(-18.1467300052869,-42.4135442807972,
124.276525572974)) ;
#63053 = CARTESIAN_POINT('Ctrl Pts',(-18.3992319711091,-42.2335552004343,
124.103577050796)) ;
#63054 = CARTESIAN_POINT('Ctrl Pts',(-18.5161004763561,-42.4334364728161,
124.654913018434)) ;
#63055 = CARTESIAN_POINT('Ctrl Pts',(-18.6947270610426,-42.2534473924532,
124.40628936176)) ;
#63056 = CARTESIAN_POINT('Ctrl Pts',(-18.9961947812989,-42.4534776033707,
124.885472692553)) ;
#63057 = CARTESIAN_POINT('Ctrl Pts',(-19.0788009536354,-42.2734885230078,
124.590739459069)) ;
#63058 = CARTESIAN_POINT('Ctrl Pts',(-19.5204288936076,-42.4732959379863,
124.938073341943)) ;
#63059 = CARTESIAN_POINT('Ctrl Pts',(-19.4981894659672,-42.2933068576234,
124.632822663084)) ;
#63060 = CARTESIAN_POINT('Ctrl Pts',(-20.0350303911064,-42.4932685032059,
124.808520139639)) ;
#63061 = CARTESIAN_POINT('Ctrl Pts',(-19.9098714983823,-42.313279422843,124.529182116314)) ;
#63062 = CARTESIAN_POINT('Ctrl Pts',(-20.473087584271,-42.5131577193775,124.512279231662)) ;
#63063 = CARTESIAN_POINT('Ctrl Pts',(-20.2603191389922,-42.3331686390146,
124.292190423348)) ;
#63064 = CARTESIAN_POINT('Ctrl Pts',(-20.7853676285003,-42.5331812937002,
124.081500341418)) ;
#63065 = CARTESIAN_POINT('Ctrl Pts',(-20.510144598529,-42.3531922133373,123.947568642154)) ;
#63066 = CARTESIAN_POINT('Ctrl Pts',(-20.9306728526506,-42.5529784567885,
123.575689148436)) ;
#63067 = CARTESIAN_POINT('Ctrl Pts',(-20.6263909037281,-42.3729893764256,
123.542918090147)) ;
#63068 = CARTESIAN_POINT('Ctrl Pts',(-20.8956352696577,-42.5729439506122,
123.046309019479)) ;
#63069 = CARTESIAN_POINT('Ctrl Pts',(-20.5983617160724,-42.3929548702494,
123.119413476898)) ;
#63070 = CARTESIAN_POINT('Ctrl Pts',(-20.6814765719901,-42.5928976583536,
122.560980844406)) ;
#63071 = CARTESIAN_POINT('Ctrl Pts',(-20.4270354944749,-42.4129085779908,
122.731150136192)) ;
#63072 = CARTESIAN_POINT('Ctrl Pts',(-20.3156068294175,-42.6128050350802,
122.178926648595)) ;
#63073 = CARTESIAN_POINT('Ctrl Pts',(-20.1343395078316,-42.4328159547174,
122.425505382769)) ;
#63074 = CARTESIAN_POINT('Ctrl Pts',(-19.8430795028509,-42.6326572466288,
121.943950043858)) ;
#63075 = CARTESIAN_POINT('Ctrl Pts',(-19.7563159223275,-42.4526681662659,
122.237523311971)) ;
#63076 = CARTESIAN_POINT('Ctrl Pts',(-19.3129641321421,-42.6527296335745,
121.884197616228)) ;
#63077 = CARTESIAN_POINT('Ctrl Pts',(-19.3322245789558,-42.4727405532116,
122.189721484159)) ;
#63078 = CARTESIAN_POINT('Ctrl Pts',(-18.8004818960636,-42.6725675032148,
122.008159120081)) ;
#63079 = CARTESIAN_POINT('Ctrl Pts',(-18.9222366927177,-42.4925784228519,
122.288891090315)) ;
#63080 = CARTESIAN_POINT('Ctrl Pts',(-18.3595239816206,-42.6924181577679,
122.297834685126)) ;
#63081 = CARTESIAN_POINT('Ctrl Pts',(-18.5694695547567,-42.5124290774051,
122.52063348008)) ;
#63082 = CARTESIAN_POINT('Ctrl Pts',(-18.0413332378271,-42.7124700921084,
122.725319925752)) ;
#63083 = CARTESIAN_POINT('Ctrl Pts',(-18.3149181158026,-42.5324810117455,
122.862621797376)) ;
#63084 = CARTESIAN_POINT('Ctrl Pts',(-17.8898151802692,-42.7323032796744,
123.230332622468)) ;
#63085 = CARTESIAN_POINT('Ctrl Pts',(-18.1937042468816,-42.5523141993116,
123.266634019015)) ;
#63086 = CARTESIAN_POINT('Ctrl Pts',(-17.9188018275413,-42.7522324919051,
123.759028000003)) ;
#63087 = CARTESIAN_POINT('Ctrl Pts',(-18.2168953694706,-42.5722434115422,
123.689590983492)) ;
#63088 = CARTESIAN_POINT('Ctrl Pts',(-18.1255818945999,-42.7721174571195,
124.245626671825)) ;
#63089 = CARTESIAN_POINT('Ctrl Pts',(-18.3823217704082,-42.5921283767566,
124.078870010309)) ;
#63090 = CARTESIAN_POINT('Ctrl Pts',(-18.4898112910282,-42.7921911982641,
124.635336040243)) ;
#63091 = CARTESIAN_POINT('Ctrl Pts',(-18.6737062691616,-42.6122021179012,
124.390635650376)) ;
#63092 = CARTESIAN_POINT('Ctrl Pts',(-18.9586591560268,-42.8119843800445,
124.874120892103)) ;
#63093 = CARTESIAN_POINT('Ctrl Pts',(-19.0487871981899,-42.6319952996816,
124.581662463708)) ;
#63094 = CARTESIAN_POINT('Ctrl Pts',(-19.4849952307029,-42.8319470880472,
124.940716397595)) ;
#63095 = CARTESIAN_POINT('Ctrl Pts',(-19.4698566611138,-42.6519580076843,
124.634936088449)) ;
#63096 = CARTESIAN_POINT('Ctrl Pts',(-20.0027532085215,-42.8519300397896,
124.822320272742)) ;
#63097 = CARTESIAN_POINT('Ctrl Pts',(-19.8840626043544,-42.6719409594268,
124.540216680374)) ;
#63098 = CARTESIAN_POINT('Ctrl Pts',(-20.4457748038711,-42.8717406595618,
124.537685736192)) ;
#63099 = CARTESIAN_POINT('Ctrl Pts',(-20.2384794300186,-42.6917515791989,
124.312505791514)) ;
#63100 = CARTESIAN_POINT('Ctrl Pts',(-20.7682626054881,-42.8917243755947,
124.115808826861)) ;
#63101 = CARTESIAN_POINT('Ctrl Pts',(-20.496467127968,-42.7117352952318,123.975002213064)) ;
#63102 = CARTESIAN_POINT('Ctrl Pts',(-20.9266062652679,-42.911605839492,123.611535793601)) ;
#63103 = CARTESIAN_POINT('Ctrl Pts',(-20.6231390533387,-42.7316167591292,
123.571582135576)) ;
#63104 = CARTESIAN_POINT('Ctrl Pts',(-20.9036603572419,-42.9315611693364,
123.081759157368)) ;
#63105 = CARTESIAN_POINT('Ctrl Pts',(-20.6047789224965,-42.7515720889735,
123.147760755325)) ;
#63106 = CARTESIAN_POINT('Ctrl Pts',(-20.7024014511106,-42.9514366301419,
122.593252469761)) ;
#63107 = CARTESIAN_POINT('Ctrl Pts',(-20.4437676559676,-42.771447549779,122.756956211372)) ;
#63108 = CARTESIAN_POINT('Ctrl Pts',(-20.3449003201343,-42.9714209501934,
122.200502446689)) ;
#63109 = CARTESIAN_POINT('Ctrl Pts',(-20.1577657851218,-42.7914318698305,
122.442758885575)) ;
#63110 = CARTESIAN_POINT('Ctrl Pts',(-19.8758679528504,-42.991348982983,121.954198379585)) ;
#63111 = CARTESIAN_POINT('Ctrl Pts',(-19.7825308096546,-42.8113599026202,
122.24571839476)) ;
#63112 = CARTESIAN_POINT('Ctrl Pts',(-19.438573167792,-43.0079577449228,121.894584975642)) ;
#63113 = CARTESIAN_POINT('Ctrl Pts',(-19.4327162628233,-42.82796866456,122.198032510649)) ;
#63114 = CARTESIAN_POINT('Ctrl Pts',(-19.0946716817039,-43.0211453836129,
121.937615803098)) ;
#63115 = CARTESIAN_POINT('Ctrl Pts',(-19.1575750804821,-42.84115630325,122.232458887897)) ;
#63116 = CARTESIAN_POINT('Ctrl Pts',(-18.8437153066299,-43.031131817973,122.014331380066)) ;
#63117 = CARTESIAN_POINT('Ctrl Pts',(-18.9568164411077,-42.8511427376102,
122.293831610718)) ;
#63118 = CARTESIAN_POINT('Ctrl Pts',(-18.6094527009105,-43.0411411919324,
122.133980200505)) ;
#63119 = CARTESIAN_POINT('Ctrl Pts',(-18.7693988622901,-42.8611521115695,
122.38956024232)) ;
#63120 = CARTESIAN_POINT('Ctrl Pts',(-18.3305857336724,-43.0544312254977,
122.344252306569)) ;
#63121 = CARTESIAN_POINT('Ctrl Pts',(-18.5463444103637,-42.8744421451348,
122.55774111295)) ;
#63122 = CARTESIAN_POINT('Ctrl Pts',(-18.0587919012148,-43.0710252131601,
122.691613440136)) ;
#63123 = CARTESIAN_POINT('Ctrl Pts',(-18.3288675517154,-42.8910361327973,
122.835684012626)) ;
#63124 = CARTESIAN_POINT('Ctrl Pts',(-17.9215463024505,-43.0876574684357,
123.111805424013)) ;
#63125 = CARTESIAN_POINT('Ctrl Pts',(-18.2190954252728,-42.9076683880728,
123.171796586433)) ;
#63126 = CARTESIAN_POINT('Ctrl Pts',(-17.9026645543824,-43.1008998521035,
123.459298795023)) ;
#63127 = CARTESIAN_POINT('Ctrl Pts',(-18.203983606276,-42.9209107717406,123.449819411052)) ;
#63128 = CARTESIAN_POINT('Ctrl Pts',(-17.9331154384697,-43.1108140603309,
123.718057560274)) ;
#63129 = CARTESIAN_POINT('Ctrl Pts',(-18.2283482599857,-42.9308249799681,
123.656820588526)) ;
#63130 = CARTESIAN_POINT('Ctrl Pts',(-18.0093888248284,-43.1208706996026,
123.971069080689)) ;
#63131 = CARTESIAN_POINT('Ctrl Pts',(-18.2893690473881,-42.9408816192397,
123.859230933456)) ;
#63132 = CARTESIAN_POINT('Ctrl Pts',(-18.1256799001394,-43.1307165060227,
124.202224696424)) ;
#63133 = CARTESIAN_POINT('Ctrl Pts',(-18.3824021684236,-42.9507274256599,
124.044152714525)) ;
#63134 = CARTESIAN_POINT('Ctrl Pts',(-18.2830849970775,-43.1407615056559,
124.414117164475)) ;
#63135 = CARTESIAN_POINT('Ctrl Pts',(-18.5083351697391,-42.960772425293,124.21367093415)) ;
#63136 = CARTESIAN_POINT('Ctrl Pts',(-18.537043251934,-43.1540425280286,124.65350405423)) ;
#63137 = CARTESIAN_POINT('Ctrl Pts',(-18.7114678288813,-42.9740534476658,
124.405150550178)) ;
#63138 = CARTESIAN_POINT('Ctrl Pts',(-18.8452649773422,-43.1672399745533,
124.820961905211)) ;
#63139 = CARTESIAN_POINT('Ctrl Pts',(-18.9580634355738,-42.9872508941904,
124.539134958599)) ;
#63140 = CARTESIAN_POINT('Ctrl Pts',(-19.1881152200042,-43.1806542723603,
124.902985565981)) ;
#63141 = CARTESIAN_POINT('Ctrl Pts',(-19.232360308715,-43.0006651919974,124.604753983446)) ;
#63142 = CARTESIAN_POINT('Ctrl Pts',(-19.4462101896744,-43.190493337763,124.918723959337)) ;
#63143 = CARTESIAN_POINT('Ctrl Pts',(-19.4388332239247,-43.0105042574002,
124.617341843955)) ;
#63144 = CARTESIAN_POINT('Ctrl Pts',(-19.7069166424415,-43.2004765440407,
124.889671060815)) ;
#63145 = CARTESIAN_POINT('Ctrl Pts',(-19.6473989352599,-43.0204874636778,
124.594097446698)) ;
#63146 = CARTESIAN_POINT('Ctrl Pts',(-19.9578281238234,-43.2104277789535,
124.815931888651)) ;
#63147 = CARTESIAN_POINT('Ctrl Pts',(-19.8481272005172,-43.0304386985906,
124.535103914391)) ;
#63148 = CARTESIAN_POINT('Ctrl Pts',(-20.1934350689946,-43.2204287786551,
124.699450981921)) ;
#63149 = CARTESIAN_POINT('Ctrl Pts',(-20.0366117625381,-43.0404396982923,
124.441917204073)) ;
#63150 = CARTESIAN_POINT('Ctrl Pts',(-20.4056235278496,-43.2304601244425,
124.543033701341)) ;
#63151 = CARTESIAN_POINT('Ctrl Pts',(-20.206361135427,-43.0504710440796,124.316781584499)) ;
#63152 = CARTESIAN_POINT('Ctrl Pts',(-20.5844761556059,-43.2403138891475,
124.355767995576)) ;
#63153 = CARTESIAN_POINT('Ctrl Pts',(-20.3494415434613,-43.0603248087846,
124.166967530126)) ;
#63154 = CARTESIAN_POINT('Ctrl Pts',(-20.7303004788071,-43.2502845428158,
124.138111587072)) ;
#63155 = CARTESIAN_POINT('Ctrl Pts',(-20.4660990801308,-43.0702954624529,
123.992841228193)) ;
#63156 = CARTESIAN_POINT('Ctrl Pts',(-20.836417878929,-43.260281786473,123.897736472941)) ;
#63157 = CARTESIAN_POINT('Ctrl Pts',(-20.5509909214164,-43.0802927061101,
123.800540288638)) ;
#63158 = CARTESIAN_POINT('Ctrl Pts',(-20.8990697974022,-43.2703152424172,
123.641641842364)) ;
#63159 = CARTESIAN_POINT('Ctrl Pts',(-20.6011102563004,-43.0903261620543,
123.595664077152)) ;
#63160 = CARTESIAN_POINT('Ctrl Pts',(-20.9164201484356,-43.2801707467176,
123.383205983392)) ;
#63161 = CARTESIAN_POINT('Ctrl Pts',(-20.6149882875894,-43.1001816663547,
123.388915428103)) ;
#63162 = CARTESIAN_POINT('Ctrl Pts',(-20.8885847142338,-43.2901701830037,
123.121956715712)) ;
#63163 = CARTESIAN_POINT('Ctrl Pts',(-20.5927177264753,-43.1101811026408,
123.17991632247)) ;
#63164 = CARTESIAN_POINT('Ctrl Pts',(-20.8168337005953,-43.3000646425196,
122.871985466953)) ;
#63165 = CARTESIAN_POINT('Ctrl Pts',(-20.5353148477446,-43.1200755621567,
122.979940136269)) ;
#63166 = CARTESIAN_POINT('Ctrl Pts',(-20.7007964614407,-43.3101277619712,
122.634405971093)) ;
#63167 = CARTESIAN_POINT('Ctrl Pts',(-20.4424830472007,-43.1301386816084,
122.789877488713)) ;
#63168 = CARTESIAN_POINT('Ctrl Pts',(-20.5489034190072,-43.3199673963832,
122.425092863815)) ;
#63169 = CARTESIAN_POINT('Ctrl Pts',(-20.3209670269666,-43.1399783160204,
122.622428563072)) ;
#63170 = CARTESIAN_POINT('Ctrl Pts',(-20.3590408300149,-43.330030603869,122.2410636791)) ;
#63171 = CARTESIAN_POINT('Ctrl Pts',(-20.1690754107749,-43.1500415235061,
122.475206756355)) ;
#63172 = CARTESIAN_POINT('Ctrl Pts',(-20.1436111274021,-43.3399247112482,
122.095429795694)) ;
#63173 = CARTESIAN_POINT('Ctrl Pts',(-19.9967306388888,-43.1599356308853,
122.358701616965)) ;
#63174 = CARTESIAN_POINT('Ctrl Pts',(-19.9053553865041,-43.3498670434406,
121.988285686092)) ;
#63175 = CARTESIAN_POINT('Ctrl Pts',(-19.8061253596654,-43.1698779630777,
122.272988371083)) ;
#63176 = CARTESIAN_POINT('Ctrl Pts',(-19.6505873376339,-43.3598676697556,
121.923617759925)) ;
#63177 = CARTESIAN_POINT('Ctrl Pts',(-19.6023104651923,-43.1798785893927,
122.221256110046)) ;
#63178 = CARTESIAN_POINT('Ctrl Pts',(-19.3874126433953,-43.3699094040375,
121.904584247529)) ;
#63179 = CARTESIAN_POINT('Ctrl Pts',(-19.391770525899,-43.1899203236746,122.206031467427)) ;
#63180 = CARTESIAN_POINT('Ctrl Pts',(-19.1304837624484,-43.3797348299866,
121.930388446646)) ;
#63181 = CARTESIAN_POINT('Ctrl Pts',(-19.1862281367957,-43.1997457496237,
122.226676884756)) ;
#63182 = CARTESIAN_POINT('Ctrl Pts',(-18.876016923458,-43.3897916565143,122.001672516022)) ;
#63183 = CARTESIAN_POINT('Ctrl Pts',(-18.9826551632411,-43.2098025761514,
122.283706165014)) ;
#63184 = CARTESIAN_POINT('Ctrl Pts',(-18.6409865992809,-43.3997190896358,
122.114930897131)) ;
#63185 = CARTESIAN_POINT('Ctrl Pts',(-18.7946320604858,-43.219730009273,122.374314665372)) ;
#63186 = CARTESIAN_POINT('Ctrl Pts',(-18.428277440835,-43.4096690820421,122.267013929381)) ;
#63187 = CARTESIAN_POINT('Ctrl Pts',(-18.6244661072569,-43.2296800016792,
122.495982618452)) ;
#63188 = CARTESIAN_POINT('Ctrl Pts',(-18.2436237169547,-43.4197242831161,
122.456000772691)) ;
#63189 = CARTESIAN_POINT('Ctrl Pts',(-18.4767445661238,-43.2397352027532,
122.647173618493)) ;
#63190 = CARTESIAN_POINT('Ctrl Pts',(-18.0976352137637,-43.4295465571684,
122.668893815947)) ;
#63191 = CARTESIAN_POINT('Ctrl Pts',(-18.3599557989295,-43.2495574768055,
122.817488687827)) ;
#63192 = CARTESIAN_POINT('Ctrl Pts',(-17.987876075402,-43.4396024511276,122.909259308021)) ;
#63193 = CARTESIAN_POINT('Ctrl Pts',(-18.272150254971,-43.2596133707647,123.009781985742)) ;
#63194 = CARTESIAN_POINT('Ctrl Pts',(-17.9227225617815,-43.4495431729727,
123.162245934171)) ;
#63195 = CARTESIAN_POINT('Ctrl Pts',(-18.2200294874287,-43.2695540926099,
123.212171536294)) ;
#63196 = CARTESIAN_POINT('Ctrl Pts',(-17.9017472036595,-43.4594475170593,
123.421680109374)) ;
#63197 = CARTESIAN_POINT('Ctrl Pts',(-18.2032511636437,-43.2794584366965,
123.41971860684)) ;
#63198 = CARTESIAN_POINT('Ctrl Pts',(-17.926651728431,-43.4694941843588,123.684496298927)) ;
#63199 = CARTESIAN_POINT('Ctrl Pts',(-18.2231767399461,-43.2895051039959,
123.629971456514)) ;
#63200 = CARTESIAN_POINT('Ctrl Pts',(-17.9955444787495,-43.4793897428087,
123.935293204385)) ;
#63201 = CARTESIAN_POINT('Ctrl Pts',(-18.2782926706353,-43.2994006624459,
123.830608021522)) ;
#63202 = CARTESIAN_POINT('Ctrl Pts',(-18.1087774586024,-43.4894518215134,
124.174200467457)) ;
#63203 = CARTESIAN_POINT('Ctrl Pts',(-18.3688808575243,-43.3094627411505,
124.021733139343)) ;
#63204 = CARTESIAN_POINT('Ctrl Pts',(-18.258354480537,-43.4992945199792,124.38525663974)) ;
#63205 = CARTESIAN_POINT('Ctrl Pts',(-18.4885436261305,-43.3193054396163,
124.19057641101)) ;
#63206 = CARTESIAN_POINT('Ctrl Pts',(-18.4445910638163,-43.5092852938737,
124.570269448432)) ;
#63207 = CARTESIAN_POINT('Ctrl Pts',(-18.6375340693141,-43.3292962135108,
124.338585274364)) ;
#63208 = CARTESIAN_POINT('Ctrl Pts',(-18.6588280253988,-43.5192131631086,
124.719179491474)) ;
#63209 = CARTESIAN_POINT('Ctrl Pts',(-18.8089243549263,-43.3392240827457,
124.457711595414)) ;
#63210 = CARTESIAN_POINT('Ctrl Pts',(-18.8969249830435,-43.5292018920784,
124.829722059016)) ;
#63211 = CARTESIAN_POINT('Ctrl Pts',(-18.9994025173376,-43.3492128117156,
124.546144008221)) ;
#63212 = CARTESIAN_POINT('Ctrl Pts',(-19.1519853155007,-43.5392412940622,
124.897107996918)) ;
#63213 = CARTESIAN_POINT('Ctrl Pts',(-19.2034513317484,-43.3592522136993,
124.600051019993)) ;
#63214 = CARTESIAN_POINT('Ctrl Pts',(-19.4096395220042,-43.549081461799,124.91925607013)) ;
#63215 = CARTESIAN_POINT('Ctrl Pts',(-19.4095740497206,-43.3690923814361,
124.617767680726)) ;
#63216 = CARTESIAN_POINT('Ctrl Pts',(-19.6726790143965,-43.5591296721735,
124.896233588286)) ;
#63217 = CARTESIAN_POINT('Ctrl Pts',(-19.6200056228297,-43.3791405918106,
124.599348022425)) ;
#63218 = CARTESIAN_POINT('Ctrl Pts',(-19.9250688422305,-43.5690768424612,
124.828171804027)) ;
#63219 = CARTESIAN_POINT('Ctrl Pts',(-19.8219167126913,-43.3890877620984,
124.544896996661)) ;
#63220 = CARTESIAN_POINT('Ctrl Pts',(-20.1612764162791,-43.5789876907163,
124.718431010593)) ;
#63221 = CARTESIAN_POINT('Ctrl Pts',(-20.0108816130576,-43.3989986103534,
124.457103131757)) ;
#63222 = CARTESIAN_POINT('Ctrl Pts',(-20.3778135163567,-43.5890440183941,
124.566965650242)) ;
#63223 = CARTESIAN_POINT('Ctrl Pts',(-20.1841104958632,-43.4090549380312,
124.335929390239)) ;
#63224 = CARTESIAN_POINT('Ctrl Pts',(-20.561112631005,-43.5988944311626,124.384166137477)) ;
#63225 = CARTESIAN_POINT('Ctrl Pts',(-20.3307480642774,-43.4189053507997,
124.189689229524)) ;
#63226 = CARTESIAN_POINT('Ctrl Pts',(-20.7130674436225,-43.6089213169963,
124.168903399289)) ;
#63227 = CARTESIAN_POINT('Ctrl Pts',(-20.4523107179373,-43.4289322366334,
124.017478157488)) ;
#63228 = CARTESIAN_POINT('Ctrl Pts',(-20.8247441401648,-43.6189499326271,
123.930180059024)) ;
#63229 = CARTESIAN_POINT('Ctrl Pts',(-20.5416506341111,-43.4389608522643,
123.82649874937)) ;
#63230 = CARTESIAN_POINT('Ctrl Pts',(-20.8924859435401,-43.6287951560046,
123.680497788512)) ;
#63231 = CARTESIAN_POINT('Ctrl Pts',(-20.5958423726042,-43.4488060756417,
123.626753399107)) ;
#63232 = CARTESIAN_POINT('Ctrl Pts',(-20.9168945752152,-43.6387858381062,
123.419083293922)) ;
#63233 = CARTESIAN_POINT('Ctrl Pts',(-20.6153678869585,-43.4587967577433,
123.417621830856)) ;
#63234 = CARTESIAN_POINT('Ctrl Pts',(-20.8948561360059,-43.6488237267386,
123.156223171646)) ;
#63235 = CARTESIAN_POINT('Ctrl Pts',(-20.5977356311787,-43.4688346463758,
123.207333751848)) ;
#63236 = CARTESIAN_POINT('Ctrl Pts',(-20.8292438813552,-43.6586680618418,
122.905971997117)) ;
#63237 = CARTESIAN_POINT('Ctrl Pts',(-20.5452447033601,-43.4786789814789,
123.00713407774)) ;
#63238 = CARTESIAN_POINT('Ctrl Pts',(-20.7201211840109,-43.6686530240393,
122.667383970185)) ;
#63239 = CARTESIAN_POINT('Ctrl Pts',(-20.4579454445687,-43.4886639436764,
122.816264379379)) ;
#63240 = CARTESIAN_POINT('Ctrl Pts',(-20.5719738572654,-43.6785919655727,
122.452232949088)) ;
#63241 = CARTESIAN_POINT('Ctrl Pts',(-20.3394267805854,-43.4986028852098,
122.644144644649)) ;
#63242 = CARTESIAN_POINT('Ctrl Pts',(-20.3868068904669,-43.6886338505441,
122.264249292356)) ;
#63243 = CARTESIAN_POINT('Ctrl Pts',(-20.1912922023766,-43.5086447701812,
122.493758541871)) ;
#63244 = CARTESIAN_POINT('Ctrl Pts',(-20.1751934660884,-43.6985203984524,
122.113473137318)) ;
#63245 = CARTESIAN_POINT('Ctrl Pts',(-20.0220013410477,-43.5185313180895,
122.373139073177)) ;
#63246 = CARTESIAN_POINT('Ctrl Pts',(-19.9382875919748,-43.7085143239524,
122.000193047115)) ;
#63247 = CARTESIAN_POINT('Ctrl Pts',(-19.8324762632877,-43.5285252435895,
122.282516123217)) ;
#63248 = CARTESIAN_POINT('Ctrl Pts',(-19.6867374287566,-43.7184504150789,
121.930037797555)) ;
#63249 = CARTESIAN_POINT('Ctrl Pts',(-19.631236272687,-43.538461334716,122.226393150879)) ;
#63250 = CARTESIAN_POINT('Ctrl Pts',(-19.4244597082895,-43.7284796840588,
121.904445450491)) ;
#63251 = CARTESIAN_POINT('Ctrl Pts',(-19.4214139225834,-43.5484906036959,
122.205920422987)) ;
#63252 = CARTESIAN_POINT('Ctrl Pts',(-19.1654713412245,-43.7383620666181,
121.924160359803)) ;
#63253 = CARTESIAN_POINT('Ctrl Pts',(-19.2142241183985,-43.5583729862552,
122.221693371168)) ;
#63254 = CARTESIAN_POINT('Ctrl Pts',(-18.909564469388,-43.748414583706,121.989548406113)) ;
#63255 = CARTESIAN_POINT('Ctrl Pts',(-19.0094986897132,-43.5684255033431,
122.274004889728)) ;
#63256 = CARTESIAN_POINT('Ctrl Pts',(-18.672555542748,-43.7583087045299,122.096577505371)) ;
#63257 = CARTESIAN_POINT('Ctrl Pts',(-18.8198926461261,-43.578319624167,122.359628808823)) ;
#63258 = CARTESIAN_POINT('Ctrl Pts',(-18.4541166120411,-43.7683706839503,
122.245521781435)) ;
#63259 = CARTESIAN_POINT('Ctrl Pts',(-18.6451418602276,-43.5883816035874,
122.478785221664)) ;
#63260 = CARTESIAN_POINT('Ctrl Pts',(-18.2688956918944,-43.7782152171792,
122.426149066543)) ;
#63261 = CARTESIAN_POINT('Ctrl Pts',(-18.4969665901332,-43.5982261368164,
122.623287037953)) ;
#63262 = CARTESIAN_POINT('Ctrl Pts',(-18.1153222214896,-43.7881752960855,
122.63809537997)) ;
#63263 = CARTESIAN_POINT('Ctrl Pts',(-18.3741086705153,-43.6081862157226,
122.792844257825)) ;
#63264 = CARTESIAN_POINT('Ctrl Pts',(-18.0004538039104,-43.7982135726581,
122.875554226971)) ;
#63265 = CARTESIAN_POINT('Ctrl Pts',(-18.2822147043336,-43.6182244922952,
122.982811851236)) ;
#63266 = CARTESIAN_POINT('Ctrl Pts',(-17.9292494152414,-43.8080869591959,
123.125095646778)) ;
#63267 = CARTESIAN_POINT('Ctrl Pts',(-18.225252205665,-43.6280978788331,123.182444339761)) ;
#63268 = CARTESIAN_POINT('Ctrl Pts',(-17.902000155212,-43.818159901963,123.388344568531)) ;
#63269 = CARTESIAN_POINT('Ctrl Pts',(-18.2034535746662,-43.6381708216001,
123.393043900429)) ;
#63270 = CARTESIAN_POINT('Ctrl Pts',(-17.9200947062017,-43.8279813160913,
123.645856942376)) ;
#63271 = CARTESIAN_POINT('Ctrl Pts',(-18.2179298642884,-43.6479922357285,
123.599052510802)) ;
#63272 = CARTESIAN_POINT('Ctrl Pts',(-17.9839061111706,-43.8380559461636,
123.902752660032)) ;
#63273 = CARTESIAN_POINT('Ctrl Pts',(-18.2689797188223,-43.6580668658008,
123.804569272354)) ;
#63274 = CARTESIAN_POINT('Ctrl Pts',(-18.0892674357171,-43.8479225834805,
124.139701464723)) ;
#63275 = CARTESIAN_POINT('Ctrl Pts',(-18.353269010714,-43.6679335031176,123.99412714447)) ;
#63276 = CARTESIAN_POINT('Ctrl Pts',(-18.2358881550822,-43.8579461288523,
124.358516056916)) ;
#63277 = CARTESIAN_POINT('Ctrl Pts',(-18.4705660406864,-43.6779570484894,
124.169178557313)) ;
#63278 = CARTESIAN_POINT('Ctrl Pts',(-18.4187926357899,-43.8679718803695,
124.54817037461)) ;
#63279 = CARTESIAN_POINT('Ctrl Pts',(-18.6168901651521,-43.6879828000066,
124.320901587011)) ;
#63280 = CARTESIAN_POINT('Ctrl Pts',(-18.6279123309116,-43.8778254673789,
124.700856473428)) ;
#63281 = CARTESIAN_POINT('Ctrl Pts',(-18.7841853999482,-43.697836387016,124.443049376181)) ;
#63282 = CARTESIAN_POINT('Ctrl Pts',(-18.8629865023443,-43.8878024276068,
124.816974766263)) ;
#63283 = CARTESIAN_POINT('Ctrl Pts',(-18.9722446774819,-43.7078133472439,
124.535943532528)) ;
#63284 = CARTESIAN_POINT('Ctrl Pts',(-19.1158727506149,-43.8978235706353,
124.890405499117)) ;
#63285 = CARTESIAN_POINT('Ctrl Pts',(-19.1745538313907,-43.7178344902724,
124.594687628449)) ;
#63286 = CARTESIAN_POINT('Ctrl Pts',(-19.3740398930884,-43.9077061766552,
124.918943559724)) ;
#63287 = CARTESIAN_POINT('Ctrl Pts',(-19.3810867133437,-43.7277170962923,
124.617517603467)) ;
#63288 = CARTESIAN_POINT('Ctrl Pts',(-19.6380282810842,-43.9177746472879,
124.901808568913)) ;
#63289 = CARTESIAN_POINT('Ctrl Pts',(-19.5922777253755,-43.737785566925,124.603809182427)) ;
#63290 = CARTESIAN_POINT('Ctrl Pts',(-19.889104080618,-43.9276047304716,124.840852015822)) ;
#63291 = CARTESIAN_POINT('Ctrl Pts',(-19.7931370891346,-43.7476156501087,
124.555043909552)) ;
#63292 = CARTESIAN_POINT('Ctrl Pts',(-20.1315321754818,-43.937671290152,124.735084209406)) ;
#63293 = CARTESIAN_POINT('Ctrl Pts',(-19.9870797585783,-43.7576822097891,
124.470429312396)) ;
#63294 = CARTESIAN_POINT('Ctrl Pts',(-20.3480256593167,-43.9475615399812,
124.591215461382)) ;
#63295 = CARTESIAN_POINT('Ctrl Pts',(-20.1602736880261,-43.7675724596183,
124.355334538994)) ;
#63296 = CARTESIAN_POINT('Ctrl Pts',(-20.5385520107773,-43.95755370573,124.41054400151)) ;
#63297 = CARTESIAN_POINT('Ctrl Pts',(-20.3126945474677,-43.7775646253671,
124.210797386208)) ;
#63298 = CARTESIAN_POINT('Ctrl Pts',(-20.6941599747678,-43.9675165493261,
124.199999732193)) ;
#63299 = CARTESIAN_POINT('Ctrl Pts',(-20.4371805360489,-43.7875274689632,
124.042362141687)) ;
#63300 = CARTESIAN_POINT('Ctrl Pts',(-20.8107661786076,-43.9774207181539,
123.967284902334)) ;
#63301 = CARTESIAN_POINT('Ctrl Pts',(-20.5304651300537,-43.797431637791,123.856190933871)) ;
#63302 = CARTESIAN_POINT('Ctrl Pts',(-20.8861267321908,-43.9874815930482,
123.713900101275)) ;
#63303 = CARTESIAN_POINT('Ctrl Pts',(-20.5907535610701,-43.8074925126853,
123.653482792957)) ;
#63304 = CARTESIAN_POINT('Ctrl Pts',(-20.9160480543138,-43.9973204963776,
123.457038808334)) ;
#63305 = CARTESIAN_POINT('Ctrl Pts',(-20.6146904768429,-43.8173314160147,
123.44799493269)) ;
#63306 = CARTESIAN_POINT('Ctrl Pts',(-20.9008215569112,-44.0073888727515,
123.192934464757)) ;
#63307 = CARTESIAN_POINT('Ctrl Pts',(-20.6025093217577,-43.8273997923886,
123.236711133605)) ;
#63308 = CARTESIAN_POINT('Ctrl Pts',(-20.8409996767229,-44.0172694893841,
122.940227571329)) ;
#63309 = CARTESIAN_POINT('Ctrl Pts',(-20.5546520629352,-43.8372804090212,
123.034546490848)) ;
#63310 = CARTESIAN_POINT('Ctrl Pts',(-20.7375752826336,-44.0272606496131,
122.698940269794)) ;
#63311 = CARTESIAN_POINT('Ctrl Pts',(-20.4719127723535,-43.8472715692502,
122.841516743795)) ;
#63312 = CARTESIAN_POINT('Ctrl Pts',(-20.5943672382838,-44.0372137230452,
122.480025241818)) ;
#63313 = CARTESIAN_POINT('Ctrl Pts',(-20.357346713871,-43.8572246426823,122.666384965214)) ;
#63314 = CARTESIAN_POINT('Ctrl Pts',(-20.413814021043,-44.0472495586578,122.28781904818)) ;
#63315 = CARTESIAN_POINT('Ctrl Pts',(-20.212904171313,-43.867260478295,122.512619815452)) ;
#63316 = CARTESIAN_POINT('Ctrl Pts',(-20.2057716275745,-44.057139685388,122.132010547474)) ;
#63317 = CARTESIAN_POINT('Ctrl Pts',(-20.0464710629452,-43.8771506050251,
122.387973367554)) ;
#63318 = CARTESIAN_POINT('Ctrl Pts',(-19.9716606492844,-44.0671318671573,
122.013118819397)) ;
#63319 = CARTESIAN_POINT('Ctrl Pts',(-19.8591825691405,-43.8871427867944,
122.292859783673)) ;
#63320 = CARTESIAN_POINT('Ctrl Pts',(-19.721585969689,-44.0770778071318,121.93711664901)) ;
#63321 = CARTESIAN_POINT('Ctrl Pts',(-19.6591233631449,-43.8970887267689,
122.232057912344)) ;
#63322 = CARTESIAN_POINT('Ctrl Pts',(-19.4621316011703,-44.0870249908912,
121.905158079447)) ;
#63323 = CARTESIAN_POINT('Ctrl Pts',(-19.4515603759915,-43.9070359105284,
122.206490695908)) ;
#63324 = CARTESIAN_POINT('Ctrl Pts',(-19.1984633098486,-44.0970729291816,
121.91916626143)) ;
#63325 = CARTESIAN_POINT('Ctrl Pts',(-19.2406255245606,-43.9170838488187,
122.217696907762)) ;
#63326 = CARTESIAN_POINT('Ctrl Pts',(-18.9462999517132,-44.1069205639951,
121.977344862777)) ;
#63327 = CARTESIAN_POINT('Ctrl Pts',(-19.0388958389278,-43.9269314836323,
122.264239147175)) ;
#63328 = CARTESIAN_POINT('Ctrl Pts',(-18.7050030349617,-44.1168822776931,
122.078833023626)) ;
#63329 = CARTESIAN_POINT('Ctrl Pts',(-18.8458584060323,-43.9368931973302,
122.345428976242)) ;
#63330 = CARTESIAN_POINT('Ctrl Pts',(-18.4836721334991,-44.1269109135143,
122.221925767037)) ;
#63331 = CARTESIAN_POINT('Ctrl Pts',(-18.6687933369296,-43.9469218331514,
122.459902775154)) ;
#63332 = CARTESIAN_POINT('Ctrl Pts',(-18.2927904240574,-44.136821228266,122.39907817817)) ;
#63333 = CARTESIAN_POINT('Ctrl Pts',(-18.5160881141208,-43.9568321479032,
122.601623829949)) ;
#63334 = CARTESIAN_POINT('Ctrl Pts',(-18.1346189321038,-44.1467560989287,
122.60679979726)) ;
#63335 = CARTESIAN_POINT('Ctrl Pts',(-18.3895506742922,-43.9667670185658,
122.767800273057)) ;
#63336 = CARTESIAN_POINT('Ctrl Pts',(-18.0138706731733,-44.1567972813305,
122.841409864127)) ;
#63337 = CARTESIAN_POINT('Ctrl Pts',(-18.2929514212946,-43.9768082009676,
122.955488165132)) ;
#63338 = CARTESIAN_POINT('Ctrl Pts',(-17.9366823755265,-44.1666842527952,
123.089522740013)) ;
#63339 = CARTESIAN_POINT('Ctrl Pts',(-18.2312003631439,-43.9866951724323,
123.153977453905)) ;
#63340 = CARTESIAN_POINT('Ctrl Pts',(-17.903048419426,-44.1766836850578,123.350101781409)) ;
#63341 = CARTESIAN_POINT('Ctrl Pts',(-18.2042924372665,-43.9966946046949,
123.36244046689)) ;
#63342 = CARTESIAN_POINT('Ctrl Pts',(-17.9149014701427,-44.1866037503144,
123.610552838708)) ;
#63343 = CARTESIAN_POINT('Ctrl Pts',(-18.213774030704,-44.0066146699516,123.570800751409)) ;
#63344 = CARTESIAN_POINT('Ctrl Pts',(-17.9724055290717,-44.1966406028986,
123.867950986159)) ;
#63345 = CARTESIAN_POINT('Ctrl Pts',(-18.2597764896288,-44.0166515225357,
123.776719574248)) ;
#63346 = CARTESIAN_POINT('Ctrl Pts',(-18.072489495965,-44.2065532622386,124.10845708331)) ;
#63347 = CARTESIAN_POINT('Ctrl Pts',(-18.33984264497,-44.0265641818757,123.969124165985)) ;
#63348 = CARTESIAN_POINT('Ctrl Pts',(-18.2134492761814,-44.2165444741535,
124.329987229818)) ;
#63349 = CARTESIAN_POINT('Ctrl Pts',(-18.4526095642665,-44.0365553937906,
124.146348659042)) ;
#63350 = CARTESIAN_POINT('Ctrl Pts',(-18.3920400927921,-44.2265861155566,
124.524226386298)) ;
#63351 = CARTESIAN_POINT('Ctrl Pts',(-18.5954817048883,-44.0465970351937,
124.301740649263)) ;
#63352 = CARTESIAN_POINT('Ctrl Pts',(-18.5968513118657,-44.2364149097636,
124.681658511536)) ;
#63353 = CARTESIAN_POINT('Ctrl Pts',(-18.7593291698146,-44.0564258294008,
124.427686424433)) ;
#63354 = CARTESIAN_POINT('Ctrl Pts',(-18.8315253713429,-44.2464913208849,
124.804205426187)) ;
#63355 = CARTESIAN_POINT('Ctrl Pts',(-18.9470682569457,-44.066502240522,124.525725008789)) ;
#63356 = CARTESIAN_POINT('Ctrl Pts',(-19.0783578845555,-44.2563434539274,
124.882525081973)) ;
#63357 = CARTESIAN_POINT('Ctrl Pts',(-19.1445330139973,-44.0763543735645,
124.588381422117)) ;
#63358 = CARTESIAN_POINT('Ctrl Pts',(-19.3406710042076,-44.2664166882687,
124.917774928891)) ;
#63359 = CARTESIAN_POINT('Ctrl Pts',(-19.3543836827224,-44.0864276079058,
124.616582420438)) ;
#63360 = CARTESIAN_POINT('Ctrl Pts',(-19.5990935689742,-44.2762581895953,
124.907117526406)) ;
#63361 = CARTESIAN_POINT('Ctrl Pts',(-19.5611207373312,-44.0962691092324,
124.608057610087)) ;
#63362 = CARTESIAN_POINT('Ctrl Pts',(-19.8549900005199,-44.2862191411901,
124.852048007979)) ;
#63363 = CARTESIAN_POINT('Ctrl Pts',(-19.7658378370726,-44.1062300608272,
124.56400332464)) ;
#63364 = CARTESIAN_POINT('Ctrl Pts',(-20.0991093096047,-44.2962569589108,
124.752132918042)) ;
#63365 = CARTESIAN_POINT('Ctrl Pts',(-19.9611338268518,-44.1162678785479,
124.484072297486)) ;
#63366 = CARTESIAN_POINT('Ctrl Pts',(-20.3188305768388,-44.3061313081678,
124.61402724624)) ;
#63367 = CARTESIAN_POINT('Ctrl Pts',(-20.1369108352661,-44.1261422278049,
124.373589272937)) ;
#63368 = CARTESIAN_POINT('Ctrl Pts',(-20.5149750943613,-44.31620085891,124.436460091646)) ;
#63369 = CARTESIAN_POINT('Ctrl Pts',(-20.2938275119669,-44.1362117785471,
124.231536305792)) ;
#63370 = CARTESIAN_POINT('Ctrl Pts',(-20.6736665782886,-44.3260348784186,
124.232462693714)) ;
#63371 = CARTESIAN_POINT('Ctrl Pts',(-20.4207810991636,-44.1460457980557,
124.068340001014)) ;
#63372 = CARTESIAN_POINT('Ctrl Pts',(-20.7975823820433,-44.3360690329981,
123.999722159393)) ;
#63373 = CARTESIAN_POINT('Ctrl Pts',(-20.5199150654758,-44.1560799526353,
123.88214817752)) ;
#63374 = CARTESIAN_POINT('Ctrl Pts',(-20.8784453196383,-44.3460849588206,
123.749227159064)) ;
#63375 = CARTESIAN_POINT('Ctrl Pts',(-20.5846066615164,-44.1660958784577,
123.681752589755)) ;
#63376 = CARTESIAN_POINT('Ctrl Pts',(-20.914563804666,-44.3559672140149,123.492051220715)) ;
#63377 = CARTESIAN_POINT('Ctrl Pts',(-20.613502746607,-44.175978133652,123.476012754182)) ;
#63378 = CARTESIAN_POINT('Ctrl Pts',(-20.9057075528016,-44.3659560205258,
123.229734225039)) ;
#63379 = CARTESIAN_POINT('Ctrl Pts',(-20.6064192252653,-44.1859669401629,
123.266159268691)) ;
#63380 = CARTESIAN_POINT('Ctrl Pts',(-20.8518375941005,-44.3759045877885,
122.973864298052)) ;
#63381 = CARTESIAN_POINT('Ctrl Pts',(-20.563324813657,-44.1959155074256,123.061463372867)) ;
#63382 = CARTESIAN_POINT('Ctrl Pts',(-20.7530825570645,-44.3859593930905,
122.728813985344)) ;
#63383 = CARTESIAN_POINT('Ctrl Pts',(-20.4843220736738,-44.2059703127276,
122.86542241497)) ;
#63384 = CARTESIAN_POINT('Ctrl Pts',(-20.616855401469,-44.3957781763541,122.509662800884)) ;
#63385 = CARTESIAN_POINT('Ctrl Pts',(-20.3753421837085,-44.2157890959912,
122.690101516828)) ;
#63386 = CARTESIAN_POINT('Ctrl Pts',(-20.4413805689007,-44.4058139487147,
122.312790934125)) ;
#63387 = CARTESIAN_POINT('Ctrl Pts',(-20.2349635031074,-44.2258248683518,
122.532602849493)) ;
#63388 = CARTESIAN_POINT('Ctrl Pts',(-20.2341379246685,-44.4158386477433,
122.150140067367)) ;
#63389 = CARTESIAN_POINT('Ctrl Pts',(-20.0691703136329,-44.2358495673804,
122.402480945821)) ;
#63390 = CARTESIAN_POINT('Ctrl Pts',(-20.0060783372853,-44.4256906510024,
122.027581366541)) ;
#63391 = CARTESIAN_POINT('Ctrl Pts',(-19.8867241261111,-44.2457015706395,
122.304432930007)) ;
#63392 = CARTESIAN_POINT('Ctrl Pts',(-19.7568956897588,-44.4356815853996,
121.944970803461)) ;
#63393 = CARTESIAN_POINT('Ctrl Pts',(-19.6873786743973,-44.2556925050367,
122.238342904726)) ;
#63394 = CARTESIAN_POINT('Ctrl Pts',(-19.4990141869541,-44.4455995078307,
121.906980973465)) ;
#63395 = CARTESIAN_POINT('Ctrl Pts',(-19.4810741764347,-44.2656104274678,
122.207949395468)) ;
#63396 = CARTESIAN_POINT('Ctrl Pts',(-19.2356052976764,-44.455627863513,121.914367687928)) ;
#63397 = CARTESIAN_POINT('Ctrl Pts',(-19.2703469878274,-44.2756387831502,
122.213857026739)) ;
#63398 = CARTESIAN_POINT('Ctrl Pts',(-18.9811319610234,-44.4655121480236,
121.966499520298)) ;
#63399 = CARTESIAN_POINT('Ctrl Pts',(-19.0667685443539,-44.2855230676607,
122.255560647816)) ;
#63400 = CARTESIAN_POINT('Ctrl Pts',(-18.7367176525546,-44.4755048319315,
122.06251590164)) ;
#63401 = CARTESIAN_POINT('Ctrl Pts',(-18.871236522365,-44.2955157515686,122.332371983472)) ;
#63402 = CARTESIAN_POINT('Ctrl Pts',(-18.5121188960608,-44.4855335689392,
122.20040107881)) ;
#63403 = CARTESIAN_POINT('Ctrl Pts',(-18.6915565682666,-44.3055444885763,
122.442678613519)) ;
#63404 = CARTESIAN_POINT('Ctrl Pts',(-18.3174591681186,-44.4954189655681,
122.372439116343)) ;
#63405 = CARTESIAN_POINT('Ctrl Pts',(-18.5358279827225,-44.3154298852052,
122.580307299376)) ;
#63406 = CARTESIAN_POINT('Ctrl Pts',(-18.1536797930773,-44.505406850982,122.577508760622)) ;
#63407 = CARTESIAN_POINT('Ctrl Pts',(-18.4048030832296,-44.3254177706191,
122.744361731314)) ;
#63408 = CARTESIAN_POINT('Ctrl Pts',(-18.0283271818904,-44.5153575536426,
122.807042074314)) ;
#63409 = CARTESIAN_POINT('Ctrl Pts',(-18.3045194438468,-44.3353684732797,
122.927987235333)) ;
#63410 = CARTESIAN_POINT('Ctrl Pts',(-17.9441368874462,-44.52539787174,123.057070192369)) ;
#63411 = CARTESIAN_POINT('Ctrl Pts',(-18.2371653982975,-44.3454087913771,
123.128009182656)) ;
#63412 = CARTESIAN_POINT('Ctrl Pts',(-17.9050280766287,-44.5352724370732,
123.313629339727)) ;
#63413 = CARTESIAN_POINT('Ctrl Pts',(-18.2058765291738,-44.3552833567104,
123.333255668068)) ;
#63414 = CARTESIAN_POINT('Ctrl Pts',(-17.9108009163294,-44.5452720971343,
123.576303554644)) ;
#63415 = CARTESIAN_POINT('Ctrl Pts',(-18.2104928246366,-44.3652830167714,
123.543394997243)) ;
#63416 = CARTESIAN_POINT('Ctrl Pts',(-17.9614015776546,-44.555181092302,123.831785012484)) ;
#63417 = CARTESIAN_POINT('Ctrl Pts',(-18.2509713159387,-44.3751920119392,
123.747780179525)) ;
#63418 = CARTESIAN_POINT('Ctrl Pts',(-18.0570243118767,-44.5652358334653,
124.078057381489)) ;
#63419 = CARTESIAN_POINT('Ctrl Pts',(-18.3274676754747,-44.3852467531024,
123.944798879371)) ;
#63420 = CARTESIAN_POINT('Ctrl Pts',(-18.1910740418543,-44.5750944453791,
124.299808917657)) ;
#63421 = CARTESIAN_POINT('Ctrl Pts',(-18.4347054549292,-44.3951053650162,
124.122200713057)) ;
#63422 = CARTESIAN_POINT('Ctrl Pts',(-18.3650377633451,-44.5851625676584,
124.499103963352)) ;
#63423 = CARTESIAN_POINT('Ctrl Pts',(-18.5738749680476,-44.4051734872955,
124.281638189971)) ;
#63424 = CARTESIAN_POINT('Ctrl Pts',(-18.5666736485935,-44.5950180383616,
124.661680062319)) ;
#63425 = CARTESIAN_POINT('Ctrl Pts',(-18.7351820039692,-44.4150289579987,
124.411700348019)) ;
#63426 = CARTESIAN_POINT('Ctrl Pts',(-18.7962745857909,-44.605012897855,124.789218966965)) ;
#63427 = CARTESIAN_POINT('Ctrl Pts',(-18.9188616496907,-44.4250238174921,
124.513733295613)) ;
#63428 = CARTESIAN_POINT('Ctrl Pts',(-19.0456348868395,-44.6150441511969,
124.874734939455)) ;
#63429 = CARTESIAN_POINT('Ctrl Pts',(-19.1183492174815,-44.435055070834,124.582148031688)) ;
#63430 = CARTESIAN_POINT('Ctrl Pts',(-19.3017226630708,-44.62491085007,124.915389460278)) ;
#63431 = CARTESIAN_POINT('Ctrl Pts',(-19.3232187005312,-44.4449217697071,
124.614673670169)) ;
#63432 = CARTESIAN_POINT('Ctrl Pts',(-19.5641051552104,-44.6348976658212,
124.911339609303)) ;
#63433 = CARTESIAN_POINT('Ctrl Pts',(-19.5331246292621,-44.4549085854583,
124.611435943813)) ;
#63434 = CARTESIAN_POINT('Ctrl Pts',(-19.8208626335505,-44.6448448710167,
124.862095013778)) ;
#63435 = CARTESIAN_POINT('Ctrl Pts',(-19.7385308356951,-44.4648557906538,
124.572042423977)) ;
#63436 = CARTESIAN_POINT('Ctrl Pts',(-20.0674296681808,-44.6548878591429,
124.76803108169)) ;
#63437 = CARTESIAN_POINT('Ctrl Pts',(-19.9357852426788,-44.4748987787801,
124.496793284832)) ;
#63438 = CARTESIAN_POINT('Ctrl Pts',(-20.2900606909374,-44.6647552137644,
124.635070010698)) ;
#63439 = CARTESIAN_POINT('Ctrl Pts',(-20.1138908853131,-44.4847661334015,
124.390426455139)) ;
#63440 = CARTESIAN_POINT('Ctrl Pts',(-20.4886282483647,-44.6747211070625,
124.464326907893)) ;
#63441 = CARTESIAN_POINT('Ctrl Pts',(-20.2727462890408,-44.4947320266996,
124.253833725483)) ;
#63442 = CARTESIAN_POINT('Ctrl Pts',(-20.6553026894128,-44.6847448844386,
124.260328412907)) ;
#63443 = CARTESIAN_POINT('Ctrl Pts',(-20.4060875193306,-44.5047558040757,
124.090636341466)) ;
#63444 = CARTESIAN_POINT('Ctrl Pts',(-20.7828007334005,-44.6946704323703,
124.032794984382)) ;
#63445 = CARTESIAN_POINT('Ctrl Pts',(-20.5080877807566,-44.5146813520074,
123.908610839297)) ;
#63446 = CARTESIAN_POINT('Ctrl Pts',(-20.8695762747895,-44.7046109087913,
123.786387153745)) ;
#63447 = CARTESIAN_POINT('Ctrl Pts',(-20.5775102739201,-44.5246218284284,
123.711485441995)) ;
#63448 = CARTESIAN_POINT('Ctrl Pts',(-20.912400649323,-44.7146571184542,123.525895807852)) ;
#63449 = CARTESIAN_POINT('Ctrl Pts',(-20.6117719585213,-44.5346680380913,
123.503092741529)) ;
#63450 = CARTESIAN_POINT('Ctrl Pts',(-20.9096780311405,-44.724518375116,123.26674378884)) ;
#63451 = CARTESIAN_POINT('Ctrl Pts',(-20.6095960943389,-44.5445292947531,
123.295771314812)) ;
#63452 = CARTESIAN_POINT('Ctrl Pts',(-20.8618140135343,-44.7345120033913,
123.008558951118)) ;
#63453 = CARTESIAN_POINT('Ctrl Pts',(-20.5713071019526,-44.5545229230284,
123.089223095259)) ;
#63454 = CARTESIAN_POINT('Ctrl Pts',(-20.7705763697433,-44.7444374007015,
122.764165937578)) ;
#63455 = CARTESIAN_POINT('Ctrl Pts',(-20.498319127258,-44.5644483203386,122.893707997254)) ;
#63456 = CARTESIAN_POINT('Ctrl Pts',(-20.6369673169243,-44.7544653086117,
122.537064718162)) ;
#63457 = CARTESIAN_POINT('Ctrl Pts',(-20.3914338502099,-44.5744762282489,
122.712025924337)) ;
#63458 = CARTESIAN_POINT('Ctrl Pts',(-20.4685272889073,-44.7643516242809,
122.33921389434)) ;
#63459 = CARTESIAN_POINT('Ctrl Pts',(-20.2566836019861,-44.584362543918,122.553743877924)) ;
#63460 = CARTESIAN_POINT('Ctrl Pts',(-20.2655021977993,-44.7743832191847,
122.171124667766)) ;
#63461 = CARTESIAN_POINT('Ctrl Pts',(-20.0942650101056,-44.5943941388218,
122.419270793338)) ;
#63462 = CARTESIAN_POINT('Ctrl Pts',(-20.0398318506451,-44.7842654621364,
122.042531241798)) ;
#63463 = CARTESIAN_POINT('Ctrl Pts',(-19.9137298912166,-44.6042763817735,
122.316394121493)) ;
#63464 = CARTESIAN_POINT('Ctrl Pts',(-19.790980965489,-44.7943249331663,121.953425884434)) ;
#63465 = CARTESIAN_POINT('Ctrl Pts',(-19.7146500072838,-44.6143358528034,
122.24510773456)) ;
#63466 = CARTESIAN_POINT('Ctrl Pts',(-19.5353894138272,-44.8041913778294,
121.909764540214)) ;
#63467 = CARTESIAN_POINT('Ctrl Pts',(-19.5101771563229,-44.6242022974665,
122.210176441665)) ;
#63468 = CARTESIAN_POINT('Ctrl Pts',(-19.2734974473692,-44.8141575022781,
121.910332881293)) ;
#63469 = CARTESIAN_POINT('Ctrl Pts',(-19.300663601662,-44.6341684219152,122.210628864892)) ;
#63470 = CARTESIAN_POINT('Ctrl Pts',(-19.0140941942044,-44.8241877456692,
121.957079096099)) ;
#63471 = CARTESIAN_POINT('Ctrl Pts',(-19.0931406459017,-44.6441986653064,
122.248023646285)) ;
#63472 = CARTESIAN_POINT('Ctrl Pts',(-18.7699778546539,-44.8340807806223,
122.04657166839)) ;
#63473 = CARTESIAN_POINT('Ctrl Pts',(-18.8978469009694,-44.6540917002594,
122.319615481204)) ;
#63474 = CARTESIAN_POINT('Ctrl Pts',(-18.5415249218624,-44.8441316948591,
122.179088598224)) ;
#63475 = CARTESIAN_POINT('Ctrl Pts',(-18.7150830028236,-44.6641426144963,
122.425627556527)) ;
#63476 = CARTESIAN_POINT('Ctrl Pts',(-18.3427444001931,-44.8540215210837,
122.346531093265)) ;
#63477 = CARTESIAN_POINT('Ctrl Pts',(-18.5560590226922,-44.6740324407208,
122.55957796272)) ;
#63478 = CARTESIAN_POINT('Ctrl Pts',(-18.1174461021876,-44.8673563361306,
122.614979487024)) ;
#63479 = CARTESIAN_POINT('Ctrl Pts',(-18.3758085267228,-44.6873672557678,
122.774344354257)) ;
#63480 = CARTESIAN_POINT('Ctrl Pts',(-17.9686335760902,-44.8806334273021,
122.934896659141)) ;
#63481 = CARTESIAN_POINT('Ctrl Pts',(-18.2567530298792,-44.7006443469392,
123.030306574973)) ;
#63482 = CARTESIAN_POINT('Ctrl Pts',(-17.9076731562678,-44.8938817159004,
123.277709414345)) ;
#63483 = CARTESIAN_POINT('Ctrl Pts',(-18.2079946998203,-44.7138926355375,
123.304511413503)) ;
#63484 = CARTESIAN_POINT('Ctrl Pts',(-17.9074623164892,-44.9039365573945,
123.541899571283)) ;
#63485 = CARTESIAN_POINT('Ctrl Pts',(-18.2078213171443,-44.7239474770316,
123.515872463229)) ;
#63486 = CARTESIAN_POINT('Ctrl Pts',(-17.9516919899064,-44.913767546702,123.796479325853)) ;
#63487 = CARTESIAN_POINT('Ctrl Pts',(-18.2432033587368,-44.7337784663392,
123.719534329518)) ;
#63488 = CARTESIAN_POINT('Ctrl Pts',(-18.0414310833544,-44.9238441110252,
124.045563596302)) ;
#63489 = CARTESIAN_POINT('Ctrl Pts',(-18.3149935556506,-44.7438550306624,
123.918803730498)) ;
#63490 = CARTESIAN_POINT('Ctrl Pts',(-18.1701298255741,-44.9336934361592,
124.270160085588)) ;
#63491 = CARTESIAN_POINT('Ctrl Pts',(-18.4179464132743,-44.7537043557963,
124.098479058977)) ;
#63492 = CARTESIAN_POINT('Ctrl Pts',(-18.3940753258795,-44.9470414357965,
124.540160290177)) ;
#63493 = CARTESIAN_POINT('Ctrl Pts',(-18.5971230250769,-44.7670523554336,
124.314496251429)) ;
#63494 = CARTESIAN_POINT('Ctrl Pts',(-18.7539725180923,-44.963626195333,124.794623795617)) ;
#63495 = CARTESIAN_POINT('Ctrl Pts',(-18.8849990055932,-44.7836371149701,
124.518050456276)) ;
#63496 = CARTESIAN_POINT('Ctrl Pts',(-19.1783954643001,-44.9801947466811,
124.911954796591)) ;
#63497 = CARTESIAN_POINT('Ctrl Pts',(-19.2246019623236,-44.8002056663183,
124.611932785891)) ;
#63498 = CARTESIAN_POINT('Ctrl Pts',(-19.5295000394639,-44.9935545715001,
124.914496420765)) ;
#63499 = CARTESIAN_POINT('Ctrl Pts',(-19.5054328311711,-44.8135654911373,
124.613960044086)) ;
#63500 = CARTESIAN_POINT('Ctrl Pts',(-19.7862085515421,-45.0034599803308,
124.87135192276)) ;
#63501 = CARTESIAN_POINT('Ctrl Pts',(-19.7108114579357,-44.8234708999679,
124.579447577859)) ;
#63502 = CARTESIAN_POINT('Ctrl Pts',(-20.0329770475992,-45.0134200069148,
124.784181635824)) ;
#63503 = CARTESIAN_POINT('Ctrl Pts',(-19.9082219143351,-44.833430926552,124.509714796774)) ;
#63504 = CARTESIAN_POINT('Ctrl Pts',(-20.3365929403509,-45.0266775911001,
124.613239797289)) ;
#63505 = CARTESIAN_POINT('Ctrl Pts',(-20.151128683135,-44.8466885107373,124.372952796465)) ;
#63506 = CARTESIAN_POINT('Ctrl Pts',(-20.6530388478672,-45.0433288025948,
124.303846929761)) ;
#63507 = CARTESIAN_POINT('Ctrl Pts',(-20.4042740591769,-44.8633397222319,
124.125452733239)) ;
#63508 = CARTESIAN_POINT('Ctrl Pts',(-20.8822225928719,-45.0632470167051,
123.826665489803)) ;
#63509 = CARTESIAN_POINT('Ctrl Pts',(-20.5876289589755,-44.8832579363422,
123.743704995004)) ;
#63510 = CARTESIAN_POINT('Ctrl Pts',(-20.9358462100671,-45.0831247799259,
123.300999284693)) ;
#63511 = CARTESIAN_POINT('Ctrl Pts',(-20.6305301436153,-44.9031356995631,
123.323172734801)) ;
#63512 = CARTESIAN_POINT('Ctrl Pts',(-20.8055712371326,-45.1031374477131,
122.785395465323)) ;
#63513 = CARTESIAN_POINT('Ctrl Pts',(-20.5263138314019,-44.9231483673502,
122.910688665346)) ;
#63514 = CARTESIAN_POINT('Ctrl Pts',(-20.5104525719544,-45.1229499703797,
122.349160972193)) ;
#63515 = CARTESIAN_POINT('Ctrl Pts',(-20.2902207745244,-44.9429608900168,
122.561698343085)) ;
#63516 = CARTESIAN_POINT('Ctrl Pts',(-20.081167872577,-45.1429332703796,122.036595982268)) ;
#63517 = CARTESIAN_POINT('Ctrl Pts',(-19.946794629083,-44.9629441900167,122.311643931763)) ;
#63518 = CARTESIAN_POINT('Ctrl Pts',(-19.5729808270998,-45.1628275474809,
121.890260817414)) ;
#63519 = CARTESIAN_POINT('Ctrl Pts',(-19.5402450431835,-44.982838467118,122.194572859151)) ;
#63520 = CARTESIAN_POINT('Ctrl Pts',(-19.0443792388159,-45.1827603092387,
121.925363493254)) ;
#63521 = CARTESIAN_POINT('Ctrl Pts',(-19.1173630609288,-45.0027712288758,
122.222652560923)) ;
#63522 = CARTESIAN_POINT('Ctrl Pts',(-18.5588123388653,-45.2027263150034,
122.139444767471)) ;
#63523 = CARTESIAN_POINT('Ctrl Pts',(-18.7289082955966,-45.0227372346405,
122.393915435072)) ;
#63524 = CARTESIAN_POINT('Ctrl Pts',(-18.1768400075753,-45.2226048471683,
122.504512707876)) ;
#63525 = CARTESIAN_POINT('Ctrl Pts',(-18.4233281318735,-45.0426157668054,
122.685968958821)) ;
#63526 = CARTESIAN_POINT('Ctrl Pts',(-17.9412382746725,-45.2425445138286,
122.979165174917)) ;
#63527 = CARTESIAN_POINT('Ctrl Pts',(-18.2348448067827,-45.0625554334657,
123.065690634958)) ;
#63528 = CARTESIAN_POINT('Ctrl Pts',(-17.8817201357155,-45.262439388474,123.504633155352)) ;
#63529 = CARTESIAN_POINT('Ctrl Pts',(-18.1872285519615,-45.0824503081111,
123.48606590208)) ;
#63530 = CARTESIAN_POINT('Ctrl Pts',(-18.0046155637013,-45.2823465277673,
124.019136501102)) ;
#63531 = CARTESIAN_POINT('Ctrl Pts',(-18.2855439122614,-45.1023574474044,
123.897669917515)) ;
#63532 = CARTESIAN_POINT('Ctrl Pts',(-18.2951592685282,-45.3022570758458,
124.461637555377)) ;
#63533 = CARTESIAN_POINT('Ctrl Pts',(-18.5179788419764,-45.1222679954829,
124.251671936744)) ;
#63534 = CARTESIAN_POINT('Ctrl Pts',(-18.7231289192442,-45.322325661203,124.779793280886)) ;
#63535 = CARTESIAN_POINT('Ctrl Pts',(-18.8603532666718,-45.1423365808401,
124.506196853283)) ;
#63536 = CARTESIAN_POINT('Ctrl Pts',(-19.2267990765381,-45.3421074585177,
124.931211593154)) ;
#63537 = CARTESIAN_POINT('Ctrl Pts',(-19.2632917257971,-45.1621183781549,
124.627332840506)) ;
#63538 = CARTESIAN_POINT('Ctrl Pts',(-19.7575625515052,-45.3621150054623,
124.902127405188)) ;
#63539 = CARTESIAN_POINT('Ctrl Pts',(-19.6879025560016,-45.1821259250994,
124.604065538221)) ;
#63540 = CARTESIAN_POINT('Ctrl Pts',(-20.2423289587424,-45.3819367437651,
124.695488931146)) ;
#63541 = CARTESIAN_POINT('Ctrl Pts',(-20.0757176520892,-45.2019476634022,
124.438753696871)) ;
#63542 = CARTESIAN_POINT('Ctrl Pts',(-20.6310564599377,-45.4019167636693,
124.333814619466)) ;
#63543 = CARTESIAN_POINT('Ctrl Pts',(-20.3866992414769,-45.2219276833064,
124.149413465804)) ;
#63544 = CARTESIAN_POINT('Ctrl Pts',(-20.8717000555941,-45.4218342149315,
123.862278018821)) ;
#63545 = CARTESIAN_POINT('Ctrl Pts',(-20.579213919715,-45.2418451345686,123.77218297004)) ;
#63546 = CARTESIAN_POINT('Ctrl Pts',(-20.9380767680918,-45.4417091361042,
123.338188475184)) ;
#63547 = CARTESIAN_POINT('Ctrl Pts',(-20.6323140215928,-45.2617200557413,
123.352909817565)) ;
#63548 = CARTESIAN_POINT('Ctrl Pts',(-20.8204289201312,-45.461733504655,122.819174893006)) ;
#63549 = CARTESIAN_POINT('Ctrl Pts',(-20.5381943820615,-45.2817444242922,
122.937699557393)) ;
#63550 = CARTESIAN_POINT('Ctrl Pts',(-20.5348026192168,-45.4816001890285,
122.374971928378)) ;
#63551 = CARTESIAN_POINT('Ctrl Pts',(-20.3096913007445,-45.3016111086656,
122.582336913759)) ;
#63552 = CARTESIAN_POINT('Ctrl Pts',(-20.113737828752,-45.5015440108747,122.053072103722)) ;
#63553 = CARTESIAN_POINT('Ctrl Pts',(-19.9728377986509,-45.3215549305118,
122.324818360673)) ;
#63554 = CARTESIAN_POINT('Ctrl Pts',(-19.6089136734289,-45.5214513801262,
121.894620584429)) ;
#63555 = CARTESIAN_POINT('Ctrl Pts',(-19.5689770139582,-45.3414622997634,
122.198058922414)) ;
#63556 = CARTESIAN_POINT('Ctrl Pts',(-19.0811541092211,-45.5413260778729,
121.916926618997)) ;
#63557 = CARTESIAN_POINT('Ctrl Pts',(-19.1467684454857,-45.3613369975101,
122.215906404225)) ;
#63558 = CARTESIAN_POINT('Ctrl Pts',(-18.5899663032709,-45.5613080203947,
122.11896949238)) ;
#63559 = CARTESIAN_POINT('Ctrl Pts',(-18.7538191655351,-45.3813189400318,
122.377543293856)) ;
#63560 = CARTESIAN_POINT('Ctrl Pts',(-18.1991325996576,-45.5812106873055,
122.475351878754)) ;
#63561 = CARTESIAN_POINT('Ctrl Pts',(-18.4411535104022,-45.4012216069426,
122.662651767787)) ;
#63562 = CARTESIAN_POINT('Ctrl Pts',(-17.9525130136247,-45.6010660448442,
122.94198968938)) ;
#63563 = CARTESIAN_POINT('Ctrl Pts',(-18.2438603264457,-45.4210769644813,
123.035964382293)) ;
#63564 = CARTESIAN_POINT('Ctrl Pts',(-17.8797853306708,-45.6211300835602,
123.470193368152)) ;
#63565 = CARTESIAN_POINT('Ctrl Pts',(-18.1856815073262,-45.4411410031973,
123.458527308833)) ;
#63566 = CARTESIAN_POINT('Ctrl Pts',(-17.9907738386166,-45.6409852632853,
123.986308188026)) ;
#63567 = CARTESIAN_POINT('Ctrl Pts',(-18.2744755604141,-45.4609961829224,
123.871419313323)) ;
#63568 = CARTESIAN_POINT('Ctrl Pts',(-18.2724161799833,-45.6609653679497,
124.436265927067)) ;
#63569 = CARTESIAN_POINT('Ctrl Pts',(-18.4997930441946,-45.4809762875868,
124.231383659367)) ;
#63570 = CARTESIAN_POINT('Ctrl Pts',(-18.6870078952182,-45.6807744731195,
124.761025281335)) ;
#63571 = CARTESIAN_POINT('Ctrl Pts',(-18.8314673456426,-45.5007853927566,
124.491189117074)) ;
#63572 = CARTESIAN_POINT('Ctrl Pts',(-19.1916999501427,-45.7007670934602,
124.926741074859)) ;
#63573 = CARTESIAN_POINT('Ctrl Pts',(-19.235230041018,-45.5207780130973,124.623756847041)) ;
#63574 = CARTESIAN_POINT('Ctrl Pts',(-19.6312118173371,-45.7173065759643,
124.913196409966)) ;
#63575 = CARTESIAN_POINT('Ctrl Pts',(-19.5868155436623,-45.5373174956014,
124.612921459841)) ;
#63576 = CARTESIAN_POINT('Ctrl Pts',(-19.9674993568783,-45.7306708940285,
124.812112387644)) ;
#63577 = CARTESIAN_POINT('Ctrl Pts',(-19.8558719099428,-45.5506818136656,
124.532044502846)) ;
#63578 = CARTESIAN_POINT('Ctrl Pts',(-20.2779790594621,-45.74388849653,124.656227492421)) ;
#63579 = CARTESIAN_POINT('Ctrl Pts',(-20.1042094374621,-45.5638994161671,
124.407362610249)) ;
#63580 = CARTESIAN_POINT('Ctrl Pts',(-20.6088613725694,-45.7605460908078,
124.362235325753)) ;
#63581 = CARTESIAN_POINT('Ctrl Pts',(-20.3689615158667,-45.5805570104449,
124.172135807522)) ;
#63582 = CARTESIAN_POINT('Ctrl Pts',(-20.8603771681575,-45.7804117928495,
123.897882285973)) ;
#63583 = CARTESIAN_POINT('Ctrl Pts',(-20.5701552926539,-45.6004227124867,
123.800652558022)) ;
#63584 = CARTESIAN_POINT('Ctrl Pts',(-20.9262145451772,-45.7970415195396,
123.460911151536)) ;
#63585 = CARTESIAN_POINT('Ctrl Pts',(-20.6228240067414,-45.6170524391767,
123.451100564137)) ;
#63586 = CARTESIAN_POINT('Ctrl Pts',(-20.8869828199733,-45.8103306346774,
123.113835882224)) ;
#63587 = CARTESIAN_POINT('Ctrl Pts',(-20.5914361114732,-45.6303415543145,
123.17341573683)) ;
#63588 = CARTESIAN_POINT('Ctrl Pts',(-20.813137221631,-45.8202949816545,122.862628158048)) ;
#63589 = CARTESIAN_POINT('Ctrl Pts',(-20.532359431995,-45.6403059012916,122.97245700907)) ;
#63590 = CARTESIAN_POINT('Ctrl Pts',(-20.6973720958994,-45.830223349656,122.628822672111)) ;
#63591 = CARTESIAN_POINT('Ctrl Pts',(-20.4397374777452,-45.6502342692931,
122.785404651052)) ;
#63592 = CARTESIAN_POINT('Ctrl Pts',(-20.491036246019,-45.8435067827447,122.347203200446)) ;
#63593 = CARTESIAN_POINT('Ctrl Pts',(-20.2747057229162,-45.6635177023819,
122.560148879039)) ;
#63594 = CARTESIAN_POINT('Ctrl Pts',(-20.145826084982,-45.8601588604851,122.070280119537)) ;
#63595 = CARTESIAN_POINT('Ctrl Pts',(-19.9984819208062,-45.6801697801222,
122.338567916265)) ;
#63596 = CARTESIAN_POINT('Ctrl Pts',(-19.7294257177558,-45.8767102297859,
121.928426697341)) ;
#63597 = CARTESIAN_POINT('Ctrl Pts',(-19.6654083759465,-45.696721149423,122.22511130924)) ;
#63598 = CARTESIAN_POINT('Ctrl Pts',(-19.3810452958569,-45.8899976579349,
121.904492705596)) ;
#63599 = CARTESIAN_POINT('Ctrl Pts',(-19.386670912546,-45.710008577572,122.205956446535)) ;
#63600 = CARTESIAN_POINT('Ctrl Pts',(-19.1186091401649,-45.900042197635,121.932658291026)) ;
#63601 = CARTESIAN_POINT('Ctrl Pts',(-19.1767289258844,-45.7200531172721,
122.228493281736)) ;
#63602 = CARTESIAN_POINT('Ctrl Pts',(-18.8700233535146,-45.9098850394588,
122.00419504513)) ;
#63603 = CARTESIAN_POINT('Ctrl Pts',(-18.9778591118884,-45.7298959590959,
122.285724283644)) ;
#63604 = CARTESIAN_POINT('Ctrl Pts',(-18.6340661750229,-45.9198693237057,
122.118877741184)) ;
#63605 = CARTESIAN_POINT('Ctrl Pts',(-18.7890948938155,-45.7398802433429,
122.377472601013)) ;
#63606 = CARTESIAN_POINT('Ctrl Pts',(-18.4223444457942,-45.9298189691049,
122.272320772615)) ;
#63607 = CARTESIAN_POINT('Ctrl Pts',(-18.6197187508759,-45.749829888742,122.500228781122)) ;
#63608 = CARTESIAN_POINT('Ctrl Pts',(-18.2393318883207,-45.9398187307933,
122.460918444187)) ;
#63609 = CARTESIAN_POINT('Ctrl Pts',(-18.4733104024896,-45.7598296504304,
122.65110845724)) ;
#63610 = CARTESIAN_POINT('Ctrl Pts',(-18.0917505487203,-45.9498500767522,
122.679344429148)) ;
#63611 = CARTESIAN_POINT('Ctrl Pts',(-18.3552472195982,-45.7698609963893,
122.825850469655)) ;
#63612 = CARTESIAN_POINT('Ctrl Pts',(-17.9858757132729,-45.9597050312293,
122.915697062005)) ;
#63613 = CARTESIAN_POINT('Ctrl Pts',(-18.2705494534768,-45.7797159508665,
123.014933412963)) ;
#63614 = CARTESIAN_POINT('Ctrl Pts',(-17.9213083460971,-45.9696775692299,
123.1696585988)) ;
#63615 = CARTESIAN_POINT('Ctrl Pts',(-18.218897762685,-45.789688488867,123.218103106479)) ;
#63616 = CARTESIAN_POINT('Ctrl Pts',(-17.9017881316978,-45.9796725629648,
123.43163061832)) ;
#63617 = CARTESIAN_POINT('Ctrl Pts',(-18.2032838339912,-45.7996834826019,
123.427680825471)) ;
#63618 = CARTESIAN_POINT('Ctrl Pts',(-17.9284695515831,-45.9897066217589,
123.693939039804)) ;
#63619 = CARTESIAN_POINT('Ctrl Pts',(-18.2246312126076,-45.809717541396,123.637527304085)) ;
#63620 = CARTESIAN_POINT('Ctrl Pts',(-17.9986278342862,-45.9995619645819,
123.943270201395)) ;
#63621 = CARTESIAN_POINT('Ctrl Pts',(-18.2807599457767,-45.819572884219,123.83699144443)) ;
#63622 = CARTESIAN_POINT('Ctrl Pts',(-18.1123057056934,-46.0095614439275,
124.180132595263)) ;
#63623 = CARTESIAN_POINT('Ctrl Pts',(-18.3717042256828,-45.8295723635646,
124.026480327799)) ;
#63624 = CARTESIAN_POINT('Ctrl Pts',(-18.2635910838762,-46.0194558926828,
124.391666206078)) ;
#63625 = CARTESIAN_POINT('Ctrl Pts',(-18.4927342046914,-45.8394668123199,
124.195705758367)) ;
#63626 = CARTESIAN_POINT('Ctrl Pts',(-18.4524598572534,-46.0295190121173,
124.576699295059)) ;
#63627 = CARTESIAN_POINT('Ctrl Pts',(-18.6438307990039,-45.8495299317544,
124.343730662622)) ;
#63628 = CARTESIAN_POINT('Ctrl Pts',(-18.6656547763294,-46.0393586573585,
124.723094304069)) ;
#63629 = CARTESIAN_POINT('Ctrl Pts',(-18.8143877068013,-45.8593695769957,
124.460844668667)) ;
#63630 = CARTESIAN_POINT('Ctrl Pts',(-18.9061641632514,-46.0494218215446,
124.832954725746)) ;
#63631 = CARTESIAN_POINT('Ctrl Pts',(-19.0067961563735,-45.8694327411817,
124.5487310367)) ;
#63632 = CARTESIAN_POINT('Ctrl Pts',(-19.1579188977088,-46.0593160912934,
124.898075179652)) ;
#63633 = CARTESIAN_POINT('Ctrl Pts',(-19.2082002369437,-45.8793270109305,
124.600825207935)) ;
#63634 = CARTESIAN_POINT('Ctrl Pts',(-19.4182795982721,-46.0692578173072,
124.919290922679)) ;
#63635 = CARTESIAN_POINT('Ctrl Pts',(-19.4164887608804,-45.8892687369444,
124.617795648672)) ;
#63636 = CARTESIAN_POINT('Ctrl Pts',(-19.6800549445947,-46.0792607059666,
124.894933738321)) ;
#63637 = CARTESIAN_POINT('Ctrl Pts',(-19.6259087706948,-45.8992716256037,
124.598307788373)) ;
#63638 = CARTESIAN_POINT('Ctrl Pts',(-19.9343703358343,-46.0893005547606,
124.824788939864)) ;
#63639 = CARTESIAN_POINT('Ctrl Pts',(-19.8293605316926,-45.9093114743977,
124.542189846149)) ;
#63640 = CARTESIAN_POINT('Ctrl Pts',(-20.1678185633982,-46.0991247702215,
124.714495173511)) ;
#63641 = CARTESIAN_POINT('Ctrl Pts',(-20.0161177505501,-45.9191356898586,
124.453953133522)) ;
#63642 = CARTESIAN_POINT('Ctrl Pts',(-20.3837390423242,-46.109181613715,124.562135863679)) ;
#63643 = CARTESIAN_POINT('Ctrl Pts',(-20.1888529869787,-45.9291925333521,
124.332063944319)) ;
#63644 = CARTESIAN_POINT('Ctrl Pts',(-20.5673296043918,-46.119110223111,124.376727071012)) ;
#63645 = CARTESIAN_POINT('Ctrl Pts',(-20.3357237457142,-45.9391211427481,
124.183735605175)) ;
#63646 = CARTESIAN_POINT('Ctrl Pts',(-20.7168895335636,-46.1290621071489,
124.162174744986)) ;
#63647 = CARTESIAN_POINT('Ctrl Pts',(-20.4553698831515,-45.949073026786,124.012092764765)) ;
#63648 = CARTESIAN_POINT('Ctrl Pts',(-20.8275975547341,-46.1391150599565,
123.922329195858)) ;
#63649 = CARTESIAN_POINT('Ctrl Pts',(-20.5439344348876,-45.9591259795936,
123.820215369618)) ;
#63650 = CARTESIAN_POINT('Ctrl Pts',(-20.8939114402365,-46.1489379364227,
123.672837152796)) ;
#63651 = CARTESIAN_POINT('Ctrl Pts',(-20.5969834127684,-45.9689488560598,
123.620621818295)) ;
#63652 = CARTESIAN_POINT('Ctrl Pts',(-20.9168785394599,-46.1589936689928,
123.409601144836)) ;
#63653 = CARTESIAN_POINT('Ctrl Pts',(-20.6153551246797,-45.9790045886299,
123.410032751232)) ;
#63654 = CARTESIAN_POINT('Ctrl Pts',(-20.893591540016,-46.1689344339805,123.149398558187)) ;
#63655 = CARTESIAN_POINT('Ctrl Pts',(-20.5967235160762,-45.9889453536176,
123.201871130652)) ;
#63656 = CARTESIAN_POINT('Ctrl Pts',(-20.8265158340173,-46.1788387668861,
122.89790937762)) ;
#63657 = CARTESIAN_POINT('Ctrl Pts',(-20.5430611920399,-45.9988496865232,
123.000680697245)) ;
#63658 = CARTESIAN_POINT('Ctrl Pts',(-20.7150751051334,-46.1888854357668,
122.658590446776)) ;
#63659 = CARTESIAN_POINT('Ctrl Pts',(-20.4539067994353,-46.0088963554039,
122.809226303556)) ;
#63660 = CARTESIAN_POINT('Ctrl Pts',(-20.5662066575866,-46.1987809990726,
122.445321690522)) ;
#63661 = CARTESIAN_POINT('Ctrl Pts',(-20.3348107319398,-46.0187919187097,
122.638612781793)) ;
#63662 = CARTESIAN_POINT('Ctrl Pts',(-20.379536426161,-46.2088430567729,122.258099155572)) ;
#63663 = CARTESIAN_POINT('Ctrl Pts',(-20.1854730795545,-46.02885397641,122.488836010064)) ;
#63664 = CARTESIAN_POINT('Ctrl Pts',(-20.1679385535702,-46.2186858344004,
122.109285146216)) ;
#63665 = CARTESIAN_POINT('Ctrl Pts',(-20.0161942548949,-46.0386967540375,
122.369786757822)) ;
#63666 = CARTESIAN_POINT('Ctrl Pts',(-19.9305238988353,-46.2286763126523,
121.997288664891)) ;
#63667 = CARTESIAN_POINT('Ctrl Pts',(-19.8262618842319,-46.0486872322894,
122.280191270744)) ;
#63668 = CARTESIAN_POINT('Ctrl Pts',(-19.6787697821799,-46.2386052852958,
121.928664786175)) ;
#63669 = CARTESIAN_POINT('Ctrl Pts',(-19.6248584943409,-46.0586162049329,
122.225294020736)) ;
#63670 = CARTESIAN_POINT('Ctrl Pts',(-19.4173499655239,-46.2485964221754,
121.904240994676)) ;
#63671 = CARTESIAN_POINT('Ctrl Pts',(-19.4157226100633,-46.0686073418125,
122.205756739917)) ;
#63672 = CARTESIAN_POINT('Ctrl Pts',(-19.1548721753511,-46.2586185396643,
121.92596250925)) ;
#63673 = CARTESIAN_POINT('Ctrl Pts',(-19.2057405118503,-46.0786294593014,
122.22313574868)) ;
#63674 = CARTESIAN_POINT('Ctrl Pts',(-18.9031822162054,-46.2685190500665,
121.991878228814)) ;
#63675 = CARTESIAN_POINT('Ctrl Pts',(-19.0043894985658,-46.0885299697036,
122.275869893625)) ;
#63676 = CARTESIAN_POINT('Ctrl Pts',(-18.6644805817943,-46.2785080428126,
122.101090338779)) ;
#63677 = CARTESIAN_POINT('Ctrl Pts',(-18.8134290284549,-46.0985189624497,
122.363241059296)) ;
#63678 = CARTESIAN_POINT('Ctrl Pts',(-18.4489924497402,-46.2884732868632,
122.249880282488)) ;
#63679 = CARTESIAN_POINT('Ctrl Pts',(-18.6410397168517,-46.1084842065003,
122.482274286718)) ;
#63680 = CARTESIAN_POINT('Ctrl Pts',(-18.2633002251361,-46.2983775513764,
122.43228474134)) ;
#63681 = CARTESIAN_POINT('Ctrl Pts',(-18.4924874591841,-46.1183884710135,
122.628198618205)) ;
#63682 = CARTESIAN_POINT('Ctrl Pts',(-18.1099129937586,-46.3084356430746,
122.64751373004)) ;
#63683 = CARTESIAN_POINT('Ctrl Pts',(-18.3697789069092,-46.1284465627118,
122.800382913545)) ;
#63684 = CARTESIAN_POINT('Ctrl Pts',(-17.9983877780156,-46.318285583503,122.881119052211)) ;
#63685 = CARTESIAN_POINT('Ctrl Pts',(-18.2805605437885,-46.1382965031402,
122.98726711269)) ;
#63686 = CARTESIAN_POINT('Ctrl Pts',(-17.9272509867176,-46.3283125946766,
123.13482951254)) ;
#63687 = CARTESIAN_POINT('Ctrl Pts',(-18.2236525328705,-46.1483235143137,
123.190235911234)) ;
#63688 = CARTESIAN_POINT('Ctrl Pts',(-17.901925769436,-46.3383411812886,123.397163125626)) ;
#63689 = CARTESIAN_POINT('Ctrl Pts',(-18.2033939634236,-46.1583521009257,
123.400103012758)) ;
#63690 = CARTESIAN_POINT('Ctrl Pts',(-17.9216676872438,-46.3481863954013,
123.655117412453)) ;
#63691 = CARTESIAN_POINT('Ctrl Pts',(-18.2191889474225,-46.1681973150384,
123.606465432505)) ;
#63692 = CARTESIAN_POINT('Ctrl Pts',(-17.9861726596863,-46.3581771435809,
123.909622518266)) ;
#63693 = CARTESIAN_POINT('Ctrl Pts',(-18.2707942272682,-46.178188063218,123.810069025763)) ;
#63694 = CARTESIAN_POINT('Ctrl Pts',(-18.0949209308514,-46.3682147771664,
124.149940691054)) ;
#63695 = CARTESIAN_POINT('Ctrl Pts',(-18.3577942543388,-46.1882256968035,
124.002323042482)) ;
#63696 = CARTESIAN_POINT('Ctrl Pts',(-18.2405394895734,-46.3780600663792,
124.363798772761)) ;
#63697 = CARTESIAN_POINT('Ctrl Pts',(-18.4742897414031,-46.1980709860163,
124.173407939844)) ;
#63698 = CARTESIAN_POINT('Ctrl Pts',(-18.4231399414147,-46.3880414671851,
124.552075901713)) ;
#63699 = CARTESIAN_POINT('Ctrl Pts',(-18.6203708816344,-46.2080523868222,
124.324028590119)) ;
#63700 = CARTESIAN_POINT('Ctrl Pts',(-18.6350962163679,-46.397993700175,124.705303329863)) ;
#63701 = CARTESIAN_POINT('Ctrl Pts',(-18.7899363575204,-46.2180046198121,
124.446609255118)) ;
#63702 = CARTESIAN_POINT('Ctrl Pts',(-18.8714017008727,-46.4079925116317,
124.820247929086)) ;
#63703 = CARTESIAN_POINT('Ctrl Pts',(-18.9789811859863,-46.2280034312688,
124.538563781757)) ;
#63704 = CARTESIAN_POINT('Ctrl Pts',(-19.1251985398827,-46.4180316155623,
124.892209201477)) ;
#63705 = CARTESIAN_POINT('Ctrl Pts',(-19.1820191456136,-46.2380425351995,
124.596131542575)) ;
#63706 = CARTESIAN_POINT('Ctrl Pts',(-19.3820108279109,-46.4278565579816,
124.918993385592)) ;
#63707 = CARTESIAN_POINT('Ctrl Pts',(-19.387468008186,-46.2478674776188,124.61755756467)) ;
#63708 = CARTESIAN_POINT('Ctrl Pts',(-19.64559328927,-46.4379112454576,124.900789356719)) ;
#63709 = CARTESIAN_POINT('Ctrl Pts',(-19.5983341049394,-46.2579221650947,
124.602993203772)) ;
#63710 = CARTESIAN_POINT('Ctrl Pts',(-19.8990733415374,-46.4478540478144,
124.837364781521)) ;
#63711 = CARTESIAN_POINT('Ctrl Pts',(-19.8011174177466,-46.2678649674515,
124.552252461191)) ;
#63712 = CARTESIAN_POINT('Ctrl Pts',(-20.1370762828401,-46.4577578437542,
124.732039090923)) ;
#63713 = CARTESIAN_POINT('Ctrl Pts',(-19.9915187270784,-46.2777687633913,
124.467991228943)) ;
#63714 = CARTESIAN_POINT('Ctrl Pts',(-20.3561848751386,-46.4678046231292,
124.584777991393)) ;
#63715 = CARTESIAN_POINT('Ctrl Pts',(-20.1668051376118,-46.2878155427663,
124.350181357414)) ;
#63716 = CARTESIAN_POINT('Ctrl Pts',(-20.5437352889847,-46.4777002814238,
124.40458454613)) ;
#63717 = CARTESIAN_POINT('Ctrl Pts',(-20.3168442299365,-46.2977112010609,
124.206026364736)) ;
#63718 = CARTESIAN_POINT('Ctrl Pts',(-20.6997061794261,-46.4877618486744,
124.191114977027)) ;
#63719 = CARTESIAN_POINT('Ctrl Pts',(-20.4416202696434,-46.3077727683115,
124.035249895047)) ;
#63720 = CARTESIAN_POINT('Ctrl Pts',(-20.8137834732747,-46.4976064931117,
123.958907813317)) ;
#63721 = CARTESIAN_POINT('Ctrl Pts',(-20.5328807279198,-46.3176174127489,
123.849484665839)) ;
#63722 = CARTESIAN_POINT('Ctrl Pts',(-20.8875519244176,-46.5075665393544,
123.707782162122)) ;
#63723 = CARTESIAN_POINT('Ctrl Pts',(-20.5918946247474,-46.3275774589915,
123.648584272298)) ;
#63724 = CARTESIAN_POINT('Ctrl Pts',(-20.9163089327259,-46.5176048353728,
123.445571143073)) ;
#63725 = CARTESIAN_POINT('Ctrl Pts',(-20.6148993352014,-46.3376157550099,
123.438815228034)) ;
#63726 = CARTESIAN_POINT('Ctrl Pts',(-20.8998770457403,-46.5274781767911,
123.186591367245)) ;
#63727 = CARTESIAN_POINT('Ctrl Pts',(-20.6017530884054,-46.3474890964282,
123.231632356186)) ;
#63728 = CARTESIAN_POINT('Ctrl Pts',(-20.8374336990215,-46.5375512805904,
122.92940409922)) ;
#63729 = CARTESIAN_POINT('Ctrl Pts',(-20.5517975371544,-46.3575622002275,
123.025882403029)) ;
#63730 = CARTESIAN_POINT('Ctrl Pts',(-20.7341962066025,-46.5473720957093,
122.692815045796)) ;
#63731 = CARTESIAN_POINT('Ctrl Pts',(-20.4692073631793,-46.3673830153464,
122.836612591769)) ;
#63732 = CARTESIAN_POINT('Ctrl Pts',(-20.5880342149854,-46.5574489607873,
122.472055591262)) ;
#63733 = CARTESIAN_POINT('Ctrl Pts',(-20.3522770187593,-46.3774598804244,
122.660005096316)) ;
#63734 = CARTESIAN_POINT('Ctrl Pts',(-20.4094709146945,-46.5673137004426,
122.28408059887)) ;
#63735 = CARTESIAN_POINT('Ctrl Pts',(-20.2094265518685,-46.3873246200797,
122.509626284042)) ;
#63736 = CARTESIAN_POINT('Ctrl Pts',(-20.1980943113753,-46.5773361036839,
122.126973882739)) ;
#63737 = CARTESIAN_POINT('Ctrl Pts',(-20.0403249282567,-46.397347023321,122.383941308971)) ;
#63738 = CARTESIAN_POINT('Ctrl Pts',(-19.962253273062,-46.5873618279724,122.009494285123)) ;
#63739 = CARTESIAN_POINT('Ctrl Pts',(-19.8516517311113,-46.4073727476095,
122.289958211651)) ;
#63740 = CARTESIAN_POINT('Ctrl Pts',(-19.7140632034375,-46.5972166109937,
121.935594664619)) ;
#63741 = CARTESIAN_POINT('Ctrl Pts',(-19.6531005311567,-46.4172275306308,
122.230839367749)) ;
#63742 = CARTESIAN_POINT('Ctrl Pts',(-19.453631099447,-46.607195454717,121.904856532763)) ;
#63743 = CARTESIAN_POINT('Ctrl Pts',(-19.4447550642986,-46.4272063743541,
122.206249292798)) ;
#63744 = CARTESIAN_POINT('Ctrl Pts',(-19.1908123744642,-46.6172143469536,
121.920317600805)) ;
#63745 = CARTESIAN_POINT('Ctrl Pts',(-19.2345001020312,-46.4372252665907,
122.218618661177)) ;
#63746 = CARTESIAN_POINT('Ctrl Pts',(-18.9379696064049,-46.6270975559946,
121.979840758629)) ;
#63747 = CARTESIAN_POINT('Ctrl Pts',(-19.0322268301204,-46.4471084756317,
122.266237355114)) ;
#63748 = CARTESIAN_POINT('Ctrl Pts',(-18.6949496716682,-46.6371658653348,
122.084353104064)) ;
#63749 = CARTESIAN_POINT('Ctrl Pts',(-18.8378107414872,-46.4571767849719,
122.349847736102)) ;
#63750 = CARTESIAN_POINT('Ctrl Pts',(-18.4787605240765,-46.6469959906675,
122.225836194928)) ;
#63751 = CARTESIAN_POINT('Ctrl Pts',(-18.6648606358559,-46.4670069103046,
122.463033810365)) ;
#63752 = CARTESIAN_POINT('Ctrl Pts',(-18.2857214966169,-46.6570625430445,
122.406651152196)) ;
#63753 = CARTESIAN_POINT('Ctrl Pts',(-18.5104293493474,-46.4770734626816,
122.607686172701)) ;
#63754 = CARTESIAN_POINT('Ctrl Pts',(-18.1298739186722,-46.6669527799382,
122.614687511568)) ;
#63755 = CARTESIAN_POINT('Ctrl Pts',(-18.3857520197668,-46.4869636995753,
122.774114761019)) ;
#63756 = CARTESIAN_POINT('Ctrl Pts',(-18.0108157653476,-46.6769450047322,
122.848713195629)) ;
#63757 = CARTESIAN_POINT('Ctrl Pts',(-18.2905057011773,-46.4969559243693,
122.96133522007)) ;
#63758 = CARTESIAN_POINT('Ctrl Pts',(-17.9346569102099,-46.6869076250832,
123.099193972045)) ;
#63759 = CARTESIAN_POINT('Ctrl Pts',(-18.2295789196735,-46.5069185447203,
123.161719551088)) ;
#63760 = CARTESIAN_POINT('Ctrl Pts',(-17.9026865142012,-46.6968126278463,
123.35753421386)) ;
#63761 = CARTESIAN_POINT('Ctrl Pts',(-18.2040027337092,-46.5168235474834,
123.368391006395)) ;
#63762 = CARTESIAN_POINT('Ctrl Pts',(-17.9164439568202,-46.7068703902444,
123.621460054285)) ;
#63763 = CARTESIAN_POINT('Ctrl Pts',(-18.2150087894346,-46.5268813098816,
123.579531944023)) ;
#63764 = CARTESIAN_POINT('Ctrl Pts',(-17.9743972615009,-46.7167209096232,
123.873771940566)) ;
#63765 = CARTESIAN_POINT('Ctrl Pts',(-18.2613712111539,-46.5367318292604,
123.781380349578)) ;
#63766 = CARTESIAN_POINT('Ctrl Pts',(-18.076585890768,-46.7267524866214,124.116760874155)) ;
#63767 = CARTESIAN_POINT('Ctrl Pts',(-18.343122043701,-46.5467634062585,123.97577162832)) ;
#63768 = CARTESIAN_POINT('Ctrl Pts',(-18.2195527491891,-46.7367622217263,
124.337596888945)) ;
#63769 = CARTESIAN_POINT('Ctrl Pts',(-18.4574955266173,-46.5567731413635,
124.15244040257)) ;
#63770 = CARTESIAN_POINT('Ctrl Pts',(-18.3966970018907,-46.7466717983526,
124.528446109055)) ;
#63771 = CARTESIAN_POINT('Ctrl Pts',(-18.5992104071735,-46.5666827179897,
124.30511928162)) ;
#63772 = CARTESIAN_POINT('Ctrl Pts',(-18.6042842738298,-46.7565991842093,
124.686473857333)) ;
#63773 = CARTESIAN_POINT('Ctrl Pts',(-18.7652796215495,-46.5766101038464,
124.431541287681)) ;
#63774 = CARTESIAN_POINT('Ctrl Pts',(-18.8389799600762,-46.7666441186995,
124.807271873775)) ;
#63775 = CARTESIAN_POINT('Ctrl Pts',(-18.9530362508393,-46.5866550383367,
124.528179918756)) ;
#63776 = CARTESIAN_POINT('Ctrl Pts',(-19.0870750670697,-46.7765300508875,
124.884401576548)) ;
#63777 = CARTESIAN_POINT('Ctrl Pts',(-19.1515114465665,-46.5965409705246,
124.589883612155)) ;
#63778 = CARTESIAN_POINT('Ctrl Pts',(-19.3475046537344,-46.7865233568405,
124.918084459445)) ;
#63779 = CARTESIAN_POINT('Ctrl Pts',(-19.3598549143501,-46.6065342764777,
124.616830206673)) ;
#63780 = CARTESIAN_POINT('Ctrl Pts',(-19.6085865453895,-46.7964689946224,
124.905990634094)) ;
#63781 = CARTESIAN_POINT('Ctrl Pts',(-19.5687199653506,-46.6164799142595,
124.607155453148)) ;
#63782 = CARTESIAN_POINT('Ctrl Pts',(-19.8637733413823,-46.8064162629683,
124.84925888775)) ;
#63783 = CARTESIAN_POINT('Ctrl Pts',(-19.7728690447604,-46.6264271826054,
124.561770566073)) ;
#63784 = CARTESIAN_POINT('Ctrl Pts',(-20.1075420667063,-46.8164641651054,
124.747800719658)) ;
#63785 = CARTESIAN_POINT('Ctrl Pts',(-19.9678843424592,-46.6364750847425,
124.480604273047)) ;
#63786 = CARTESIAN_POINT('Ctrl Pts',(-20.3256846821778,-46.8263118599456,
124.608569806517)) ;
#63787 = CARTESIAN_POINT('Ctrl Pts',(-20.1423977064483,-46.6463227795827,
124.369220481856)) ;
#63788 = CARTESIAN_POINT('Ctrl Pts',(-20.5190914280319,-46.83627336969,124.432171593144)) ;
#63789 = CARTESIAN_POINT('Ctrl Pts',(-20.297123242795,-46.6562842893271,124.2281026054)) ;
#63790 = CARTESIAN_POINT('Ctrl Pts',(-20.6797539090321,-46.8463027612989,
124.223227378211)) ;
#63791 = CARTESIAN_POINT('Ctrl Pts',(-20.42565368723,-46.666313680936,124.060947484944)) ;
#63792 = CARTESIAN_POINT('Ctrl Pts',(-20.8003366055072,-46.8562102568536,
123.992472885729)) ;
#63793 = CARTESIAN_POINT('Ctrl Pts',(-20.5221200032968,-46.6762211764908,
123.876344781865)) ;
#63794 = CARTESIAN_POINT('Ctrl Pts',(-20.8798121649612,-46.8661556485166,
123.743517315993)) ;
#63795 = CARTESIAN_POINT('Ctrl Pts',(-20.5857009581305,-46.6861665681538,
123.6771809766)) ;
#63796 = CARTESIAN_POINT('Ctrl Pts',(-20.915214625767,-46.876157566114,123.48303667498)) ;
#63797 = CARTESIAN_POINT('Ctrl Pts',(-20.614023626857,-46.6961684857511,123.468796661138)) ;
#63798 = CARTESIAN_POINT('Ctrl Pts',(-20.9043274469187,-46.8861976336662,
123.219443241607)) ;
#63799 = CARTESIAN_POINT('Ctrl Pts',(-20.605314478917,-46.7062085533033,123.257921751627)) ;
#63800 = CARTESIAN_POINT('Ctrl Pts',(-20.8496146260734,-46.896021945106,122.967111685229)) ;
#63801 = CARTESIAN_POINT('Ctrl Pts',(-20.5615452065626,-46.7160328647431,
123.056057541106)) ;
#63802 = CARTESIAN_POINT('Ctrl Pts',(-20.7499690603553,-46.9060781862621,
122.722378928017)) ;
#63803 = CARTESIAN_POINT('Ctrl Pts',(-20.481829431188,-46.7260891058992,122.860270789842)) ;
#63804 = CARTESIAN_POINT('Ctrl Pts',(-20.6108065948018,-46.9160091079977,
122.501569334543)) ;
#63805 = CARTESIAN_POINT('Ctrl Pts',(-20.3705003850126,-46.7360200276349,
122.683623170689)) ;
#63806 = CARTESIAN_POINT('Ctrl Pts',(-20.4356383205666,-46.925952344074,122.307725777461)) ;
#63807 = CARTESIAN_POINT('Ctrl Pts',(-20.2303667445202,-46.7459632637111,
122.528548091162)) ;
#63808 = CARTESIAN_POINT('Ctrl Pts',(-20.2287819479061,-46.9359336280864,
122.146383450111)) ;
#63809 = CARTESIAN_POINT('Ctrl Pts',(-20.0648823935122,-46.7559445477236,
122.399473615786)) ;
#63810 = CARTESIAN_POINT('Ctrl Pts',(-19.9954418662365,-46.9459779297121,
122.023069093696)) ;
#63811 = CARTESIAN_POINT('Ctrl Pts',(-19.8782105832335,-46.7659888493492,
122.300821320702)) ;
#63812 = CARTESIAN_POINT('Ctrl Pts',(-19.7497569427276,-46.9558060109315,
121.943291660823)) ;
#63813 = CARTESIAN_POINT('Ctrl Pts',(-19.6816640439892,-46.7758169305687,
122.236998801319)) ;
#63814 = CARTESIAN_POINT('Ctrl Pts',(-19.4875976586509,-46.9658826137807,
121.90636263565)) ;
#63815 = CARTESIAN_POINT('Ctrl Pts',(-19.4719364151813,-46.7858935334178,
122.207454534728)) ;
#63816 = CARTESIAN_POINT('Ctrl Pts',(-19.228788648694,-46.9757346928992,121.915184765414)) ;
#63817 = CARTESIAN_POINT('Ctrl Pts',(-19.2648901580032,-46.7957456125364,
122.214511170181)) ;
#63818 = CARTESIAN_POINT('Ctrl Pts',(-18.9698079849325,-46.9858079512082,
121.969772870616)) ;
#63819 = CARTESIAN_POINT('Ctrl Pts',(-19.0577050887598,-46.8058188708453,
122.258180656131)) ;
#63820 = CARTESIAN_POINT('Ctrl Pts',(-18.7298606158885,-46.9956494105884,
122.066316849577)) ;
#63821 = CARTESIAN_POINT('Ctrl Pts',(-18.8657477611846,-46.8156603302256,
122.335414457744)) ;
#63822 = CARTESIAN_POINT('Ctrl Pts',(-18.507158497528,-47.0056105060008,122.203869923558)) ;
#63823 = CARTESIAN_POINT('Ctrl Pts',(-18.6875856641331,-46.8256214256379,
122.445455650075)) ;
#63824 = CARTESIAN_POINT('Ctrl Pts',(-18.3105700406655,-47.0156477903975,
122.379722097263)) ;
#63825 = CARTESIAN_POINT('Ctrl Pts',(-18.5303140387269,-46.8356587100347,
122.586136582411)) ;
#63826 = CARTESIAN_POINT('Ctrl Pts',(-18.1497383800558,-47.0255241291328,
122.583459652795)) ;
#63827 = CARTESIAN_POINT('Ctrl Pts',(-18.4016482050606,-46.8455350487699,
122.749125213228)) ;
#63828 = CARTESIAN_POINT('Ctrl Pts',(-18.0243973839348,-47.0355862552861,
122.816248967698)) ;
#63829 = CARTESIAN_POINT('Ctrl Pts',(-18.3013741678358,-46.8555971749232,
122.935356256442)) ;
#63830 = CARTESIAN_POINT('Ctrl Pts',(-17.942900261197,-47.0454544292626,123.062469015826)) ;
#63831 = CARTESIAN_POINT('Ctrl Pts',(-18.2361754986026,-46.8654653488997,
123.132331099916)) ;
#63832 = CARTESIAN_POINT('Ctrl Pts',(-17.9043551712799,-47.0554599777664,
123.322528432364)) ;
#63833 = CARTESIAN_POINT('Ctrl Pts',(-18.2053380449325,-46.8754708974035,
123.340378359643)) ;
#63834 = CARTESIAN_POINT('Ctrl Pts',(-17.911626244223,-47.065442609662,123.58480879542)) ;
#63835 = CARTESIAN_POINT('Ctrl Pts',(-18.2111535111412,-46.8854535292991,
123.55020250964)) ;
#63836 = CARTESIAN_POINT('Ctrl Pts',(-17.964905818864,-47.0754865520838,123.843296984547)) ;
#63837 = CARTESIAN_POINT('Ctrl Pts',(-18.2537758946358,-46.8954974717209,
123.756993455038)) ;
#63838 = CARTESIAN_POINT('Ctrl Pts',(-18.0598529385593,-47.0853147001109,
124.083485382796)) ;
#63839 = CARTESIAN_POINT('Ctrl Pts',(-18.3297319083217,-46.9053256197481,
123.949143731469)) ;
#63840 = CARTESIAN_POINT('Ctrl Pts',(-18.1965689479448,-47.0953045674853,
124.307600675723)) ;
#63841 = CARTESIAN_POINT('Ctrl Pts',(-18.4391033021549,-46.9153154871225,
124.128436666438)) ;
#63842 = CARTESIAN_POINT('Ctrl Pts',(-18.3715713484641,-47.1053483064408,
124.505180389695)) ;
#63843 = CARTESIAN_POINT('Ctrl Pts',(-18.5791042261939,-46.925359226078,124.286501476418)) ;
#63844 = CARTESIAN_POINT('Ctrl Pts',(-18.5733188648744,-47.1151700549788,
124.666164420579)) ;
#63845 = CARTESIAN_POINT('Ctrl Pts',(-18.7405004989235,-46.9351809746159,
124.41528928464)) ;
#63846 = CARTESIAN_POINT('Ctrl Pts',(-18.8045645528301,-47.1252050325885,
124.792922450378)) ;
#63847 = CARTESIAN_POINT('Ctrl Pts',(-18.9254963238758,-46.9452159522256,
124.516697207204)) ;
#63848 = CARTESIAN_POINT('Ctrl Pts',(-19.0542980945525,-47.1352299453462,
124.876825162639)) ;
#63849 = CARTESIAN_POINT('Ctrl Pts',(-19.1252826902165,-46.9552408649833,
124.583820828544)) ;
#63850 = CARTESIAN_POINT('Ctrl Pts',(-19.3102255315884,-47.14508188844,124.915973693937)) ;
#63851 = CARTESIAN_POINT('Ctrl Pts',(-19.3300235960743,-46.9650928080772,
124.615141143761)) ;
#63852 = CARTESIAN_POINT('Ctrl Pts',(-19.5726863790115,-47.1550728497691,
124.910409512825)) ;
#63853 = CARTESIAN_POINT('Ctrl Pts',(-19.5399921733102,-46.9750837694063,
124.61069150596)) ;
#63854 = CARTESIAN_POINT('Ctrl Pts',(-19.8284072327233,-47.1649907246376,
124.859887472714)) ;
#63855 = CARTESIAN_POINT('Ctrl Pts',(-19.7445687433349,-46.9850016442747,
124.570275659941)) ;
#63856 = CARTESIAN_POINT('Ctrl Pts',(-20.074151105226,-47.1750192436388,124.764752235649)) ;
#63857 = CARTESIAN_POINT('Ctrl Pts',(-19.9411644966269,-46.9950301632759,
124.494169084387)) ;
#63858 = CARTESIAN_POINT('Ctrl Pts',(-20.2964844789698,-47.1849029224366,
124.630459757665)) ;
#63859 = CARTESIAN_POINT('Ctrl Pts',(-20.1190316002392,-47.0049138420738,
124.386736915918)) ;
#63860 = CARTESIAN_POINT('Ctrl Pts',(-20.4946972413566,-47.1948978658764,
124.458122754185)) ;
#63861 = CARTESIAN_POINT('Ctrl Pts',(-20.2776029447661,-47.0149087855135,
124.248868788224)) ;
#63862 = CARTESIAN_POINT('Ctrl Pts',(-20.6601527760735,-47.2049247196988,
124.253049913782)) ;
#63863 = CARTESIAN_POINT('Ctrl Pts',(-20.4099687724888,-47.0249356393359,
124.084811622413)) ;
#63864 = CARTESIAN_POINT('Ctrl Pts',(-20.7859931800233,-47.2148088840377,
124.025810555363)) ;
#63865 = CARTESIAN_POINT('Ctrl Pts',(-20.5106424360365,-47.0348198036749,
123.90302151066)) ;
#63866 = CARTESIAN_POINT('Ctrl Pts',(-20.8716717234267,-47.2247969820801,
123.777738571855)) ;
#63867 = CARTESIAN_POINT('Ctrl Pts',(-20.5791870192374,-47.0448079017172,
123.704564663885)) ;
#63868 = CARTESIAN_POINT('Ctrl Pts',(-20.912975435298,-47.2347480885372,123.519483140428)) ;
#63869 = CARTESIAN_POINT('Ctrl Pts',(-20.6122318336066,-47.0547590081743,
123.497960883868)) ;
#63870 = CARTESIAN_POINT('Ctrl Pts',(-20.908624300372,-47.2447931397053,123.255561025828)) ;
#63871 = CARTESIAN_POINT('Ctrl Pts',(-20.6087528155346,-47.0648040593424,
123.286823089854)) ;
#63872 = CARTESIAN_POINT('Ctrl Pts',(-20.8595658745191,-47.2546549000636,
123.001088343712)) ;
#63873 = CARTESIAN_POINT('Ctrl Pts',(-20.5695080656259,-47.0746658197007,
123.083245164195)) ;
#63874 = CARTESIAN_POINT('Ctrl Pts',(-20.7668750532524,-47.264617716894,122.756231591829)) ;
#63875 = CARTESIAN_POINT('Ctrl Pts',(-20.4953573697405,-47.0846286365312,
122.887359233057)) ;
#63876 = CARTESIAN_POINT('Ctrl Pts',(-20.6317297453688,-47.2746523981748,
122.529807845383)) ;
#63877 = CARTESIAN_POINT('Ctrl Pts',(-20.3872427942103,-47.0946633178119,
122.706219207797)) ;
#63878 = CARTESIAN_POINT('Ctrl Pts',(-20.4621990513068,-47.2845374279556,
122.332938364002)) ;
#63879 = CARTESIAN_POINT('Ctrl Pts',(-20.2516200615866,-47.1045483475927,
122.548722648107)) ;
#63880 = CARTESIAN_POINT('Ctrl Pts',(-20.2574099722437,-47.2946030213536,
122.16558837992)) ;
#63881 = CARTESIAN_POINT('Ctrl Pts',(-20.0877899799016,-47.1146139409907,
122.414841027643)) ;
#63882 = CARTESIAN_POINT('Ctrl Pts',(-20.0319196599626,-47.3044421897151,
122.038978242884)) ;
#63883 = CARTESIAN_POINT('Ctrl Pts',(-19.9073992209969,-47.1244531093522,
122.313551415424)) ;
#63884 = CARTESIAN_POINT('Ctrl Pts',(-19.7825183008089,-47.3145047874566,
121.95118250225)) ;
#63885 = CARTESIAN_POINT('Ctrl Pts',(-19.7078787262288,-47.1345157070937,
122.243312822989)) ;
#63886 = CARTESIAN_POINT('Ctrl Pts',(-19.5258624977633,-47.3244017998635,
121.909002521009)) ;
#63887 = CARTESIAN_POINT('Ctrl Pts',(-19.502554784226,-47.1444127195006,122.209566874311)) ;
#63888 = CARTESIAN_POINT('Ctrl Pts',(-19.2648924723534,-47.3343331216891,
121.911168475374)) ;
#63889 = CARTESIAN_POINT('Ctrl Pts',(-19.2937789864561,-47.1543440413262,
122.211297494334)) ;
#63890 = CARTESIAN_POINT('Ctrl Pts',(-19.0054588236434,-47.3443748844436,
121.959423773206)) ;
#63891 = CARTESIAN_POINT('Ctrl Pts',(-19.0862316578282,-47.1643858040807,
122.249899661236)) ;
#63892 = CARTESIAN_POINT('Ctrl Pts',(-18.7620408415515,-47.3542630833343,
122.050409572673)) ;
#63893 = CARTESIAN_POINT('Ctrl Pts',(-18.8914968446578,-47.1742740029714,
122.322686186617)) ;
#63894 = CARTESIAN_POINT('Ctrl Pts',(-18.5355442147587,-47.3642570219342,
122.18331150089)) ;
#63895 = CARTESIAN_POINT('Ctrl Pts',(-18.7102985172249,-47.1842679415713,
122.429005819235)) ;
#63896 = CARTESIAN_POINT('Ctrl Pts',(-18.3366094811848,-47.374197842971,122.352654796007)) ;
#63897 = CARTESIAN_POINT('Ctrl Pts',(-18.551149473623,-47.1942087626082,122.564478686452)) ;
#63898 = CARTESIAN_POINT('Ctrl Pts',(-18.1695526330089,-47.3841572252593,
122.554106932035)) ;
#63899 = CARTESIAN_POINT('Ctrl Pts',(-18.417502400572,-47.2041681448964,122.725638889882)) ;
#63900 = CARTESIAN_POINT('Ctrl Pts',(-18.0393553532008,-47.3941549849116,
122.782338451518)) ;
#63901 = CARTESIAN_POINT('Ctrl Pts',(-18.3133427031119,-47.2141659045487,
122.908222957332)) ;
#63902 = CARTESIAN_POINT('Ctrl Pts',(-17.9507774145601,-47.4041911211139,
123.03075086766)) ;
#63903 = CARTESIAN_POINT('Ctrl Pts',(-18.2424783105885,-47.224202040751,123.106952144432)) ;
#63904 = CARTESIAN_POINT('Ctrl Pts',(-17.9071905133116,-47.4140419186048,
123.285921661673)) ;
#63905 = CARTESIAN_POINT('Ctrl Pts',(-18.2076066786079,-47.2340528382419,
123.311088103092)) ;
#63906 = CARTESIAN_POINT('Ctrl Pts',(-17.9078079177087,-47.4240027836811,
123.547672833049)) ;
#63907 = CARTESIAN_POINT('Ctrl Pts',(-18.2080983638521,-47.2440137033182,
123.520488944659)) ;
#63908 = CARTESIAN_POINT('Ctrl Pts',(-17.9544972057267,-47.4340316513115,
123.807067402969)) ;
#63909 = CARTESIAN_POINT('Ctrl Pts',(-18.2454476048845,-47.2540425709486,
123.728004959381)) ;
#63910 = CARTESIAN_POINT('Ctrl Pts',(-18.0443558522348,-47.4439418874479,
124.051493099895)) ;
#63911 = CARTESIAN_POINT('Ctrl Pts',(-18.3173323750563,-47.263952807085,123.923546127263)) ;
#63912 = CARTESIAN_POINT('Ctrl Pts',(-18.1750338402729,-47.4538768407624,
124.27752403088)) ;
#63913 = CARTESIAN_POINT('Ctrl Pts',(-18.4218727658216,-47.2738877603996,
124.10437190683)) ;
#63914 = CARTESIAN_POINT('Ctrl Pts',(-18.3449402389459,-47.463917771172,124.479398422713)) ;
#63915 = CARTESIAN_POINT('Ctrl Pts',(-18.5577961461573,-47.2839286908091,
124.265872834734)) ;
#63916 = CARTESIAN_POINT('Ctrl Pts',(-18.5441394208993,-47.4738056679536,
124.646262687843)) ;
#63917 = CARTESIAN_POINT('Ctrl Pts',(-18.717153951654,-47.2938165875907,124.399365886383)) ;
#63918 = CARTESIAN_POINT('Ctrl Pts',(-18.7713398491585,-47.4837951196123,
124.777752129253)) ;
#63919 = CARTESIAN_POINT('Ctrl Pts',(-18.8989131176986,-47.3038060392494,
124.504559363541)) ;
#63920 = CARTESIAN_POINT('Ctrl Pts',(-19.0172406224052,-47.4937542099777,
124.867323859579)) ;
#63921 = CARTESIAN_POINT('Ctrl Pts',(-19.0956328934438,-47.3137651296148,
124.576218838424)) ;
#63922 = CARTESIAN_POINT('Ctrl Pts',(-19.2732681589925,-47.503651522284,124.913214982479)) ;
#63923 = CARTESIAN_POINT('Ctrl Pts',(-19.3004544847699,-47.3236624419211,
124.612933948275)) ;
#63924 = CARTESIAN_POINT('Ctrl Pts',(-19.5375180334294,-47.5137079481842,
124.913840318976)) ;
#63925 = CARTESIAN_POINT('Ctrl Pts',(-19.5118543105369,-47.3337188678213,
124.613436469234)) ;
#63926 = CARTESIAN_POINT('Ctrl Pts',(-19.7931038035126,-47.523577950774,124.86953541503)) ;
#63927 = CARTESIAN_POINT('Ctrl Pts',(-19.7163232953093,-47.3435888704111,
124.577994777982)) ;
#63928 = CARTESIAN_POINT('Ctrl Pts',(-20.0405538778607,-47.5335818839512,
124.780842159389)) ;
#63929 = CARTESIAN_POINT('Ctrl Pts',(-19.9142841000956,-47.3535928035883,
124.507042257219)) ;
#63930 = CARTESIAN_POINT('Ctrl Pts',(-20.2684557085201,-47.5435691444151,
124.650592871632)) ;
#63931 = CARTESIAN_POINT('Ctrl Pts',(-20.096606520165,-47.3635800640522,124.402844965088)) ;
#63932 = CARTESIAN_POINT('Ctrl Pts',(-20.470938720581,-47.5535961960008,124.482002870623)) ;
#63933 = CARTESIAN_POINT('Ctrl Pts',(-20.2585947483738,-47.3736071156379,
124.267974120626)) ;
#63934 = CARTESIAN_POINT('Ctrl Pts',(-20.6389889194383,-47.5634872858269,
124.283677447582)) ;
#63935 = CARTESIAN_POINT('Ctrl Pts',(-20.3930350147794,-47.383498205464,124.109317524504)) ;
#63936 = CARTESIAN_POINT('Ctrl Pts',(-20.8155222736475,-47.576785040608,123.982153459967)) ;
#63937 = CARTESIAN_POINT('Ctrl Pts',(-20.5342723572746,-47.3967959602451,
123.86808831075)) ;
#63938 = CARTESIAN_POINT('Ctrl Pts',(-20.9091627271371,-47.5899831002161,
123.644050843664)) ;
#63939 = CARTESIAN_POINT('Ctrl Pts',(-20.6091851817961,-47.4099940198532,
123.597577609492)) ;
#63940 = CARTESIAN_POINT('Ctrl Pts',(-20.911961468793,-47.6033798407853,123.29203099922)) ;
#63941 = CARTESIAN_POINT('Ctrl Pts',(-20.6114219138469,-47.4233907604224,
123.316008249511)) ;
#63942 = CARTESIAN_POINT('Ctrl Pts',(-20.8692234169841,-47.6132507528587,
123.036128094905)) ;
#63943 = CARTESIAN_POINT('Ctrl Pts',(-20.5772346237464,-47.4332616724959,
123.111276038365)) ;
#63944 = CARTESIAN_POINT('Ctrl Pts',(-20.7809529679,-47.6233243146269,122.78661751852)) ;
#63945 = CARTESIAN_POINT('Ctrl Pts',(-20.5066201804174,-47.443335234264,122.911669620032)) ;
#63946 = CARTESIAN_POINT('Ctrl Pts',(-20.6541739490141,-47.6331457272152,
122.561735103917)) ;
#63947 = CARTESIAN_POINT('Ctrl Pts',(-20.405198506557,-47.4531566468523,122.731761296753)) ;
#63948 = CARTESIAN_POINT('Ctrl Pts',(-20.4863320285724,-47.6432197444462,
122.357091382162)) ;
#63949 = CARTESIAN_POINT('Ctrl Pts',(-20.2709276233739,-47.4632306640834,
122.568046598626)) ;
#63950 = CARTESIAN_POINT('Ctrl Pts',(-20.2240587467137,-47.6563785314108,
122.131615915309)) ;
#63951 = CARTESIAN_POINT('Ctrl Pts',(-20.0611061721674,-47.4763894510479,
122.387657331464)) ;
#63952 = CARTESIAN_POINT('Ctrl Pts',(-19.904396611808,-47.669744634505,121.976897634996)) ;
#63953 = CARTESIAN_POINT('Ctrl Pts',(-19.8053424387584,-47.4897555541421,
122.263873680573)) ;
#63954 = CARTESIAN_POINT('Ctrl Pts',(-19.5604802159987,-47.683058569394,121.912018372431)) ;
#63955 = CARTESIAN_POINT('Ctrl Pts',(-19.5302562121692,-47.5030694890312,
122.211981762191)) ;
#63956 = CARTESIAN_POINT('Ctrl Pts',(-19.3003815270742,-47.6929586088415,
121.908333183184)) ;
#63957 = CARTESIAN_POINT('Ctrl Pts',(-19.322167620802,-47.5129695284786,122.209028724385)) ;
#63958 = CARTESIAN_POINT('Ctrl Pts',(-19.0418005240808,-47.702923011976,121.949706846036)) ;
#63959 = CARTESIAN_POINT('Ctrl Pts',(-19.1153050560258,-47.5229339316132,
122.242126300754)) ;
#63960 = CARTESIAN_POINT('Ctrl Pts',(-18.7927924422109,-47.7129529790972,
122.036134213176)) ;
#63961 = CARTESIAN_POINT('Ctrl Pts',(-18.9160968262407,-47.5329638987343,
122.311266676217)) ;
#63962 = CARTESIAN_POINT('Ctrl Pts',(-18.5654632174081,-47.7228552557062,
122.162745640329)) ;
#63963 = CARTESIAN_POINT('Ctrl Pts',(-18.734234498539,-47.5428661753434,122.412551849973)) ;
#63964 = CARTESIAN_POINT('Ctrl Pts',(-18.2943866086344,-47.7361211848754,
122.382011147429)) ;
#63965 = CARTESIAN_POINT('Ctrl Pts',(-18.5173605390981,-47.5561321045125,
122.587974585937)) ;
#63966 = CARTESIAN_POINT('Ctrl Pts',(-18.0346303797176,-47.7527427159818,
122.739250673809)) ;
#63967 = CARTESIAN_POINT('Ctrl Pts',(-18.3095657843141,-47.5727536356189,
122.873754271504)) ;
#63968 = CARTESIAN_POINT('Ctrl Pts',(-17.8876997701404,-47.7726175446265,
123.246720784385)) ;
#63969 = CARTESIAN_POINT('Ctrl Pts',(-18.192010176043,-47.5926284642636,123.27971738618)) ;
#63970 = CARTESIAN_POINT('Ctrl Pts',(-17.917000592734,-47.7892907527283,123.68884871812)) ;
#63971 = CARTESIAN_POINT('Ctrl Pts',(-18.2154597786599,-47.6093016723655,
123.63347188355)) ;
#63972 = CARTESIAN_POINT('Ctrl Pts',(-18.0293936752082,-47.8025418777096,
124.018462677686)) ;
#63973 = CARTESIAN_POINT('Ctrl Pts',(-18.305361509496,-47.6225527973467,123.897116801206)) ;
#63974 = CARTESIAN_POINT('Ctrl Pts',(-18.1961054880451,-47.8157841965304,
124.323995100748)) ;
#63975 = CARTESIAN_POINT('Ctrl Pts',(-18.4387378061925,-47.6357951161676,
124.141559984397)) ;
#63976 = CARTESIAN_POINT('Ctrl Pts',(-18.5033373266895,-47.8325174368699,
124.645448284564)) ;
#63977 = CARTESIAN_POINT('Ctrl Pts',(-18.6845128198436,-47.652528356507,124.398713602975)) ;
#63978 = CARTESIAN_POINT('Ctrl Pts',(-18.9757346113331,-47.8523465850579,
124.879336049279)) ;
#63979 = CARTESIAN_POINT('Ctrl Pts',(-19.0624327890952,-47.672357504695,124.585830613588)) ;
#63980 = CARTESIAN_POINT('Ctrl Pts',(-19.5017537468954,-47.8722712801585,
124.939516678205)) ;
#63981 = CARTESIAN_POINT('Ctrl Pts',(-19.4832476587856,-47.6922821997956,
124.633977069387)) ;
#63982 = CARTESIAN_POINT('Ctrl Pts',(-20.016875861944,-47.8921945087419,124.816493222092)) ;
#63983 = CARTESIAN_POINT('Ctrl Pts',(-19.8953467115458,-47.7122054283791,
124.535561030838)) ;
#63984 = CARTESIAN_POINT('Ctrl Pts',(-20.4591503180632,-47.912121647868,124.525228376918)) ;
#63985 = CARTESIAN_POINT('Ctrl Pts',(-20.2491681384619,-47.7321325675052,
124.302550855083)) ;
#63986 = CARTESIAN_POINT('Ctrl Pts',(-20.7752836476955,-47.9319981104837,
124.101934449769)) ;
#63987 = CARTESIAN_POINT('Ctrl Pts',(-20.5020771966928,-47.7520090301208,
123.963916114928)) ;
#63988 = CARTESIAN_POINT('Ctrl Pts',(-20.9290246638759,-47.951975339089,123.593724361099)) ;
#63989 = CARTESIAN_POINT('Ctrl Pts',(-20.6250718773028,-47.7719862587261,
123.557348393509)) ;
#63990 = CARTESIAN_POINT('Ctrl Pts',(-20.899749641412,-47.9719101970627,123.064652071563)) ;
#63991 = CARTESIAN_POINT('Ctrl Pts',(-20.6016537118098,-47.7919211166998,
123.134089837888)) ;
#63992 = CARTESIAN_POINT('Ctrl Pts',(-20.6926191392148,-47.9918066459935,
122.578134849579)) ;
#63993 = CARTESIAN_POINT('Ctrl Pts',(-20.4359502844163,-47.8118175656306,
122.744874452236)) ;
#63994 = CARTESIAN_POINT('Ctrl Pts',(-20.3318393279067,-48.0117279300601,
122.190571444876)) ;
#63995 = CARTESIAN_POINT('Ctrl Pts',(-20.147326663776,-47.8317388496972,122.434822343269)) ;
#63996 = CARTESIAN_POINT('Ctrl Pts',(-19.859543379667,-48.0316845797311,121.949105900427)) ;
#63997 = CARTESIAN_POINT('Ctrl Pts',(-19.7694899560227,-47.8516954993682,
122.241648817227)) ;
#63998 = CARTESIAN_POINT('Ctrl Pts',(-19.3354077539481,-48.0515618728427,
121.883411775971)) ;
#63999 = CARTESIAN_POINT('Ctrl Pts',(-19.3501800444516,-47.8715727924798,
122.189092575261)) ;
#64000 = CARTESIAN_POINT('Ctrl Pts',(-18.8196458602332,-48.0714483450711,
121.999233714919)) ;
#64001 = CARTESIAN_POINT('Ctrl Pts',(-18.9375691001692,-47.8914592647082,
122.281750583357)) ;
#64002 = CARTESIAN_POINT('Ctrl Pts',(-18.3709126385938,-48.0915099109951,
122.287270877205)) ;
#64003 = CARTESIAN_POINT('Ctrl Pts',(-18.578583226595,-47.9115208306322,122.512179806311)) ;
#64004 = CARTESIAN_POINT('Ctrl Pts',(-18.0514008754144,-48.1113503185359,
122.706744756814)) ;
#64005 = CARTESIAN_POINT('Ctrl Pts',(-18.3229724703465,-47.931361238173,122.847760542803)) ;
#64006 = CARTESIAN_POINT('Ctrl Pts',(-17.8920053839532,-48.1312016425088,
123.209726070964)) ;
#64007 = CARTESIAN_POINT('Ctrl Pts',(-18.1954566722783,-47.9512125621459,
123.250147612826)) ;
#64008 = CARTESIAN_POINT('Ctrl Pts',(-17.9148449517258,-48.1512549124602,
123.742150506195)) ;
#64009 = CARTESIAN_POINT('Ctrl Pts',(-18.2137292815851,-47.9712658320974,
123.676086505446)) ;
#64010 = CARTESIAN_POINT('Ctrl Pts',(-18.1156214422887,-48.1710755698436,
124.229345578872)) ;
#64011 = CARTESIAN_POINT('Ctrl Pts',(-18.3743523078456,-47.9910864894807,
124.065843886977)) ;
#64012 = CARTESIAN_POINT('Ctrl Pts',(-18.4724496628158,-48.1910469911741,
124.622086302263)) ;
#64013 = CARTESIAN_POINT('Ctrl Pts',(-18.659816387674,-48.0110579108112,124.380035522052)) ;
#64014 = CARTESIAN_POINT('Ctrl Pts',(-18.9403084788893,-48.2109404835378,
124.86880464151)) ;
#64015 = CARTESIAN_POINT('Ctrl Pts',(-19.03410518183,-48.0309514031749,124.577408955661)) ;
#64016 = CARTESIAN_POINT('Ctrl Pts',(-19.4674642242549,-48.2309645697788,
124.941135895711)) ;
#64017 = CARTESIAN_POINT('Ctrl Pts',(-19.4558298576854,-48.050975489416,124.635271999274)) ;
#64018 = CARTESIAN_POINT('Ctrl Pts',(-19.982186864098,-48.2507694488917,124.830704772301)) ;
#64019 = CARTESIAN_POINT('Ctrl Pts',(-19.867609211054,-48.0707803685288,124.546924581979)) ;
#64020 = CARTESIAN_POINT('Ctrl Pts',(-20.4325013285474,-48.2707284645896,
124.550337764469)) ;
#64021 = CARTESIAN_POINT('Ctrl Pts',(-20.227859532346,-48.0907393842267,124.32262844544)) ;
#64022 = CARTESIAN_POINT('Ctrl Pts',(-20.7595855617661,-48.2907144882186,
124.131795730191)) ;
#64023 = CARTESIAN_POINT('Ctrl Pts',(-20.4895249857821,-48.1107254078558,
123.987793147059)) ;
#64024 = CARTESIAN_POINT('Ctrl Pts',(-20.9237469669242,-48.3105229839791,
123.631516939085)) ;
#64025 = CARTESIAN_POINT('Ctrl Pts',(-20.6208517088242,-48.1305339036163,
123.587567868658)) ;
#64026 = CARTESIAN_POINT('Ctrl Pts',(-20.9078563777569,-48.3305056230847,
123.100761863428)) ;
#64027 = CARTESIAN_POINT('Ctrl Pts',(-20.6081359619185,-48.1505165427219,
123.162963825818)) ;
#64028 = CARTESIAN_POINT('Ctrl Pts',(-20.7125774921877,-48.3503870708787,
122.609609792286)) ;
#64029 = CARTESIAN_POINT('Ctrl Pts',(-20.4519095117402,-48.1703979905159,
122.770042764306)) ;
#64030 = CARTESIAN_POINT('Ctrl Pts',(-20.3605699834758,-48.3703435376163,
122.212992650453)) ;
#64031 = CARTESIAN_POINT('Ctrl Pts',(-20.1703007092997,-48.1903544572534,
122.452751209908)) ;
#64032 = CARTESIAN_POINT('Ctrl Pts',(-19.8961915070511,-48.3902209345718,
121.960894036844)) ;
#64033 = CARTESIAN_POINT('Ctrl Pts',(-19.7987956286007,-48.210231854209,122.2510753083)) ;
#64034 = CARTESIAN_POINT('Ctrl Pts',(-19.3710944052881,-48.4102028807471,
121.881710834972)) ;
#64035 = CARTESIAN_POINT('Ctrl Pts',(-19.3787173826546,-48.2302138003843,
122.1877323754)) ;
#64036 = CARTESIAN_POINT('Ctrl Pts',(-18.8517658005324,-48.4301319797839,
121.986485155074)) ;
#64037 = CARTESIAN_POINT('Ctrl Pts',(-18.9632548451584,-48.250142899421,122.271556232587)) ;
#64038 = CARTESIAN_POINT('Ctrl Pts',(-18.3995108077568,-48.4500606029965,
122.262000851826)) ;
#64039 = CARTESIAN_POINT('Ctrl Pts',(-18.6014532429342,-48.2700715226336,
122.491970142446)) ;
#64040 = CARTESIAN_POINT('Ctrl Pts',(-18.0691275875861,-48.4698949271029,
122.672852581631)) ;
#64041 = CARTESIAN_POINT('Ctrl Pts',(-18.337147399175,-48.28990584674,122.820662663942)) ;
#64042 = CARTESIAN_POINT('Ctrl Pts',(-17.9257131670204,-48.4865472144863,
123.091471777967)) ;
#64043 = CARTESIAN_POINT('Ctrl Pts',(-18.2224260058625,-48.3065581341234,
123.155533896471)) ;
#64044 = CARTESIAN_POINT('Ctrl Pts',(-17.9020712050957,-48.4998077155085,
123.439203218313)) ;
#64045 = CARTESIAN_POINT('Ctrl Pts',(-18.2035092593179,-48.3198186351457,
123.433741819018)) ;
#64046 = CARTESIAN_POINT('Ctrl Pts',(-17.9295520562288,-48.5098091927098,
123.700586123899)) ;
#64047 = CARTESIAN_POINT('Ctrl Pts',(-18.2254971398453,-48.3298201123469,
123.642843255364)) ;
#64048 = CARTESIAN_POINT('Ctrl Pts',(-18.002650404669,-48.5198412135693,123.953887639431)) ;
#64049 = CARTESIAN_POINT('Ctrl Pts',(-18.2839780158191,-48.3398521332064,
123.845485394046)) ;
#64050 = CARTESIAN_POINT('Ctrl Pts',(-18.116381192127,-48.5297047572949,124.186799307421)) ;
#64051 = CARTESIAN_POINT('Ctrl Pts',(-18.3749628126578,-48.349715676932,124.031812191722)) ;
#64052 = CARTESIAN_POINT('Ctrl Pts',(-18.2698960730485,-48.539673470965,124.399078392856)) ;
#64053 = CARTESIAN_POINT('Ctrl Pts',(-18.4977838735188,-48.3596843906021,
124.201640071483)) ;
#64054 = CARTESIAN_POINT('Ctrl Pts',(-18.5219675225796,-48.5530192183687,
124.642888173834)) ;
#64055 = CARTESIAN_POINT('Ctrl Pts',(-18.6994062245984,-48.3730301380058,
124.396656830868)) ;
#64056 = CARTESIAN_POINT('Ctrl Pts',(-18.8271260677206,-48.5661697734414,
124.813370160914)) ;
#64057 = CARTESIAN_POINT('Ctrl Pts',(-18.9435542458751,-48.3861806930785,
124.533062412033)) ;
#64058 = CARTESIAN_POINT('Ctrl Pts',(-19.1680417733709,-48.5795551539912,
124.899907926004)) ;
#64059 = CARTESIAN_POINT('Ctrl Pts',(-19.2163009890961,-48.3995660736284,
124.602291912706)) ;
#64060 = CARTESIAN_POINT('Ctrl Pts',(-19.4272046606678,-48.5894430899841,
124.919132760716)) ;
#64061 = CARTESIAN_POINT('Ctrl Pts',(-19.4236288223874,-48.4094540096212,
124.617669122976)) ;
#64062 = CARTESIAN_POINT('Ctrl Pts',(-19.6884474342547,-48.5994342797967,
124.893240945766)) ;
#64063 = CARTESIAN_POINT('Ctrl Pts',(-19.6326235030201,-48.4194451994339,
124.596953556144)) ;
#64064 = CARTESIAN_POINT('Ctrl Pts',(-19.9403393905158,-48.609386378335,124.822747843543)) ;
#64065 = CARTESIAN_POINT('Ctrl Pts',(-19.834136251256,-48.4293972979721,124.540556882283)) ;
#64066 = CARTESIAN_POINT('Ctrl Pts',(-20.1782692262088,-48.6194326347855,
124.708388111913)) ;
#64067 = CARTESIAN_POINT('Ctrl Pts',(-20.0244791282803,-48.4394435544226,
124.449067115827)) ;
#64068 = CARTESIAN_POINT('Ctrl Pts',(-20.3886560573569,-48.6292820821796,
124.557608789877)) ;
#64069 = CARTESIAN_POINT('Ctrl Pts',(-20.1927872963318,-48.4492930018168,
124.328441805435)) ;
#64070 = CARTESIAN_POINT('Ctrl Pts',(-20.572326095922,-48.6392447346748,124.371049479693)) ;
#64071 = CARTESIAN_POINT('Ctrl Pts',(-20.3397216706453,-48.4592556543119,
124.179192818539)) ;
#64072 = CARTESIAN_POINT('Ctrl Pts',(-20.7214277473186,-48.6492678203169,
124.153918077393)) ;
#64073 = CARTESIAN_POINT('Ctrl Pts',(-20.4590011009063,-48.469278739954,124.005486461818)) ;
#64074 = CARTESIAN_POINT('Ctrl Pts',(-20.8297802315917,-48.6591929360738,
123.916635975645)) ;
#64075 = CARTESIAN_POINT('Ctrl Pts',(-20.5456810096503,-48.479203855711,123.815659897724)) ;
#64076 = CARTESIAN_POINT('Ctrl Pts',(-20.8960112318138,-48.6692454144736,
123.660930444406)) ;
#64077 = CARTESIAN_POINT('Ctrl Pts',(-20.5986636102316,-48.4892563341108,
123.611094951253)) ;
#64078 = CARTESIAN_POINT('Ctrl Pts',(-20.9165980681484,-48.6790969131764,
123.402843889694)) ;
#64079 = CARTESIAN_POINT('Ctrl Pts',(-20.6151308203117,-48.4991078328135,
123.404625622349)) ;
#64080 = CARTESIAN_POINT('Ctrl Pts',(-20.8924457354999,-48.6890686523789,
123.141945824781)) ;
#64081 = CARTESIAN_POINT('Ctrl Pts',(-20.5958067228006,-48.509079572016,123.195907470545)) ;
#64082 = CARTESIAN_POINT('Ctrl Pts',(-20.8231457686488,-48.6990638601446,
122.888545055584)) ;
#64083 = CARTESIAN_POINT('Ctrl Pts',(-20.5403646013204,-48.5190747797817,
122.993187508509)) ;
#64084 = CARTESIAN_POINT('Ctrl Pts',(-20.71020152793,-48.7090978616136,122.650301300846)) ;
#64085 = CARTESIAN_POINT('Ctrl Pts',(-20.4500071819512,-48.5291087812508,
122.802593499085)) ;
#64086 = CARTESIAN_POINT('Ctrl Pts',(-20.5606310889083,-48.718953219706,122.438836911348)) ;
#64087 = CARTESIAN_POINT('Ctrl Pts',(-20.3303491093556,-48.5389641393431,
122.633423436185)) ;
#64088 = CARTESIAN_POINT('Ctrl Pts',(-20.3742255768515,-48.7289526952993,
122.253690036881)) ;
#64089 = CARTESIAN_POINT('Ctrl Pts',(-20.1812231766611,-48.5489636149364,
122.485307572519)) ;
#64090 = CARTESIAN_POINT('Ctrl Pts',(-20.1608603226581,-48.7388471437944,
122.104999075767)) ;
#64091 = CARTESIAN_POINT('Ctrl Pts',(-20.0105298816174,-48.5588580634315,
122.366356738769)) ;
#64092 = CARTESIAN_POINT('Ctrl Pts',(-19.9209501103882,-48.7489102680221,
121.993860313604)) ;
#64093 = CARTESIAN_POINT('Ctrl Pts',(-19.8186007515957,-48.5689211876593,
122.277447732973)) ;
#64094 = CARTESIAN_POINT('Ctrl Pts',(-19.6710512311322,-48.7587498943507,
121.927273469944)) ;
#64095 = CARTESIAN_POINT('Ctrl Pts',(-19.6186814015643,-48.5787608139879,
122.224180469347)) ;
#64096 = CARTESIAN_POINT('Ctrl Pts',(-19.4076398792598,-48.7688131293937,
121.904256633562)) ;
#64097 = CARTESIAN_POINT('Ctrl Pts',(-19.4079520936183,-48.5888240490308,
122.205769170456)) ;
#64098 = CARTESIAN_POINT('Ctrl Pts',(-19.1486188793919,-48.7787071346277,
121.927163232832)) ;
#64099 = CARTESIAN_POINT('Ctrl Pts',(-19.2007357506879,-48.5987180542649,
122.224096613958)) ;
#64100 = CARTESIAN_POINT('Ctrl Pts',(-18.8961432339119,-48.7886498478435,
121.99432181877)) ;
#64101 = CARTESIAN_POINT('Ctrl Pts',(-18.9987559919676,-48.6086607674806,
122.27782549784)) ;
#64102 = CARTESIAN_POINT('Ctrl Pts',(-18.6575880747036,-48.7986555876417,
122.104972809918)) ;
#64103 = CARTESIAN_POINT('Ctrl Pts',(-18.8079128155078,-48.6186665072788,
122.366348201292)) ;
#64104 = CARTESIAN_POINT('Ctrl Pts',(-18.4417397385889,-48.8086764897881,
122.255816146101)) ;
#64105 = CARTESIAN_POINT('Ctrl Pts',(-18.6352354003947,-48.6286874094252,
122.487024632224)) ;
#64106 = CARTESIAN_POINT('Ctrl Pts',(-18.2575608011542,-48.818567259837,122.439229061463)) ;
#64107 = CARTESIAN_POINT('Ctrl Pts',(-18.4878939926653,-48.6385781794741,
122.633756241431)) ;
#64108 = CARTESIAN_POINT('Ctrl Pts',(-18.106193675921,-48.8285586706167,122.653759103654)) ;
#64109 = CARTESIAN_POINT('Ctrl Pts',(-18.3668020674057,-48.6485695902538,
122.805381400602)) ;
#64110 = CARTESIAN_POINT('Ctrl Pts',(-17.9949337392161,-48.8385070162812,
122.890328842219)) ;
#64111 = CARTESIAN_POINT('Ctrl Pts',(-18.2777961188115,-48.6585179359183,
122.994637890624)) ;
#64112 = CARTESIAN_POINT('Ctrl Pts',(-17.9259246879504,-48.8484518743424,
123.142417551886)) ;
#64113 = CARTESIAN_POINT('Ctrl Pts',(-18.2225909149543,-48.6684627939795,
123.196309167332)) ;
#64114 = CARTESIAN_POINT('Ctrl Pts',(-17.9018586345267,-48.8585067097353,
123.405524737978)) ;
#64115 = CARTESIAN_POINT('Ctrl Pts',(-18.2033401477523,-48.6785176293724,
123.406795195145)) ;
#64116 = CARTESIAN_POINT('Ctrl Pts',(-17.9228907005279,-48.8683290818368,
123.662811089171)) ;
#64117 = CARTESIAN_POINT('Ctrl Pts',(-18.2201677808873,-48.6883400014739,
123.612623483924)) ;
#64118 = CARTESIAN_POINT('Ctrl Pts',(-17.9893599290882,-48.8783849492805,
123.918552606262)) ;
#64119 = CARTESIAN_POINT('Ctrl Pts',(-18.2733451048243,-48.6983958689176,
123.817216284864)) ;
#64120 = CARTESIAN_POINT('Ctrl Pts',(-18.0984022475195,-48.8883256791384,
124.155949320405)) ;
#64121 = CARTESIAN_POINT('Ctrl Pts',(-18.360580702555,-48.7083365987755,124.007132560782)) ;
#64122 = CARTESIAN_POINT('Ctrl Pts',(-18.2457897778608,-48.8982300176895,
124.370478803514)) ;
#64123 = CARTESIAN_POINT('Ctrl Pts',(-18.4784920796112,-48.7182409373267,
124.178754699922)) ;
#64124 = CARTESIAN_POINT('Ctrl Pts',(-18.4309099578703,-48.908276699118,124.558689346407)) ;
#64125 = CARTESIAN_POINT('Ctrl Pts',(-18.6265896773682,-48.7282876187551,
124.329321820861)) ;
#64126 = CARTESIAN_POINT('Ctrl Pts',(-18.6425771224679,-48.9181722065873,
124.709824664085)) ;
#64127 = CARTESIAN_POINT('Ctrl Pts',(-18.7959241464339,-48.7381831262244,
124.450228239053)) ;
#64128 = CARTESIAN_POINT('Ctrl Pts',(-18.8811535876977,-48.9282344750859,
124.823761366572)) ;
#64129 = CARTESIAN_POINT('Ctrl Pts',(-18.986786280884,-48.748245394723,124.541375925979)) ;
#64130 = CARTESIAN_POINT('Ctrl Pts',(-19.1303382919628,-48.9380764653565,
124.893166471091)) ;
#64131 = CARTESIAN_POINT('Ctrl Pts',(-19.18613388542,-48.7580873849936,124.596897991502)) ;
#64132 = CARTESIAN_POINT('Ctrl Pts',(-19.3916192445913,-48.9480698822375,
124.919216288475)) ;
#64133 = CARTESIAN_POINT('Ctrl Pts',(-19.3951586909665,-48.7680808018746,
124.617736026515)) ;
#64134 = CARTESIAN_POINT('Ctrl Pts',(-19.6517180268275,-48.9579943700896,
124.899657271309)) ;
#64135 = CARTESIAN_POINT('Ctrl Pts',(-19.6032371787446,-48.7780052897268,
124.602087041937)) ;
#64136 = CARTESIAN_POINT('Ctrl Pts',(-19.9064040385048,-48.9679940039981,
124.835026142014)) ;
#64137 = CARTESIAN_POINT('Ctrl Pts',(-19.8069854638334,-48.7880049236352,
124.550380450082)) ;
#64138 = CARTESIAN_POINT('Ctrl Pts',(-20.145734566015,-48.9779801142549,124.72728379971)) ;
#64139 = CARTESIAN_POINT('Ctrl Pts',(-19.9984490348426,-48.797991033892,124.464185028181)) ;
#64140 = CARTESIAN_POINT('Ctrl Pts',(-20.363595758635,-48.988016065442,124.578693439179)) ;
#64141 = CARTESIAN_POINT('Ctrl Pts',(-20.1727370240025,-48.8080269850791,
124.345311205248)) ;
#64142 = CARTESIAN_POINT('Ctrl Pts',(-20.5492835774246,-48.9978727037768,
124.398066759077)) ;
#64143 = CARTESIAN_POINT('Ctrl Pts',(-20.321285535719,-48.8178836234139,124.200809123624)) ;
#64144 = CARTESIAN_POINT('Ctrl Pts',(-20.7032232576622,-49.0078716638548,
124.185175408038)) ;
#64145 = CARTESIAN_POINT('Ctrl Pts',(-20.4444358521844,-48.8278825834919,
124.030495143245)) ;
#64146 = CARTESIAN_POINT('Ctrl Pts',(-20.8169628556699,-49.0177668941686,
123.951284538968)) ;
#64147 = CARTESIAN_POINT('Ctrl Pts',(-20.5354258074483,-48.8377778138057,
123.84338226399)) ;
#64148 = CARTESIAN_POINT('Ctrl Pts',(-20.8895070310717,-49.0278274066372,
123.697088016909)) ;
#64149 = CARTESIAN_POINT('Ctrl Pts',(-20.5934596252462,-48.8478383262744,
123.640024411145)) ;
#64150 = CARTESIAN_POINT('Ctrl Pts',(-20.9163903855367,-49.0376766981834,
123.439638200355)) ;
#64151 = CARTESIAN_POINT('Ctrl Pts',(-20.6149646209664,-48.8576876178205,
123.434065220729)) ;
#64152 = CARTESIAN_POINT('Ctrl Pts',(-20.8985020837487,-49.0477038841156,
123.176748817994)) ;
#64153 = CARTESIAN_POINT('Ctrl Pts',(-20.6006524960591,-48.8677148037527,
123.223753784893)) ;
#64154 = CARTESIAN_POINT('Ctrl Pts',(-20.8345541010092,-49.0577324205749,
122.921071960557)) ;
#64155 = CARTESIAN_POINT('Ctrl Pts',(-20.5494925272255,-48.8777433402121,
123.019212637237)) ;
#64156 = CARTESIAN_POINT('Ctrl Pts',(-20.7296054273253,-49.0675776605399,
122.68460614522)) ;
#64157 = CARTESIAN_POINT('Ctrl Pts',(-20.4655325601765,-48.887588580177,122.830041421681)) ;
#64158 = CARTESIAN_POINT('Ctrl Pts',(-20.5836317515741,-49.0775683554631,
122.466374760989)) ;
#64159 = CARTESIAN_POINT('Ctrl Pts',(-20.3487525572943,-48.8975792751002,
122.655457213119)) ;
#64160 = CARTESIAN_POINT('Ctrl Pts',(-20.4007099669352,-49.0876061762217,
122.276320211683)) ;
#64161 = CARTESIAN_POINT('Ctrl Pts',(-20.202413975225,-48.9076170958588,122.503414537184)) ;
#64162 = CARTESIAN_POINT('Ctrl Pts',(-20.1919240683842,-49.0974507699987,
122.123545795109)) ;
#64163 = CARTESIAN_POINT('Ctrl Pts',(-20.0353851785869,-48.9174616896358,
122.381196695483)) ;
#64164 = CARTESIAN_POINT('Ctrl Pts',(-19.9567693977097,-49.1074347653747,
122.00723791885)) ;
#64165 = CARTESIAN_POINT('Ctrl Pts',(-19.8472610587631,-48.9274456850118,
122.288151648235)) ;
#64166 = CARTESIAN_POINT('Ctrl Pts',(-19.705830459049,-49.1173838139361,121.933802445044)) ;
#64167 = CARTESIAN_POINT('Ctrl Pts',(-19.646509912876,-48.9373947335732,122.229404623023)) ;
#64168 = CARTESIAN_POINT('Ctrl Pts',(-19.4445921214419,-49.1273862529106,
121.904618015651)) ;
#64169 = CARTESIAN_POINT('Ctrl Pts',(-19.437519186954,-48.9473971725478,122.206058321962)) ;
#64170 = CARTESIAN_POINT('Ctrl Pts',(-19.1817922313132,-49.137407494207,121.921624060379)) ;
#64171 = CARTESIAN_POINT('Ctrl Pts',(-19.2272793333639,-48.9574184138441,
122.219664472921)) ;
#64172 = CARTESIAN_POINT('Ctrl Pts',(-18.9291459751133,-49.1473001726465,
121.982897915693)) ;
#64173 = CARTESIAN_POINT('Ctrl Pts',(-19.025163319022,-48.9673110922836,122.268684604712)) ;
#64174 = CARTESIAN_POINT('Ctrl Pts',(-18.6884670363836,-49.1572902265941,
122.087747388181)) ;
#64175 = CARTESIAN_POINT('Ctrl Pts',(-18.8326207934705,-48.9773011462313,
122.352565175257)) ;
#64176 = CARTESIAN_POINT('Ctrl Pts',(-18.4704519830292,-49.1672485877426,
122.232485671817)) ;
#64177 = CARTESIAN_POINT('Ctrl Pts',(-18.6582097022475,-48.9872595073797,
122.468356610712)) ;
#64178 = CARTESIAN_POINT('Ctrl Pts',(-18.2815383415692,-49.1771482146274,
122.411369259889)) ;
#64179 = CARTESIAN_POINT('Ctrl Pts',(-18.5070800263305,-48.9971591342646,
122.611463763631)) ;
#64180 = CARTESIAN_POINT('Ctrl Pts',(-18.1243345330828,-49.1871961114308,
122.623486945981)) ;
#64181 = CARTESIAN_POINT('Ctrl Pts',(-18.3813177411218,-49.0072070310679,
122.781158694447)) ;
#64182 = CARTESIAN_POINT('Ctrl Pts',(-18.0079271717103,-49.1970914690668,
122.856062333984)) ;
#64183 = CARTESIAN_POINT('Ctrl Pts',(-18.2881931003449,-49.0171023887039,
122.967218812396)) ;
#64184 = CARTESIAN_POINT('Ctrl Pts',(-17.9324068931307,-49.2071531215235,
123.109426695893)) ;
#64185 = CARTESIAN_POINT('Ctrl Pts',(-18.2277777834536,-49.0271640411606,
123.169910844373)) ;
#64186 = CARTESIAN_POINT('Ctrl Pts',(-17.9026375541845,-49.2169977257954,
123.366423552934)) ;
#64187 = CARTESIAN_POINT('Ctrl Pts',(-18.2039634417627,-49.0370086454325,
123.375507396247)) ;
#64188 = CARTESIAN_POINT('Ctrl Pts',(-17.9171858178237,-49.2269578474934,
123.62775607521)) ;
#64189 = CARTESIAN_POINT('Ctrl Pts',(-18.2156028245757,-49.0469687671305,
123.584573004918)) ;
#64190 = CARTESIAN_POINT('Ctrl Pts',(-17.9778519477484,-49.2369958818559,
123.884464098742)) ;
#64191 = CARTESIAN_POINT('Ctrl Pts',(-18.2641366483863,-49.0570068014931,
123.789939339049)) ;
#64192 = CARTESIAN_POINT('Ctrl Pts',(-18.0800477463435,-49.2468701944424,
124.123014445666)) ;
#64193 = CARTESIAN_POINT('Ctrl Pts',(-18.3458936691752,-49.0668811140795,
123.980778477681)) ;
#64194 = CARTESIAN_POINT('Ctrl Pts',(-18.2248917333607,-49.2569396752251,
124.344424493672)) ;
#64195 = CARTESIAN_POINT('Ctrl Pts',(-18.4617697106575,-49.0769505948622,
124.157906347072)) ;
#64196 = CARTESIAN_POINT('Ctrl Pts',(-18.4016886197062,-49.2667740112422,
124.532954912051)) ;
#64197 = CARTESIAN_POINT('Ctrl Pts',(-18.6032069775405,-49.0867849308793,
124.308729299601)) ;
#64198 = CARTESIAN_POINT('Ctrl Pts',(-18.612254092902,-49.2768069689704,124.691612235755)) ;
#64199 = CARTESIAN_POINT('Ctrl Pts',(-18.7716597901353,-49.0968178886076,
124.435654741883)) ;
#64200 = CARTESIAN_POINT('Ctrl Pts',(-18.8472145112584,-49.2868273675456,
124.810505656813)) ;
#64201 = CARTESIAN_POINT('Ctrl Pts',(-18.9596285027308,-49.1068382871827,
124.530768800945)) ;
#64202 = CARTESIAN_POINT('Ctrl Pts',(-19.0951813191321,-49.2966929413168,
124.886249263445)) ;
#64203 = CARTESIAN_POINT('Ctrl Pts',(-19.158001200267,-49.116703860954,124.59136281955)) ;
#64204 = CARTESIAN_POINT('Ctrl Pts',(-19.3577881565911,-49.3067618159729,
124.918435602837)) ;
#64205 = CARTESIAN_POINT('Ctrl Pts',(-19.3680870720684,-49.12677273561,124.617111322248)) ;
#64206 = CARTESIAN_POINT('Ctrl Pts',(-19.6161749842658,-49.3166072468784,
124.904881658473)) ;
#64207 = CARTESIAN_POINT('Ctrl Pts',(-19.5747953751554,-49.1366181665155,
124.606267622671)) ;
#64208 = CARTESIAN_POINT('Ctrl Pts',(-19.8718870581051,-49.3265868717491,
124.846704436863)) ;
#64209 = CARTESIAN_POINT('Ctrl Pts',(-19.7793647044864,-49.1465977913862,
124.55972551948)) ;
#64210 = CARTESIAN_POINT('Ctrl Pts',(-20.1143655069739,-49.3366055546632,
124.74415269252)) ;
#64211 = CARTESIAN_POINT('Ctrl Pts',(-19.9733472699668,-49.1566164743003,
124.477683643661)) ;
#64212 = CARTESIAN_POINT('Ctrl Pts',(-20.3326993754849,-49.346488819847,124.603431043373)) ;
#64213 = CARTESIAN_POINT('Ctrl Pts',(-20.148013421792,-49.1664997394842,124.365106482365)) ;
#64214 = CARTESIAN_POINT('Ctrl Pts',(-20.5267164375359,-49.3565571139384,
124.423600519391)) ;
#64215 = CARTESIAN_POINT('Ctrl Pts',(-20.3032270348823,-49.1765680335755,
124.221241540364)) ;
#64216 = CARTESIAN_POINT('Ctrl Pts',(-20.6830755384687,-49.3663872441237,
124.217913860219)) ;
#64217 = CARTESIAN_POINT('Ctrl Pts',(-20.4283133065888,-49.1863981637609,
124.056692994351)) ;
#64218 = CARTESIAN_POINT('Ctrl Pts',(-20.8044543031149,-49.3764537923389,
123.982913211132)) ;
#64219 = CARTESIAN_POINT('Ctrl Pts',(-20.5254162463695,-49.196464711976,123.868692079819)) ;
#64220 = CARTESIAN_POINT('Ctrl Pts',(-20.881675014768,-49.3863440410275,123.734710364339)) ;
#64221 = CARTESIAN_POINT('Ctrl Pts',(-20.5871922922867,-49.2063549606646,
123.670130518056)) ;
#64222 = CARTESIAN_POINT('Ctrl Pts',(-20.9155298639726,-49.3963362228035,
123.474333218862)) ;
#64223 = CARTESIAN_POINT('Ctrl Pts',(-20.6142760088709,-49.2163471424406,
123.461828953088)) ;
#64224 = CARTESIAN_POINT('Ctrl Pts',(-20.9034492216854,-49.4062990034313,
123.212805454271)) ;
#64225 = CARTESIAN_POINT('Ctrl Pts',(-20.6046113070106,-49.2263099230684,
123.252607116101)) ;
#64226 = CARTESIAN_POINT('Ctrl Pts',(-20.847109080545,-49.4162034081051,122.958679801309)) ;
#64227 = CARTESIAN_POINT('Ctrl Pts',(-20.5595393178523,-49.2362143277422,
123.04930733304)) ;
#64228 = CARTESIAN_POINT('Ctrl Pts',(-20.7457693980106,-49.4262634025841,
122.714534227944)) ;
#64229 = CARTESIAN_POINT('Ctrl Pts',(-20.4784673873757,-49.2462743222212,
122.853990658576)) ;
#64230 = CARTESIAN_POINT('Ctrl Pts',(-20.6067290420419,-49.4361120245539,
122.496219298933)) ;
#64231 = CARTESIAN_POINT('Ctrl Pts',(-20.3672356811197,-49.256122944191,122.679339680775)) ;
#64232 = CARTESIAN_POINT('Ctrl Pts',(-20.4291275579387,-49.4461424639657,
122.301465539573)) ;
#64233 = CARTESIAN_POINT('Ctrl Pts',(-20.2251545164189,-49.2661533836029,
122.523536525192)) ;
#64234 = CARTESIAN_POINT('Ctrl Pts',(-20.2204806965298,-49.4561521796005,
122.141233524308)) ;
#64235 = CARTESIAN_POINT('Ctrl Pts',(-20.0582370435673,-49.2761630992376,
122.395350947196)) ;
#64236 = CARTESIAN_POINT('Ctrl Pts',(-19.9896519589518,-49.4660629322931,
122.020664911616)) ;
#64237 = CARTESIAN_POINT('Ctrl Pts',(-19.8735747112757,-49.2860738519302,
122.298896350739)) ;
#64238 = CARTESIAN_POINT('Ctrl Pts',(-19.7410945155268,-49.4759922052395,
121.941224683221)) ;
#64239 = CARTESIAN_POINT('Ctrl Pts',(-19.674729389547,-49.2960031248766,122.235344147617)) ;
#64240 = CARTESIAN_POINT('Ctrl Pts',(-19.4795590978915,-49.4860348966322,
121.90597303431)) ;
#64241 = CARTESIAN_POINT('Ctrl Pts',(-19.4655009066754,-49.3060458162693,
122.207142650007)) ;
#64242 = CARTESIAN_POINT('Ctrl Pts',(-19.219942862055,-49.4959214298497,121.916333239462)) ;
#64243 = CARTESIAN_POINT('Ctrl Pts',(-19.2578087796181,-49.3159323494868,
122.215430581112)) ;
#64244 = CARTESIAN_POINT('Ctrl Pts',(-18.9632658837388,-49.5059145747817,
121.971768765229)) ;
#64245 = CARTESIAN_POINT('Ctrl Pts',(-19.0524672904058,-49.3259254944189,
122.259778662686)) ;
#64246 = CARTESIAN_POINT('Ctrl Pts',(-18.7212920167133,-49.5158602556182,
122.070557018529)) ;
#64247 = CARTESIAN_POINT('Ctrl Pts',(-18.8588885297617,-49.3358711752553,
122.338808821512)) ;
#64248 = CARTESIAN_POINT('Ctrl Pts',(-18.499816284014,-49.5258075127667,122.209435357243)) ;
#64249 = CARTESIAN_POINT('Ctrl Pts',(-18.6817081096544,-49.3458184324039,
122.449910892272)) ;
#64250 = CARTESIAN_POINT('Ctrl Pts',(-18.3040709556974,-49.5358554166387,
122.386637839566)) ;
#64251 = CARTESIAN_POINT('Ctrl Pts',(-18.5251114670603,-49.3558663362759,
122.591672756877)) ;
#64252 = CARTESIAN_POINT('Ctrl Pts',(-18.1451172426182,-49.5457031157367,
122.590856449756)) ;
#64253 = CARTESIAN_POINT('Ctrl Pts',(-18.3979488685203,-49.3657140353738,
122.755046516047)) ;
#64254 = CARTESIAN_POINT('Ctrl Pts',(-18.0219137176075,-49.5556646067154,
122.821817640682)) ;
#64255 = CARTESIAN_POINT('Ctrl Pts',(-18.2993856846161,-49.3756755263525,
122.939814861468)) ;
#64256 = CARTESIAN_POINT('Ctrl Pts',(-17.940459021946,-49.5656940691293,123.072489705636)) ;
#64257 = CARTESIAN_POINT('Ctrl Pts',(-18.2342214104261,-49.3857049887665,
123.140352429838)) ;
#64258 = CARTESIAN_POINT('Ctrl Pts',(-17.9040753303837,-49.5756013002292,
123.330287135663)) ;
#64259 = CARTESIAN_POINT('Ctrl Pts',(-18.2051140105785,-49.3956122198664,
123.346589589261)) ;
#64260 = CARTESIAN_POINT('Ctrl Pts',(-17.9125098782815,-49.5855476789066,
123.591516015328)) ;
#64261 = CARTESIAN_POINT('Ctrl Pts',(-18.2118609481446,-49.4055585985438,
123.555572243342)) ;
#64262 = CARTESIAN_POINT('Ctrl Pts',(-17.9664056109614,-49.5955524477155,
123.848870528812)) ;
#64263 = CARTESIAN_POINT('Ctrl Pts',(-18.2549768267066,-49.4155633673526,
123.761455926636)) ;
#64264 = CARTESIAN_POINT('Ctrl Pts',(-18.0645967713653,-49.6055735687357,
124.09321890463)) ;
#64265 = CARTESIAN_POINT('Ctrl Pts',(-18.3335291813953,-49.4255844883728,
123.95693488968)) ;
#64266 = CARTESIAN_POINT('Ctrl Pts',(-18.201669169235,-49.6154644345883,124.314070124033)) ;
#64267 = CARTESIAN_POINT('Ctrl Pts',(-18.4431860779359,-49.4354753542255,
124.133615557219)) ;
#64268 = CARTESIAN_POINT('Ctrl Pts',(-18.3764527037186,-49.6254552433476,
124.509963682935)) ;
#64269 = CARTESIAN_POINT('Ctrl Pts',(-18.5830121977067,-49.4454661629847,
124.290330807483)) ;
#64270 = CARTESIAN_POINT('Ctrl Pts',(-18.5818191091062,-49.6354059015279,
124.671858407225)) ;
#64271 = CARTESIAN_POINT('Ctrl Pts',(-18.747304497956,-49.4554168211651,124.41984693504)) ;
#64272 = CARTESIAN_POINT('Ctrl Pts',(-18.8116465771157,-49.64534211117,124.795748611683)) ;
#64273 = CARTESIAN_POINT('Ctrl Pts',(-18.9311656103158,-49.4653530308072,
124.518959622352)) ;
#64274 = CARTESIAN_POINT('Ctrl Pts',(-19.0606091019556,-49.6553252778949,
124.878578886078)) ;
#64275 = CARTESIAN_POINT('Ctrl Pts',(-19.1303351363198,-49.475336197532,124.585224676569)) ;
#64276 = CARTESIAN_POINT('Ctrl Pts',(-19.3217571085356,-49.6653690751052,
124.916663479526)) ;
#64277 = CARTESIAN_POINT('Ctrl Pts',(-19.3392535710715,-49.4853799947423,
124.615693198187)) ;
#64278 = CARTESIAN_POINT('Ctrl Pts',(-19.5799756953038,-49.6751972912734,
124.909602892924)) ;
#64279 = CARTESIAN_POINT('Ctrl Pts',(-19.5458273138333,-49.4952082109106,
124.610045737877)) ;
#64280 = CARTESIAN_POINT('Ctrl Pts',(-19.8393726054235,-49.6852738587427,
124.85664781919)) ;
#64281 = CARTESIAN_POINT('Ctrl Pts',(-19.7533453820382,-49.5052847783798,
124.567682597387)) ;
#64282 = CARTESIAN_POINT('Ctrl Pts',(-20.0802989166778,-49.6951259444321,
124.761703259049)) ;
#64283 = CARTESIAN_POINT('Ctrl Pts',(-19.9460858927394,-49.5151368640692,
124.491728274294)) ;
#64284 = CARTESIAN_POINT('Ctrl Pts',(-20.3060674976311,-49.7051992118375,
124.623574721995)) ;
#64285 = CARTESIAN_POINT('Ctrl Pts',(-20.1267015988155,-49.5252101314746,
124.381226205106)) ;
#64286 = CARTESIAN_POINT('Ctrl Pts',(-20.4998566127892,-49.7150406282611,
124.452283158232)) ;
#64287 = CARTESIAN_POINT('Ctrl Pts',(-20.2817328184751,-49.5350515478982,
124.244194445969)) ;
#64288 = CARTESIAN_POINT('Ctrl Pts',(-20.6636690759953,-49.7250018864038,
124.248115309277)) ;
#64289 = CARTESIAN_POINT('Ctrl Pts',(-20.412783592269,-49.545012806041,124.080861225897)) ;
#64290 = CARTESIAN_POINT('Ctrl Pts',(-20.7900512077694,-49.7350385628358,
124.016618869433)) ;
#64291 = CARTESIAN_POINT('Ctrl Pts',(-20.5138903779245,-49.5550494824729,
123.895664546268)) ;
#64292 = CARTESIAN_POINT('Ctrl Pts',(-20.8734168716423,-49.7449171706996,
123.770739635616)) ;
#64293 = CARTESIAN_POINT('Ctrl Pts',(-20.5805838585332,-49.5649280903367,
123.698962322209)) ;
#64294 = CARTESIAN_POINT('Ctrl Pts',(-20.9135969834897,-49.7549773993384,
123.509473505377)) ;
#64295 = CARTESIAN_POINT('Ctrl Pts',(-20.6127292533526,-49.5749883189755,
123.489949387837)) ;
#64296 = CARTESIAN_POINT('Ctrl Pts',(-20.9079881465136,-49.7648443834992,
123.250206599961)) ;
#64297 = CARTESIAN_POINT('Ctrl Pts',(-20.6082434986379,-49.5848553031363,
123.282536664813)) ;
#64298 = CARTESIAN_POINT('Ctrl Pts',(-20.8572486896229,-49.7748499497519,
122.992248525013)) ;
#64299 = CARTESIAN_POINT('Ctrl Pts',(-20.5676533267145,-49.594860869389,123.076169999909)) ;
#64300 = CARTESIAN_POINT('Ctrl Pts',(-20.762604793769,-49.7848337381665,122.747500893272)) ;
#64301 = CARTESIAN_POINT('Ctrl Pts',(-20.4919395690296,-49.6048446578036,
122.88037156088)) ;
#64302 = CARTESIAN_POINT('Ctrl Pts',(-20.6258474889343,-49.7948795949691,
122.521714953431)) ;
#64303 = CARTESIAN_POINT('Ctrl Pts',(-20.3825347960662,-49.6148905146063,
122.699742010315)) ;
#64304 = CARTESIAN_POINT('Ctrl Pts',(-20.4560100049214,-49.8047054721851,
122.327215170071)) ;
#64305 = CARTESIAN_POINT('Ctrl Pts',(-20.246666541654,-49.6247163918222,122.544142037423)) ;
#64306 = CARTESIAN_POINT('Ctrl Pts',(-20.2521537953988,-49.8146959480264,
122.161777820883)) ;
#64307 = CARTESIAN_POINT('Ctrl Pts',(-20.0835826717048,-49.6347068676635,
122.411791024612)) ;
#64308 = CARTESIAN_POINT('Ctrl Pts',(-20.0211126978458,-49.8247395239252,
122.03417835331)) ;
#64309 = CARTESIAN_POINT('Ctrl Pts',(-19.8987503848234,-49.6447504435623,
122.30971013817)) ;
#64310 = CARTESIAN_POINT('Ctrl Pts',(-19.7771162248852,-49.8345613162232,
121.950011278901)) ;
#64311 = CARTESIAN_POINT('Ctrl Pts',(-19.7035546511395,-49.6545722358604,
122.242375346219)) ;
#64312 = CARTESIAN_POINT('Ctrl Pts',(-19.5167805110166,-49.8445962818491,
121.907971037279)) ;
#64313 = CARTESIAN_POINT('Ctrl Pts',(-19.4952862619387,-49.6646072014862,
122.208741497832)) ;
#64314 = CARTESIAN_POINT('Ctrl Pts',(-19.25336832143,-49.8546211987822,121.912502122807)) ;
#64315 = CARTESIAN_POINT('Ctrl Pts',(-19.2845564644904,-49.6746321184193,
122.212364842142)) ;
#64316 = CARTESIAN_POINT('Ctrl Pts',(-18.9991000929311,-49.8644731371583,
121.961278882292)) ;
#64317 = CARTESIAN_POINT('Ctrl Pts',(-19.0811423664437,-49.6844840567954,
122.251384496068)) ;
#64318 = CARTESIAN_POINT('Ctrl Pts',(-18.7536426685323,-49.8744641131831,
122.054376600934)) ;
#64319 = CARTESIAN_POINT('Ctrl Pts',(-18.8847759503893,-49.6944750328202,
122.325861028897)) ;
#64320 = CARTESIAN_POINT('Ctrl Pts',(-18.5295831349131,-49.8843819339867,
122.187580190448)) ;
#64321 = CARTESIAN_POINT('Ctrl Pts',(-18.7055278321113,-49.7043928536238,
122.432422178777)) ;
#64322 = CARTESIAN_POINT('Ctrl Pts',(-18.3298664401693,-49.8944106545513,
122.359492881508)) ;
#64323 = CARTESIAN_POINT('Ctrl Pts',(-18.5457533183806,-49.7144215741884,
122.569951033302)) ;
#64324 = CARTESIAN_POINT('Ctrl Pts',(-18.1652873217021,-49.9042935811605,
122.56043375668)) ;
#64325 = CARTESIAN_POINT('Ctrl Pts',(-18.4140890357409,-49.7243045007976,
122.730702147218)) ;
#64326 = CARTESIAN_POINT('Ctrl Pts',(-18.0361983461571,-49.91429786628,122.789426912467)) ;
#64327 = CARTESIAN_POINT('Ctrl Pts',(-18.3108162891678,-49.7343087859171,
122.913895707216)) ;
#64328 = CARTESIAN_POINT('Ctrl Pts',(-17.949014297203,-49.9242815474878,123.036925185848)) ;
#64329 = CARTESIAN_POINT('Ctrl Pts',(-18.2410673737591,-49.7442924671249,
123.111893582383)) ;
#64330 = CARTESIAN_POINT('Ctrl Pts',(-17.9061915789435,-49.9343225462177,
123.297274155865)) ;
#64331 = CARTESIAN_POINT('Ctrl Pts',(-18.2068074268591,-49.7543334658549,
123.32017254399)) ;
#64332 = CARTESIAN_POINT('Ctrl Pts',(-17.9087977233851,-49.9441549910849,
123.555650792521)) ;
#64333 = CARTESIAN_POINT('Ctrl Pts',(-18.2088904958492,-49.764165910722,123.526873108748)) ;
#64334 = CARTESIAN_POINT('Ctrl Pts',(-17.9562480238635,-49.9541499895152,
123.81397987155)) ;
#64335 = CARTESIAN_POINT('Ctrl Pts',(-18.2468487951362,-49.7741609091523,
123.733536626353)) ;
#64336 = CARTESIAN_POINT('Ctrl Pts',(-18.0487030674048,-49.9641815382648,
124.060868717992)) ;
#64337 = CARTESIAN_POINT('Ctrl Pts',(-18.3208110873252,-49.7841924579019,
123.93104838714)) ;
#64338 = CARTESIAN_POINT('Ctrl Pts',(-18.1801084382992,-49.9740469165703,
124.284334653721)) ;
#64339 = CARTESIAN_POINT('Ctrl Pts',(-18.4259334333969,-49.7940578362074,
124.109821606921)) ;
#64340 = CARTESIAN_POINT('Ctrl Pts',(-18.3494144439518,-49.9840087640306,
124.484014610873)) ;
#64341 = CARTESIAN_POINT('Ctrl Pts',(-18.56137656749,-49.8040196836677,124.269566724914)) ;
#64342 = CARTESIAN_POINT('Ctrl Pts',(-18.5525546909306,-49.9940437048448,
124.652146083478)) ;
#64343 = CARTESIAN_POINT('Ctrl Pts',(-18.7238875347409,-49.814054624482,124.404073431929)) ;
#64344 = CARTESIAN_POINT('Ctrl Pts',(-18.7782043027359,-50.003928665862,124.780909685819)) ;
#64345 = CARTESIAN_POINT('Ctrl Pts',(-18.9044058329455,-49.8239395854991,
124.507085842024)) ;
#64346 = CARTESIAN_POINT('Ctrl Pts',(-19.0271970940224,-50.0139942747808,
124.870056934491)) ;
#64347 = CARTESIAN_POINT('Ctrl Pts',(-19.1035994992475,-49.8340051944179,
124.578405575516)) ;
#64348 = CARTESIAN_POINT('Ctrl Pts',(-19.2820603187455,-50.0238334498225,
124.913884244235)) ;
#64349 = CARTESIAN_POINT('Ctrl Pts',(-19.3074891770789,-49.8438443694597,
124.613469338266)) ;
#64350 = CARTESIAN_POINT('Ctrl Pts',(-19.5464617510403,-50.0338960053224,
124.913133557086)) ;
#64351 = CARTESIAN_POINT('Ctrl Pts',(-19.5190104339783,-49.8539069249596,
124.61287087145)) ;
#64352 = CARTESIAN_POINT('Ctrl Pts',(-19.8024340996347,-50.0437931800154,
124.866966630769)) ;
#64353 = CARTESIAN_POINT('Ctrl Pts',(-19.7237883101448,-49.8638040996525,
124.575939415286)) ;
#64354 = CARTESIAN_POINT('Ctrl Pts',(-20.0476128622874,-50.0537238949387,
124.777581121014)) ;
#64355 = CARTESIAN_POINT('Ctrl Pts',(-19.9199318279951,-49.8737348145758,
124.504433101703)) ;
#64356 = CARTESIAN_POINT('Ctrl Pts',(-20.2759720546877,-50.0637679230163,
124.645229703549)) ;
#64357 = CARTESIAN_POINT('Ctrl Pts',(-20.1026202614428,-49.8837788426534,
124.398553782836)) ;
#64358 = CARTESIAN_POINT('Ctrl Pts',(-20.4748580560086,-50.0736541248696,
124.478049522978)) ;
#64359 = CARTESIAN_POINT('Ctrl Pts',(-20.2617301731961,-49.8936650445067,
124.264811487387)) ;
#64360 = CARTESIAN_POINT('Ctrl Pts',(-20.6437749690615,-50.0836472913365,
124.277011182732)) ;
#64361 = CARTESIAN_POINT('Ctrl Pts',(-20.396865308046,-49.9036582109736,124.103982270604)) ;
#64362 = CARTESIAN_POINT('Ctrl Pts',(-20.7746102355523,-50.0935867623236,
124.050904663364)) ;
#64363 = CARTESIAN_POINT('Ctrl Pts',(-20.5015353032639,-49.9135976819608,
123.92309830424)) ;
#64364 = CARTESIAN_POINT('Ctrl Pts',(-20.8649209945911,-50.1036032766778,
123.803687664981)) ;
#64365 = CARTESIAN_POINT('Ctrl Pts',(-20.5737859376745,-49.9236141963149,
123.725325490292)) ;
#64366 = CARTESIAN_POINT('Ctrl Pts',(-20.9107662307901,-50.1135333031546,
123.546758707773)) ;
#64367 = CARTESIAN_POINT('Ctrl Pts',(-20.610464245172,-49.9335442227918,123.519782903442)) ;
#64368 = CARTESIAN_POINT('Ctrl Pts',(-20.9111940114087,-50.1235858386641,
123.282611468914)) ;
#64369 = CARTESIAN_POINT('Ctrl Pts',(-20.6108086511653,-49.9435967583012,
123.308465098402)) ;
#64370 = CARTESIAN_POINT('Ctrl Pts',(-20.8668229607071,-50.1334322418838,
123.02768188537)) ;
#64371 = CARTESIAN_POINT('Ctrl Pts',(-20.5753140241265,-49.9534431615209,
123.104521371413)) ;
#64372 = CARTESIAN_POINT('Ctrl Pts',(-20.7786326898469,-50.1433942847378,
122.781207115451)) ;
#64373 = CARTESIAN_POINT('Ctrl Pts',(-20.5047639491462,-49.963405204375,122.907340893886)) ;
#64374 = CARTESIAN_POINT('Ctrl Pts',(-20.6478070135381,-50.1534228355285,
122.552412487854)) ;
#64375 = CARTESIAN_POINT('Ctrl Pts',(-20.400105350936,-49.9734337551656,122.724304121501)) ;
#64376 = CARTESIAN_POINT('Ctrl Pts',(-20.4813154002532,-50.1633331612461,
122.352163354463)) ;
#64377 = CARTESIAN_POINT('Ctrl Pts',(-20.2669138792127,-49.9833440808833,
122.564103520818)) ;
#64378 = CARTESIAN_POINT('Ctrl Pts',(-20.2825162867384,-50.1732680730757,
122.182913771946)) ;
#64379 = CARTESIAN_POINT('Ctrl Pts',(-20.107876126385,-49.9932789927128,122.42870221035)) ;
#64380 = CARTESIAN_POINT('Ctrl Pts',(-20.0548359115821,-50.1833090798438,
122.049558725394)) ;
#64381 = CARTESIAN_POINT('Ctrl Pts',(-19.9257329909012,-50.0033199994809,
122.322016258521)) ;
#64382 = CARTESIAN_POINT('Ctrl Pts',(-19.8112788264307,-50.193196712676,121.958995011386)) ;
#64383 = CARTESIAN_POINT('Ctrl Pts',(-19.7308882259912,-50.0132076323131,
122.249563225972)) ;
#64384 = CARTESIAN_POINT('Ctrl Pts',(-19.5531495649687,-50.203187143774,121.911155500967)) ;
#64385 = CARTESIAN_POINT('Ctrl Pts',(-19.5243852785124,-50.0231980634112,
122.211289414015)) ;
#64386 = CARTESIAN_POINT('Ctrl Pts',(-19.2915318676096,-50.2131425803313,
121.909011127631)) ;
#64387 = CARTESIAN_POINT('Ctrl Pts',(-19.3150912261265,-50.0331534999684,
122.209571651062)) ;
#64388 = CARTESIAN_POINT('Ctrl Pts',(-19.0346123538421,-50.2230535284306,
121.951656547324)) ;
#64389 = CARTESIAN_POINT('Ctrl Pts',(-19.1095552462161,-50.0430644480677,
122.243685801554)) ;
#64390 = CARTESIAN_POINT('Ctrl Pts',(-18.7863546985664,-50.2330656045283,
122.038872975967)) ;
#64391 = CARTESIAN_POINT('Ctrl Pts',(-18.9109485915979,-50.0530765241654,
122.31345662738)) ;
#64392 = CARTESIAN_POINT('Ctrl Pts',(-18.5569655230889,-50.2430929266033,
122.168505406507)) ;
#64393 = CARTESIAN_POINT('Ctrl Pts',(-18.727435583092,-50.0631038462404,122.417161230504)) ;
#64394 = CARTESIAN_POINT('Ctrl Pts',(-18.3565173091822,-50.2529517015574,
122.332725267675)) ;
#64395 = CARTESIAN_POINT('Ctrl Pts',(-18.5670778973102,-50.0729626211945,
122.548532925854)) ;
#64396 = CARTESIAN_POINT('Ctrl Pts',(-18.126853897068,-50.2663778943698,122.600443072369)) ;
#64397 = CARTESIAN_POINT('Ctrl Pts',(-18.3833334664102,-50.086388814007,122.762717346392)) ;
#64398 = CARTESIAN_POINT('Ctrl Pts',(-17.975652168747,-50.2794619101513,122.913754436189)) ;
#64399 = CARTESIAN_POINT('Ctrl Pts',(-18.2623681321715,-50.0994728297884,
123.013391525604)) ;
#64400 = CARTESIAN_POINT('Ctrl Pts',(-17.909201931477,-50.2929353589065,123.261460162963)) ;
#64401 = CARTESIAN_POINT('Ctrl Pts',(-18.2092179634923,-50.1129462785436,
123.291511896051)) ;
#64402 = CARTESIAN_POINT('Ctrl Pts',(-17.9058612706939,-50.3027683167123,
123.519872041659)) ;
#64403 = CARTESIAN_POINT('Ctrl Pts',(-18.2065406001334,-50.1227792363495,
123.498250245797)) ;
#64404 = CARTESIAN_POINT('Ctrl Pts',(-17.9468858271895,-50.312731590163,123.778444889116)) ;
#64405 = CARTESIAN_POINT('Ctrl Pts',(-18.2393587805037,-50.1327425098001,
123.705106558061)) ;
#64406 = CARTESIAN_POINT('Ctrl Pts',(-18.0333597051189,-50.322768663981,124.027627149675)) ;
#64407 = CARTESIAN_POINT('Ctrl Pts',(-18.3085355866663,-50.1427795836181,
123.904453627933)) ;
#64408 = CARTESIAN_POINT('Ctrl Pts',(-18.1593001786209,-50.3326436669926,
124.254558222492)) ;
#64409 = CARTESIAN_POINT('Ctrl Pts',(-18.409286108333,-50.1526545866297,124.085999460383)) ;
#64410 = CARTESIAN_POINT('Ctrl Pts',(-18.3258841681713,-50.3427113466188,
124.460049111905)) ;
#64411 = CARTESIAN_POINT('Ctrl Pts',(-18.5425518166163,-50.1627222662559,
124.250393776869)) ;
#64412 = CARTESIAN_POINT('Ctrl Pts',(-18.5210703743217,-50.3525521968365,
124.629743114865)) ;
#64413 = CARTESIAN_POINT('Ctrl Pts',(-18.6986983036897,-50.1725631164736,
124.386149592484)) ;
#64414 = CARTESIAN_POINT('Ctrl Pts',(-18.8210606852671,-50.3658883953125,
124.810877501075)) ;
#64415 = CARTESIAN_POINT('Ctrl Pts',(-18.9386954921332,-50.1858993149496,
124.531065583499)) ;
#64416 = CARTESIAN_POINT('Ctrl Pts',(-19.1585310682997,-50.3791059191269,
124.908576997203)) ;
#64417 = CARTESIAN_POINT('Ctrl Pts',(-19.2087060042156,-50.199116838764,124.609228123008)) ;
#64418 = CARTESIAN_POINT('Ctrl Pts',(-19.5088595130066,-50.3924408456182,
124.916046147867)) ;
#64419 = CARTESIAN_POINT('Ctrl Pts',(-19.4889209379206,-50.2124517652553,
124.615199985815)) ;
#64420 = CARTESIAN_POINT('Ctrl Pts',(-19.7681867122454,-50.4024239462128,
124.876091752188)) ;
#64421 = CARTESIAN_POINT('Ctrl Pts',(-19.696392649381,-50.2224348658499,124.583239677521)) ;
#64422 = CARTESIAN_POINT('Ctrl Pts',(-20.0179829922131,-50.4124687221124,
124.790847910221)) ;
#64423 = CARTESIAN_POINT('Ctrl Pts',(-19.896227454566,-50.2324796417495,124.515046638421)) ;
#64424 = CARTESIAN_POINT('Ctrl Pts',(-20.2442444733831,-50.4222866452983,
124.666833014598)) ;
#64425 = CARTESIAN_POINT('Ctrl Pts',(-20.0772393601815,-50.2422975649354,
124.415835165722)) ;
#64426 = CARTESIAN_POINT('Ctrl Pts',(-20.4505999318951,-50.4323359592536,
124.502045800867)) ;
#64427 = CARTESIAN_POINT('Ctrl Pts',(-20.2423227107125,-50.2523468788908,
124.284011299718)) ;
#64428 = CARTESIAN_POINT('Ctrl Pts',(-20.6812147142531,-50.4456396998762,
124.239319481561)) ;
#64429 = CARTESIAN_POINT('Ctrl Pts',(-20.4268261522775,-50.2656506195133,
124.073810794489)) ;
#64430 = CARTESIAN_POINT('Ctrl Pts',(-20.8766371020504,-50.4621298953529,
123.846918741757)) ;
#64431 = CARTESIAN_POINT('Ctrl Pts',(-20.5831565547659,-50.28214081499,123.759929216494)) ;
#64432 = CARTESIAN_POINT('Ctrl Pts',(-20.9269267933237,-50.4788490602775,
123.405534034858)) ;
#64433 = CARTESIAN_POINT('Ctrl Pts',(-20.6233943759952,-50.2988599799146,
123.406758446571)) ;
#64434 = CARTESIAN_POINT('Ctrl Pts',(-20.8757804021482,-50.4920100539476,
123.063406602128)) ;
#64435 = CARTESIAN_POINT('Ctrl Pts',(-20.5824794341171,-50.3120209735847,
123.13310677555)) ;
#64436 = CARTESIAN_POINT('Ctrl Pts',(-20.7933286314175,-50.5020062760529,
122.814013822185)) ;
#64437 = CARTESIAN_POINT('Ctrl Pts',(-20.5165192334636,-50.32201719569,122.933581356952)) ;
#64438 = CARTESIAN_POINT('Ctrl Pts',(-20.66794702487,-50.5120301155866,122.58234791319)) ;
#64439 = CARTESIAN_POINT('Ctrl Pts',(-20.4162173324879,-50.3320410352238,
122.748251908727)) ;
#64440 = CARTESIAN_POINT('Ctrl Pts',(-20.4530703195707,-50.5252234375799,
122.310222407941)) ;
#64441 = CARTESIAN_POINT('Ctrl Pts',(-20.2443087067898,-50.345234357217,122.530542413722)) ;
#64442 = CARTESIAN_POINT('Ctrl Pts',(-20.0984605249334,-50.5418826093572,
122.04515035663)) ;
#64443 = CARTESIAN_POINT('Ctrl Pts',(-19.9606321286751,-50.3618935289943,
122.318489942363)) ;
#64444 = CARTESIAN_POINT('Ctrl Pts',(-19.5917715291836,-50.5617927848429,
121.89245685484)) ;
#64445 = CARTESIAN_POINT('Ctrl Pts',(-19.5552782569538,-50.38180370448,122.196329454903)) ;
#64446 = CARTESIAN_POINT('Ctrl Pts',(-19.0638261203489,-50.5816827726873,
121.920703930916)) ;
#64447 = CARTESIAN_POINT('Ctrl Pts',(-19.132921841017,-50.4016936923244,122.218924915738)) ;
#64448 = CARTESIAN_POINT('Ctrl Pts',(-18.5747132438789,-50.6016882207021,
122.12899945876)) ;
#64449 = CARTESIAN_POINT('Ctrl Pts',(-18.7416302351988,-50.4216991403392,
122.385558456999)) ;
#64450 = CARTESIAN_POINT('Ctrl Pts',(-18.1887817456848,-50.6215246147294,
122.488396023025)) ;
#64451 = CARTESIAN_POINT('Ctrl Pts',(-18.4328823682395,-50.4415355343665,
122.673074725378)) ;
#64452 = CARTESIAN_POINT('Ctrl Pts',(-17.9465286197536,-50.6415324086261,
122.961624501261)) ;
#64453 = CARTESIAN_POINT('Ctrl Pts',(-18.2390777138567,-50.4615433282632,
123.051656336489)) ;
#64454 = CARTESIAN_POINT('Ctrl Pts',(-17.880692353325,-50.66135904492,123.484550765059)) ;
#64455 = CARTESIAN_POINT('Ctrl Pts',(-18.1864063185633,-50.4813699645572,
123.469998611925)) ;
#64456 = CARTESIAN_POINT('Ctrl Pts',(-17.9971845806245,-50.6813379878739,
124.002602226816)) ;
#64457 = CARTESIAN_POINT('Ctrl Pts',(-18.2795984569262,-50.501348907511,123.884440399758)) ;
#64458 = CARTESIAN_POINT('Ctrl Pts',(-18.2835587250181,-50.701269789743,124.448196582327)) ;
#64459 = CARTESIAN_POINT('Ctrl Pts',(-18.5086966003631,-50.5212807093801,
124.240917422711)) ;
#64460 = CARTESIAN_POINT('Ctrl Pts',(-18.7016353948024,-50.7210940902405,
124.769140330186)) ;
#64461 = CARTESIAN_POINT('Ctrl Pts',(-18.843158485295,-50.5411050098776,124.497674650865)) ;
#64462 = CARTESIAN_POINT('Ctrl Pts',(-19.2109425558882,-50.7411900915803,
124.929317666213)) ;
#64463 = CARTESIAN_POINT('Ctrl Pts',(-19.2506040110265,-50.5612010112175,
124.625816398005)) ;
#64464 = CARTESIAN_POINT('Ctrl Pts',(-19.7359254653028,-50.7609485076843,
124.90700825648)) ;
#64465 = CARTESIAN_POINT('Ctrl Pts',(-19.6705889099247,-50.5809594273214,
124.607973339329)) ;
#64466 = CARTESIAN_POINT('Ctrl Pts',(-20.2295077365795,-50.7810422005684,
124.703903011743)) ;
#64467 = CARTESIAN_POINT('Ctrl Pts',(-20.0654722041603,-50.6010531202055,
124.445475287471)) ;
#64468 = CARTESIAN_POINT('Ctrl Pts',(-20.4872438678407,-50.7941531664751,
124.469055541275)) ;
#64469 = CARTESIAN_POINT('Ctrl Pts',(-20.2716279488377,-50.6141640861122,
124.257625239002)) ;
#64470 = CARTESIAN_POINT('Ctrl Pts',(-20.5950497967257,-50.8008665412629,
124.330315451401)) ;
#64471 = CARTESIAN_POINT('Ctrl Pts',(-20.357892637621,-50.6208774609001,124.146615798218)) ;
#64472 = CARTESIAN_POINT('',(-18.1577260363418,-12.,123.523171848835)) ;
#64473 = CARTESIAN_POINT('Ctrl Pts',(-17.9274924084134,-12.1498929727495,
123.644402320537)) ;
#64474 = CARTESIAN_POINT('Ctrl Pts',(-17.9447322736189,-12.1380608032114,
123.631287153522)) ;
#64475 = CARTESIAN_POINT('Ctrl Pts',(-17.9630111136594,-12.1257315979358,
123.61865820345)) ;
#64476 = CARTESIAN_POINT('Ctrl Pts',(-17.9820336742706,-12.1130842288466,
123.606705870659)) ;
#64477 = CARTESIAN_POINT('Ctrl Pts',(-18.0012480997282,-12.1003092961987,
123.594632984565)) ;
#64478 = CARTESIAN_POINT('Ctrl Pts',(-18.0212209537106,-12.0872097491302,
123.583250489011)) ;
#64479 = CARTESIAN_POINT('Ctrl Pts',(-18.0416342610097,-12.073969917745,123.572702334622)) ;
#64480 = CARTESIAN_POINT('Ctrl Pts',(-18.0628845294966,-12.0601872431625,
123.561721697849)) ;
#64481 = CARTESIAN_POINT('Ctrl Pts',(-18.0846116965369,-12.046252544725,123.551645261562)) ;
#64482 = CARTESIAN_POINT('Ctrl Pts',(-18.1064482931762,-12.0323737605024,
123.542577794954)) ;
#64483 = CARTESIAN_POINT('Ctrl Pts',(-18.1235331135845,-12.0215150841324,
123.535483464225)) ;
#64484 = CARTESIAN_POINT('Ctrl Pts',(-18.1406846749009,-12.0106906348965,
123.52900545476)) ;
#64485 = CARTESIAN_POINT('Ctrl Pts',(-18.1577260360659,-11.9999999999988,
123.52317184888)) ;
#64486 = CARTESIAN_POINT('Ctrl Pts',(-18.1577260360659,-11.9999999999988,
123.52317184888)) ;
#64487 = CARTESIAN_POINT('Ctrl Pts',(-18.1523700395754,-11.9999999999989,
123.490912584228)) ;
#64488 = CARTESIAN_POINT('Ctrl Pts',(-18.1482641940248,-12.,123.458366720246)) ;
#64489 = CARTESIAN_POINT('Ctrl Pts',(-18.1454318173621,-12.,123.425634822543)) ;
#64490 = CARTESIAN_POINT('Ctrl Pts',(-18.1391124983055,-12.,123.352606645309)) ;
#64491 = CARTESIAN_POINT('Ctrl Pts',(-18.139130762036,-12.,123.278629626742)) ;
#64492 = CARTESIAN_POINT('Ctrl Pts',(-18.1456716811646,-12.,123.204576506712)) ;
#64493 = CARTESIAN_POINT('Ctrl Pts',(-18.1517101445967,-12.,123.136211946846)) ;
#64494 = CARTESIAN_POINT('Ctrl Pts',(-18.1633098563508,-11.9999999994,123.067757580192)) ;
#64495 = CARTESIAN_POINT('Ctrl Pts',(-18.180582178177,-11.9999999999304,123.000096158631)) ;
#64496 = CARTESIAN_POINT('Ctrl Pts',(-18.1819709423,-11.9999999999731,122.994655908286)) ;
#64497 = CARTESIAN_POINT('Ctrl Pts',(-18.1833963771835,-12.,122.989220812084)) ;
#64498 = CARTESIAN_POINT('Ctrl Pts',(-18.1848585399242,-12.,122.983791343577)) ;
#64499 = CARTESIAN_POINT('Ctrl Pts',(-18.2003846048102,-12.,122.926138198693)) ;
#64500 = CARTESIAN_POINT('Ctrl Pts',(-18.2200467363594,-12.0000000052168,
122.869141588207)) ;
#64501 = CARTESIAN_POINT('Ctrl Pts',(-18.2435971844896,-12.0000000018168,
122.813603051952)) ;
#64502 = CARTESIAN_POINT('Ctrl Pts',(-18.2497774297557,-12.0000000009246,
122.799028306967)) ;
#64503 = CARTESIAN_POINT('Ctrl Pts',(-18.2562253303416,-12.,122.784554225748)) ;
#64504 = CARTESIAN_POINT('Ctrl Pts',(-18.2629361382999,-12.,122.770195825027)) ;
#64505 = CARTESIAN_POINT('Ctrl Pts',(-18.2951446697432,-12.,122.701282662267)) ;
#64506 = CARTESIAN_POINT('Ctrl Pts',(-18.3334226087301,-12.,122.635003694009)) ;
#64507 = CARTESIAN_POINT('Ctrl Pts',(-18.3779347229611,-12.,122.57166047214)) ;
#64508 = CARTESIAN_POINT('Ctrl Pts',(-18.4098344464478,-12.,122.526265385942)) ;
#64509 = CARTESIAN_POINT('Ctrl Pts',(-18.4449399291145,-12.0000000149114,
122.482373487453)) ;
#64510 = CARTESIAN_POINT('Ctrl Pts',(-18.482822642223,-12.0000000073334,122.440677242729)) ;
#64511 = CARTESIAN_POINT('Ctrl Pts',(-18.4976553716752,-12.0000000043663,
122.424351349823)) ;
#64512 = CARTESIAN_POINT('Ctrl Pts',(-18.5129135125104,-12.,122.408362500768)) ;
#64513 = CARTESIAN_POINT('Ctrl Pts',(-18.5285699207533,-12.,122.392753917874)) ;
#64514 = CARTESIAN_POINT('Ctrl Pts',(-18.5841047825192,-12.,122.337388697449)) ;
#64515 = CARTESIAN_POINT('Ctrl Pts',(-18.6446065470671,-12.,122.28685455902)) ;
#64516 = CARTESIAN_POINT('Ctrl Pts',(-18.7093690801587,-12.,122.241689425851)) ;
#64517 = CARTESIAN_POINT('Ctrl Pts',(-18.7739954385736,-12.,122.19661926036)) ;
#64518 = CARTESIAN_POINT('Ctrl Pts',(-18.8429277799953,-12.,122.156848889559)) ;
#64519 = CARTESIAN_POINT('Ctrl Pts',(-18.9158209517903,-12.,122.123023408323)) ;
#64520 = CARTESIAN_POINT('Ctrl Pts',(-18.97041252654,-12.,122.097690633773)) ;
#64521 = CARTESIAN_POINT('Ctrl Pts',(-19.0272216439489,-12.0000000102563,
122.07569526255)) ;
#64522 = CARTESIAN_POINT('Ctrl Pts',(-19.0855066103726,-12.0000000043775,
122.057451417983)) ;
#64523 = CARTESIAN_POINT('Ctrl Pts',(-19.1048218044881,-12.0000000024293,
122.051405546794)) ;
#64524 = CARTESIAN_POINT('Ctrl Pts',(-19.1242986823222,-12.,122.045771825291)) ;
#64525 = CARTESIAN_POINT('Ctrl Pts',(-19.1439090623038,-12.,122.040565761127)) ;
#64526 = CARTESIAN_POINT('Ctrl Pts',(-19.2140201463212,-12.,122.02195302632)) ;
#64527 = CARTESIAN_POINT('Ctrl Pts',(-19.2857743787866,-12.0000000003845,
122.008825196783)) ;
#64528 = CARTESIAN_POINT('Ctrl Pts',(-19.3581616094974,-12.0000000000663,
122.001266834043)) ;
#64529 = CARTESIAN_POINT('Ctrl Pts',(-19.3669843878261,-12.0000000000275,
122.000345597544)) ;
#64530 = CARTESIAN_POINT('Ctrl Pts',(-19.3758165065751,-12.,121.999507090169)) ;
#64531 = CARTESIAN_POINT('Ctrl Pts',(-19.3846560842804,-12.,121.998751458056)) ;
#64532 = CARTESIAN_POINT('Ctrl Pts',(-19.4614572885066,-12.,121.99218627382)) ;
#64533 = CARTESIAN_POINT('Ctrl Pts',(-19.538903862666,-11.9999999928402,121.991868832861)) ;
#64534 = CARTESIAN_POINT('Ctrl Pts',(-19.6170404757029,-11.9999999993994,
121.998118870204)) ;
#64535 = CARTESIAN_POINT('Ctrl Pts',(-19.6215372909564,-11.9999999997768,
121.998478564106)) ;
#64536 = CARTESIAN_POINT('Ctrl Pts',(-19.6260364054519,-12.,121.998860014342)) ;
#64537 = CARTESIAN_POINT('Ctrl Pts',(-19.630537832746,-12.,121.999263283676)) ;
#64538 = CARTESIAN_POINT('Ctrl Pts',(-19.6881089405452,-12.,122.004420906088)) ;
#64539 = CARTESIAN_POINT('Ctrl Pts',(-19.7460667548092,-12.0000000189751,
122.013148289636)) ;
#64540 = CARTESIAN_POINT('Ctrl Pts',(-19.8035599226054,-12.0000000101354,
122.02543377879)) ;
#64541 = CARTESIAN_POINT('Ctrl Pts',(-19.8284255246479,-12.0000000063122,
122.030747211601)) ;
#64542 = CARTESIAN_POINT('Ctrl Pts',(-19.8532035599087,-12.,122.036726116961)) ;
#64543 = CARTESIAN_POINT('Ctrl Pts',(-19.8778221613683,-12.,122.043369085461)) ;
#64544 = CARTESIAN_POINT('Ctrl Pts',(-19.9591906752725,-12.,122.065325185429)) ;
#64545 = CARTESIAN_POINT('Ctrl Pts',(-20.0387357146672,-12.,122.094515610606)) ;
#64546 = CARTESIAN_POINT('Ctrl Pts',(-20.1155608588238,-12.,122.13054538147)) ;
#64547 = CARTESIAN_POINT('Ctrl Pts',(-20.1922295232036,-12.,122.166501765807)) ;
#64548 = CARTESIAN_POINT('Ctrl Pts',(-20.2662621433006,-12.,122.209300999016)) ;
#64549 = CARTESIAN_POINT('Ctrl Pts',(-20.3368145274386,-12.,122.259002783194)) ;
#64550 = CARTESIAN_POINT('Ctrl Pts',(-20.3861836086094,-12.,122.293781642156)) ;
#64551 = CARTESIAN_POINT('Ctrl Pts',(-20.4338172518609,-12.0000000080963,
122.331920190157)) ;
#64552 = CARTESIAN_POINT('Ctrl Pts',(-20.4789726009455,-12.0000000042853,
122.372781155038)) ;
#64553 = CARTESIAN_POINT('Ctrl Pts',(-20.49821889138,-12.0000000026609,122.390197076152)) ;
#64554 = CARTESIAN_POINT('Ctrl Pts',(-20.5170145004755,-12.,122.408107114264)) ;
#64555 = CARTESIAN_POINT('Ctrl Pts',(-20.5352999373477,-12.,122.426459820579)) ;
#64556 = CARTESIAN_POINT('Ctrl Pts',(-20.548691568813,-12.,122.439900717894)) ;
#64557 = CARTESIAN_POINT('Ctrl Pts',(-20.5618056963188,-12.,122.453575160092)) ;
#64558 = CARTESIAN_POINT('Ctrl Pts',(-20.5746457983858,-12.,122.467488525849)) ;
#64559 = CARTESIAN_POINT('Origin',(-20.3808735729049,-12.,126.250122109236)) ;
#64560 = CARTESIAN_POINT('',(-20.8451118552234,-12.,123.237406292887)) ;
#64561 = CARTESIAN_POINT('Origin',(-20.3808735729049,-12.,126.250122109236)) ;
#64562 = CARTESIAN_POINT('',(-18.1577260363418,-12.,123.523171848835)) ;
#64563 = CARTESIAN_POINT('',(-20.4601832664426,-12.,122.734993854115)) ;
#64564 = CARTESIAN_POINT('Ctrl Pts',(-20.8283303706881,10.,122.926041870813)) ;
#64565 = CARTESIAN_POINT('Ctrl Pts',(-20.5445170967909,9.82001091963712,123.023196933748)) ;
#64566 = CARTESIAN_POINT('Ctrl Pts',(-20.8845408159969,10.0066268508181,123.090165629856)) ;
#64567 = CARTESIAN_POINT('Ctrl Pts',(-20.5894888524673,9.82663777045524,123.154521539138)) ;
#64568 = CARTESIAN_POINT('Ctrl Pts',(-20.9394617690737,10.0198574772991,123.437507823531)) ;
#64569 = CARTESIAN_POINT('Ctrl Pts',(-20.633420846741,9.83986839693625,123.432353293108)) ;
#64570 = CARTESIAN_POINT('Ctrl Pts',(-20.8387858493119,10.0398330985578,123.958797508285)) ;
#64571 = CARTESIAN_POINT('Ctrl Pts',(-20.5528814274113,9.85984401819488,123.849407562291)) ;
#64572 = CARTESIAN_POINT('Ctrl Pts',(-20.5666727975867,10.0597504334597,124.412849839357)) ;
#64573 = CARTESIAN_POINT('Ctrl Pts',(-20.3351890331055,9.87976135309682,124.212644574099)) ;
#64574 = CARTESIAN_POINT('Ctrl Pts',(-20.157556275784,10.0796237101757,124.747029739186)) ;
#64575 = CARTESIAN_POINT('Ctrl Pts',(-20.007894029438,9.89963462981282,124.479989709356)) ;
#64576 = CARTESIAN_POINT('Ctrl Pts',(-19.6551315118144,10.0996482003397,124.922482691163)) ;
#64577 = CARTESIAN_POINT('Ctrl Pts',(-19.6059539581694,9.91965911997678,124.6203502007)) ;
#64578 = CARTESIAN_POINT('Ctrl Pts',(-19.1270395366036,10.1195160414904,124.915890798164)) ;
#64579 = CARTESIAN_POINT('Ctrl Pts',(-19.183479078867,9.9395269611275,124.615075206311)) ;
#64580 = CARTESIAN_POINT('Ctrl Pts',(-18.6307952228403,10.1394616923699,124.72957580943)) ;
#64581 = CARTESIAN_POINT('Ctrl Pts',(-18.7864838467008,9.95947261200706,124.466021078065)) ;
#64582 = CARTESIAN_POINT('Ctrl Pts',(-18.2288224078826,10.1593670929869,124.385607616877)) ;
#64583 = CARTESIAN_POINT('Ctrl Pts',(-18.4649063275282,9.97937801262402,124.19084435197)) ;
#64584 = CARTESIAN_POINT('Ctrl Pts',(-17.9678535157127,10.1792413208033,123.926349000794)) ;
#64585 = CARTESIAN_POINT('Ctrl Pts',(-18.2561329793354,9.99925224044038,123.823435269459)) ;
#64586 = CARTESIAN_POINT('Ctrl Pts',(-17.878734209588,10.1992271116809,123.402675114316)) ;
#64587 = CARTESIAN_POINT('Ctrl Pts',(-18.1848402358937,10.019238031318,123.404495614569)) ;
#64588 = CARTESIAN_POINT('Ctrl Pts',(-17.973517700436,10.2191213543406,122.882519965019)) ;
#64589 = CARTESIAN_POINT('Ctrl Pts',(-18.2606699231879,10.0391322739778,122.988371207676)) ;
#64590 = CARTESIAN_POINT('Ctrl Pts',(-18.2387528910803,10.2390000704127,122.425502981447)) ;
#64591 = CARTESIAN_POINT('Ctrl Pts',(-18.4728612986517,10.0590109900498,122.62275860733)) ;
#64592 = CARTESIAN_POINT('Ctrl Pts',(-18.647614090005,10.2590395202573,122.084258749108)) ;
#64593 = CARTESIAN_POINT('Ctrl Pts',(-18.7999520972875,10.0790504398944,122.349765888777)) ;
#64594 = CARTESIAN_POINT('Ctrl Pts',(-19.1441721121047,10.2789026817952,121.90452088182)) ;
#64595 = CARTESIAN_POINT('Ctrl Pts',(-19.1972003931787,10.0989136014323,122.205978444044)) ;
#64596 = CARTESIAN_POINT('Ctrl Pts',(-19.6750232066901,10.2988820498094,121.904721686728)) ;
#64597 = CARTESIAN_POINT('Ctrl Pts',(-19.6218814079036,10.1188929694465,122.206142590273)) ;
#64598 = CARTESIAN_POINT('Ctrl Pts',(-20.1701799765179,10.3186926303322,122.084083785786)) ;
#64599 = CARTESIAN_POINT('Ctrl Pts',(-20.0180064135448,10.1387035499693,122.349636107043)) ;
#64600 = CARTESIAN_POINT('Ctrl Pts',(-20.578226084171,10.3386735586178,122.423812224567)) ;
#64601 = CARTESIAN_POINT('Ctrl Pts',(-20.3444408940403,10.1586844782549,122.621421767106)) ;
#64602 = CARTESIAN_POINT('Ctrl Pts',(-20.8444469588477,10.3585662304872,122.880680954098)) ;
#64603 = CARTESIAN_POINT('Ctrl Pts',(-20.5574140513056,10.1785771501243,122.986919611144)) ;
#64604 = CARTESIAN_POINT('Ctrl Pts',(-20.9398341757817,10.3784925607743,123.40162915944)) ;
#64605 = CARTESIAN_POINT('Ctrl Pts',(-20.6337210673662,10.1985034804115,123.403677177554)) ;
#64606 = CARTESIAN_POINT('Ctrl Pts',(-20.8510572230715,10.3984631148666,123.924927290891)) ;
#64607 = CARTESIAN_POINT('Ctrl Pts',(-20.5626906127405,10.2184740345037,123.822322291595)) ;
#64608 = CARTESIAN_POINT('Ctrl Pts',(-20.6345446351863,10.4149949539542,124.307272603886)) ;
#64609 = CARTESIAN_POINT('Ctrl Pts',(-20.3894922234183,10.2350058735914,124.128174543065)) ;
#64610 = CARTESIAN_POINT('Ctrl Pts',(-20.3891097552813,10.4283346927818,124.557601822174)) ;
#64611 = CARTESIAN_POINT('Ctrl Pts',(-20.1931290434829,10.2483456124189,124.328455837242)) ;
#64612 = CARTESIAN_POINT('Ctrl Pts',(-20.1744300570267,10.4383669350004,124.710615084593)) ;
#64613 = CARTESIAN_POINT('Ctrl Pts',(-20.0213869924123,10.2583778546375,124.450860682641)) ;
#64614 = CARTESIAN_POINT('Ctrl Pts',(-19.9407404802418,10.4482246356439,124.822421617883)) ;
#64615 = CARTESIAN_POINT('Ctrl Pts',(-19.8344327400403,10.268235555281,124.540305070127)) ;
#64616 = CARTESIAN_POINT('Ctrl Pts',(-19.6879423525307,10.4582165002831,124.893352629427)) ;
#64617 = CARTESIAN_POINT('Ctrl Pts',(-19.6321963403517,10.2782274199202,124.597047919264)) ;
#64618 = CARTESIAN_POINT('Ctrl Pts',(-19.4284710425139,10.4681390500432,124.919080315321)) ;
#64619 = CARTESIAN_POINT('Ctrl Pts',(-19.4246096943487,10.2881499696804,124.61762631767)) ;
#64620 = CARTESIAN_POINT('Ctrl Pts',(-19.0804105140851,10.4814168235367,124.893583985624)) ;
#64621 = CARTESIAN_POINT('Ctrl Pts',(-19.14620736525,10.3014277431738,124.597234554234)) ;
#64622 = CARTESIAN_POINT('Ctrl Pts',(-18.7455859092888,10.4947641624773,124.776616835755)) ;
#64623 = CARTESIAN_POINT('Ctrl Pts',(-18.8783191462352,10.3147750821144,124.503658407746)) ;
#64624 = CARTESIAN_POINT('Ctrl Pts',(-18.4584522382473,10.5079713942705,124.581549246914)) ;
#64625 = CARTESIAN_POINT('Ctrl Pts',(-18.648603078249,10.3279823139076,124.347593121025)) ;
#64626 = CARTESIAN_POINT('Ctrl Pts',(-18.269958838059,10.5179585103602,124.398989341533)) ;
#64627 = CARTESIAN_POINT('Ctrl Pts',(-18.497812104421,10.3379694299973,124.201545371492)) ;
#64628 = CARTESIAN_POINT('Ctrl Pts',(-18.1163933969716,10.52790941594,124.187269395838)) ;
#64629 = CARTESIAN_POINT('Ctrl Pts',(-18.3749610183035,10.3479203355771,124.032167599002)) ;
#64630 = CARTESIAN_POINT('Ctrl Pts',(-18.0010345813923,10.5379645179474,123.949583784548)) ;
#64631 = CARTESIAN_POINT('Ctrl Pts',(-18.2826761214566,10.3579754375845,123.842018479487)) ;
#64632 = CARTESIAN_POINT('Ctrl Pts',(-17.9299233421522,10.5477861912685,123.701439503961)) ;
#64633 = CARTESIAN_POINT('Ctrl Pts',(-18.2257894437957,10.3677971109056,123.643501792389)) ;
#64634 = CARTESIAN_POINT('Ctrl Pts',(-17.9019040586336,10.5578446623434,123.43862866708)) ;
#64635 = CARTESIAN_POINT('Ctrl Pts',(-18.2033755364028,10.3778555819805,123.43325511011)) ;
#64636 = CARTESIAN_POINT('Ctrl Pts',(-17.9200547531203,10.5677692735199,123.178437417212)) ;
#64637 = CARTESIAN_POINT('Ctrl Pts',(-18.2179011304931,10.387780193157,123.22509433493)) ;
#64638 = CARTESIAN_POINT('Ctrl Pts',(-18.0035329037317,10.5810466124203,122.839624585047)) ;
#64639 = CARTESIAN_POINT('Ctrl Pts',(-18.2846726619434,10.4010575320574,122.954084471608)) ;
#64640 = CARTESIAN_POINT('Ctrl Pts',(-18.174078890485,10.5943454916579,122.53009645584)) ;
#64641 = CARTESIAN_POINT('Ctrl Pts',(-18.4211116702471,10.414356411295,122.706442742821)) ;
#64642 = CARTESIAN_POINT('Ctrl Pts',(-18.4148290889509,10.6075843638286,122.278909287836)) ;
#64643 = CARTESIAN_POINT('Ctrl Pts',(-18.61372828438,10.4275952834657,122.505480269817)) ;
#64644 = CARTESIAN_POINT('Ctrl Pts',(-18.6267237904145,10.6175909819652,122.123170592624)) ;
#64645 = CARTESIAN_POINT('Ctrl Pts',(-18.7832424340302,10.4376019016023,122.380894154854)) ;
#64646 = CARTESIAN_POINT('Ctrl Pts',(-18.8632279358434,10.6276219270267,122.006771081612)) ;
#64647 = CARTESIAN_POINT('Ctrl Pts',(-18.9724474943499,10.4476328466638,122.287775782223)) ;
#64648 = CARTESIAN_POINT('Ctrl Pts',(-19.1118308518252,10.6374781003785,121.93402103227)) ;
#64649 = CARTESIAN_POINT('Ctrl Pts',(-19.1713300681509,10.4574890200157,122.229578162461)) ;
#64650 = CARTESIAN_POINT('Ctrl Pts',(-19.3729271808616,10.6474773713414,121.904805274484)) ;
#64651 = CARTESIAN_POINT('Ctrl Pts',(-19.3802073636504,10.4674882909785,122.206207726809)) ;
#64652 = CARTESIAN_POINT('Ctrl Pts',(-19.63249343999,10.6573718230987,121.920897070182)) ;
#64653 = CARTESIAN_POINT('Ctrl Pts',(-19.5878600087485,10.4773827427359,122.219083373213)) ;
#64654 = CARTESIAN_POINT('Ctrl Pts',(-19.8895240952696,10.6674351389081,121.982913347126)) ;
#64655 = CARTESIAN_POINT('Ctrl Pts',(-19.7934840442871,10.4874460585452,122.268698557826)) ;
#64656 = CARTESIAN_POINT('Ctrl Pts',(-20.1266813029374,10.6772739956477,122.086019825898)) ;
#64657 = CARTESIAN_POINT('Ctrl Pts',(-19.9832086272329,10.4972849152848,122.351185625972)) ;
#64658 = CARTESIAN_POINT('Ctrl Pts',(-20.3474018172676,10.6873401174653,122.231740902041)) ;
#64659 = CARTESIAN_POINT('Ctrl Pts',(-20.1597838722231,10.5073510371024,122.46776433411)) ;
#64660 = CARTESIAN_POINT('Ctrl Pts',(-20.5359503275351,10.6972233451896,122.410409425907)) ;
#64661 = CARTESIAN_POINT('Ctrl Pts',(-20.3106209609387,10.5172342648267,122.6107005406)) ;
#64662 = CARTESIAN_POINT('Ctrl Pts',(-20.6926994160287,10.7072128064683,122.620953380555)) ;
#64663 = CARTESIAN_POINT('Ctrl Pts',(-20.4360184466383,10.5272237261055,122.779136903454)) ;
#64664 = CARTESIAN_POINT('Ctrl Pts',(-20.8101391925705,10.7171765168948,122.854988704109)) ;
#64665 = CARTESIAN_POINT('Ctrl Pts',(-20.5299682760089,10.5371874365319,122.966365995585)) ;
#64666 = CARTESIAN_POINT('Ctrl Pts',(-20.8856615342042,10.7271715196257,123.106575647569)) ;
#64667 = CARTESIAN_POINT('Ctrl Pts',(-20.5903840854433,10.5471824392628,123.167636082224)) ;
#64668 = CARTESIAN_POINT('Ctrl Pts',(-20.9160649147156,10.737207850636,123.368548316933)) ;
#64669 = CARTESIAN_POINT('Ctrl Pts',(-20.6147046374483,10.5572187702731,123.377214485628)) ;
#64670 = CARTESIAN_POINT('Ctrl Pts',(-20.901237668564,10.7470540799783,123.626888226543)) ;
#64671 = CARTESIAN_POINT('Ctrl Pts',(-20.6028407406531,10.5670649996154,123.583885836904)) ;
#64672 = CARTESIAN_POINT('Ctrl Pts',(-20.8414280631531,10.7570395782535,123.88234711985)) ;
#64673 = CARTESIAN_POINT('Ctrl Pts',(-20.5549910573095,10.5770504978907,123.788252351213)) ;
#64674 = CARTESIAN_POINT('Ctrl Pts',(-20.7388329136923,10.7669744812365,124.122475498249)) ;
#64675 = CARTESIAN_POINT('Ctrl Pts',(-20.4729131488679,10.5869854008736,123.98035400456)) ;
#64676 = CARTESIAN_POINT('Ctrl Pts',(-20.5941893977946,10.7770319843317,124.343638489499)) ;
#64677 = CARTESIAN_POINT('Ctrl Pts',(-20.3571965368945,10.5970429039689,124.157283333151)) ;
#64678 = CARTESIAN_POINT('Ctrl Pts',(-20.4178270374552,10.7868536407023,124.532127444505)) ;
#64679 = CARTESIAN_POINT('Ctrl Pts',(-20.216105589301,10.6068645603394,124.308072644051)) ;
#64680 = CARTESIAN_POINT('Ctrl Pts',(-20.2068264505713,10.7969097033674,124.691194003415)) ;
#64681 = CARTESIAN_POINT('Ctrl Pts',(-20.0473038554878,10.6169206230045,124.435324362058)) ;
#64682 = CARTESIAN_POINT('Ctrl Pts',(-19.9738709151238,10.8068503680706,124.809425923824)) ;
#64683 = CARTESIAN_POINT('Ctrl Pts',(-19.8609387422743,10.6268612877077,124.529907956941)) ;
#64684 = CARTESIAN_POINT('Ctrl Pts',(-19.7250819168071,10.8167547720191,124.885913848072)) ;
#64685 = CARTESIAN_POINT('Ctrl Pts',(-19.6619073830525,10.6367656916563,124.591096321636)) ;
#64686 = CARTESIAN_POINT('Ctrl Pts',(-19.4630900672441,10.8268012570127,124.918337587752)) ;
#64687 = CARTESIAN_POINT('Ctrl Pts',(-19.4523135810077,10.6468121766498,124.617033381453)) ;
#64688 = CARTESIAN_POINT('Ctrl Pts',(-19.2033217042056,10.8366974848244,124.905200421478)) ;
#64689 = CARTESIAN_POINT('Ctrl Pts',(-19.2444994521855,10.6567084044615,124.606521750019)) ;
#64690 = CARTESIAN_POINT('Ctrl Pts',(-18.9456501548748,10.8467570683879,124.846258925075)) ;
#64691 = CARTESIAN_POINT('Ctrl Pts',(-19.0383625055845,10.666767988025,124.559366649145)) ;
#64692 = CARTESIAN_POINT('Ctrl Pts',(-18.7071032762899,10.8566090780567,124.745604613553)) ;
#64693 = CARTESIAN_POINT('Ctrl Pts',(-18.8475263594419,10.6766199976938,124.478841692918)) ;
#64694 = CARTESIAN_POINT('Ctrl Pts',(-18.4867618466311,10.8665716094963,124.604236201826)) ;
#64695 = CARTESIAN_POINT('Ctrl Pts',(-18.6712543942556,10.6865825291334,124.36574560245)) ;
#64696 = CARTESIAN_POINT('Ctrl Pts',(-18.2932415519936,10.8766031577357,124.425213596724)) ;
#64697 = CARTESIAN_POINT('Ctrl Pts',(-18.5164393722649,10.6966140773728,124.222526126703)) ;
#64698 = CARTESIAN_POINT('Ctrl Pts',(-18.1357799386366,10.8864945689487,124.218398117847)) ;
#64699 = CARTESIAN_POINT('Ctrl Pts',(-18.3904718496513,10.7065054885858,124.057073085295)) ;
#64700 = CARTESIAN_POINT('Ctrl Pts',(-18.0146891209222,10.8965108226567,123.984678099418)) ;
#64701 = CARTESIAN_POINT('Ctrl Pts',(-18.2936007418435,10.7165217422938,123.870096295635)) ;
#64702 = CARTESIAN_POINT('Ctrl Pts',(-17.9364599064937,10.9065409255014,123.732978598351)) ;
#64703 = CARTESIAN_POINT('Ctrl Pts',(-18.2310191023128,10.7265518451385,123.66873611636)) ;
#64704 = CARTESIAN_POINT('Ctrl Pts',(-17.9032046926023,10.9163973744551,123.476088297528)) ;
#64705 = CARTESIAN_POINT('Ctrl Pts',(-18.2044167490604,10.7364082940922,123.463224374815)) ;
#64706 = CARTESIAN_POINT('Ctrl Pts',(-17.9148974747618,10.9263963852274,123.213627004979)) ;
#64707 = CARTESIAN_POINT('Ctrl Pts',(-18.2137726540653,10.7464073048645,123.253255524932)) ;
#64708 = CARTESIAN_POINT('Ctrl Pts',(-17.9711291549323,10.9362916021454,122.959700121601)) ;
#64709 = CARTESIAN_POINT('Ctrl Pts',(-18.2587594621295,10.7563025217825,123.050114944414)) ;
#64710 = CARTESIAN_POINT('Ctrl Pts',(-18.0722565351528,10.9463521175027,122.715462501341)) ;
#64711 = CARTESIAN_POINT('Ctrl Pts',(-18.3396629540108,10.7663630371399,122.854725296797)) ;
#64712 = CARTESIAN_POINT('Ctrl Pts',(-18.2111793287984,10.9562014108898,122.497051143162)) ;
#64713 = CARTESIAN_POINT('Ctrl Pts',(-18.4508020993981,10.7762123305269,122.679997778405)) ;
#64714 = CARTESIAN_POINT('Ctrl Pts',(-18.388559678523,10.9662285865698,122.302199917963)) ;
#64715 = CARTESIAN_POINT('Ctrl Pts',(-18.5927074978848,10.7862395062069,122.524117774987)) ;
#64716 = CARTESIAN_POINT('Ctrl Pts',(-18.5975457775489,10.976257162197,122.141622604304)) ;
#64717 = CARTESIAN_POINT('Ctrl Pts',(-18.7598974069773,10.7962680818341,122.395657172665)) ;
#64718 = CARTESIAN_POINT('Ctrl Pts',(-18.8267122580128,10.9861022557429,122.021573575598)) ;
#64719 = CARTESIAN_POINT('Ctrl Pts',(-18.9432305035226,10.80611317538,122.299619713947)) ;
#64720 = CARTESIAN_POINT('Ctrl Pts',(-19.0767061726053,10.9960934971746,121.941311591283)) ;
#64721 = CARTESIAN_POINT('Ctrl Pts',(-19.1432259108285,10.8161044168118,122.235411491827)) ;
#64722 = CARTESIAN_POINT('Ctrl Pts',(-19.3380760888337,11.0061292783179,121.906059986019)) ;
#64723 = CARTESIAN_POINT('Ctrl Pts',(-19.3523221423469,10.826140197955,122.20721167611)) ;
#64724 = CARTESIAN_POINT('Ctrl Pts',(-19.5967752495355,11.0159814840476,121.916185579079)) ;
#64725 = CARTESIAN_POINT('Ctrl Pts',(-19.5592805072898,10.8359924036847,122.215313538143)) ;
#64726 = CARTESIAN_POINT('Ctrl Pts',(-19.8527735772293,11.0259435781646,121.970943280899)) ;
#64727 = CARTESIAN_POINT('Ctrl Pts',(-19.7640785909624,10.8459544978017,122.259120868789)) ;
#64728 = CARTESIAN_POINT('Ctrl Pts',(-20.0967309229679,11.0359661389917,122.070215768955)) ;
#64729 = CARTESIAN_POINT('Ctrl Pts',(-19.9592439949302,10.8559770586288,122.338540107306)) ;
#64730 = CARTESIAN_POINT('Ctrl Pts',(-20.3177943873502,11.0458939106433,122.208809071659)) ;
#64731 = CARTESIAN_POINT('Ctrl Pts',(-20.1360936655196,10.8659048302804,122.449415566975)) ;
#64732 = CARTESIAN_POINT('Ctrl Pts',(-20.513619210783,11.0559362947681,122.385690857822)) ;
#64733 = CARTESIAN_POINT('Ctrl Pts',(-20.2927527608326,10.8759472144052,122.590922041084)) ;
#64734 = CARTESIAN_POINT('Ctrl Pts',(-20.6733901753496,11.0658255188387,122.590674219405)) ;
#64735 = CARTESIAN_POINT('Ctrl Pts',(-20.4205680784334,10.8858364384758,122.754908921902)) ;
#64736 = CARTESIAN_POINT('Ctrl Pts',(-20.7967974985103,11.075814767006,122.822355021181)) ;
#64737 = CARTESIAN_POINT('Ctrl Pts',(-20.5192928376293,10.8958256866432,122.940253955908)) ;
#64738 = CARTESIAN_POINT('Ctrl Pts',(-20.8776639039544,11.085773344048,123.07124139589)) ;
#64739 = CARTESIAN_POINT('Ctrl Pts',(-20.5839847120867,10.9057842636851,123.139363096927)) ;
#64740 = CARTESIAN_POINT('Ctrl Pts',(-20.9145104547189,11.0956729131393,123.328785419539)) ;
#64741 = CARTESIAN_POINT('Ctrl Pts',(-20.6134608083522,10.9156838327764,123.34539776855)) ;
#64742 = CARTESIAN_POINT('Ctrl Pts',(-20.9058609614056,11.1057208252233,123.592665004876)) ;
#64743 = CARTESIAN_POINT('Ctrl Pts',(-20.6065401309608,10.9257317448604,123.556501576119)) ;
#64744 = CARTESIAN_POINT('Ctrl Pts',(-20.8525354819136,11.1156161795305,123.847220118537)) ;
#64745 = CARTESIAN_POINT('Ctrl Pts',(-20.5638788889721,10.9356270991676,123.760144740549)) ;
#64746 = CARTESIAN_POINT('Ctrl Pts',(-20.7542573598821,11.1256778300217,124.092654877015)) ;
#64747 = CARTESIAN_POINT('Ctrl Pts',(-20.485255344439,10.9456887496588,123.95649240933)) ;
#64748 = CARTESIAN_POINT('Ctrl Pts',(-20.6178768119318,11.1355224454842,124.31250491989)) ;
#64749 = CARTESIAN_POINT('Ctrl Pts',(-20.3761506014328,10.9555333651213,124.132371010177)) ;
#64750 = CARTESIAN_POINT('Ctrl Pts',(-20.4440816600714,11.1454825243856,124.508211665868)) ;
#64751 = CARTESIAN_POINT('Ctrl Pts',(-20.2371141294296,10.9654934440227,124.288935606726)) ;
#64752 = CARTESIAN_POINT('Ctrl Pts',(-20.2370227832588,11.1555207187439,124.671637321506)) ;
#64753 = CARTESIAN_POINT('Ctrl Pts',(-20.0714663599296,10.9755316383811,124.419675493237)) ;
#64754 = CARTESIAN_POINT('Ctrl Pts',(-20.0087297938616,11.1653944341435,124.795026404838)) ;
#64755 = CARTESIAN_POINT('Ctrl Pts',(-19.8888323768802,10.9854053537807,124.518385630322)) ;
#64756 = CARTESIAN_POINT('Ctrl Pts',(-19.7576006730884,11.1754661436778,124.87849507525)) ;
#64757 = CARTESIAN_POINT('Ctrl Pts',(-19.6879285180809,10.9954770633149,124.585159904661)) ;
#64758 = CARTESIAN_POINT('Ctrl Pts',(-19.5019775459593,11.1852985841303,124.916330182897)) ;
#64759 = CARTESIAN_POINT('Ctrl Pts',(-19.4834310649531,11.0053095037674,124.61542705853)) ;
#64760 = CARTESIAN_POINT('Ctrl Pts',(-19.2384391664689,11.1953304050557,124.909797495667)) ;
#64761 = CARTESIAN_POINT('Ctrl Pts',(-19.2726002800821,11.0153413246928,124.610200312681)) ;
#64762 = CARTESIAN_POINT('Ctrl Pts',(-18.9804733109709,11.2053507749413,124.856926970494)) ;
#64763 = CARTESIAN_POINT('Ctrl Pts',(-19.0662277209886,11.0253616945784,124.567903126728)) ;
#64764 = CARTESIAN_POINT('Ctrl Pts',(-18.7390964607104,11.215217546075,124.762178595596)) ;
#64765 = CARTESIAN_POINT('Ctrl Pts',(-18.8731273657641,11.0352284657122,124.492104212861)) ;
#64766 = CARTESIAN_POINT('Ctrl Pts',(-18.5133063352698,11.2252883172644,124.624178813688)) ;
#64767 = CARTESIAN_POINT('Ctrl Pts',(-18.6924953042277,11.0452992369015,124.381703691916)) ;
#64768 = CARTESIAN_POINT('Ctrl Pts',(-18.3193404016488,11.235131477786,124.453023478491)) ;
#64769 = CARTESIAN_POINT('Ctrl Pts',(-18.5373238034759,11.0551423974231,124.24477971788)) ;
#64770 = CARTESIAN_POINT('Ctrl Pts',(-18.1551353492722,11.2451117109724,124.248529269541)) ;
#64771 = CARTESIAN_POINT('Ctrl Pts',(-18.4059602224555,11.0651226306096,124.081184300254)) ;
#64772 = CARTESIAN_POINT('Ctrl Pts',(-18.028891195577,11.2551302310076,124.017503067163)) ;
#64773 = CARTESIAN_POINT('Ctrl Pts',(-18.3049653496854,11.0751411506447,123.896363082341)) ;
#64774 = CARTESIAN_POINT('Ctrl Pts',(-17.94527872475,11.2650135393913,123.771572840937)) ;
#64775 = CARTESIAN_POINT('Ctrl Pts',(-18.2380760136292,11.0850244590284,123.699619611155)) ;
#64776 = CARTESIAN_POINT('Ctrl Pts',(-17.9050223248742,11.2750818235621,123.510113552435)) ;
#64777 = CARTESIAN_POINT('Ctrl Pts',(-18.2058712472604,11.0950927431992,123.490451793453)) ;
#64778 = CARTESIAN_POINT('Ctrl Pts',(-17.9103370638304,11.2849119502298,123.251798025967)) ;
#64779 = CARTESIAN_POINT('Ctrl Pts',(-18.2101233434264,11.1049228698669,123.283800611474)) ;
#64780 = CARTESIAN_POINT('Ctrl Pts',(-17.9612752714376,11.2949785224363,122.992253063296)) ;
#64781 = CARTESIAN_POINT('Ctrl Pts',(-18.2508742115829,11.1149894420734,123.07616437634)) ;
#64782 = CARTESIAN_POINT('Ctrl Pts',(-18.0550114914209,11.304868678677,122.749806436418)) ;
#64783 = CARTESIAN_POINT('Ctrl Pts',(-18.3258631525923,11.1248795983141,122.882207960884)) ;
#64784 = CARTESIAN_POINT('Ctrl Pts',(-18.1902998279982,11.3148612062534,122.524765958901)) ;
#64785 = CARTESIAN_POINT('Ctrl Pts',(-18.4340938564837,11.1348721258905,122.702175798357)) ;
#64786 = CARTESIAN_POINT('Ctrl Pts',(-18.362252777776,11.3248226961277,122.327384835979)) ;
#64787 = CARTESIAN_POINT('Ctrl Pts',(-18.57165612635,11.1448336157648,122.544271311536)) ;
#64788 = CARTESIAN_POINT('Ctrl Pts',(-18.5644303505552,11.3347319180149,122.163249256382)) ;
#64789 = CARTESIAN_POINT('Ctrl Pts',(-18.7333976447445,11.154742837652,122.412963346025)) ;
#64790 = CARTESIAN_POINT('Ctrl Pts',(-18.7952595963488,11.3447804978252,122.035028175252)) ;
#64791 = CARTESIAN_POINT('Ctrl Pts',(-18.9180612583401,11.1647914174624,122.310386442191)) ;
#64792 = CARTESIAN_POINT('Ctrl Pts',(-19.0407305551564,11.3546634722953,121.950157334317)) ;
#64793 = CARTESIAN_POINT('Ctrl Pts',(-19.1144372025468,11.1746743919324,122.242490108327)) ;
#64794 = CARTESIAN_POINT('Ctrl Pts',(-19.3000011957523,11.364658383438,121.908176471057)) ;
#64795 = CARTESIAN_POINT('Ctrl Pts',(-19.3218535588989,11.1846693030751,122.208905345717)) ;
#64796 = CARTESIAN_POINT('Ctrl Pts',(-19.5633130308643,11.3746787700116,121.912223489131)) ;
#64797 = CARTESIAN_POINT('Ctrl Pts',(-19.532503054688,11.1946896896487,122.212142961274)) ;
#64798 = CARTESIAN_POINT('Ctrl Pts',(-19.8190707586081,11.3845888738687,121.961229817149)) ;
#64799 = CARTESIAN_POINT('Ctrl Pts',(-19.7371085224044,11.2045997935058,122.251347849191)) ;
#64800 = CARTESIAN_POINT('Ctrl Pts',(-20.0631345837218,11.3945165860786,122.053434027889)) ;
#64801 = CARTESIAN_POINT('Ctrl Pts',(-19.9323591038037,11.2145275057157,122.325110807346)) ;
#64802 = CARTESIAN_POINT('Ctrl Pts',(-20.2899581915959,11.4045596958458,122.18834359306)) ;
#64803 = CARTESIAN_POINT('Ctrl Pts',(-20.1138182163407,11.2245706154829,122.433038412383)) ;
#64804 = CARTESIAN_POINT('Ctrl Pts',(-20.4869200798739,11.4144461163014,122.357790944953)) ;
#64805 = CARTESIAN_POINT('Ctrl Pts',(-20.2713871970456,11.2344570359385,122.568595575828)) ;
#64806 = CARTESIAN_POINT('Ctrl Pts',(-20.653571934063,11.424439293907,122.560728657171)) ;
#64807 = CARTESIAN_POINT('Ctrl Pts',(-20.4047088177741,11.2444502135441,122.730945421941)) ;
#64808 = CARTESIAN_POINT('Ctrl Pts',(-20.7817631202176,11.4343849568109,122.788494689918)) ;
#64809 = CARTESIAN_POINT('Ctrl Pts',(-20.5072617816881,11.254395876448,122.913157693448)) ;
#64810 = CARTESIAN_POINT('Ctrl Pts',(-20.8689810112581,11.4443322530161,123.034933251578)) ;
#64811 = CARTESIAN_POINT('Ctrl Pts',(-20.5770363372179,11.2643431726532,123.11030796952)) ;
#64812 = CARTESIAN_POINT('Ctrl Pts',(-20.9122274632139,11.454380018594,123.295405142899)) ;
#64813 = CARTESIAN_POINT('Ctrl Pts',(-20.611633872492,11.2743909382311,123.318685623006)) ;
#64814 = CARTESIAN_POINT('Ctrl Pts',(-20.909847955661,11.4642282318116,123.554192250672)) ;
#64815 = CARTESIAN_POINT('Ctrl Pts',(-20.6097306740805,11.2842391514487,123.525714196094)) ;
#64816 = CARTESIAN_POINT('Ctrl Pts',(-20.8628861917845,11.4741878046057,123.811671085768)) ;
#64817 = CARTESIAN_POINT('Ctrl Pts',(-20.5721619350103,11.2941987242428,123.731697005072)) ;
#64818 = CARTESIAN_POINT('Ctrl Pts',(-20.7707963194684,11.4842244256382,124.058815012756)) ;
#64819 = CARTESIAN_POINT('Ctrl Pts',(-20.4984904591295,11.3042353452753,123.929412437981)) ;
#64820 = CARTESIAN_POINT('Ctrl Pts',(-20.6396015638057,11.4941049404486,124.282914554949)) ;
#64821 = CARTESIAN_POINT('Ctrl Pts',(-20.3935356247347,11.3141158600857,124.108691603462)) ;
#64822 = CARTESIAN_POINT('Ctrl Pts',(-20.4686789714687,11.5041575917556,124.484292270277)) ;
#64823 = CARTESIAN_POINT('Ctrl Pts',(-20.2567978844015,11.3241685113927,124.26979434849)) ;
#64824 = CARTESIAN_POINT('Ctrl Pts',(-20.2685707709031,11.5140529900356,124.650429772369)) ;
#64825 = CARTESIAN_POINT('Ctrl Pts',(-20.0967123281824,11.3340639096727,124.402704356806)) ;
#64826 = CARTESIAN_POINT('Ctrl Pts',(-20.0392516106828,11.5241031117417,124.781376915193)) ;
#64827 = CARTESIAN_POINT('Ctrl Pts',(-19.9132571537407,11.3441140313788,124.50746276443)) ;
#64828 = CARTESIAN_POINT('Ctrl Pts',(-19.794737934636,11.5339873912836,124.869107009898)) ;
#64829 = CARTESIAN_POINT('Ctrl Pts',(-19.7176472402292,11.3539983109207,124.577647198776)) ;
#64830 = CARTESIAN_POINT('Ctrl Pts',(-19.5359779545354,11.5439821725755,124.914016452958)) ;
#64831 = CARTESIAN_POINT('Ctrl Pts',(-19.5106395508264,11.3639930922127,124.613575518455)) ;
#64832 = CARTESIAN_POINT('Ctrl Pts',(-19.2745423776044,11.5539300177623,124.913217278818)) ;
#64833 = CARTESIAN_POINT('Ctrl Pts',(-19.3014915210338,11.3739409373994,124.612936961295)) ;
#64834 = CARTESIAN_POINT('Ctrl Pts',(-19.0174715357979,11.5638669811497,124.867467500935)) ;
#64835 = CARTESIAN_POINT('Ctrl Pts',(-19.0958351968564,11.3838779007868,124.576338085747)) ;
#64836 = CARTESIAN_POINT('Ctrl Pts',(-18.7709478903475,11.5738499458869,124.77765044511)) ;
#64837 = CARTESIAN_POINT('Ctrl Pts',(-18.8986161489032,11.3938608655241,124.504485401762)) ;
#64838 = CARTESIAN_POINT('Ctrl Pts',(-18.5426769439724,11.5838937973026,124.645205762056)) ;
#64839 = CARTESIAN_POINT('Ctrl Pts',(-18.7159988423959,11.4039047169397,124.398530300539)) ;
#64840 = CARTESIAN_POINT('Ctrl Pts',(-18.3447570490132,11.5937219986373,124.479210868658)) ;
#64841 = CARTESIAN_POINT('Ctrl Pts',(-18.5576631821431,11.4137329182744,124.265735876442)) ;
#64842 = CARTESIAN_POINT('Ctrl Pts',(-18.1744334770806,11.6037985712354,124.27652667465)) ;
#64843 = CARTESIAN_POINT('Ctrl Pts',(-18.4214033306732,11.4238094908725,124.103588905207)) ;
#64844 = CARTESIAN_POINT('Ctrl Pts',(-18.0446742700679,11.6136506512429,124.052422800966)) ;
#64845 = CARTESIAN_POINT('Ctrl Pts',(-18.3175955633479,11.43366157088,123.924307178956)) ;
#64846 = CARTESIAN_POINT('Ctrl Pts',(-17.9536271837052,11.623723936247,123.80390465869)) ;
#64847 = CARTESIAN_POINT('Ctrl Pts',(-18.2447567627859,11.4437348558841,123.725492737883)) ;
#64848 = CARTESIAN_POINT('Ctrl Pts',(-17.9082400349615,11.6335652879575,123.549277141686)) ;
#64849 = CARTESIAN_POINT('Ctrl Pts',(-18.2084461725825,11.4535762075946,123.521791939049)) ;
#64850 = CARTESIAN_POINT('Ctrl Pts',(-17.9067818389188,11.643526787354,123.287519099378)) ;
#64851 = CARTESIAN_POINT('Ctrl Pts',(-18.2072783316507,11.4635377069911,123.312385832505)) ;
#64852 = CARTESIAN_POINT('Ctrl Pts',(-17.951583816689,11.653562563484,123.027613430416)) ;
#64853 = CARTESIAN_POINT('Ctrl Pts',(-18.2431187615393,11.4735734831211,123.104461008452)) ;
#64854 = CARTESIAN_POINT('Ctrl Pts',(-18.0392630064654,11.6634509901216,122.782997517006)) ;
#64855 = CARTESIAN_POINT('Ctrl Pts',(-18.3132606925425,11.4834619097587,122.908768552732)) ;
#64856 = CARTESIAN_POINT('Ctrl Pts',(-18.169309686562,11.6734663121965,122.55416670281)) ;
#64857 = CARTESIAN_POINT('Ctrl Pts',(-18.4172968626864,11.4934772318336,122.72570323888)) ;
#64858 = CARTESIAN_POINT('Ctrl Pts',(-18.337832034103,11.6834966610967,122.351486710983)) ;
#64859 = CARTESIAN_POINT('Ctrl Pts',(-18.5521138475697,11.5035075807338,122.563558413002)) ;
#64860 = CARTESIAN_POINT('Ctrl Pts',(-18.5348954406339,11.6933400367034,122.18392868398)) ;
#64861 = CARTESIAN_POINT('Ctrl Pts',(-18.7097629733351,11.5133509563405,122.429511607795)) ;
#64862 = CARTESIAN_POINT('Ctrl Pts',(-18.7619871989816,11.7033694736005,122.05014873987)) ;
#64863 = CARTESIAN_POINT('Ctrl Pts',(-18.8914356924309,11.5233803932376,122.322486374189)) ;
#64864 = CARTESIAN_POINT('Ctrl Pts',(-19.0091747229,11.7134013515334,121.958483598159)) ;
#64865 = CARTESIAN_POINT('Ctrl Pts',(-19.0891853235092,11.5334122711706,122.24915301597)) ;
#64866 = CARTESIAN_POINT('Ctrl Pts',(-19.2631763810942,11.7232309746389,121.91157223852)) ;
#64867 = CARTESIAN_POINT('Ctrl Pts',(-19.2923853954677,11.543241894276,122.211622724481)) ;
#64868 = CARTESIAN_POINT('Ctrl Pts',(-19.5256800788775,11.733220445792,121.908654949481)) ;
#64869 = CARTESIAN_POINT('Ctrl Pts',(-19.5023881948005,11.5532313654291,122.209287326421)) ;
#64870 = CARTESIAN_POINT('Ctrl Pts',(-19.7859934259949,11.7432642945544,121.95225353693)) ;
#64871 = CARTESIAN_POINT('Ctrl Pts',(-19.7106392257516,11.5632752141915,122.244164799925)) ;
#64872 = CARTESIAN_POINT('Ctrl Pts',(-20.0294606191008,11.7530860000861,122.037936667196)) ;
#64873 = CARTESIAN_POINT('Ctrl Pts',(-19.9054125518466,11.5730969197232,122.312709519324)) ;
#64874 = CARTESIAN_POINT('Ctrl Pts',(-20.2595522204667,11.7631210399139,122.166778899388)) ;
#64875 = CARTESIAN_POINT('Ctrl Pts',(-20.0894867189853,11.583131959551,122.415781895507)) ;
#64876 = CARTESIAN_POINT('Ctrl Pts',(-20.4631137171743,11.7731457468054,122.334014058184)) ;
#64877 = CARTESIAN_POINT('Ctrl Pts',(-20.2523368993887,11.5931566664425,122.549568855976)) ;
#64878 = CARTESIAN_POINT('Ctrl Pts',(-20.6320140503155,11.7829984511461,122.530257519376)) ;
#64879 = CARTESIAN_POINT('Ctrl Pts',(-20.3874578756258,11.6030093707832,122.706561953202)) ;
#64880 = CARTESIAN_POINT('Ctrl Pts',(-20.7664764699797,11.7929865733538,122.755655719711)) ;
#64881 = CARTESIAN_POINT('Ctrl Pts',(-20.4950292060904,11.6129974929909,122.886879510142)) ;
#64882 = CARTESIAN_POINT('Ctrl Pts',(-20.8592244692304,11.8029150434611,122.999531121806)) ;
#64883 = CARTESIAN_POINT('Ctrl Pts',(-20.5692290568483,11.6229259630982,123.081978836487)) ;
#64884 = CARTESIAN_POINT('Ctrl Pts',(-20.9089464870837,11.8129040206283,123.257291767332)) ;
#64885 = CARTESIAN_POINT('Ctrl Pts',(-20.609008398413,11.6329149402654,123.288186875209)) ;
#64886 = CARTESIAN_POINT('Ctrl Pts',(-20.912726728438,11.822941827908,123.521040547069)) ;
#64887 = CARTESIAN_POINT('Ctrl Pts',(-20.6120343028068,11.6429527475451,123.499185942152)) ;
#64888 = CARTESIAN_POINT('Ctrl Pts',(-20.8718727620384,11.8327881287713,123.776548267499)) ;
#64889 = CARTESIAN_POINT('Ctrl Pts',(-20.5793530040237,11.6527990484084,123.703591663681)) ;
#64890 = CARTESIAN_POINT('Ctrl Pts',(-20.7862889531826,11.8428138721506,124.025729898005)) ;
#64891 = CARTESIAN_POINT('Ctrl Pts',(-20.5108877193562,11.6628247917877,123.902937607542)) ;
#64892 = CARTESIAN_POINT('Ctrl Pts',(-20.6580711492051,11.8528447385896,124.256054351195)) ;
#64893 = CARTESIAN_POINT('Ctrl Pts',(-20.4083150016841,11.6728556582267,124.087198055119)) ;
#64894 = CARTESIAN_POINT('Ctrl Pts',(-20.4954300469777,11.8626820973884,124.456984258248)) ;
#64895 = CARTESIAN_POINT('Ctrl Pts',(-20.2782040287213,11.6826930170255,124.24794255801)) ;
#64896 = CARTESIAN_POINT('Ctrl Pts',(-20.2977609080492,11.8726740583222,124.62982526479)) ;
#64897 = CARTESIAN_POINT('Ctrl Pts',(-20.1200700801293,11.6926849779593,124.386216765177)) ;
#64898 = CARTESIAN_POINT('Ctrl Pts',(-20.0718918884167,11.8827064208787,124.765820716401)) ;
#64899 = CARTESIAN_POINT('Ctrl Pts',(-19.9393758049619,11.7027173405158,124.495014745963)) ;
#64900 = CARTESIAN_POINT('Ctrl Pts',(-19.830074922632,11.8925715814531,124.859237594725)) ;
#64901 = CARTESIAN_POINT('Ctrl Pts',(-19.7459234677896,11.7125825010902,124.569749829709)) ;
#64902 = CARTESIAN_POINT('Ctrl Pts',(-19.5733413955139,11.9025334860308,124.910472534242)) ;
#64903 = CARTESIAN_POINT('Ctrl Pts',(-19.5405372387899,11.7225444056679,124.610739722214)) ;
#64904 = CARTESIAN_POINT('Ctrl Pts',(-19.3097054567228,11.9125684161065,124.915962853087)) ;
#64905 = CARTESIAN_POINT('Ctrl Pts',(-19.3296285015763,11.7325793357437,124.615133939698)) ;
#64906 = CARTESIAN_POINT('Ctrl Pts',(-19.0528979312036,11.9224533629601,124.876622619197)) ;
#64907 = CARTESIAN_POINT('Ctrl Pts',(-19.1241826214947,11.7424642825973,124.583663814499)) ;
#64908 = CARTESIAN_POINT('Ctrl Pts',(-18.8024198540435,11.9325190392716,124.791735612442)) ;
#64909 = CARTESIAN_POINT('Ctrl Pts',(-18.9237994015907,11.7525299589087,124.515756076817)) ;
#64910 = CARTESIAN_POINT('Ctrl Pts',(-18.5755065294971,11.9423579589065,124.667701912514)) ;
#64911 = CARTESIAN_POINT('Ctrl Pts',(-18.7422682586687,11.7623688785436,124.416531178168)) ;
#64912 = CARTESIAN_POINT('Ctrl Pts',(-18.3688173844643,11.9524214686409,124.502784044984)) ;
#64913 = CARTESIAN_POINT('Ctrl Pts',(-18.576915561043,11.7724323882781,124.284598445225)) ;
#64914 = CARTESIAN_POINT('Ctrl Pts',(-18.1969723593472,11.9623150818027,124.307637940785)) ;
#64915 = CARTESIAN_POINT('Ctrl Pts',(-18.4394382482953,11.7823260014398,124.128483203739)) ;
#64916 = CARTESIAN_POINT('Ctrl Pts',(-18.0603757685369,11.9722590886161,124.08490476088)) ;
#64917 = CARTESIAN_POINT('Ctrl Pts',(-18.3301592733883,11.7922700082532,123.950297959954)) ;
#64918 = CARTESIAN_POINT('Ctrl Pts',(-17.9638367967476,11.9822600429704,123.840420099808)) ;
#64919 = CARTESIAN_POINT('Ctrl Pts',(-18.2529261323973,11.8022709626075,123.754711076634)) ;
#64920 = CARTESIAN_POINT('Ctrl Pts',(-17.9114896578375,11.9922988006627,123.58188181945)) ;
#64921 = CARTESIAN_POINT('Ctrl Pts',(-18.2110463657214,11.8123097202998,123.547880858099)) ;
#64922 = CARTESIAN_POINT('Ctrl Pts',(-17.9044041219212,12.0021229848327,123.323787975382)) ;
#64923 = CARTESIAN_POINT('Ctrl Pts',(-18.2053758050296,11.8221339044698,123.341406308645)) ;
#64924 = CARTESIAN_POINT('Ctrl Pts',(-17.9427499485555,12.0121810504321,123.062292370625)) ;
#64925 = CARTESIAN_POINT('Ctrl Pts',(-18.2360503193674,11.8321919700692,123.132209452442)) ;
#64926 = CARTESIAN_POINT('Ctrl Pts',(-18.0251977237691,12.0221110972068,122.814691316201)) ;
#64927 = CARTESIAN_POINT('Ctrl Pts',(-18.3020064298566,11.8421220168439,122.934128140568)) ;
#64928 = CARTESIAN_POINT('Ctrl Pts',(-18.1490393731302,12.0320625395439,122.584356522223)) ;
#64929 = CARTESIAN_POINT('Ctrl Pts',(-18.4010777391838,11.8520734591811,122.749859395245)) ;
#64930 = CARTESIAN_POINT('Ctrl Pts',(-18.3128249788135,12.0421093367232,122.377284739554)) ;
#64931 = CARTESIAN_POINT('Ctrl Pts',(-18.5321045207289,11.8621202563603,122.584200615192)) ;
#64932 = CARTESIAN_POINT('Ctrl Pts',(-18.5060148098008,12.0519572774033,122.205087588693)) ;
#64933 = CARTESIAN_POINT('Ctrl Pts',(-18.6866546893362,11.8719681970404,122.446441468451)) ;
#64934 = CARTESIAN_POINT('Ctrl Pts',(-18.7282729224672,12.0619189087459,122.066794754727)) ;
#64935 = CARTESIAN_POINT('Ctrl Pts',(-18.8644599124411,11.881929828383,122.335805352937)) ;
#64936 = CARTESIAN_POINT('Ctrl Pts',(-18.9729503385559,12.0719475681218,121.968835081685)) ;
#64937 = CARTESIAN_POINT('Ctrl Pts',(-19.0602009883113,11.8919584877589,122.257435568384)) ;
#64938 = CARTESIAN_POINT('Ctrl Pts',(-19.227831787757,12.08185787101,121.915407496624)) ;
#64939 = CARTESIAN_POINT('Ctrl Pts',(-19.2641055266912,11.9018687906471,122.214691356274)) ;
#64940 = CARTESIAN_POINT('Ctrl Pts',(-19.4887612039821,12.0917927655722,121.906342273827)) ;
#64941 = CARTESIAN_POINT('Ctrl Pts',(-19.472848876618,11.9118036852093,122.207436933983)) ;
#64942 = CARTESIAN_POINT('Ctrl Pts',(-19.7500144690061,12.1018338642391,121.943349818059)) ;
#64943 = CARTESIAN_POINT('Ctrl Pts',(-19.6818517658866,11.9218447838762,122.23704074526)) ;
#64944 = CARTESIAN_POINT('Ctrl Pts',(-19.9971083719985,12.1117211467435,122.023739879768)) ;
#64945 = CARTESIAN_POINT('Ctrl Pts',(-19.8795274617952,11.9317320663806,122.301350619632)) ;
#64946 = CARTESIAN_POINT('Ctrl Pts',(-20.2290950029525,12.121712887254,122.146694306298)) ;
#64947 = CARTESIAN_POINT('Ctrl Pts',(-20.0651177734983,11.9417238068911,122.399712142644)) ;
#64948 = CARTESIAN_POINT('Ctrl Pts',(-20.4353231818005,12.1316634364894,122.307485013012)) ;
#64949 = CARTESIAN_POINT('Ctrl Pts',(-20.230101643679,11.9516743561265,122.528342886444)) ;
#64950 = CARTESIAN_POINT('Ctrl Pts',(-20.6105080303125,12.1415991141242,122.501068844292)) ;
#64951 = CARTESIAN_POINT('Ctrl Pts',(-20.3702511605467,11.9616100337613,122.683208400421)) ;
#64952 = CARTESIAN_POINT('Ctrl Pts',(-20.750371753253,12.151584531917,122.723117938316)) ;
#64953 = CARTESIAN_POINT('Ctrl Pts',(-20.4821440178031,11.9715954515541,122.860846434547)) ;
#64954 = CARTESIAN_POINT('Ctrl Pts',(-20.8496752814087,12.1616133247875,122.967237619846)) ;
#64955 = CARTESIAN_POINT('Ctrl Pts',(-20.5615889029913,11.9816242444246,123.056141266303)) ;
#64956 = CARTESIAN_POINT('Ctrl Pts',(-20.9045281450594,12.1714928360155,123.220996340645)) ;
#64957 = CARTESIAN_POINT('Ctrl Pts',(-20.6054733938422,11.9915037556526,123.259147756982)) ;
#64958 = CARTESIAN_POINT('Ctrl Pts',(-20.9152054113298,12.1814863726884,123.483408955597)) ;
#64959 = CARTESIAN_POINT('Ctrl Pts',(-20.6140174445098,12.0014972923255,123.469077721808)) ;
#64960 = CARTESIAN_POINT('Ctrl Pts',(-20.8794802827671,12.1915186409522,123.744603500789)) ;
#64961 = CARTESIAN_POINT('Ctrl Pts',(-20.5854395864625,12.0115295605894,123.678033578765)) ;
#64962 = CARTESIAN_POINT('Ctrl Pts',(-20.8008139737887,12.2013826029581,123.991621606298)) ;
#64963 = CARTESIAN_POINT('Ctrl Pts',(-20.522508650298,12.0213935225952,123.875648805063)) ;
#64964 = CARTESIAN_POINT('Ctrl Pts',(-20.678002189668,12.211452664303,124.225997440401)) ;
#64965 = CARTESIAN_POINT('Ctrl Pts',(-20.4242612619508,12.0314635839401,124.063150402527)) ;
#64966 = CARTESIAN_POINT('Ctrl Pts',(-20.5199833626838,12.2212950286517,124.430776031763)) ;
#64967 = CARTESIAN_POINT('Ctrl Pts',(-20.2978478905724,12.0413059482889,124.22697474946)) ;
#64968 = CARTESIAN_POINT('Ctrl Pts',(-20.327174746647,12.2312557011542,124.607803018266)) ;
#64969 = CARTESIAN_POINT('Ctrl Pts',(-20.1436024451247,12.0512666207913,124.368597976752)) ;
#64970 = CARTESIAN_POINT('Ctrl Pts',(-20.1045650508631,12.241293772222,124.749310160051)) ;
#64971 = CARTESIAN_POINT('Ctrl Pts',(-19.9655159909283,12.0613046918591,124.48180549562)) ;
#64972 = CARTESIAN_POINT('Ctrl Pts',(-19.8649051459857,12.2511673871824,124.84884392232)) ;
#64973 = CARTESIAN_POINT('Ctrl Pts',(-19.7737886892284,12.0711783068196,124.561434593888)) ;
#64974 = CARTESIAN_POINT('Ctrl Pts',(-19.6065797304044,12.2612396217637,124.906300997495)) ;
#64975 = CARTESIAN_POINT('Ctrl Pts',(-19.5671291439869,12.0812505414008,124.607402358508)) ;
#64976 = CARTESIAN_POINT('Ctrl Pts',(-19.3486297183306,12.2710636402125,124.918040759663)) ;
#64977 = CARTESIAN_POINT('Ctrl Pts',(-19.3607684323741,12.0910745598496,124.616796316392)) ;
#64978 = CARTESIAN_POINT('Ctrl Pts',(-19.0863456687476,12.2811285611885,124.884353810211)) ;
#64979 = CARTESIAN_POINT('Ctrl Pts',(-19.1509427633031,12.1011394808256,124.589849001883)) ;
#64980 = CARTESIAN_POINT('Ctrl Pts',(-18.7548496615759,12.2943388594833,124.781008020348)) ;
#64981 = CARTESIAN_POINT('Ctrl Pts',(-18.8857366261165,12.1143497791204,124.507174493907)) ;
#64982 = CARTESIAN_POINT('Ctrl Pts',(-18.4555083325038,12.3076543062152,124.592460114452)) ;
#64983 = CARTESIAN_POINT('Ctrl Pts',(-18.646238230641,12.1276652258523,124.356312323164)) ;
#64984 = CARTESIAN_POINT('Ctrl Pts',(-18.2182158984291,12.3209445514825,124.336043204847)) ;
#64985 = CARTESIAN_POINT('Ctrl Pts',(-18.4564387255934,12.1409554711196,124.15121228678)) ;
#64986 = CARTESIAN_POINT('Ctrl Pts',(-18.0753697674858,12.3309953010896,124.113946532571)) ;
#64987 = CARTESIAN_POINT('Ctrl Pts',(-18.3421528585355,12.1510062207267,123.973529844557)) ;
#64988 = CARTESIAN_POINT('Ctrl Pts',(-17.9751686262583,12.3408079080718,123.876303265546)) ;
#64989 = CARTESIAN_POINT('Ctrl Pts',(-18.261991656828,12.160818827709,123.783417405138)) ;
#64990 = CARTESIAN_POINT('Ctrl Pts',(-17.9159132713503,12.3508790060661,123.61839959421)) ;
#64991 = CARTESIAN_POINT('Ctrl Pts',(-18.2145854546591,12.1708899257032,123.577093729689)) ;
#64992 = CARTESIAN_POINT('Ctrl Pts',(-17.9028470180164,12.360768578841,123.358821518713)) ;
#64993 = CARTESIAN_POINT('Ctrl Pts',(-18.2041287543014,12.1807794984781,123.369434895776)) ;
#64994 = CARTESIAN_POINT('Ctrl Pts',(-17.9449900324593,12.3740386856443,123.012644489447)) ;
#64995 = CARTESIAN_POINT('Ctrl Pts',(-18.2378495546872,12.1940496052814,123.092473752692)) ;
#64996 = CARTESIAN_POINT('Ctrl Pts',(-18.1100382420715,12.3906553725668,122.603018959482)) ;
#64997 = CARTESIAN_POINT('Ctrl Pts',(-18.3698647094851,12.2106662922039,122.764802568865)) ;
#64998 = CARTESIAN_POINT('Ctrl Pts',(-18.403953809166,12.407229415883,122.274921978595)) ;
#64999 = CARTESIAN_POINT('Ctrl Pts',(-18.6050396625321,12.2272403355201,122.502279805884)) ;
#65000 = CARTESIAN_POINT('Ctrl Pts',(-18.6963080999561,12.4205259833148,122.083501484983)) ;
#65001 = CARTESIAN_POINT('Ctrl Pts',(-18.838884457567,12.2405369029519,122.349174750329)) ;
#65002 = CARTESIAN_POINT('Ctrl Pts',(-18.9385791929077,12.4305560468922,121.979673523522)) ;
#65003 = CARTESIAN_POINT('Ctrl Pts',(-19.0327084258361,12.2505669665293,122.266104229579)) ;
#65004 = CARTESIAN_POINT('Ctrl Pts',(-19.1916818709481,12.4404499387414,121.920281628208)) ;
#65005 = CARTESIAN_POINT('Ctrl Pts',(-19.2351869221464,12.2604608583786,122.218590195066)) ;
#65006 = CARTESIAN_POINT('Ctrl Pts',(-19.5394009792638,12.453702694527,121.899549493621)) ;
#65007 = CARTESIAN_POINT('Ctrl Pts',(-19.5133723354866,12.2737136141641,122.202003998467)) ;
#65008 = CARTESIAN_POINT('Ctrl Pts',(-19.9747293753154,12.4704307995194,121.989564308867)) ;
#65009 = CARTESIAN_POINT('Ctrl Pts',(-19.8616245760486,12.2904417191566,122.274010791926)) ;
#65010 = CARTESIAN_POINT('Ctrl Pts',(-20.423556659189,12.4902616359979,122.266069036656)) ;
#65011 = CARTESIAN_POINT('Ctrl Pts',(-20.2206924545975,12.3102725556351,122.495213082915)) ;
#65012 = CARTESIAN_POINT('Ctrl Pts',(-20.7535327226879,12.5101870278881,122.680135635484)) ;
#65013 = CARTESIAN_POINT('Ctrl Pts',(-20.4846749563749,12.3301979475252,122.826464874533)) ;
#65014 = CARTESIAN_POINT('Ctrl Pts',(-20.9224041261077,12.5301122412401,123.18215712058)) ;
#65015 = CARTESIAN_POINT('Ctrl Pts',(-20.6197750512931,12.3501231608772,123.228081791924)) ;
#65016 = CARTESIAN_POINT('Ctrl Pts',(-20.9099617273115,12.5500372547252,123.711523704258)) ;
#65017 = CARTESIAN_POINT('Ctrl Pts',(-20.6098235773023,12.3700481743623,123.651575730201)) ;
#65018 = CARTESIAN_POINT('Ctrl Pts',(-20.7187360422604,12.5699137264252,124.204018044716)) ;
#65019 = CARTESIAN_POINT('Ctrl Pts',(-20.4568446351546,12.3899246460623,124.045573021246)) ;
#65020 = CARTESIAN_POINT('Ctrl Pts',(-20.3693300643289,12.5898930443341,124.603877601687)) ;
#65021 = CARTESIAN_POINT('Ctrl Pts',(-20.1773211406971,12.4099039639712,124.365462064758)) ;
#65022 = CARTESIAN_POINT('Ctrl Pts',(-19.9052905888142,12.6098260479101,124.859582769263)) ;
#65023 = CARTESIAN_POINT('Ctrl Pts',(-19.8060899284359,12.4298369675472,124.570028153243)) ;
#65024 = CARTESIAN_POINT('Ctrl Pts',(-19.3829989743676,12.6297213179378,124.941977004567)) ;
#65025 = CARTESIAN_POINT('Ctrl Pts',(-19.388255790433,12.4497322375749,124.635945220169)) ;
#65026 = CARTESIAN_POINT('Ctrl Pts',(-18.8631060156455,12.6496426558436,124.841587523865)) ;
#65027 = CARTESIAN_POINT('Ctrl Pts',(-18.9723403696999,12.4696535754807,124.555634564112)) ;
#65028 = CARTESIAN_POINT('Ctrl Pts',(-18.4079042835162,12.6696002791098,124.569214868981)) ;
#65029 = CARTESIAN_POINT('Ctrl Pts',(-18.6081780879779,12.4896111987469,124.337737060207)) ;
#65030 = CARTESIAN_POINT('Ctrl Pts',(-18.0742532724176,12.689480111067,124.15962015315)) ;
#65031 = CARTESIAN_POINT('Ctrl Pts',(-18.3412557256098,12.5094910307041,124.010060596195)) ;
#65032 = CARTESIAN_POINT('Ctrl Pts',(-17.8989480657597,12.7093619623639,123.661012507451)) ;
#65033 = CARTESIAN_POINT('Ctrl Pts',(-18.2010112129469,12.529372882001,123.611173006021)) ;
#65034 = CARTESIAN_POINT('Ctrl Pts',(-17.9053743363839,12.7294329794677,123.127663535506)) ;
#65035 = CARTESIAN_POINT('Ctrl Pts',(-18.206152086956,12.5494438991048,123.184494766924)) ;
#65036 = CARTESIAN_POINT('Ctrl Pts',(-18.0909224032866,12.7492402032208,122.634900991628)) ;
#65037 = CARTESIAN_POINT('Ctrl Pts',(-18.3545915317239,12.5692511228579,122.79028245245)) ;
#65038 = CARTESIAN_POINT('Ctrl Pts',(-18.4354537167374,12.7692213387896,122.230824135122)) ;
#65039 = CARTESIAN_POINT('Ctrl Pts',(-18.630217413786,12.5892322584267,122.467021418923)) ;
#65040 = CARTESIAN_POINT('Ctrl Pts',(-18.8964641846084,12.7891488321288,121.970176160961)) ;
#65041 = CARTESIAN_POINT('Ctrl Pts',(-18.9990268654917,12.6091597517659,122.258503153768)) ;
#65042 = CARTESIAN_POINT('Ctrl Pts',(-19.415834432645,12.8089694934866,121.881151656097)) ;
#65043 = CARTESIAN_POINT('Ctrl Pts',(-19.4145251819836,12.6289804131237,122.187284802725)) ;
#65044 = CARTESIAN_POINT('Ctrl Pts',(-19.9411566590933,12.8290666827084,121.976780870031)) ;
#65045 = CARTESIAN_POINT('Ctrl Pts',(-19.8347817388246,12.6490776023455,122.26378939332)) ;
#65046 = CARTESIAN_POINT('Ctrl Pts',(-20.3952240684518,12.8488303617167,122.241384544964)) ;
#65047 = CARTESIAN_POINT('Ctrl Pts',(-20.1980368260556,12.6688412813539,122.475474968688)) ;
#65048 = CARTESIAN_POINT('Ctrl Pts',(-20.7368987004041,12.8688876403898,122.650278783027)) ;
#65049 = CARTESIAN_POINT('Ctrl Pts',(-20.471374567732,12.6888985600269,122.802591330888)) ;
#65050 = CARTESIAN_POINT('Ctrl Pts',(-20.915999998585,12.8886830641372,123.145136393717)) ;
#65051 = CARTESIAN_POINT('Ctrl Pts',(-20.6146542216816,12.7086939837743,123.198479843696)) ;
#65052 = CARTESIAN_POINT('Ctrl Pts',(-20.9171224626081,12.9086467088648,123.675675466344)) ;
#65053 = CARTESIAN_POINT('Ctrl Pts',(-20.6155493596477,12.7286576285019,123.62291137376)) ;
#65054 = CARTESIAN_POINT('Ctrl Pts',(-20.7357148689362,12.9286302001389,124.174870580485)) ;
#65055 = CARTESIAN_POINT('Ctrl Pts',(-20.4704208498852,12.748641119776,124.022266714748)) ;
#65056 = CARTESIAN_POINT('Ctrl Pts',(-20.3986521463145,12.9484376952882,124.579332558867)) ;
#65057 = CARTESIAN_POINT('Ctrl Pts',(-20.2007674929157,12.7684486149253,124.345835452123)) ;
#65058 = CARTESIAN_POINT('Ctrl Pts',(-19.9402235763069,12.9684202860083,124.847283742868)) ;
#65059 = CARTESIAN_POINT('Ctrl Pts',(-19.8340229155712,12.7884312056454,124.560193612836)) ;
#65060 = CARTESIAN_POINT('Ctrl Pts',(-19.4202416053834,12.9883029399995,124.942191223807)) ;
#65061 = CARTESIAN_POINT('Ctrl Pts',(-19.4180360713643,12.8083138596367,124.636116448561)) ;
#65062 = CARTESIAN_POINT('Ctrl Pts',(-18.8972653738817,13.0082611848626,124.854056149815)) ;
#65063 = CARTESIAN_POINT('Ctrl Pts',(-18.9996554343786,12.8282721044997,124.565604873839)) ;
#65064 = CARTESIAN_POINT('Ctrl Pts',(-18.4373467193133,13.0281367719042,124.594021898923)) ;
#65065 = CARTESIAN_POINT('Ctrl Pts',(-18.6317218256589,12.8481476915413,124.357573939608)) ;
#65066 = CARTESIAN_POINT('Ctrl Pts',(-18.0917408140289,13.0481176600395,124.190855292359)) ;
#65067 = CARTESIAN_POINT('Ctrl Pts',(-18.355239878661,12.8681285796766,124.035038248343)) ;
#65068 = CARTESIAN_POINT('Ctrl Pts',(-17.9052414355018,13.0680528011505,123.694844185524)) ;
#65069 = CARTESIAN_POINT('Ctrl Pts',(-18.2060442903282,12.8880637207876,123.63822733448)) ;
#65070 = CARTESIAN_POINT('Ctrl Pts',(-17.8988271166947,13.0879648191615,123.165702838927)) ;
#65071 = CARTESIAN_POINT('Ctrl Pts',(-18.200915253109,12.9079757387987,123.21491552465)) ;
#65072 = CARTESIAN_POINT('Ctrl Pts',(-18.072637630343,13.1078530374051,122.666485551976)) ;
#65073 = CARTESIAN_POINT('Ctrl Pts',(-18.3399734826579,12.9278639570422,122.815536572551)) ;
#65074 = CARTESIAN_POINT('Ctrl Pts',(-18.3508356377982,13.124451341252,122.324166060085)) ;
#65075 = CARTESIAN_POINT('Ctrl Pts',(-18.562516670019,12.9444622608891,122.54170220006)) ;
#65076 = CARTESIAN_POINT('Ctrl Pts',(-18.6332461345771,13.1377239311548,122.119417599801)) ;
#65077 = CARTESIAN_POINT('Ctrl Pts',(-18.7884633789187,12.957734850792,122.37788874013)) ;
#65078 = CARTESIAN_POINT('Ctrl Pts',(-18.8696106143661,13.1477313461057,122.004127651261)) ;
#65079 = CARTESIAN_POINT('Ctrl Pts',(-18.9775498041114,12.9677422657428,122.285661949653)) ;
#65080 = CARTESIAN_POINT('Ctrl Pts',(-19.1224757065835,13.1577386928383,121.931849416177)) ;
#65081 = CARTESIAN_POINT('Ctrl Pts',(-19.1798541601348,12.9777496124754,122.22784121804)) ;
#65082 = CARTESIAN_POINT('Ctrl Pts',(-19.4692111889447,13.1710050526399,121.895476582139)) ;
#65083 = CARTESIAN_POINT('Ctrl Pts',(-19.4571883101494,12.991015972277,122.198742524881)) ;
#65084 = CARTESIAN_POINT('Ctrl Pts',(-19.9027886653172,13.1875197102629,121.963391453896)) ;
#65085 = CARTESIAN_POINT('Ctrl Pts',(-19.8041192330616,13.0075306299,122.253086454829)) ;
#65086 = CARTESIAN_POINT('Ctrl Pts',(-20.2896179416635,13.2041171435055,122.175375538865)) ;
#65087 = CARTESIAN_POINT('Ctrl Pts',(-20.1135332169725,13.0241280631426,122.422657930658)) ;
#65088 = CARTESIAN_POINT('Ctrl Pts',(-20.5428541366256,13.2174651406505,122.418153018463)) ;
#65089 = CARTESIAN_POINT('Ctrl Pts',(-20.3161488901095,13.0374760602876,122.61689817093)) ;
#65090 = CARTESIAN_POINT('Ctrl Pts',(-20.6967627804406,13.2273608950021,122.62776755716)) ;
#65091 = CARTESIAN_POINT('Ctrl Pts',(-20.4392682594011,13.0473718146392,122.784587934019)) ;
#65092 = CARTESIAN_POINT('Ctrl Pts',(-20.8132896637095,13.2373488489335,122.862934128972)) ;
#65093 = CARTESIAN_POINT('Ctrl Pts',(-20.5324892841562,13.0573597685706,122.972723020215)) ;
#65094 = CARTESIAN_POINT('Ctrl Pts',(-20.887111769064,13.2473060726382,123.114002366625)) ;
#65095 = CARTESIAN_POINT('Ctrl Pts',(-20.591544390908,13.0673169922753,123.17357799442)) ;
#65096 = CARTESIAN_POINT('Ctrl Pts',(-20.9163194697392,13.2573416191949,123.376085199788)) ;
#65097 = CARTESIAN_POINT('Ctrl Pts',(-20.6149084219131,13.077352538832,123.383244498507)) ;
#65098 = CARTESIAN_POINT('Ctrl Pts',(-20.9000197111728,13.267228730471,123.635413520908)) ;
#65099 = CARTESIAN_POINT('Ctrl Pts',(-20.6018663387177,13.0872396501081,123.590707013406)) ;
#65100 = CARTESIAN_POINT('Ctrl Pts',(-20.8387093067046,13.2772201355718,123.890705618829)) ;
#65101 = CARTESIAN_POINT('Ctrl Pts',(-20.5528158398965,13.0972310552089,123.794940111806)) ;
#65102 = CARTESIAN_POINT('Ctrl Pts',(-20.7344045824693,13.2871657567866,124.130350209159)) ;
#65103 = CARTESIAN_POINT('Ctrl Pts',(-20.4693700045889,13.1071766764237,123.986654845543)) ;
#65104 = CARTESIAN_POINT('Ctrl Pts',(-20.5904556480587,13.2971150050549,124.348628887742)) ;
#65105 = CARTESIAN_POINT('Ctrl Pts',(-20.3542090074305,13.117125924692,124.161276491165)) ;
#65106 = CARTESIAN_POINT('Ctrl Pts',(-20.4088310489179,13.3071615002235,124.540222615066)) ;
#65107 = CARTESIAN_POINT('Ctrl Pts',(-20.208907719291,13.1271724198607,124.314549885357)) ;
#65108 = CARTESIAN_POINT('Ctrl Pts',(-20.2009526790891,13.3170128430151,124.69453910851)) ;
#65109 = CARTESIAN_POINT('Ctrl Pts',(-20.0426037537448,13.1370237626522,124.438001210113)) ;
#65110 = CARTESIAN_POINT('Ctrl Pts',(-19.9669434550335,13.3269846231424,124.812406349802)) ;
#65111 = CARTESIAN_POINT('Ctrl Pts',(-19.85539544562,13.1469955427795,124.532292952135)) ;
#65112 = CARTESIAN_POINT('Ctrl Pts',(-19.7153564891379,13.3369798231201,124.888022808457)) ;
#65113 = CARTESIAN_POINT('Ctrl Pts',(-19.6541252878157,13.1569907427572,124.592783951486)) ;
#65114 = CARTESIAN_POINT('Ctrl Pts',(-19.4534753611638,13.3470138148161,124.918598821052)) ;
#65115 = CARTESIAN_POINT('Ctrl Pts',(-19.4446201537456,13.1670247344533,124.617242515926)) ;
#65116 = CARTESIAN_POINT('Ctrl Pts',(-19.1948766730221,13.3568692197886,124.903920505576)) ;
#65117 = CARTESIAN_POINT('Ctrl Pts',(-19.2377415186523,13.1768801394258,124.605497635822)) ;
#65118 = CARTESIAN_POINT('Ctrl Pts',(-18.9390603846793,13.3668685176344,124.844062381727)) ;
#65119 = CARTESIAN_POINT('Ctrl Pts',(-19.0330890674642,13.1868794372715,124.557608978315)) ;
#65120 = CARTESIAN_POINT('Ctrl Pts',(-18.6998481883594,13.3767636302396,124.741995186928)) ;
#65121 = CARTESIAN_POINT('Ctrl Pts',(-18.8417203716604,13.1967745498767,124.475953269536)) ;
#65122 = CARTESIAN_POINT('Ctrl Pts',(-18.4784292945889,13.3868242757746,124.597585675323)) ;
#65123 = CARTESIAN_POINT('Ctrl Pts',(-18.6645864484423,13.2068351954117,124.360423788125)) ;
#65124 = CARTESIAN_POINT('Ctrl Pts',(-18.2893688821215,13.3966731527638,124.420799145494)) ;
#65125 = CARTESIAN_POINT('Ctrl Pts',(-18.5133398551408,13.2166840724009,124.218993165454)) ;
#65126 = CARTESIAN_POINT('Ctrl Pts',(-18.1305208053495,13.4067018638574,124.210511784196)) ;
#65127 = CARTESIAN_POINT('Ctrl Pts',(-18.3862631410708,13.2267127834945,124.050761997541)) ;
#65128 = CARTESIAN_POINT('Ctrl Pts',(-18.0112247910287,13.4167312651135,123.975488167396)) ;
#65129 = CARTESIAN_POINT('Ctrl Pts',(-18.2908283055355,13.2367421847506,123.862742104803)) ;
#65130 = CARTESIAN_POINT('Ctrl Pts',(-17.9354445009214,13.4265714569095,123.72824647118)) ;
#65131 = CARTESIAN_POINT('Ctrl Pts',(-18.2302062650651,13.2465823765466,123.664948483144)) ;
#65132 = CARTESIAN_POINT('Ctrl Pts',(-17.9027395319079,13.4365748861025,123.467435684465)) ;
#65133 = CARTESIAN_POINT('Ctrl Pts',(-18.2040444166883,13.2565858057396,123.456299663574)) ;
#65134 = CARTESIAN_POINT('Ctrl Pts',(-17.9158814573718,13.4465603985687,123.205311390375)) ;
#65135 = CARTESIAN_POINT('Ctrl Pts',(-18.2145600879431,13.2665713182058,123.24660043712)) ;
#65136 = CARTESIAN_POINT('Ctrl Pts',(-17.9749065837832,13.4566014949527,122.948155155583)) ;
#65137 = CARTESIAN_POINT('Ctrl Pts',(-18.2617823053095,13.2766124145898,123.040875912254)) ;
#65138 = CARTESIAN_POINT('Ctrl Pts',(-18.0753470360815,13.4664446909037,122.709757985454)) ;
#65139 = CARTESIAN_POINT('Ctrl Pts',(-18.3421364530239,13.2864556105408,122.850159423479)) ;
#65140 = CARTESIAN_POINT('Ctrl Pts',(-18.217218281521,13.4764310019581,122.489035231126)) ;
#65141 = CARTESIAN_POINT('Ctrl Pts',(-18.455635132101,13.2964419215952,122.673582454515)) ;
#65142 = CARTESIAN_POINT('Ctrl Pts',(-18.3942732512551,13.4863656872158,122.297106419642)) ;
#65143 = CARTESIAN_POINT('Ctrl Pts',(-18.5972804423146,13.3063766068529,122.520040993049)) ;
#65144 = CARTESIAN_POINT('Ctrl Pts',(-18.6046031877743,13.4964232484328,122.137116873894)) ;
#65145 = CARTESIAN_POINT('Ctrl Pts',(-18.7655457306992,13.31643416807,122.392050961701)) ;
#65146 = CARTESIAN_POINT('Ctrl Pts',(-18.8338850495127,13.5062448900414,122.018535713195)) ;
#65147 = CARTESIAN_POINT('Ctrl Pts',(-18.9489715980104,13.3262558096786,122.297188133943)) ;
#65148 = CARTESIAN_POINT('Ctrl Pts',(-19.0859583258846,13.5163009536324,121.939273611562)) ;
#65149 = CARTESIAN_POINT('Ctrl Pts',(-19.1506308986353,13.3363118732695,122.233780316748)) ;
#65150 = CARTESIAN_POINT('Ctrl Pts',(-19.3450516698222,13.5262416293942,121.905839973782)) ;
#65151 = CARTESIAN_POINT('Ctrl Pts',(-19.3579055692691,13.3462525490313,122.207035465221)) ;
#65152 = CARTESIAN_POINT('Ctrl Pts',(-19.6050909750196,13.5361459881825,121.917041144644)) ;
#65153 = CARTESIAN_POINT('Ctrl Pts',(-19.565936503742,13.3561569078197,122.215998316432)) ;
#65154 = CARTESIAN_POINT('Ctrl Pts',(-19.862825851585,13.5461926427583,121.97418792217)) ;
#65155 = CARTESIAN_POINT('Ctrl Pts',(-19.7721240620941,13.3662035623955,122.261717666906)) ;
#65156 = CARTESIAN_POINT('Ctrl Pts',(-20.1031997643857,13.5560882374012,122.073508487898)) ;
#65157 = CARTESIAN_POINT('Ctrl Pts',(-19.9644220277355,13.3760991570383,122.341175720192)) ;
#65158 = CARTESIAN_POINT('Ctrl Pts',(-20.3263218440362,13.5661501840581,122.215343672236)) ;
#65159 = CARTESIAN_POINT('Ctrl Pts',(-20.1429187779707,13.3861611036952,122.454645564345)) ;
#65160 = CARTESIAN_POINT('Ctrl Pts',(-20.5173749645332,13.5759998079902,122.38999462014)) ;
#65161 = CARTESIAN_POINT('Ctrl Pts',(-20.295759491306,13.3960107276274,122.594367286313)) ;
#65162 = CARTESIAN_POINT('Ctrl Pts',(-20.6776884554839,13.5859630470201,122.596980439567)) ;
#65163 = CARTESIAN_POINT('Ctrl Pts',(-20.4240087199095,13.4059739666572,122.759956837706)) ;
#65164 = CARTESIAN_POINT('Ctrl Pts',(-20.8000704181908,13.5959876217959,122.830280403309)) ;
#65165 = CARTESIAN_POINT('Ctrl Pts',(-20.5219126738478,13.415998541433,122.946597684399)) ;
#65166 = CARTESIAN_POINT('Ctrl Pts',(-20.8793920083737,13.6059061844836,123.07855998187)) ;
#65167 = CARTESIAN_POINT('Ctrl Pts',(-20.5853680842003,13.4259171041207,123.145221485307)) ;
#65168 = CARTESIAN_POINT('Ctrl Pts',(-20.9151199375489,13.6158983712076,123.338717822216)) ;
#65169 = CARTESIAN_POINT('Ctrl Pts',(-20.6139486858676,13.4359092908447,123.353347860863)) ;
#65170 = CARTESIAN_POINT('Ctrl Pts',(-20.9046168525977,13.6259331697918,123.6022019633)) ;
#65171 = CARTESIAN_POINT('Ctrl Pts',(-20.605544399225,13.4459440894289,123.564135168279)) ;
#65172 = CARTESIAN_POINT('Ctrl Pts',(-20.8499556627768,13.6357883604655,123.855372966742)) ;
#65173 = CARTESIAN_POINT('Ctrl Pts',(-20.5618138995585,13.4557992801026,123.766670884377)) ;
#65174 = CARTESIAN_POINT('Ctrl Pts',(-20.7510855573927,13.6457877086185,124.098788324435)) ;
#65175 = CARTESIAN_POINT('Ctrl Pts',(-20.4827162949927,13.4657986282556,123.961402436991)) ;
#65176 = CARTESIAN_POINT('Ctrl Pts',(-20.6130996723433,13.6556828342936,124.319242233489)) ;
#65177 = CARTESIAN_POINT('Ctrl Pts',(-20.3723265173656,13.4756937539307,124.137764200893)) ;
#65178 = CARTESIAN_POINT('Ctrl Pts',(-20.4360519660016,13.6657433772417,124.515540628893)) ;
#65179 = CARTESIAN_POINT('Ctrl Pts',(-20.2306870063593,13.4857542968788,124.294801963191)) ;
#65180 = CARTESIAN_POINT('Ctrl Pts',(-20.2320341456861,13.6755926515086,124.674850714962)) ;
#65181 = CARTESIAN_POINT('Ctrl Pts',(-20.0674724171004,13.4956035711457,124.422248249584)) ;
#65182 = CARTESIAN_POINT('Ctrl Pts',(-19.9996623311131,13.6856198760785,124.799086161189)) ;
#65183 = CARTESIAN_POINT('Ctrl Pts',(-19.8815742380617,13.5056307957156,124.521635311594)) ;
#65184 = CARTESIAN_POINT('Ctrl Pts',(-19.7489854254844,13.6956482752663,124.880448501815)) ;
#65185 = CARTESIAN_POINT('Ctrl Pts',(-19.6810321616281,13.5156591949034,124.586723663228)) ;
#65186 = CARTESIAN_POINT('Ctrl Pts',(-19.4928401900497,13.7054940256798,124.916853671087)) ;
#65187 = CARTESIAN_POINT('Ctrl Pts',(-19.4761166444092,13.5255049453169,124.615846163914)) ;
#65188 = CARTESIAN_POINT('Ctrl Pts',(-19.230454887784,13.7154828160805,124.908839488335)) ;
#65189 = CARTESIAN_POINT('Ctrl Pts',(-19.2662086080236,13.5354937357177,124.609433445062)) ;
#65190 = CARTESIAN_POINT('Ctrl Pts',(-18.9721627761797,13.7255277444802,124.854438840815)) ;
#65191 = CARTESIAN_POINT('Ctrl Pts',(-19.0595750986044,13.5455386641174,124.565911420256)) ;
#65192 = CARTESIAN_POINT('Ctrl Pts',(-18.7323658376547,13.7353522292692,124.758724681303)) ;
#65193 = CARTESIAN_POINT('Ctrl Pts',(-18.8677390346098,13.5553631489063,124.489339193207)) ;
#65194 = CARTESIAN_POINT('Ctrl Pts',(-18.507457139982,13.7454096268104,124.619951807237)) ;
#65195 = CARTESIAN_POINT('Ctrl Pts',(-18.6878125850875,13.5654205464475,124.378319667226)) ;
#65196 = CARTESIAN_POINT('Ctrl Pts',(-18.3128349524813,13.7553357183966,124.44624656969)) ;
#65197 = CARTESIAN_POINT('Ctrl Pts',(-18.5321161260099,13.5753466380337,124.239354778128)) ;
#65198 = CARTESIAN_POINT('Ctrl Pts',(-18.1503452309715,13.7652905035412,124.241231958245)) ;
#65199 = CARTESIAN_POINT('Ctrl Pts',(-18.4021255453027,13.5853014231783,124.075342601526)) ;
#65200 = CARTESIAN_POINT('Ctrl Pts',(-18.0251465109341,13.7753278731988,124.009068223143)) ;
#65201 = CARTESIAN_POINT('Ctrl Pts',(-18.3019676694534,13.5953387928359,123.889610906895)) ;
#65202 = CARTESIAN_POINT('Ctrl Pts',(-17.9431959784106,13.7852166833204,123.762452941019)) ;
#65203 = CARTESIAN_POINT('Ctrl Pts',(-18.2364086692508,13.6052276029575,123.692318981433)) ;
#65204 = CARTESIAN_POINT('Ctrl Pts',(-17.9044614031139,13.7952060423715,123.502822293364)) ;
#65205 = CARTESIAN_POINT('Ctrl Pts',(-18.2054221786113,13.6152169620086,123.484614462953)) ;
#65206 = CARTESIAN_POINT('Ctrl Pts',(-17.9115693386521,13.8051645898276,123.241226463732)) ;
#65207 = CARTESIAN_POINT('Ctrl Pts',(-18.2111097180374,13.6251755094647,123.275338178328)) ;
#65208 = CARTESIAN_POINT('Ctrl Pts',(-17.9630567197968,13.8150641663786,122.986205100608)) ;
#65209 = CARTESIAN_POINT('Ctrl Pts',(-18.2523005182494,13.6350750860157,123.071321986717)) ;
#65210 = CARTESIAN_POINT('Ctrl Pts',(-18.0595361492998,13.8251120782093,122.740443216478)) ;
#65211 = CARTESIAN_POINT('Ctrl Pts',(-18.329485128724,13.6451229978464,122.874712710548)) ;
#65212 = CARTESIAN_POINT('Ctrl Pts',(-18.1949930036132,13.8350074260699,122.518422190268)) ;
#65213 = CARTESIAN_POINT('Ctrl Pts',(-18.4378511109109,13.655018345707,122.697097049966)) ;
#65214 = CARTESIAN_POINT('Ctrl Pts',(-18.3697572977927,13.845069102601,122.320042659935)) ;
#65215 = CARTESIAN_POINT('Ctrl Pts',(-18.5776634866624,13.6650800222382,122.538393906198)) ;
#65216 = CARTESIAN_POINT('Ctrl Pts',(-18.5718588198519,13.8549136203502,122.158525512922)) ;
#65217 = CARTESIAN_POINT('Ctrl Pts',(-18.7393445112275,13.6749245399873,122.409181641225)) ;
#65218 = CARTESIAN_POINT('Ctrl Pts',(-18.8011469810602,13.864874064065,122.032284729829)) ;
#65219 = CARTESIAN_POINT('Ctrl Pts',(-18.9227751038679,13.6848849837021,122.308189886519)) ;
#65220 = CARTESIAN_POINT('Ctrl Pts',(-19.0509301231226,13.8749108968832,121.947590007007)) ;
#65221 = CARTESIAN_POINT('Ctrl Pts',(-19.1226020288338,13.6949218165203,122.240434931693)) ;
#65222 = CARTESIAN_POINT('Ctrl Pts',(-19.3074865101994,13.88478969363,121.907757156992)) ;
#65223 = CARTESIAN_POINT('Ctrl Pts',(-19.3278463927919,13.7048006132671,122.208569584531)) ;
#65224 = CARTESIAN_POINT('Ctrl Pts',(-19.5717537455678,13.8948490097584,121.91308802529)) ;
#65225 = CARTESIAN_POINT('Ctrl Pts',(-19.5392604248098,13.7148599293955,122.212835072421)) ;
#65226 = CARTESIAN_POINT('Ctrl Pts',(-19.8262549511952,13.9047194565116,121.963266910915)) ;
#65227 = CARTESIAN_POINT('Ctrl Pts',(-19.7428603300386,13.7247303761487,122.252978777756)) ;
#65228 = CARTESIAN_POINT('Ctrl Pts',(-20.0714142577279,13.9147120947696,122.057363864517)) ;
#65229 = CARTESIAN_POINT('Ctrl Pts',(-19.9389874113429,13.7347230144067,122.328256860103)) ;
#65230 = CARTESIAN_POINT('Ctrl Pts',(-20.2970965036502,13.9247441103175,122.193613633218)) ;
#65231 = CARTESIAN_POINT('Ctrl Pts',(-20.1195328981886,13.7447550299547,122.437257373362)) ;
#65232 = CARTESIAN_POINT('Ctrl Pts',(-20.4928009018349,13.9346099666241,122.363706237578)) ;
#65233 = CARTESIAN_POINT('Ctrl Pts',(-20.2760952675698,13.7546208862612,122.573331276944)) ;
#65234 = CARTESIAN_POINT('Ctrl Pts',(-20.6593476164435,13.9446792560932,122.569291069351)) ;
#65235 = CARTESIAN_POINT('Ctrl Pts',(-20.4093323747788,13.7646901757304,122.737799786026)) ;
#65236 = CARTESIAN_POINT('Ctrl Pts',(-20.7848399902421,13.9545228136445,122.795508554596)) ;
#65237 = CARTESIAN_POINT('Ctrl Pts',(-20.509725196703,13.7745337332817,122.91877307958)) ;
#65238 = CARTESIAN_POINT('Ctrl Pts',(-20.871120064522,13.9645029404324,123.043168459414)) ;
#65239 = CARTESIAN_POINT('Ctrl Pts',(-20.578748805291,13.7845138600695,123.116900896814)) ;
#65240 = CARTESIAN_POINT('Ctrl Pts',(-20.9127502836893,13.9745214890323,123.303126129535)) ;
#65241 = CARTESIAN_POINT('Ctrl Pts',(-20.6120524706176,13.7945324086694,123.324867123436)) ;
#65242 = CARTESIAN_POINT('Ctrl Pts',(-20.9092186327094,13.9844047895555,123.562857078074)) ;
#65243 = CARTESIAN_POINT('Ctrl Pts',(-20.609226783806,13.8044157091926,123.532650998994)) ;
#65244 = CARTESIAN_POINT('Ctrl Pts',(-20.8596340362664,13.9944730766036,123.822708783211)) ;
#65245 = CARTESIAN_POINT('Ctrl Pts',(-20.5695586439728,13.8144839962408,123.740532609343)) ;
#65246 = CARTESIAN_POINT('Ctrl Pts',(-20.7681595371697,14.0043031996223,124.064344085627)) ;
#65247 = CARTESIAN_POINT('Ctrl Pts',(-20.4963791721871,13.8243141192594,123.933839581481)) ;
#65248 = CARTESIAN_POINT('Ctrl Pts',(-20.6332814623007,14.0143697835476,124.291865630646)) ;
#65249 = CARTESIAN_POINT('Ctrl Pts',(-20.3884763385761,13.8343807031847,124.11585696606)) ;
#65250 = CARTESIAN_POINT('Ctrl Pts',(-20.4637992773007,14.0242598965621,124.488951781943)) ;
#65251 = CARTESIAN_POINT('Ctrl Pts',(-20.2528909214938,13.8442708161992,124.273525063999)) ;
#65252 = CARTESIAN_POINT('Ctrl Pts',(-20.2609821100153,14.0342525853247,124.655717889191)) ;
#65253 = CARTESIAN_POINT('Ctrl Pts',(-20.090637223389,13.8542635049618,124.406937730911)) ;
#65254 = CARTESIAN_POINT('Ctrl Pts',(-20.0328972096088,14.0442134736805,124.784181661414)) ;
#65255 = CARTESIAN_POINT('Ctrl Pts',(-19.9081695446619,13.8642243933176,124.509708392774)) ;
#65256 = CARTESIAN_POINT('Ctrl Pts',(-19.7872119388903,14.0541314185605,124.87112949854)) ;
#65257 = CARTESIAN_POINT('Ctrl Pts',(-19.7116219327022,13.8741423381976,124.579266367016)) ;
#65258 = CARTESIAN_POINT('Ctrl Pts',(-19.527842932523,14.0641391716567,124.914794637581)) ;
#65259 = CARTESIAN_POINT('Ctrl Pts',(-19.5041267743093,13.8841500912938,124.614198467582)) ;
#65260 = CARTESIAN_POINT('Ctrl Pts',(-19.2642632651857,14.0741702656157,124.912222739613)) ;
#65261 = CARTESIAN_POINT('Ctrl Pts',(-19.2932629428853,13.8941811852529,124.612140811124)) ;
#65262 = CARTESIAN_POINT('Ctrl Pts',(-19.0097259981526,14.0840182336437,124.865371406458)) ;
#65263 = CARTESIAN_POINT('Ctrl Pts',(-19.0896342385044,13.9040291532808,124.57465995883)) ;
#65264 = CARTESIAN_POINT('Ctrl Pts',(-18.7618772164016,14.0940801897696,124.773301901415)) ;
#65265 = CARTESIAN_POINT('Ctrl Pts',(-18.89135492329,13.9140911094067,124.501004319296)) ;
#65266 = CARTESIAN_POINT('Ctrl Pts',(-18.5376101429091,14.1039774013707,124.641559789166)) ;
#65267 = CARTESIAN_POINT('Ctrl Pts',(-18.7119419501136,13.9239883210078,124.395611039838)) ;
#65268 = CARTESIAN_POINT('Ctrl Pts',(-18.3384000135968,14.1139085680353,124.472965869001)) ;
#65269 = CARTESIAN_POINT('Ctrl Pts',(-18.5525741413936,13.9339194876725,124.26073644889)) ;
#65270 = CARTESIAN_POINT('Ctrl Pts',(-18.169843513441,14.1239507522395,124.269917095288)) ;
#65271 = CARTESIAN_POINT('Ctrl Pts',(-18.4177287173971,13.9439616718766,124.098297399059)) ;
#65272 = CARTESIAN_POINT('Ctrl Pts',(-18.0409566998773,14.1338374204927,124.044314253981)) ;
#65273 = CARTESIAN_POINT('Ctrl Pts',(-18.3146195241724,13.9538483401298,123.91781597991)) ;
#65274 = CARTESIAN_POINT('Ctrl Pts',(-17.9518498698231,14.1438305324709,123.797299870393)) ;
#65275 = CARTESIAN_POINT('Ctrl Pts',(-18.2433338227016,13.963841452108,123.720204732081)) ;
#65276 = CARTESIAN_POINT('Ctrl Pts',(-17.9072936184703,14.1537762100867,123.539763194409)) ;
#65277 = CARTESIAN_POINT('Ctrl Pts',(-18.2076886217236,13.9737871297239,123.514175908959)) ;
#65278 = CARTESIAN_POINT('Ctrl Pts',(-17.9075982211722,14.1637235130717,123.278346044345)) ;
#65279 = CARTESIAN_POINT('Ctrl Pts',(-18.2079318833263,13.9837344327088,123.305042647858)) ;
#65280 = CARTESIAN_POINT('Ctrl Pts',(-17.9540338467725,14.1737712368185,123.018424649771)) ;
#65281 = CARTESIAN_POINT('Ctrl Pts',(-18.245080078658,13.9937821564556,123.097105274778)) ;
#65282 = CARTESIAN_POINT('Ctrl Pts',(-18.0429036250617,14.183619610581,122.775359841272)) ;
#65283 = CARTESIAN_POINT('Ctrl Pts',(-18.3161751445601,14.0036305302181,122.90265434045)) ;
#65284 = CARTESIAN_POINT('Ctrl Pts',(-18.1733306008267,14.1935785830267,122.54846390798)) ;
#65285 = CARTESIAN_POINT('Ctrl Pts',(-18.4205160052355,14.0135895026638,122.721137613016)) ;
#65286 = CARTESIAN_POINT('Ctrl Pts',(-18.3428801887918,14.2036174449079,122.346364098552)) ;
#65287 = CARTESIAN_POINT('Ctrl Pts',(-18.5561553752817,14.023628364545,122.559457349719)) ;
#65288 = CARTESIAN_POINT('Ctrl Pts',(-18.5414813532127,14.2134960490797,122.179140432255)) ;
#65289 = CARTESIAN_POINT('Ctrl Pts',(-18.7150352359828,14.0335069687168,122.425678533261)) ;
#65290 = CARTESIAN_POINT('Ctrl Pts',(-18.7699215575239,14.223547590283,122.046595739492)) ;
#65291 = CARTESIAN_POINT('Ctrl Pts',(-18.8977872771299,14.0435585099201,122.319642127634)) ;
#65292 = CARTESIAN_POINT('Ctrl Pts',(-19.0141015690712,14.2334429882633,121.957035255779)) ;
#65293 = CARTESIAN_POINT('Ctrl Pts',(-19.0931303423171,14.0534539079004,122.247993398259)) ;
#65294 = CARTESIAN_POINT('Ctrl Pts',(-19.2740491001981,14.2434942208086,121.910385335695)) ;
#65295 = CARTESIAN_POINT('Ctrl Pts',(-19.3010884541272,14.0635051404457,122.210672757379)) ;
#65296 = CARTESIAN_POINT('Ctrl Pts',(-19.5338747027506,14.2533804114329,121.909562985904)) ;
#65297 = CARTESIAN_POINT('Ctrl Pts',(-19.5089480881137,14.07339133107,122.210014195614)) ;
#65298 = CARTESIAN_POINT('Ctrl Pts',(-19.7926811889532,14.2633729507487,121.953859464746)) ;
#65299 = CARTESIAN_POINT('Ctrl Pts',(-19.7159932556982,14.0833838703858,122.245450559124)) ;
#65300 = CARTESIAN_POINT('Ctrl Pts',(-20.0387837794866,14.2733213966434,122.042123340413)) ;
#65301 = CARTESIAN_POINT('Ctrl Pts',(-19.9128751830492,14.0933323162805,122.316060778059)) ;
#65302 = CARTESIAN_POINT('Ctrl Pts',(-20.2657069288235,14.2832581991753,122.171283774759)) ;
#65303 = CARTESIAN_POINT('Ctrl Pts',(-20.0944136903199,14.1032691188124,122.419388116494)) ;
#65304 = CARTESIAN_POINT('Ctrl Pts',(-20.4679459835233,14.2932412066266,122.338438899069)) ;
#65305 = CARTESIAN_POINT('Ctrl Pts',(-20.2562053796479,14.1132521262637,122.55311135473)) ;
#65306 = CARTESIAN_POINT('Ctrl Pts',(-20.6387149774407,14.3032850480414,122.539652891498)) ;
#65307 = CARTESIAN_POINT('Ctrl Pts',(-20.3928213084693,14.1232959676785,122.714082124582)) ;
#65308 = CARTESIAN_POINT('Ctrl Pts',(-20.7696539436816,14.3131132466653,122.762322078436)) ;
#65309 = CARTESIAN_POINT('Ctrl Pts',(-20.4975727394675,14.1331241663024,122.892215983891)) ;
#65310 = CARTESIAN_POINT('Ctrl Pts',(-20.8623069213888,14.3231898401075,123.010327296333)) ;
#65311 = CARTESIAN_POINT('Ctrl Pts',(-20.5716961867102,14.1432007597447,123.090620129128)) ;
#65312 = CARTESIAN_POINT('Ctrl Pts',(-20.909567306365,14.3330418394491,123.264936220785)) ;
#65313 = CARTESIAN_POINT('Ctrl Pts',(-20.6095053328595,14.1530527590862,123.294306109493)) ;
#65314 = CARTESIAN_POINT('Ctrl Pts',(-20.9121706248892,14.343115426273,123.529600919858)) ;
#65315 = CARTESIAN_POINT('Ctrl Pts',(-20.6115890777029,14.1631263459101,123.506038179509)) ;
#65316 = CARTESIAN_POINT('Ctrl Pts',(-20.8697248958235,14.3529556513705,123.784708643342)) ;
#65317 = CARTESIAN_POINT('Ctrl Pts',(-20.5776337239948,14.1729665710076,123.710123503099)) ;
#65318 = CARTESIAN_POINT('Ctrl Pts',(-20.7834156858806,14.3629213553991,124.031943418832)) ;
#65319 = CARTESIAN_POINT('Ctrl Pts',(-20.5085876682656,14.1829322750362,123.907911452828)) ;
#65320 = CARTESIAN_POINT('Ctrl Pts',(-20.6543560175008,14.3729479887057,124.26167893838)) ;
#65321 = CARTESIAN_POINT('Ctrl Pts',(-20.405340950833,14.1929589083428,124.091700497226)) ;
#65322 = CARTESIAN_POINT('Ctrl Pts',(-20.4893881315526,14.3828622844175,124.463327357308)) ;
#65323 = CARTESIAN_POINT('Ctrl Pts',(-20.273367967042,14.2028732040546,124.253019557366)) ;
#65324 = CARTESIAN_POINT('Ctrl Pts',(-20.29073289972,14.39285057311,124.634911409917)) ;
#65325 = CARTESIAN_POINT('Ctrl Pts',(-20.1144447718736,14.2128614927471,124.390287707971)) ;
#65326 = CARTESIAN_POINT('Ctrl Pts',(-20.0639385669575,14.4028893062683,124.769650931547)) ;
#65327 = CARTESIAN_POINT('Ctrl Pts',(-19.933009840498,14.2229002259054,124.498080437852)) ;
#65328 = CARTESIAN_POINT('Ctrl Pts',(-19.8221438934761,14.4127326380959,124.861560677325)) ;
#65329 = CARTESIAN_POINT('Ctrl Pts',(-19.7395754882741,14.232743557733,124.571609123733)) ;
#65330 = CARTESIAN_POINT('Ctrl Pts',(-19.5634174500474,14.4227603639755,124.911597480083)) ;
#65331 = CARTESIAN_POINT('Ctrl Pts',(-19.532594551231,14.2427712836126,124.611640002553)) ;
#65332 = CARTESIAN_POINT('Ctrl Pts',(-19.2997938732283,14.432792700364,124.915236180486)) ;
#65333 = CARTESIAN_POINT('Ctrl Pts',(-19.3216956393782,14.2528036200011,124.614552265305)) ;
#65334 = CARTESIAN_POINT('Ctrl Pts',(-19.0447452472327,14.4426222006646,124.874418148553)) ;
#65335 = CARTESIAN_POINT('Ctrl Pts',(-19.1176575176957,14.2626331203018,124.581899394182)) ;
#65336 = CARTESIAN_POINT('Ctrl Pts',(-18.796407103076,14.4526117045814,124.789299015739)) ;
#65337 = CARTESIAN_POINT('Ctrl Pts',(-18.9189866276755,14.2726226242185,124.513805617526)) ;
#65338 = CARTESIAN_POINT('Ctrl Pts',(-18.5657044122553,14.4626555450938,124.661080239922)) ;
#65339 = CARTESIAN_POINT('Ctrl Pts',(-18.734423674689,14.2826664647309,124.411231794536)) ;
#65340 = CARTESIAN_POINT('Ctrl Pts',(-18.3649628204512,14.4724772508619,124.498843726449)) ;
#65341 = CARTESIAN_POINT('Ctrl Pts',(-18.5738302074953,14.292488170499,124.281444409)) ;
#65342 = CARTESIAN_POINT('Ctrl Pts',(-18.1912720235427,14.4825122979942,124.300414746533)) ;
#65343 = CARTESIAN_POINT('Ctrl Pts',(-18.4348762631959,14.3025232176314,124.122702256751)) ;
#65344 = CARTESIAN_POINT('Ctrl Pts',(-18.055432254409,14.4925369754311,124.074689127998)) ;
#65345 = CARTESIAN_POINT('Ctrl Pts',(-18.3262031311123,14.3125478950683,123.942122532093)) ;
#65346 = CARTESIAN_POINT('Ctrl Pts',(-17.9619640242889,14.5023897902856,123.833226852752)) ;
#65347 = CARTESIAN_POINT('Ctrl Pts',(-18.2514273185047,14.3224007099227,123.748954049798)) ;
#65348 = CARTESIAN_POINT('Ctrl Pts',(-17.9107066774369,14.5123774998931,123.575833839664)) ;
#65349 = CARTESIAN_POINT('Ctrl Pts',(-18.210419791455,14.3323884195303,123.543040117254)) ;
#65350 = CARTESIAN_POINT('Ctrl Pts',(-17.9049402191342,14.5223075098872,123.314937805648)) ;
#65351 = CARTESIAN_POINT('Ctrl Pts',(-18.2058049219443,14.3423184295243,123.33432374461)) ;
#65352 = CARTESIAN_POINT('Ctrl Pts',(-17.9443990827381,14.5322972651064,123.055394867544)) ;
#65353 = CARTESIAN_POINT('Ctrl Pts',(-18.237370231834,14.3523081847435,123.126689256779)) ;
#65354 = CARTESIAN_POINT('Ctrl Pts',(-18.0289554645481,14.5423238737893,122.80583753216)) ;
#65355 = CARTESIAN_POINT('Ctrl Pts',(-18.3050137161035,14.3623347934264,122.927042810016)) ;
#65356 = CARTESIAN_POINT('Ctrl Pts',(-18.1535342537274,14.5522078138111,122.577928818094)) ;
#65357 = CARTESIAN_POINT('Ctrl Pts',(-18.4046749159261,14.3722187334482,122.744715509039)) ;
#65358 = CARTESIAN_POINT('Ctrl Pts',(-18.3170525414426,14.5621970413496,122.372560685954)) ;
#65359 = CARTESIAN_POINT('Ctrl Pts',(-18.5354880122314,14.3822079609867,122.580419941737)) ;
#65360 = CARTESIAN_POINT('Ctrl Pts',(-18.5151557257719,14.5722399118733,122.198188061704)) ;
#65361 = CARTESIAN_POINT('Ctrl Pts',(-18.6939694414926,14.3922508315104,122.440920462388)) ;
#65362 = CARTESIAN_POINT('Ctrl Pts',(-18.7355880780577,14.5820722986287,122.063388638443)) ;
#65363 = CARTESIAN_POINT('Ctrl Pts',(-18.8703137118598,14.4020832182658,122.333079750593)) ;
#65364 = CARTESIAN_POINT('Ctrl Pts',(-18.9797323076057,14.5920655918003,121.966658037112)) ;
#65365 = CARTESIAN_POINT('Ctrl Pts',(-19.0656282824221,14.4120765114374,122.255693489777)) ;
#65366 = CARTESIAN_POINT('Ctrl Pts',(-19.2380876823601,14.6020975974487,121.914120317295)) ;
#65367 = CARTESIAN_POINT('Ctrl Pts',(-19.2723122376113,14.4221085170859,122.213661473719)) ;
#65368 = CARTESIAN_POINT('Ctrl Pts',(-19.4972262784199,14.6119628534177,121.907034280981)) ;
#65369 = CARTESIAN_POINT('Ctrl Pts',(-19.479622479628,14.4319737730548,122.207990741055)) ;
#65370 = CARTESIAN_POINT('Ctrl Pts',(-19.7562992627137,14.6219247333252,121.944692330567)) ;
#65371 = CARTESIAN_POINT('Ctrl Pts',(-19.6868809582063,14.4419356529623,122.238115153452)) ;
#65372 = CARTESIAN_POINT('Ctrl Pts',(-20.0065648350329,14.6319596666871,122.027765848265)) ;
#65373 = CARTESIAN_POINT('Ctrl Pts',(-19.8870940599284,14.4519705863242,122.304572113767)) ;
#65374 = CARTESIAN_POINT('Ctrl Pts',(-20.2353895991265,14.6418446250664,122.150798715635)) ;
#65375 = CARTESIAN_POINT('Ctrl Pts',(-20.0701544291512,14.4618555447035,122.402996417728)) ;
#65376 = CARTESIAN_POINT('Ctrl Pts',(-20.4430039039663,14.6519102519891,122.314630587451)) ;
#65377 = CARTESIAN_POINT('Ctrl Pts',(-20.2362472126455,14.4719211716262,122.534060408975)) ;
#65378 = CARTESIAN_POINT('Ctrl Pts',(-20.6153099874822,14.6617493576534,122.507469086936)) ;
#65379 = CARTESIAN_POINT('Ctrl Pts',(-20.3740932248574,14.4817602772905,122.688329427988)) ;
#65380 = CARTESIAN_POINT('Ctrl Pts',(-20.7548702754188,14.6718121726588,122.732041086105)) ;
#65381 = CARTESIAN_POINT('Ctrl Pts',(-20.4857432796024,14.4918230922959,122.867986018619)) ;
#65382 = CARTESIAN_POINT('Ctrl Pts',(-20.8514895076296,14.6817083787074,122.973518167656)) ;
#65383 = CARTESIAN_POINT('Ctrl Pts',(-20.5630404332213,14.5017192983446,123.061166569921)) ;
#65384 = CARTESIAN_POINT('Ctrl Pts',(-20.905652298732,14.6916492017327,123.229045388477)) ;
#65385 = CARTESIAN_POINT('Ctrl Pts',(-20.6063727060311,14.5116601213698,123.265587688841)) ;
#65386 = CARTESIAN_POINT('Ctrl Pts',(-20.9147482972179,14.7016537847114,123.49182757385)) ;
#65387 = CARTESIAN_POINT('Ctrl Pts',(-20.6136516339194,14.5216647043485,123.475813306976)) ;
#65388 = CARTESIAN_POINT('Ctrl Pts',(-20.8777060565819,14.7116746791561,123.752541737872)) ;
#65389 = CARTESIAN_POINT('Ctrl Pts',(-20.584019929086,14.5316855987932,123.684384908824)) ;
#65390 = CARTESIAN_POINT('Ctrl Pts',(-20.7973137583484,14.7215665997455,123.999754867603)) ;
#65391 = CARTESIAN_POINT('Ctrl Pts',(-20.5197082201853,14.5415775193826,123.882155761826)) ;
#65392 = CARTESIAN_POINT('Ctrl Pts',(-20.6743041569518,14.7315600320909,124.231770792966)) ;
#65393 = CARTESIAN_POINT('Ctrl Pts',(-20.4213024934147,14.551570951728,124.067769440875)) ;
#65394 = CARTESIAN_POINT('Ctrl Pts',(-20.5135786631871,14.7415056369908,124.437867633095)) ;
#65395 = CARTESIAN_POINT('Ctrl Pts',(-20.2927239143119,14.5615165566279,124.232648095339)) ;
#65396 = CARTESIAN_POINT('Ctrl Pts',(-20.3198218573511,14.7514529104723,124.613360457444)) ;
#65397 = CARTESIAN_POINT('Ctrl Pts',(-20.137720063294,14.5714638301094,124.373043875978)) ;
#65398 = CARTESIAN_POINT('Ctrl Pts',(-20.0961599099383,14.7615008249487,124.753689774848)) ;
#65399 = CARTESIAN_POINT('Ctrl Pts',(-19.9587916558263,14.5815117445858,124.485309178269)) ;
#65400 = CARTESIAN_POINT('Ctrl Pts',(-19.8564776376663,14.771348465296,124.851279444888)) ;
#65401 = CARTESIAN_POINT('Ctrl Pts',(-19.7670469592938,14.5913593849331,124.563382825184)) ;
#65402 = CARTESIAN_POINT('Ctrl Pts',(-19.6007489896213,14.7813101806726,124.907199618394)) ;
#65403 = CARTESIAN_POINT('Ctrl Pts',(-19.5624646160184,14.6013211003097,124.608121129999)) ;
#65404 = CARTESIAN_POINT('Ctrl Pts',(-19.3373962978428,14.7913388042454,124.917606836282)) ;
#65405 = CARTESIAN_POINT('Ctrl Pts',(-19.3517825852773,14.6113497238825,124.616449119218)) ;
#65406 = CARTESIAN_POINT('Ctrl Pts',(-19.0793336231031,14.8012491663118,124.882634265756)) ;
#65407 = CARTESIAN_POINT('Ctrl Pts',(-19.1453323129572,14.6212600859489,124.58847329103)) ;
#65408 = CARTESIAN_POINT('Ctrl Pts',(-18.8304237660988,14.8111838599642,124.803839977348)) ;
#65409 = CARTESIAN_POINT('Ctrl Pts',(-18.9462038486766,14.6311947796013,124.52544003625)) ;
#65410 = CARTESIAN_POINT('Ctrl Pts',(-18.5966220485025,14.8212257030921,124.681499373881)) ;
#65411 = CARTESIAN_POINT('Ctrl Pts',(-18.7591614689245,14.6412366227292,124.427569556202)) ;
#65412 = CARTESIAN_POINT('Ctrl Pts',(-18.390716860511,14.8311102086625,124.523104155642)) ;
#65413 = CARTESIAN_POINT('Ctrl Pts',(-18.5944360498318,14.6511211282996,124.300855240205)) ;
#65414 = CARTESIAN_POINT('Ctrl Pts',(-18.2131739736385,14.8411123124477,124.329336878928)) ;
#65415 = CARTESIAN_POINT('Ctrl Pts',(-18.4524001167752,14.6611232320848,124.145842979682)) ;
#65416 = CARTESIAN_POINT('Ctrl Pts',(-18.0729290956816,14.8510306638627,124.109588770675)) ;
#65417 = CARTESIAN_POINT('Ctrl Pts',(-18.3402023497202,14.6710415834998,123.970045780687)) ;
#65418 = CARTESIAN_POINT('Ctrl Pts',(-17.9717628132547,14.8610783198836,123.865741080711)) ;
#65419 = CARTESIAN_POINT('Ctrl Pts',(-18.2592672790845,14.6810892395207,123.774968483768)) ;
#65420 = CARTESIAN_POINT('Ctrl Pts',(-17.9151745106479,14.8709495129118,123.612528140335)) ;
#65421 = CARTESIAN_POINT('Ctrl Pts',(-18.2139943885735,14.6909604325489,123.572398901037)) ;
#65422 = CARTESIAN_POINT('Ctrl Pts',(-17.9031429831484,14.8810152260553,123.34834743098)) ;
#65423 = CARTESIAN_POINT('Ctrl Pts',(-18.204367144922,14.7010261456924,123.361053634231)) ;
#65424 = CARTESIAN_POINT('Ctrl Pts',(-17.9361624249687,14.890867686628,123.091474379834)) ;
#65425 = CARTESIAN_POINT('Ctrl Pts',(-18.2307796125064,14.7108786062651,123.155558165158)) ;
#65426 = CARTESIAN_POINT('Ctrl Pts',(-18.0413449335706,14.9042961493505,122.754742299802)) ;
#65427 = CARTESIAN_POINT('Ctrl Pts',(-18.3149269800469,14.7243070689876,122.88615548597)) ;
#65428 = CARTESIAN_POINT('Ctrl Pts',(-18.2267874470069,14.9173770968676,122.460483907588)) ;
#65429 = CARTESIAN_POINT('Ctrl Pts',(-18.4633001749267,14.7373880165047,122.65073212564)) ;
#65430 = CARTESIAN_POINT('Ctrl Pts',(-18.4863543902938,14.9308515951022,122.219747666857)) ;
#65431 = CARTESIAN_POINT('Ctrl Pts',(-18.6709215324032,14.7508625147393,122.458175060593)) ;
#65432 = CARTESIAN_POINT('Ctrl Pts',(-18.7036544341988,14.9406836987116,122.079886991967)) ;
#65433 = CARTESIAN_POINT('Ctrl Pts',(-18.8447666073225,14.7606946183488,122.346277773026)) ;
#65434 = CARTESIAN_POINT('Ctrl Pts',(-18.9446987351203,14.9506496018383,121.977572951031)) ;
#65435 = CARTESIAN_POINT('Ctrl Pts',(-19.0375992137508,14.7706605214754,122.264426179784)) ;
#65436 = CARTESIAN_POINT('Ctrl Pts',(-19.2015765911018,14.9606770111485,121.918685704724)) ;
#65437 = CARTESIAN_POINT('Ctrl Pts',(-19.2431028113862,14.7806879307857,122.217314368209)) ;
#65438 = CARTESIAN_POINT('Ctrl Pts',(-19.4616556588049,14.9705880425151,121.905384721623)) ;
#65439 = CARTESIAN_POINT('Ctrl Pts',(-19.4511604538144,14.7905989621522,122.206669246989)) ;
#65440 = CARTESIAN_POINT('Ctrl Pts',(-19.8072618039374,14.9838323501362,121.947128778354)) ;
#65441 = CARTESIAN_POINT('Ctrl Pts',(-19.7276732696558,14.8038432697733,122.24007284524)) ;
#65442 = CARTESIAN_POINT('Ctrl Pts',(-20.2188550941679,15.0005328328073,122.113045312188)) ;
#65443 = CARTESIAN_POINT('Ctrl Pts',(-20.0569081396409,14.8205437524445,122.372778876184)) ;
#65444 = CARTESIAN_POINT('Ctrl Pts',(-20.5455679441702,15.0170396619631,122.405960959497)) ;
#65445 = CARTESIAN_POINT('Ctrl Pts',(-20.3183298372832,14.8370505816002,122.607156832751)) ;
#65446 = CARTESIAN_POINT('Ctrl Pts',(-20.7373262391937,15.0303502902007,122.698457845509)) ;
#65447 = CARTESIAN_POINT('Ctrl Pts',(-20.4717022185341,14.8503612098378,122.841112812095)) ;
#65448 = CARTESIAN_POINT('Ctrl Pts',(-20.8410482037776,15.0403428537408,122.939743261889)) ;
#65449 = CARTESIAN_POINT('Ctrl Pts',(-20.5546889224827,14.8603537733779,123.034149304461)) ;
#65450 = CARTESIAN_POINT('Ctrl Pts',(-20.9012011780977,15.0503729367423,123.196334518998)) ;
#65451 = CARTESIAN_POINT('Ctrl Pts',(-20.6028117682902,14.8703838563795,123.239415751326)) ;
#65452 = CARTESIAN_POINT('Ctrl Pts',(-20.9212136813736,15.0635465407401,123.542009444152)) ;
#65453 = CARTESIAN_POINT('Ctrl Pts',(-20.6188231356047,14.8835574603772,123.515975765134)) ;
#65454 = CARTESIAN_POINT('Ctrl Pts',(-20.8322977307926,15.0801842459715,123.97501211203)) ;
#65455 = CARTESIAN_POINT('Ctrl Pts',(-20.5476923868234,14.9001951656086,123.862358789437)) ;
#65456 = CARTESIAN_POINT('Ctrl Pts',(-20.5559470864143,15.1000660085389,124.425649304088)) ;
#65457 = CARTESIAN_POINT('Ctrl Pts',(-20.3266297541307,14.9200769281761,124.222868808078)) ;
#65458 = CARTESIAN_POINT('Ctrl Pts',(-20.2087222530336,15.1167623607554,124.70175262575)) ;
#65459 = CARTESIAN_POINT('Ctrl Pts',(-20.0488038623269,14.9367732803926,124.443780904704)) ;
#65460 = CARTESIAN_POINT('Ctrl Pts',(-19.8917080630513,15.1299193885445,124.839949683673)) ;
#65461 = CARTESIAN_POINT('Ctrl Pts',(-19.7952369425697,14.9499303081817,124.554316138444)) ;
#65462 = CARTESIAN_POINT('Ctrl Pts',(-19.5501536847632,15.1432967431881,124.92300774244)) ;
#65463 = CARTESIAN_POINT('Ctrl Pts',(-19.5219730467639,14.9633076628252,124.620769728734)) ;
#65464 = CARTESIAN_POINT('Ctrl Pts',(-19.1108554066313,15.1598275774469,124.912748434119)) ;
#65465 = CARTESIAN_POINT('Ctrl Pts',(-19.170551068665,14.979838497084,124.612563667479)) ;
#65466 = CARTESIAN_POINT('Ctrl Pts',(-18.616168502824,15.17979226719,124.720920100906)) ;
#65467 = CARTESIAN_POINT('Ctrl Pts',(-18.7747945577077,14.9998031868271,124.45910447757)) ;
#65468 = CARTESIAN_POINT('Ctrl Pts',(-18.2178819295255,15.1997087606136,124.372224270615)) ;
#65469 = CARTESIAN_POINT('Ctrl Pts',(-18.4561642627655,15.0197196802507,124.180149816018)) ;
#65470 = CARTESIAN_POINT('Ctrl Pts',(-17.9618943674429,15.2195984799632,123.909642300137)) ;
#65471 = CARTESIAN_POINT('Ctrl Pts',(-18.2513709039393,15.0396093996003,123.810084995758)) ;
#65472 = CARTESIAN_POINT('Ctrl Pts',(-17.8790867340295,15.239605209611,123.384461553137)) ;
#65473 = CARTESIAN_POINT('Ctrl Pts',(-18.1851220450662,15.0596161292481,123.389940905044)) ;
#65474 = CARTESIAN_POINT('Ctrl Pts',(-17.9792551414852,15.2594432632579,122.866690154571)) ;
#65475 = CARTESIAN_POINT('Ctrl Pts',(-18.2652543890131,15.079454182895,122.975722039237)) ;
#65476 = CARTESIAN_POINT('Ctrl Pts',(-18.2516493430185,15.2794366014715,122.410539526417)) ;
#65477 = CARTESIAN_POINT('Ctrl Pts',(-18.4831677681727,15.0994475211086,122.610800270065)) ;
#65478 = CARTESIAN_POINT('Ctrl Pts',(-18.661435692982,15.2993194008781,122.076711965965)) ;
#65479 = CARTESIAN_POINT('Ctrl Pts',(-18.8109961779416,15.1193303205152,122.34373578517)) ;
#65480 = CARTESIAN_POINT('Ctrl Pts',(-19.1602442446391,15.3192115817968,121.901912195536)) ;
#65481 = CARTESIAN_POINT('Ctrl Pts',(-19.2100434562284,15.1392225014339,122.203893842988)) ;
#65482 = CARTESIAN_POINT('Ctrl Pts',(-19.6893450348153,15.3391137602919,121.906937811211)) ;
#65483 = CARTESIAN_POINT('Ctrl Pts',(-19.6333250670439,15.159124679929,122.207913017499)) ;
#65484 = CARTESIAN_POINT('Ctrl Pts',(-20.1877316480936,15.3591510714956,122.094234259217)) ;
#65485 = CARTESIAN_POINT('Ctrl Pts',(-20.0320345164081,15.1791619911328,122.357748581197)) ;
#65486 = CARTESIAN_POINT('Ctrl Pts',(-20.5885091138174,15.3789635130365,122.4361550605)) ;
#65487 = CARTESIAN_POINT('Ctrl Pts',(-20.352658713179,15.1989744326736,122.631285748145)) ;
#65488 = CARTESIAN_POINT('Ctrl Pts',(-20.8514802727897,15.3990287537714,122.899819819407)) ;
#65489 = CARTESIAN_POINT('Ctrl Pts',(-20.5630361534512,15.2190396734085,123.002216473756)) ;
#65490 = CARTESIAN_POINT('Ctrl Pts',(-20.939569466923,15.4187859586272,123.417748054594)) ;
#65491 = CARTESIAN_POINT('Ctrl Pts',(-20.6335085384984,15.2387968782644,123.416561832562)) ;
#65492 = CARTESIAN_POINT('Ctrl Pts',(-20.8451846342489,15.4388192312729,123.941494843128)) ;
#65493 = CARTESIAN_POINT('Ctrl Pts',(-20.5580007277665,15.2588301509101,123.835558979513)) ;
#65494 = CARTESIAN_POINT('Ctrl Pts',(-20.5803681949361,15.4586321397268,124.396932991369)) ;
#65495 = CARTESIAN_POINT('Ctrl Pts',(-20.3461462373689,15.2786430593639,124.199911406604)) ;
#65496 = CARTESIAN_POINT('Ctrl Pts',(-20.1731096405733,15.4786282858542,124.738024765008)) ;
#65497 = CARTESIAN_POINT('Ctrl Pts',(-20.0203388220478,15.2986392054913,124.472784322776)) ;
#65498 = CARTESIAN_POINT('Ctrl Pts',(-19.6769061894164,15.4984900390767,124.918856330261)) ;
#65499 = CARTESIAN_POINT('Ctrl Pts',(-19.6233743087396,15.3185009587138,124.617449135294)) ;
#65500 = CARTESIAN_POINT('Ctrl Pts',(-19.1436360482035,15.5185585562048,124.919177517765)) ;
#65501 = CARTESIAN_POINT('Ctrl Pts',(-19.1967589767419,15.3385694758419,124.617705010039)) ;
#65502 = CARTESIAN_POINT('Ctrl Pts',(-18.6481039856445,15.5383894292016,124.739248841471)) ;
#65503 = CARTESIAN_POINT('Ctrl Pts',(-18.8003319653689,15.3584003488387,124.473760421146)) ;
#65504 = CARTESIAN_POINT('Ctrl Pts',(-18.2411262734598,15.5583113400183,124.400722475563)) ;
#65505 = CARTESIAN_POINT('Ctrl Pts',(-18.4747503480826,15.3783222596554,124.202937369334)) ;
#65506 = CARTESIAN_POINT('Ctrl Pts',(-17.9740267390617,15.5782407834536,123.943204335233)) ;
#65507 = CARTESIAN_POINT('Ctrl Pts',(-18.2610720716113,15.3982517030907,123.836921334488)) ;
#65508 = CARTESIAN_POINT('Ctrl Pts',(-17.8790194223619,15.59815045357,123.422718308582)) ;
#65509 = CARTESIAN_POINT('Ctrl Pts',(-18.1850681984714,15.4181613732071,123.42053129134)) ;
#65510 = CARTESIAN_POINT('Ctrl Pts',(-17.9662605748662,15.6180238108329,122.901708304058)) ;
#65511 = CARTESIAN_POINT('Ctrl Pts',(-18.254863873094,15.43803473047,123.00372270003)) ;
#65512 = CARTESIAN_POINT('Ctrl Pts',(-18.2276238439571,15.6380153454508,122.439173769157)) ;
#65513 = CARTESIAN_POINT('Ctrl Pts',(-18.4639568825122,15.4580262650879,122.633696362136)) ;
#65514 = CARTESIAN_POINT('Ctrl Pts',(-18.6285678009232,15.6578809628615,122.095505124988)) ;
#65515 = CARTESIAN_POINT('Ctrl Pts',(-18.7847146580216,15.4778918824987,122.358763014861)) ;
#65516 = CARTESIAN_POINT('Ctrl Pts',(-19.1253095706751,15.6778618926898,121.907746174012)) ;
#65517 = CARTESIAN_POINT('Ctrl Pts',(-19.1821092675839,15.4978728123269,122.208558782164)) ;
#65518 = CARTESIAN_POINT('Ctrl Pts',(-19.6552143908038,15.6978003547729,121.901373660419)) ;
#65519 = CARTESIAN_POINT('Ctrl Pts',(-19.6060335509028,15.51781127441,122.203463873449)) ;
#65520 = CARTESIAN_POINT('Ctrl Pts',(-20.1546433032014,15.7176925479946,122.075043824401)) ;
#65521 = CARTESIAN_POINT('Ctrl Pts',(-20.0055761682767,15.5377034676318,122.342403428384)) ;
#65522 = CARTESIAN_POINT('Ctrl Pts',(-20.5661496331982,15.73766326303,122.410119645807)) ;
#65523 = CARTESIAN_POINT('Ctrl Pts',(-20.3347791384015,15.5576741826671,122.610466906619)) ;
#65524 = CARTESIAN_POINT('Ctrl Pts',(-20.8373123753955,15.7574729346961,122.861577302707)) ;
#65525 = CARTESIAN_POINT('Ctrl Pts',(-20.5517067350592,15.5774838543332,122.97163565789)) ;
#65526 = CARTESIAN_POINT('Ctrl Pts',(-20.9393997364478,15.7774661513873,123.382866096592)) ;
#65527 = CARTESIAN_POINT('Ctrl Pts',(-20.6333723462591,15.5974770710244,123.388667788783)) ;
#65528 = CARTESIAN_POINT('Ctrl Pts',(-20.8584216081124,15.7973170635836,123.904440437728)) ;
#65529 = CARTESIAN_POINT('Ctrl Pts',(-20.5685874513888,15.6173279832208,123.805925914107)) ;
#65530 = CARTESIAN_POINT('Ctrl Pts',(-20.6013666268889,15.8173916699027,124.371819409561)) ;
#65531 = CARTESIAN_POINT('Ctrl Pts',(-20.3629338879566,15.6374025895398,124.17983155202)) ;
#65532 = CARTESIAN_POINT('Ctrl Pts',(-20.2709357008999,15.833908301786,124.661071335312)) ;
#65533 = CARTESIAN_POINT('Ctrl Pts',(-20.098605819619,15.6539192214231,124.411216220692)) ;
#65534 = CARTESIAN_POINT('Ctrl Pts',(-19.9567400193657,15.8472470094801,124.816295036982)) ;
#65535 = CARTESIAN_POINT('Ctrl Pts',(-19.8472304865429,15.6672579291172,124.535405548964)) ;
#65536 = CARTESIAN_POINT('Ctrl Pts',(-19.7085577801769,15.8570893837884,124.889269258747)) ;
#65537 = CARTESIAN_POINT('Ctrl Pts',(-19.6486898643955,15.6771003034255,124.593781066732)) ;
#65538 = CARTESIAN_POINT('Ctrl Pts',(-19.4460289923727,15.8671444037711,124.918903925048)) ;
#65539 = CARTESIAN_POINT('Ctrl Pts',(-19.438655254333,15.6871553234083,124.617484843905)) ;
#65540 = CARTESIAN_POINT('Ctrl Pts',(-19.0989283678214,15.8803765604287,124.897309206157)) ;
#65541 = CARTESIAN_POINT('Ctrl Pts',(-19.1610280086618,15.7003874800658,124.600218444694)) ;
#65542 = CARTESIAN_POINT('Ctrl Pts',(-18.680086550223,15.8969915277738,124.757481852894)) ;
#65543 = CARTESIAN_POINT('Ctrl Pts',(-18.8258890338263,15.717002447411,124.488333567479)) ;
#65544 = CARTESIAN_POINT('Ctrl Pts',(-18.3346327392559,15.913586114785,124.48329340641)) ;
#65545 = CARTESIAN_POINT('Ctrl Pts',(-18.549571248321,15.7335970344222,124.26900587412)) ;
#65546 = CARTESIAN_POINT('Ctrl Pts',(-18.1268897362054,15.9268196831404,124.204366870051)) ;
#65547 = CARTESIAN_POINT('Ctrl Pts',(-18.3833541247988,15.7468306027775,124.045842691326)) ;
#65548 = CARTESIAN_POINT('Ctrl Pts',(-18.0083439444997,15.9368633009491,123.968576154149)) ;
#65549 = CARTESIAN_POINT('Ctrl Pts',(-18.288524508184,15.7568742205862,123.857213407479)) ;
#65550 = CARTESIAN_POINT('Ctrl Pts',(-17.9336253681816,15.9467502251839,123.719711066793)) ;
#65551 = CARTESIAN_POINT('Ctrl Pts',(-18.228750615402,15.766761144821,123.658118921018)) ;
#65552 = CARTESIAN_POINT('Ctrl Pts',(-17.9024744065932,15.9567408796307,123.459039355824)) ;
#65553 = CARTESIAN_POINT('Ctrl Pts',(-18.2038316647778,15.7767517992678,123.44958390152)) ;
#65554 = CARTESIAN_POINT('Ctrl Pts',(-17.9170694041595,15.9667026380847,123.197660756749)) ;
#65555 = CARTESIAN_POINT('Ctrl Pts',(-18.2155127307376,15.7867135577218,123.240472575159)) ;
#65556 = CARTESIAN_POINT('Ctrl Pts',(-17.9967391763496,15.9800425031519,122.856207482281)) ;
#65557 = CARTESIAN_POINT('Ctrl Pts',(-18.2792369334935,15.800053422789,122.967353118238)) ;
#65558 = CARTESIAN_POINT('Ctrl Pts',(-18.1639736695918,15.9933512860652,122.544568270991)) ;
#65559 = CARTESIAN_POINT('Ctrl Pts',(-18.4130291807897,15.8133622057023,122.718017643817)) ;
#65560 = CARTESIAN_POINT('Ctrl Pts',(-18.4009205226991,16.0065470435093,122.291373958012)) ;
#65561 = CARTESIAN_POINT('Ctrl Pts',(-18.6026009981143,15.8265579631464,122.515452269556)) ;
#65562 = CARTESIAN_POINT('Ctrl Pts',(-18.6098352782094,16.0165089271858,122.133609050801)) ;
#65563 = CARTESIAN_POINT('Ctrl Pts',(-18.7697316665217,15.8365198468229,122.389244599765)) ;
#65564 = CARTESIAN_POINT('Ctrl Pts',(-18.8450601920169,16.0265520367004,122.013933523829)) ;
#65565 = CARTESIAN_POINT('Ctrl Pts',(-18.9579132372001,15.8465629563375,122.293505565848)) ;
#65566 = CARTESIAN_POINT('Ctrl Pts',(-19.0926161288735,16.0364042866996,121.938083702946)) ;
#65567 = CARTESIAN_POINT('Ctrl Pts',(-19.1559583816547,15.8564152063368,122.232828069619)) ;
#65568 = CARTESIAN_POINT('Ctrl Pts',(-19.3525761374353,16.0463758236501,121.90535120371)) ;
#65569 = CARTESIAN_POINT('Ctrl Pts',(-19.3639266242928,15.8663867432872,122.206644267402)) ;
#65570 = CARTESIAN_POINT('Ctrl Pts',(-19.6149622143192,16.0563710891276,121.918309627861)) ;
#65571 = CARTESIAN_POINT('Ctrl Pts',(-19.5738352989783,15.8763820087648,122.217013257549)) ;
#65572 = CARTESIAN_POINT('Ctrl Pts',(-19.8719707676213,16.0664050620013,121.977157725234)) ;
#65573 = CARTESIAN_POINT('Ctrl Pts',(-19.7794416116365,15.8864159816384,122.264093925763)) ;
#65574 = CARTESIAN_POINT('Ctrl Pts',(-20.1107386746183,16.0762604767636,122.077550542983)) ;
#65575 = CARTESIAN_POINT('Ctrl Pts',(-19.9704548934143,15.8962713964007,122.344410174474)) ;
#65576 = CARTESIAN_POINT('Ctrl Pts',(-20.3317609231274,16.0862597542724,122.219585083318)) ;
#65577 = CARTESIAN_POINT('Ctrl Pts',(-20.1472714239141,15.9062706739096,122.458039646496)) ;
#65578 = CARTESIAN_POINT('Ctrl Pts',(-20.5230102658078,16.0961549384354,122.395838020282)) ;
#65579 = CARTESIAN_POINT('Ctrl Pts',(-20.3002692442417,15.9161658580725,122.599043480994)) ;
#65580 = CARTESIAN_POINT('Ctrl Pts',(-20.6833117694189,16.1062153180762,122.606026601043)) ;
#65581 = CARTESIAN_POINT('Ctrl Pts',(-20.4285086974711,15.9262262377133,122.76719571147)) ;
#65582 = CARTESIAN_POINT('Ctrl Pts',(-20.8023123453152,16.1160651870843,122.835923343469)) ;
#65583 = CARTESIAN_POINT('Ctrl Pts',(-20.5237070533521,15.9360761067214,122.951113839647)) ;
#65584 = CARTESIAN_POINT('Ctrl Pts',(-20.8815749658397,16.1260967482922,123.087326542233)) ;
#65585 = CARTESIAN_POINT('Ctrl Pts',(-20.5871150742216,15.9461076679293,123.152237028848)) ;
#65586 = CARTESIAN_POINT('Ctrl Pts',(-20.9153886455586,16.1361071971745,123.3482327168)) ;
#65587 = CARTESIAN_POINT('Ctrl Pts',(-20.6141638267646,15.9561181168116,123.360962211071)) ;
#65588 = CARTESIAN_POINT('Ctrl Pts',(-20.9038000062041,16.1460139365915,123.608304860459)) ;
#65589 = CARTESIAN_POINT('Ctrl Pts',(-20.604890742972,15.9660248562286,123.569019582891)) ;
#65590 = CARTESIAN_POINT('Ctrl Pts',(-20.8475493442764,16.1559519526599,123.863320444448)) ;
#65591 = CARTESIAN_POINT('Ctrl Pts',(-20.5598881638927,15.9759628722971,123.773031376224)) ;
#65592 = CARTESIAN_POINT('Ctrl Pts',(-20.7473434745622,16.1659571991111,124.106434248665)) ;
#65593 = CARTESIAN_POINT('Ctrl Pts',(-20.4797215247247,15.9859681187482,123.967521547182)) ;
#65594 = CARTESIAN_POINT('Ctrl Pts',(-20.6056840713685,16.1759912601674,124.328819428175)) ;
#65595 = CARTESIAN_POINT('Ctrl Pts',(-20.3663921647497,15.9960021798045,124.145428536233)) ;
#65596 = CARTESIAN_POINT('Ctrl Pts',(-20.4312280688443,16.1858363412255,124.519891626386)) ;
#65597 = CARTESIAN_POINT('Ctrl Pts',(-20.2268260969221,16.0058472608626,124.298284524298)) ;
#65598 = CARTESIAN_POINT('Ctrl Pts',(-20.2236607634961,16.195822147179,124.680379963816)) ;
#65599 = CARTESIAN_POINT('Ctrl Pts',(-20.0607710803416,16.0158330668161,124.426673466983)) ;
#65600 = CARTESIAN_POINT('Ctrl Pts',(-19.9925740517516,16.2057569677332,124.801974564811)) ;
#65601 = CARTESIAN_POINT('Ctrl Pts',(-19.8759009849248,16.0257678873703,124.523947205164)) ;
#65602 = CARTESIAN_POINT('Ctrl Pts',(-19.7408239243177,16.2158144928654,124.88232980859)) ;
#65603 = CARTESIAN_POINT('Ctrl Pts',(-19.674500158399,16.0358254125025,124.588229439226)) ;
#65604 = CARTESIAN_POINT('Ctrl Pts',(-19.4850756391553,16.2256361435168,124.917322735119)) ;
#65605 = CARTESIAN_POINT('Ctrl Pts',(-19.4699018773493,16.0456470631539,124.616221674339)) ;
#65606 = CARTESIAN_POINT('Ctrl Pts',(-19.2210119356238,16.2356922070215,124.90763544783)) ;
#65607 = CARTESIAN_POINT('Ctrl Pts',(-19.258650898185,16.0557031266586,124.608469860502)) ;
#65608 = CARTESIAN_POINT('Ctrl Pts',(-18.965674000184,16.2456328740854,124.852413667813)) ;
#65609 = CARTESIAN_POINT('Ctrl Pts',(-19.0543812431617,16.0656437937226,124.564290497931)) ;
#65610 = CARTESIAN_POINT('Ctrl Pts',(-18.7243829673979,16.2555372677514,124.754815092852)) ;
#65611 = CARTESIAN_POINT('Ctrl Pts',(-18.8613495382106,16.0755481873885,124.486210004982)) ;
#65612 = CARTESIAN_POINT('Ctrl Pts',(-18.5006518515227,16.2655837915144,124.614693286642)) ;
#65613 = CARTESIAN_POINT('Ctrl Pts',(-18.6823656136091,16.0855947111516,124.374110855756)) ;
#65614 = CARTESIAN_POINT('Ctrl Pts',(-18.3073636533246,16.2754798745308,124.440639733717)) ;
#65615 = CARTESIAN_POINT('Ctrl Pts',(-18.5277366902723,16.0954907941679,124.234866901715)) ;
#65616 = CARTESIAN_POINT('Ctrl Pts',(-18.1445816442607,16.2855465737608,124.232170442766)) ;
#65617 = CARTESIAN_POINT('Ctrl Pts',(-18.3975125052179,16.105557493398,124.068090149545)) ;
#65618 = CARTESIAN_POINT('Ctrl Pts',(-18.0231616074987,16.2953701841619,124.004307681981)) ;
#65619 = CARTESIAN_POINT('Ctrl Pts',(-18.3003785015697,16.115381103799,123.885799728941)) ;
#65620 = CARTESIAN_POINT('Ctrl Pts',(-17.9408403240638,16.3054260443394,123.753235338654)) ;
#65621 = CARTESIAN_POINT('Ctrl Pts',(-18.2345231623342,16.1254369639765,123.684941163944)) ;
#65622 = CARTESIAN_POINT('Ctrl Pts',(-17.904145201317,16.3153591906443,123.494762458891)) ;
#65623 = CARTESIAN_POINT('Ctrl Pts',(-18.2051689666766,16.1353701102815,123.478162945526)) ;
#65624 = CARTESIAN_POINT('Ctrl Pts',(-17.9123613233359,16.3253044464149,123.233570994404)) ;
#65625 = CARTESIAN_POINT('Ctrl Pts',(-18.2117436421572,16.1453153660521,123.269210168122)) ;
#65626 = CARTESIAN_POINT('Ctrl Pts',(-17.9658149650056,16.3352877448534,122.976690048544)) ;
#65627 = CARTESIAN_POINT('Ctrl Pts',(-18.2545082370437,16.1552986644905,123.063705923525)) ;
#65628 = CARTESIAN_POINT('Ctrl Pts',(-18.0638986666255,16.345324925,122.731859880856)) ;
#65629 = CARTESIAN_POINT('Ctrl Pts',(-18.3329769087346,16.1653358446372,122.867842396204)) ;
#65630 = CARTESIAN_POINT('Ctrl Pts',(-18.2001537297579,16.3551794777095,122.511606700127)) ;
#65631 = CARTESIAN_POINT('Ctrl Pts',(-18.4419820544397,16.1751903973466,122.691641395589)) ;
#65632 = CARTESIAN_POINT('Ctrl Pts',(-18.3747984971053,16.3651789961568,122.315323705892)) ;
#65633 = CARTESIAN_POINT('Ctrl Pts',(-18.5816990552253,16.185189915794,122.534616199794)) ;
#65634 = CARTESIAN_POINT('Ctrl Pts',(-18.5786176379803,16.3750740786189,122.153776522294)) ;
#65635 = CARTESIAN_POINT('Ctrl Pts',(-18.7447549194951,16.195084998256,122.405380095778)) ;
#65636 = CARTESIAN_POINT('Ctrl Pts',(-18.8111591522696,16.385134624125,122.028064933009)) ;
#65637 = CARTESIAN_POINT('Ctrl Pts',(-18.9307890798417,16.2051455437621,122.304812173805)) ;
#65638 = CARTESIAN_POINT('Ctrl Pts',(-19.0567347651697,16.394983931373,121.946236873333)) ;
#65639 = CARTESIAN_POINT('Ctrl Pts',(-19.1272492874052,16.2149948510101,122.239351517279)) ;
#65640 = CARTESIAN_POINT('Ctrl Pts',(-19.3172847594668,16.4050110214604,121.906948036796)) ;
#65641 = CARTESIAN_POINT('Ctrl Pts',(-19.3356895344519,16.2250219410975,122.207921911425)) ;
#65642 = CARTESIAN_POINT('Ctrl Pts',(-19.5807454043777,16.4150399255973,121.91419747043)) ;
#65643 = CARTESIAN_POINT('Ctrl Pts',(-19.5464580626688,16.2350508452344,122.213723077586)) ;
#65644 = CARTESIAN_POINT('Ctrl Pts',(-19.8342636546748,16.4248837906966,121.965599859095)) ;
#65645 = CARTESIAN_POINT('Ctrl Pts',(-19.7492714785227,16.2448947103337,122.254846299181)) ;
#65646 = CARTESIAN_POINT('Ctrl Pts',(-20.0789676317228,16.434879617405,122.0611017389)) ;
#65647 = CARTESIAN_POINT('Ctrl Pts',(-19.9450340249279,16.2548905370421,122.331249046834)) ;
#65648 = CARTESIAN_POINT('Ctrl Pts',(-20.3037842341569,16.444904834054,122.198459857618)) ;
#65649 = CARTESIAN_POINT('Ctrl Pts',(-20.1248865660534,16.2649157536911,122.441136831011)) ;
#65650 = CARTESIAN_POINT('Ctrl Pts',(-20.4988993121104,16.4547946662116,122.370150559373)) ;
#65651 = CARTESIAN_POINT('Ctrl Pts',(-20.2809771772072,16.2748055858487,122.578490004565)) ;
#65652 = CARTESIAN_POINT('Ctrl Pts',(-20.6631697043296,16.4647855222963,122.574949866266)) ;
#65653 = CARTESIAN_POINT('Ctrl Pts',(-20.4123923501296,16.2847964419335,122.742330173249)) ;
#65654 = CARTESIAN_POINT('Ctrl Pts',(-20.7887677400445,16.4747306168892,122.804137700936)) ;
#65655 = CARTESIAN_POINT('Ctrl Pts',(-20.512869395449,16.2947415365263,122.925680738138)) ;
#65656 = CARTESIAN_POINT('Ctrl Pts',(-20.8731883104183,16.4846825206573,123.051673973059)) ;
#65657 = CARTESIAN_POINT('Ctrl Pts',(-20.5804045428109,16.3046934402944,123.123709795798)) ;
#65658 = CARTESIAN_POINT('Ctrl Pts',(-20.9134563188917,16.4947189201267,123.312320962728)) ;
#65659 = CARTESIAN_POINT('Ctrl Pts',(-20.612617681498,16.3147298397639,123.332227690102)) ;
#65660 = CARTESIAN_POINT('Ctrl Pts',(-20.9081282976239,16.5046079902154,123.572149884728)) ;
#65661 = CARTESIAN_POINT('Ctrl Pts',(-20.6083540200427,16.3246189098525,123.540090066167)) ;
#65662 = CARTESIAN_POINT('Ctrl Pts',(-20.8577220598271,16.5145972795863,123.829766727629)) ;
#65663 = CARTESIAN_POINT('Ctrl Pts',(-20.5680279279272,16.3346081992234,123.746183149683)) ;
#65664 = CARTESIAN_POINT('Ctrl Pts',(-20.76345961891,16.524555845796,124.073893348995)) ;
#65665 = CARTESIAN_POINT('Ctrl Pts',(-20.4926169796923,16.3445667654331,123.941483690802)) ;
#65666 = CARTESIAN_POINT('Ctrl Pts',(-20.6295786198911,16.5344554170128,124.296968784774)) ;
#65667 = CARTESIAN_POINT('Ctrl Pts',(-20.3855116377468,16.3544663366499,124.119942892736)) ;
#65668 = CARTESIAN_POINT('Ctrl Pts',(-20.4564004098396,16.5445033314271,124.49625876178)) ;
#65669 = CARTESIAN_POINT('Ctrl Pts',(-20.246968141716,16.3645142510642,124.279374299401)) ;
#65670 = CARTESIAN_POINT('Ctrl Pts',(-20.254440134761,16.5543986742876,124.660130610446)) ;
#65671 = CARTESIAN_POINT('Ctrl Pts',(-20.0853998401919,16.3744095939248,124.410470518004)) ;
#65672 = CARTESIAN_POINT('Ctrl Pts',(-20.0233532789183,16.5644603682351,124.788566418278)) ;
#65673 = CARTESIAN_POINT('Ctrl Pts',(-19.9005296298809,16.3844712878722,124.513218396484)) ;
#65674 = CARTESIAN_POINT('Ctrl Pts',(-19.7788459931032,16.5743048213192,124.873119039239)) ;
#65675 = CARTESIAN_POINT('Ctrl Pts',(-19.7049244705946,16.3943157409564,124.580859189868)) ;
#65676 = CARTESIAN_POINT('Ctrl Pts',(-19.5205255375102,16.5842655062777,124.915317433973)) ;
#65677 = CARTESIAN_POINT('Ctrl Pts',(-19.4982683335334,16.4042764259148,124.614617059786)) ;
#65678 = CARTESIAN_POINT('Ctrl Pts',(-19.2568102129339,16.5943014387862,124.911553126493)) ;
#65679 = CARTESIAN_POINT('Ctrl Pts',(-19.2872959783146,16.4143123584233,124.611604711671)) ;
#65680 = CARTESIAN_POINT('Ctrl Pts',(-19.0015211293968,16.6041900544743,124.863040443295)) ;
#65681 = CARTESIAN_POINT('Ctrl Pts',(-19.0830656658347,16.4242009741114,124.572793892405)) ;
#65682 = CARTESIAN_POINT('Ctrl Pts',(-18.7552356821971,16.6142044636167,124.770248444018)) ;
#65683 = CARTESIAN_POINT('Ctrl Pts',(-18.8860375696502,16.4342153832538,124.498559626099)) ;
#65684 = CARTESIAN_POINT('Ctrl Pts',(-18.5287435554736,16.6242382725745,124.635270964711)) ;
#65685 = CARTESIAN_POINT('Ctrl Pts',(-18.7048442231239,16.4442491922116,124.390576829673)) ;
#65686 = CARTESIAN_POINT('Ctrl Pts',(-18.3326680459431,16.6340687268307,124.467023867572)) ;
#65687 = CARTESIAN_POINT('Ctrl Pts',(-18.5479851753716,16.4540796464678,124.255979389229)) ;
#65688 = CARTESIAN_POINT('Ctrl Pts',(-18.164649593129,16.6441463944089,124.262383242805)) ;
#65689 = CARTESIAN_POINT('Ctrl Pts',(-18.4135707132439,16.464157314046,124.092266173035)) ;
#65690 = CARTESIAN_POINT('Ctrl Pts',(-18.037457177748,16.6539982625311,124.03681949593)) ;
#65691 = CARTESIAN_POINT('Ctrl Pts',(-18.3118178639604,16.4740091821683,123.911815773256)) ;
#65692 = CARTESIAN_POINT('Ctrl Pts',(-17.949256848314,16.6640713000965,123.787285292001)) ;
#65693 = CARTESIAN_POINT('Ctrl Pts',(-18.241258048914,16.4840822197336,123.712187880445)) ;
#65694 = CARTESIAN_POINT('Ctrl Pts',(-17.9067465102641,16.6739138534474,123.53212739955)) ;
#65695 = CARTESIAN_POINT('Ctrl Pts',(-18.2072505652693,16.4939247730845,123.508062584724)) ;
#65696 = CARTESIAN_POINT('Ctrl Pts',(-17.908337764321,16.6838942489408,123.269869124294)) ;
#65697 = CARTESIAN_POINT('Ctrl Pts',(-18.208523956492,16.5039051685779,123.29825621506)) ;
#65698 = CARTESIAN_POINT('Ctrl Pts',(-17.9561266808866,16.6939127269186,123.010973721011)) ;
#65699 = CARTESIAN_POINT('Ctrl Pts',(-18.2467556009483,16.5139236465557,123.091139978071)) ;
#65700 = CARTESIAN_POINT('Ctrl Pts',(-18.046394284067,16.7037960412247,122.767407615452)) ;
#65701 = CARTESIAN_POINT('Ctrl Pts',(-18.3189697326464,16.5238069608618,122.896288048403)) ;
#65702 = CARTESIAN_POINT('Ctrl Pts',(-18.1800998015951,16.7138643437634,122.539143460683)) ;
#65703 = CARTESIAN_POINT('Ctrl Pts',(-18.4259346651635,16.5338752634005,122.713676647449)) ;
#65704 = CARTESIAN_POINT('Ctrl Pts',(-18.3471784469217,16.7236943910368,122.342066798614)) ;
#65705 = CARTESIAN_POINT('Ctrl Pts',(-18.5595970360175,16.543705310674,122.556016471638)) ;
#65706 = CARTESIAN_POINT('Ctrl Pts',(-18.5504420735912,16.7337612624523,122.172817736648)) ;
#65707 = CARTESIAN_POINT('Ctrl Pts',(-18.7222083400755,16.5537721820895,122.420617207245)) ;
#65708 = CARTESIAN_POINT('Ctrl Pts',(-18.7760904676618,16.7436503012514,122.043833574538)) ;
#65709 = CARTESIAN_POINT('Ctrl Pts',(-18.9027264648716,16.5636612208885,122.317430542113)) ;
#65710 = CARTESIAN_POINT('Ctrl Pts',(-19.0231340623094,16.7536469993855,121.95457073187)) ;
#65711 = CARTESIAN_POINT('Ctrl Pts',(-19.1003612452814,16.5736579190226,122.246020463371)) ;
#65712 = CARTESIAN_POINT('Ctrl Pts',(-19.2808414151497,16.7635994250975,121.909859064209)) ;
#65713 = CARTESIAN_POINT('Ctrl Pts',(-19.306526737126,16.5836103447346,122.210251379847)) ;
#65714 = CARTESIAN_POINT('Ctrl Pts',(-19.5420687997964,16.7735407273304,121.910209653822)) ;
#65715 = CARTESIAN_POINT('Ctrl Pts',(-19.515508139504,16.5935516469676,122.210531942016)) ;
#65716 = CARTESIAN_POINT('Ctrl Pts',(-19.8004505578449,16.7835239664143,121.955836958364)) ;
#65717 = CARTESIAN_POINT('Ctrl Pts',(-19.7222133350524,16.6035348860515,122.247033765642)) ;
#65718 = CARTESIAN_POINT('Ctrl Pts',(-20.0481664431086,16.7935627679829,122.04650185724)) ;
#65719 = CARTESIAN_POINT('Ctrl Pts',(-19.9203861326362,16.6135736876201,122.319565851317)) ;
#65720 = CARTESIAN_POINT('Ctrl Pts',(-20.27233537467,16.8034108741046,122.175874106053)) ;
#65721 = CARTESIAN_POINT('Ctrl Pts',(-20.0997202925184,16.6234217937417,122.423063076114)) ;
#65722 = CARTESIAN_POINT('Ctrl Pts',(-20.4750293998556,16.8134710696799,122.345566817946)) ;
#65723 = CARTESIAN_POINT('Ctrl Pts',(-20.2618757772164,16.633481989317,122.55881737648)) ;
#65724 = CARTESIAN_POINT('Ctrl Pts',(-20.6422713390571,16.8233687529913,122.544786148084)) ;
#65725 = CARTESIAN_POINT('Ctrl Pts',(-20.3956688189713,16.6433796726285,122.718192224318)) ;
#65726 = CARTESIAN_POINT('Ctrl Pts',(-20.7735531876702,16.8332997933653,122.770334392659)) ;
#65727 = CARTESIAN_POINT('Ctrl Pts',(-20.5006942028639,16.6533107130024,122.898630207615)) ;
#65728 = CARTESIAN_POINT('Ctrl Pts',(-20.864420100794,16.8433420110219,123.018091751125)) ;
#65729 = CARTESIAN_POINT('Ctrl Pts',(-20.5733879339271,16.6633529306591,123.096836198398)) ;
#65730 = CARTESIAN_POINT('Ctrl Pts',(-20.9103551819919,16.8532286717559,123.273822728003)) ;
#65731 = CARTESIAN_POINT('Ctrl Pts',(-20.61013604196,16.673239591393,123.30142008903)) ;
#65732 = CARTESIAN_POINT('Ctrl Pts',(-20.9116383536201,16.8632217803584,123.536414570098)) ;
#65733 = CARTESIAN_POINT('Ctrl Pts',(-20.6111628897148,16.6832326999955,123.511493398078)) ;
#65734 = CARTESIAN_POINT('Ctrl Pts',(-20.8674180471858,16.8731674789966,123.794009449891)) ;
#65735 = CARTESIAN_POINT('Ctrl Pts',(-20.5757870061501,16.6931783986337,123.717568881039)) ;
#65736 = CARTESIAN_POINT('Ctrl Pts',(-20.7796283027966,16.8831147012677,124.04024353424)) ;
#65737 = CARTESIAN_POINT('Ctrl Pts',(-20.5055557607933,16.7031256209048,123.91455585675)) ;
#65738 = CARTESIAN_POINT('Ctrl Pts',(-20.6488602156385,16.8931627268478,124.269630633099)) ;
#65739 = CARTESIAN_POINT('Ctrl Pts',(-20.4009414915831,16.7131736464849,124.0980658808)) ;
#65740 = CARTESIAN_POINT('Ctrl Pts',(-20.4837823786232,16.9030099739907,124.468914512535)) ;
#65741 = CARTESIAN_POINT('Ctrl Pts',(-20.2688802436977,16.7230208936278,124.257492376889)) ;
#65742 = CARTESIAN_POINT('Ctrl Pts',(-20.2848296697992,16.9129731510814,124.639107596571)) ;
#65743 = CARTESIAN_POINT('Ctrl Pts',(-20.1097187494631,16.7329840707186,124.393647070472)) ;
#65744 = CARTESIAN_POINT('Ctrl Pts',(-20.0576375877666,16.9230028721148,124.772718133945)) ;
#65745 = CARTESIAN_POINT('Ctrl Pts',(-19.9279652726105,16.743013791752,124.500535980068)) ;
#65746 = CARTESIAN_POINT('Ctrl Pts',(-19.8138676646833,16.9329073396477,124.864008421836)) ;
#65747 = CARTESIAN_POINT('Ctrl Pts',(-19.7329502140236,16.7529182592849,124.573568505699)) ;
#65748 = CARTESIAN_POINT('Ctrl Pts',(-19.5549188176407,16.9429318254775,124.912240141092)) ;
#65749 = CARTESIAN_POINT('Ctrl Pts',(-19.5257912019944,16.7629427451146,124.612154489046)) ;
#65750 = CARTESIAN_POINT('Ctrl Pts',(-19.2946338276999,16.9528356606014,124.914963066489)) ;
#65751 = CARTESIAN_POINT('Ctrl Pts',(-19.3175639397184,16.7728465802385,124.614333480641)) ;
#65752 = CARTESIAN_POINT('Ctrl Pts',(-19.0340655773043,16.9628868513114,124.871886584455)) ;
#65753 = CARTESIAN_POINT('Ctrl Pts',(-19.1091090337395,16.7828977709485,124.579872926838)) ;
#65754 = CARTESIAN_POINT('Ctrl Pts',(-18.7889990253017,16.9727712939697,124.785703184415)) ;
#65755 = CARTESIAN_POINT('Ctrl Pts',(-18.9130563598052,16.7927822136068,124.510927134029)) ;
#65756 = CARTESIAN_POINT('Ctrl Pts',(-18.5599373549121,16.9827643018216,124.657327597577)) ;
#65757 = CARTESIAN_POINT('Ctrl Pts',(-18.7298067701624,16.8027752214587,124.408227443796)) ;
#65758 = CARTESIAN_POINT('Ctrl Pts',(-18.3575795915092,16.9927126215379,124.491777975001)) ;
#65759 = CARTESIAN_POINT('Ctrl Pts',(-18.5679204008152,16.812723541175,124.275788625095)) ;
#65760 = CARTESIAN_POINT('Ctrl Pts',(-18.186980138861,17.0026494602473,124.294109650112)) ;
#65761 = CARTESIAN_POINT('Ctrl Pts',(-18.4314405125063,16.8226603798844,124.117654920075)) ;
#65762 = CARTESIAN_POINT('Ctrl Pts',(-18.0523597654586,17.0126324491669,124.06890152174)) ;
#65763 = CARTESIAN_POINT('Ctrl Pts',(-18.3237435055854,16.832643368804,123.93748907981)) ;
#65764 = CARTESIAN_POINT('Ctrl Pts',(-17.9587951854769,17.022676328531,123.82213239202)) ;
#65765 = CARTESIAN_POINT('Ctrl Pts',(-18.2488910084418,16.8426872481681,123.740073929916)) ;
#65766 = CARTESIAN_POINT('Ctrl Pts',(-17.9099416408422,17.0325043938894,123.568481191394)) ;
#65767 = CARTESIAN_POINT('Ctrl Pts',(-18.2098074301906,16.8525153135265,123.537154287906)) ;
#65768 = CARTESIAN_POINT('Ctrl Pts',(-17.9056580144789,17.0425814824443,123.303759681484)) ;
#65769 = CARTESIAN_POINT('Ctrl Pts',(-18.2063795179285,16.8625924020815,123.325376748704)) ;
#65770 = CARTESIAN_POINT('Ctrl Pts',(-17.9463150166963,17.0524316346006,123.048052157451)) ;
#65771 = CARTESIAN_POINT('Ctrl Pts',(-18.2389039336585,16.8724425542378,123.120811549314)) ;
#65772 = CARTESIAN_POINT('Ctrl Pts',(-18.032582786432,17.062512115053,122.797658849589)) ;
#65773 = CARTESIAN_POINT('Ctrl Pts',(-18.3079172569512,16.8825230346901,122.920496215202)) ;
#65774 = CARTESIAN_POINT('Ctrl Pts',(-18.1574904407852,17.0723266128218,122.571941098829)) ;
#65775 = CARTESIAN_POINT('Ctrl Pts',(-18.4078418212507,16.8923375324589,122.739922521317)) ;
#65776 = CARTESIAN_POINT('Ctrl Pts',(-18.3234861663821,17.0823949088419,122.36598619016)) ;
#65777 = CARTESIAN_POINT('Ctrl Pts',(-18.5406376345855,16.9024058284791,122.575157613041)) ;
#65778 = CARTESIAN_POINT('Ctrl Pts',(-18.5195111943069,17.0922937413247,122.194881832912)) ;
#65779 = CARTESIAN_POINT('Ctrl Pts',(-18.697456370269,16.9123046609618,122.438273670192)) ;
#65780 = CARTESIAN_POINT('Ctrl Pts',(-18.7455842875903,17.1023466213392,122.058305557914)) ;
#65781 = CARTESIAN_POINT('Ctrl Pts',(-18.878314382243,16.9223575409764,122.329011510998)) ;
#65782 = CARTESIAN_POINT('Ctrl Pts',(-18.9874629412991,17.1122164368354,121.964526142813)) ;
#65783 = CARTESIAN_POINT('Ctrl Pts',(-19.0718160746585,16.9322273564725,122.253987102022)) ;
#65784 = CARTESIAN_POINT('Ctrl Pts',(-19.2470688770235,17.1222891179182,121.913081725806)) ;
#65785 = CARTESIAN_POINT('Ctrl Pts',(-19.2795008526622,16.9423000375553,122.212830257528)) ;
#65786 = CARTESIAN_POINT('Ctrl Pts',(-19.505422587486,17.1321215964892,121.907524515032)) ;
#65787 = CARTESIAN_POINT('Ctrl Pts',(-19.4861827690057,16.9521325161263,122.208383209402)) ;
#65788 = CARTESIAN_POINT('Ctrl Pts',(-19.7660419704814,17.1421522304753,121.946947546496)) ;
#65789 = CARTESIAN_POINT('Ctrl Pts',(-19.6946785626933,16.9621631501124,122.239920201912)) ;
#65790 = CARTESIAN_POINT('Ctrl Pts',(-20.0156574864725,17.1521837876944,122.031770159067)) ;
#65791 = CARTESIAN_POINT('Ctrl Pts',(-19.8943714558458,16.9721947073315,122.307777083162)) ;
#65792 = CARTESIAN_POINT('Ctrl Pts',(-20.2423350956265,17.1620134965661,122.155604235088)) ;
#65793 = CARTESIAN_POINT('Ctrl Pts',(-20.075713330144,16.9820244162032,122.406842617996)) ;
#65794 = CARTESIAN_POINT('Ctrl Pts',(-20.4478540416198,17.1720029453682,122.318940433098)) ;
#65795 = CARTESIAN_POINT('Ctrl Pts',(-20.2401293518006,16.9920138650053,122.537510260585)) ;
#65796 = CARTESIAN_POINT('Ctrl Pts',(-20.6223297569369,17.1820467977682,122.516986010216)) ;
#65797 = CARTESIAN_POINT('Ctrl Pts',(-20.379711079171,17.0020577174053,122.69594586157)) ;
#65798 = CARTESIAN_POINT('Ctrl Pts',(-20.7571853342976,17.1918685111003,122.737058592109)) ;
#65799 = CARTESIAN_POINT('Ctrl Pts',(-20.4875963345862,17.0118794307374,122.872002271996)) ;
#65800 = CARTESIAN_POINT('Ctrl Pts',(-20.8544363834582,17.201903516089,122.982179630652)) ;
#65801 = CARTESIAN_POINT('Ctrl Pts',(-20.5653987506376,17.0219144357261,123.068098568077)) ;
#65802 = CARTESIAN_POINT('Ctrl Pts',(-20.9068811373926,17.2119283545366,123.240357855693)) ;
#65803 = CARTESIAN_POINT('Ctrl Pts',(-20.6073560524299,17.0319392741737,123.274640863138)) ;
#65804 = CARTESIAN_POINT('Ctrl Pts',(-20.9141373279082,17.2217805674918,123.499162698651)) ;
#65805 = CARTESIAN_POINT('Ctrl Pts',(-20.6131626102164,17.0417914871289,123.481683887994)) ;
#65806 = CARTESIAN_POINT('Ctrl Pts',(-20.8762617532287,17.2317705236856,123.758921385039)) ;
#65807 = CARTESIAN_POINT('Ctrl Pts',(-20.5828638652605,17.0517814433227,123.689490938947)) ;
#65808 = CARTESIAN_POINT('Ctrl Pts',(-20.7943806135892,17.2416986339689,124.006649024893)) ;
#65809 = CARTESIAN_POINT('Ctrl Pts',(-20.5173607099962,17.061709553606,123.887673192447)) ;
#65810 = CARTESIAN_POINT('Ctrl Pts',(-20.670345385213,17.2516872340484,124.237992487124)) ;
#65811 = CARTESIAN_POINT('Ctrl Pts',(-20.4181341594561,17.0716981536855,124.07274868766)) ;
#65812 = CARTESIAN_POINT('Ctrl Pts',(-20.5071235397933,17.2617138259759,124.444842800166)) ;
#65813 = CARTESIAN_POINT('Ctrl Pts',(-20.2875580171586,17.081724745613,124.23823002585)) ;
#65814 = CARTESIAN_POINT('Ctrl Pts',(-20.3134293623449,17.2715989540401,124.617932746978)) ;
#65815 = CARTESIAN_POINT('Ctrl Pts',(-20.1326042907807,17.0916098736772,124.376702907249)) ;
#65816 = CARTESIAN_POINT('Ctrl Pts',(-20.0905573668405,17.2815900715136,124.756745161351)) ;
#65817 = CARTESIAN_POINT('Ctrl Pts',(-19.9543077846783,17.1016009911507,124.487754352768)) ;
#65818 = CARTESIAN_POINT('Ctrl Pts',(-19.8455645964301,17.2916306873654,124.854716110604)) ;
#65819 = CARTESIAN_POINT('Ctrl Pts',(-19.7583141598722,17.1116416070025,124.566132786485)) ;
#65820 = CARTESIAN_POINT('Ctrl Pts',(-19.5927130154484,17.3014636782191,124.907962066392)) ;
#65821 = CARTESIAN_POINT('Ctrl Pts',(-19.5560340209557,17.1214745978562,124.60873119612)) ;
#65822 = CARTESIAN_POINT('Ctrl Pts',(-19.330277450202,17.3114568096694,124.917387511024)) ;
#65823 = CARTESIAN_POINT('Ctrl Pts',(-19.3460857391731,17.1314677293065,124.616273501047)) ;
#65824 = CARTESIAN_POINT('Ctrl Pts',(-19.0692386893252,17.3214888581048,124.88041535309)) ;
#65825 = CARTESIAN_POINT('Ctrl Pts',(-19.1372544392363,17.1414997777419,124.58669762411)) ;
#65826 = CARTESIAN_POINT('Ctrl Pts',(-18.822677257513,17.3313541046472,124.800350459875)) ;
#65827 = CARTESIAN_POINT('Ctrl Pts',(-18.9400052547958,17.1513650242843,124.522647715831)) ;
#65828 = CARTESIAN_POINT('Ctrl Pts',(-18.5911545600622,17.341315979474,124.678145049276)) ;
#65829 = CARTESIAN_POINT('Ctrl Pts',(-18.7547863323555,17.1613268991111,124.424885267182)) ;
#65830 = CARTESIAN_POINT('Ctrl Pts',(-18.38313341919,17.3513509425853,124.516091097511)) ;
#65831 = CARTESIAN_POINT('Ctrl Pts',(-18.5883681924007,17.1713618622224,124.295243637103)) ;
#65832 = CARTESIAN_POINT('Ctrl Pts',(-18.2086914290502,17.3612357870477,124.323563591818)) ;
#65833 = CARTESIAN_POINT('Ctrl Pts',(-18.4488134084025,17.1812467066848,124.1412233211)) ;
#65834 = CARTESIAN_POINT('Ctrl Pts',(-18.0678947666769,17.3713018398884,124.099676485538)) ;
#65835 = CARTESIAN_POINT('Ctrl Pts',(-18.3361743120959,17.1913127595256,123.962114606341)) ;
#65836 = CARTESIAN_POINT('Ctrl Pts',(-17.9700726313909,17.3811393557974,123.860326944384)) ;
#65837 = CARTESIAN_POINT('Ctrl Pts',(-18.2579149281125,17.2011502754345,123.770636270255)) ;
#65838 = CARTESIAN_POINT('Ctrl Pts',(-17.9137531151006,17.3912081039063,123.601841075206)) ;
#65839 = CARTESIAN_POINT('Ctrl Pts',(-18.2128572598282,17.2112190235434,123.563847905866)) ;
#65840 = CARTESIAN_POINT('Ctrl Pts',(-17.9034613928053,17.4010886209373,123.342355402501)) ;
#65841 = CARTESIAN_POINT('Ctrl Pts',(-18.2046218361467,17.2210995405744,123.356259859083)) ;
#65842 = CARTESIAN_POINT('Ctrl Pts',(-17.9382344928248,17.4110798078718,123.082149155382)) ;
#65843 = CARTESIAN_POINT('Ctrl Pts',(-18.2324382019981,17.2310907275089,123.148094673223)) ;
#65844 = CARTESIAN_POINT('Ctrl Pts',(-18.0173408799565,17.4210328741467,122.832800782693)) ;
#65845 = CARTESIAN_POINT('Ctrl Pts',(-18.2957212338474,17.2410437937838,122.948615510215)) ;
#65846 = CARTESIAN_POINT('Ctrl Pts',(-18.1395964065383,17.4310687116793,122.599142062341)) ;
#65847 = CARTESIAN_POINT('Ctrl Pts',(-18.3935237856952,17.2510796313164,122.761687546562)) ;
#65848 = CARTESIAN_POINT('Ctrl Pts',(-18.2981116221672,17.4409588378907,122.393154239559)) ;
#65849 = CARTESIAN_POINT('Ctrl Pts',(-18.5203340659042,17.2609697575279,122.596896255148)) ;
#65850 = CARTESIAN_POINT('Ctrl Pts',(-18.4916578231572,17.4509510197987,122.215719190812)) ;
#65851 = CARTESIAN_POINT('Ctrl Pts',(-18.6751695002837,17.2709619394358,122.454946675199)) ;
#65852 = CARTESIAN_POINT('Ctrl Pts',(-18.7121069676179,17.4608969597373,122.075305569039)) ;
#65853 = CARTESIAN_POINT('Ctrl Pts',(-18.8515275002128,17.2809078793744,122.342614056364)) ;
#65854 = CARTESIAN_POINT('Ctrl Pts',(-18.9534274542707,17.4708441435014,121.974794440461)) ;
#65855 = CARTESIAN_POINT('Ctrl Pts',(-19.0445828970662,17.2908550631385,122.262203186491)) ;
#65856 = CARTESIAN_POINT('Ctrl Pts',(-19.211160386698,17.4808920818088,121.917426601221)) ;
#65857 = CARTESIAN_POINT('Ctrl Pts',(-19.2507687776007,17.300903001446,122.216306788302)) ;
#65858 = CARTESIAN_POINT('Ctrl Pts',(-19.4696824314095,17.4907397165491,121.905695967141)) ;
#65859 = CARTESIAN_POINT('Ctrl Pts',(-19.4575859964064,17.3107506361862,122.206920105047)) ;
#65860 = CARTESIAN_POINT('Ctrl Pts',(-19.7293772423961,17.5007014305229,121.938602055784)) ;
#65861 = CARTESIAN_POINT('Ctrl Pts',(-19.6653420282454,17.3207123501601,122.233242742379)) ;
#65862 = CARTESIAN_POINT('Ctrl Pts',(-19.9810217545707,17.5107300653138,122.016948020053)) ;
#65863 = CARTESIAN_POINT('Ctrl Pts',(-19.8666582637803,17.3307409849509,122.295917385593)) ;
#65864 = CARTESIAN_POINT('Ctrl Pts',(-20.2124907996332,17.5206403839109,122.136283881726)) ;
#65865 = CARTESIAN_POINT('Ctrl Pts',(-20.0518343705786,17.340651303548,122.391384019584)) ;
#65866 = CARTESIAN_POINT('Ctrl Pts',(-20.4206686080383,17.5305752402224,122.293854796919)) ;
#65867 = CARTESIAN_POINT('Ctrl Pts',(-20.2183778909395,17.3505861598595,122.517438895075)) ;
#65868 = CARTESIAN_POINT('Ctrl Pts',(-20.6000255828736,17.5406164761831,122.487384162176)) ;
#65869 = CARTESIAN_POINT('Ctrl Pts',(-20.3618650889074,17.3606273958202,122.672260836499)) ;
#65870 = CARTESIAN_POINT('Ctrl Pts',(-20.7410561133952,17.5505032477631,122.70562002418)) ;
#65871 = CARTESIAN_POINT('Ctrl Pts',(-20.4746913307344,17.3705141674002,122.846848200213)) ;
#65872 = CARTESIAN_POINT('Ctrl Pts',(-20.8434772707178,17.5605034264693,122.947591960567)) ;
#65873 = CARTESIAN_POINT('Ctrl Pts',(-20.5566303111727,17.3805143461064,123.040424818321)) ;
#65874 = CARTESIAN_POINT('Ctrl Pts',(-20.9020786278622,17.5704207046789,123.201578349681)) ;
#65875 = CARTESIAN_POINT('Ctrl Pts',(-20.6035135750036,17.390431624316,123.24361335474)) ;
#65876 = CARTESIAN_POINT('Ctrl Pts',(-20.91578288945,17.5804679510926,123.465216930615)) ;
#65877 = CARTESIAN_POINT('Ctrl Pts',(-20.6144792336198,17.4004788707297,123.454524044763)) ;
#65878 = CARTESIAN_POINT('Ctrl Pts',(-20.8843256015444,17.5903418400739,123.722819361991)) ;
#65879 = CARTESIAN_POINT('Ctrl Pts',(-20.5893156441907,17.410352759711,123.660606216813)) ;
#65880 = CARTESIAN_POINT('Ctrl Pts',(-20.8073356878369,17.6004038576544,123.975747950634)) ;
#65881 = CARTESIAN_POINT('Ctrl Pts',(-20.527725890698,17.4204147772915,123.862949679042)) ;
#65882 = CARTESIAN_POINT('Ctrl Pts',(-20.6898154915697,17.6102749193887,124.207021563565)) ;
#65883 = CARTESIAN_POINT('Ctrl Pts',(-20.4337117468578,17.4302858390258,124.047969580495)) ;
#65884 = CARTESIAN_POINT('Ctrl Pts',(-20.5325789116341,17.620268982749,124.417385133982)) ;
#65885 = CARTESIAN_POINT('Ctrl Pts',(-20.307924299848,17.4402799023861,124.216261749645)) ;
#65886 = CARTESIAN_POINT('Ctrl Pts',(-20.3400800616733,17.6303011407824,124.597505830153)) ;
#65887 = CARTESIAN_POINT('Ctrl Pts',(-20.1539268192864,17.4503120604195,124.360359893607)) ;
#65888 = CARTESIAN_POINT('Ctrl Pts',(-20.1232165512678,17.6401650170226,124.739545873156)) ;
#65889 = CARTESIAN_POINT('Ctrl Pts',(-19.9804371926355,17.4601759366597,124.473993837202)) ;
#65890 = CARTESIAN_POINT('Ctrl Pts',(-19.8800594521067,17.6502355316608,124.843920027478)) ;
#65891 = CARTESIAN_POINT('Ctrl Pts',(-19.7859124646786,17.470246451298,124.557495161762)) ;
#65892 = CARTESIAN_POINT('Ctrl Pts',(-19.6283095577294,17.6600761686018,124.90314183829)) ;
#65893 = CARTESIAN_POINT('Ctrl Pts',(-19.5845130945949,17.4800870882389,124.60487484599)) ;
#65894 = CARTESIAN_POINT('Ctrl Pts',(-19.366875274711,17.670043297442,124.918801259543)) ;
#65895 = CARTESIAN_POINT('Ctrl Pts',(-19.375365146763,17.4900542170791,124.61740447096)) ;
#65896 = CARTESIAN_POINT('Ctrl Pts',(-19.1054626465016,17.6800572705665,124.888408905222)) ;
#65897 = CARTESIAN_POINT('Ctrl Pts',(-19.1662371963715,17.5000681902037,124.593093168698)) ;
#65898 = CARTESIAN_POINT('Ctrl Pts',(-18.7709105569482,17.6933420044298,124.788587304081)) ;
#65899 = CARTESIAN_POINT('Ctrl Pts',(-18.8985830635496,17.5133529240669,124.513236786793)) ;
#65900 = CARTESIAN_POINT('Ctrl Pts',(-18.4713115759659,17.7065672691446,124.604860086354)) ;
#65901 = CARTESIAN_POINT('Ctrl Pts',(-18.6588815387832,17.5265781887817,124.36623312436)) ;
#65902 = CARTESIAN_POINT('Ctrl Pts',(-18.23024753484,17.7198777916994,124.351352544017)) ;
#65903 = CARTESIAN_POINT('Ctrl Pts',(-18.4660643742217,17.5398887113366,124.163459835131)) ;
#65904 = CARTESIAN_POINT('Ctrl Pts',(-18.0847456433107,17.7299064366016,124.131627885447)) ;
#65905 = CARTESIAN_POINT('Ctrl Pts',(-18.3496538990184,17.5499173562387,123.987675132136)) ;
#65906 = CARTESIAN_POINT('Ctrl Pts',(-17.9809344252587,17.7397874689555,123.893612632043)) ;
#65907 = CARTESIAN_POINT('Ctrl Pts',(-18.2666046634578,17.5597983885926,123.797265517451)) ;
#65908 = CARTESIAN_POINT('Ctrl Pts',(-17.9188829813947,17.7497684416356,123.638771587196)) ;
#65909 = CARTESIAN_POINT('Ctrl Pts',(-18.2169614863476,17.5697793612727,123.593391459913)) ;
#65910 = CARTESIAN_POINT('Ctrl Pts',(-17.9022490540845,17.7597495692216,123.377020959202)) ;
#65911 = CARTESIAN_POINT('Ctrl Pts',(-18.2036504220169,17.5797604888587,123.383995815664)) ;
#65912 = CARTESIAN_POINT('Ctrl Pts',(-17.940086062115,17.772992759483,123.030998917188)) ;
#65913 = CARTESIAN_POINT('Ctrl Pts',(-18.233927074126,17.5930036791201,123.10715455913)) ;
#65914 = CARTESIAN_POINT('Ctrl Pts',(-18.1006895820262,17.7896607548438,122.618237447441)) ;
#65915 = CARTESIAN_POINT('Ctrl Pts',(-18.3623849444853,17.6096716744809,122.776980015619)) ;
#65916 = CARTESIAN_POINT('Ctrl Pts',(-18.3897812209932,17.8061812548558,122.28765824502)) ;
#65917 = CARTESIAN_POINT('Ctrl Pts',(-18.5937018866241,17.626192174493,122.512467686169)) ;
#65918 = CARTESIAN_POINT('Ctrl Pts',(-18.6800705190158,17.8194942711718,122.092466331838)) ;
#65919 = CARTESIAN_POINT('Ctrl Pts',(-18.8258934626634,17.639505190809,122.356347530936)) ;
#65920 = CARTESIAN_POINT('Ctrl Pts',(-18.9181973224567,17.8294108294048,121.986503440751)) ;
#65921 = CARTESIAN_POINT('Ctrl Pts',(-19.016402860702,17.649421749042,122.271568344734)) ;
#65922 = CARTESIAN_POINT('Ctrl Pts',(-19.1738622433935,17.8394384977077,121.92290647105)) ;
#65923 = CARTESIAN_POINT('Ctrl Pts',(-19.2209295533305,17.6594494173448,122.220690413991)) ;
#65924 = CARTESIAN_POINT('Ctrl Pts',(-19.5194723945054,17.8526190874524,121.898080551952)) ;
#65925 = CARTESIAN_POINT('Ctrl Pts',(-19.4974317792493,17.6726300070895,122.200829004453)) ;
#65926 = CARTESIAN_POINT('Ctrl Pts',(-19.9563231936178,17.8693672265717,121.982455382444)) ;
#65927 = CARTESIAN_POINT('Ctrl Pts',(-19.8468977311799,17.6893781462089,122.268323444308)) ;
#65928 = CARTESIAN_POINT('Ctrl Pts',(-20.4081951552472,17.8891619690823,122.252387033747)) ;
#65929 = CARTESIAN_POINT('Ctrl Pts',(-20.2084028189433,17.7091728887194,122.484267129473)) ;
#65930 = CARTESIAN_POINT('Ctrl Pts',(-20.7451718132866,17.9092063618911,122.66478304066)) ;
#65931 = CARTESIAN_POINT('Ctrl Pts',(-20.4779852136411,17.7292172815282,122.814181443718)) ;
#65932 = CARTESIAN_POINT('Ctrl Pts',(-20.9190608630453,17.9290455441898,123.162728597956)) ;
#65933 = CARTESIAN_POINT('Ctrl Pts',(-20.6171002151294,17.7490564638269,123.212537829593)) ;
#65934 = CARTESIAN_POINT('Ctrl Pts',(-20.9138698455996,17.9489708678827,123.692157121899)) ;
#65935 = CARTESIAN_POINT('Ctrl Pts',(-20.6129501230136,17.7689817875198,123.636081264938)) ;
#65936 = CARTESIAN_POINT('Ctrl Pts',(-20.7282004987486,17.9688945059342,124.188169695646)) ;
#65937 = CARTESIAN_POINT('Ctrl Pts',(-20.4644169876035,17.7889054255713,124.032892793635)) ;
#65938 = CARTESIAN_POINT('Ctrl Pts',(-20.3846133570625,17.9888193793997,124.591069561661)) ;
#65939 = CARTESIAN_POINT('Ctrl Pts',(-20.1895487840061,17.8088302990368,124.355214802049)) ;
#65940 = CARTESIAN_POINT('Ctrl Pts',(-19.9254924402877,18.0086979864787,124.852574068712)) ;
#65941 = CARTESIAN_POINT('Ctrl Pts',(-19.8222521396401,17.8287089061158,124.564420818094)) ;
#65942 = CARTESIAN_POINT('Ctrl Pts',(-19.4021887856867,18.0286754293106,124.94239921452)) ;
#65943 = CARTESIAN_POINT('Ctrl Pts',(-19.403609335955,17.8486863489478,124.636282835405)) ;
#65944 = CARTESIAN_POINT('Ctrl Pts',(-18.8808448567372,18.0486072773953,124.848094480769)) ;
#65945 = CARTESIAN_POINT('Ctrl Pts',(-18.9865332449473,17.8686181970324,124.560840796153)) ;
#65946 = CARTESIAN_POINT('Ctrl Pts',(-18.4236271458194,18.0685025457379,124.582520931676)) ;
#65947 = CARTESIAN_POINT('Ctrl Pts',(-18.620757360624,17.888513465375,124.348382725567)) ;
#65948 = CARTESIAN_POINT('Ctrl Pts',(-18.083533966346,18.08842504415,124.176653707817)) ;
#65949 = CARTESIAN_POINT('Ctrl Pts',(-18.3486814135184,17.9084359637871,124.023689002201)) ;
#65950 = CARTESIAN_POINT('Ctrl Pts',(-17.9021445000866,18.108384526026,123.678105539859)) ;
#65951 = CARTESIAN_POINT('Ctrl Pts',(-18.2035687540983,17.9283954456631,123.624850383669)) ;
#65952 = CARTESIAN_POINT('Ctrl Pts',(-17.901677043034,18.1282622784854,123.149870596743)) ;
#65953 = CARTESIAN_POINT('Ctrl Pts',(-18.2031940192158,17.9482731981225,123.202260912629)) ;
#65954 = CARTESIAN_POINT('Ctrl Pts',(-18.0801792550787,18.1481440692199,122.65239779122)) ;
#65955 = CARTESIAN_POINT('Ctrl Pts',(-18.3459964494123,17.9681549888571,122.804281306169)) ;
#65956 = CARTESIAN_POINT('Ctrl Pts',(-18.4216843162061,18.1682174080709,122.242598944837)) ;
#65957 = CARTESIAN_POINT('Ctrl Pts',(-18.6191997939776,17.988228327708,122.476442865587)) ;
#65958 = CARTESIAN_POINT('Ctrl Pts',(-18.8764446818162,18.1880218753067,121.977323375824)) ;
#65959 = CARTESIAN_POINT('Ctrl Pts',(-18.983010300815,18.0080327949438,122.26422127326)) ;
#65960 = CARTESIAN_POINT('Ctrl Pts',(-19.3987200282656,18.2080052157145,121.881178045719)) ;
#65961 = CARTESIAN_POINT('Ctrl Pts',(-19.4008309101687,18.0280161353516,122.187305861256)) ;
#65962 = CARTESIAN_POINT('Ctrl Pts',(-19.9205934708167,18.2279201803125,121.969578565073)) ;
#65963 = CARTESIAN_POINT('Ctrl Pts',(-19.8183305317221,18.0479310999496,122.258027130134)) ;
#65964 = CARTESIAN_POINT('Ctrl Pts',(-20.3807158505364,18.2477887150289,122.228912632756)) ;
#65965 = CARTESIAN_POINT('Ctrl Pts',(-20.1864289023512,18.067799634666,122.465496375139)) ;
#65966 = CARTESIAN_POINT('Ctrl Pts',(-20.7270809482803,18.2678410992406,122.6337729235)) ;
#65967 = CARTESIAN_POINT('Ctrl Pts',(-20.4635196475679,18.0878520188777,122.789385098956)) ;
#65968 = CARTESIAN_POINT('Ctrl Pts',(-20.9126860426018,18.2876150630298,123.125692137824)) ;
#65969 = CARTESIAN_POINT('Ctrl Pts',(-20.6120028561782,18.1076259826669,123.182923161825)) ;
#65970 = CARTESIAN_POINT('Ctrl Pts',(-20.919787056096,18.3076694420512,123.658444810698)) ;
#65971 = CARTESIAN_POINT('Ctrl Pts',(-20.6176815610967,18.1276803616883,123.609124837985)) ;
#65972 = CARTESIAN_POINT('Ctrl Pts',(-20.7465962162573,18.3274661796244,124.155452562203)) ;
#65973 = CARTESIAN_POINT('Ctrl Pts',(-20.4791262659657,18.1474770992615,124.006732040671)) ;
#65974 = CARTESIAN_POINT('Ctrl Pts',(-20.4126446942546,18.3474339919759,124.567768827108)) ;
#65975 = CARTESIAN_POINT('Ctrl Pts',(-20.2119627251939,18.167444911613,124.336583477204)) ;
#65976 = CARTESIAN_POINT('Ctrl Pts',(-19.9576212451287,18.3673929680409,124.840656736435)) ;
#65977 = CARTESIAN_POINT('Ctrl Pts',(-19.8479423832508,18.187403887678,124.554891689415)) ;
#65978 = CARTESIAN_POINT('Ctrl Pts',(-19.4386451944303,18.3872878863183,124.941871042673)) ;
#65979 = CARTESIAN_POINT('Ctrl Pts',(-19.4327602304496,18.2072988059554,124.635860461353)) ;
#65980 = CARTESIAN_POINT('Ctrl Pts',(-18.9161726453232,18.4071841987686,124.860555263088)) ;
#65981 = CARTESIAN_POINT('Ctrl Pts',(-19.0147819951874,18.2271951184057,124.570804600373)) ;
#65982 = CARTESIAN_POINT('Ctrl Pts',(-18.4521815633956,18.4270921321427,124.606153931591)) ;
#65983 = CARTESIAN_POINT('Ctrl Pts',(-18.6435902854391,18.2471030517799,124.367280294003)) ;
#65984 = CARTESIAN_POINT('Ctrl Pts',(-18.1022181077,18.4470420224312,124.207874213592)) ;
#65985 = CARTESIAN_POINT('Ctrl Pts',(-18.3636220163142,18.2670529420683,124.048653992795)) ;
#65986 = CARTESIAN_POINT('Ctrl Pts',(-17.9093397630461,18.4669192529325,123.715982843254)) ;
#65987 = CARTESIAN_POINT('Ctrl Pts',(-18.2093224069639,18.2869301725696,123.655139058645)) ;
#65988 = CARTESIAN_POINT('Ctrl Pts',(-17.8955552161801,18.4869019218035,123.185081472576)) ;
#65989 = CARTESIAN_POINT('Ctrl Pts',(-18.1982991666636,18.3069128414406,123.230417568849)) ;
#65990 = CARTESIAN_POINT('Ctrl Pts',(-18.0637189576036,18.5068348083839,122.682625101242)) ;
#65991 = CARTESIAN_POINT('Ctrl Pts',(-18.3328317622398,18.326845728021,122.82845440733)) ;
#65992 = CARTESIAN_POINT('Ctrl Pts',(-18.3925705510188,18.5267475544018,122.267998602716)) ;
#65993 = CARTESIAN_POINT('Ctrl Pts',(-18.5959242479568,18.3467584740389,122.496751834392)) ;
#65994 = CARTESIAN_POINT('Ctrl Pts',(-18.767281881698,18.5433172757436,122.036622749478)) ;
#65995 = CARTESIAN_POINT('Ctrl Pts',(-18.8956708387233,18.3633281953808,122.311665074245)) ;
#65996 = CARTESIAN_POINT('Ctrl Pts',(-19.1020056145289,18.5566172870486,121.936011376313)) ;
#65997 = CARTESIAN_POINT('Ctrl Pts',(-19.1634797346767,18.3766282066857,122.231169157369)) ;
#65998 = CARTESIAN_POINT('Ctrl Pts',(-19.4482877506077,18.5698874747985,121.89465138511)) ;
#65999 = CARTESIAN_POINT('Ctrl Pts',(-19.4404490281102,18.3898983944356,122.198083477283)) ;
#66000 = CARTESIAN_POINT('Ctrl Pts',(-19.8857560482088,18.5865148571639,121.957313792384)) ;
#66001 = CARTESIAN_POINT('Ctrl Pts',(-19.7904920476466,18.406525776801,122.248222840253)) ;
#66002 = CARTESIAN_POINT('Ctrl Pts',(-20.2753787251303,18.6031371469091,122.165595250357)) ;
#66003 = CARTESIAN_POINT('Ctrl Pts',(-20.1021439506729,18.4231480665462,122.414835475618)) ;
#66004 = CARTESIAN_POINT('Ctrl Pts',(-20.5295847929134,18.6163823613036,122.403352527217)) ;
#66005 = CARTESIAN_POINT('Ctrl Pts',(-20.3055329796882,18.4363932809408,122.60505706455)) ;
#66006 = CARTESIAN_POINT('Ctrl Pts',(-20.6866624263127,18.6262943262643,122.611158628173)) ;
#66007 = CARTESIAN_POINT('Ctrl Pts',(-20.4311881581819,18.4463052459014,122.771300643665)) ;
#66008 = CARTESIAN_POINT('Ctrl Pts',(-20.8067318368115,18.6363529494288,122.846612050245)) ;
#66009 = CARTESIAN_POINT('Ctrl Pts',(-20.5272430699789,18.4563638690659,122.959664983458)) ;
#66010 = CARTESIAN_POINT('Ctrl Pts',(-20.882799746978,18.6461930635446,123.093798587262)) ;
#66011 = CARTESIAN_POINT('Ctrl Pts',(-20.5880949652043,18.4662039831817,123.157414861851)) ;
#66012 = CARTESIAN_POINT('Ctrl Pts',(-20.9157793856879,18.6562588485022,123.356213554678)) ;
#66013 = CARTESIAN_POINT('Ctrl Pts',(-20.6144765429298,18.4762697681393,123.367347025587)) ;
#66014 = CARTESIAN_POINT('Ctrl Pts',(-20.9028157443252,18.6661421662901,123.615646798569)) ;
#66015 = CARTESIAN_POINT('Ctrl Pts',(-20.6041033763825,18.4861530859272,123.574893593804)) ;
#66016 = CARTESIAN_POINT('Ctrl Pts',(-20.8449533316139,18.6761316041487,123.871675964814)) ;
#66017 = CARTESIAN_POINT('Ctrl Pts',(-20.5578112681338,18.4961425237858,123.779716386074)) ;
#66018 = CARTESIAN_POINT('Ctrl Pts',(-20.7436744284095,18.6860953182014,124.113145006398)) ;
#66019 = CARTESIAN_POINT('Ctrl Pts',(-20.4767860825283,18.5061062378385,123.972890731368)) ;
#66020 = CARTESIAN_POINT('Ctrl Pts',(-20.6017905558508,18.6960903298606,124.334207674781)) ;
#66021 = CARTESIAN_POINT('Ctrl Pts',(-20.3632771185327,18.5161012494978,124.149739604004)) ;
#66022 = CARTESIAN_POINT('Ctrl Pts',(-20.4226612590053,18.7061266215549,124.527770408748)) ;
#66023 = CARTESIAN_POINT('Ctrl Pts',(-20.2199720814813,18.526137541192,124.304588217699)) ;
#66024 = CARTESIAN_POINT('Ctrl Pts',(-20.2168518529892,18.7159729992483,124.684624557531)) ;
#66025 = CARTESIAN_POINT('Ctrl Pts',(-20.0553231661172,18.5359839188854,124.430069764472)) ;
#66026 = CARTESIAN_POINT('Ctrl Pts',(-19.9839760536042,18.725957943399,124.805452933041)) ;
#66027 = CARTESIAN_POINT('Ctrl Pts',(-19.8690215418316,18.5459688630361,124.526730426201)) ;
#66028 = CARTESIAN_POINT('Ctrl Pts',(-19.7348307743134,18.735894914529,124.883803103654)) ;
#66029 = CARTESIAN_POINT('Ctrl Pts',(-19.6697046968684,18.5559058341661,124.589408393291)) ;
#66030 = CARTESIAN_POINT('Ctrl Pts',(-19.4729748038764,18.7459446991607,124.917940423187)) ;
#66031 = CARTESIAN_POINT('Ctrl Pts',(-19.4602196750584,18.5659556187978,124.616716001048)) ;
#66032 = CARTESIAN_POINT('Ctrl Pts',(-19.21434799551,18.7557951612382,124.906522324717)) ;
#66033 = CARTESIAN_POINT('Ctrl Pts',(-19.2533184225446,18.5758060808753,124.607579270633)) ;
#66034 = CARTESIAN_POINT('Ctrl Pts',(-18.9584174462669,18.7657671747586,124.850357148989)) ;
#66035 = CARTESIAN_POINT('Ctrl Pts',(-19.0485745563845,18.5857780943957,124.562644952603)) ;
#66036 = CARTESIAN_POINT('Ctrl Pts',(-18.7155078312172,18.775762321878,124.750315034863)) ;
#66037 = CARTESIAN_POINT('Ctrl Pts',(-18.8542477777451,18.5957732415151,124.48260921036)) ;
#66038 = CARTESIAN_POINT('Ctrl Pts',(-18.493022848757,18.7857962916141,124.608834245128)) ;
#66039 = CARTESIAN_POINT('Ctrl Pts',(-18.6762610286674,18.6058072112512,124.369422690082)) ;
#66040 = CARTESIAN_POINT('Ctrl Pts',(-18.3016334315015,18.7956518372847,124.434305714712)) ;
#66041 = CARTESIAN_POINT('Ctrl Pts',(-18.5231511449158,18.6156627569218,124.229798335907)) ;
#66042 = CARTESIAN_POINT('Ctrl Pts',(-18.140904940295,18.8056505942979,124.226495189743)) ;
#66043 = CARTESIAN_POINT('Ctrl Pts',(-18.394570163324,18.6256615139351,124.063548607924)) ;
#66044 = CARTESIAN_POINT('Ctrl Pts',(-18.019684455447,18.8155477295351,123.99634137885)) ;
#66045 = CARTESIAN_POINT('Ctrl Pts',(-18.2975958304662,18.6355586491722,123.87942470902)) ;
#66046 = CARTESIAN_POINT('Ctrl Pts',(-17.93899129175,18.8256008253747,123.744810345997)) ;
#66047 = CARTESIAN_POINT('Ctrl Pts',(-18.2330434068114,18.6456117450119,123.678199198287)) ;
#66048 = CARTESIAN_POINT('Ctrl Pts',(-17.9037702162779,18.8354843341053,123.487463211661)) ;
#66049 = CARTESIAN_POINT('Ctrl Pts',(-18.2048687720169,18.6554952537425,123.472321440138)) ;
#66050 = CARTESIAN_POINT('Ctrl Pts',(-17.9132654845491,18.8454792067514,123.224988077224)) ;
#66051 = CARTESIAN_POINT('Ctrl Pts',(-18.2124671563329,18.6654901263886,123.262341496769)) ;
#66052 = CARTESIAN_POINT('Ctrl Pts',(-17.9687343278623,18.8554991683871,122.967567757792)) ;
#66053 = CARTESIAN_POINT('Ctrl Pts',(-18.2568443761274,18.6755100880243,123.056405729243)) ;
#66054 = CARTESIAN_POINT('Ctrl Pts',(-18.0667115840973,18.865404532187,122.726412358638)) ;
#66055 = CARTESIAN_POINT('Ctrl Pts',(-18.3352281137652,18.6854154518241,122.863482464888)) ;
#66056 = CARTESIAN_POINT('Ctrl Pts',(-18.2051056278125,18.8753451197945,122.504876382137)) ;
#66057 = CARTESIAN_POINT('Ctrl Pts',(-18.4459450547457,18.6953560394316,122.68625500378)) ;
#66058 = CARTESIAN_POINT('Ctrl Pts',(-18.3808775940096,18.8853479378952,122.309383985207)) ;
#66059 = CARTESIAN_POINT('Ctrl Pts',(-18.5865641665979,18.7053588575323,122.529862558861)) ;
#66060 = CARTESIAN_POINT('Ctrl Pts',(-18.5888129419843,18.8953826496193,122.147230647452)) ;
#66061 = CARTESIAN_POINT('Ctrl Pts',(-18.7529137900349,18.7153935692564,122.40014159165)) ;
#66062 = CARTESIAN_POINT('Ctrl Pts',(-18.8171608789422,18.9052275563566,122.025580674038)) ;
#66063 = CARTESIAN_POINT('Ctrl Pts',(-18.9355927397188,18.7252384759937,122.302823704996)) ;
#66064 = CARTESIAN_POINT('Ctrl Pts',(-19.066475495053,18.9152134089256,121.943828689904)) ;
#66065 = CARTESIAN_POINT('Ctrl Pts',(-19.1350449591221,18.7352243285627,122.237424137714)) ;
#66066 = CARTESIAN_POINT('Ctrl Pts',(-19.3249330398174,18.9251482173387,121.906600838846)) ;
#66067 = CARTESIAN_POINT('Ctrl Pts',(-19.3418110288155,18.7451591369758,122.207643930442)) ;
#66068 = CARTESIAN_POINT('Ctrl Pts',(-19.5890580305708,18.9352057444197,121.915149697282)) ;
#66069 = CARTESIAN_POINT('Ctrl Pts',(-19.5531110478041,18.7552166640568,122.214485107576)) ;
#66070 = CARTESIAN_POINT('Ctrl Pts',(-19.8417664438443,18.9450273994168,121.967782613312)) ;
#66071 = CARTESIAN_POINT('Ctrl Pts',(-19.7552767463782,18.7650383190539,122.256593308813)) ;
#66072 = CARTESIAN_POINT('Ctrl Pts',(-20.0873540689241,18.9550834435898,122.065301218056)) ;
#66073 = CARTESIAN_POINT('Ctrl Pts',(-19.9517461977428,18.775094363227,122.334610067724)) ;
#66074 = CARTESIAN_POINT('Ctrl Pts',(-20.3094798342934,18.965024183635,122.20280861514)) ;
#66075 = CARTESIAN_POINT('Ctrl Pts',(-20.1294455077566,18.7850351032721,122.444617579698)) ;
#66076 = CARTESIAN_POINT('Ctrl Pts',(-20.5041752042223,18.9749283047079,122.375539516404)) ;
#66077 = CARTESIAN_POINT('Ctrl Pts',(-20.2852002006892,18.794939224345,122.582803465436)) ;
#66078 = CARTESIAN_POINT('Ctrl Pts',(-20.6681231446912,18.9849758458621,122.58248803559)) ;
#66079 = CARTESIAN_POINT('Ctrl Pts',(-20.416357069613,18.8049867654992,122.748363557921)) ;
#66080 = CARTESIAN_POINT('Ctrl Pts',(-20.7919825435621,18.9948745974625,122.811275811282)) ;
#66081 = CARTESIAN_POINT('Ctrl Pts',(-20.5154426771701,18.8148855170996,122.931394296776)) ;
#66082 = CARTESIAN_POINT('Ctrl Pts',(-20.8755683816824,19.0049230764283,123.061730492506)) ;
#66083 = CARTESIAN_POINT('Ctrl Pts',(-20.5823095619046,18.8249339960654,123.131758740942)) ;
#66084 = CARTESIAN_POINT('Ctrl Pts',(-20.9138033739238,19.014810573512,123.318762800787)) ;
#66085 = CARTESIAN_POINT('Ctrl Pts',(-20.612895591588,18.8348214931492,123.33738436397)) ;
#66086 = CARTESIAN_POINT('Ctrl Pts',(-20.9072423074913,19.0248036638101,123.581265757207)) ;
#66087 = CARTESIAN_POINT('Ctrl Pts',(-20.6076449012029,18.8448145834472,123.547386559869)) ;
#66088 = CARTESIAN_POINT('Ctrl Pts',(-20.8553184944048,19.0347558338704,123.837608299615)) ;
#66089 = CARTESIAN_POINT('Ctrl Pts',(-20.5661040904152,18.8547667535075,123.752459944652)) ;
#66090 = CARTESIAN_POINT('Ctrl Pts',(-20.7601517684657,19.0446942537849,124.080804362951)) ;
#66091 = CARTESIAN_POINT('Ctrl Pts',(-20.4899691655713,18.864705173422,123.947015810628)) ;
#66092 = CARTESIAN_POINT('Ctrl Pts',(-20.6237942335491,19.0546793838705,124.305021774752)) ;
#66093 = CARTESIAN_POINT('Ctrl Pts',(-20.3808817246997,18.8746903035076,124.126388699509)) ;
#66094 = CARTESIAN_POINT('Ctrl Pts',(-20.4494165139908,19.0647160732846,124.502884010772)) ;
#66095 = CARTESIAN_POINT('Ctrl Pts',(-20.2413781403973,18.8847269929217,124.284677342677)) ;
#66096 = CARTESIAN_POINT('Ctrl Pts',(-20.2472957009717,19.0745707572771,124.664826057112)) ;
#66097 = CARTESIAN_POINT('Ctrl Pts',(-20.0796809747905,18.8945816769142,124.414229158598)) ;
#66098 = CARTESIAN_POINT('Ctrl Pts',(-20.0170234288064,19.0845702413249,124.791326058903)) ;
#66099 = CARTESIAN_POINT('Ctrl Pts',(-19.8954624401579,18.9045811609621,124.515427632247)) ;
#66100 = CARTESIAN_POINT('Ctrl Pts',(-19.7708869846679,19.0944653301018,124.875329679388)) ;
#66101 = CARTESIAN_POINT('Ctrl Pts',(-19.6985533150144,18.914476249739,124.582628795942)) ;
#66102 = CARTESIAN_POINT('Ctrl Pts',(-19.5096800897201,19.104525884748,124.915950078661)) ;
#66103 = CARTESIAN_POINT('Ctrl Pts',(-19.4895873565871,18.9245368043851,124.61512352611)) ;
#66104 = CARTESIAN_POINT('Ctrl Pts',(-19.2508813050788,19.1143751491209,124.910856545189)) ;
#66105 = CARTESIAN_POINT('Ctrl Pts',(-19.2825491948916,18.934386068758,124.611047106101)) ;
#66106 = CARTESIAN_POINT('Ctrl Pts',(-18.99220707569,19.1244024015687,124.86066175785)) ;
#66107 = CARTESIAN_POINT('Ctrl Pts',(-19.0756100641405,18.9444133212059,124.570889813033)) ;
#66108 = CARTESIAN_POINT('Ctrl Pts',(-18.7463833099064,19.1344306991389,124.765652294078)) ;
#66109 = CARTESIAN_POINT('Ctrl Pts',(-18.8789515818906,18.954441618776,124.49488071212)) ;
#66110 = CARTESIAN_POINT('Ctrl Pts',(-18.5246504442198,19.1442768281449,124.632315524006)) ;
#66111 = CARTESIAN_POINT('Ctrl Pts',(-18.7015668443456,18.964287747782,124.388210457223)) ;
#66112 = CARTESIAN_POINT('Ctrl Pts',(-18.3260692253604,19.154270733507,124.460445802928)) ;
#66113 = CARTESIAN_POINT('Ctrl Pts',(-18.54270288402,18.9742816531441,124.250713721188)) ;
#66114 = CARTESIAN_POINT('Ctrl Pts',(-18.1602075359614,19.16429483119,124.255787351941)) ;
#66115 = CARTESIAN_POINT('Ctrl Pts',(-18.4100146618778,18.9843057508271,124.0869859934)) ;
#66116 = CARTESIAN_POINT('Ctrl Pts',(-18.0338280399953,19.174184659044,124.028684394348)) ;
#66117 = CARTESIAN_POINT('Ctrl Pts',(-18.3089126375273,18.9941955786812,123.905303536338)) ;
#66118 = CARTESIAN_POINT('Ctrl Pts',(-17.947565914458,19.1841766404745,123.780690475578)) ;
#66119 = CARTESIAN_POINT('Ctrl Pts',(-18.2399042544237,19.0041875601116,123.706908101772)) ;
#66120 = CARTESIAN_POINT('Ctrl Pts',(-17.9059220811503,19.1941236452403,123.522631607328)) ;
#66121 = CARTESIAN_POINT('Ctrl Pts',(-18.2065905909474,19.0141345648774,123.500461190172)) ;
#66122 = CARTESIAN_POINT('Ctrl Pts',(-17.9092390395663,19.2040732966301,123.261175270493)) ;
#66123 = CARTESIAN_POINT('Ctrl Pts',(-18.2092454041741,19.0240842162672,123.291296521161)) ;
#66124 = CARTESIAN_POINT('Ctrl Pts',(-17.958538306793,19.2141102996075,123.002069408009)) ;
#66125 = CARTESIAN_POINT('Ctrl Pts',(-18.2486861142578,19.0341212192446,123.084011970538)) ;
#66126 = CARTESIAN_POINT('Ctrl Pts',(-18.0505326598567,19.2239992080425,122.759016798404)) ;
#66127 = CARTESIAN_POINT('Ctrl Pts',(-18.3222825144302,19.0440101276797,122.88957101701)) ;
#66128 = CARTESIAN_POINT('Ctrl Pts',(-18.1842635126106,19.23398854052,122.533132432072)) ;
#66129 = CARTESIAN_POINT('Ctrl Pts',(-18.429268104139,19.0539994601571,122.708864261039)) ;
#66130 = CARTESIAN_POINT('Ctrl Pts',(-18.3548053010277,19.2439470959571,122.334641591459)) ;
#66131 = CARTESIAN_POINT('Ctrl Pts',(-18.5657022198966,19.0639580155942,122.550072634139)) ;
#66132 = CARTESIAN_POINT('Ctrl Pts',(-18.5556335270977,19.2538466671576,122.169248739393)) ;
#66133 = CARTESIAN_POINT('Ctrl Pts',(-18.7263649283418,19.0738575867947,122.417759614696)) ;
#66134 = CARTESIAN_POINT('Ctrl Pts',(-18.7855306745994,19.2638945924096,122.039423510114)) ;
#66135 = CARTESIAN_POINT('Ctrl Pts',(-18.910283328349,19.0839055120467,122.313900283675)) ;
#66136 = CARTESIAN_POINT('Ctrl Pts',(-19.0306926009335,19.2737898919356,121.952607002251)) ;
#66137 = CARTESIAN_POINT('Ctrl Pts',(-19.1064125243075,19.0938008115727,122.244448292274)) ;
#66138 = CARTESIAN_POINT('Ctrl Pts',(-19.2914444276105,19.2838517483836,121.908933829335)) ;
#66139 = CARTESIAN_POINT('Ctrl Pts',(-19.3150144124183,19.1038626680207,122.209510720343)) ;
#66140 = CARTESIAN_POINT('Ctrl Pts',(-19.5501343610573,19.2936955948002,121.911097613413)) ;
#66141 = CARTESIAN_POINT('Ctrl Pts',(-19.5219652921603,19.1137065144373,122.211242751695)) ;
#66142 = CARTESIAN_POINT('Ctrl Pts',(-19.8077343935755,19.3036585439283,121.957822195286)) ;
#66143 = CARTESIAN_POINT('Ctrl Pts',(-19.7280448206616,19.1236694635654,122.248623138328)) ;
#66144 = CARTESIAN_POINT('Ctrl Pts',(-20.0549291177178,19.3136925803563,122.049626315006)) ;
#66145 = CARTESIAN_POINT('Ctrl Pts',(-19.9258003882064,19.1337034999934,122.322067316074)) ;
#66146 = CARTESIAN_POINT('Ctrl Pts',(-20.2792335465816,19.3235800073143,122.18076820435)) ;
#66147 = CARTESIAN_POINT('Ctrl Pts',(-20.1052428067102,19.1435909269514,122.426981141854)) ;
#66148 = CARTESIAN_POINT('Ctrl Pts',(-20.4802444747173,19.3335944416507,122.350655841088)) ;
#66149 = CARTESIAN_POINT('Ctrl Pts',(-20.2660510795986,19.1536053612878,122.562891792175)) ;
#66150 = CARTESIAN_POINT('Ctrl Pts',(-20.6485175407954,19.3436293862856,122.553674509814)) ;
#66151 = CARTESIAN_POINT('Ctrl Pts',(-20.4006689258585,19.1636403059227,122.725307374417)) ;
#66152 = CARTESIAN_POINT('Ctrl Pts',(-20.7769890298325,19.3534617363166,122.777893029322)) ;
#66153 = CARTESIAN_POINT('Ctrl Pts',(-20.5034449148929,19.1734726559537,122.904681511226)) ;
#66154 = CARTESIAN_POINT('Ctrl Pts',(-20.8667862746344,19.3635371754338,123.026918659849)) ;
#66155 = CARTESIAN_POINT('Ctrl Pts',(-20.5752821883899,19.183548095071,123.103902590368)) ;
#66156 = CARTESIAN_POINT('Ctrl Pts',(-20.9111458115105,19.3733896406684,123.282059452494)) ;
#66157 = CARTESIAN_POINT('Ctrl Pts',(-20.6107689973514,19.1934005603056,123.308014298688)) ;
#66158 = CARTESIAN_POINT('Ctrl Pts',(-20.9107290324318,19.3834625182453,123.546718673386)) ;
#66159 = CARTESIAN_POINT('Ctrl Pts',(-20.6104349741825,19.2034734378824,123.519742024396)) ;
#66160 = CARTESIAN_POINT('Ctrl Pts',(-20.8653781808651,19.3933051144378,123.801387925564)) ;
#66161 = CARTESIAN_POINT('Ctrl Pts',(-20.5741538923526,19.2133160340749,123.723476203268)) ;
#66162 = CARTESIAN_POINT('Ctrl Pts',(-20.7760923678515,19.4032854985531,124.047984519831)) ;
#66163 = CARTESIAN_POINT('Ctrl Pts',(-20.5027249602154,19.2232964181902,123.920753112728)) ;
#66164 = CARTESIAN_POINT('Ctrl Pts',(-20.6443997501556,19.4133039792019,124.275948701137)) ;
#66165 = CARTESIAN_POINT('Ctrl Pts',(-20.3973704129932,19.233314898839,124.103124205952)) ;
#66166 = CARTESIAN_POINT('Ctrl Pts',(-20.4778099653252,19.4231872942023,124.475248963833)) ;
#66167 = CARTESIAN_POINT('Ctrl Pts',(-20.2640988584677,19.2431982138394,124.262563499982)) ;
#66168 = CARTESIAN_POINT('Ctrl Pts',(-20.2754104277972,19.4332555912927,124.645589428262)) ;
#66169 = CARTESIAN_POINT('Ctrl Pts',(-20.1021787138093,19.2532665109298,124.398835770553)) ;
#66170 = CARTESIAN_POINT('Ctrl Pts',(-20.0520012191522,19.443085659665,124.775372441285)) ;
#66171 = CARTESIAN_POINT('Ctrl Pts',(-19.9234522479264,19.2630965793021,124.502661276645)) ;
#66172 = CARTESIAN_POINT('Ctrl Pts',(-19.8038135625138,19.4531524521334,124.86681341649)) ;
#66173 = CARTESIAN_POINT('Ctrl Pts',(-19.7249017349538,19.2731633717705,124.575813934512)) ;
#66174 = CARTESIAN_POINT('Ctrl Pts',(-19.5479941097252,19.4630417856219,124.912847154411)) ;
#66175 = CARTESIAN_POINT('Ctrl Pts',(-19.5202469635521,19.2830527052591,124.612640501714)) ;
#66176 = CARTESIAN_POINT('Ctrl Pts',(-19.2851987471319,19.473043917038,124.914186378401)) ;
#66177 = CARTESIAN_POINT('Ctrl Pts',(-19.3100107840446,19.2930548366751,124.613711708274)) ;
#66178 = CARTESIAN_POINT('Ctrl Pts',(-19.0280693627692,19.482967786659,124.870372052193)) ;
#66179 = CARTESIAN_POINT('Ctrl Pts',(-19.1043078948215,19.3029787062961,124.578660218181)) ;
#66180 = CARTESIAN_POINT('Ctrl Pts',(-18.7796000674895,19.4930113021762,124.781474531052)) ;
#66181 = CARTESIAN_POINT('Ctrl Pts',(-18.9055323440351,19.3130222218133,124.507542000366)) ;
#66182 = CARTESIAN_POINT('Ctrl Pts',(-18.5537969176444,19.5028935150645,124.653102676941)) ;
#66183 = CARTESIAN_POINT('Ctrl Pts',(-18.7248906370469,19.3229044347016,124.404844891224)) ;
#66184 = CARTESIAN_POINT('Ctrl Pts',(-18.3500292628219,19.5129615922839,124.484417808806)) ;
#66185 = CARTESIAN_POINT('Ctrl Pts',(-18.5618763184921,19.332972511921,124.269896733581)) ;
#66186 = CARTESIAN_POINT('Ctrl Pts',(-18.1823173295114,19.5228000970181,124.287590469283)) ;
#66187 = CARTESIAN_POINT('Ctrl Pts',(-18.4277075526952,19.3428110166552,124.112435753387)) ;
#66188 = CARTESIAN_POINT('Ctrl Pts',(-18.04805852035,19.5328628654475,124.059806889975)) ;
#66189 = CARTESIAN_POINT('Ctrl Pts',(-18.3203002879426,19.3528737850846,123.930208672601)) ;
#66190 = CARTESIAN_POINT('Ctrl Pts',(-17.9571650618813,19.5427598587302,123.816107138229)) ;
#66191 = CARTESIAN_POINT('Ctrl Pts',(-18.247585798284,19.3627707783674,123.735249623978)) ;
#66192 = CARTESIAN_POINT('Ctrl Pts',(-17.9089504191746,19.552691086365,123.559623490826)) ;
#66193 = CARTESIAN_POINT('Ctrl Pts',(-18.2090139678198,19.3727020060021,123.530063314493)) ;
#66194 = CARTESIAN_POINT('Ctrl Pts',(-17.9062584823097,19.5627332450072,123.295743025407)) ;
#66195 = CARTESIAN_POINT('Ctrl Pts',(-18.2068602643135,19.3827441646443,123.318958777135)) ;
#66196 = CARTESIAN_POINT('Ctrl Pts',(-17.9485751372052,19.5726199545382,123.039387974114)) ;
#66197 = CARTESIAN_POINT('Ctrl Pts',(-18.240713249619,19.3926308741753,123.113875561071)) ;
#66198 = CARTESIAN_POINT('Ctrl Pts',(-18.035260566707,19.5826129269668,122.791515506251)) ;
#66199 = CARTESIAN_POINT('Ctrl Pts',(-18.3100612446795,19.4026238466039,122.915577638234)) ;
#66200 = CARTESIAN_POINT('Ctrl Pts',(-18.1631676695922,19.5925591215034,122.563579250553)) ;
#66201 = CARTESIAN_POINT('Ctrl Pts',(-18.4123864487675,19.4125700411405,122.733228908367)) ;
#66202 = CARTESIAN_POINT('Ctrl Pts',(-18.3282687771438,19.6025044963549,122.360947075224)) ;
#66203 = CARTESIAN_POINT('Ctrl Pts',(-18.5444667060827,19.422515415992,122.571123262125)) ;
#66204 = CARTESIAN_POINT('Ctrl Pts',(-18.5284509193618,19.6125594157148,122.188521930226)) ;
#66205 = CARTESIAN_POINT('Ctrl Pts',(-18.7046123935706,19.4325703353519,122.433182741857)) ;
#66206 = CARTESIAN_POINT('Ctrl Pts',(-18.750061582201,19.6223809351583,122.056150769602)) ;
#66207 = CARTESIAN_POINT('Ctrl Pts',(-18.8818995815922,19.4423918547954,122.327286088883)) ;
#66208 = CARTESIAN_POINT('Ctrl Pts',(-18.9970975872,19.6324467039252,121.961712899097)) ;
#66209 = CARTESIAN_POINT('Ctrl Pts',(-19.0795284847268,19.4524576235623,122.251735185212)) ;
#66210 = CARTESIAN_POINT('Ctrl Pts',(-19.2526602063055,19.6423486255803,121.912488218236)) ;
#66211 = CARTESIAN_POINT('Ctrl Pts',(-19.2839777620693,19.4623595452174,122.212355084193)) ;
#66212 = CARTESIAN_POINT('Ctrl Pts',(-19.5165208729935,19.6523916844013,121.908094752818)) ;
#66213 = CARTESIAN_POINT('Ctrl Pts',(-19.4950664570593,19.4724026040384,122.208839744185)) ;
#66214 = CARTESIAN_POINT('Ctrl Pts',(-19.7735886685139,19.662297678444,121.949158051718)) ;
#66215 = CARTESIAN_POINT('Ctrl Pts',(-19.7007200621191,19.4823085980811,122.241689749395)) ;
#66216 = CARTESIAN_POINT('Ctrl Pts',(-20.0206528799151,19.6722354515258,122.033777229908)) ;
#66217 = CARTESIAN_POINT('Ctrl Pts',(-19.8983711686072,19.4922463711629,122.30938424429)) ;
#66218 = CARTESIAN_POINT('Ctrl Pts',(-20.2514911587077,19.6822758152581,122.161558568198)) ;
#66219 = CARTESIAN_POINT('Ctrl Pts',(-20.0830422357934,19.5022867348952,122.411608819251)) ;
#66220 = CARTESIAN_POINT('Ctrl Pts',(-20.4536472526372,19.6921631589816,122.324810150255)) ;
#66221 = CARTESIAN_POINT('Ctrl Pts',(-20.2447669012231,19.5121740786187,122.542209021845)) ;
#66222 = CARTESIAN_POINT('Ctrl Pts',(-20.6265036649569,19.7021553895503,122.522452222942)) ;
#66223 = CARTESIAN_POINT('Ctrl Pts',(-20.3830525266567,19.5221663091874,122.700322030319)) ;
#66224 = CARTESIAN_POINT('Ctrl Pts',(-20.7617787531808,19.7121039173339,122.746188030278)) ;
#66225 = CARTESIAN_POINT('Ctrl Pts',(-20.4912730421252,19.532114836971,122.879309900702)) ;
#66226 = CARTESIAN_POINT('Ctrl Pts',(-20.856369565108,19.7220407010572,122.989558473137)) ;
#66227 = CARTESIAN_POINT('Ctrl Pts',(-20.5669463183877,19.5420516206943,123.074005464355)) ;
#66228 = CARTESIAN_POINT('Ctrl Pts',(-20.9078402627332,19.7320237018542,123.246836830907)) ;
#66229 = CARTESIAN_POINT('Ctrl Pts',(-20.6081237656465,19.5520346214913,123.279827763413)) ;
#66230 = CARTESIAN_POINT('Ctrl Pts',(-20.9134056044351,19.7420675886949,123.510689929292)) ;
#66231 = CARTESIAN_POINT('Ctrl Pts',(-20.6125768755946,19.562078508332,123.490910375999)) ;
#66232 = CARTESIAN_POINT('Ctrl Pts',(-20.8745366916682,19.7518956122695,123.766060949729)) ;
#66233 = CARTESIAN_POINT('Ctrl Pts',(-20.5814828864297,19.5719065319066,123.69520619847)) ;
#66234 = CARTESIAN_POINT('Ctrl Pts',(-20.7899593277774,19.7619728604831,124.016948250578)) ;
#66235 = CARTESIAN_POINT('Ctrl Pts',(-20.513821837292,19.5819837801202,123.895916689788)) ;
#66236 = CARTESIAN_POINT('Ctrl Pts',(-20.6660660069028,19.7718224157884,124.244285226899)) ;
#66237 = CARTESIAN_POINT('Ctrl Pts',(-20.4147085725534,19.5918333354255,124.077785895298)) ;
#66238 = CARTESIAN_POINT('Ctrl Pts',(-20.5009161893016,19.7819051239861,124.451396677659)) ;
#66239 = CARTESIAN_POINT('Ctrl Pts',(-20.2825893295826,19.6019160436232,124.243476002834)) ;
#66240 = CARTESIAN_POINT('Ctrl Pts',(-20.307696830118,19.7917177169126,124.622248846254)) ;
#66241 = CARTESIAN_POINT('Ctrl Pts',(-20.1280154809097,19.6117286365497,124.380157782015)) ;
#66242 = CARTESIAN_POINT('Ctrl Pts',(-20.0823669714035,19.8017849091705,124.760755273323)) ;
#66243 = CARTESIAN_POINT('Ctrl Pts',(-19.9477519880674,19.6217958288076,124.490964105197)) ;
#66244 = CARTESIAN_POINT('Ctrl Pts',(-19.8403718039497,19.8116837386331,124.856362880226)) ;
#66245 = CARTESIAN_POINT('Ctrl Pts',(-19.7541569135087,19.6316946582702,124.567451052078)) ;
#66246 = CARTESIAN_POINT('Ctrl Pts',(-19.581599257843,19.8217377298233,124.90940442077)) ;
#66247 = CARTESIAN_POINT('Ctrl Pts',(-19.5471389315843,19.6417486494604,124.609885512907)) ;
#66248 = CARTESIAN_POINT('Ctrl Pts',(-19.3222318233483,19.8316094546065,124.916810422138)) ;
#66249 = CARTESIAN_POINT('Ctrl Pts',(-19.339645850064,19.6516203742436,124.615811552476)) ;
#66250 = CARTESIAN_POINT('Ctrl Pts',(-19.0604406240858,19.8416798967367,124.878387276188)) ;
#66251 = CARTESIAN_POINT('Ctrl Pts',(-19.1302124239704,19.6616908163738,124.585074260848)) ;
#66252 = CARTESIAN_POINT('Ctrl Pts',(-18.8151144576531,19.851512975167,124.797145106877)) ;
#66253 = CARTESIAN_POINT('Ctrl Pts',(-18.9339520539141,19.6715238948041,124.52008208332)) ;
#66254 = CARTESIAN_POINT('Ctrl Pts',(-18.5827297027157,19.8615434486684,124.672758530689)) ;
#66255 = CARTESIAN_POINT('Ctrl Pts',(-18.7480434996773,19.6815543683055,124.420574076199)) ;
#66256 = CARTESIAN_POINT('Ctrl Pts',(-18.3759053294246,19.8715750479671,124.509274829673)) ;
#66257 = CARTESIAN_POINT('Ctrl Pts',(-18.5825831437698,19.6915859676042,124.289788093677)) ;
#66258 = CARTESIAN_POINT('Ctrl Pts',(-18.2037555511074,19.8814047490052,124.31670801897)) ;
#66259 = CARTESIAN_POINT('Ctrl Pts',(-18.4448629441187,19.7014156686424,124.135736342827)) ;
#66260 = CARTESIAN_POINT('Ctrl Pts',(-18.0647658072952,19.8913941870617,124.094000670336)) ;
#66261 = CARTESIAN_POINT('Ctrl Pts',(-18.3336698936195,19.7114051066988,123.957571414372)) ;
#66262 = CARTESIAN_POINT('Ctrl Pts',(-17.9666480383149,19.9014380902778,123.848976044792)) ;
#66263 = CARTESIAN_POINT('Ctrl Pts',(-18.2551743019667,19.7214490099149,123.761552138209)) ;
#66264 = CARTESIAN_POINT('Ctrl Pts',(-17.9132339251412,19.9112596110913,123.596462120658)) ;
#66265 = CARTESIAN_POINT('Ctrl Pts',(-18.212441709217,19.7312705307284,123.559542293389)) ;
#66266 = CARTESIAN_POINT('Ctrl Pts',(-17.9036546813369,19.9212953353384,123.332913768264)) ;
#66267 = CARTESIAN_POINT('Ctrl Pts',(-18.2047766510836,19.7413062549755,123.348703585753)) ;
#66268 = CARTESIAN_POINT('Ctrl Pts',(-17.9406113337571,19.9313174892709,123.072128085455)) ;
#66269 = CARTESIAN_POINT('Ctrl Pts',(-18.2343404591825,19.751328408908,123.140074813286)) ;
#66270 = CARTESIAN_POINT('Ctrl Pts',(-18.0205697573143,19.9411797210282,122.825622198603)) ;
#66271 = CARTESIAN_POINT('Ctrl Pts',(-18.2983054242486,19.7611906406653,122.942870341222)) ;
#66272 = CARTESIAN_POINT('Ctrl Pts',(-18.1426708877126,19.9511387914861,122.594127929803)) ;
#66273 = CARTESIAN_POINT('Ctrl Pts',(-18.3959846585781,19.7711497111232,122.757674351822)) ;
#66274 = CARTESIAN_POINT('Ctrl Pts',(-18.3046496822276,19.9611739638623,122.386036391047)) ;
#66275 = CARTESIAN_POINT('Ctrl Pts',(-18.525566417151,19.7811848834994,122.591200043048)) ;
#66276 = CARTESIAN_POINT('Ctrl Pts',(-18.4970491714254,19.9710543490205,122.211642765681)) ;
#66277 = CARTESIAN_POINT('Ctrl Pts',(-18.6794843828221,19.7910652686577,122.451684269361)) ;
#66278 = CARTESIAN_POINT('Ctrl Pts',(-18.720627652709,19.9811110636145,122.070778322321)) ;
#66279 = CARTESIAN_POINT('Ctrl Pts',(-18.8583463631659,19.8011219832516,122.338991147531)) ;
#66280 = CARTESIAN_POINT('Ctrl Pts',(-18.960996130641,19.9909903321865,121.972639347132)) ;
#66281 = CARTESIAN_POINT('Ctrl Pts',(-19.0506399085198,19.8110012518237,122.260478581221)) ;
#66282 = CARTESIAN_POINT('Ctrl Pts',(-19.2174586026876,20.0009812896722,121.916419162101)) ;
#66283 = CARTESIAN_POINT('Ctrl Pts',(-19.2558093721547,19.8209922093093,122.21550063503)) ;
#66284 = CARTESIAN_POINT('Ctrl Pts',(-19.4811173295918,20.0110219483074,121.906111456795)) ;
#66285 = CARTESIAN_POINT('Ctrl Pts',(-19.4667363549532,19.8310328679445,122.207252696804)) ;
#66286 = CARTESIAN_POINT('Ctrl Pts',(-19.7372046092749,20.0208549280154,121.940573290861)) ;
#66287 = CARTESIAN_POINT('Ctrl Pts',(-19.6716056688886,19.8408658476525,122.234820236614)) ;
#66288 = CARTESIAN_POINT('Ctrl Pts',(-19.9876565139675,20.0308480612651,122.019537420732)) ;
#66289 = CARTESIAN_POINT('Ctrl Pts',(-19.871967684399,19.8508589809022,122.297989646812)) ;
#66290 = CARTESIAN_POINT('Ctrl Pts',(-20.2212609501245,20.0408801136485,122.141754795336)) ;
#66291 = CARTESIAN_POINT('Ctrl Pts',(-20.0588521268464,19.8608910332856,122.395761901234)) ;
#66292 = CARTESIAN_POINT('Ctrl Pts',(-20.4267990069944,20.0507453425998,122.29973257063)) ;
#66293 = CARTESIAN_POINT('Ctrl Pts',(-20.2232832806594,19.8707562622369,122.522142243935)) ;
#66294 = CARTESIAN_POINT('Ctrl Pts',(-20.6040593213488,20.060707283843,122.492388017739)) ;
#66295 = CARTESIAN_POINT('Ctrl Pts',(-20.3650928817087,19.8807182034801,122.676265086268)) ;
#66296 = CARTESIAN_POINT('Ctrl Pts',(-20.7458379853386,20.0707419988798,122.71471883926)) ;
#66297 = CARTESIAN_POINT('Ctrl Pts',(-20.4785174821517,19.8907529185169,122.854128710767)) ;
#66298 = CARTESIAN_POINT('Ctrl Pts',(-20.8457638320152,20.0806277692238,122.954554133205)) ;
#66299 = CARTESIAN_POINT('Ctrl Pts',(-20.5584598470704,19.9006386888609,123.045995755698)) ;
#66300 = CARTESIAN_POINT('Ctrl Pts',(-20.9035264743855,20.0906903666126,123.212570178599)) ;
#66301 = CARTESIAN_POINT('Ctrl Pts',(-20.6046719531102,19.9107012862497,123.252408261689)) ;
#66302 = CARTESIAN_POINT('Ctrl Pts',(-20.9154749497781,20.1005407784478,123.471173528851)) ;
#66303 = CARTESIAN_POINT('Ctrl Pts',(-20.6142327359483,19.9205516980849,123.459290308044)) ;
#66304 = CARTESIAN_POINT('Ctrl Pts',(-20.8824212203225,20.1105679477337,123.732588303383)) ;
#66305 = CARTESIAN_POINT('Ctrl Pts',(-20.5877918409855,19.9305788673709,123.668422402238)) ;
#66306 = CARTESIAN_POINT('Ctrl Pts',(-20.8038130480593,20.1205954284479,123.984115444725)) ;
#66307 = CARTESIAN_POINT('Ctrl Pts',(-20.5249072402036,19.940606348085,123.86964471591)) ;
#66308 = CARTESIAN_POINT('Ctrl Pts',(-20.6854052876472,20.1304384810272,124.214077225316)) ;
#66309 = CARTESIAN_POINT('Ctrl Pts',(-20.4301831161523,19.9504494006643,124.053614646428)) ;
#66310 = CARTESIAN_POINT('Ctrl Pts',(-20.5269966913248,20.1404323844658,124.423553915828)) ;
#66311 = CARTESIAN_POINT('Ctrl Pts',(-20.3034580001774,19.9604433041029,124.221197233981)) ;
#66312 = CARTESIAN_POINT('Ctrl Pts',(-20.3336481312429,20.1504595072422,124.602587618317)) ;
#66313 = CARTESIAN_POINT('Ctrl Pts',(-20.1487805945953,19.9704704268793,124.364425725248)) ;
#66314 = CARTESIAN_POINT('Ctrl Pts',(-20.1153421998912,20.1603502121343,124.743661057522)) ;
#66315 = CARTESIAN_POINT('Ctrl Pts',(-19.9741372834993,19.9803611317714,124.477286090543)) ;
#66316 = CARTESIAN_POINT('Ctrl Pts',(-19.873563628878,20.1703422389846,124.846066786522)) ;
#66317 = CARTESIAN_POINT('Ctrl Pts',(-19.7807153501285,19.9903531586217,124.559212634884)) ;
#66318 = CARTESIAN_POINT('Ctrl Pts',(-19.618831660715,20.1802882204731,124.904591118333)) ;
#66319 = CARTESIAN_POINT('Ctrl Pts',(-19.5769304388928,20.0002991401102,124.60603416333)) ;
#66320 = CARTESIAN_POINT('Ctrl Pts',(-19.3577875500338,20.190235393095,124.918525903528)) ;
#66321 = CARTESIAN_POINT('Ctrl Pts',(-19.3680954272052,20.0102463127322,124.61718417711)) ;
#66322 = CARTESIAN_POINT('Ctrl Pts',(-19.0957195762214,20.2002833344212,124.886313111744)) ;
#66323 = CARTESIAN_POINT('Ctrl Pts',(-19.1584407747982,20.0202942540583,124.591416103589)) ;
#66324 = CARTESIAN_POINT('Ctrl Pts',(-18.8481841830687,20.210130968229,124.810831448379)) ;
#66325 = CARTESIAN_POINT('Ctrl Pts',(-18.9604121247911,20.0301418878661,124.531032963021)) ;
#66326 = CARTESIAN_POINT('Ctrl Pts',(-18.6144848557031,20.220092682914,124.692895466025)) ;
#66327 = CARTESIAN_POINT('Ctrl Pts',(-18.7734517428529,20.0401036025511,124.436686220242)) ;
#66328 = CARTESIAN_POINT('Ctrl Pts',(-18.4035822760522,20.2301213157925,124.534835645106)) ;
#66329 = CARTESIAN_POINT('Ctrl Pts',(-18.6047283766993,20.0501322354297,124.310240160807)) ;
#66330 = CARTESIAN_POINT('Ctrl Pts',(-18.2254094105789,20.2400316413277,124.34490354003)) ;
#66331 = CARTESIAN_POINT('Ctrl Pts',(-18.4621885771613,20.0600425609648,124.158296117052)) ;
#66332 = CARTESIAN_POINT('Ctrl Pts',(-18.0819921054121,20.2499664717994,124.126739575367)) ;
#66333 = CARTESIAN_POINT('Ctrl Pts',(-18.347452906344,20.0699773914365,123.983766287248)) ;
#66334 = CARTESIAN_POINT('Ctrl Pts',(-17.9777343205273,20.2600078041814,123.884334153632)) ;
#66335 = CARTESIAN_POINT('Ctrl Pts',(-18.2640446533727,20.0800187238185,123.789842799783)) ;
#66336 = CARTESIAN_POINT('Ctrl Pts',(-17.9179543452334,20.2699006776202,123.631328380915)) ;
#66337 = CARTESIAN_POINT('Ctrl Pts',(-18.2162184451713,20.0899115972573,123.587439083643)) ;
#66338 = CARTESIAN_POINT('Ctrl Pts',(-17.9022315156781,20.2798698434381,123.369810686241)) ;
#66339 = CARTESIAN_POINT('Ctrl Pts',(-18.2036382029103,20.0998807630752,123.37822414266)) ;
#66340 = CARTESIAN_POINT('Ctrl Pts',(-17.9327660607719,20.2898985771546,123.108061591331)) ;
#66341 = CARTESIAN_POINT('Ctrl Pts',(-18.2280625915591,20.1099094967917,123.168828314924)) ;
#66342 = CARTESIAN_POINT('Ctrl Pts',(-18.0314212956118,20.3030910959258,122.775637805959)) ;
#66343 = CARTESIAN_POINT('Ctrl Pts',(-18.3069888734284,20.1231020155629,122.902870362102)) ;
#66344 = CARTESIAN_POINT('Ctrl Pts',(-18.2167817772954,20.3164509639684,122.472918789065)) ;
#66345 = CARTESIAN_POINT('Ctrl Pts',(-18.455294322149,20.1364618836056,122.660681237817)) ;
#66346 = CARTESIAN_POINT('Ctrl Pts',(-18.4689719567282,20.3296763011173,122.233665328807)) ;
#66347 = CARTESIAN_POINT('Ctrl Pts',(-18.657015967816,20.1496872207544,122.469309185131)) ;
#66348 = CARTESIAN_POINT('Ctrl Pts',(-18.6872891439649,20.3396575269579,122.0882957323)) ;
#66349 = CARTESIAN_POINT('Ctrl Pts',(-18.8316741569079,20.1596684465951,122.353005054526)) ;
#66350 = CARTESIAN_POINT('Ctrl Pts',(-18.9290457583576,20.3496930939408,121.982939786469)) ;
#66351 = CARTESIAN_POINT('Ctrl Pts',(-19.0250769393784,20.1697040135779,122.268720036234)) ;
#66352 = CARTESIAN_POINT('Ctrl Pts',(-19.1809279027677,20.3595561719029,121.921703115503)) ;
#66353 = CARTESIAN_POINT('Ctrl Pts',(-19.2265826009953,20.17956709154,122.219728036107)) ;
#66354 = CARTESIAN_POINT('Ctrl Pts',(-19.4449915418395,20.369626470704,121.904729894139)) ;
#66355 = CARTESIAN_POINT('Ctrl Pts',(-19.4378331366122,20.1896373903411,122.206147360686)) ;
#66356 = CARTESIAN_POINT('Ctrl Pts',(-19.7020745055463,20.3794687692718,121.933224576347)) ;
#66357 = CARTESIAN_POINT('Ctrl Pts',(-19.6434999173445,20.1994796889089,122.228940862857)) ;
#66358 = CARTESIAN_POINT('Ctrl Pts',(-19.9535442296739,20.3894294674416,122.005865433082)) ;
#66359 = CARTESIAN_POINT('Ctrl Pts',(-19.844676334268,20.2094403870787,122.287051467107)) ;
#66360 = CARTESIAN_POINT('Ctrl Pts',(-20.1901714045228,20.3994675016211,122.122429978516)) ;
#66361 = CARTESIAN_POINT('Ctrl Pts',(-20.0339789452335,20.2194784212582,122.380301057783)) ;
#66362 = CARTESIAN_POINT('Ctrl Pts',(-20.3998046709007,20.4093412384676,122.275390622965)) ;
#66363 = CARTESIAN_POINT('Ctrl Pts',(-20.2016870029984,20.2293521581047,122.502667926402)) ;
#66364 = CARTESIAN_POINT('Ctrl Pts',(-20.5832300951106,20.4194130223928,122.466148916955)) ;
#66365 = CARTESIAN_POINT('Ctrl Pts',(-20.3484287872655,20.2394239420299,122.655272907251)) ;
#66366 = CARTESIAN_POINT('Ctrl Pts',(-20.7274022481108,20.429245143594,122.680593266604)) ;
#66367 = CARTESIAN_POINT('Ctrl Pts',(-20.4637684999712,20.2492560632311,122.826827448914)) ;
#66368 = CARTESIAN_POINT('Ctrl Pts',(-20.83492227229,20.4392781676194,122.921317142792)) ;
#66369 = CARTESIAN_POINT('Ctrl Pts',(-20.549786401994,20.2592890872566,123.019405611083)) ;
#66370 = CARTESIAN_POINT('Ctrl Pts',(-20.8982551027824,20.4492940478161,123.176808341218)) ;
#66371 = CARTESIAN_POINT('Ctrl Pts',(-20.6004547451558,20.2693049674532,123.223797857408)) ;
#66372 = CARTESIAN_POINT('Ctrl Pts',(-20.9165069215087,20.4591775669103,123.435894221683)) ;
#66373 = CARTESIAN_POINT('Ctrl Pts',(-20.615058364723,20.2791884865474,123.43106704069)) ;
#66374 = CARTESIAN_POINT('Ctrl Pts',(-20.8895420040221,20.469167979274,123.697025786576)) ;
#66375 = CARTESIAN_POINT('Ctrl Pts',(-20.5934884233315,20.2891788989111,123.639971206989)) ;
#66376 = CARTESIAN_POINT('Ctrl Pts',(-20.7941934591565,20.4824311424774,124.032297261989)) ;
#66377 = CARTESIAN_POINT('Ctrl Pts',(-20.5172126368922,20.3024420621145,123.908195802062)) ;
#66378 = CARTESIAN_POINT('Ctrl Pts',(-20.61364497499,20.4957087127286,124.335469275498)) ;
#66379 = CARTESIAN_POINT('Ctrl Pts',(-20.3727498733357,20.3157196323657,124.15076100523)) ;
#66380 = CARTESIAN_POINT('Ctrl Pts',(-20.3624251620307,20.5090390152352,124.579659196355)) ;
#66381 = CARTESIAN_POINT('Ctrl Pts',(-20.1718067039307,20.3290499348723,124.346077405116)) ;
#66382 = CARTESIAN_POINT('Ctrl Pts',(-20.1474678125217,20.5189376970516,124.726143222167)) ;
#66383 = CARTESIAN_POINT('Ctrl Pts',(-19.9998354017675,20.3389486166887,124.463273991554)) ;
#66384 = CARTESIAN_POINT('Ctrl Pts',(-19.9082988338251,20.5289272120991,124.834343756603)) ;
#66385 = CARTESIAN_POINT('Ctrl Pts',(-19.8085028501753,20.3489381317363,124.549834241605)) ;
#66386 = CARTESIAN_POINT('Ctrl Pts',(-19.6550087594271,20.5388752638742,124.899096739163)) ;
#66387 = CARTESIAN_POINT('Ctrl Pts',(-19.6058699022926,20.3588861835113,124.601638844772)) ;
#66388 = CARTESIAN_POINT('Ctrl Pts',(-19.3945515389815,20.5488166671527,124.919199688652)) ;
#66389 = CARTESIAN_POINT('Ctrl Pts',(-19.3975068666403,20.3688275867898,124.617723886778)) ;
#66390 = CARTESIAN_POINT('Ctrl Pts',(-19.0469745337114,20.5621033319336,124.885630332357)) ;
#66391 = CARTESIAN_POINT('Ctrl Pts',(-19.1194311731786,20.3821142515707,124.590866211464)) ;
#66392 = CARTESIAN_POINT('Ctrl Pts',(-18.6334863377988,20.5787137535884,124.731039345078)) ;
#66393 = CARTESIAN_POINT('Ctrl Pts',(-18.788654663985,20.3987246732255,124.467201404259)) ;
#66394 = CARTESIAN_POINT('Ctrl Pts',(-18.2305106418667,20.5986250158392,124.387975748647)) ;
#66395 = CARTESIAN_POINT('Ctrl Pts',(-18.4662665446094,20.4186359354763,124.192751186382)) ;
#66396 = CARTESIAN_POINT('Ctrl Pts',(-17.9681790722083,20.6185691450041,123.927324296484)) ;
#66397 = CARTESIAN_POINT('Ctrl Pts',(-18.2563995729899,20.4385800646412,123.824231859657)) ;
#66398 = CARTESIAN_POINT('Ctrl Pts',(-17.8789643904274,20.6384923076093,123.405418987404)) ;
#66399 = CARTESIAN_POINT('Ctrl Pts',(-18.1850241788991,20.4585032272464,123.406707562409)) ;
#66400 = CARTESIAN_POINT('Ctrl Pts',(-17.9722011638597,20.6583824300158,122.884976490813)) ;
#66401 = CARTESIAN_POINT('Ctrl Pts',(-18.2596109762183,20.4783933496529,122.990352318436)) ;
#66402 = CARTESIAN_POINT('Ctrl Pts',(-18.2392413285999,20.6783873836159,122.425297035635)) ;
#66403 = CARTESIAN_POINT('Ctrl Pts',(-18.4732405399828,20.498398303253,122.622607344408)) ;
#66404 = CARTESIAN_POINT('Ctrl Pts',(-18.6435876221089,20.6982256406315,122.086739272797)) ;
#66405 = CARTESIAN_POINT('Ctrl Pts',(-18.7967168578306,20.5182365602686,122.35175829032)) ;
#66406 = CARTESIAN_POINT('Ctrl Pts',(-19.1427514572152,20.718219941418,121.904613931299)) ;
#66407 = CARTESIAN_POINT('Ctrl Pts',(-19.1960471830647,20.5382308610552,122.206055793577)) ;
#66408 = CARTESIAN_POINT('Ctrl Pts',(-19.6712810445263,20.7381051834625,121.904239572849)) ;
#66409 = CARTESIAN_POINT('Ctrl Pts',(-19.6188718571092,20.5581161030996,122.205753939832)) ;
#66410 = CARTESIAN_POINT('Ctrl Pts',(-20.168447470455,20.7579801299384,122.082748587511)) ;
#66411 = CARTESIAN_POINT('Ctrl Pts',(-20.0166067329943,20.5779910495756,122.348559983418)) ;
#66412 = CARTESIAN_POINT('Ctrl Pts',(-20.5778609764888,20.7780131998795,122.423240113376)) ;
#66413 = CARTESIAN_POINT('Ctrl Pts',(-20.3441382911306,20.5980241195166,122.620951670167)) ;
#66414 = CARTESIAN_POINT('Ctrl Pts',(-20.8439482662448,20.7979017067799,122.879935963145)) ;
#66415 = CARTESIAN_POINT('Ctrl Pts',(-20.5570102575303,20.617912626417,122.986308438082)) ;
#66416 = CARTESIAN_POINT('Ctrl Pts',(-20.9398845189848,20.8177565665612,123.398932664504)) ;
#66417 = CARTESIAN_POINT('Ctrl Pts',(-20.6337603893495,20.6377674861983,123.401507281384)) ;
#66418 = CARTESIAN_POINT('Ctrl Pts',(-20.8512719992327,20.8378074003489,123.924305207163)) ;
#66419 = CARTESIAN_POINT('Ctrl Pts',(-20.5628715067338,20.657818319986,123.821804891128)) ;
#66420 = CARTESIAN_POINT('Ctrl Pts',(-20.5928049104702,20.8575733422382,124.381835472892)) ;
#66421 = CARTESIAN_POINT('Ctrl Pts',(-20.3560969395519,20.6775842618753,124.187831867116)) ;
#66422 = CARTESIAN_POINT('Ctrl Pts',(-20.1896580437569,20.8775860736975,124.728578782344)) ;
#66423 = CARTESIAN_POINT('Ctrl Pts',(-20.0335794046623,20.6975969933346,124.465226382195)) ;
#66424 = CARTESIAN_POINT('Ctrl Pts',(-19.6948360554275,20.8974789086411,124.915243821142)) ;
#66425 = CARTESIAN_POINT('Ctrl Pts',(-19.6377205723978,20.7174898282782,124.61455887421)) ;
#66426 = CARTESIAN_POINT('Ctrl Pts',(-19.1659236264529,20.9173859319806,124.922728039924)) ;
#66427 = CARTESIAN_POINT('Ctrl Pts',(-19.2145894369091,20.7373968516177,124.620545637084)) ;
#66428 = CARTESIAN_POINT('Ctrl Pts',(-18.6655619227043,20.9373011968813,124.749682544139)) ;
#66429 = CARTESIAN_POINT('Ctrl Pts',(-18.8142995780805,20.7573121165184,124.482107923995)) ;
#66430 = CARTESIAN_POINT('Ctrl Pts',(-18.2524397020174,20.957332889041,124.413908184194)) ;
#66431 = CARTESIAN_POINT('Ctrl Pts',(-18.4838026915331,20.7773438086781,124.21348792732)) ;
#66432 = CARTESIAN_POINT('Ctrl Pts',(-17.9811972981208,20.977175935614,123.961546540794)) ;
#66433 = CARTESIAN_POINT('Ctrl Pts',(-18.2668088563855,20.7971868552511,123.8515965203)) ;
#66434 = CARTESIAN_POINT('Ctrl Pts',(-17.8790621516814,20.9970924835138,123.442223784006)) ;
#66435 = CARTESIAN_POINT('Ctrl Pts',(-18.1851023793624,20.8171034031509,123.436137129649)) ;
#66436 = CARTESIAN_POINT('Ctrl Pts',(-17.9604499278885,21.0170247265051,122.918699625149)) ;
#66437 = CARTESIAN_POINT('Ctrl Pts',(-18.2502146020831,20.8370356461422,123.017317483767)) ;
#66438 = CARTESIAN_POINT('Ctrl Pts',(-18.2149540834011,21.0369285613144,122.454965536719)) ;
#66439 = CARTESIAN_POINT('Ctrl Pts',(-18.4538202863488,20.8569394809515,122.646330486718)) ;
#66440 = CARTESIAN_POINT('Ctrl Pts',(-18.6119399166127,21.0568289615019,122.105461255144)) ;
#66441 = CARTESIAN_POINT('Ctrl Pts',(-18.7714112568372,20.876839881139,122.366728442058)) ;
#66442 = CARTESIAN_POINT('Ctrl Pts',(-19.1055245267092,21.0767786378812,121.91171422936)) ;
#66443 = CARTESIAN_POINT('Ctrl Pts',(-19.1662802778635,20.8967895575183,122.211733244875)) ;
#66444 = CARTESIAN_POINT('Ctrl Pts',(-19.6351319246211,21.0967111621016,121.898157078062)) ;
#66445 = CARTESIAN_POINT('Ctrl Pts',(-19.5899667460685,20.9167220817387,122.200890351572)) ;
#66446 = CARTESIAN_POINT('Ctrl Pts',(-20.1374331359232,21.1166311710878,122.065615887878)) ;
#66447 = CARTESIAN_POINT('Ctrl Pts',(-19.9918072525265,20.9366420907249,122.334860475937)) ;
#66448 = CARTESIAN_POINT('Ctrl Pts',(-20.5530840765956,21.136588077264,122.395047352195)) ;
#66449 = CARTESIAN_POINT('Ctrl Pts',(-20.3243262285862,20.9565989969011,122.598408332127)) ;
#66450 = CARTESIAN_POINT('Ctrl Pts',(-20.8308668599276,21.1564739167655,122.844813593085)) ;
#66451 = CARTESIAN_POINT('Ctrl Pts',(-20.5465500430235,20.9764848364026,122.958223574526)) ;
#66452 = CARTESIAN_POINT('Ctrl Pts',(-20.9388483133597,21.1764450889013,123.364394953387)) ;
#66453 = CARTESIAN_POINT('Ctrl Pts',(-20.6329313716892,20.9964560085384,123.373889855656)) ;
#66454 = CARTESIAN_POINT('Ctrl Pts',(-20.8643333248033,21.1962592858857,123.885809151916)) ;
#66455 = CARTESIAN_POINT('Ctrl Pts',(-20.5733172829464,21.0162702055228,123.791020397466)) ;
#66456 = CARTESIAN_POINT('Ctrl Pts',(-20.6149914724651,21.2162404718539,124.35458992427)) ;
#66457 = CARTESIAN_POINT('Ctrl Pts',(-20.3738339226301,21.0362513914911,124.166047707023)) ;
#66458 = CARTESIAN_POINT('Ctrl Pts',(-20.2875771231592,21.2328159772432,124.649450004713)) ;
#66459 = CARTESIAN_POINT('Ctrl Pts',(-20.1119198605758,21.0528268968803,124.401919518092)) ;
#66460 = CARTESIAN_POINT('Ctrl Pts',(-19.976190695121,21.2461254251068,124.808734121278)) ;
#66461 = CARTESIAN_POINT('Ctrl Pts',(-19.8627850672793,21.0661363447439,124.529357922434)) ;
#66462 = CARTESIAN_POINT('Ctrl Pts',(-19.6403422561752,21.2594931228834,124.911767929916)) ;
#66463 = CARTESIAN_POINT('Ctrl Pts',(-19.5941577979202,21.0795040425205,124.611771756262)) ;
#66464 = CARTESIAN_POINT('Ctrl Pts',(-19.2023540010426,21.2759836945493,124.927912591737)) ;
#66465 = CARTESIAN_POINT('Ctrl Pts',(-19.2437108124987,21.0959946141864,124.62469560568)) ;
#66466 = CARTESIAN_POINT('Ctrl Pts',(-18.6980130161789,21.2959039668821,124.76705541604)) ;
#66467 = CARTESIAN_POINT('Ctrl Pts',(-18.8402511097492,21.1159148865192,124.495996295646)) ;
#66468 = CARTESIAN_POINT('Ctrl Pts',(-18.3484015779916,21.3125210026031,124.497134075246)) ;
#66469 = CARTESIAN_POINT('Ctrl Pts',(-18.5605800541927,21.1325319222402,124.280076149471)) ;
#66470 = CARTESIAN_POINT('Ctrl Pts',(-18.1364098503999,21.3258118528842,124.219524949621)) ;
#66471 = CARTESIAN_POINT('Ctrl Pts',(-18.3909714359101,21.1458227725213,124.057970053224)) ;
#66472 = CARTESIAN_POINT('Ctrl Pts',(-18.0158871388316,21.3357808980387,123.986950081581)) ;
#66473 = CARTESIAN_POINT('Ctrl Pts',(-18.2945586408566,21.1557918176758,123.871912706625)) ;
#66474 = CARTESIAN_POINT('Ctrl Pts',(-17.9375848219816,21.3456842886722,123.7387264045)) ;
#66475 = CARTESIAN_POINT('Ctrl Pts',(-18.2319181148261,21.1656952083094,123.673331434388)) ;
#66476 = CARTESIAN_POINT('Ctrl Pts',(-17.9031917373362,21.355742074785,123.476694986446)) ;
#66477 = CARTESIAN_POINT('Ctrl Pts',(-18.2044053250832,21.1757529944221,123.463708741263)) ;
#66478 = CARTESIAN_POINT('Ctrl Pts',(-17.9143537185253,21.3655941114347,123.218009520766)) ;
#66479 = CARTESIAN_POINT('Ctrl Pts',(-18.2133399425486,21.1856050310718,123.256751469431)) ;
#66480 = CARTESIAN_POINT('Ctrl Pts',(-17.9896212280947,21.3789592355779,122.874956968011)) ;
#66481 = CARTESIAN_POINT('Ctrl Pts',(-18.2735425071571,21.198970155215,122.982353715324)) ;
#66482 = CARTESIAN_POINT('Ctrl Pts',(-18.1513956643206,21.3921852985409,122.562838107837)) ;
#66483 = CARTESIAN_POINT('Ctrl Pts',(-18.4029674268594,21.2121962181781,122.732632497982)) ;
#66484 = CARTESIAN_POINT('Ctrl Pts',(-18.3866109363659,21.4054889468232,122.304222180962)) ;
#66485 = CARTESIAN_POINT('Ctrl Pts',(-18.5911529954546,21.2254998664603,122.525730915353)) ;
#66486 = CARTESIAN_POINT('Ctrl Pts',(-18.5942688365872,21.4154804779862,122.143483381919)) ;
#66487 = CARTESIAN_POINT('Ctrl Pts',(-18.7572784100833,21.2354913976233,122.397143875669)) ;
#66488 = CARTESIAN_POINT('Ctrl Pts',(-18.8279161165822,21.4255199257855,122.020995347853)) ;
#66489 = CARTESIAN_POINT('Ctrl Pts',(-18.9441978151252,21.2455308454226,122.299154881713)) ;
#66490 = CARTESIAN_POINT('Ctrl Pts',(-19.0743002770801,21.4353637012994,121.942115783865)) ;
#66491 = CARTESIAN_POINT('Ctrl Pts',(-19.1413056995706,21.2553746209365,122.236053522357)) ;
#66492 = CARTESIAN_POINT('Ctrl Pts',(-19.3342026170286,21.445349342687,121.90619908811)) ;
#66493 = CARTESIAN_POINT('Ctrl Pts',(-19.3492278602432,21.2653602623241,122.207322374569)) ;
#66494 = CARTESIAN_POINT('Ctrl Pts',(-19.5951977714836,21.4552861270488,121.915768063468)) ;
#66495 = CARTESIAN_POINT('Ctrl Pts',(-19.5580238317526,21.2752970466859,122.214979818382)) ;
#66496 = CARTESIAN_POINT('Ctrl Pts',(-19.8533761099886,21.4653359615162,121.971250859302)) ;
#66497 = CARTESIAN_POINT('Ctrl Pts',(-19.7645659845222,21.2853468811533,122.259368252402)) ;
#66498 = CARTESIAN_POINT('Ctrl Pts',(-20.0932613278945,21.4751864110193,122.068581121297)) ;
#66499 = CARTESIAN_POINT('Ctrl Pts',(-19.9564732213435,21.2951973306564,122.337234519556)) ;
#66500 = CARTESIAN_POINT('Ctrl Pts',(-20.3156279272745,21.4851584250014,122.207174295959)) ;
#66501 = CARTESIAN_POINT('Ctrl Pts',(-20.1343652320431,21.3051693446385,122.448110919028)) ;
#66502 = CARTESIAN_POINT('Ctrl Pts',(-20.5110376061981,21.4951535828485,122.382755229701)) ;
#66503 = CARTESIAN_POINT('Ctrl Pts',(-20.290691427895,21.3151645024856,122.588577292965)) ;
#66504 = CARTESIAN_POINT('Ctrl Pts',(-20.6733301023097,21.5051875092122,122.590546133602)) ;
#66505 = CARTESIAN_POINT('Ctrl Pts',(-20.4205236271332,21.3251984288494,122.754811381595)) ;
#66506 = CARTESIAN_POINT('Ctrl Pts',(-20.7952585397872,21.5150432176446,122.819075138393)) ;
#66507 = CARTESIAN_POINT('Ctrl Pts',(-20.5180643101211,21.3350541372817,122.937635474695)) ;
#66508 = CARTESIAN_POINT('Ctrl Pts',(-20.8771547988309,21.5250413669833,123.068682710145)) ;
#66509 = CARTESIAN_POINT('Ctrl Pts',(-20.5835791727783,21.3450522866204,123.13732215833)) ;
#66510 = CARTESIAN_POINT('Ctrl Pts',(-20.9143410126104,21.5349407701568,123.326195883179)) ;
#66511 = CARTESIAN_POINT('Ctrl Pts',(-20.6133259222408,21.354951689794,123.343332810001)) ;
#66512 = CARTESIAN_POINT('Ctrl Pts',(-20.9061846999684,21.5449919670453,123.590176807784)) ;
#66513 = CARTESIAN_POINT('Ctrl Pts',(-20.6067986577069,21.3650028866824,123.554517489311)) ;
#66514 = CARTESIAN_POINT('Ctrl Pts',(-20.853249823519,21.5548742908582,123.844441837906)) ;
#66515 = CARTESIAN_POINT('Ctrl Pts',(-20.5644486425954,21.3748852104953,123.7579288163)) ;
#66516 = CARTESIAN_POINT('Ctrl Pts',(-20.7564330306425,21.5648691865148,124.088593766656)) ;
#66517 = CARTESIAN_POINT('Ctrl Pts',(-20.4869932187418,21.3848801061519,123.953249478274)) ;
#66518 = CARTESIAN_POINT('Ctrl Pts',(-20.6179931768872,21.5748902858973,124.312627761359)) ;
#66519 = CARTESIAN_POINT('Ctrl Pts',(-20.3762394774589,21.3949012055344,124.132475496053)) ;
#66520 = CARTESIAN_POINT('Ctrl Pts',(-20.4449112034606,21.5847975537594,124.507113190861)) ;
#66521 = CARTESIAN_POINT('Ctrl Pts',(-20.2377724303908,21.4048084733965,124.288062198318)) ;
#66522 = CARTESIAN_POINT('Ctrl Pts',(-20.2403849662515,21.5947358975846,124.669500522451)) ;
#66523 = CARTESIAN_POINT('Ctrl Pts',(-20.0741502752422,21.4147468172218,124.417970248963)) ;
#66524 = CARTESIAN_POINT('Ctrl Pts',(-20.0093045735368,21.6047393168851,124.79489097273)) ;
#66525 = CARTESIAN_POINT('Ctrl Pts',(-19.8892850037941,21.4247502365222,124.518280706296)) ;
#66526 = CARTESIAN_POINT('Ctrl Pts',(-19.7590892507398,21.6147738675922,124.878084487071)) ;
#66527 = CARTESIAN_POINT('Ctrl Pts',(-19.6891120481609,21.4347847872293,124.584833462809)) ;
#66528 = CARTESIAN_POINT('Ctrl Pts',(-19.5031930456652,21.6246188171978,124.916282417656)) ;
#66529 = CARTESIAN_POINT('Ctrl Pts',(-19.4843952188806,21.4446297368349,124.615389634999)) ;
#66530 = CARTESIAN_POINT('Ctrl Pts',(-19.2408957415365,21.6346046593107,124.909864611199)) ;
#66531 = CARTESIAN_POINT('Ctrl Pts',(-19.274557555605,21.4546155789478,124.610253310096)) ;
#66532 = CARTESIAN_POINT('Ctrl Pts',(-18.9848863453834,21.6445394666798,124.858431106566)) ;
#66533 = CARTESIAN_POINT('Ctrl Pts',(-19.0697507008442,21.4645503863169,124.569104541095)) ;
#66534 = CARTESIAN_POINT('Ctrl Pts',(-18.738859338082,21.6545970083931,124.761963952245)) ;
#66535 = CARTESIAN_POINT('Ctrl Pts',(-18.8729297698642,21.4746079280302,124.491928838993)) ;
#66536 = CARTESIAN_POINT('Ctrl Pts',(-18.5183469904694,21.6644186059052,124.627779140097)) ;
#66537 = CARTESIAN_POINT('Ctrl Pts',(-18.696521489678,21.4844295255424,124.384579574157)) ;
#66538 = CARTESIAN_POINT('Ctrl Pts',(-18.3195680415686,21.6744748653857,124.453674665829)) ;
#66539 = CARTESIAN_POINT('Ctrl Pts',(-18.5374995695825,21.4944857850228,124.245294444731)) ;
#66540 = CARTESIAN_POINT('Ctrl Pts',(-18.1562878546674,21.6844148016861,124.249767117428)) ;
#66541 = CARTESIAN_POINT('Ctrl Pts',(-18.4068771805631,21.5044257213232,124.082167340354)) ;
#66542 = CARTESIAN_POINT('Ctrl Pts',(-18.0306281552504,21.6943219224305,124.021754765608)) ;
#66543 = CARTESIAN_POINT('Ctrl Pts',(-18.3063513226383,21.5143328420676,123.899756895081)) ;
#66544 = CARTESIAN_POINT('Ctrl Pts',(-17.9454073048491,21.7043648283558,123.771982422679)) ;
#66545 = CARTESIAN_POINT('Ctrl Pts',(-18.2381764644056,21.5243757479929,123.699938324042)) ;
#66546 = CARTESIAN_POINT('Ctrl Pts',(-17.9053416812303,21.714272609455,123.51470692144)) ;
#66547 = CARTESIAN_POINT('Ctrl Pts',(-18.2061259509787,21.5342835290921,123.494118036696)) ;
#66548 = CARTESIAN_POINT('Ctrl Pts',(-17.9101476585179,21.7242829784574,123.251680239082)) ;
#66549 = CARTESIAN_POINT('Ctrl Pts',(-18.2099726089032,21.5442938980945,123.283696771005)) ;
#66550 = CARTESIAN_POINT('Ctrl Pts',(-17.9611784249865,21.7343138170262,122.993069233019)) ;
#66551 = CARTESIAN_POINT('Ctrl Pts',(-18.25079914997,21.5543247366633,123.076808307396)) ;
#66552 = CARTESIAN_POINT('Ctrl Pts',(-18.0542181019441,21.7441666566659,122.751434398998)) ;
#66553 = CARTESIAN_POINT('Ctrl Pts',(-18.3252324147839,21.564177576303,122.883501741555)) ;
#66554 = CARTESIAN_POINT('Ctrl Pts',(-18.1892070598107,21.7541546578309,122.526357242308)) ;
#66555 = CARTESIAN_POINT('Ctrl Pts',(-18.433225062823,21.574165577468,122.703441075812)) ;
#66556 = CARTESIAN_POINT('Ctrl Pts',(-18.3602212353183,21.76408347681,122.32928753721)) ;
#66557 = CARTESIAN_POINT('Ctrl Pts',(-18.5700375178516,21.5840943964472,122.545786794347)) ;
#66558 = CARTESIAN_POINT('Ctrl Pts',(-18.5637837492857,21.7740711795323,122.163582862095)) ;
#66559 = CARTESIAN_POINT('Ctrl Pts',(-18.7328885150387,21.5940820991695,122.413224497597)) ;
#66560 = CARTESIAN_POINT('Ctrl Pts',(-18.7943281092038,21.784107179335,122.035521757821)) ;
#66561 = CARTESIAN_POINT('Ctrl Pts',(-18.9173249461088,21.6041180989721,122.310777167978)) ;
#66562 = CARTESIAN_POINT('Ctrl Pts',(-19.038997751584,21.7939620491364,121.950573239043)) ;
#66563 = CARTESIAN_POINT('Ctrl Pts',(-19.1130605360951,21.6139729687736,122.242820240775)) ;
#66564 = CARTESIAN_POINT('Ctrl Pts',(-19.2983295791008,21.80396147956,121.908451210414)) ;
#66565 = CARTESIAN_POINT('Ctrl Pts',(-19.3205261622003,21.6239723991971,122.209124297681)) ;
#66566 = CARTESIAN_POINT('Ctrl Pts',(-19.5583862373949,21.8138565970253,121.911683181411)) ;
#66567 = CARTESIAN_POINT('Ctrl Pts',(-19.5285708804354,21.6338675166624,122.21171149709)) ;
#66568 = CARTESIAN_POINT('Ctrl Pts',(-19.8181211650492,21.8239170905422,121.96083913654)) ;
#66569 = CARTESIAN_POINT('Ctrl Pts',(-19.7363587075279,21.6439280101794,122.251037906807)) ;
#66570 = CARTESIAN_POINT('Ctrl Pts',(-20.0602885784198,21.8337665707434,122.052271697296)) ;
#66571 = CARTESIAN_POINT('Ctrl Pts',(-19.930091288856,21.6537774903805,122.324185167146)) ;
#66572 = CARTESIAN_POINT('Ctrl Pts',(-20.2872285089844,21.8437930210072,122.186139952124)) ;
#66573 = CARTESIAN_POINT('Ctrl Pts',(-20.1116425053652,21.6638039406443,122.431281064082)) ;
#66574 = CARTESIAN_POINT('Ctrl Pts',(-20.4871079315352,21.8538243114853,122.35801891506)) ;
#66575 = CARTESIAN_POINT('Ctrl Pts',(-20.2715450314613,21.6738352311224,122.568785502684)) ;
#66576 = CARTESIAN_POINT('Ctrl Pts',(-20.6513791646752,21.8636656991371,122.557772038563)) ;
#66577 = CARTESIAN_POINT('Ctrl Pts',(-20.4029602709634,21.6836766187742,122.728588256116)) ;
#66578 = CARTESIAN_POINT('Ctrl Pts',(-20.7809938111829,21.8736691000283,122.786445434062)) ;
#66579 = CARTESIAN_POINT('Ctrl Pts',(-20.5066507156167,21.6936800196655,122.91152759353)) ;
#66580 = CARTESIAN_POINT('Ctrl Pts',(-20.8686887483206,21.8836534828195,123.033784325657)) ;
#66581 = CARTESIAN_POINT('Ctrl Pts',(-20.5768052604981,21.7036644024566,123.109399027828)) ;
#66582 = CARTESIAN_POINT('Ctrl Pts',(-20.9120839655183,21.8936925728329,123.293981074003)) ;
#66583 = CARTESIAN_POINT('Ctrl Pts',(-20.6115199849103,21.71370349247,123.317556776986)) ;
#66584 = CARTESIAN_POINT('Ctrl Pts',(-20.9100499298834,21.9035383817421,123.552730180815)) ;
#66585 = CARTESIAN_POINT('Ctrl Pts',(-20.609891351577,21.7235493013792,123.524555112863)) ;
#66586 = CARTESIAN_POINT('Ctrl Pts',(-20.8629939222876,21.9135228045611,123.810817924676)) ;
#66587 = CARTESIAN_POINT('Ctrl Pts',(-20.5722453017055,21.7335337241982,123.73102487777)) ;
#66588 = CARTESIAN_POINT('Ctrl Pts',(-20.7723283116897,21.9234624298023,124.05581995963)) ;
#66589 = CARTESIAN_POINT('Ctrl Pts',(-20.4997117680828,21.7434733494394,123.927025654345)) ;
#66590 = CARTESIAN_POINT('Ctrl Pts',(-20.6391479210158,21.9335021193209,124.283546922036)) ;
#66591 = CARTESIAN_POINT('Ctrl Pts',(-20.3931662819036,21.7535130389581,124.109206674248)) ;
#66592 = CARTESIAN_POINT('Ctrl Pts',(-20.4711013650952,21.9433903077395,124.481766445994)) ;
#66593 = CARTESIAN_POINT('Ctrl Pts',(-20.2587285516933,21.7634012273766,124.267780913417)) ;
#66594 = CARTESIAN_POINT('Ctrl Pts',(-20.2694747065142,21.9533798337416,124.649861363959)) ;
#66595 = CARTESIAN_POINT('Ctrl Pts',(-20.097426616492,21.7733907533787,124.402255850537)) ;
#66596 = CARTESIAN_POINT('Ctrl Pts',(-20.0423296292845,21.9633383350968,124.779814856002)) ;
#66597 = CARTESIAN_POINT('Ctrl Pts',(-19.915710259167,21.7833492547339,124.506217429302)) ;
#66598 = CARTESIAN_POINT('Ctrl Pts',(-19.7977240449736,21.9732379291004,124.868443422786)) ;
#66599 = CARTESIAN_POINT('Ctrl Pts',(-19.7200260940079,21.7932488487375,124.577119050715)) ;
#66600 = CARTESIAN_POINT('Ctrl Pts',(-19.5376330731142,21.9832858172217,124.913825837491)) ;
#66601 = CARTESIAN_POINT('Ctrl Pts',(-19.5119529591425,21.8032967368588,124.61342395089)) ;
#66602 = CARTESIAN_POINT('Ctrl Pts',(-19.2775503015537,21.9931812424672,124.913569399124)) ;
#66603 = CARTESIAN_POINT('Ctrl Pts',(-19.3038874739033,21.8131921621044,124.613217771097)) ;
#66604 = CARTESIAN_POINT('Ctrl Pts',(-19.017233305932,22.0032426331678,124.86744619023)) ;
#66605 = CARTESIAN_POINT('Ctrl Pts',(-19.0956337981961,21.8232535528049,124.576318149791)) ;
#66606 = CARTESIAN_POINT('Ctrl Pts',(-18.7741467328486,22.0130882168545,124.778797095436)) ;
#66607 = CARTESIAN_POINT('Ctrl Pts',(-18.9011658833268,21.8330991364916,124.505398287498)) ;
#66608 = CARTESIAN_POINT('Ctrl Pts',(-18.5470623486079,22.0230511901637,124.648524437436)) ;
#66609 = CARTESIAN_POINT('Ctrl Pts',(-18.7194990790042,21.8430621098008,124.401179638259)) ;
#66610 = CARTESIAN_POINT('Ctrl Pts',(-18.3449798305692,22.0330768569895,124.479454619294)) ;
#66611 = CARTESIAN_POINT('Ctrl Pts',(-18.5578335854537,21.8530877766266,124.265923060778)) ;
#66612 = CARTESIAN_POINT('Ctrl Pts',(-18.1771126653133,22.0429913348558,124.28020996493)) ;
#66613 = CARTESIAN_POINT('Ctrl Pts',(-18.4235409199083,21.8630022544929,124.106527278134)) ;
#66614 = CARTESIAN_POINT('Ctrl Pts',(-18.0449474119808,22.0529798495308,124.053398711337)) ;
#66615 = CARTESIAN_POINT('Ctrl Pts',(-18.317809439298,21.8729907691679,123.925078062203)) ;
#66616 = CARTESIAN_POINT('Ctrl Pts',(-17.954211848732,22.0630239604462,123.805561752125)) ;
#66617 = CARTESIAN_POINT('Ctrl Pts',(-18.2452217507632,21.8830348800833,123.726808050528)) ;
#66618 = CARTESIAN_POINT('Ctrl Pts',(-17.9082542485454,22.0728520980408,123.551371969022)) ;
#66619 = CARTESIAN_POINT('Ctrl Pts',(-18.2084565831269,21.8928630176779,123.523457276199)) ;
#66620 = CARTESIAN_POINT('Ctrl Pts',(-17.9069805912369,22.0829286660997,123.286627562761)) ;
#66621 = CARTESIAN_POINT('Ctrl Pts',(-18.2074383400266,21.9029395857368,123.311661381763)) ;
#66622 = CARTESIAN_POINT('Ctrl Pts',(-17.9505873022016,22.0927808280039,123.031363437666)) ;
#66623 = CARTESIAN_POINT('Ctrl Pts',(-18.2423241725982,21.912791747641,123.107451229462)) ;
#66624 = CARTESIAN_POINT('Ctrl Pts',(-18.0395690380517,22.1028537899607,122.782109150564)) ;
#66625 = CARTESIAN_POINT('Ctrl Pts',(-18.3135102432881,21.9228647095978,122.908047671536)) ;
#66626 = CARTESIAN_POINT('Ctrl Pts',(-18.1675496052933,22.1126963519636,122.557311692099)) ;
#66627 = CARTESIAN_POINT('Ctrl Pts',(-18.4158946651662,21.9327072716007,122.728210991207)) ;
#66628 = CARTESIAN_POINT('Ctrl Pts',(-18.3342296705409,22.1226767884574,122.354827390352)) ;
#66629 = CARTESIAN_POINT('Ctrl Pts',(-18.5492388606532,21.9426877080945,122.566223989023)) ;
#66630 = CARTESIAN_POINT('Ctrl Pts',(-18.5346278830778,22.1326950937818,122.184094281001)) ;
#66631 = CARTESIAN_POINT('Ctrl Pts',(-18.7095577721264,21.9527060134189,122.429637890191)) ;
#66632 = CARTESIAN_POINT('Ctrl Pts',(-18.7583362356547,22.1425790577013,122.052058163512)) ;
#66633 = CARTESIAN_POINT('Ctrl Pts',(-18.8885238944235,21.9625899773384,122.32400976912)) ;
#66634 = CARTESIAN_POINT('Ctrl Pts',(-19.0060171333251,22.1526449344398,121.959277593487)) ;
#66635 = CARTESIAN_POINT('Ctrl Pts',(-19.0866690470502,21.9726558540769,122.249785576266)) ;
#66636 = CARTESIAN_POINT('Ctrl Pts',(-19.2602098520566,22.1624840353007,121.911823353389)) ;
#66637 = CARTESIAN_POINT('Ctrl Pts',(-19.2900221324471,21.9824949549378,122.211822750592)) ;
#66638 = CARTESIAN_POINT('Ctrl Pts',(-19.5238350449174,22.1725171181664,121.908510218283)) ;
#66639 = CARTESIAN_POINT('Ctrl Pts',(-19.5009223790608,21.9925280378036,122.209172428358)) ;
#66640 = CARTESIAN_POINT('Ctrl Pts',(-19.7836614016497,22.1825388034419,121.951624796669)) ;
#66641 = CARTESIAN_POINT('Ctrl Pts',(-19.7087834435619,22.002549723079,122.243664446075)) ;
#66642 = CARTESIAN_POINT('Ctrl Pts',(-20.0283161574298,22.1924054985404,122.037437936202)) ;
#66643 = CARTESIAN_POINT('Ctrl Pts',(-19.9045062201637,22.0124164181775,122.312314862293)) ;
#66644 = CARTESIAN_POINT('Ctrl Pts',(-20.2568547840646,22.2023653882749,122.165037255751)) ;
#66645 = CARTESIAN_POINT('Ctrl Pts',(-20.0873367614171,22.0223763079121,122.414394197747)) ;
#66646 = CARTESIAN_POINT('Ctrl Pts',(-20.4610185638516,22.2124003761004,122.331922477437)) ;
#66647 = CARTESIAN_POINT('Ctrl Pts',(-20.2506677635409,22.0324112957375,122.547902586744)) ;
#66648 = CARTESIAN_POINT('Ctrl Pts',(-20.6309241388541,22.2222870801747,122.528528183517)) ;
#66649 = CARTESIAN_POINT('Ctrl Pts',(-20.3865915994159,22.0422979998118,122.705186531169)) ;
#66650 = CARTESIAN_POINT('Ctrl Pts',(-20.766416856272,22.2323522244076,122.755640405164)) ;
#66651 = CARTESIAN_POINT('Ctrl Pts',(-20.4949858643928,22.0523631440447,122.88687662059)) ;
#66652 = CARTESIAN_POINT('Ctrl Pts',(-20.8585847061565,22.2421915151362,122.997265190441)) ;
#66653 = CARTESIAN_POINT('Ctrl Pts',(-20.5687197080449,22.0622024347733,123.080175347708)) ;
#66654 = CARTESIAN_POINT('Ctrl Pts',(-20.9088481489483,22.2522540725746,123.256845872699)) ;
#66655 = CARTESIAN_POINT('Ctrl Pts',(-20.6089305940997,22.0722649922117,123.287840171023)) ;
#66656 = CARTESIAN_POINT('Ctrl Pts',(-20.9129252441028,22.2621511238267,123.516913308371)) ;
#66657 = CARTESIAN_POINT('Ctrl Pts',(-20.6121922611426,22.0821620434638,123.495893317472)) ;
#66658 = CARTESIAN_POINT('Ctrl Pts',(-20.8725051637196,22.272082330575,123.774739999813)) ;
#66659 = CARTESIAN_POINT('Ctrl Pts',(-20.5798565101102,22.0920932502121,123.702154136205)) ;
#66660 = CARTESIAN_POINT('Ctrl Pts',(-20.786712131682,22.2821245147938,124.024299304319)) ;
#66661 = CARTESIAN_POINT('Ctrl Pts',(-20.5112221742166,22.1021354344309,123.901801786887)) ;
#66662 = CARTESIAN_POINT('Ctrl Pts',(-20.6610284500015,22.2920111429047,124.25170115506)) ;
#66663 = CARTESIAN_POINT('Ctrl Pts',(-20.4106758246915,22.1120220625418,124.083722603376)) ;
#66664 = CARTESIAN_POINT('Ctrl Pts',(-20.4963649928319,22.3020044154371,124.45625910245)) ;
#66665 = CARTESIAN_POINT('Ctrl Pts',(-20.2789454023778,22.1220153350742,124.247369029717)) ;
#66666 = CARTESIAN_POINT('Ctrl Pts',(-20.2995680280399,22.3119494909786,124.628229064092)) ;
#66667 = CARTESIAN_POINT('Ctrl Pts',(-20.1215083814713,22.1319604106157,124.384944899341)) ;
#66668 = CARTESIAN_POINT('Ctrl Pts',(-20.0760548364874,22.3218990417068,124.763918115327)) ;
#66669 = CARTESIAN_POINT('Ctrl Pts',(-19.9426984210111,22.141909961344,124.493496265617)) ;
#66670 = CARTESIAN_POINT('Ctrl Pts',(-19.8301102215282,22.3319383765548,124.859349625922)) ;
#66671 = CARTESIAN_POINT('Ctrl Pts',(-19.7459427347351,22.1519492961919,124.569841851037)) ;
#66672 = CARTESIAN_POINT('Ctrl Pts',(-19.5752934234394,22.3418245154987,124.910085821145)) ;
#66673 = CARTESIAN_POINT('Ctrl Pts',(-19.5420902200881,22.1618354351359,124.610431044817)) ;
#66674 = CARTESIAN_POINT('Ctrl Pts',(-19.3126560173104,22.3518226284724,124.916205138615)) ;
#66675 = CARTESIAN_POINT('Ctrl Pts',(-19.3319804315117,22.1718335481096,124.615326989773)) ;
#66676 = CARTESIAN_POINT('Ctrl Pts',(-19.0548963059002,22.3617423908249,124.877085616116)) ;
#66677 = CARTESIAN_POINT('Ctrl Pts',(-19.1257731976824,22.181753310462,124.584031994196)) ;
#66678 = CARTESIAN_POINT('Ctrl Pts',(-18.8048804750818,22.3717817864375,124.792892259255)) ;
#66679 = CARTESIAN_POINT('Ctrl Pts',(-18.9257602220697,22.1917927060747,124.51667778619)) ;
#66680 = CARTESIAN_POINT('Ctrl Pts',(-18.5763093840162,22.3816909722258,124.668127742339)) ;
#66681 = CARTESIAN_POINT('Ctrl Pts',(-18.7429037235827,22.2017018918629,124.41686698238)) ;
#66682 = CARTESIAN_POINT('Ctrl Pts',(-18.3718830460784,22.3916261563833,124.505717216813)) ;
#66683 = CARTESIAN_POINT('Ctrl Pts',(-18.5793626191556,22.2116370760204,124.286939448208)) ;
#66684 = CARTESIAN_POINT('Ctrl Pts',(-18.1971172156532,22.4016672137692,124.308030847448)) ;
#66685 = CARTESIAN_POINT('Ctrl Pts',(-18.4395493697844,22.2216781334063,124.128790671233)) ;
#66686 = CARTESIAN_POINT('Ctrl Pts',(-18.0612726927552,22.4115543718025,124.086530580778)) ;
#66687 = CARTESIAN_POINT('Ctrl Pts',(-18.330873593402,22.2315652914396,123.951591529793)) ;
#66688 = CARTESIAN_POINT('Ctrl Pts',(-17.9645436848904,22.4215466514784,123.842428732897)) ;
#66689 = CARTESIAN_POINT('Ctrl Pts',(-18.2534897026088,22.2415575711155,123.756310497809)) ;
#66690 = CARTESIAN_POINT('Ctrl Pts',(-17.9119640315032,22.4314951685235,123.586318714181)) ;
#66691 = CARTESIAN_POINT('Ctrl Pts',(-18.211425301115,22.2515060881606,123.551423064664)) ;
#66692 = CARTESIAN_POINT('Ctrl Pts',(-17.9042933598069,22.4414319460939,123.325324977717)) ;
#66693 = CARTESIAN_POINT('Ctrl Pts',(-18.2052879085007,22.261442865731,123.342628610746)) ;
#66694 = CARTESIAN_POINT('Ctrl Pts',(-17.9419119920911,22.4514149822408,123.065658904093)) ;
#66695 = CARTESIAN_POINT('Ctrl Pts',(-18.235381847005,22.2714259018779,123.134895818999)) ;
#66696 = CARTESIAN_POINT('Ctrl Pts',(-18.0249844510094,22.4614587338345,122.815165001349)) ;
#66697 = CARTESIAN_POINT('Ctrl Pts',(-18.3018390701171,22.2814696534717,122.934500290776)) ;
#66698 = CARTESIAN_POINT('Ctrl Pts',(-18.1471041894676,22.4712872630471,122.587531223368)) ;
#66699 = CARTESIAN_POINT('Ctrl Pts',(-18.3995334548748,22.2912981826842,122.752393822393)) ;
#66700 = CARTESIAN_POINT('Ctrl Pts',(-18.310736925562,22.4813626239558,122.379445782567)) ;
#66701 = CARTESIAN_POINT('Ctrl Pts',(-18.5304390610458,22.3013735435929,122.585924577045)) ;
#66702 = CARTESIAN_POINT('Ctrl Pts',(-18.5037504475988,22.491219222843,122.2066258693)) ;
#66703 = CARTESIAN_POINT('Ctrl Pts',(-18.684848467763,22.3112301424801,122.447668526044)) ;
#66704 = CARTESIAN_POINT('Ctrl Pts',(-18.7282113464719,22.5012822168609,122.066906399844)) ;
#66705 = CARTESIAN_POINT('Ctrl Pts',(-18.8644168289928,22.321293136498,122.335891884029)) ;
#66706 = CARTESIAN_POINT('Ctrl Pts',(-18.9691081441337,22.5111601511503,121.970077874885)) ;
#66707 = CARTESIAN_POINT('Ctrl Pts',(-19.0571331080001,22.3311710707875,122.258428360996)) ;
#66708 = CARTESIAN_POINT('Ctrl Pts',(-19.2261379991879,22.5211607987084,121.915505689096)) ;
#66709 = CARTESIAN_POINT('Ctrl Pts',(-19.2627566457403,22.3411717183456,122.214769480072)) ;
#66710 = CARTESIAN_POINT('Ctrl Pts',(-19.4866516087189,22.5310786451465,121.906267040837)) ;
#66711 = CARTESIAN_POINT('Ctrl Pts',(-19.4711669227681,22.3510895647836,122.207377364757)) ;
#66712 = CARTESIAN_POINT('Ctrl Pts',(-19.7481817747748,22.5411297621521,121.942948938101)) ;
#66713 = CARTESIAN_POINT('Ctrl Pts',(-19.6803913883822,22.3611406817893,122.236721714525)) ;
#66714 = CARTESIAN_POINT('Ctrl Pts',(-19.9950390178656,22.5510004974627,122.022770439589)) ;
#66715 = CARTESIAN_POINT('Ctrl Pts',(-19.8778767883679,22.3710114170999,122.300577456873)) ;
#66716 = CARTESIAN_POINT('Ctrl Pts',(-20.2288742155722,22.5610712047057,122.146611832965)) ;
#66717 = CARTESIAN_POINT('Ctrl Pts',(-20.0649457944915,22.3810821243429,122.399649573841)) ;
#66718 = CARTESIAN_POINT('Ctrl Pts',(-20.432852059648,22.5709042121576,122.305284591667)) ;
#66719 = CARTESIAN_POINT('Ctrl Pts',(-20.2281280611383,22.3909151317947,122.526586124132)) ;
#66720 = CARTESIAN_POINT('Ctrl Pts',(-20.6101957114275,22.5809347044599,122.50028265826)) ;
#66721 = CARTESIAN_POINT('Ctrl Pts',(-20.3700041091279,22.400945624097,122.682583647088)) ;
#66722 = CARTESIAN_POINT('Ctrl Pts',(-20.7503657377508,22.5909662995333,122.723566173364)) ;
#66723 = CARTESIAN_POINT('Ctrl Pts',(-20.4821412655094,22.4109772191704,122.861209824262)) ;
#66724 = CARTESIAN_POINT('Ctrl Pts',(-20.848126630718,22.6007959986715,122.962648437251)) ;
#66725 = CARTESIAN_POINT('Ctrl Pts',(-20.5603509034017,22.4208069183087,123.052474161789)) ;
#66726 = CARTESIAN_POINT('Ctrl Pts',(-20.904551077241,22.6107854485531,123.219033095629)) ;
#66727 = CARTESIAN_POINT('Ctrl Pts',(-20.6054919617955,22.4307963681902,123.257581413107)) ;
#66728 = CARTESIAN_POINT('Ctrl Pts',(-20.9149919746047,22.6208293063688,123.482765312887)) ;
#66729 = CARTESIAN_POINT('Ctrl Pts',(-20.6138461187708,22.4408402260059,123.46856724786)) ;
#66730 = CARTESIAN_POINT('Ctrl Pts',(-20.8807975538298,22.630650996959,123.738595413769)) ;
#66731 = CARTESIAN_POINT('Ctrl Pts',(-20.5864922425363,22.4506619165961,123.673230544663)) ;
#66732 = CARTESIAN_POINT('Ctrl Pts',(-20.8016166335874,22.6406860874994,123.990134218036)) ;
#66733 = CARTESIAN_POINT('Ctrl Pts',(-20.5231490649285,22.4606970071365,123.874462168931)) ;
#66734 = CARTESIAN_POINT('Ctrl Pts',(-20.6794595798729,22.6507106064821,124.223553358068)) ;
#66735 = CARTESIAN_POINT('Ctrl Pts',(-20.4254247725794,22.4707215261192,124.061198201126)) ;
#66736 = CARTESIAN_POINT('Ctrl Pts',(-20.5216428899484,22.6605704518923,124.429030130044)) ;
#66737 = CARTESIAN_POINT('Ctrl Pts',(-20.2991731733227,22.4805813715294,124.22557998796)) ;
#66738 = CARTESIAN_POINT('Ctrl Pts',(-20.3290800370369,22.670530228208,124.606303874563)) ;
#66739 = CARTESIAN_POINT('Ctrl Pts',(-20.1451242645067,22.4905411478451,124.367400086112)) ;
#66740 = CARTESIAN_POINT('Ctrl Pts',(-20.1069583810948,22.6805584255226,124.748107125882)) ;
#66741 = CARTESIAN_POINT('Ctrl Pts',(-19.9674278116215,22.5005693451597,124.480844120942)) ;
#66742 = CARTESIAN_POINT('Ctrl Pts',(-19.8666123895492,22.6904659678129,124.848267265594)) ;
#66743 = CARTESIAN_POINT('Ctrl Pts',(-19.7751521487821,22.51047688745,124.5609736348)) ;
#66744 = CARTESIAN_POINT('Ctrl Pts',(-19.6093776535577,22.7004986183768,124.905971284957)) ;
#66745 = CARTESIAN_POINT('Ctrl Pts',(-19.569364702959,22.5205095380139,124.607138561972)) ;
#66746 = CARTESIAN_POINT('Ctrl Pts',(-19.349909838197,22.7103825748034,124.918032249207)) ;
#66747 = CARTESIAN_POINT('Ctrl Pts',(-19.3617911229907,22.5303934944406,124.616789062543)) ;
#66748 = CARTESIAN_POINT('Ctrl Pts',(-19.0894539708058,22.7203722761653,124.88515179817)) ;
#66749 = CARTESIAN_POINT('Ctrl Pts',(-19.1534263193822,22.5403831958024,124.590486565815)) ;
#66750 = CARTESIAN_POINT('Ctrl Pts',(-18.8375462307077,22.7304132714413,124.806612946757)) ;
#66751 = CARTESIAN_POINT('Ctrl Pts',(-18.9518995301889,22.5504241910784,124.527657156544)) ;
#66752 = CARTESIAN_POINT('Ctrl Pts',(-18.6077694357356,22.7402461607097,124.68841772116)) ;
#66753 = CARTESIAN_POINT('Ctrl Pts',(-18.7680779300007,22.5602570803468,124.4331029628)) ;
#66754 = CARTESIAN_POINT('Ctrl Pts',(-18.3981964690907,22.7502393190771,124.530174726569)) ;
#66755 = CARTESIAN_POINT('Ctrl Pts',(-18.6004184592641,22.5702502387142,124.306510187023)) ;
#66756 = CARTESIAN_POINT('Ctrl Pts',(-18.2189780474116,22.7602713614292,124.336812835409)) ;
#66757 = CARTESIAN_POINT('Ctrl Pts',(-18.457042329262,22.5802822810663,124.151821925346)) ;
#66758 = CARTESIAN_POINT('Ctrl Pts',(-18.078177052041,22.7701366053876,124.11914781899)) ;
#66759 = CARTESIAN_POINT('Ctrl Pts',(-18.3444002370286,22.5901475250248,123.97769144434)) ;
#66760 = CARTESIAN_POINT('Ctrl Pts',(-17.9756297430813,22.7800984966336,123.878272519234)) ;
#66761 = CARTESIAN_POINT('Ctrl Pts',(-18.262360610908,22.6001094162708,123.784992180742)) ;
#66762 = CARTESIAN_POINT('Ctrl Pts',(-17.9164527324428,22.7901333966521,123.621304920688)) ;
#66763 = CARTESIAN_POINT('Ctrl Pts',(-18.2150170837711,22.6101443162892,123.579418516256)) ;
#66764 = CARTESIAN_POINT('Ctrl Pts',(-17.9025653496462,22.8000184770667,123.361873137659)) ;
#66765 = CARTESIAN_POINT('Ctrl Pts',(-18.2039051888414,22.6200293967038,123.371873646667)) ;
#66766 = CARTESIAN_POINT('Ctrl Pts',(-17.9345250196897,22.8100836491915,123.099344214703)) ;
#66767 = CARTESIAN_POINT('Ctrl Pts',(-18.229470937305,22.6300945688287,123.161850152158)) ;
#66768 = CARTESIAN_POINT('Ctrl Pts',(-18.0097882001565,22.819930883915,122.851728714304)) ;
#66769 = CARTESIAN_POINT('Ctrl Pts',(-18.2896793803027,22.6399418035521,122.963757680924)) ;
#66770 = CARTESIAN_POINT('Ctrl Pts',(-18.1285132437623,22.8299616952328,122.616400101498)) ;
#66771 = CARTESIAN_POINT('Ctrl Pts',(-18.3846575488646,22.6499726148699,122.775493825297)) ;
#66772 = CARTESIAN_POINT('Ctrl Pts',(-18.2864226563192,22.8399713111463,122.40599165732)) ;
#66773 = CARTESIAN_POINT('Ctrl Pts',(-18.5109834183892,22.6599822307834,122.607165884196)) ;
#66774 = CARTESIAN_POINT('Ctrl Pts',(-18.4763564295643,22.84988209055,122.227822802769)) ;
#66775 = CARTESIAN_POINT('Ctrl Pts',(-18.6629287774965,22.6698930101871,122.464629519222)) ;
#66776 = CARTESIAN_POINT('Ctrl Pts',(-18.6944202111758,22.859811356339,122.084505529354)) ;
#66777 = CARTESIAN_POINT('Ctrl Pts',(-18.8373784211579,22.6798222759761,122.349974053439)) ;
#66778 = CARTESIAN_POINT('Ctrl Pts',(-18.9368601501301,22.8698540496516,121.980263237278)) ;
#66779 = CARTESIAN_POINT('Ctrl Pts',(-19.0313295614933,22.6898649692887,122.266578267691)) ;
#66780 = CARTESIAN_POINT('Ctrl Pts',(-19.1897096706424,22.8797405823464,121.920470478153)) ;
#66781 = CARTESIAN_POINT('Ctrl Pts',(-19.2336083570812,22.6997515019835,122.218742067114)) ;
#66782 = CARTESIAN_POINT('Ctrl Pts',(-19.4518420605083,22.8897337274496,121.904884777647)) ;
#66783 = CARTESIAN_POINT('Ctrl Pts',(-19.4433140578841,22.7097446470868,122.206271347572)) ;
#66784 = CARTESIAN_POINT('Ctrl Pts',(-19.7114632832621,22.8996794081237,121.935008316747)) ;
#66785 = CARTESIAN_POINT('Ctrl Pts',(-19.6510111009045,22.7196903277608,122.230368013377)) ;
#66786 = CARTESIAN_POINT('Ctrl Pts',(-19.9621146837926,22.9096266657504,122.009255961602)) ;
#66787 = CARTESIAN_POINT('Ctrl Pts',(-19.8515326922247,22.7296375853876,122.289763976907)) ;
#66788 = CARTESIAN_POINT('Ctrl Pts',(-20.1982818352397,22.9196745678719,122.127332902665)) ;
#66789 = CARTESIAN_POINT('Ctrl Pts',(-20.0404673939253,22.739685487509,122.38422358596)) ;
#66790 = CARTESIAN_POINT('Ctrl Pts',(-20.4062715090379,22.9295222734936,122.281319880695)) ;
#66791 = CARTESIAN_POINT('Ctrl Pts',(-20.2068601821527,22.7495331931307,122.507411217)) ;
#66792 = CARTESIAN_POINT('Ctrl Pts',(-20.5870134936696,22.9394837401277,122.470672801482)) ;
#66793 = CARTESIAN_POINT('Ctrl Pts',(-20.3514553209462,22.7594946597648,122.658891935936)) ;
#66794 = CARTESIAN_POINT('Ctrl Pts',(-20.7328386955894,22.9495132933959,122.690234279952)) ;
#66795 = CARTESIAN_POINT('Ctrl Pts',(-20.4681173105457,22.769524213033,122.834539862625)) ;
#66796 = CARTESIAN_POINT('Ctrl Pts',(-20.8371700436695,22.9594201854233,122.928761227148)) ;
#66797 = CARTESIAN_POINT('Ctrl Pts',(-20.5515843614637,22.7794311050604,123.025360373342)) ;
#66798 = CARTESIAN_POINT('Ctrl Pts',(-20.8992391770811,22.9693678295363,123.182677656175)) ;
#66799 = CARTESIAN_POINT('Ctrl Pts',(-20.6012418268376,22.7893787491735,123.228492885336)) ;
#66800 = CARTESIAN_POINT('Ctrl Pts',(-20.9165341377211,22.9793678725652,123.444932969306)) ;
#66801 = CARTESIAN_POINT('Ctrl Pts',(-20.6150800337761,22.7993787922023,123.438296931167)) ;
#66802 = CARTESIAN_POINT('Ctrl Pts',(-20.8874593437994,22.9894066385592,123.707113721901)) ;
#66803 = CARTESIAN_POINT('Ctrl Pts',(-20.5918224275554,22.8094175581963,123.648041733911)) ;
#66804 = CARTESIAN_POINT('Ctrl Pts',(-20.8153966815368,22.9992317005814,123.955064177239)) ;
#66805 = CARTESIAN_POINT('Ctrl Pts',(-20.5341744977842,22.8192426202186,123.846402585896)) ;
#66806 = CARTESIAN_POINT('Ctrl Pts',(-20.6991206973961,23.0092862479078,124.192308936938)) ;
#66807 = CARTESIAN_POINT('Ctrl Pts',(-20.4411557498176,22.8292971675449,124.036199358367)) ;
#66808 = CARTESIAN_POINT('Ctrl Pts',(-20.5447615013441,23.019229491357,124.403151003466)) ;
#66809 = CARTESIAN_POINT('Ctrl Pts',(-20.3176702602204,22.8392404109942,124.204874274932)) ;
#66810 = CARTESIAN_POINT('Ctrl Pts',(-20.357481348229,23.0291316629649,124.583821375332)) ;
#66811 = CARTESIAN_POINT('Ctrl Pts',(-20.1678477266094,22.849142582602,124.349412166951)) ;
#66812 = CARTESIAN_POINT('Ctrl Pts',(-20.1383129462667,23.0391844985751,124.731298547748)) ;
#66813 = CARTESIAN_POINT('Ctrl Pts',(-19.9925143364415,22.8591954182122,124.4673957384)) ;
#66814 = CARTESIAN_POINT('Ctrl Pts',(-19.9012076725115,23.0490575562606,124.836667408501)) ;
#66815 = CARTESIAN_POINT('Ctrl Pts',(-19.8028309876301,22.8690684758978,124.551692871464)) ;
#66816 = CARTESIAN_POINT('Ctrl Pts',(-19.6464624451115,23.0590528177863,124.90066823185)) ;
#66817 = CARTESIAN_POINT('Ctrl Pts',(-19.5990355883761,22.8790637374234,124.602895734181)) ;
#66818 = CARTESIAN_POINT('Ctrl Pts',(-19.3836439744441,23.0690781872068,124.919051527796)) ;
#66819 = CARTESIAN_POINT('Ctrl Pts',(-19.3887803013881,22.8890891068439,124.617604464544)) ;
#66820 = CARTESIAN_POINT('Ctrl Pts',(-19.1251242692714,23.0789680197334,124.892233416081)) ;
#66821 = CARTESIAN_POINT('Ctrl Pts',(-19.1819670497776,22.8989789393705,124.59615274981)) ;
#66822 = CARTESIAN_POINT('Ctrl Pts',(-18.7890035337137,23.0922659905428,124.796782825436)) ;
#66823 = CARTESIAN_POINT('Ctrl Pts',(-18.9130558291102,22.9122769101799,124.519792421691)) ;
#66824 = CARTESIAN_POINT('Ctrl Pts',(-18.4874072190834,23.105464385652,124.617549791502)) ;
#66825 = CARTESIAN_POINT('Ctrl Pts',(-18.6717586476981,22.9254753052891,124.376385659626)) ;
#66826 = CARTESIAN_POINT('Ctrl Pts',(-18.2417519026231,23.1188598279314,124.365440342986)) ;
#66827 = CARTESIAN_POINT('Ctrl Pts',(-18.4752682092803,22.9388707475686,124.1747301264)) ;
#66828 = CARTESIAN_POINT('Ctrl Pts',(-18.0954516814504,23.1287356661704,124.151032241541)) ;
#66829 = CARTESIAN_POINT('Ctrl Pts',(-18.3582189589316,22.9487465858075,124.003198627306)) ;
#66830 = CARTESIAN_POINT('Ctrl Pts',(-17.9865146772214,23.1387970687681,123.910158781384)) ;
#66831 = CARTESIAN_POINT('Ctrl Pts',(-18.2710692167074,22.9588079884053,123.810502898505)) ;
#66832 = CARTESIAN_POINT('Ctrl Pts',(-17.922240462111,23.1486621257033,123.658970587668)) ;
#66833 = CARTESIAN_POINT('Ctrl Pts',(-18.2196477108387,22.9686730453404,123.60955078964)) ;
#66834 = CARTESIAN_POINT('Ctrl Pts',(-17.9018022904604,23.1586742216521,123.396691351192)) ;
#66835 = CARTESIAN_POINT('Ctrl Pts',(-18.2032931318325,22.9786851412892,123.399733036954)) ;
#66836 = CARTESIAN_POINT('Ctrl Pts',(-17.9355630207714,23.1719515307975,123.049376976604)) ;
#66837 = CARTESIAN_POINT('Ctrl Pts',(-18.230309065925,22.9919624504346,123.121854826151)) ;
#66838 = CARTESIAN_POINT('Ctrl Pts',(-18.0899419028751,23.1885505563048,122.636110521846)) ;
#66839 = CARTESIAN_POINT('Ctrl Pts',(-18.3537865821073,23.0085614759419,122.791280237995)) ;
#66840 = CARTESIAN_POINT('Ctrl Pts',(-18.3760258329839,23.2051496043378,122.300311520429)) ;
#66841 = CARTESIAN_POINT('Ctrl Pts',(-18.5826974346445,23.025160523975,122.522589580736)) ;
#66842 = CARTESIAN_POINT('Ctrl Pts',(-18.6623130734036,23.2183930163688,122.102367993719)) ;
#66843 = CARTESIAN_POINT('Ctrl Pts',(-18.8116871062911,23.0384039360059,122.364269513183)) ;
#66844 = CARTESIAN_POINT('Ctrl Pts',(-18.9019676656497,23.2284304440572,121.992209381467)) ;
#66845 = CARTESIAN_POINT('Ctrl Pts',(-19.0034183798067,23.0484413636943,122.27613348672)) ;
#66846 = CARTESIAN_POINT('Ctrl Pts',(-19.1537511180854,23.2383347460128,121.926257438649)) ;
#66847 = CARTESIAN_POINT('Ctrl Pts',(-19.2048396762017,23.0583456656499,122.223371601155)) ;
#66848 = CARTESIAN_POINT('Ctrl Pts',(-19.5011668383559,23.251601585988,121.896906683047)) ;
#66849 = CARTESIAN_POINT('Ctrl Pts',(-19.4827890606653,23.0716125056251,122.199889201105)) ;
#66850 = CARTESIAN_POINT('Ctrl Pts',(-19.9361152832958,23.2682277840779,121.974875772965)) ;
#66851 = CARTESIAN_POINT('Ctrl Pts',(-19.8307319806188,23.088238703715,122.262263124349)) ;
#66852 = CARTESIAN_POINT('Ctrl Pts',(-20.394142712814,23.2881468994613,122.240416456631)) ;
#66853 = CARTESIAN_POINT('Ctrl Pts',(-20.1971528580598,23.1081578190985,122.474678337376)) ;
#66854 = CARTESIAN_POINT('Ctrl Pts',(-20.6777956763041,23.3047533225956,122.578559316856)) ;
#66855 = CARTESIAN_POINT('Ctrl Pts',(-20.4241051196912,23.1247642422327,122.745236815236)) ;
#66856 = CARTESIAN_POINT('Ctrl Pts',(-20.8254141685684,23.3180495430913,122.895260367424)) ;
#66857 = CARTESIAN_POINT('Ctrl Pts',(-20.5421769247472,23.1380604627284,122.998554989249)) ;
#66858 = CARTESIAN_POINT('Ctrl Pts',(-20.9163840285696,23.3313183754327,123.231954203337)) ;
#66859 = CARTESIAN_POINT('Ctrl Pts',(-20.614959974584,23.1513292950698,123.26792816828)) ;
#66860 = CARTESIAN_POINT('Ctrl Pts',(-20.9167633041339,23.3480096234658,123.675476169135)) ;
#66861 = CARTESIAN_POINT('Ctrl Pts',(-20.6152647077734,23.1680205431029,123.622731052057)) ;
#66862 = CARTESIAN_POINT('Ctrl Pts',(-20.7380527826187,23.3678193551386,124.170798980292)) ;
#66863 = CARTESIAN_POINT('Ctrl Pts',(-20.4722993945024,23.1878302747757,124.018996228655)) ;
#66864 = CARTESIAN_POINT('Ctrl Pts',(-20.3990487800684,23.3877969624672,124.579436972735)) ;
#66865 = CARTESIAN_POINT('Ctrl Pts',(-20.2010981192601,23.2078078821043,124.345907297091)) ;
#66866 = CARTESIAN_POINT('Ctrl Pts',(-19.9416700356385,23.407723271525,124.846309372867)) ;
#66867 = CARTESIAN_POINT('Ctrl Pts',(-19.8351962131263,23.2277341911621,124.559408404364)) ;
#66868 = CARTESIAN_POINT('Ctrl Pts',(-19.423672280542,23.4275401316897,124.942420637845)) ;
#66869 = CARTESIAN_POINT('Ctrl Pts',(-19.4207968852883,23.2475510513268,124.636299832249)) ;
#66870 = CARTESIAN_POINT('Ctrl Pts',(-18.897005210854,23.4476399472837,124.853997620555)) ;
#66871 = CARTESIAN_POINT('Ctrl Pts',(-18.9994637104009,23.2676508669208,124.565563970077)) ;
#66872 = CARTESIAN_POINT('Ctrl Pts',(-18.4395858732156,23.4673969111663,124.595670036021)) ;
#66873 = CARTESIAN_POINT('Ctrl Pts',(-18.6335252687433,23.2874078308034,124.358902707329)) ;
#66874 = CARTESIAN_POINT('Ctrl Pts',(-18.0924014778527,23.4874338372357,124.192088863914)) ;
#66875 = CARTESIAN_POINT('Ctrl Pts',(-18.3557767077419,23.3074447568728,124.036039090244)) ;
#66876 = CARTESIAN_POINT('Ctrl Pts',(-17.9060208621862,23.5073034196172,123.697826439083)) ;
#66877 = CARTESIAN_POINT('Ctrl Pts',(-18.206670079505,23.3273143392544,123.64062860021)) ;
#66878 = CARTESIAN_POINT('Ctrl Pts',(-17.8981510516399,23.5272079913704,123.168957382108)) ;
#66879 = CARTESIAN_POINT('Ctrl Pts',(-18.2003731028714,23.3472189110075,123.217532238313)) ;
#66880 = CARTESIAN_POINT('Ctrl Pts',(-18.0717585757874,23.5471605935689,122.667777463739)) ;
#66881 = CARTESIAN_POINT('Ctrl Pts',(-18.3392584148753,23.367171513206,122.816587536918)) ;
#66882 = CARTESIAN_POINT('Ctrl Pts',(-18.4052588840874,23.5670700845392,122.257079257931)) ;
#66883 = CARTESIAN_POINT('Ctrl Pts',(-18.6060587086755,23.3870810041763,122.488027567399)) ;
#66884 = CARTESIAN_POINT('Ctrl Pts',(-18.8570010753677,23.5869214532386,121.984239388305)) ;
#66885 = CARTESIAN_POINT('Ctrl Pts',(-18.9674541463767,23.4069323728757,122.269754763327)) ;
#66886 = CARTESIAN_POINT('Ctrl Pts',(-19.3806182677798,23.6070016493746,121.881570519937)) ;
#66887 = CARTESIAN_POINT('Ctrl Pts',(-19.3863468682687,23.4270125690117,122.187619790065)) ;
#66888 = CARTESIAN_POINT('Ctrl Pts',(-19.9007519851589,23.62680259295,121.962636023239)) ;
#66889 = CARTESIAN_POINT('Ctrl Pts',(-19.8024563004733,23.4468135125871,122.252472687978)) ;
#66890 = CARTESIAN_POINT('Ctrl Pts',(-20.366645013507,23.6467865694595,122.217519363045)) ;
#66891 = CARTESIAN_POINT('Ctrl Pts',(-20.1751704371761,23.4667974890966,122.456380235725)) ;
#66892 = CARTESIAN_POINT('Ctrl Pts',(-20.7158350928187,23.6667025324351,122.615335633075)) ;
#66893 = CARTESIAN_POINT('Ctrl Pts',(-20.4545226369622,23.4867134520722,122.774634459819)) ;
#66894 = CARTESIAN_POINT('Ctrl Pts',(-20.909269753505,23.686572967257,123.106869748193)) ;
#66895 = CARTESIAN_POINT('Ctrl Pts',(-20.6092694713509,23.5065838868942,123.167863591692)) ;
#66896 = CARTESIAN_POINT('Ctrl Pts',(-20.922587690353,23.7066232524901,123.639453176953)) ;
#66897 = CARTESIAN_POINT('Ctrl Pts',(-20.6199224768603,23.5266341721272,123.593929874628)) ;
#66898 = CARTESIAN_POINT('Ctrl Pts',(-20.7562955195823,23.7263972212494,124.138232320058)) ;
#66899 = CARTESIAN_POINT('Ctrl Pts',(-20.4868863698106,23.5464081408865,123.992954730668)) ;
#66900 = CARTESIAN_POINT('Ctrl Pts',(-20.4256681461167,23.746453679369,124.556107455173)) ;
#66901 = CARTESIAN_POINT('Ctrl Pts',(-20.2223831283312,23.5664645990061,124.327253151564)) ;
#66902 = CARTESIAN_POINT('Ctrl Pts',(-19.9777988611578,23.76624856236,124.832456311627)) ;
#66903 = CARTESIAN_POINT('Ctrl Pts',(-19.8640850333811,23.5862594819971,124.548331359068)) ;
#66904 = CARTESIAN_POINT('Ctrl Pts',(-19.4586032621524,23.7862152176623,124.941723989977)) ;
#66905 = CARTESIAN_POINT('Ctrl Pts',(-19.4487277454471,23.6062261372994,124.635742813942)) ;
#66906 = CARTESIAN_POINT('Ctrl Pts',(-18.9333997951415,23.8061741877388,124.86638911577)) ;
#66907 = CARTESIAN_POINT('Ctrl Pts',(-19.0285650781102,23.6261851073759,124.575472274884)) ;
#66908 = CARTESIAN_POINT('Ctrl Pts',(-18.466838553606,23.8260702753289,124.617539311619)) ;
#66909 = CARTESIAN_POINT('Ctrl Pts',(-18.6553167537536,23.6460811949661,124.376389529742)) ;
#66910 = CARTESIAN_POINT('Ctrl Pts',(-18.1127087822637,23.8459684452405,124.224807490326)) ;
#66911 = CARTESIAN_POINT('Ctrl Pts',(-18.3720148240515,23.6659793648776,124.062201436306)) ;
#66912 = CARTESIAN_POINT('Ctrl Pts',(-17.9132245363324,23.8658742806076,123.734750368409)) ;
#66913 = CARTESIAN_POINT('Ctrl Pts',(-18.2124303796564,23.6858852002447,123.670153955737)) ;
#66914 = CARTESIAN_POINT('Ctrl Pts',(-17.8929172316979,23.8858242055455,123.204950398228)) ;
#66915 = CARTESIAN_POINT('Ctrl Pts',(-18.1961880248625,23.7058351251827,123.246313584245)) ;
#66916 = CARTESIAN_POINT('Ctrl Pts',(-18.0536055022471,23.9057033954559,122.701563671004)) ;
#66917 = CARTESIAN_POINT('Ctrl Pts',(-18.3247423344152,23.725714315093,122.843604744158)) ;
#66918 = CARTESIAN_POINT('Ctrl Pts',(-18.3778029519875,23.9256847197365,122.280987362701)) ;
#66919 = CARTESIAN_POINT('Ctrl Pts',(-18.584103378577,23.7456956393736,122.507146042841)) ;
#66920 = CARTESIAN_POINT('Ctrl Pts',(-18.8251843464588,23.9456145039448,121.997171158723)) ;
#66921 = CARTESIAN_POINT('Ctrl Pts',(-18.9420106639801,23.765625423582,122.280096052287)) ;
#66922 = CARTESIAN_POINT('Ctrl Pts',(-19.3420527237489,23.9655344933356,121.8830575886)) ;
#66923 = CARTESIAN_POINT('Ctrl Pts',(-19.3555069146509,23.7855454129728,122.188809484294)) ;
#66924 = CARTESIAN_POINT('Ctrl Pts',(-19.8655341729859,23.9853896886896,121.950798016933)) ;
#66925 = CARTESIAN_POINT('Ctrl Pts',(-19.7742905208817,23.8054006083268,122.243004187493)) ;
#66926 = CARTESIAN_POINT('Ctrl Pts',(-20.3385180584329,24.005435690349,122.195770834828)) ;
#66927 = CARTESIAN_POINT('Ctrl Pts',(-20.1526809568724,23.8254466099861,122.438992919313)) ;
#66928 = CARTESIAN_POINT('Ctrl Pts',(-20.6359495242104,24.0219354375588,122.518207743344)) ;
#66929 = CARTESIAN_POINT('Ctrl Pts',(-20.3906069626951,23.8419463571959,122.696923825608)) ;
#66930 = CARTESIAN_POINT('Ctrl Pts',(-20.7997715920691,24.0353240420069,122.829526935845)) ;
#66931 = CARTESIAN_POINT('Ctrl Pts',(-20.5216768386143,23.855334961644,122.945999782161)) ;
#66932 = CARTESIAN_POINT('Ctrl Pts',(-20.8788004514205,24.0451858703418,123.076353832387)) ;
#66933 = CARTESIAN_POINT('Ctrl Pts',(-20.5848955788943,23.8651967899789,123.143455681254)) ;
#66934 = CARTESIAN_POINT('Ctrl Pts',(-20.9149604443776,24.0551520130994,123.335751428972)) ;
#66935 = CARTESIAN_POINT('Ctrl Pts',(-20.6138199293417,23.8751629327365,123.350985772304)) ;
#66936 = CARTESIAN_POINT('Ctrl Pts',(-20.9016757192965,24.0685137592243,123.68657640661)) ;
#66937 = CARTESIAN_POINT('Ctrl Pts',(-20.6032002770534,23.8885246788614,123.631591920217)) ;
#66938 = CARTESIAN_POINT('Ctrl Pts',(-20.7738010339285,24.0849680881794,124.104947280262)) ;
#66939 = CARTESIAN_POINT('Ctrl Pts',(-20.5008787101127,23.9049790078165,123.966355119094)) ;
#66940 = CARTESIAN_POINT('Ctrl Pts',(-20.506074005893,24.1017353332277,124.460989068715)) ;
#66941 = CARTESIAN_POINT('Ctrl Pts',(-20.2867199296873,23.9217462528648,124.251141688073)) ;
#66942 = CARTESIAN_POINT('Ctrl Pts',(-20.2328267963323,24.1149218985017,124.674311881725)) ;
#66943 = CARTESIAN_POINT('Ctrl Pts',(-20.0681001136612,23.9349328181389,124.421823903416)) ;
#66944 = CARTESIAN_POINT('Ctrl Pts',(-20.0014355866622,24.1249113572463,124.798149275947)) ;
#66945 = CARTESIAN_POINT('Ctrl Pts',(-19.8829901714832,23.9449222768835,124.520886542304)) ;
#66946 = CARTESIAN_POINT('Ctrl Pts',(-19.7528479925732,24.1348651297274,124.879719694348)) ;
#66947 = CARTESIAN_POINT('Ctrl Pts',(-19.6841183272593,23.9548760493646,124.586142147501)) ;
#66948 = CARTESIAN_POINT('Ctrl Pts',(-19.4914820582763,24.1449129462601,124.917021763208)) ;
#66949 = CARTESIAN_POINT('Ctrl Pts',(-19.4750256307248,23.9649238658972,124.615981190194)) ;
#66950 = CARTESIAN_POINT('Ctrl Pts',(-19.2329600579686,24.1547544793826,124.90885452434)) ;
#66951 = CARTESIAN_POINT('Ctrl Pts',(-19.268207989371,23.9747653990197,124.609445249634)) ;
#66952 = CARTESIAN_POINT('Ctrl Pts',(-18.9760140363379,24.1647407216023,124.855708116863)) ;
#66953 = CARTESIAN_POINT('Ctrl Pts',(-19.0626517155432,23.9847516412394,124.566925893019)) ;
#66954 = CARTESIAN_POINT('Ctrl Pts',(-18.7332816198796,24.1746773450272,124.759326036302)) ;
#66955 = CARTESIAN_POINT('Ctrl Pts',(-18.8684666629235,23.9946882646643,124.489818160608)) ;
#66956 = CARTESIAN_POINT('Ctrl Pts',(-18.5085675410313,24.1847272224102,124.620623799681)) ;
#66957 = CARTESIAN_POINT('Ctrl Pts',(-18.6886966289881,24.0047381420473,124.378854470344)) ;
#66958 = CARTESIAN_POINT('Ctrl Pts',(-18.3151003354371,24.1945776611878,124.448610838)) ;
#66959 = CARTESIAN_POINT('Ctrl Pts',(-18.5339244352023,24.0145885808249,124.241242476954)) ;
#66960 = CARTESIAN_POINT('Ctrl Pts',(-18.1519526133633,24.2045496751565,124.243579488805)) ;
#66961 = CARTESIAN_POINT('Ctrl Pts',(-18.4034080760509,24.0245605947936,124.077216069596)) ;
#66962 = CARTESIAN_POINT('Ctrl Pts',(-18.0265886284109,24.2145448437826,124.012717326557)) ;
#66963 = CARTESIAN_POINT('Ctrl Pts',(-18.303118890646,24.0345557634197,123.892525324631)) ;
#66964 = CARTESIAN_POINT('Ctrl Pts',(-17.9432101173695,24.2245787270438,123.762588848226)) ;
#66965 = CARTESIAN_POINT('Ctrl Pts',(-18.2364182327103,24.0445896466809,123.692421857217)) ;
#66966 = CARTESIAN_POINT('Ctrl Pts',(-17.9048199953682,24.2344345971071,123.506429025599)) ;
#66967 = CARTESIAN_POINT('Ctrl Pts',(-18.2057083811246,24.0544455167443,123.487493852008)) ;
#66968 = CARTESIAN_POINT('Ctrl Pts',(-17.9111670277577,24.2444321430243,123.243809194865)) ;
#66969 = CARTESIAN_POINT('Ctrl Pts',(-18.2107882352827,24.0644430626614,123.277398119021)) ;
#66970 = CARTESIAN_POINT('Ctrl Pts',(-17.9624791058961,24.2543402699236,122.988529382377)) ;
#66971 = CARTESIAN_POINT('Ctrl Pts',(-18.2518400388648,24.0743511895607,123.073174891986)) ;
#66972 = CARTESIAN_POINT('Ctrl Pts',(-18.0578908532251,24.2643506414457,122.743365948088)) ;
#66973 = CARTESIAN_POINT('Ctrl Pts',(-18.3281714650137,24.0843615610829,122.877044994232)) ;
#66974 = CARTESIAN_POINT('Ctrl Pts',(-18.1951870356825,24.2743810841931,122.518367543358)) ;
#66975 = CARTESIAN_POINT('Ctrl Pts',(-18.4380103114372,24.0943920038303,122.697047441839)) ;
#66976 = CARTESIAN_POINT('Ctrl Pts',(-18.3658593160879,24.2842290367464,122.323803295538)) ;
#66977 = CARTESIAN_POINT('Ctrl Pts',(-18.574549574067,24.1042399563836,122.541397733003)) ;
#66978 = CARTESIAN_POINT('Ctrl Pts',(-18.5719589574334,24.2942917057674,122.158164871478)) ;
#66979 = CARTESIAN_POINT('Ctrl Pts',(-18.7394306821448,24.1143026254045,122.408888674427)) ;
#66980 = CARTESIAN_POINT('Ctrl Pts',(-18.7999455381362,24.3041860812313,122.033096218261)) ;
#66981 = CARTESIAN_POINT('Ctrl Pts',(-18.9218207704429,24.1241970008685,122.308835803467)) ;
#66982 = CARTESIAN_POINT('Ctrl Pts',(-19.0470862012802,24.3141278795495,121.948467825779)) ;
#66983 = CARTESIAN_POINT('Ctrl Pts',(-19.1195337945076,24.1341387991866,122.24113518591)) ;
#66984 = CARTESIAN_POINT('Ctrl Pts',(-19.306793360523,24.3241303732768,121.9076794678)) ;
#66985 = CARTESIAN_POINT('Ctrl Pts',(-19.3272997862454,24.1441412929139,122.208506614045)) ;
#66986 = CARTESIAN_POINT('Ctrl Pts',(-19.5704262020177,24.3341651717837,121.913035104117)) ;
#66987 = CARTESIAN_POINT('Ctrl Pts',(-19.5382060289476,24.1541760914208,122.212793292696)) ;
#66988 = CARTESIAN_POINT('Ctrl Pts',(-19.8243456090835,24.3440100557631,121.962698662003)) ;
#66989 = CARTESIAN_POINT('Ctrl Pts',(-19.7413407004111,24.1640209754002,122.252526140925)) ;
#66990 = CARTESIAN_POINT('Ctrl Pts',(-20.069363913774,24.3539959125811,122.056545067836)) ;
#66991 = CARTESIAN_POINT('Ctrl Pts',(-19.937354478382,24.1740068322182,122.327605165077)) ;
#66992 = CARTESIAN_POINT('Ctrl Pts',(-20.2933885436929,24.3639307267559,122.190706447143)) ;
#66993 = CARTESIAN_POINT('Ctrl Pts',(-20.1165729005004,24.183941646393,122.434935898804)) ;
#66994 = CARTESIAN_POINT('Ctrl Pts',(-20.4929322997301,24.3739882265412,122.363960667453)) ;
#66995 = CARTESIAN_POINT('Ctrl Pts',(-20.2762066070936,24.1939991461783,122.573540913657)) ;
#66996 = CARTESIAN_POINT('Ctrl Pts',(-20.6558088061112,24.3838099849595,122.564221525997)) ;
#66997 = CARTESIAN_POINT('Ctrl Pts',(-20.4065058327547,24.2038209045966,122.733750399107)) ;
#66998 = CARTESIAN_POINT('Ctrl Pts',(-20.7848399620391,24.3938656427435,122.794804496023)) ;
#66999 = CARTESIAN_POINT('Ctrl Pts',(-20.5097290712294,24.2138765623806,122.918217820985)) ;
#67000 = CARTESIAN_POINT('Ctrl Pts',(-20.8704564403244,24.4038078249235,123.041662828752)) ;
#67001 = CARTESIAN_POINT('Ctrl Pts',(-20.5782202377542,24.2238187445607,123.11570490205)) ;
#67002 = CARTESIAN_POINT('Ctrl Pts',(-20.9125354801232,24.4137130336182,123.298533938)) ;
#67003 = CARTESIAN_POINT('Ctrl Pts',(-20.6118814893409,24.2337239532553,123.321201684156)) ;
#67004 = CARTESIAN_POINT('Ctrl Pts',(-20.909246248355,24.4237548245807,123.562396507273)) ;
#67005 = CARTESIAN_POINT('Ctrl Pts',(-20.6092481539301,24.2437657442178,123.532291786414)) ;
#67006 = CARTESIAN_POINT('Ctrl Pts',(-20.8608714359243,24.4336625990529,123.818239689833)) ;
#67007 = CARTESIAN_POINT('Ctrl Pts',(-20.5705464711203,24.25367351869,123.736965560673)) ;
#67008 = CARTESIAN_POINT('Ctrl Pts',(-20.7683009426795,24.4436740992805,124.064515066611)) ;
#67009 = CARTESIAN_POINT('Ctrl Pts',(-20.496488335269,24.2636850189176,123.933985158452)) ;
#67010 = CARTESIAN_POINT('Ctrl Pts',(-20.6336219825576,24.4537068596732,124.291169915681)) ;
#67011 = CARTESIAN_POINT('Ctrl Pts',(-20.388743464398,24.2737177793103,124.115308070656)) ;
#67012 = CARTESIAN_POINT('Ctrl Pts',(-20.4650972755638,24.4635574288081,124.487670909562)) ;
#67013 = CARTESIAN_POINT('Ctrl Pts',(-20.2539226994214,24.2835683484452,124.272507129792)) ;
#67014 = CARTESIAN_POINT('Ctrl Pts',(-20.262546647733,24.473546038338,124.654592807145)) ;
#67015 = CARTESIAN_POINT('Ctrl Pts',(-20.0918811554699,24.2935569579751,124.40604315333)) ;
#67016 = CARTESIAN_POINT('Ctrl Pts',(-20.035434390892,24.4834746943621,124.783046651201)) ;
#67017 = CARTESIAN_POINT('Ctrl Pts',(-19.910190795979,24.3034856139992,124.508804458404)) ;
#67018 = CARTESIAN_POINT('Ctrl Pts',(-19.788147480938,24.4934624405399,124.871054527459)) ;
#67019 = CARTESIAN_POINT('Ctrl Pts',(-19.7123608220074,24.313473360177,124.579209069275)) ;
#67020 = CARTESIAN_POINT('Ctrl Pts',(-19.5280364525962,24.5034984294756,124.914557400059)) ;
#67021 = CARTESIAN_POINT('Ctrl Pts',(-19.5042716307132,24.3235093491128,124.614009587492)) ;
#67022 = CARTESIAN_POINT('Ctrl Pts',(-19.2690459880752,24.5133532992892,124.912706949231)) ;
#67023 = CARTESIAN_POINT('Ctrl Pts',(-19.2970800077781,24.3333642189264,124.612527489391)) ;
#67024 = CARTESIAN_POINT('Ctrl Pts',(-19.0105743992336,24.523352740531,124.865592193593)) ;
#67025 = CARTESIAN_POINT('Ctrl Pts',(-19.0903031443664,24.3433636601681,124.574834047047)) ;
#67026 = CARTESIAN_POINT('Ctrl Pts',(-18.7666019329129,24.5332478147111,124.775498416424)) ;
#67027 = CARTESIAN_POINT('Ctrl Pts',(-18.8951262877469,24.3532587343482,124.502757699957)) ;
#67028 = CARTESIAN_POINT('Ctrl Pts',(-18.5383021509909,24.5433084705508,124.642232833805)) ;
#67029 = CARTESIAN_POINT('Ctrl Pts',(-18.7124871214675,24.3633193901879,124.39614372167)) ;
#67030 = CARTESIAN_POINT('Ctrl Pts',(-18.3407179161461,24.5531573447464,124.475027408876)) ;
#67031 = CARTESIAN_POINT('Ctrl Pts',(-18.5544214106381,24.3731682643835,124.262378691614)) ;
#67032 = CARTESIAN_POINT('Ctrl Pts',(-18.1716495641239,24.5631860567097,124.272865839476)) ;
#67033 = CARTESIAN_POINT('Ctrl Pts',(-18.4191678481287,24.3831969763468,124.100648461118)) ;
#67034 = CARTESIAN_POINT('Ctrl Pts',(-18.0408595712216,24.5732154572928,124.044039432676)) ;
#67035 = CARTESIAN_POINT('Ctrl Pts',(-18.3145372315862,24.3932263769299,123.917586479356)) ;
#67036 = CARTESIAN_POINT('Ctrl Pts',(-17.9529267054046,24.5830556509096,123.80085466428)) ;
#67037 = CARTESIAN_POINT('Ctrl Pts',(-18.2441926703123,24.4030665705467,123.723039009644)) ;
#67038 = CARTESIAN_POINT('Ctrl Pts',(-17.9073440510645,24.5930590734848,123.541984051105)) ;
#67039 = CARTESIAN_POINT('Ctrl Pts',(-18.2077279538104,24.4130699931219,123.515942359835)) ;
#67040 = CARTESIAN_POINT('Ctrl Pts',(-17.9074876720707,24.6030446105779,123.279530447817)) ;
#67041 = CARTESIAN_POINT('Ctrl Pts',(-18.2078442820345,24.423055530215,123.305979644887)) ;
#67042 = CARTESIAN_POINT('Ctrl Pts',(-17.953701474388,24.6130856150647,123.019767558698)) ;
#67043 = CARTESIAN_POINT('Ctrl Pts',(-18.2448168072216,24.4330965347018,123.098169488521)) ;
#67044 = CARTESIAN_POINT('Ctrl Pts',(-18.0422190940517,24.6229291540059,122.776684574555)) ;
#67045 = CARTESIAN_POINT('Ctrl Pts',(-18.3156319085525,24.442940073643,122.903704466201)) ;
#67046 = CARTESIAN_POINT('Ctrl Pts',(-18.1729536422505,24.6329141849967,122.549220386111)) ;
#67047 = CARTESIAN_POINT('Ctrl Pts',(-18.42022057525,24.4529251046338,122.72173393716)) ;
#67048 = CARTESIAN_POINT('Ctrl Pts',(-18.3403982888488,24.6428536475187,122.348704583029)) ;
#67049 = CARTESIAN_POINT('Ctrl Pts',(-18.5541769923721,24.4628645671558,122.56132244681)) ;
#67050 = CARTESIAN_POINT('Ctrl Pts',(-18.5421236161833,24.6528933797425,122.178692975382)) ;
#67051 = CARTESIAN_POINT('Ctrl Pts',(-18.7155581760706,24.4729042993796,122.425314071837)) ;
#67052 = CARTESIAN_POINT('Ctrl Pts',(-18.766826532383,24.6627815600597,122.048158969798)) ;
#67053 = CARTESIAN_POINT('Ctrl Pts',(-18.8953205045771,24.4827924796968,122.320888330278)) ;
#67054 = CARTESIAN_POINT('Ctrl Pts',(-19.0130885634454,24.6727710757622,121.957251380598)) ;
#67055 = CARTESIAN_POINT('Ctrl Pts',(-19.0923303688238,24.4927819953993,122.248163402219)) ;
#67056 = CARTESIAN_POINT('Ctrl Pts',(-19.2706307855915,24.6827296264169,121.910828202634)) ;
#67057 = CARTESIAN_POINT('Ctrl Pts',(-19.2983640185096,24.502740546054,122.211026103761)) ;
#67058 = CARTESIAN_POINT('Ctrl Pts',(-19.5307897392351,24.6926290335219,121.909185754216)) ;
#67059 = CARTESIAN_POINT('Ctrl Pts',(-19.5064904836855,24.5126399531591,122.209713204043)) ;
#67060 = CARTESIAN_POINT('Ctrl Pts',(-19.7910790035536,24.7026776199382,121.953496342207)) ;
#67061 = CARTESIAN_POINT('Ctrl Pts',(-19.7147218884372,24.5226885395753,122.245162768907)) ;
#67062 = CARTESIAN_POINT('Ctrl Pts',(-20.0360311856884,24.7125704389027,122.040742561825)) ;
#67063 = CARTESIAN_POINT('Ctrl Pts',(-19.9106825930213,24.5325813585398,122.31496045899)) ;
#67064 = CARTESIAN_POINT('Ctrl Pts',(-20.2660472328048,24.7226415564325,122.171540812148)) ;
#67065 = CARTESIAN_POINT('Ctrl Pts',(-20.0946951781208,24.5426524760696,122.419600117649)) ;
#67066 = CARTESIAN_POINT('Ctrl Pts',(-20.4649896868534,24.7324572503985,122.33580820644)) ;
#67067 = CARTESIAN_POINT('Ctrl Pts',(-20.2538475822672,24.5524681700357,122.55101399222)) ;
#67068 = CARTESIAN_POINT('Ctrl Pts',(-20.6368834830163,24.7425236278958,122.536807653796)) ;
#67069 = CARTESIAN_POINT('Ctrl Pts',(-20.3913621437234,24.562534547533,122.711814344018)) ;
#67070 = CARTESIAN_POINT('Ctrl Pts',(-20.7690258159267,24.7524226139777,122.760956322212)) ;
#67071 = CARTESIAN_POINT('Ctrl Pts',(-20.4970748780025,24.5724335336148,122.891133115402)) ;
#67072 = CARTESIAN_POINT('Ctrl Pts',(-20.8617232642626,24.7624767939712,123.008312860307)) ;
#67073 = CARTESIAN_POINT('Ctrl Pts',(-20.5712320948138,24.5824877136083,123.089018856006)) ;
#67074 = CARTESIAN_POINT('Ctrl Pts',(-20.9094544648808,24.7723476069039,123.263341038962)) ;
#67075 = CARTESIAN_POINT('Ctrl Pts',(-20.6094160886339,24.592358526541,123.293040642391)) ;
#67076 = CARTESIAN_POINT('Ctrl Pts',(-20.9122265609454,24.7824215077577,123.527995577717)) ;
#67077 = CARTESIAN_POINT('Ctrl Pts',(-20.6116329563875,24.6024324273948,123.504764628738)) ;
#67078 = CARTESIAN_POINT('Ctrl Pts',(-20.8703860648763,24.7922416631444,123.782706579754)) ;
#67079 = CARTESIAN_POINT('Ctrl Pts',(-20.5781600363798,24.6122525827815,123.708532082081)) ;
#67080 = CARTESIAN_POINT('Ctrl Pts',(-20.7829843523247,24.8023203700966,124.032658419494)) ;
#67081 = CARTESIAN_POINT('Ctrl Pts',(-20.5082379034631,24.6223312897337,123.90849368722)) ;
#67082 = CARTESIAN_POINT('Ctrl Pts',(-20.6564437174401,24.8121719586354,124.258586397133)) ;
#67083 = CARTESIAN_POINT('Ctrl Pts',(-20.4070053415969,24.6321828782725,124.08923482883)) ;
#67084 = CARTESIAN_POINT('Ctrl Pts',(-20.4891628443996,24.8222450751604,124.463680852311)) ;
#67085 = CARTESIAN_POINT('Ctrl Pts',(-20.2731799578671,24.6422559947975,124.253310286516)) ;
#67086 = CARTESIAN_POINT('Ctrl Pts',(-20.2933179390205,24.8320875922562,124.632670356776)) ;
#67087 = CARTESIAN_POINT('Ctrl Pts',(-20.116504494174,24.6520985118933,124.388500688278)) ;
#67088 = CARTESIAN_POINT('Ctrl Pts',(-20.0684748873038,24.8420680538102,124.767681031673)) ;
#67089 = CARTESIAN_POINT('Ctrl Pts',(-19.9366300648084,24.6620789734473,124.496508766413)) ;
#67090 = CARTESIAN_POINT('Ctrl Pts',(-19.8224883546883,24.8520863038009,124.861485946865)) ;
#67091 = CARTESIAN_POINT('Ctrl Pts',(-19.7398406470911,24.6720972234381,124.571552218075)) ;
#67092 = CARTESIAN_POINT('Ctrl Pts',(-19.5674837085229,24.8619704639947,124.911020996683)) ;
#67093 = CARTESIAN_POINT('Ctrl Pts',(-19.535837716226,24.6819813836318,124.611179716792)) ;
#67094 = CARTESIAN_POINT('Ctrl Pts',(-19.3030511330044,24.8720356109697,124.915550386411)) ;
#67095 = CARTESIAN_POINT('Ctrl Pts',(-19.3242913349557,24.6920465306068,124.614802835819)) ;
#67096 = CARTESIAN_POINT('Ctrl Pts',(-19.0475737608601,24.8818774346105,124.875152002711)) ;
#67097 = CARTESIAN_POINT('Ctrl Pts',(-19.1199106517723,24.7018883542476,124.582483957355)) ;
#67098 = CARTESIAN_POINT('Ctrl Pts',(-18.7981220481967,24.8919069070713,124.790082006543)) ;
#67099 = CARTESIAN_POINT('Ctrl Pts',(-18.9203492635413,24.7119178267085,124.514427763563)) ;
#67100 = CARTESIAN_POINT('Ctrl Pts',(-18.5676370265376,24.9019337623334,124.662373648599)) ;
#67101 = CARTESIAN_POINT('Ctrl Pts',(-18.7359613597194,24.7219446819705,124.41226071562)) ;
#67102 = CARTESIAN_POINT('Ctrl Pts',(-18.3661893963596,24.9117770124439,124.500103756191)) ;
#67103 = CARTESIAN_POINT('Ctrl Pts',(-18.5748042848117,24.731787932081,124.282445362066)) ;
#67104 = CARTESIAN_POINT('Ctrl Pts',(-18.1921666070184,24.9218254520271,124.30150622892)) ;
#67105 = CARTESIAN_POINT('Ctrl Pts',(-18.4355860078039,24.7418363716642,124.123567103051)) ;
#67106 = CARTESIAN_POINT('Ctrl Pts',(-18.056967678217,24.931774946275,124.077710500125)) ;
#67107 = CARTESIAN_POINT('Ctrl Pts',(-18.3274273007974,24.7517858659121,123.944530798796)) ;
#67108 = CARTESIAN_POINT('Ctrl Pts',(-17.9623422828139,24.941682802001,123.835129981)) ;
#67109 = CARTESIAN_POINT('Ctrl Pts',(-18.25172727253,24.7616937216381,123.750467050901)) ;
#67110 = CARTESIAN_POINT('Ctrl Pts',(-17.9107761380726,24.9517422786509,123.575884197323)) ;
#67111 = CARTESIAN_POINT('Ctrl Pts',(-18.2104744001724,24.771753198288,123.543070133189)) ;
#67112 = CARTESIAN_POINT('Ctrl Pts',(-17.9047808645182,24.9615830880596,123.317314560702)) ;
#67113 = CARTESIAN_POINT('Ctrl Pts',(-18.2056782172109,24.7815940076967,123.336215598447)) ;
#67114 = CARTESIAN_POINT('Ctrl Pts',(-17.9443132377084,24.9716452383604,123.055891956674)) ;
#67115 = CARTESIAN_POINT('Ctrl Pts',(-18.237304086214,24.7916561579975,123.127077212028)) ;
#67116 = CARTESIAN_POINT('Ctrl Pts',(-18.027522505227,24.981542399483,122.809459900675)) ;
#67117 = CARTESIAN_POINT('Ctrl Pts',(-18.3038712398251,24.8015533191201,122.929932325436)) ;
#67118 = CARTESIAN_POINT('Ctrl Pts',(-18.15191407074,24.991473573887,122.580036852208)) ;
#67119 = CARTESIAN_POINT('Ctrl Pts',(-18.4033840182732,24.8114844935241,122.746394285566)) ;
#67120 = CARTESIAN_POINT('Ctrl Pts',(-18.3162936300384,25.001515777612,122.373591256392)) ;
#67121 = CARTESIAN_POINT('Ctrl Pts',(-18.5348876504328,24.8215266972492,122.581237583697)) ;
#67122 = CARTESIAN_POINT('Ctrl Pts',(-18.5108445770742,25.0114023600425,122.201377852405)) ;
#67123 = CARTESIAN_POINT('Ctrl Pts',(-18.6905276243258,24.8314132796796,122.443467286876)) ;
#67124 = CARTESIAN_POINT('Ctrl Pts',(-18.7344855027603,25.0213957957908,122.063738108185)) ;
#67125 = CARTESIAN_POINT('Ctrl Pts',(-18.8694400641659,24.8414067154279,122.333355312054)) ;
#67126 = CARTESIAN_POINT('Ctrl Pts',(-18.9774777481212,25.031340264149,121.967563232072)) ;
#67127 = CARTESIAN_POINT('Ctrl Pts',(-19.0638333079419,24.8513511837861,122.256415320713)) ;
#67128 = CARTESIAN_POINT('Ctrl Pts',(-19.2335763972328,25.0412920803945,121.914516693683)) ;
#67129 = CARTESIAN_POINT('Ctrl Pts',(-19.2687117105756,24.8613030000317,122.213977773435)) ;
#67130 = CARTESIAN_POINT('Ctrl Pts',(-19.4972265998584,25.051329516509,121.906917954592)) ;
#67131 = CARTESIAN_POINT('Ctrl Pts',(-19.4796319935927,24.8713404361461,122.207898425137)) ;
#67132 = CARTESIAN_POINT('Ctrl Pts',(-19.7542997604475,25.0612144756854,121.944387345544)) ;
#67133 = CARTESIAN_POINT('Ctrl Pts',(-19.6852897308738,24.8812253953225,122.237873404825)) ;
#67134 = CARTESIAN_POINT('Ctrl Pts',(-20.0038315528282,25.0712125938973,122.026544562977)) ;
#67135 = CARTESIAN_POINT('Ctrl Pts',(-19.8849152007323,24.8912235135344,122.303598670447)) ;
#67136 = CARTESIAN_POINT('Ctrl Pts',(-20.2336588620757,25.0811335264093,122.149690526495)) ;
#67137 = CARTESIAN_POINT('Ctrl Pts',(-20.0687767521282,24.9011444460464,122.402114675573)) ;
#67138 = CARTESIAN_POINT('Ctrl Pts',(-20.4411095234431,25.0911748266313,122.31274727971)) ;
#67139 = CARTESIAN_POINT('Ctrl Pts',(-20.2347377340864,24.9111857462685,122.532559732178)) ;
#67140 = CARTESIAN_POINT('Ctrl Pts',(-20.6146855652456,25.1010817450213,122.506787487702)) ;
#67141 = CARTESIAN_POINT('Ctrl Pts',(-20.3735984857151,24.9210926646584,122.687791010339)) ;
#67142 = CARTESIAN_POINT('Ctrl Pts',(-20.7529678400047,25.1110175367304,122.728267052382)) ;
#67143 = CARTESIAN_POINT('Ctrl Pts',(-20.4842246343113,24.9310284563675,122.86497383834)) ;
#67144 = CARTESIAN_POINT('Ctrl Pts',(-20.8514767358832,25.1210584313083,122.973046599286)) ;
#67145 = CARTESIAN_POINT('Ctrl Pts',(-20.5630324089093,24.9410693509454,123.060797371555)) ;
#67146 = CARTESIAN_POINT('Ctrl Pts',(-20.9053425589782,25.1309456330221,123.227241473632)) ;
#67147 = CARTESIAN_POINT('Ctrl Pts',(-20.6061255751286,24.9509565526592,123.264152313877)) ;
#67148 = CARTESIAN_POINT('Ctrl Pts',(-20.9147827032288,25.1409379007837,123.489640019812)) ;
#67149 = CARTESIAN_POINT('Ctrl Pts',(-20.6136784849478,24.9609488204208,123.474070959372)) ;
#67150 = CARTESIAN_POINT('Ctrl Pts',(-20.8786010725189,25.1508864218055,123.748576028363)) ;
#67151 = CARTESIAN_POINT('Ctrl Pts',(-20.5847340147397,24.9708973414426,123.681219445159)) ;
#67152 = CARTESIAN_POINT('Ctrl Pts',(-20.7984664179347,25.1608231953832,123.997081667606)) ;
#67153 = CARTESIAN_POINT('Ctrl Pts',(-20.5206272762469,24.9808341150203,123.880023738464)) ;
#67154 = CARTESIAN_POINT('Ctrl Pts',(-20.6760989906385,25.1708062435242,124.229175844446)) ;
#67155 = CARTESIAN_POINT('Ctrl Pts',(-20.4227342680816,24.9908171631614,124.065699340434)) ;
#67156 = CARTESIAN_POINT('Ctrl Pts',(-20.5139718407011,25.1808499511343,124.437414474404)) ;
#67157 = CARTESIAN_POINT('Ctrl Pts',(-20.2930331145472,25.0008608707714,124.232290876119)) ;
#67158 = CARTESIAN_POINT('Ctrl Pts',(-20.3226951495202,25.1906786442876,124.611032523133)) ;
#67159 = CARTESIAN_POINT('Ctrl Pts',(-20.1400132673799,25.0106895639247,124.371185263449)) ;
#67160 = CARTESIAN_POINT('Ctrl Pts',(-20.098868954127,25.200753393417,124.752367074633)) ;
#67161 = CARTESIAN_POINT('Ctrl Pts',(-19.9609525783771,25.0207643130542,124.484253941825)) ;
#67162 = CARTESIAN_POINT('Ctrl Pts',(-19.858910190644,25.2106187192126,124.850577176108)) ;
#67163 = CARTESIAN_POINT('Ctrl Pts',(-19.7689867940253,25.0306296388497,124.562822605687)) ;
#67164 = CARTESIAN_POINT('Ctrl Pts',(-19.6016970937392,25.2206408935695,124.907156637884)) ;
#67165 = CARTESIAN_POINT('Ctrl Pts',(-19.5632165305531,25.0406518132067,124.608087310509)) ;
#67166 = CARTESIAN_POINT('Ctrl Pts',(-19.33841109203,25.2306669467765,124.91757426496)) ;
#67167 = CARTESIAN_POINT('Ctrl Pts',(-19.3525877130776,25.0506778664136,124.616422422536)) ;
#67168 = CARTESIAN_POINT('Ctrl Pts',(-19.0817846505437,25.2405206436227,124.883149004069)) ;
#67169 = CARTESIAN_POINT('Ctrl Pts',(-19.1472873801373,25.0605315632599,124.588883436946)) ;
#67170 = CARTESIAN_POINT('Ctrl Pts',(-18.8321213569949,25.2504800483757,124.804588928289)) ;
#67171 = CARTESIAN_POINT('Ctrl Pts',(-18.9475566863649,25.0704909680128,124.526036697892)) ;
#67172 = CARTESIAN_POINT('Ctrl Pts',(-18.5982908950502,25.2605182940806,124.68251138002)) ;
#67173 = CARTESIAN_POINT('Ctrl Pts',(-18.7604916748522,25.0805292137177,124.428375651128)) ;
#67174 = CARTESIAN_POINT('Ctrl Pts',(-18.3923032184799,25.2703924782426,124.52465527997)) ;
#67175 = CARTESIAN_POINT('Ctrl Pts',(-18.5957014002325,25.0904033978798,124.302092277131)) ;
#67176 = CARTESIAN_POINT('Ctrl Pts',(-18.2134348354326,25.2804622613806,124.32968799242)) ;
#67177 = CARTESIAN_POINT('Ctrl Pts',(-18.4526055652732,25.1004731810177,124.146119103615)) ;
#67178 = CARTESIAN_POINT('Ctrl Pts',(-18.0743301698985,25.2902955164013,124.111890050986)) ;
#67179 = CARTESIAN_POINT('Ctrl Pts',(-18.341321285219,25.1103064360384,123.971882314404)) ;
#67180 = CARTESIAN_POINT('Ctrl Pts',(-17.9724906536207,25.300325942533,123.868778335182)) ;
#67181 = CARTESIAN_POINT('Ctrl Pts',(-18.2598482995309,25.1203368621701,123.777393441329)) ;
#67182 = CARTESIAN_POINT('Ctrl Pts',(-17.9151462002579,25.31035755472,123.611455902983)) ;
#67183 = CARTESIAN_POINT('Ctrl Pts',(-18.213971454411,25.1303684743571,123.571535713818)) ;
#67184 = CARTESIAN_POINT('Ctrl Pts',(-17.9030533678709,25.3201872515746,123.353441667699)) ;
#67185 = CARTESIAN_POINT('Ctrl Pts',(-18.2042958249843,25.1401981712117,123.365125405049)) ;
#67186 = CARTESIAN_POINT('Ctrl Pts',(-17.935703946638,25.3301766934771,123.092960405583)) ;
#67187 = CARTESIAN_POINT('Ctrl Pts',(-18.2304147144429,25.1501876131142,123.156740340782)) ;
#67188 = CARTESIAN_POINT('Ctrl Pts',(-18.01414488107,25.3402205854928,122.840945210804)) ;
#67189 = CARTESIAN_POINT('Ctrl Pts',(-18.293166125743,25.1602315051299,122.955127645986)) ;
#67190 = CARTESIAN_POINT('Ctrl Pts',(-18.1320014123289,25.350042147262,122.611326074322)) ;
#67191 = CARTESIAN_POINT('Ctrl Pts',(-18.3874495259112,25.1700530668991,122.771432519081)) ;
#67192 = CARTESIAN_POINT('Ctrl Pts',(-18.290812004256,25.3600777188862,122.400775785575)) ;
#67193 = CARTESIAN_POINT('Ctrl Pts',(-18.5144967171378,25.1800886385233,122.602991221329)) ;
#67194 = CARTESIAN_POINT('Ctrl Pts',(-18.4841839838092,25.370106993168,122.221692735608)) ;
#67195 = CARTESIAN_POINT('Ctrl Pts',(-18.6691932985931,25.1901179128051,122.459723641306)) ;
#67196 = CARTESIAN_POINT('Ctrl Pts',(-18.7010269361118,25.3799408302867,122.081101987193)) ;
#67197 = CARTESIAN_POINT('Ctrl Pts',(-18.8426660234848,25.1999517499238,122.347250143643)) ;
#67198 = CARTESIAN_POINT('Ctrl Pts',(-18.9441309444256,25.3899932263748,121.977771975232)) ;
#67199 = CARTESIAN_POINT('Ctrl Pts',(-19.037148711284,25.2100041460119,122.264584503233)) ;
#67200 = CARTESIAN_POINT('Ctrl Pts',(-19.1986250893084,25.3999299933253,121.919230643914)) ;
#67201 = CARTESIAN_POINT('Ctrl Pts',(-19.2407432792532,25.2199409129625,122.21774992714)) ;
#67202 = CARTESIAN_POINT('Ctrl Pts',(-19.459301128586,25.4098642283046,121.905097168243)) ;
#67203 = CARTESIAN_POINT('Ctrl Pts',(-19.4492836234959,25.2298751479417,122.206441411335)) ;
#67204 = CARTESIAN_POINT('Ctrl Pts',(-19.72078773703,25.4198879916314,121.936883279556)) ;
#67205 = CARTESIAN_POINT('Ctrl Pts',(-19.6584731310004,25.2398989112685,122.231868582496)) ;
#67206 = CARTESIAN_POINT('Ctrl Pts',(-19.9693851432808,25.429774333016,122.012355109386)) ;
#67207 = CARTESIAN_POINT('Ctrl Pts',(-19.8573510090563,25.2497852526532,122.292244189265)) ;
#67208 = CARTESIAN_POINT('Ctrl Pts',(-20.2037937296493,25.439763381783,122.130525368287)) ;
#67209 = CARTESIAN_POINT('Ctrl Pts',(-20.0448786033805,25.2597743014202,122.38677867719)) ;
#67210 = CARTESIAN_POINT('Ctrl Pts',(-20.4148854638875,25.4498046024804,122.288855457116)) ;
#67211 = CARTESIAN_POINT('Ctrl Pts',(-20.213753113731,25.2698155221175,122.513441372726)) ;
#67212 = CARTESIAN_POINT('Ctrl Pts',(-20.5918392755866,25.4596372426583,122.477141002139)) ;
#67213 = CARTESIAN_POINT('Ctrl Pts',(-20.3553169822991,25.2796481622954,122.664067990868)) ;
#67214 = CARTESIAN_POINT('Ctrl Pts',(-20.7363655379612,25.4696311719663,122.696425976588)) ;
#67215 = CARTESIAN_POINT('Ctrl Pts',(-20.4709395700862,25.2896420916034,122.839494814172)) ;
#67216 = CARTESIAN_POINT('Ctrl Pts',(-20.8404780632738,25.4796603796468,122.93854969465)) ;
#67217 = CARTESIAN_POINT('Ctrl Pts',(-20.5542313158732,25.2996712992839,123.033193065027)) ;
#67218 = CARTESIAN_POINT('Ctrl Pts',(-20.9004575630717,25.4895361913509,123.191064817286)) ;
#67219 = CARTESIAN_POINT('Ctrl Pts',(-20.6022166706708,25.309547110988,123.235204193094)) ;
#67220 = CARTESIAN_POINT('Ctrl Pts',(-20.9161564441938,25.4995354183223,123.453329386861)) ;
#67221 = CARTESIAN_POINT('Ctrl Pts',(-20.6147777399727,25.3195463379594,123.445015642034)) ;
#67222 = CARTESIAN_POINT('Ctrl Pts',(-20.8865881009697,25.509444899478,123.712094698215)) ;
#67223 = CARTESIAN_POINT('Ctrl Pts',(-20.5911250962336,25.3294558191151,123.65202774278)) ;
#67224 = CARTESIAN_POINT('Ctrl Pts',(-20.81145089258,25.5194981297789,123.965343699702)) ;
#67225 = CARTESIAN_POINT('Ctrl Pts',(-20.5310172244404,25.339509049416,123.854627590473)) ;
#67226 = CARTESIAN_POINT('Ctrl Pts',(-20.6957175422055,25.52936874633,124.197502953534)) ;
#67227 = CARTESIAN_POINT('Ctrl Pts',(-20.438432564313,25.3493796659671,124.040355455078)) ;
#67228 = CARTESIAN_POINT('Ctrl Pts',(-20.5395534186836,25.539390408062,124.409561109384)) ;
#67229 = CARTESIAN_POINT('Ctrl Pts',(-20.3135029430388,25.3594013276991,124.210003211742)) ;
#67230 = CARTESIAN_POINT('Ctrl Pts',(-20.3484908449209,25.5494132212431,124.590878299816)) ;
#67231 = CARTESIAN_POINT('Ctrl Pts',(-20.1606542784881,25.3694241408802,124.355058414572)) ;
#67232 = CARTESIAN_POINT('Ctrl Pts',(-20.1325195803171,25.5592803857031,124.734357216796)) ;
#67233 = CARTESIAN_POINT('Ctrl Pts',(-19.987878794653,25.3792913053402,124.469843008238)) ;
#67234 = CARTESIAN_POINT('Ctrl Pts',(-19.8920996177146,25.569273827923,124.840044812153)) ;
#67235 = CARTESIAN_POINT('Ctrl Pts',(-19.7955437603287,25.3892847475601,124.554394994497)) ;
#67236 = CARTESIAN_POINT('Ctrl Pts',(-19.6358915111173,25.5793055015233,124.902119378316)) ;
#67237 = CARTESIAN_POINT('Ctrl Pts',(-19.5905777624909,25.3993164211604,124.604056661626)) ;
#67238 = CARTESIAN_POINT('Ctrl Pts',(-19.377143513442,25.5891719366363,124.918889100785)) ;
#67239 = CARTESIAN_POINT('Ctrl Pts',(-19.3835799123551,25.4091828562734,124.617474520486)) ;
#67240 = CARTESIAN_POINT('Ctrl Pts',(-19.1162493958071,25.5991593871694,124.890557819024)) ;
#67241 = CARTESIAN_POINT('Ctrl Pts',(-19.1748644832375,25.4191703068065,124.594811646345)) ;
#67242 = CARTESIAN_POINT('Ctrl Pts',(-18.8652039002789,25.6091043169973,124.817783333034)) ;
#67243 = CARTESIAN_POINT('Ctrl Pts',(-18.9740276649419,25.4291152366345,124.536594184406)) ;
#67244 = CARTESIAN_POINT('Ctrl Pts',(-18.6283721225821,25.6191492120525,124.701260743701)) ;
#67245 = CARTESIAN_POINT('Ctrl Pts',(-18.784561279619,25.4391601316896,124.443378036371)) ;
#67246 = CARTESIAN_POINT('Ctrl Pts',(-18.419077049514,25.6290112737383,124.548382059341)) ;
#67247 = CARTESIAN_POINT('Ctrl Pts',(-18.6171242178969,25.4490221933754,124.321077040016)) ;
#67248 = CARTESIAN_POINT('Ctrl Pts',(-18.2367942709095,25.6390029965252,124.359421375143)) ;
#67249 = CARTESIAN_POINT('Ctrl Pts',(-18.4712964601253,25.4590139161623,124.169910079133)) ;
#67250 = CARTESIAN_POINT('Ctrl Pts',(-18.091029495205,25.6489352107651,124.142904444548)) ;
#67251 = CARTESIAN_POINT('Ctrl Pts',(-18.3546829152542,25.4689461304023,123.996697908865)) ;
#67252 = CARTESIAN_POINT('Ctrl Pts',(-17.9844458363519,25.6588745293309,123.904437503963)) ;
#67253 = CARTESIAN_POINT('Ctrl Pts',(-18.2694140074215,25.478885448968,123.805925391818)) ;
#67254 = CARTESIAN_POINT('Ctrl Pts',(-17.9204539831751,25.6689187041067,123.648365609469)) ;
#67255 = CARTESIAN_POINT('Ctrl Pts',(-18.2182183772246,25.4889296237439,123.60106842999)) ;
#67256 = CARTESIAN_POINT('Ctrl Pts',(-17.9020768058315,25.6787892581717,123.389630116784)) ;
#67257 = CARTESIAN_POINT('Ctrl Pts',(-18.2035144291742,25.4988001778088,123.394080402049)) ;
#67258 = CARTESIAN_POINT('Ctrl Pts',(-17.9284060681277,25.6887542405259,123.1290873224)) ;
#67259 = CARTESIAN_POINT('Ctrl Pts',(-18.2245755901221,25.508765160163,123.185646014976)) ;
#67260 = CARTESIAN_POINT('Ctrl Pts',(-18.000430199717,25.6987849434157,122.875529417126)) ;
#67261 = CARTESIAN_POINT('Ctrl Pts',(-18.2821927290592,25.5187958630528,122.98279912396)) ;
#67262 = CARTESIAN_POINT('Ctrl Pts',(-18.1134771988756,25.7086772834409,122.641401239108)) ;
#67263 = CARTESIAN_POINT('Ctrl Pts',(-18.3726282522614,25.528688203078,122.795495711768)) ;
#67264 = CARTESIAN_POINT('Ctrl Pts',(-18.2678679863379,25.7187305166009,122.427066576845)) ;
#67265 = CARTESIAN_POINT('Ctrl Pts',(-18.4961390336313,25.538741436238,122.624026697012)) ;
#67266 = CARTESIAN_POINT('Ctrl Pts',(-18.4538393268546,25.7286117610776,122.245777047898)) ;
#67267 = CARTESIAN_POINT('Ctrl Pts',(-18.6449144658524,25.5486226807147,122.478993530744)) ;
#67268 = CARTESIAN_POINT('Ctrl Pts',(-18.6715752593228,25.7386448819486,122.097176077592)) ;
#67269 = CARTESIAN_POINT('Ctrl Pts',(-18.8191018953641,25.5586558015858,122.360110920692)) ;
#67270 = CARTESIAN_POINT('Ctrl Pts',(-18.9081608033064,25.7485260922237,121.990030737852)) ;
#67271 = CARTESIAN_POINT('Ctrl Pts',(-19.0083693555972,25.5685370118608,122.274392619025)) ;
#67272 = CARTESIAN_POINT('Ctrl Pts',(-19.1642552672847,25.758588167993,121.924365385186)) ;
#67273 = CARTESIAN_POINT('Ctrl Pts',(-19.2132442996693,25.5785990876302,122.2218581685)) ;
#67274 = CARTESIAN_POINT('Ctrl Pts',(-19.4225607860531,25.7684452263748,121.904478285387)) ;
#67275 = CARTESIAN_POINT('Ctrl Pts',(-19.4198885350739,25.5884561460119,122.205946244612)) ;
#67276 = CARTESIAN_POINT('Ctrl Pts',(-19.6839642883553,25.7784397816638,121.929561151871)) ;
#67277 = CARTESIAN_POINT('Ctrl Pts',(-19.6290115124918,25.5984507013009,122.226010297302)) ;
#67278 = CARTESIAN_POINT('Ctrl Pts',(-19.9354025958823,25.7883656691993,121.999101330404)) ;
#67279 = CARTESIAN_POINT('Ctrl Pts',(-19.8301627662093,25.6083765888364,122.281640286907)) ;
#67280 = CARTESIAN_POINT('Ctrl Pts',(-20.1732821454297,25.7983906891946,122.112270545144)) ;
#67281 = CARTESIAN_POINT('Ctrl Pts',(-20.020467298116,25.6184016088317,122.372173604384)) ;
#67282 = CARTESIAN_POINT('Ctrl Pts',(-20.3852412939983,25.8082880662982,122.26301982624)) ;
#67283 = CARTESIAN_POINT('Ctrl Pts',(-20.1900359672413,25.6282989859354,122.49277124775)) ;
#67284 = CARTESIAN_POINT('Ctrl Pts',(-20.5699265939808,25.8182783033791,122.449617357553)) ;
#67285 = CARTESIAN_POINT('Ctrl Pts',(-20.3377857573925,25.6382892230162,122.64204770688)) ;
#67286 = CARTESIAN_POINT('Ctrl Pts',(-20.7196773404664,25.8283149161879,122.666729559919)) ;
#67287 = CARTESIAN_POINT('Ctrl Pts',(-20.4575881296598,25.648325835825,122.815736096847)) ;
#67288 = CARTESIAN_POINT('Ctrl Pts',(-20.8278012350198,25.8381647996059,122.901920140004)) ;
#67289 = CARTESIAN_POINT('Ctrl Pts',(-20.5440893331541,25.658175719243,123.003887861845)) ;
#67290 = CARTESIAN_POINT('Ctrl Pts',(-20.8949727103039,25.8481684165084,123.156051177432)) ;
#67291 = CARTESIAN_POINT('Ctrl Pts',(-20.5978286197024,25.6681793361455,123.207191954639)) ;
#67292 = CARTESIAN_POINT('Ctrl Pts',(-20.9168297433397,25.8581578282735,123.417692998704)) ;
#67293 = CARTESIAN_POINT('Ctrl Pts',(-20.6153163642316,25.6781687479106,123.416505743654)) ;
#67294 = CARTESIAN_POINT('Ctrl Pts',(-20.8926982525151,25.8681765896183,123.67984195633)) ;
#67295 = CARTESIAN_POINT('Ctrl Pts',(-20.5960135622755,25.6881875092555,123.626222991465)) ;
#67296 = CARTESIAN_POINT('Ctrl Pts',(-20.8017581311539,25.8813952649994,124.015153473732)) ;
#67297 = CARTESIAN_POINT('Ctrl Pts',(-20.5232632286193,25.7014061846365,123.894483244612)) ;
#67298 = CARTESIAN_POINT('Ctrl Pts',(-20.6243920028856,25.8947055722441,124.321133430442)) ;
#67299 = CARTESIAN_POINT('Ctrl Pts',(-20.3813483028792,25.7147164918812,124.139291566757)) ;
#67300 = CARTESIAN_POINT('Ctrl Pts',(-20.3779377392562,25.9079432384701,124.566705392269)) ;
#67301 = CARTESIAN_POINT('Ctrl Pts',(-20.1842168620273,25.7279541581072,124.335714004042)) ;
#67302 = CARTESIAN_POINT('Ctrl Pts',(-20.1646098417396,25.9178629338808,124.716521317829)) ;
#67303 = CARTESIAN_POINT('Ctrl Pts',(-20.0135493900519,25.7378738535179,124.455576016923)) ;
#67304 = CARTESIAN_POINT('Ctrl Pts',(-19.9252257840937,25.9279158008794,124.828226044214)) ;
#67305 = CARTESIAN_POINT('Ctrl Pts',(-19.8220451597961,25.7479267205165,124.544939701704)) ;
#67306 = CARTESIAN_POINT('Ctrl Pts',(-19.6751350635831,25.9377712092086,124.895616007158)) ;
#67307 = CARTESIAN_POINT('Ctrl Pts',(-19.6219710432747,25.7577821288458,124.598853833472)) ;
#67308 = CARTESIAN_POINT('Ctrl Pts',(-19.4124225556355,25.9478098408852,124.919414322609)) ;
#67309 = CARTESIAN_POINT('Ctrl Pts',(-19.4118058300607,25.7678207605223,124.617896055851)) ;
#67310 = CARTESIAN_POINT('Ctrl Pts',(-19.0641152659986,25.9611120231522,124.889602889987)) ;
#67311 = CARTESIAN_POINT('Ctrl Pts',(-19.1331381422336,25.7811229427894,124.594040874612)) ;
#67312 = CARTESIAN_POINT('Ctrl Pts',(-18.6502847526992,25.9776570362351,124.740819809691)) ;
#67313 = CARTESIAN_POINT('Ctrl Pts',(-18.8021063710032,25.7976679558722,124.475037523198)) ;
#67314 = CARTESIAN_POINT('Ctrl Pts',(-18.3098802866931,25.9943090523113,124.458074394266)) ;
#67315 = CARTESIAN_POINT('Ctrl Pts',(-18.5297345562069,25.8143199719484,124.248799717003)) ;
#67316 = CARTESIAN_POINT('Ctrl Pts',(-18.1090436808664,26.0075321432166,124.174455573223)) ;
#67317 = CARTESIAN_POINT('Ctrl Pts',(-18.369098690815,25.8275430628537,124.021942719457)) ;
#67318 = CARTESIAN_POINT('Ctrl Pts',(-17.9965176539852,26.0174931027759,123.938117510176)) ;
#67319 = CARTESIAN_POINT('Ctrl Pts',(-18.2790691278245,25.837504022413,123.832864843426)) ;
#67320 = CARTESIAN_POINT('Ctrl Pts',(-17.9266031351628,26.027517899527,123.684128674994)) ;
#67321 = CARTESIAN_POINT('Ctrl Pts',(-18.223137350365,25.8475288191641,123.629678646653)) ;
#67322 = CARTESIAN_POINT('Ctrl Pts',(-17.8934600554389,26.0407423469228,123.338151922398)) ;
#67323 = CARTESIAN_POINT('Ctrl Pts',(-18.1966218500974,25.8607532665599,123.352885080339)) ;
#67324 = CARTESIAN_POINT('Ctrl Pts',(-17.9661098980233,26.0573761316219,122.902122581917)) ;
#67325 = CARTESIAN_POINT('Ctrl Pts',(-18.2547370849816,25.877387051259,123.004073841914)) ;
#67326 = CARTESIAN_POINT('Ctrl Pts',(-18.2260016702492,26.0772787983468,122.441338078492)) ;
#67327 = CARTESIAN_POINT('Ctrl Pts',(-18.4626485568475,25.897289717984,122.6354399701)) ;
#67328 = CARTESIAN_POINT('Ctrl Pts',(-18.6269689740633,26.0971790261287,122.096464789941)) ;
#67329 = CARTESIAN_POINT('Ctrl Pts',(-18.7834208261286,25.9171899457658,122.359539719814)) ;
#67330 = CARTESIAN_POINT('Ctrl Pts',(-19.1218834344603,26.1170965136602,121.908606135804)) ;
#67331 = CARTESIAN_POINT('Ctrl Pts',(-19.1793520415274,25.9371074332973,122.209249695182)) ;
#67332 = CARTESIAN_POINT('Ctrl Pts',(-19.6515421009118,26.1370260394771,121.900579250022)) ;
#67333 = CARTESIAN_POINT('Ctrl Pts',(-19.6030795010678,25.9570369591142,122.202825735213)) ;
#67334 = CARTESIAN_POINT('Ctrl Pts',(-20.1529386123422,26.1569883073634,122.074158377623)) ;
#67335 = CARTESIAN_POINT('Ctrl Pts',(-20.0041977734396,25.9769992270005,122.341686821222)) ;
#67336 = CARTESIAN_POINT('Ctrl Pts',(-20.5634651727886,26.1768785023156,122.407118082729)) ;
#67337 = CARTESIAN_POINT('Ctrl Pts',(-20.3326212396169,25.9968894219527,122.608053440236)) ;
#67338 = CARTESIAN_POINT('Ctrl Pts',(-20.8369695350651,26.1967687470618,122.859653772299)) ;
#67339 = CARTESIAN_POINT('Ctrl Pts',(-20.5514266616668,26.016779666699,122.970082039285)) ;
#67340 = CARTESIAN_POINT('Ctrl Pts',(-20.9394612388346,26.2168431196243,123.383189522101)) ;
#67341 = CARTESIAN_POINT('Ctrl Pts',(-20.6334217424483,26.0368540392614,123.388909499368)) ;
#67342 = CARTESIAN_POINT('Ctrl Pts',(-20.858478621002,26.2366284969846,123.902848054689)) ;
#67343 = CARTESIAN_POINT('Ctrl Pts',(-20.5686369629156,26.0566394166217,123.80463880822)) ;
#67344 = CARTESIAN_POINT('Ctrl Pts',(-20.604272042101,26.2565903710517,124.368482650199)) ;
#67345 = CARTESIAN_POINT('Ctrl Pts',(-20.3652721856668,26.0766012906889,124.177147290224)) ;
#67346 = CARTESIAN_POINT('Ctrl Pts',(-20.2051802401964,26.2765703465422,124.718824795122)) ;
#67347 = CARTESIAN_POINT('Ctrl Pts',(-20.0459994054117,26.0965812661794,124.457422009913)) ;
#67348 = CARTESIAN_POINT('Ctrl Pts',(-19.7149987089246,26.2963827764202,124.911292999828)) ;
#67349 = CARTESIAN_POINT('Ctrl Pts',(-19.6538521960381,26.1163936960573,124.611397916623)) ;
#67350 = CARTESIAN_POINT('Ctrl Pts',(-19.1842547999823,26.3163628845105,124.925735636618)) ;
#67351 = CARTESIAN_POINT('Ctrl Pts',(-19.2292567523326,26.1363738041476,124.622952026166)) ;
#67352 = CARTESIAN_POINT('Ctrl Pts',(-18.6824717518944,26.3362572681077,124.758627144309)) ;
#67353 = CARTESIAN_POINT('Ctrl Pts',(-18.8278291137582,26.1562681877448,124.489264722442)) ;
#67354 = CARTESIAN_POINT('Ctrl Pts',(-18.2670439988586,26.3561841960849,124.430303289928)) ;
#67355 = CARTESIAN_POINT('Ctrl Pts',(-18.4954865238769,26.1761951157221,124.226604620263)) ;
#67356 = CARTESIAN_POINT('Ctrl Pts',(-17.9883141683562,26.3760790533862,123.980817223551)) ;
#67357 = CARTESIAN_POINT('Ctrl Pts',(-18.2725029335029,26.1960899730233,123.867014230406)) ;
#67358 = CARTESIAN_POINT('Ctrl Pts',(-17.8794749235701,26.3961182469898,123.459500138785)) ;
#67359 = CARTESIAN_POINT('Ctrl Pts',(-18.1854325963948,26.2161291666269,123.449960783738)) ;
#67360 = CARTESIAN_POINT('Ctrl Pts',(-17.9544430376458,26.4159582149006,122.937489228161)) ;
#67361 = CARTESIAN_POINT('Ctrl Pts',(-18.2454084587968,26.2359691345377,123.032350471907)) ;
#67362 = CARTESIAN_POINT('Ctrl Pts',(-18.2027276437108,26.4358730318646,122.470081707864)) ;
#67363 = CARTESIAN_POINT('Ctrl Pts',(-18.4440381844851,26.2558839515018,122.658424577818)) ;
#67364 = CARTESIAN_POINT('Ctrl Pts',(-18.596400995126,26.4558152772609,122.115240379138)) ;
#67365 = CARTESIAN_POINT('Ctrl Pts',(-18.7589785547177,26.275826196898,122.374552517246)) ;
#67366 = CARTESIAN_POINT('Ctrl Pts',(-19.0856111707764,26.4756873253754,121.915849802114)) ;
#67367 = CARTESIAN_POINT('Ctrl Pts',(-19.1503485944393,26.2956982450125,122.215041802279)) ;
#67368 = CARTESIAN_POINT('Ctrl Pts',(-19.6169161682822,26.4956983903295,121.895626311636)) ;
#67369 = CARTESIAN_POINT('Ctrl Pts',(-19.57539261041,26.3157093099666,122.198865364486)) ;
#67370 = CARTESIAN_POINT('Ctrl Pts',(-20.118823655691,26.5155099146331,122.055636433992)) ;
#67371 = CARTESIAN_POINT('Ctrl Pts',(-19.9769191395575,26.3355208342703,122.326876501952)) ;
#67372 = CARTESIAN_POINT('Ctrl Pts',(-20.5414187886625,26.5356051265965,122.381904092641)) ;
#67373 = CARTESIAN_POINT('Ctrl Pts',(-20.3149929725486,26.3556160462336,122.587892382152)) ;
#67374 = CARTESIAN_POINT('Ctrl Pts',(-20.8229786362358,26.5553858505163,122.826139617815)) ;
#67375 = CARTESIAN_POINT('Ctrl Pts',(-20.5402392941985,26.3753967701534,122.943283661868)) ;
#67376 = CARTESIAN_POINT('Ctrl Pts',(-20.9383530388371,26.5753769261591,123.344589665565)) ;
#67377 = CARTESIAN_POINT('Ctrl Pts',(-20.6325355740105,26.3953878457962,123.358044462546)) ;
#67378 = CARTESIAN_POINT('Ctrl Pts',(-20.86985320622,26.5952588652021,123.868710610695)) ;
#67379 = CARTESIAN_POINT('Ctrl Pts',(-20.577732355409,26.4152697848392,123.777341477282)) ;
#67380 = CARTESIAN_POINT('Ctrl Pts',(-20.6263804833536,26.6152114697054,124.339726432393)) ;
#67381 = CARTESIAN_POINT('Ctrl Pts',(-20.3829508664611,26.4352223893425,124.154152702177)) ;
#67382 = CARTESIAN_POINT('Ctrl Pts',(-20.2377323609478,26.635110338436,124.698507478413)) ;
#67383 = CARTESIAN_POINT('Ctrl Pts',(-20.0720296498314,26.4551212580731,124.441175303376)) ;
#67384 = CARTESIAN_POINT('Ctrl Pts',(-19.750506384729,26.6550037382456,124.903616092832)) ;
#67385 = CARTESIAN_POINT('Ctrl Pts',(-19.6822465171285,26.4750146578827,124.605258460819)) ;
#67386 = CARTESIAN_POINT('Ctrl Pts',(-19.2219548120851,26.6749128690856,124.930993209538)) ;
#67387 = CARTESIAN_POINT('Ctrl Pts',(-19.2594063325904,26.4949237887228,124.627157492375)) ;
#67388 = CARTESIAN_POINT('Ctrl Pts',(-18.7130356342311,26.6949449688492,124.774763267432)) ;
#67389 = CARTESIAN_POINT('Ctrl Pts',(-18.8522664567341,26.5149558884863,124.502164665301)) ;
#67390 = CARTESIAN_POINT('Ctrl Pts',(-18.3620528555376,26.7114770420187,124.510268121194)) ;
#67391 = CARTESIAN_POINT('Ctrl Pts',(-18.5715001976287,26.5314879616558,124.290581423656)) ;
#67392 = CARTESIAN_POINT('Ctrl Pts',(-18.1460617747501,26.7248123826246,124.234367496516)) ;
#67393 = CARTESIAN_POINT('Ctrl Pts',(-18.3986933386626,26.5448233022617,124.069844646193)) ;
#67394 = CARTESIAN_POINT('Ctrl Pts',(-18.0239800547126,26.7346549411643,124.006303612785)) ;
#67395 = CARTESIAN_POINT('Ctrl Pts',(-18.3010327997462,26.5546658608015,123.887397815469)) ;
#67396 = CARTESIAN_POINT('Ctrl Pts',(-17.9413973813911,26.7447068480142,123.755428033597)) ;
#67397 = CARTESIAN_POINT('Ctrl Pts',(-18.2349681691499,26.5647177676514,123.686685201408)) ;
#67398 = CARTESIAN_POINT('Ctrl Pts',(-17.891686149238,26.7579553624051,123.410787353362)) ;
#67399 = CARTESIAN_POINT('Ctrl Pts',(-18.1952008751101,26.5779662820423,123.411026738166)) ;
#67400 = CARTESIAN_POINT('Ctrl Pts',(-17.9431815127596,26.7745545373529,122.972680824458)) ;
#67401 = CARTESIAN_POINT('Ctrl Pts',(-18.2364062949001,26.59456545699,123.060472645166)) ;
#67402 = CARTESIAN_POINT('Ctrl Pts',(-18.1408483242503,26.7911433231479,122.578566000262)) ;
#67403 = CARTESIAN_POINT('Ctrl Pts',(-18.3945264353871,26.6111542427851,122.745229800877)) ;
#67404 = CARTESIAN_POINT('Ctrl Pts',(-18.3723926843041,26.8044191394899,122.317598644227)) ;
#67405 = CARTESIAN_POINT('Ctrl Pts',(-18.5797786876683,26.624430059127,122.536429224287)) ;
#67406 = CARTESIAN_POINT('Ctrl Pts',(-18.5775216542846,26.8143929902837,122.15442033865)) ;
#67407 = CARTESIAN_POINT('Ctrl Pts',(-18.7438803146688,26.6344039099208,122.405894095803)) ;
#67408 = CARTESIAN_POINT('Ctrl Pts',(-18.8092589677791,26.8244220223761,122.028905565457)) ;
#67409 = CARTESIAN_POINT('Ctrl Pts',(-18.9292719326846,26.6444329420132,122.305482723991)) ;
#67410 = CARTESIAN_POINT('Ctrl Pts',(-19.0557421895212,26.834312147878,121.946421302957)) ;
#67411 = CARTESIAN_POINT('Ctrl Pts',(-19.1264590870646,26.6543230675151,122.239497816618)) ;
#67412 = CARTESIAN_POINT('Ctrl Pts',(-19.3153650354541,26.8443046261495,121.907247691411)) ;
#67413 = CARTESIAN_POINT('Ctrl Pts',(-19.3341577092669,26.6643155457866,122.208161046948)) ;
#67414 = CARTESIAN_POINT('Ctrl Pts',(-19.5768371046668,26.8542558412469,121.913582155201)) ;
#67415 = CARTESIAN_POINT('Ctrl Pts',(-19.5433352791444,26.674266760884,122.213230894477)) ;
#67416 = CARTESIAN_POINT('Ctrl Pts',(-19.8356332457282,26.8643043430019,121.965922317603)) ;
#67417 = CARTESIAN_POINT('Ctrl Pts',(-19.7503716736977,26.6843152626391,122.255105201927)) ;
#67418 = CARTESIAN_POINT('Ctrl Pts',(-20.0765024472187,26.8741456926187,122.060153190044)) ;
#67419 = CARTESIAN_POINT('Ctrl Pts',(-19.9430662458474,26.6941566122558,122.330492010687)) ;
#67420 = CARTESIAN_POINT('Ctrl Pts',(-20.3008378724975,26.8841319836389,122.196241980051)) ;
#67421 = CARTESIAN_POINT('Ctrl Pts',(-20.1225333562957,26.7041429032761,122.439364943551)) ;
#67422 = CARTESIAN_POINT('Ctrl Pts',(-20.4973053062689,26.8940685953675,122.368314358404)) ;
#67423 = CARTESIAN_POINT('Ctrl Pts',(-20.2797057735737,26.7140795150047,122.577024505294)) ;
#67424 = CARTESIAN_POINT('Ctrl Pts',(-20.662628518743,26.9041184707351,122.574234184223)) ;
#67425 = CARTESIAN_POINT('Ctrl Pts',(-20.4119625510863,26.7241293903722,122.741761744443)) ;
#67426 = CARTESIAN_POINT('Ctrl Pts',(-20.7873567686691,26.9139689292705,122.801084418396)) ;
#67427 = CARTESIAN_POINT('Ctrl Pts',(-20.5117431267573,26.7339798489077,122.92324293676)) ;
#67428 = CARTESIAN_POINT('Ctrl Pts',(-20.8724634669083,26.9239408662233,123.048897162386)) ;
#67429 = CARTESIAN_POINT('Ctrl Pts',(-20.5798263274072,26.7439517858604,123.121493774499)) ;
#67430 = CARTESIAN_POINT('Ctrl Pts',(-20.9133152577875,26.9339363231554,123.308411671272)) ;
#67431 = CARTESIAN_POINT('Ctrl Pts',(-20.6125055330845,26.7539472427925,123.329105668054)) ;
#67432 = CARTESIAN_POINT('Ctrl Pts',(-20.9081708679061,26.9439691302085,123.571995622508)) ;
#67433 = CARTESIAN_POINT('Ctrl Pts',(-20.6083877656907,26.7639800498456,123.539972753807)) ;
#67434 = CARTESIAN_POINT('Ctrl Pts',(-20.8585534427238,26.9538290167985,123.826321841959)) ;
#67435 = CARTESIAN_POINT('Ctrl Pts',(-20.5686916578816,26.7738399364356,123.743433118056)) ;
#67436 = CARTESIAN_POINT('Ctrl Pts',(-20.7647835915375,26.9638180973637,124.071480590036)) ;
#67437 = CARTESIAN_POINT('Ctrl Pts',(-20.4936737272855,26.7838290170008,123.939559239062)) ;
#67438 = CARTESIAN_POINT('Ctrl Pts',(-20.6306305349959,26.9737495765729,124.29536007837)) ;
#67439 = CARTESIAN_POINT('Ctrl Pts',(-20.3863494522034,26.79376049621,124.118661555198)) ;
#67440 = CARTESIAN_POINT('Ctrl Pts',(-20.4590264458182,26.9837354360188,124.493916247248)) ;
#67441 = CARTESIAN_POINT('Ctrl Pts',(-20.2490645750113,26.8037463556559,124.277504981672)) ;
#67442 = CARTESIAN_POINT('Ctrl Pts',(-20.254221659418,26.993773586666,124.66014484481)) ;
#67443 = CARTESIAN_POINT('Ctrl Pts',(-20.0852193413478,26.8137845063031,124.410486127387)) ;
#67444 = CARTESIAN_POINT('Ctrl Pts',(-20.0282504284219,27.0036216771704,124.786342691733)) ;
#67445 = CARTESIAN_POINT('Ctrl Pts',(-19.9044415680484,26.8236325968075,124.511442329042)) ;
#67446 = CARTESIAN_POINT('Ctrl Pts',(-19.7786397745395,27.0136825856884,124.873419336829)) ;
#67447 = CARTESIAN_POINT('Ctrl Pts',(-19.7047522927702,26.8336935053255,124.581101595474)) ;
#67448 = CARTESIAN_POINT('Ctrl Pts',(-19.5219286374244,27.0235774328464,124.914963808306)) ;
#67449 = CARTESIAN_POINT('Ctrl Pts',(-19.4993832936596,26.8435883524835,124.614334963387)) ;
#67450 = CARTESIAN_POINT('Ctrl Pts',(-19.2607200330095,27.0335191048914,124.911983091372)) ;
#67451 = CARTESIAN_POINT('Ctrl Pts',(-19.2904166467755,26.8535300245285,124.611948249213)) ;
#67452 = CARTESIAN_POINT('Ctrl Pts',(-19.002340474553,27.0435216320169,124.863486618766)) ;
#67453 = CARTESIAN_POINT('Ctrl Pts',(-19.0837134587159,26.863532551654,124.573148990088)) ;
#67454 = CARTESIAN_POINT('Ctrl Pts',(-18.755708647713,27.0535564232043,124.770193481186)) ;
#67455 = CARTESIAN_POINT('Ctrl Pts',(-18.8864087522121,26.8735673428414,124.498512445791)) ;
#67456 = CARTESIAN_POINT('Ctrl Pts',(-18.53306086531,27.0634013030634,124.63840012197)) ;
#67457 = CARTESIAN_POINT('Ctrl Pts',(-18.7082920013057,26.8834122227005,124.393076157916)) ;
#67458 = CARTESIAN_POINT('Ctrl Pts',(-18.3335903392706,27.0733871836819,124.467951336687)) ;
#67459 = CARTESIAN_POINT('Ctrl Pts',(-18.5487170321478,26.893398103319,124.256715629541)) ;
#67460 = CARTESIAN_POINT('Ctrl Pts',(-18.1673965821684,27.0833219067751,124.266543402248)) ;
#67461 = CARTESIAN_POINT('Ctrl Pts',(-18.4157637799795,26.9033328264122,124.095588174979)) ;
#67462 = CARTESIAN_POINT('Ctrl Pts',(-18.0373591121067,27.0933797470863,124.03648134582)) ;
#67463 = CARTESIAN_POINT('Ctrl Pts',(-18.3117355760186,26.9133906667234,123.911537419721)) ;
#67464 = CARTESIAN_POINT('Ctrl Pts',(-17.9509061764655,27.1032002344828,123.793285094069)) ;
#67465 = CARTESIAN_POINT('Ctrl Pts',(-18.242575359153,26.9232111541199,123.716980330585)) ;
#67466 = CARTESIAN_POINT('Ctrl Pts',(-17.9065238901742,27.1132606358279,123.532692664086)) ;
#67467 = CARTESIAN_POINT('Ctrl Pts',(-18.2070714726686,26.9332715554651,123.508505957209)) ;
#67468 = CARTESIAN_POINT('Ctrl Pts',(-17.9083966530251,27.1231916013808,123.271694164607)) ;
#67469 = CARTESIAN_POINT('Ctrl Pts',(-18.2085717099821,26.943202521018,123.299707472759)) ;
#67470 = CARTESIAN_POINT('Ctrl Pts',(-17.9550143490479,27.1331304637173,123.014732779571)) ;
#67471 = CARTESIAN_POINT('Ctrl Pts',(-18.2458677394245,26.9531413833544,123.094139009809)) ;
#67472 = CARTESIAN_POINT('Ctrl Pts',(-18.0458227293772,27.1431161946435,122.768499870868)) ;
#67473 = CARTESIAN_POINT('Ctrl Pts',(-18.3185162096812,26.9631271142806,122.897153472277)) ;
#67474 = CARTESIAN_POINT('Ctrl Pts',(-18.1787338062467,27.1531405800709,122.54108010085)) ;
#67475 = CARTESIAN_POINT('Ctrl Pts',(-18.4248467768607,26.9731514997081,122.715218646662)) ;
#67476 = CARTESIAN_POINT('Ctrl Pts',(-18.3467863406668,27.1630438644242,122.342321573022)) ;
#67477 = CARTESIAN_POINT('Ctrl Pts',(-18.5592899783311,26.9830547840613,122.556213402555)) ;
#67478 = CARTESIAN_POINT('Ctrl Pts',(-18.5499675318017,27.1731038690022,122.173235543931)) ;
#67479 = CARTESIAN_POINT('Ctrl Pts',(-18.7218362738242,26.9931147886393,122.420945971278)) ;
#67480 = CARTESIAN_POINT('Ctrl Pts',(-18.7744378365037,27.1829471380713,122.044638016558)) ;
#67481 = CARTESIAN_POINT('Ctrl Pts',(-18.9014128616889,27.0029580577084,122.318069943643)) ;
#67482 = CARTESIAN_POINT('Ctrl Pts',(-19.0212070083882,27.192937703679,121.955103241881)) ;
#67483 = CARTESIAN_POINT('Ctrl Pts',(-19.0988286849585,27.0129486233161,122.246443874494)) ;
#67484 = CARTESIAN_POINT('Ctrl Pts',(-19.2782077784814,27.2028658354578,121.910092465526)) ;
#67485 = CARTESIAN_POINT('Ctrl Pts',(-19.3044292293712,27.022876755095,122.210437108631)) ;
#67486 = CARTESIAN_POINT('Ctrl Pts',(-19.5406906769413,27.2128537225387,121.909933250644)) ;
#67487 = CARTESIAN_POINT('Ctrl Pts',(-19.5144154029953,27.0328646421759,122.210311478194)) ;
#67488 = CARTESIAN_POINT('Ctrl Pts',(-19.8003580009036,27.2228896721074,121.956008127035)) ;
#67489 = CARTESIAN_POINT('Ctrl Pts',(-19.7221490136593,27.0429005917445,122.247173180015)) ;
#67490 = CARTESIAN_POINT('Ctrl Pts',(-20.0437890490973,27.2327445584862,122.044444124203)) ;
#67491 = CARTESIAN_POINT('Ctrl Pts',(-19.9168925651677,27.0527554781234,122.317923364294)) ;
#67492 = CARTESIAN_POINT('Ctrl Pts',(-20.2715790260407,27.2427439728341,122.175359156114)) ;
#67493 = CARTESIAN_POINT('Ctrl Pts',(-20.0991236143385,27.0627548924712,122.422656796826)) ;
#67494 = CARTESIAN_POINT('Ctrl Pts',(-20.47132188163,27.2526391380246,122.341923187153)) ;
#67495 = CARTESIAN_POINT('Ctrl Pts',(-20.2589164031302,27.0726500576617,122.555908896478)) ;
#67496 = CARTESIAN_POINT('Ctrl Pts',(-20.6418377253297,27.2626994567166,122.543912452748)) ;
#67497 = CARTESIAN_POINT('Ctrl Pts',(-20.3953279507184,27.0827103763537,122.717501514616)) ;
#67498 = CARTESIAN_POINT('Ctrl Pts',(-20.7720769168341,27.2725495884926,122.767639569015)) ;
#67499 = CARTESIAN_POINT('Ctrl Pts',(-20.4995174924838,27.0925605081298,122.89648329143)) ;
#67500 = CARTESIAN_POINT('Ctrl Pts',(-20.8637005068752,27.2825801589429,123.014783157539)) ;
#67501 = CARTESIAN_POINT('Ctrl Pts',(-20.5728149832003,27.10259107858,123.094198725936)) ;
#67502 = CARTESIAN_POINT('Ctrl Pts',(-20.9103706252309,27.2925943096157,123.273787983254)) ;
#67503 = CARTESIAN_POINT('Ctrl Pts',(-20.6101494956889,27.1126052292528,123.301402858841)) ;
#67504 = CARTESIAN_POINT('Ctrl Pts',(-20.911768495837,27.3024872431611,123.533764947733)) ;
#67505 = CARTESIAN_POINT('Ctrl Pts',(-20.6112662665047,27.1224981627982,123.509383800559)) ;
#67506 = CARTESIAN_POINT('Ctrl Pts',(-20.8678776029836,27.3124767571514,123.792558185261)) ;
#67507 = CARTESIAN_POINT('Ctrl Pts',(-20.5761521325388,27.1324876767885,123.716417986733)) ;
#67508 = CARTESIAN_POINT('Ctrl Pts',(-20.7801754400193,27.3224305278038,124.03903194835)) ;
#67509 = CARTESIAN_POINT('Ctrl Pts',(-20.505989170069,27.1424414474409,123.913596190151)) ;
#67510 = CARTESIAN_POINT('Ctrl Pts',(-20.6496157399914,27.3324782964644,124.26850963764)) ;
#67511 = CARTESIAN_POINT('Ctrl Pts',(-20.4015400481253,27.1524892161015,124.097177744708)) ;
#67512 = CARTESIAN_POINT('Ctrl Pts',(-20.4848531000536,27.3423200229042,124.467895083723)) ;
#67513 = CARTESIAN_POINT('Ctrl Pts',(-20.2697294497831,27.1623309425413,124.256684466489)) ;
#67514 = CARTESIAN_POINT('Ctrl Pts',(-20.2855162962699,27.3523055397269,124.638488743857)) ;
#67515 = CARTESIAN_POINT('Ctrl Pts',(-20.1102593118314,27.172316459364,124.393158279408)) ;
#67516 = CARTESIAN_POINT('Ctrl Pts',(-20.0606131128351,27.3622448714225,124.771385186807)) ;
#67517 = CARTESIAN_POINT('Ctrl Pts',(-19.9303364915707,27.1822557910596,124.499474112979)) ;
#67518 = CARTESIAN_POINT('Ctrl Pts',(-19.8136159800649,27.37228464112,124.864066326302)) ;
#67519 = CARTESIAN_POINT('Ctrl Pts',(-19.7327382216027,27.1922955607571,124.57361785765)) ;
#67520 = CARTESIAN_POINT('Ctrl Pts',(-19.5581817302825,27.3821728023688,124.911855032732)) ;
#67521 = CARTESIAN_POINT('Ctrl Pts',(-19.5283913156951,27.2021837220059,124.61184744574)) ;
#67522 = CARTESIAN_POINT('Ctrl Pts',(-19.2956955404914,27.3921623568712,124.915085978907)) ;
#67523 = CARTESIAN_POINT('Ctrl Pts',(-19.318402520903,27.2121732765083,124.614431045079)) ;
#67524 = CARTESIAN_POINT('Ctrl Pts',(-19.0374725439821,27.4021207713948,124.872626590807)) ;
#67525 = CARTESIAN_POINT('Ctrl Pts',(-19.1118246609645,27.222131691032,124.580462405806)) ;
#67526 = CARTESIAN_POINT('Ctrl Pts',(-18.7917647458714,27.4120206842242,124.787079499337)) ;
#67527 = CARTESIAN_POINT('Ctrl Pts',(-18.9152594335383,27.2320316038613,124.51202396635)) ;
#67528 = CARTESIAN_POINT('Ctrl Pts',(-18.5613480077617,27.4220673838741,124.658240132733)) ;
#67529 = CARTESIAN_POINT('Ctrl Pts',(-18.7309264191264,27.2420783035112,124.40895145111)) ;
#67530 = CARTESIAN_POINT('Ctrl Pts',(-18.3596364546277,27.4319672441797,124.493876043428)) ;
#67531 = CARTESIAN_POINT('Ctrl Pts',(-18.5695583841052,27.2519781638168,124.277459828361)) ;
#67532 = CARTESIAN_POINT('Ctrl Pts',(-18.186909253097,27.4420186483852,124.294086730336)) ;
#67533 = CARTESIAN_POINT('Ctrl Pts',(-18.4313772630263,27.2620295680223,124.117627563925)) ;
#67534 = CARTESIAN_POINT('Ctrl Pts',(-18.0536713291326,27.4518996853063,124.071168267617)) ;
#67535 = CARTESIAN_POINT('Ctrl Pts',(-18.3247881999234,27.2719106049434,123.939292985394)) ;
#67536 = CARTESIAN_POINT('Ctrl Pts',(-17.9597465513536,27.4618995174838,123.825788262627)) ;
#67537 = CARTESIAN_POINT('Ctrl Pts',(-18.24964927092,27.2819104371209,123.742988761484)) ;
#67538 = CARTESIAN_POINT('Ctrl Pts',(-17.9100347106082,27.4718175204687,123.56989145949)) ;
#67539 = CARTESIAN_POINT('Ctrl Pts',(-18.2098807623671,27.2918284401058,123.538271752722)) ;
#67540 = CARTESIAN_POINT('Ctrl Pts',(-17.9055372820663,27.4818688263432,123.305836914717)) ;
#67541 = CARTESIAN_POINT('Ctrl Pts',(-18.2062837024167,27.3018797459804,123.327027911082)) ;
#67542 = CARTESIAN_POINT('Ctrl Pts',(-17.9459117765369,27.4917386497348,123.049572996332)) ;
#67543 = CARTESIAN_POINT('Ctrl Pts',(-18.2385839520129,27.3117495693719,123.122017805772)) ;
#67544 = CARTESIAN_POINT('Ctrl Pts',(-18.0318915985893,27.5018128157851,122.799249602971)) ;
#67545 = CARTESIAN_POINT('Ctrl Pts',(-18.3073686920026,27.3218237354222,122.921759028966)) ;
#67546 = CARTESIAN_POINT('Ctrl Pts',(-18.1565773494833,27.5116328999267,122.573239483822)) ;
#67547 = CARTESIAN_POINT('Ctrl Pts',(-18.4071173341134,27.3316438195639,122.740952378761)) ;
#67548 = CARTESIAN_POINT('Ctrl Pts',(-18.3226042808018,27.5217116266626,122.366962086733)) ;
#67549 = CARTESIAN_POINT('Ctrl Pts',(-18.5399396427468,27.3417225462997,122.575930590935)) ;
#67550 = CARTESIAN_POINT('Ctrl Pts',(-18.5174703780383,27.5315632073121,122.196424414338)) ;
#67551 = CARTESIAN_POINT('Ctrl Pts',(-18.6958321561076,27.3515741269492,122.439501639971)) ;
#67552 = CARTESIAN_POINT('Ctrl Pts',(-18.7437532834736,27.5416363356105,122.05915550415)) ;
#67553 = CARTESIAN_POINT('Ctrl Pts',(-18.8768590906674,27.3616472552476,122.329686841586)) ;
#67554 = CARTESIAN_POINT('Ctrl Pts',(-18.9848658829686,27.5514788135019,121.965469396346)) ;
#67555 = CARTESIAN_POINT('Ctrl Pts',(-19.0697483336544,27.3714897331391,122.25473893346)) ;
#67556 = CARTESIAN_POINT('Ctrl Pts',(-19.2419340497948,27.5614594201,121.913511275121)) ;
#67557 = CARTESIAN_POINT('Ctrl Pts',(-19.2754027022882,27.3814703397371,122.213172868281)) ;
#67558 = CARTESIAN_POINT('Ctrl Pts',(-19.505118136635,27.5714771291188,121.907449255122)) ;
#67559 = CARTESIAN_POINT('Ctrl Pts',(-19.4859499875362,27.3914880487559,122.208323766678)) ;
#67560 = CARTESIAN_POINT('Ctrl Pts',(-19.7620374996728,27.5813633081562,121.946159440311)) ;
#67561 = CARTESIAN_POINT('Ctrl Pts',(-19.6914845708838,27.4013742277934,122.239292171034)) ;
#67562 = CARTESIAN_POINT('Ctrl Pts',(-20.0125674013974,27.5914209207286,122.030295059284)) ;
#67563 = CARTESIAN_POINT('Ctrl Pts',(-19.8919086080025,27.4114318403657,122.306601108605)) ;
#67564 = CARTESIAN_POINT('Ctrl Pts',(-20.2405477178494,27.6012973141007,122.154372035112)) ;
#67565 = CARTESIAN_POINT('Ctrl Pts',(-20.0742918644194,27.4213082337378,122.405862575282)) ;
#67566 = CARTESIAN_POINT('Ctrl Pts',(-20.4463485472987,27.6112923422511,122.317564461287)) ;
#67567 = CARTESIAN_POINT('Ctrl Pts',(-20.2389322836839,27.4313032618883,122.53641659574)) ;
#67568 = CARTESIAN_POINT('Ctrl Pts',(-20.6208115759906,27.6213130890971,122.51483046535)) ;
#67569 = CARTESIAN_POINT('Ctrl Pts',(-20.3785024861279,27.4413240087343,122.694229642115)) ;
#67570 = CARTESIAN_POINT('Ctrl Pts',(-20.7569960330264,27.6312151577635,122.736562250952)) ;
#67571 = CARTESIAN_POINT('Ctrl Pts',(-20.4874494348297,27.4512260774006,122.871614548114)) ;
#67572 = CARTESIAN_POINT('Ctrl Pts',(-20.8538296011518,27.6412058975832,122.980600241119)) ;
#67573 = CARTESIAN_POINT('Ctrl Pts',(-20.5649160765477,27.4612168172203,123.066844821881)) ;
#67574 = CARTESIAN_POINT('Ctrl Pts',(-20.9064812123952,27.6511690937935,123.237061229662)) ;
#67575 = CARTESIAN_POINT('Ctrl Pts',(-20.6070370952218,27.4711800134306,123.272013299712)) ;
#67576 = CARTESIAN_POINT('Ctrl Pts',(-20.9144047817725,27.6610732780936,123.497236530681)) ;
#67577 = CARTESIAN_POINT('Ctrl Pts',(-20.6133758900281,27.4810841977308,123.480152789572)) ;
#67578 = CARTESIAN_POINT('Ctrl Pts',(-20.8762301626549,27.6711337384845,123.758811110914)) ;
#67579 = CARTESIAN_POINT('Ctrl Pts',(-20.5828360598664,27.4911446581216,123.689412720083)) ;
#67580 = CARTESIAN_POINT('Ctrl Pts',(-20.7953249519176,27.6809742843553,124.004465402187)) ;
#67581 = CARTESIAN_POINT('Ctrl Pts',(-20.5181122497151,27.5009852039924,123.88593503245)) ;
#67582 = CARTESIAN_POINT('Ctrl Pts',(-20.6705674371017,27.6910365050671,124.237576347375)) ;
#67583 = CARTESIAN_POINT('Ctrl Pts',(-20.4183061644665,27.5110474247042,124.072424084696)) ;
#67584 = CARTESIAN_POINT('Ctrl Pts',(-20.5096693378974,27.7009336480836,124.441939302609)) ;
#67585 = CARTESIAN_POINT('Ctrl Pts',(-20.2895881841943,27.5209445677207,124.235913821433)) ;
#67586 = CARTESIAN_POINT('Ctrl Pts',(-20.315658373556,27.7108648245008,124.61649018712)) ;
#67587 = CARTESIAN_POINT('Ctrl Pts',(-20.1343799929666,27.5308757441379,124.375554311888)) ;
#67588 = CARTESIAN_POINT('Ctrl Pts',(-20.091657303987,27.7209070382794,124.756002912722)) ;
#67589 = CARTESIAN_POINT('Ctrl Pts',(-19.9551790760134,27.5409179579165,124.487164709501)) ;
#67590 = CARTESIAN_POINT('Ctrl Pts',(-19.8506842942627,27.7307935784821,124.85316185408)) ;
#67591 = CARTESIAN_POINT('Ctrl Pts',(-19.7624015506141,27.5508044981193,124.564891723896)) ;
#67592 = CARTESIAN_POINT('Ctrl Pts',(-19.5938710456304,27.7407871730876,124.907993194414)) ;
#67593 = CARTESIAN_POINT('Ctrl Pts',(-19.5569511707671,27.5607980927247,124.608757063164)) ;
#67594 = CARTESIAN_POINT('Ctrl Pts',(-19.3327071093546,27.7507310482451,124.917315275339)) ;
#67595 = CARTESIAN_POINT('Ctrl Pts',(-19.3480205279212,27.5707419678822,124.616215008341)) ;
#67596 = CARTESIAN_POINT('Ctrl Pts',(-19.0734423500519,27.7606915843599,124.881432829596)) ;
#67597 = CARTESIAN_POINT('Ctrl Pts',(-19.1406090425669,27.5807025039971,124.587509484983)) ;
#67598 = CARTESIAN_POINT('Ctrl Pts',(-18.823353749831,27.7706881876827,124.800925220385)) ;
#67599 = CARTESIAN_POINT('Ctrl Pts',(-18.9405381483672,27.5906991073198,124.523103835156)) ;
#67600 = CARTESIAN_POINT('Ctrl Pts',(-18.5903995182117,27.7807212706372,124.677453935382)) ;
#67601 = CARTESIAN_POINT('Ctrl Pts',(-18.7541745110723,27.6007321902743,124.424327045669)) ;
#67602 = CARTESIAN_POINT('Ctrl Pts',(-18.3859904696139,27.7905724393387,124.518604840361)) ;
#67603 = CARTESIAN_POINT('Ctrl Pts',(-18.5906478871506,27.6105833589758,124.297248765221)) ;
#67604 = CARTESIAN_POINT('Ctrl Pts',(-18.2097360022858,27.8005349300376,124.325031213336)) ;
#67605 = CARTESIAN_POINT('Ctrl Pts',(-18.4496441165959,27.6205458496747,124.142390542805)) ;
#67606 = CARTESIAN_POINT('Ctrl Pts',(-18.0691061956658,27.8105633584554,124.102135115778)) ;
#67607 = CARTESIAN_POINT('Ctrl Pts',(-18.3371397875157,27.6305742780925,123.964073876923)) ;
#67608 = CARTESIAN_POINT('Ctrl Pts',(-17.9704213296521,27.8204737258199,123.861134793012)) ;
#67609 = CARTESIAN_POINT('Ctrl Pts',(-18.2581916587335,27.640484645457,123.771274472976)) ;
#67610 = CARTESIAN_POINT('Ctrl Pts',(-17.9142719852206,27.830408593435,123.606158130962)) ;
#67611 = CARTESIAN_POINT('Ctrl Pts',(-18.2132716018524,27.6504195130721,123.567293812213)) ;
#67612 = CARTESIAN_POINT('Ctrl Pts',(-17.9033759753097,27.840449735414,123.342521266579)) ;
#67613 = CARTESIAN_POINT('Ctrl Pts',(-18.2045541379343,27.6604606550512,123.356384198053)) ;
#67614 = CARTESIAN_POINT('Ctrl Pts',(-17.9377060396121,27.8503368716172,123.084960416994)) ;
#67615 = CARTESIAN_POINT('Ctrl Pts',(-18.2320173908359,27.6703477912543,123.150336250561)) ;
#67616 = CARTESIAN_POINT('Ctrl Pts',(-18.0166431581778,27.8603291540206,122.834538577221)) ;
#67617 = CARTESIAN_POINT('Ctrl Pts',(-18.2951662729315,27.6803400736577,122.94999869318)) ;
#67618 = CARTESIAN_POINT('Ctrl Pts',(-18.137412126526,27.8702776819858,122.602650848213)) ;
#67619 = CARTESIAN_POINT('Ctrl Pts',(-18.3917805539364,27.6902886016229,122.764488533233)) ;
#67620 = CARTESIAN_POINT('Ctrl Pts',(-18.2961056898845,27.8802144131479,122.395304507949)) ;
#67621 = CARTESIAN_POINT('Ctrl Pts',(-18.5187344032728,27.7002253327851,122.598611336762)) ;
#67622 = CARTESIAN_POINT('Ctrl Pts',(-18.4891076721817,27.8901976240079,122.217558370946)) ;
#67623 = CARTESIAN_POINT('Ctrl Pts',(-18.6731351964962,27.710208543645,122.456413869143)) ;
#67624 = CARTESIAN_POINT('Ctrl Pts',(-18.7115707177152,27.9002407231578,122.075605016214)) ;
#67625 = CARTESIAN_POINT('Ctrl Pts',(-18.8511053106445,27.7202516427949,122.342850400546)) ;
#67626 = CARTESIAN_POINT('Ctrl Pts',(-18.9499871891245,27.9100716874327,121.976015433695)) ;
#67627 = CARTESIAN_POINT('Ctrl Pts',(-19.041837051544,27.7300826070698,122.263178278936)) ;
#67628 = CARTESIAN_POINT('Ctrl Pts',(-19.2081615249894,27.9201445398186,121.917767583989)) ;
#67629 = CARTESIAN_POINT('Ctrl Pts',(-19.2483766156714,27.7401554594558,122.216578932533)) ;
#67630 = CARTESIAN_POINT('Ctrl Pts',(-19.4671216625185,27.9300086675304,121.905533740892)) ;
#67631 = CARTESIAN_POINT('Ctrl Pts',(-19.4555437647533,27.7500195871675,122.206790898622)) ;
#67632 = CARTESIAN_POINT('Ctrl Pts',(-19.7284352632182,27.9400308696653,121.938326646805)) ;
#67633 = CARTESIAN_POINT('Ctrl Pts',(-19.6645948238701,27.7600417893024,122.233024081806)) ;
#67634 = CARTESIAN_POINT('Ctrl Pts',(-19.980050984628,27.9500580626337,122.016636385366)) ;
#67635 = CARTESIAN_POINT('Ctrl Pts',(-19.8658877542819,27.7700689822708,122.295670925777)) ;
#67636 = CARTESIAN_POINT('Ctrl Pts',(-20.2103950643466,27.9599136566007,122.135000592785)) ;
#67637 = CARTESIAN_POINT('Ctrl Pts',(-20.0501626545512,27.7799245762378,122.39036086436)) ;
#67638 = CARTESIAN_POINT('Ctrl Pts',(-20.4193072748828,27.969870828466,122.29257198083)) ;
#67639 = CARTESIAN_POINT('Ctrl Pts',(-20.2172929209471,27.7898817481031,122.5164167495)) ;
#67640 = CARTESIAN_POINT('Ctrl Pts',(-20.5987996284151,27.9799096724644,122.485885053549)) ;
#67641 = CARTESIAN_POINT('Ctrl Pts',(-20.3608877406853,27.7999205921015,122.67106648784)) ;
#67642 = CARTESIAN_POINT('Ctrl Pts',(-20.7400613604965,27.98978369634,122.703583668428)) ;
#67643 = CARTESIAN_POINT('Ctrl Pts',(-20.4738977561458,27.8097946159771,122.845224005242)) ;
#67644 = CARTESIAN_POINT('Ctrl Pts',(-20.8433506853364,27.9998535223304,122.947177423952)) ;
#67645 = CARTESIAN_POINT('Ctrl Pts',(-20.5565304991962,27.8198644419675,123.040098768756)) ;
#67646 = CARTESIAN_POINT('Ctrl Pts',(-20.9015266940339,28.0096867662276,123.198973980949)) ;
#67647 = CARTESIAN_POINT('Ctrl Pts',(-20.6030723456922,27.8296976858648,123.241534723945)) ;
#67648 = CARTESIAN_POINT('Ctrl Pts',(-20.9161142994382,28.0197171940007,123.462150342134)) ;
#67649 = CARTESIAN_POINT('Ctrl Pts',(-20.6147438907103,27.8397281136378,123.452075801618)) ;
#67650 = CARTESIAN_POINT('Ctrl Pts',(-20.8840166201033,28.0297488107458,123.72382387547)) ;
#67651 = CARTESIAN_POINT('Ctrl Pts',(-20.5890670287782,27.8497597303829,123.661414851897)) ;
#67652 = CARTESIAN_POINT('Ctrl Pts',(-20.80904662986,28.0395784877265,123.971001465148)) ;
#67653 = CARTESIAN_POINT('Ctrl Pts',(-20.5290926826595,27.8595894073637,123.859156362875)) ;
#67654 = CARTESIAN_POINT('Ctrl Pts',(-20.6910868706554,28.0495680045665,124.205529304447)) ;
#67655 = CARTESIAN_POINT('Ctrl Pts',(-20.4347263402333,27.8695789242036,124.046779212421)) ;
#67656 = CARTESIAN_POINT('Ctrl Pts',(-20.5328182779669,28.0596116167062,124.416742316167)) ;
#67657 = CARTESIAN_POINT('Ctrl Pts',(-20.308112543254,27.8796225363434,124.215750577102)) ;
#67658 = CARTESIAN_POINT('Ctrl Pts',(-20.3448814894554,28.0694342230415,124.593693576125)) ;
#67659 = CARTESIAN_POINT('Ctrl Pts',(-20.1577648989237,27.8894451426787,124.357312023611)) ;
#67660 = CARTESIAN_POINT('Ctrl Pts',(-20.124678185504,28.0794724529408,124.73892784558)) ;
#67661 = CARTESIAN_POINT('Ctrl Pts',(-19.9816030855766,27.8994833725779,124.473500876513)) ;
#67662 = CARTESIAN_POINT('Ctrl Pts',(-19.8829899980489,28.0894834877327,124.842887131756)) ;
#67663 = CARTESIAN_POINT('Ctrl Pts',(-19.7882531778609,27.9094944073698,124.556669703237)) ;
#67664 = CARTESIAN_POINT('Ctrl Pts',(-19.6299384968335,28.0993812186998,124.903017471924)) ;
#67665 = CARTESIAN_POINT('Ctrl Pts',(-19.5858129211223,27.919392138337,124.60477541441)) ;
#67666 = CARTESIAN_POINT('Ctrl Pts',(-19.3678981582499,28.1093708465503,124.918781274721)) ;
#67667 = CARTESIAN_POINT('Ctrl Pts',(-19.3761808908369,27.9293817661874,124.617388123224)) ;
#67668 = CARTESIAN_POINT('Ctrl Pts',(-19.1079954571358,28.1193266369963,124.888817431813)) ;
#67669 = CARTESIAN_POINT('Ctrl Pts',(-19.1682588492881,27.9393375566334,124.593418735249)) ;
#67670 = CARTESIAN_POINT('Ctrl Pts',(-18.8578037171305,28.1292540355584,124.814868421456)) ;
#67671 = CARTESIAN_POINT('Ctrl Pts',(-18.968105356819,27.9492649551955,124.534261321663)) ;
#67672 = CARTESIAN_POINT('Ctrl Pts',(-18.6219935808609,28.1392796306682,124.697390886151)) ;
#67673 = CARTESIAN_POINT('Ctrl Pts',(-18.7794564590463,27.9592905503054,124.440280839266)) ;
#67674 = CARTESIAN_POINT('Ctrl Pts',(-18.413012495007,28.1491654813378,124.543058534145)) ;
#67675 = CARTESIAN_POINT('Ctrl Pts',(-18.612271014501,27.9691764009749,124.316816723086)) ;
#67676 = CARTESIAN_POINT('Ctrl Pts',(-18.2316780606301,28.159154661182,124.353241304876)) ;
#67677 = CARTESIAN_POINT('Ctrl Pts',(-18.4672022077259,27.9791655808191,124.164964317004)) ;
#67678 = CARTESIAN_POINT('Ctrl Pts',(-18.085762555499,28.1691958482856,124.133385523761)) ;
#67679 = CARTESIAN_POINT('Ctrl Pts',(-18.3504682851199,27.9892067679227,123.989080612378)) ;
#67680 = CARTESIAN_POINT('Ctrl Pts',(-17.9820414176768,28.1790284917615,123.896729581303)) ;
#67681 = CARTESIAN_POINT('Ctrl Pts',(-18.2674899943736,27.9990394113987,123.799757297218)) ;
#67682 = CARTESIAN_POINT('Ctrl Pts',(-17.9192545217861,28.189022441471,123.641716424028)) ;
#67683 = CARTESIAN_POINT('Ctrl Pts',(-18.2172586037933,28.0090333611081,123.595747332759)) ;
#67684 = CARTESIAN_POINT('Ctrl Pts',(-17.9021928664862,28.1990515642475,123.378711840277)) ;
#67685 = CARTESIAN_POINT('Ctrl Pts',(-18.2036074112526,28.0190624838847,123.385343770105)) ;
#67686 = CARTESIAN_POINT('Ctrl Pts',(-17.9302039422221,28.2089276951662,123.120680343544)) ;
#67687 = CARTESIAN_POINT('Ctrl Pts',(-18.2260142937599,28.0289386148033,123.178918899042)) ;
#67688 = CARTESIAN_POINT('Ctrl Pts',(-18.0031776926144,28.2189257301832,122.86831261201)) ;
#67689 = CARTESIAN_POINT('Ctrl Pts',(-18.2843913725109,28.0389366498204,122.977024252251)) ;
#67690 = CARTESIAN_POINT('Ctrl Pts',(-18.117736776842,28.2288396599419,122.634287677194)) ;
#67691 = CARTESIAN_POINT('Ctrl Pts',(-18.376036681339,28.0488505795791,122.789803759949)) ;
#67692 = CARTESIAN_POINT('Ctrl Pts',(-18.2731150794606,28.2388828476797,122.420974122389)) ;
#67693 = CARTESIAN_POINT('Ctrl Pts',(-18.5003377353294,28.0588937673169,122.619151688384)) ;
#67694 = CARTESIAN_POINT('Ctrl Pts',(-18.4604722427515,28.2487826898201,122.24045743561)) ;
#67695 = CARTESIAN_POINT('Ctrl Pts',(-18.6502217887544,28.0687936094572,122.474737169911)) ;
#67696 = CARTESIAN_POINT('Ctrl Pts',(-18.6779981948743,28.2587739566281,122.093415286291)) ;
#67697 = CARTESIAN_POINT('Ctrl Pts',(-18.8242413102653,28.0787848762652,122.357101786154)) ;
#67698 = CARTESIAN_POINT('Ctrl Pts',(-18.918918044841,28.2688060587601,121.986355077235)) ;
#67699 = CARTESIAN_POINT('Ctrl Pts',(-19.0169763807828,28.0888169783972,122.271451769572)) ;
#67700 = CARTESIAN_POINT('Ctrl Pts',(-19.1704626082505,28.2786729397148,121.923469734543)) ;
#67701 = CARTESIAN_POINT('Ctrl Pts',(-19.2182110752363,28.098683859352,122.221141611949)) ;
#67702 = CARTESIAN_POINT('Ctrl Pts',(-19.432345213223,28.288664731003,121.904359612356)) ;
#67703 = CARTESIAN_POINT('Ctrl Pts',(-19.4277169183523,28.1086756506401,122.20585140049)) ;
#67704 = CARTESIAN_POINT('Ctrl Pts',(-19.694564039776,28.2986968469145,121.93162572317)) ;
#67705 = CARTESIAN_POINT('Ctrl Pts',(-19.6374921940647,28.1187077665516,122.227662228157)) ;
#67706 = CARTESIAN_POINT('Ctrl Pts',(-19.943995852301,28.3085631637145,122.002434913296)) ;
#67707 = CARTESIAN_POINT('Ctrl Pts',(-19.8370378243453,28.1285740833517,122.284307435928)) ;
#67708 = CARTESIAN_POINT('Ctrl Pts',(-20.1803573809643,28.3185506451881,122.116461326157)) ;
#67709 = CARTESIAN_POINT('Ctrl Pts',(-20.0261278945652,28.1385615648253,122.375526584252)) ;
#67710 = CARTESIAN_POINT('Ctrl Pts',(-20.3925607131235,28.328495569567,122.269070719418)) ;
#67711 = CARTESIAN_POINT('Ctrl Pts',(-20.1958916697619,28.1485064892042,122.497612235911)) ;
#67712 = CARTESIAN_POINT('Ctrl Pts',(-20.5767268496923,28.3385404554777,122.458146387094)) ;
#67713 = CARTESIAN_POINT('Ctrl Pts',(-20.343226130455,28.1585513751149,122.648871279974)) ;
#67714 = CARTESIAN_POINT('Ctrl Pts',(-20.7227745276264,28.3484025591903,122.672264744843)) ;
#67715 = CARTESIAN_POINT('Ctrl Pts',(-20.4600658712918,28.1684134788274,122.820164463442)) ;
#67716 = CARTESIAN_POINT('Ctrl Pts',(-20.8312927348308,28.3583941230148,122.911337082898)) ;
#67717 = CARTESIAN_POINT('Ctrl Pts',(-20.5468824144814,28.1784050426519,123.011421352625)) ;
#67718 = CARTESIAN_POINT('Ctrl Pts',(-20.8961668071842,28.3683269310777,123.164169825498)) ;
#67719 = CARTESIAN_POINT('Ctrl Pts',(-20.5987837570556,28.1883378507148,123.213686829248)) ;
#67720 = CARTESIAN_POINT('Ctrl Pts',(-20.9168053566465,28.378264033314,123.424505796562)) ;
#67721 = CARTESIAN_POINT('Ctrl Pts',(-20.615296810215,28.1982749529511,123.421955292323)) ;
#67722 = CARTESIAN_POINT('Ctrl Pts',(-20.8912939664117,28.3883164795844,123.687418366482)) ;
#67723 = CARTESIAN_POINT('Ctrl Pts',(-20.5948899052389,28.2083273992215,123.632285549448)) ;
#67724 = CARTESIAN_POINT('Ctrl Pts',(-20.8223185569164,28.398162595166,123.936824298385)) ;
#67725 = CARTESIAN_POINT('Ctrl Pts',(-20.5397117877283,28.2181735148031,123.831810673226)) ;
#67726 = CARTESIAN_POINT('Ctrl Pts',(-20.709193147176,28.4082106148809,124.175395051952)) ;
#67727 = CARTESIAN_POINT('Ctrl Pts',(-20.4492134944853,28.228221534518,124.022668227718)) ;
#67728 = CARTESIAN_POINT('Ctrl Pts',(-20.5576594223878,28.4181525665098,124.388243230741)) ;
#67729 = CARTESIAN_POINT('Ctrl Pts',(-20.3279884025434,28.238163486147,124.192947972631)) ;
#67730 = CARTESIAN_POINT('Ctrl Pts',(-20.3719920554206,28.4280913475089,124.571940487482)) ;
#67731 = CARTESIAN_POINT('Ctrl Pts',(-20.1794561524199,28.248102267146,124.339907313728)) ;
#67732 = CARTESIAN_POINT('Ctrl Pts',(-20.155266255181,28.438117396235,124.721739105602)) ;
#67733 = CARTESIAN_POINT('Ctrl Pts',(-20.0060768524774,28.2581283158721,124.45974803094)) ;
#67734 = CARTESIAN_POINT('Ctrl Pts',(-19.9192398618305,28.4480042566432,124.830426395165)) ;
#67735 = CARTESIAN_POINT('Ctrl Pts',(-19.8172566995611,28.2680151762803,124.546699853667)) ;
#67736 = CARTESIAN_POINT('Ctrl Pts',(-19.6643603212813,28.458035531775,124.897541005947)) ;
#67737 = CARTESIAN_POINT('Ctrl Pts',(-19.6133539336829,28.2780464514121,124.600393764835)) ;
#67738 = CARTESIAN_POINT('Ctrl Pts',(-19.405507635062,28.4679185090754,124.919330220156)) ;
#67739 = CARTESIAN_POINT('Ctrl Pts',(-19.4062711317406,28.2879294287125,124.617827171934)) ;
#67740 = CARTESIAN_POINT('Ctrl Pts',(-19.14236864725,28.4779753624826,124.895445755536)) ;
#67741 = CARTESIAN_POINT('Ctrl Pts',(-19.1957631355811,28.2979862821197,124.598722613177)) ;
#67742 = CARTESIAN_POINT('Ctrl Pts',(-18.8081529113529,28.4911436035585,124.80533200887)) ;
#67743 = CARTESIAN_POINT('Ctrl Pts',(-18.9283732060215,28.3111545231956,124.526630734819)) ;
#67744 = CARTESIAN_POINT('Ctrl Pts',(-18.4999549682012,28.504544632785,124.627092881207)) ;
#67745 = CARTESIAN_POINT('Ctrl Pts',(-18.681798248427,28.3245555524222,124.384021484789)) ;
#67746 = CARTESIAN_POINT('Ctrl Pts',(-18.2548346129752,28.5177575495159,124.381018273064)) ;
#67747 = CARTESIAN_POINT('Ctrl Pts',(-18.4857344323844,28.337768469153,124.187192189279)) ;
#67748 = CARTESIAN_POINT('Ctrl Pts',(-18.1049098192041,28.5276859439691,124.167554176501)) ;
#67749 = CARTESIAN_POINT('Ctrl Pts',(-18.3657857952432,28.3476968636062,124.016416466804)) ;
#67750 = CARTESIAN_POINT('Ctrl Pts',(-17.9935167509591,28.5376674440972,123.930036177092)) ;
#67751 = CARTESIAN_POINT('Ctrl Pts',(-18.2766712098695,28.3576783637344,123.826404555807)) ;
#67752 = CARTESIAN_POINT('Ctrl Pts',(-17.9250194853092,28.5477079873673,123.675241990111)) ;
#67753 = CARTESIAN_POINT('Ctrl Pts',(-18.2218707823498,28.3677189070045,123.622569449493)) ;
#67754 = CARTESIAN_POINT('Ctrl Pts',(-17.9019033242933,28.5575573191504,123.417442838969)) ;
#67755 = CARTESIAN_POINT('Ctrl Pts',(-18.2033757289784,28.3775682387876,123.416330378134)) ;
#67756 = CARTESIAN_POINT('Ctrl Pts',(-17.9235537436292,28.5675527236221,123.155670875178)) ;
#67757 = CARTESIAN_POINT('Ctrl Pts',(-18.2206940100474,28.3875636432592,123.206912092977)) ;
#67758 = CARTESIAN_POINT('Ctrl Pts',(-17.990923682755,28.5775690510707,122.901217359065)) ;
#67759 = CARTESIAN_POINT('Ctrl Pts',(-18.2745872927144,28.3975799707078,123.003350782383)) ;
#67760 = CARTESIAN_POINT('Ctrl Pts',(-18.1363563321866,28.5907927082372,122.585573838039)) ;
#67761 = CARTESIAN_POINT('Ctrl Pts',(-18.3909334946143,28.4108036278744,122.750824793006)) ;
#67762 = CARTESIAN_POINT('Ctrl Pts',(-18.361738888197,28.6040869996266,122.313564150216)) ;
#67763 = CARTESIAN_POINT('Ctrl Pts',(-18.5712653371683,28.4240979192637,122.533196651324)) ;
#67764 = CARTESIAN_POINT('Ctrl Pts',(-18.6465253994931,28.6173713505581,122.111531614028)) ;
#67765 = CARTESIAN_POINT('Ctrl Pts',(-18.7990570818657,28.4373822701952,122.371600047551)) ;
#67766 = CARTESIAN_POINT('Ctrl Pts',(-18.8832307222806,28.6273437316199,121.999158080089)) ;
#67767 = CARTESIAN_POINT('Ctrl Pts',(-18.9884277554392,28.447354651257,122.281692950129)) ;
#67768 = CARTESIAN_POINT('Ctrl Pts',(-19.1341788049863,28.6372521112455,121.929579826141)) ;
#67769 = CARTESIAN_POINT('Ctrl Pts',(-19.1891837168037,28.4572630308826,122.22602983351)) ;
#67770 = CARTESIAN_POINT('Ctrl Pts',(-19.3971551455222,28.6473061099936,121.904389073441)) ;
#67771 = CARTESIAN_POINT('Ctrl Pts',(-19.3995659464143,28.4673170296307,122.205875390456)) ;
#67772 = CARTESIAN_POINT('Ctrl Pts',(-19.6555567772795,28.6571683071099,121.924649710965)) ;
#67773 = CARTESIAN_POINT('Ctrl Pts',(-19.6062837665613,28.477179226747,122.222079569028)) ;
#67774 = CARTESIAN_POINT('Ctrl Pts',(-19.9952798306344,28.670515433484,122.011813758423)) ;
#67775 = CARTESIAN_POINT('Ctrl Pts',(-19.8780825920856,28.4905263531211,122.291820399844)) ;
#67776 = CARTESIAN_POINT('Ctrl Pts',(-20.3783371558031,28.6870523991254,122.227433848027)) ;
#67777 = CARTESIAN_POINT('Ctrl Pts',(-20.1845001448543,28.5070633187626,122.464288220489)) ;
#67778 = CARTESIAN_POINT('Ctrl Pts',(-20.6669572705968,28.7036870032994,122.562229846375)) ;
#67779 = CARTESIAN_POINT('Ctrl Pts',(-20.4154369512327,28.5236979229365,122.73217404382)) ;
#67780 = CARTESIAN_POINT('Ctrl Pts',(-20.818619503667,28.716976796542,122.876897221786)) ;
#67781 = CARTESIAN_POINT('Ctrl Pts',(-20.536739963039,28.5369877161791,122.983864515057)) ;
#67782 = CARTESIAN_POINT('Ctrl Pts',(-20.8898646071741,28.7269294278014,123.12852052043)) ;
#67783 = CARTESIAN_POINT('Ctrl Pts',(-20.5937435077852,28.5469403474385,123.185172022197)) ;
#67784 = CARTESIAN_POINT('Ctrl Pts',(-20.916646989976,28.7368813951061,123.388702342932)) ;
#67785 = CARTESIAN_POINT('Ctrl Pts',(-20.6151704550531,28.5568923147432,123.393312774312)) ;
#67786 = CARTESIAN_POINT('Ctrl Pts',(-20.891192739327,28.7502486535699,123.739016958567)) ;
#67787 = CARTESIAN_POINT('Ctrl Pts',(-20.5948058393565,28.570259573207,123.673577519016)) ;
#67788 = CARTESIAN_POINT('Ctrl Pts',(-20.7477418810432,28.7667654655191,124.154036877155)) ;
#67789 = CARTESIAN_POINT('Ctrl Pts',(-20.4800520421779,28.5867763851562,124.005580886931)) ;
#67790 = CARTESIAN_POINT('Ctrl Pts',(-20.4126932064644,28.7867913605254,124.567418944492)) ;
#67791 = CARTESIAN_POINT('Ctrl Pts',(-20.2120144196254,28.6068022801626,124.336293127083)) ;
#67792 = CARTESIAN_POINT('Ctrl Pts',(-19.9614615275447,28.8066020906556,124.838970603354)) ;
#67793 = CARTESIAN_POINT('Ctrl Pts',(-19.8510300684342,28.6266130102927,124.553536623259)) ;
#67794 = CARTESIAN_POINT('Ctrl Pts',(-19.4406750274565,28.8265793067854,124.942183198345)) ;
#67795 = CARTESIAN_POINT('Ctrl Pts',(-19.4344011473137,28.6465902264226,124.636109825958)) ;
#67796 = CARTESIAN_POINT('Ctrl Pts',(-18.9173848458449,28.8465061821807,124.860730356123)) ;
#67797 = CARTESIAN_POINT('Ctrl Pts',(-19.015768045154,28.6665171018178,124.570950325204)) ;
#67798 = CARTESIAN_POINT('Ctrl Pts',(-18.4548495376105,28.866327643657,124.608386572972)) ;
#67799 = CARTESIAN_POINT('Ctrl Pts',(-18.6457373585372,28.6863385632941,124.36907662557)) ;
#67800 = CARTESIAN_POINT('Ctrl Pts',(-18.1021082199431,28.8864019614663,124.20819190284)) ;
#67801 = CARTESIAN_POINT('Ctrl Pts',(-18.3635430360855,28.7064128811034,124.048922914079)) ;
#67802 = CARTESIAN_POINT('Ctrl Pts',(-17.9097030414757,28.9062499304742,123.716849978485)) ;
#67803 = CARTESIAN_POINT('Ctrl Pts',(-18.2096162521416,28.7262608501113,123.655848998423)) ;
#67804 = CARTESIAN_POINT('Ctrl Pts',(-17.8953659112392,28.9261969645374,123.187000088179)) ;
#67805 = CARTESIAN_POINT('Ctrl Pts',(-18.1981447291151,28.7462078841745,123.231968583052)) ;
#67806 = CARTESIAN_POINT('Ctrl Pts',(-18.0624463345147,28.9460929155096,122.685244684184)) ;
#67807 = CARTESIAN_POINT('Ctrl Pts',(-18.3318078029622,28.7661038351467,122.830562717796)) ;
#67808 = CARTESIAN_POINT('Ctrl Pts',(-18.3899816868081,28.9659883951278,122.270147568337)) ;
#67809 = CARTESIAN_POINT('Ctrl Pts',(-18.5938359071739,28.7859993147649,122.498483387)) ;
#67810 = CARTESIAN_POINT('Ctrl Pts',(-18.8408757372252,28.9859445060926,121.990748528834)) ;
#67811 = CARTESIAN_POINT('Ctrl Pts',(-18.9545510633946,28.8059554257297,122.274963123727)) ;
#67812 = CARTESIAN_POINT('Ctrl Pts',(-19.3586261760562,29.0058490541326,121.882442313881)) ;
#67813 = CARTESIAN_POINT('Ctrl Pts',(-19.3687524196573,28.8258599737697,122.188317114002)) ;
#67814 = CARTESIAN_POINT('Ctrl Pts',(-19.8818129365437,29.0257231784517,121.95590917428)) ;
#67815 = CARTESIAN_POINT('Ctrl Pts',(-19.7873033983275,28.8457340980888,122.24709086078)) ;
#67816 = CARTESIAN_POINT('Ctrl Pts',(-20.3522418344828,29.0457777084507,122.206339109689)) ;
#67817 = CARTESIAN_POINT('Ctrl Pts',(-20.1636459491141,28.8657886280878,122.447434352417)) ;
#67818 = CARTESIAN_POINT('Ctrl Pts',(-20.7048254925126,29.0655852222107,122.597429836113)) ;
#67819 = CARTESIAN_POINT('Ctrl Pts',(-20.4457143874069,28.8855961418478,122.760308841788)) ;
#67820 = CARTESIAN_POINT('Ctrl Pts',(-20.9055115949536,29.0855685779784,123.089100356984)) ;
#67821 = CARTESIAN_POINT('Ctrl Pts',(-20.6062625174432,28.9055794976156,123.153645765125)) ;
#67822 = CARTESIAN_POINT('Ctrl Pts',(-20.9255057422183,29.1054868805624,123.618111697477)) ;
#67823 = CARTESIAN_POINT('Ctrl Pts',(-20.622257172822,28.9254978001995,123.576855858986)) ;
#67824 = CARTESIAN_POINT('Ctrl Pts',(-20.7655021762044,29.1253550960081,124.121463964361)) ;
#67825 = CARTESIAN_POINT('Ctrl Pts',(-20.4942524673024,28.9453660156452,123.979538536319)) ;
#67826 = CARTESIAN_POINT('Ctrl Pts',(-20.4398756731327,29.1454054128044,124.543114839599)) ;
#67827 = CARTESIAN_POINT('Ctrl Pts',(-20.2337505118372,28.9654163324415,124.316858031653)) ;
#67828 = CARTESIAN_POINT('Ctrl Pts',(-19.9961359923068,29.1651814746869,124.82522657557)) ;
#67829 = CARTESIAN_POINT('Ctrl Pts',(-19.878755955537,28.985192394324,124.542547120948)) ;
#67830 = CARTESIAN_POINT('Ctrl Pts',(-19.4760372478541,29.1852360803793,124.9408742549)) ;
#67831 = CARTESIAN_POINT('Ctrl Pts',(-19.4626769826316,29.0052470000165,124.63506310846)) ;
#67832 = CARTESIAN_POINT('Ctrl Pts',(-18.9542188864203,29.2050297695352,124.872787108227)) ;
#67833 = CARTESIAN_POINT('Ctrl Pts',(-19.0452207775086,29.0250406891723,124.580591027841)) ;
#67834 = CARTESIAN_POINT('Ctrl Pts',(-18.4824497195716,29.2249964611296,124.630017164074)) ;
#67835 = CARTESIAN_POINT('Ctrl Pts',(-18.667806512202,29.0450073807667,124.386372476876)) ;
#67836 = CARTESIAN_POINT('Ctrl Pts',(-18.1224282621344,29.2449565068806,124.240242601981)) ;
#67837 = CARTESIAN_POINT('Ctrl Pts',(-18.3797910944419,29.0649674265177,124.074550845858)) ;
#67838 = CARTESIAN_POINT('Ctrl Pts',(-17.9173907834527,29.2648547670308,123.752777846934)) ;
#67839 = CARTESIAN_POINT('Ctrl Pts',(-18.2157634593431,29.084865686668,123.68457721216)) ;
#67840 = CARTESIAN_POINT('Ctrl Pts',(-17.8903701259974,29.28474968258,123.224718223152)) ;
#67841 = CARTESIAN_POINT('Ctrl Pts',(-18.1941500680826,29.1047606022171,123.262128658022)) ;
#67842 = CARTESIAN_POINT('Ctrl Pts',(-18.0448227791641,29.3046598629936,122.718584462674)) ;
#67843 = CARTESIAN_POINT('Ctrl Pts',(-18.3177155786987,29.1246707826307,122.857222129875)) ;
#67844 = CARTESIAN_POINT('Ctrl Pts',(-18.3629508949474,29.3245956621079,122.294833096222)) ;
#67845 = CARTESIAN_POINT('Ctrl Pts',(-18.5722211306576,29.144606581745,122.518222926126)) ;
#67846 = CARTESIAN_POINT('Ctrl Pts',(-18.8065966645385,29.344533523762,122.005031573975)) ;
#67847 = CARTESIAN_POINT('Ctrl Pts',(-18.9271398869184,29.1645444433991,122.28638447727)) ;
#67848 = CARTESIAN_POINT('Ctrl Pts',(-19.3219781329333,29.3644525703997,121.88380547982)) ;
#67849 = CARTESIAN_POINT('Ctrl Pts',(-19.339446619592,29.1844634900368,122.189407632627)) ;
#67850 = CARTESIAN_POINT('Ctrl Pts',(-19.8485530096058,29.3844014684538,121.945745518254)) ;
#67851 = CARTESIAN_POINT('Ctrl Pts',(-19.7607049211448,29.2044123880909,122.238961921839)) ;
#67852 = CARTESIAN_POINT('Ctrl Pts',(-20.3214474198052,29.4043072958969,122.18303123303)) ;
#67853 = CARTESIAN_POINT('Ctrl Pts',(-20.1390239324075,29.224318215534,122.428800199034)) ;
#67854 = CARTESIAN_POINT('Ctrl Pts',(-20.6245684184595,29.4208899912622,122.502888255951)) ;
#67855 = CARTESIAN_POINT('Ctrl Pts',(-20.381503037069,29.2409009108993,122.684669703668)) ;
#67856 = CARTESIAN_POINT('Ctrl Pts',(-20.791234180934,29.4341642049858,122.809390920718)) ;
#67857 = CARTESIAN_POINT('Ctrl Pts',(-20.5148468140483,29.2541751246229,122.929890379545)) ;
#67858 = CARTESIAN_POINT('Ctrl Pts',(-20.8750220852076,29.4442109241851,123.05973121324)) ;
#67859 = CARTESIAN_POINT('Ctrl Pts',(-20.5818729237177,29.2642218438223,123.13015699649)) ;
#67860 = CARTESIAN_POINT('Ctrl Pts',(-20.9135737768039,29.4540549588308,123.315549607641)) ;
#67861 = CARTESIAN_POINT('Ctrl Pts',(-20.6127109316255,29.2740658784679,123.334824035889)) ;
#67862 = CARTESIAN_POINT('Ctrl Pts',(-20.9056110532671,29.4673893437353,123.665862635849)) ;
#67863 = CARTESIAN_POINT('Ctrl Pts',(-20.6063479581414,29.2874002633725,123.615020710436)) ;
#67864 = CARTESIAN_POINT('Ctrl Pts',(-20.7817183691016,29.4839765610351,124.089008121444)) ;
#67865 = CARTESIAN_POINT('Ctrl Pts',(-20.5072137252115,29.3039874806722,123.953603177572)) ;
#67866 = CARTESIAN_POINT('Ctrl Pts',(-20.5204871039959,29.500609773073,124.445591168462)) ;
#67867 = CARTESIAN_POINT('Ctrl Pts',(-20.2982490932776,29.3206206927101,124.238824480431)) ;
#67868 = CARTESIAN_POINT('Ctrl Pts',(-20.2482786094575,29.5138922153452,124.664142759317)) ;
#67869 = CARTESIAN_POINT('Ctrl Pts',(-20.0804621387608,29.3339031349823,124.413688421931)) ;
#67870 = CARTESIAN_POINT('Ctrl Pts',(-20.0203496111071,29.5237981032594,124.789853895898)) ;
#67871 = CARTESIAN_POINT('Ctrl Pts',(-19.8981216151747,29.3438090228965,124.514250475789)) ;
#67872 = CARTESIAN_POINT('Ctrl Pts',(-19.7720804977814,29.5337865213645,124.875101645455)) ;
#67873 = CARTESIAN_POINT('Ctrl Pts',(-19.699504035617,29.3537974410017,124.582447706781)) ;
#67874 = CARTESIAN_POINT('Ctrl Pts',(-19.5118312861888,29.5438099486033,124.9158105401)) ;
#67875 = CARTESIAN_POINT('Ctrl Pts',(-19.4913069695219,29.3638208682404,124.615012953148)) ;
#67876 = CARTESIAN_POINT('Ctrl Pts',(-19.2516162816116,29.5537143797203,124.910922144998)) ;
#67877 = CARTESIAN_POINT('Ctrl Pts',(-19.2831262502567,29.3737252993574,124.611097513249)) ;
#67878 = CARTESIAN_POINT('Ctrl Pts',(-18.9093488133413,29.5669775323307,124.844857601197)) ;
#67879 = CARTESIAN_POINT('Ctrl Pts',(-19.0093557497466,29.3869884519678,124.558255787372)) ;
#67880 = CARTESIAN_POINT('Ctrl Pts',(-18.5909285364746,29.5803024302346,124.689972489664)) ;
#67881 = CARTESIAN_POINT('Ctrl Pts',(-18.7545953313426,29.4003133498717,124.434343999134)) ;
#67882 = CARTESIAN_POINT('Ctrl Pts',(-18.3276416499704,29.5935581738502,124.461801734779)) ;
#67883 = CARTESIAN_POINT('Ctrl Pts',(-18.5439553434392,29.4135690934873,124.251793461498)) ;
#67884 = CARTESIAN_POINT('Ctrl Pts',(-18.1623453454126,29.6035175472975,124.258928464813)) ;
#67885 = CARTESIAN_POINT('Ctrl Pts',(-18.4117225892705,29.4235284669346,124.089495803923)) ;
#67886 = CARTESIAN_POINT('Ctrl Pts',(-18.0346636089127,29.6134613712245,124.030895956569)) ;
#67887 = CARTESIAN_POINT('Ctrl Pts',(-18.3095785285436,29.4334722908616,123.907068119568)) ;
#67888 = CARTESIAN_POINT('Ctrl Pts',(-17.9478442966657,29.6235093153718,123.781548712612)) ;
#67889 = CARTESIAN_POINT('Ctrl Pts',(-18.2401254083158,29.4435202350089,123.707589793291)) ;
#67890 = CARTESIAN_POINT('Ctrl Pts',(-17.906234953778,29.6333602865899,123.526025793516)) ;
#67891 = CARTESIAN_POINT('Ctrl Pts',(-18.2068401299479,29.4533712062271,123.503171143586)) ;
#67892 = CARTESIAN_POINT('Ctrl Pts',(-17.9089904954044,29.643332104032,123.264021399714)) ;
#67893 = CARTESIAN_POINT('Ctrl Pts',(-18.2090468245195,29.4633430236691,123.293567757575)) ;
#67894 = CARTESIAN_POINT('Ctrl Pts',(-17.9573656877064,29.6533275263241,123.005808163303)) ;
#67895 = CARTESIAN_POINT('Ctrl Pts',(-18.2477491698236,29.4733384459612,123.086997640274)) ;
#67896 = CARTESIAN_POINT('Ctrl Pts',(-18.0504309097234,29.6633605914478,122.75912999775)) ;
#67897 = CARTESIAN_POINT('Ctrl Pts',(-18.3222034468051,29.4833715110849,122.88965593636)) ;
#67898 = CARTESIAN_POINT('Ctrl Pts',(-18.1824501820335,29.673225924113,122.536018472183)) ;
#67899 = CARTESIAN_POINT('Ctrl Pts',(-18.4278207101303,29.4932368437501,122.711168011498)) ;
#67900 = CARTESIAN_POINT('Ctrl Pts',(-18.352254460823,29.6831864667106,122.336809734032)) ;
#67901 = CARTESIAN_POINT('Ctrl Pts',(-18.5636657405991,29.5031973863477,122.551802554504)) ;
#67902 = CARTESIAN_POINT('Ctrl Pts',(-18.5558196647205,29.6932201522123,122.169242143868)) ;
#67903 = CARTESIAN_POINT('Ctrl Pts',(-18.7265193140521,29.5132310718494,122.417750218351)) ;
#67904 = CARTESIAN_POINT('Ctrl Pts',(-18.7818025397086,29.7031049842026,122.041072921772)) ;
#67905 = CARTESIAN_POINT('Ctrl Pts',(-18.9073065097523,29.5231159038397,122.315216877536)) ;
#67906 = CARTESIAN_POINT('Ctrl Pts',(-19.0310733364163,29.7131724109624,121.952565569517)) ;
#67907 = CARTESIAN_POINT('Ctrl Pts',(-19.1067239210886,29.5331833305995,122.24441307792)) ;
#67908 = CARTESIAN_POINT('Ctrl Pts',(-19.286036901977,29.7230109001213,121.909416064618)) ;
#67909 = CARTESIAN_POINT('Ctrl Pts',(-19.3106948134357,29.5430218197584,122.209895699158)) ;
#67910 = CARTESIAN_POINT('Ctrl Pts',(-19.550453199473,29.7330743813114,121.910880737687)) ;
#67911 = CARTESIAN_POINT('Ctrl Pts',(-19.5222278763447,29.5530853009485,122.211069619433)) ;
#67912 = CARTESIAN_POINT('Ctrl Pts',(-19.8062464008285,29.7429685391265,121.957671456219)) ;
#67913 = CARTESIAN_POINT('Ctrl Pts',(-19.7268617815842,29.5629794587636,122.248504306379)) ;
#67914 = CARTESIAN_POINT('Ctrl Pts',(-20.0513931602021,29.7529103958708,122.047912589705)) ;
#67915 = CARTESIAN_POINT('Ctrl Pts',(-19.9229782497092,29.5729213155079,122.320699150998)) ;
#67916 = CARTESIAN_POINT('Ctrl Pts',(-20.27863327422,29.7629128735422,122.180100002924)) ;
#67917 = CARTESIAN_POINT('Ctrl Pts',(-20.1047692120472,29.5829237931793,122.426450889047)) ;
#67918 = CARTESIAN_POINT('Ctrl Pts',(-20.4798098359431,29.7729476778465,122.350566712122)) ;
#67919 = CARTESIAN_POINT('Ctrl Pts',(-20.265709069093,29.5929585974836,122.562825920578)) ;
#67920 = CARTESIAN_POINT('Ctrl Pts',(-20.64549843004,29.7827925546922,122.549284780308)) ;
#67921 = CARTESIAN_POINT('Ctrl Pts',(-20.3982580187208,29.6028034743293,122.721801389537)) ;
#67922 = CARTESIAN_POINT('Ctrl Pts',(-20.7764071388104,29.7927784342477,122.776669844146)) ;
#67923 = CARTESIAN_POINT('Ctrl Pts',(-20.5029831155846,29.6127893538848,122.903710368416)) ;
#67924 = CARTESIAN_POINT('Ctrl Pts',(-20.8655976909384,29.8027131646062,123.022090489185)) ;
#67925 = CARTESIAN_POINT('Ctrl Pts',(-20.5743335346531,29.6227240842433,123.100047340193)) ;
#67926 = CARTESIAN_POINT('Ctrl Pts',(-20.911118673284,29.8127709769191,123.2824053866)) ;
#67927 = CARTESIAN_POINT('Ctrl Pts',(-20.6107482780399,29.6327818965562,123.308299712704)) ;
#67928 = CARTESIAN_POINT('Ctrl Pts',(-20.9112011989042,29.8225915690435,123.540523528446)) ;
#67929 = CARTESIAN_POINT('Ctrl Pts',(-20.610812264355,29.6426024886806,123.514793589066)) ;
#67930 = CARTESIAN_POINT('Ctrl Pts',(-20.8656816934186,29.8326581546532,123.801062971402)) ;
#67931 = CARTESIAN_POINT('Ctrl Pts',(-20.5743946700159,29.6526690742904,123.723224921033)) ;
#67932 = CARTESIAN_POINT('Ctrl Pts',(-20.7770260888292,29.8425577352351,124.045706385067)) ;
#67933 = CARTESIAN_POINT('Ctrl Pts',(-20.503468442044,29.6625686548722,123.918938590259)) ;
#67934 = CARTESIAN_POINT('Ctrl Pts',(-20.6453879764234,29.8526093349133,124.274656477308)) ;
#67935 = CARTESIAN_POINT('Ctrl Pts',(-20.398156179075,29.6726202545505,124.102097751505)) ;
#67936 = CARTESIAN_POINT('Ctrl Pts',(-20.4790736605817,29.8624835213303,124.473897491922)) ;
#67937 = CARTESIAN_POINT('Ctrl Pts',(-20.2651035506588,29.6824944409674,124.261488905988)) ;
#67938 = CARTESIAN_POINT('Ctrl Pts',(-20.2772141277769,29.8725399972112,124.644389380226)) ;
#67939 = CARTESIAN_POINT('Ctrl Pts',(-20.1036145883348,29.6925509168483,124.39788099837)) ;
#67940 = CARTESIAN_POINT('Ctrl Pts',(-20.0524919644059,29.8824329285138,124.775217544899)) ;
#67941 = CARTESIAN_POINT('Ctrl Pts',(-19.9238362960661,29.7024438481509,124.502541627271)) ;
#67942 = CARTESIAN_POINT('Ctrl Pts',(-19.8043884253136,29.8924957072264,124.866595201475)) ;
#67943 = CARTESIAN_POINT('Ctrl Pts',(-19.7253526612113,29.7125066268636,124.57564199753)) ;
#67944 = CARTESIAN_POINT('Ctrl Pts',(-19.5498333322758,29.9023382328076,124.91262179111)) ;
#67945 = CARTESIAN_POINT('Ctrl Pts',(-19.5217089312482,29.7223491524447,124.612461273201)) ;
#67946 = CARTESIAN_POINT('Ctrl Pts',(-19.2873260771025,29.9123289982325,124.914394172825)) ;
#67947 = CARTESIAN_POINT('Ctrl Pts',(-19.3117032550328,29.7323399178696,124.613877366799)) ;
#67948 = CARTESIAN_POINT('Ctrl Pts',(-19.0300851291776,29.9222570742305,124.870781057726)) ;
#67949 = CARTESIAN_POINT('Ctrl Pts',(-19.1059111853094,29.7422679938676,124.578985150407)) ;
#67950 = CARTESIAN_POINT('Ctrl Pts',(-18.7826904157509,29.9322449846175,124.783069756764)) ;
#67951 = CARTESIAN_POINT('Ctrl Pts',(-18.9079961342318,29.7522559042547,124.508814517184)) ;
#67952 = CARTESIAN_POINT('Ctrl Pts',(-18.5534253143983,29.9422808967425,124.652734665094)) ;
#67953 = CARTESIAN_POINT('Ctrl Pts',(-18.7245848901154,29.7622918163796,124.404544830416)) ;
#67954 = CARTESIAN_POINT('Ctrl Pts',(-18.3536388771245,29.9521359095901,124.487912827377)) ;
#67955 = CARTESIAN_POINT('Ctrl Pts',(-18.5647574170873,29.7721468292273,124.272686483657)) ;
#67956 = CARTESIAN_POINT('Ctrl Pts',(-18.1828123336801,29.9621348555064,124.288313606199)) ;
#67957 = CARTESIAN_POINT('Ctrl Pts',(-18.4280975323811,29.7821457751435,124.113006096126)) ;
#67958 = CARTESIAN_POINT('Ctrl Pts',(-18.0503403718914,29.9720317679544,124.064451745925)) ;
#67959 = CARTESIAN_POINT('Ctrl Pts',(-18.3221216633801,29.7920426875915,123.933916272445)) ;
#67960 = CARTESIAN_POINT('Ctrl Pts',(-17.9572951648542,29.9820855660479,123.817209301492)) ;
#67961 = CARTESIAN_POINT('Ctrl Pts',(-18.2476869703767,29.802096485685,123.736121602035)) ;
#67962 = CARTESIAN_POINT('Ctrl Pts',(-17.9093444927588,29.9919664868746,123.56198502385)) ;
#67963 = CARTESIAN_POINT('Ctrl Pts',(-18.2093281437484,29.8119774065117,123.53194254377)) ;
#67964 = CARTESIAN_POINT('Ctrl Pts',(-17.9059278138796,30.0019710128723,123.299129283876)) ;
#67965 = CARTESIAN_POINT('Ctrl Pts',(-18.2065963307077,29.8219819325095,123.321658010208)) ;
#67966 = CARTESIAN_POINT('Ctrl Pts',(-17.9482064112771,30.0119549764898,123.040145215749)) ;
#67967 = CARTESIAN_POINT('Ctrl Pts',(-18.2404207028938,29.8319658961269,123.114471165854)) ;
#67968 = CARTESIAN_POINT('Ctrl Pts',(-18.035508186737,30.0219946170411,122.791197498885)) ;
#67969 = CARTESIAN_POINT('Ctrl Pts',(-18.3102636613557,29.8420055366782,122.915313421293)) ;
#67970 = CARTESIAN_POINT('Ctrl Pts',(-18.161925212928,30.0318386426558,122.565497657734)) ;
#67971 = CARTESIAN_POINT('Ctrl Pts',(-18.411398175043,29.8518495622929,122.734755088774)) ;
#67972 = CARTESIAN_POINT('Ctrl Pts',(-18.3274685805744,30.0418296484732,122.361708399386)) ;
#67973 = CARTESIAN_POINT('Ctrl Pts',(-18.5438338428557,29.8618405681103,122.571724671418)) ;
#67974 = CARTESIAN_POINT('Ctrl Pts',(-18.5272036340267,30.0518674400053,122.189409573137)) ;
#67975 = CARTESIAN_POINT('Ctrl Pts',(-18.7036229469901,29.8718783596425,122.433886677935)) ;
#67976 = CARTESIAN_POINT('Ctrl Pts',(-18.749230903998,30.0617118397937,122.056613364073)) ;
#67977 = CARTESIAN_POINT('Ctrl Pts',(-18.8812446799317,29.8817227594309,122.327651401076)) ;
#67978 = CARTESIAN_POINT('Ctrl Pts',(-18.994164126273,30.0716966403505,121.962602178295)) ;
#67979 = CARTESIAN_POINT('Ctrl Pts',(-19.0771915377067,29.8917075599876,122.252443739457)) ;
#67980 = CARTESIAN_POINT('Ctrl Pts',(-19.2505801464928,30.0816361637616,121.912649736868)) ;
#67981 = CARTESIAN_POINT('Ctrl Pts',(-19.2823241699332,29.9016470833988,122.212483121513)) ;
#67982 = CARTESIAN_POINT('Ctrl Pts',(-19.5143516088782,30.0916758828626,121.907994125418)) ;
#67983 = CARTESIAN_POINT('Ctrl Pts',(-19.4933414803542,29.9116868024998,122.208759920945)) ;
#67984 = CARTESIAN_POINT('Ctrl Pts',(-19.7710473972636,30.1015640547819,121.948463714533)) ;
#67985 = CARTESIAN_POINT('Ctrl Pts',(-19.6986971847122,29.921574974419,122.241136724367)) ;
#67986 = CARTESIAN_POINT('Ctrl Pts',(-20.0194726827981,30.1115536171989,122.033282181041)) ;
#67987 = CARTESIAN_POINT('Ctrl Pts',(-19.897436877706,29.931564536836,122.30899253618)) ;
#67988 = CARTESIAN_POINT('Ctrl Pts',(-20.2485888048623,30.1215119893936,122.159725978258)) ;
#67989 = CARTESIAN_POINT('Ctrl Pts',(-20.0807288910839,29.9415229090307,122.410148456545)) ;
#67990 = CARTESIAN_POINT('Ctrl Pts',(-20.451481155513,30.1314120636243,122.322590700227)) ;
#67991 = CARTESIAN_POINT('Ctrl Pts',(-20.2430415629541,29.9514229832614,122.540440622386)) ;
#67992 = CARTESIAN_POINT('Ctrl Pts',(-20.6255019413428,30.1414581599979,122.521102011054)) ;
#67993 = CARTESIAN_POINT('Ctrl Pts',(-20.3822574929672,29.961469079635,122.699250490915)) ;
#67994 = CARTESIAN_POINT('Ctrl Pts',(-20.7605632740528,30.151366743995,122.743737177707)) ;
#67995 = CARTESIAN_POINT('Ctrl Pts',(-20.4903053110624,29.9713776636321,122.877358615472)) ;
#67996 = CARTESIAN_POINT('Ctrl Pts',(-20.8563375787038,30.1613773225859,122.988755129718)) ;
#67997 = CARTESIAN_POINT('Ctrl Pts',(-20.5669238525766,29.981388242223,123.073373289288)) ;
#67998 = CARTESIAN_POINT('Ctrl Pts',(-20.9076881587369,30.1714064806987,123.247269528944)) ;
#67999 = CARTESIAN_POINT('Ctrl Pts',(-20.6080032779403,29.9914174003359,123.28018509895)) ;
#68000 = CARTESIAN_POINT('Ctrl Pts',(-20.913643859901,30.1812593625368,123.506108579083)) ;
#68001 = CARTESIAN_POINT('Ctrl Pts',(-20.6127668237937,30.0012702821739,123.4872553494)) ;
#68002 = CARTESIAN_POINT('Ctrl Pts',(-20.8749374874299,30.1912189236878,123.764965708006)) ;
#68003 = CARTESIAN_POINT('Ctrl Pts',(-20.5818009891085,30.0112298433249,123.694340561445)) ;
#68004 = CARTESIAN_POINT('Ctrl Pts',(-20.7907663164554,30.2012573582769,124.014958246547)) ;
#68005 = CARTESIAN_POINT('Ctrl Pts',(-20.5144631445051,30.021268277914,123.89433442643)) ;
#68006 = CARTESIAN_POINT('Ctrl Pts',(-20.6669470046296,30.211130630504,124.243014320118)) ;
#68007 = CARTESIAN_POINT('Ctrl Pts',(-20.4154074251945,30.0311415501411,124.07677811357)) ;
#68008 = CARTESIAN_POINT('Ctrl Pts',(-20.5021342923516,30.2212038724976,124.450093173102)) ;
#68009 = CARTESIAN_POINT('Ctrl Pts',(-20.2835564026306,30.0412147921347,124.242440954527)) ;
#68010 = CARTESIAN_POINT('Ctrl Pts',(-20.3089888716899,30.2310242040306,124.621335698669)) ;
#68011 = CARTESIAN_POINT('Ctrl Pts',(-20.1290405109537,30.0510351236678,124.379433600609)) ;
#68012 = CARTESIAN_POINT('Ctrl Pts',(-20.0834917211719,30.2411028652574,124.760137415769)) ;
#68013 = CARTESIAN_POINT('Ctrl Pts',(-19.9486421144359,30.0611137848945,124.49047459601)) ;
#68014 = CARTESIAN_POINT('Ctrl Pts',(-19.8427824861803,30.2509544605516,124.855609977345)) ;
#68015 = CARTESIAN_POINT('Ctrl Pts',(-19.7560754671688,30.0709653801888,124.566851648864)) ;
#68016 = CARTESIAN_POINT('Ctrl Pts',(-19.5836045391597,30.2610275957804,124.909215904106)) ;
#68017 = CARTESIAN_POINT('Ctrl Pts',(-19.5487326449223,30.0810385154176,124.609735875249)) ;
#68018 = CARTESIAN_POINT('Ctrl Pts',(-19.3250420856673,30.2708700313055,124.916790254833)) ;
#68019 = CARTESIAN_POINT('Ctrl Pts',(-19.3418837978834,30.0908809509426,124.615794714185)) ;
#68020 = CARTESIAN_POINT('Ctrl Pts',(-19.0654078751379,30.2808508004389,124.879699535808)) ;
#68021 = CARTESIAN_POINT('Ctrl Pts',(-19.1341767293187,30.100861720076,124.58612178724)) ;
#68022 = CARTESIAN_POINT('Ctrl Pts',(-18.8153894691253,30.2908679016827,124.797325621791)) ;
#68023 = CARTESIAN_POINT('Ctrl Pts',(-18.9341621618172,30.1108788213199,124.520222166044)) ;
#68024 = CARTESIAN_POINT('Ctrl Pts',(-18.5862012535222,30.3007563492846,124.674812609811)) ;
#68025 = CARTESIAN_POINT('Ctrl Pts',(-18.75081252989,30.1207672689217,124.422211818588)) ;
#68026 = CARTESIAN_POINT('Ctrl Pts',(-18.378326748722,30.3108120634654,124.511700910524)) ;
#68027 = CARTESIAN_POINT('Ctrl Pts',(-18.5845129649496,30.1308229831026,124.29172200353)) ;
#68028 = CARTESIAN_POINT('Ctrl Pts',(-18.2050407985295,30.3206872698793,124.31849941652)) ;
#68029 = CARTESIAN_POINT('Ctrl Pts',(-18.4458851060229,30.1406981895164,124.137161249517)) ;
#68030 = CARTESIAN_POINT('Ctrl Pts',(-18.065746667546,30.330682322352,124.095826539079)) ;
#68031 = CARTESIAN_POINT('Ctrl Pts',(-18.3344500579577,30.1506932419891,123.959022954298)) ;
#68032 = CARTESIAN_POINT('Ctrl Pts',(-17.9673568014916,30.3407042063141,123.851520456621)) ;
#68033 = CARTESIAN_POINT('Ctrl Pts',(-18.2557384543419,30.1607151259512,123.763577933142)) ;
#68034 = CARTESIAN_POINT('Ctrl Pts',(-17.9132391133063,30.3506081788434,123.596944459868)) ;
#68035 = CARTESIAN_POINT('Ctrl Pts',(-18.2124447103049,30.1706190984805,123.559917834642)) ;
#68036 = CARTESIAN_POINT('Ctrl Pts',(-17.9036909635563,30.3605966755043,123.334628818861)) ;
#68037 = CARTESIAN_POINT('Ctrl Pts',(-18.2048063513031,30.1806075951414,123.350065504462)) ;
#68038 = CARTESIAN_POINT('Ctrl Pts',(-17.9399190541115,30.3705604727523,123.075322497842)) ;
#68039 = CARTESIAN_POINT('Ctrl Pts',(-18.2337889737254,30.1905713923894,123.142620833117)) ;
#68040 = CARTESIAN_POINT('Ctrl Pts',(-18.019542401481,30.3804644960603,122.827507706759)) ;
#68041 = CARTESIAN_POINT('Ctrl Pts',(-18.2974874574404,30.2004754156974,122.944369728192)) ;
#68042 = CARTESIAN_POINT('Ctrl Pts',(-18.1430719623568,30.3905249993819,122.593799613876)) ;
#68043 = CARTESIAN_POINT('Ctrl Pts',(-18.3963113223776,30.2105359190191,122.757403048071)) ;
#68044 = CARTESIAN_POINT('Ctrl Pts',(-18.3015384279696,30.4003655345218,122.38939813401)) ;
#68045 = CARTESIAN_POINT('Ctrl Pts',(-18.5230837819883,30.2203764541589,122.593882800201)) ;
#68046 = CARTESIAN_POINT('Ctrl Pts',(-18.4971286724099,30.4104277552264,122.211494771059)) ;
#68047 = CARTESIAN_POINT('Ctrl Pts',(-18.6795561458151,30.2304386748635,122.451559855394)) ;
#68048 = CARTESIAN_POINT('Ctrl Pts',(-18.7171521979687,30.4203249090026,122.072778646605)) ;
#68049 = CARTESIAN_POINT('Ctrl Pts',(-18.8555742859337,30.2403358286398,122.340587380024)) ;
#68050 = CARTESIAN_POINT('Ctrl Pts',(-18.9583979844501,30.4302560423881,121.973238309069)) ;
#68051 = CARTESIAN_POINT('Ctrl Pts',(-19.0485702956595,30.2502669620252,122.260955120397)) ;
#68052 = CARTESIAN_POINT('Ctrl Pts',(-19.216180617271,30.4402984175338,121.916755158295)) ;
#68053 = CARTESIAN_POINT('Ctrl Pts',(-19.2547965323524,30.260309337171,122.215768415683)) ;
#68054 = CARTESIAN_POINT('Ctrl Pts',(-19.4757597411927,30.4501843553,121.905857590778)) ;
#68055 = CARTESIAN_POINT('Ctrl Pts',(-19.4624589536106,30.2701952749371,122.207050197027)) ;
#68056 = CARTESIAN_POINT('Ctrl Pts',(-19.7361687240311,30.4601801982848,121.940170527014)) ;
#68057 = CARTESIAN_POINT('Ctrl Pts',(-19.6707860227431,30.2801911179219,122.234500220989)) ;
#68058 = CARTESIAN_POINT('Ctrl Pts',(-19.9853388632678,30.4701221761634,122.018791502423)) ;
#68059 = CARTESIAN_POINT('Ctrl Pts',(-19.8701217511132,30.2901330958005,122.297396567724)) ;
#68060 = CARTESIAN_POINT('Ctrl Pts',(-20.2176167858868,30.4800815506444,122.139363771227)) ;
#68061 = CARTESIAN_POINT('Ctrl Pts',(-20.0559439306465,30.3000924702815,122.393853866718)) ;
#68062 = CARTESIAN_POINT('Ctrl Pts',(-20.4263236161457,30.4900781664782,122.298948878856)) ;
#68063 = CARTESIAN_POINT('Ctrl Pts',(-20.2229095545966,30.3100890861153,122.521521545282)) ;
#68064 = CARTESIAN_POINT('Ctrl Pts',(-20.6045380695498,30.5001123850517,122.493286837832)) ;
#68065 = CARTESIAN_POINT('Ctrl Pts',(-20.3654814345688,30.3201233046888,122.676991771903)) ;
#68066 = CARTESIAN_POINT('Ctrl Pts',(-20.7440103711108,30.5099654522623,122.711437778196)) ;
#68067 = CARTESIAN_POINT('Ctrl Pts',(-20.477059029593,30.3299763718994,122.851511380086)) ;
#68068 = CARTESIAN_POINT('Ctrl Pts',(-20.8452704862501,30.5199257101399,122.952793072304)) ;
#68069 = CARTESIAN_POINT('Ctrl Pts',(-20.5580675344423,30.339936629777,123.044595041422)) ;
#68070 = CARTESIAN_POINT('Ctrl Pts',(-20.9031858777252,30.5299547368455,123.209917654151)) ;
#68071 = CARTESIAN_POINT('Ctrl Pts',(-20.604400374506,30.3499656564826,123.250294668849)) ;
#68072 = CARTESIAN_POINT('Ctrl Pts',(-20.9155052003231,30.5398649438799,123.470044892547)) ;
#68073 = CARTESIAN_POINT('Ctrl Pts',(-20.6142563408965,30.3598758635171,123.458395733584)) ;
#68074 = CARTESIAN_POINT('Ctrl Pts',(-20.8830672767706,30.5497998545275,123.729108750999)) ;
#68075 = CARTESIAN_POINT('Ctrl Pts',(-20.5883067737471,30.3698107741647,123.665646384641)) ;
#68076 = CARTESIAN_POINT('Ctrl Pts',(-20.8050869196827,30.5598409847068,123.981184304442)) ;
#68077 = CARTESIAN_POINT('Ctrl Pts',(-20.5259230651749,30.3798519043439,123.867307162557)) ;
#68078 = CARTESIAN_POINT('Ctrl Pts',(-20.6865234424483,30.5697281250767,124.212396007676)) ;
#68079 = CARTESIAN_POINT('Ctrl Pts',(-20.4310732809217,30.3897390447139,124.052276102492)) ;
#68080 = CARTESIAN_POINT('Ctrl Pts',(-20.5283158328247,30.5797204026127,124.421949250781)) ;
#68081 = CARTESIAN_POINT('Ctrl Pts',(-20.3045079305415,30.3997313222498,124.219919049695)) ;
#68082 = CARTESIAN_POINT('Ctrl Pts',(-20.336893127493,30.589668945881,124.600034325977)) ;
#68083 = CARTESIAN_POINT('Ctrl Pts',(-20.1513706158548,30.4096798655181,124.362387386942)) ;
#68084 = CARTESIAN_POINT('Ctrl Pts',(-20.117949669728,30.5996056206982,124.742302120517)) ;
#68085 = CARTESIAN_POINT('Ctrl Pts',(-19.9762167528585,30.4196165403353,124.476202075347)) ;
#68086 = CARTESIAN_POINT('Ctrl Pts',(-19.8765801266705,30.6095890416346,124.845182022236)) ;
#68087 = CARTESIAN_POINT('Ctrl Pts',(-19.7831216739518,30.4295999612717,124.558506786004)) ;
#68088 = CARTESIAN_POINT('Ctrl Pts',(-19.619448424608,30.6196313568238,124.904513792509)) ;
#68089 = CARTESIAN_POINT('Ctrl Pts',(-19.577416370328,30.4396422764609,124.605973056573)) ;
#68090 = CARTESIAN_POINT('Ctrl Pts',(-19.3612267210301,30.629471674263,124.918439915204)) ;
#68091 = CARTESIAN_POINT('Ctrl Pts',(-19.3708401454886,30.4494825939001,124.617114839488)) ;
#68092 = CARTESIAN_POINT('Ctrl Pts',(-19.0994956244019,30.6395013783205,124.887333257162)) ;
#68093 = CARTESIAN_POINT('Ctrl Pts',(-19.1614550554373,30.4595122979576,124.592230579924)) ;
#68094 = CARTESIAN_POINT('Ctrl Pts',(-18.84757050077,30.649522335043,124.810642476183)) ;
#68095 = CARTESIAN_POINT('Ctrl Pts',(-18.9599146662731,30.4695332546801,124.530878830767)) ;
#68096 = CARTESIAN_POINT('Ctrl Pts',(-18.6160882477537,30.6593888773466,124.69379526334)) ;
#68097 = CARTESIAN_POINT('Ctrl Pts',(-18.7747291880007,30.4793997969837,124.437402426566)) ;
#68098 = CARTESIAN_POINT('Ctrl Pts',(-18.4041389450964,30.6694599772918,124.535339469786)) ;
#68099 = CARTESIAN_POINT('Ctrl Pts',(-18.6051688617141,30.4894708969289,124.310638472156)) ;
#68100 = CARTESIAN_POINT('Ctrl Pts',(-18.2270241518516,30.6793020514693,124.346845255088)) ;
#68101 = CARTESIAN_POINT('Ctrl Pts',(-18.4634769547701,30.4993129711065,124.159844592022)) ;
#68102 = CARTESIAN_POINT('Ctrl Pts',(-18.0828214570917,30.6892628460564,124.128395071014)) ;
#68103 = CARTESIAN_POINT('Ctrl Pts',(-18.3481139027231,30.5092737656935,123.98508542601)) ;
#68104 = CARTESIAN_POINT('Ctrl Pts',(-17.9784145006715,30.6993007189572,123.886162207482)) ;
#68105 = CARTESIAN_POINT('Ctrl Pts',(-18.2645872182837,30.5193116385943,123.791299501671)) ;
#68106 = CARTESIAN_POINT('Ctrl Pts',(-17.9181661940265,30.7091750045013,123.63373426702)) ;
#68107 = CARTESIAN_POINT('Ctrl Pts',(-18.216387518212,30.5291859241384,123.589358233217)) ;
#68108 = CARTESIAN_POINT('Ctrl Pts',(-17.9023753757216,30.7192447549152,123.369619175597)) ;
#68109 = CARTESIAN_POINT('Ctrl Pts',(-18.203753574066,30.5392556745523,123.378065957705)) ;
#68110 = CARTESIAN_POINT('Ctrl Pts',(-17.9318397718058,30.7290780394499,123.112874144442)) ;
#68111 = CARTESIAN_POINT('Ctrl Pts',(-18.2273236794525,30.549088959087,123.172670800708)) ;
#68112 = CARTESIAN_POINT('Ctrl Pts',(-18.0061852690051,30.7391083802499,122.859997359419)) ;
#68113 = CARTESIAN_POINT('Ctrl Pts',(-18.2867986965905,30.559119299887,122.970368894539)) ;
#68114 = CARTESIAN_POINT('Ctrl Pts',(-18.1240293775023,30.7491403042495,122.624160309324)) ;
#68115 = CARTESIAN_POINT('Ctrl Pts',(-18.381072852259,30.5691512238866,122.781698614195)) ;
#68116 = CARTESIAN_POINT('Ctrl Pts',(-18.2773844645063,30.7589688391854,122.416346355351)) ;
#68117 = CARTESIAN_POINT('Ctrl Pts',(-18.5037551769327,30.5789797588226,122.615447430621)) ;
#68118 = CARTESIAN_POINT('Ctrl Pts',(-18.4671493140597,30.7689626169501,122.234795344671)) ;
#68119 = CARTESIAN_POINT('Ctrl Pts',(-18.6555658924433,30.5889735365872,122.470205578814)) ;
#68120 = CARTESIAN_POINT('Ctrl Pts',(-18.6865926220814,30.7789903274356,122.088882738916)) ;
#68121 = CARTESIAN_POINT('Ctrl Pts',(-18.8311197585545,30.5990012470728,122.353474263841)) ;
#68122 = CARTESIAN_POINT('Ctrl Pts',(-18.924548918543,30.7888787382696,121.984461740876)) ;
#68123 = CARTESIAN_POINT('Ctrl Pts',(-19.0214835756871,30.6088896579067,122.269936340011)) ;
#68124 = CARTESIAN_POINT('Ctrl Pts',(-19.1791493957345,30.7988555888051,121.921954029357)) ;
#68125 = CARTESIAN_POINT('Ctrl Pts',(-19.2251633755617,30.6188665084423,122.219928660186)) ;
#68126 = CARTESIAN_POINT('Ctrl Pts',(-19.4411836962534,30.8088473853556,121.904551040875)) ;
#68127 = CARTESIAN_POINT('Ctrl Pts',(-19.4347905867356,30.6288583049927,122.206004671625)) ;
#68128 = CARTESIAN_POINT('Ctrl Pts',(-19.7033209422536,30.8188833914493,121.933349289194)) ;
#68129 = CARTESIAN_POINT('Ctrl Pts',(-19.6445006241245,30.6388943110864,122.229041739031)) ;
#68130 = CARTESIAN_POINT('Ctrl Pts',(-19.9519531581678,30.8287341257121,122.005489324719)) ;
#68131 = CARTESIAN_POINT('Ctrl Pts',(-19.84340606214,30.6487450453492,122.286751981054)) ;
#68132 = CARTESIAN_POINT('Ctrl Pts',(-20.1877451626918,30.8387253842403,122.12090221111)) ;
#68133 = CARTESIAN_POINT('Ctrl Pts',(-20.0320402961377,30.6587363038774,122.379080697725)) ;
#68134 = CARTESIAN_POINT('Ctrl Pts',(-20.3985067246429,30.8486432791435,122.274284311981)) ;
#68135 = CARTESIAN_POINT('Ctrl Pts',(-20.2006501933195,30.6686541987806,122.50178471108)) ;
#68136 = CARTESIAN_POINT('Ctrl Pts',(-20.5814557895788,30.8586714208065,122.463931047394)) ;
#68137 = CARTESIAN_POINT('Ctrl Pts',(-20.3470107187746,30.6786823404437,122.653500909386)) ;
#68138 = CARTESIAN_POINT('Ctrl Pts',(-20.726703975958,30.8685565889224,122.679309656422)) ;
#68139 = CARTESIAN_POINT('Ctrl Pts',(-20.4632103980333,30.6885675085595,122.82580232508)) ;
#68140 = CARTESIAN_POINT('Ctrl Pts',(-20.8340446604117,30.8785459524284,122.918876333056)) ;
#68141 = CARTESIAN_POINT('Ctrl Pts',(-20.5490845941834,30.6985568720655,123.017454790216)) ;
#68142 = CARTESIAN_POINT('Ctrl Pts',(-20.8979488651774,30.8885870874385,123.174891648262)) ;
#68143 = CARTESIAN_POINT('Ctrl Pts',(-20.6002096966955,30.7085980070756,123.222266683441)) ;
#68144 = CARTESIAN_POINT('Ctrl Pts',(-20.916470523059,30.8984197556265,123.432614768819)) ;
#68145 = CARTESIAN_POINT('Ctrl Pts',(-20.6150288055355,30.7184306752636,123.42844428619)) ;
#68146 = CARTESIAN_POINT('Ctrl Pts',(-20.8902751541959,30.908413658581,123.693933046635)) ;
#68147 = CARTESIAN_POINT('Ctrl Pts',(-20.5940744640968,30.7284245782181,123.637499006698)) ;
#68148 = CARTESIAN_POINT('Ctrl Pts',(-20.8183135578191,30.9184429436655,123.947479863912)) ;
#68149 = CARTESIAN_POINT('Ctrl Pts',(-20.5365069824791,30.7384538633026,123.840336987593)) ;
#68150 = CARTESIAN_POINT('Ctrl Pts',(-20.705558307434,30.9283184721074,124.181239071671)) ;
#68151 = CARTESIAN_POINT('Ctrl Pts',(-20.4463047552757,30.7483293917445,124.027344708354)) ;
#68152 = CARTESIAN_POINT('Ctrl Pts',(-20.55227636311,30.9383187547235,124.394663488926)) ;
#68153 = CARTESIAN_POINT('Ctrl Pts',(-20.3236808563954,30.7583296743606,124.198085320578)) ;
#68154 = CARTESIAN_POINT('Ctrl Pts',(-20.3660263502005,30.9482307707805,124.576805636963)) ;
#68155 = CARTESIAN_POINT('Ctrl Pts',(-20.1746825091219,30.7682416904176,124.343800207381)) ;
#68156 = CARTESIAN_POINT('Ctrl Pts',(-20.148238159027,30.9582728461195,124.725798531691)) ;
#68157 = CARTESIAN_POINT('Ctrl Pts',(-20.0004530415488,30.7782837657566,124.462996211481)) ;
#68158 = CARTESIAN_POINT('Ctrl Pts',(-19.9112599341149,30.9681726787756,124.833177229003)) ;
#68159 = CARTESIAN_POINT('Ctrl Pts',(-19.8108716507074,30.7881835984127,124.548900832387)) ;
#68160 = CARTESIAN_POINT('Ctrl Pts',(-19.6570385216495,30.9781650793536,124.898943043692)) ;
#68161 = CARTESIAN_POINT('Ctrl Pts',(-19.6074951324964,30.7981759989908,124.601515467701)) ;
#68162 = CARTESIAN_POINT('Ctrl Pts',(-19.3941289164041,30.988199101113,124.91918719167)) ;
#68163 = CARTESIAN_POINT('Ctrl Pts',(-19.3971675920454,30.8082100207501,124.617712800097)) ;
#68164 = CARTESIAN_POINT('Ctrl Pts',(-19.1361050769742,30.9980637119542,124.894240456014)) ;
#68165 = CARTESIAN_POINT('Ctrl Pts',(-19.1907487911247,30.8180746315913,124.597757506025)) ;
#68166 = CARTESIAN_POINT('Ctrl Pts',(-18.8829168166101,31.0080561114154,124.824588928341)) ;
#68167 = CARTESIAN_POINT('Ctrl Pts',(-18.9881977022827,30.8280670310525,124.542038356411)) ;
#68168 = CARTESIAN_POINT('Ctrl Pts',(-18.6449556256928,31.0180880647483,124.711122383822)) ;
#68169 = CARTESIAN_POINT('Ctrl Pts',(-18.7978278575721,30.8380989843854,124.451266991065)) ;
#68170 = CARTESIAN_POINT('Ctrl Pts',(-18.433613598993,31.0279544236899,124.56090527812)) ;
#68171 = CARTESIAN_POINT('Ctrl Pts',(-18.6287533485745,30.8479653433271,124.331095266806)) ;
#68172 = CARTESIAN_POINT('Ctrl Pts',(-18.2490556295149,31.0379418991757,124.374338785496)) ;
#68173 = CARTESIAN_POINT('Ctrl Pts',(-18.4811055111565,30.8579528188129,124.181843656717)) ;
#68174 = CARTESIAN_POINT('Ctrl Pts',(-18.1001763827017,31.0478868053642,124.159502137119)) ;
#68175 = CARTESIAN_POINT('Ctrl Pts',(-18.3620004446378,30.8678977250013,124.009975722139)) ;
#68176 = CARTESIAN_POINT('Ctrl Pts',(-17.9899251037199,31.0579317700244,123.919685682728)) ;
#68177 = CARTESIAN_POINT('Ctrl Pts',(-18.2737974607781,30.8779426896616,123.818123443375)) ;
#68178 = CARTESIAN_POINT('Ctrl Pts',(-17.9239698947395,31.0677935769293,123.669038395262)) ;
#68179 = CARTESIAN_POINT('Ctrl Pts',(-18.221031284142,30.8878044965664,123.617606494588)) ;
#68180 = CARTESIAN_POINT('Ctrl Pts',(-17.9017545884407,31.0777862492351,123.407409964502)) ;
#68181 = CARTESIAN_POINT('Ctrl Pts',(-18.2032568478911,30.8977971688722,123.408304011957)) ;
#68182 = CARTESIAN_POINT('Ctrl Pts',(-17.9251878868137,31.0877149201804,123.147532162219)) ;
#68183 = CARTESIAN_POINT('Ctrl Pts',(-18.2220012797528,30.9077258398175,123.200401751263)) ;
#68184 = CARTESIAN_POINT('Ctrl Pts',(-17.9931295756622,31.0976674624057,122.894987346514)) ;
#68185 = CARTESIAN_POINT('Ctrl Pts',(-18.2763524482962,30.9176783820428,122.998365442682)) ;
#68186 = CARTESIAN_POINT('Ctrl Pts',(-18.1043255909368,31.1076688184016,122.656813330348)) ;
#68187 = CARTESIAN_POINT('Ctrl Pts',(-18.3653072153254,30.9276797380387,122.807825340817)) ;
#68188 = CARTESIAN_POINT('Ctrl Pts',(-18.2558710625769,31.1176974306763,122.441217023634)) ;
#68189 = CARTESIAN_POINT('Ctrl Pts',(-18.486541760213,30.9377083503134,122.63534705266)) ;
#68190 = CARTESIAN_POINT('Ctrl Pts',(-18.4392436560099,31.1275617652258,122.257966085798)) ;
#68191 = CARTESIAN_POINT('Ctrl Pts',(-18.6332381127442,30.9475726848629,122.488744871235)) ;
#68192 = CARTESIAN_POINT('Ctrl Pts',(-18.6541277020736,31.1375540893024,122.107106052772)) ;
#68193 = CARTESIAN_POINT('Ctrl Pts',(-18.805144006808,30.9575650089395,122.368055041523)) ;
#68194 = CARTESIAN_POINT('Ctrl Pts',(-18.8903979931826,31.1474815816683,121.99639777191)) ;
#68195 = CARTESIAN_POINT('Ctrl Pts',(-18.9941591920697,30.9674925013054,122.279486427225)) ;
#68196 = CARTESIAN_POINT('Ctrl Pts',(-19.1447705223875,31.1575089402191,121.927739862365)) ;
#68197 = CARTESIAN_POINT('Ctrl Pts',(-19.1976565800842,30.9775198598562,122.224557940461)) ;
#68198 = CARTESIAN_POINT('Ctrl Pts',(-19.403557785468,31.1673953582702,121.904339822956)) ;
#68199 = CARTESIAN_POINT('Ctrl Pts',(-19.40468609459,30.9874062779074,122.205835676203)) ;
#68200 = CARTESIAN_POINT('Ctrl Pts',(-19.6662117593913,31.1774270930056,121.926411212978)) ;
#68201 = CARTESIAN_POINT('Ctrl Pts',(-19.6148094082564,30.9974380126427,122.223490535075)) ;
#68202 = CARTESIAN_POINT('Ctrl Pts',(-19.9173816828502,31.1873086742489,121.992520931665)) ;
#68203 = CARTESIAN_POINT('Ctrl Pts',(-19.815745871323,31.007319593886,122.276376119868)) ;
#68204 = CARTESIAN_POINT('Ctrl Pts',(-20.1575099536661,31.1973706522812,122.103127502672)) ;
#68205 = CARTESIAN_POINT('Ctrl Pts',(-20.0078493692217,31.0173815719183,122.364859298836)) ;
#68206 = CARTESIAN_POINT('Ctrl Pts',(-20.3704779128565,31.2072277306429,122.250647114545)) ;
#68207 = CARTESIAN_POINT('Ctrl Pts',(-20.1782250129861,31.02723865028,122.482873132973)) ;
#68208 = CARTESIAN_POINT('Ctrl Pts',(-20.557479635411,31.2172223037489,122.435014859895)) ;
#68209 = CARTESIAN_POINT('Ctrl Pts',(-20.3278279402508,31.037233223386,122.630365704853)) ;
#68210 = CARTESIAN_POINT('Ctrl Pts',(-20.7087042530508,31.2271481000365,122.647587798087)) ;
#68211 = CARTESIAN_POINT('Ctrl Pts',(-20.4488094657624,31.0471590196736,122.8004227559)) ;
#68212 = CARTESIAN_POINT('Ctrl Pts',(-20.8218837391766,31.2371734672062,122.885470873075)) ;
#68213 = CARTESIAN_POINT('Ctrl Pts',(-20.539355037212,31.0571843868434,122.99072823021)) ;
#68214 = CARTESIAN_POINT('Ctrl Pts',(-20.8912500206041,31.2470695468601,123.136118325641)) ;
#68215 = CARTESIAN_POINT('Ctrl Pts',(-20.594850255258,31.0670804664972,123.191245492355)) ;
#68216 = CARTESIAN_POINT('Ctrl Pts',(-20.916817797818,31.2570646265657,123.397534145115)) ;
#68217 = CARTESIAN_POINT('Ctrl Pts',(-20.6153065879517,31.0770755462028,123.400378543151)) ;
#68218 = CARTESIAN_POINT('Ctrl Pts',(-20.8960973227342,31.2670897143815,123.660166672547)) ;
#68219 = CARTESIAN_POINT('Ctrl Pts',(-20.5987327498281,31.0871006340186,123.610482259063)) ;
#68220 = CARTESIAN_POINT('Ctrl Pts',(-20.809893476644,31.2802735367488,123.995726533553)) ;
#68221 = CARTESIAN_POINT('Ctrl Pts',(-20.5297709305419,31.1002844563859,123.87894293253)) ;
#68222 = CARTESIAN_POINT('Ctrl Pts',(-20.6369390480152,31.2935956548947,124.30466223955)) ;
#68223 = CARTESIAN_POINT('Ctrl Pts',(-20.3913865526123,31.1136065745318,124.126114241275)) ;
#68224 = CARTESIAN_POINT('Ctrl Pts',(-20.3908148582284,31.3069748645223,124.555818133117)) ;
#68225 = CARTESIAN_POINT('Ctrl Pts',(-20.1945187656795,31.1269857841594,124.327003669048)) ;
#68226 = CARTESIAN_POINT('Ctrl Pts',(-20.1809438414753,31.3168131017665,124.706820601801)) ;
#68227 = CARTESIAN_POINT('Ctrl Pts',(-20.0266169655379,31.1368240214036,124.447815030813)) ;
#68228 = CARTESIAN_POINT('Ctrl Pts',(-19.9425721439745,31.3268860250252,124.821852782534)) ;
#68229 = CARTESIAN_POINT('Ctrl Pts',(-19.8359226633174,31.1468969446624,124.539840740485)) ;
#68230 = CARTESIAN_POINT('Ctrl Pts',(-19.6932575438715,31.3367426664803,124.89218888602)) ;
#68231 = CARTESIAN_POINT('Ctrl Pts',(-19.6364695236485,31.1567535861175,124.596111832383)) ;
#68232 = CARTESIAN_POINT('Ctrl Pts',(-19.4322556852193,31.3467280419864,124.919201640466)) ;
#68233 = CARTESIAN_POINT('Ctrl Pts',(-19.4276731793723,31.1667389616235,124.617725775355)) ;
#68234 = CARTESIAN_POINT('Ctrl Pts',(-19.0841345592013,31.3600120734468,124.893999424143)) ;
#68235 = CARTESIAN_POINT('Ctrl Pts',(-19.1491518620383,31.180022993084,124.597557799836)) ;
#68236 = CARTESIAN_POINT('Ctrl Pts',(-18.6686831095259,31.3765308653172,124.751522351196)) ;
#68237 = CARTESIAN_POINT('Ctrl Pts',(-18.8168267270378,31.1965417849543,124.483599784169)) ;
#68238 = CARTESIAN_POINT('Ctrl Pts',(-18.3221176258635,31.3933165823238,124.470780414967)) ;
#68239 = CARTESIAN_POINT('Ctrl Pts',(-18.5395236640967,31.2133275019609,124.258964588696)) ;
#68240 = CARTESIAN_POINT('Ctrl Pts',(-18.1195171640873,31.4064297308328,124.19192546978)) ;
#68241 = CARTESIAN_POINT('Ctrl Pts',(-18.3774781924197,31.2264406504699,124.035919165873)) ;
#68242 = CARTESIAN_POINT('Ctrl Pts',(-18.0029767278721,31.416465279913,123.955390640417)) ;
#68243 = CARTESIAN_POINT('Ctrl Pts',(-18.2842367998029,31.2364761995501,123.846683979849)) ;
#68244 = CARTESIAN_POINT('Ctrl Pts',(-17.930131161295,31.4264813360924,123.702427282653)) ;
#68245 = CARTESIAN_POINT('Ctrl Pts',(-18.2259601153952,31.2464922557295,123.644318871564)) ;
#68246 = CARTESIAN_POINT('Ctrl Pts',(-17.8927981854828,31.4396593719584,123.358188928687)) ;
#68247 = CARTESIAN_POINT('Ctrl Pts',(-18.1960923899022,31.2596702915955,123.368912638922)) ;
#68248 = CARTESIAN_POINT('Ctrl Pts',(-17.9589427761027,31.4562612491455,122.921846253614)) ;
#68249 = CARTESIAN_POINT('Ctrl Pts',(-18.2490034305915,31.2762721687826,123.019854359994)) ;
#68250 = CARTESIAN_POINT('Ctrl Pts',(-18.2153452936868,31.4763243937614,122.454312103361)) ;
#68251 = CARTESIAN_POINT('Ctrl Pts',(-18.4541225899952,31.2963353133985,122.645820297505)) ;
#68252 = CARTESIAN_POINT('Ctrl Pts',(-18.6105119795525,31.4961252838451,122.106643007625)) ;
#68253 = CARTESIAN_POINT('Ctrl Pts',(-18.7702543020853,31.3161362034822,122.36768303858)) ;
#68254 = CARTESIAN_POINT('Ctrl Pts',(-19.1034924936999,31.5160684091238,121.912133008607)) ;
#68255 = CARTESIAN_POINT('Ctrl Pts',(-19.164637971874,31.3360793287609,122.212071605184)) ;
#68256 = CARTESIAN_POINT('Ctrl Pts',(-19.6321465341764,31.5359664542434,121.89791137193)) ;
#68257 = CARTESIAN_POINT('Ctrl Pts',(-19.5875618065476,31.3559773738805,122.200691277358)) ;
#68258 = CARTESIAN_POINT('Ctrl Pts',(-20.1341066883384,31.5558522138702,122.063616102464)) ;
#68259 = CARTESIAN_POINT('Ctrl Pts',(-19.9891315918773,31.3758631335073,122.333252851735)) ;
#68260 = CARTESIAN_POINT('Ctrl Pts',(-20.5525283110554,31.57591738905,122.394200252169)) ;
#68261 = CARTESIAN_POINT('Ctrl Pts',(-20.3238701259959,31.3959283086872,122.597717694145)) ;
#68262 = CARTESIAN_POINT('Ctrl Pts',(-20.8296000415882,31.5957440321528,122.84254361497)) ;
#68263 = CARTESIAN_POINT('Ctrl Pts',(-20.5455305086285,31.41575495179,122.95639217086)) ;
#68264 = CARTESIAN_POINT('Ctrl Pts',(-20.9388687495492,31.6156527416012,123.360136077141)) ;
#68265 = CARTESIAN_POINT('Ctrl Pts',(-20.6329476561718,31.4356636612383,123.370466593898)) ;
#68266 = CARTESIAN_POINT('Ctrl Pts',(-20.8648791195812,31.635604578633,123.885385533411)) ;
#68267 = CARTESIAN_POINT('Ctrl Pts',(-20.573757693884,31.4556154982701,123.790666808917)) ;
#68268 = CARTESIAN_POINT('Ctrl Pts',(-20.6147262487971,31.6556130533361,124.354604940983)) ;
#68269 = CARTESIAN_POINT('Ctrl Pts',(-20.3736372170781,31.4756239729733,124.166043186308)) ;
#68270 = CARTESIAN_POINT('Ctrl Pts',(-20.2239265792252,31.6754145120976,124.70712499995)) ;
#68271 = CARTESIAN_POINT('Ctrl Pts',(-20.0609969972757,31.4954254317348,124.448061814946)) ;
#68272 = CARTESIAN_POINT('Ctrl Pts',(-19.7329944592127,31.6953714003336,124.907950846951)) ;
#68273 = CARTESIAN_POINT('Ctrl Pts',(-19.6682511534378,31.5153823199707,124.608723469387)) ;
#68274 = CARTESIAN_POINT('Ctrl Pts',(-19.2022559885623,31.7153552377477,124.928017723692)) ;
#68275 = CARTESIAN_POINT('Ctrl Pts',(-19.2436602612597,31.5353661573848,124.624778160052)) ;
#68276 = CARTESIAN_POINT('Ctrl Pts',(-18.7005580952729,31.7351636769686,124.768181953029)) ;
#68277 = CARTESIAN_POINT('Ctrl Pts',(-18.8422995577168,31.5551745966057,124.496909315192)) ;
#68278 = CARTESIAN_POINT('Ctrl Pts',(-18.2796327533169,31.7551493863488,124.444432947283)) ;
#68279 = CARTESIAN_POINT('Ctrl Pts',(-18.505559042595,31.5751603059859,124.237909991823)) ;
#68280 = CARTESIAN_POINT('Ctrl Pts',(-17.9957625956122,31.7750189093641,123.998861683797)) ;
#68281 = CARTESIAN_POINT('Ctrl Pts',(-18.2784622930544,31.5950298290012,123.881451524151)) ;
#68282 = CARTESIAN_POINT('Ctrl Pts',(-17.8804111930879,31.7950396484813,123.479601508631)) ;
#68283 = CARTESIAN_POINT('Ctrl Pts',(-18.1861815644187,31.6150505681184,123.466043484708)) ;
#68284 = CARTESIAN_POINT('Ctrl Pts',(-17.947813732566,31.8148437134583,122.957375358431)) ;
#68285 = CARTESIAN_POINT('Ctrl Pts',(-18.240104726759,31.6348546330954,123.048260409413)) ;
#68286 = CARTESIAN_POINT('Ctrl Pts',(-18.1922019497661,31.834905677189,122.483631625261)) ;
#68287 = CARTESIAN_POINT('Ctrl Pts',(-18.4356159960294,31.6549165968261,122.669266566499)) ;
#68288 = CARTESIAN_POINT('Ctrl Pts',(-18.579670503548,31.8547388574775,122.126047237428)) ;
#68289 = CARTESIAN_POINT('Ctrl Pts',(-18.7455928985157,31.6747497771146,122.383198612062)) ;
#68290 = CARTESIAN_POINT('Ctrl Pts',(-19.0672415407129,31.8746580548036,121.919977102834)) ;
#68291 = CARTESIAN_POINT('Ctrl Pts',(-19.1356512341748,31.6946689744407,122.218343904972)) ;
#68292 = CARTESIAN_POINT('Ctrl Pts',(-19.596473798273,31.8945960799169,121.892968380712)) ;
#68293 = CARTESIAN_POINT('Ctrl Pts',(-19.559037724007,31.714606999554,122.196738778409)) ;
#68294 = CARTESIAN_POINT('Ctrl Pts',(-20.1018977424829,31.914474125973,122.047010861552)) ;
#68295 = CARTESIAN_POINT('Ctrl Pts',(-19.9633772292207,31.7344850456101,122.319975266152)) ;
#68296 = CARTESIAN_POINT('Ctrl Pts',(-20.5266155989396,31.934458860261,122.365876034326)) ;
#68297 = CARTESIAN_POINT('Ctrl Pts',(-20.3031501256687,31.7544697798982,122.575069435507)) ;
#68298 = CARTESIAN_POINT('Ctrl Pts',(-20.8161540516341,31.9543696769395,122.809022005469)) ;
#68299 = CARTESIAN_POINT('Ctrl Pts',(-20.5347790794781,31.7743805965766,122.92958819007)) ;
#68300 = CARTESIAN_POINT('Ctrl Pts',(-20.9372264313366,31.9743686524582,123.326459903439)) ;
#68301 = CARTESIAN_POINT('Ctrl Pts',(-20.6316344224308,31.7943795720954,123.343539156427)) ;
#68302 = CARTESIAN_POINT('Ctrl Pts',(-20.8757007542274,31.9941735731034,123.849340834267)) ;
#68303 = CARTESIAN_POINT('Ctrl Pts',(-20.5824107852335,31.8141844927406,123.761844941543)) ;
#68304 = CARTESIAN_POINT('Ctrl Pts',(-20.6381061492539,32.0141575333947,124.324236585198)) ;
#68305 = CARTESIAN_POINT('Ctrl Pts',(-20.3923321320177,31.8341684530318,124.141760152678)) ;
#68306 = CARTESIAN_POINT('Ctrl Pts',(-20.254277484515,32.0340437371186,124.687750970673)) ;
#68307 = CARTESIAN_POINT('Ctrl Pts',(-20.085266409861,31.8540546567557,124.432569686706)) ;
#68308 = CARTESIAN_POINT('Ctrl Pts',(-19.7682819396191,32.0539929154418,124.89962239012)) ;
#68309 = CARTESIAN_POINT('Ctrl Pts',(-19.696468384716,31.8740038350789,124.60206379762)) ;
#68310 = CARTESIAN_POINT('Ctrl Pts',(-19.2403770539516,32.0738947146813,124.932732853793)) ;
#68311 = CARTESIAN_POINT('Ctrl Pts',(-19.2741434998259,31.8939056343185,124.628548078608)) ;
#68312 = CARTESIAN_POINT('Ctrl Pts',(-18.7330993587673,32.0937733197337,124.784941725984)) ;
#68313 = CARTESIAN_POINT('Ctrl Pts',(-18.868322906955,31.9137842393708,124.510313181707)) ;
#68314 = CARTESIAN_POINT('Ctrl Pts',(-18.3035498467669,32.1138056794594,124.470304693559)) ;
#68315 = CARTESIAN_POINT('Ctrl Pts',(-18.5246822315973,31.9338165990965,124.258593399843)) ;
#68316 = CARTESIAN_POINT('Ctrl Pts',(-18.0587930611329,32.1303874054155,124.103782576889)) ;
#68317 = CARTESIAN_POINT('Ctrl Pts',(-18.3288903810443,31.9503983250526,123.965395758089)) ;
#68318 = CARTESIAN_POINT('Ctrl Pts',(-17.9464384610694,32.1435815757134,123.775785395635)) ;
#68319 = CARTESIAN_POINT('Ctrl Pts',(-18.2389994529127,31.9635924953505,123.702969740174)) ;
#68320 = CARTESIAN_POINT('Ctrl Pts',(-17.8916962164165,32.1568937538066,123.430264324837)) ;
#68321 = CARTESIAN_POINT('Ctrl Pts',(-18.1952099799321,31.9769046734437,123.426608864667)) ;
#68322 = CARTESIAN_POINT('Ctrl Pts',(-17.9374894753685,32.1734599333999,122.99232521224)) ;
#68323 = CARTESIAN_POINT('Ctrl Pts',(-18.2318514252023,31.9934708530371,123.076188915836)) ;
#68324 = CARTESIAN_POINT('Ctrl Pts',(-18.1302718088824,32.1900881282601,122.594703559392)) ;
#68325 = CARTESIAN_POINT('Ctrl Pts',(-18.3860665483606,32.0100990478972,122.758138239794)) ;
#68326 = CARTESIAN_POINT('Ctrl Pts',(-18.3588141057148,32.2033767099699,122.330591540781)) ;
#68327 = CARTESIAN_POINT('Ctrl Pts',(-18.5689151874287,32.023387629607,122.546823962737)) ;
#68328 = CARTESIAN_POINT('Ctrl Pts',(-18.5618539277949,32.2133449580735,122.165112713871)) ;
#68329 = CARTESIAN_POINT('Ctrl Pts',(-18.7313457221629,32.0333558777106,122.414447852175)) ;
#68330 = CARTESIAN_POINT('Ctrl Pts',(-18.7891790717996,32.2232597143296,122.037790376024)) ;
#68331 = CARTESIAN_POINT('Ctrl Pts',(-18.9132084602232,32.0432706339667,122.312590559703)) ;
#68332 = CARTESIAN_POINT('Ctrl Pts',(-19.037513591275,32.2332728649808,121.95074327932)) ;
#68333 = CARTESIAN_POINT('Ctrl Pts',(-19.1118736703297,32.0532837846179,122.242954838167)) ;
#68334 = CARTESIAN_POINT('Ctrl Pts',(-19.2972230251791,32.2432855721828,121.908553873528)) ;
#68335 = CARTESIAN_POINT('Ctrl Pts',(-19.3196523089538,32.0632964918199,122.209207408094)) ;
#68336 = CARTESIAN_POINT('Ctrl Pts',(-19.6446403660395,32.2565048608741,121.9125795524)) ;
#68337 = CARTESIAN_POINT('Ctrl Pts',(-19.5975327596128,32.0765157805112,122.212420869537)) ;
#68338 = CARTESIAN_POINT('Ctrl Pts',(-20.0699198327109,32.2731235418722,122.031411460383)) ;
#68339 = CARTESIAN_POINT('Ctrl Pts',(-19.937823277613,32.0931344615093,122.307507212326)) ;
#68340 = CARTESIAN_POINT('Ctrl Pts',(-20.4284615240151,32.2896884496456,122.28707638829)) ;
#68341 = CARTESIAN_POINT('Ctrl Pts',(-20.224607600475,32.1096993692827,122.512015776509)) ;
#68342 = CARTESIAN_POINT('Ctrl Pts',(-20.6522321703216,32.3030869212564,122.55890721292)) ;
#68343 = CARTESIAN_POINT('Ctrl Pts',(-20.4036500863331,32.1230978408936,122.729503326657)) ;
#68344 = CARTESIAN_POINT('Ctrl Pts',(-20.7796679108865,32.3129281767434,122.783972393412)) ;
#68345 = CARTESIAN_POINT('Ctrl Pts',(-20.5055910403937,32.1329390963805,122.909552376083)) ;
#68346 = CARTESIAN_POINT('Ctrl Pts',(-20.8678841148157,32.3229144923316,123.031085830974)) ;
#68347 = CARTESIAN_POINT('Ctrl Pts',(-20.576163376053,32.1429254119687,123.107244959995)) ;
#68348 = CARTESIAN_POINT('Ctrl Pts',(-20.9117732133019,32.332851099918,123.288538866815)) ;
#68349 = CARTESIAN_POINT('Ctrl Pts',(-20.6112720124456,32.1528620195551,123.313207406856)) ;
#68350 = CARTESIAN_POINT('Ctrl Pts',(-20.910145815352,32.3429009672863,123.552606824038)) ;
#68351 = CARTESIAN_POINT('Ctrl Pts',(-20.6099679432151,32.1629118869234,123.524461792942)) ;
#68352 = CARTESIAN_POINT('Ctrl Pts',(-20.8638163142715,32.3527514619611,123.807307622436)) ;
#68353 = CARTESIAN_POINT('Ctrl Pts',(-20.5729021084178,32.1727623815982,123.72822191254)) ;
#68354 = CARTESIAN_POINT('Ctrl Pts',(-20.773519983493,32.3627232623556,124.053271401024)) ;
#68355 = CARTESIAN_POINT('Ctrl Pts',(-20.5006629717372,32.1827341819927,123.924992078725)) ;
#68356 = CARTESIAN_POINT('Ctrl Pts',(-20.6415042015941,32.3727192293814,124.280422776241)) ;
#68357 = CARTESIAN_POINT('Ctrl Pts',(-20.3950484362192,32.1927301490186,124.106711993813)) ;
#68358 = CARTESIAN_POINT('Ctrl Pts',(-20.4711197706811,32.3827566887626,124.481749462152)) ;
#68359 = CARTESIAN_POINT('Ctrl Pts',(-20.2587391854302,32.2027676083997,124.267771863989)) ;
#68360 = CARTESIAN_POINT('Ctrl Pts',(-20.2726207381904,32.3925973896634,124.6475312724)) ;
#68361 = CARTESIAN_POINT('Ctrl Pts',(-20.0999386785007,32.2126083093005,124.400395461972)) ;
#68362 = CARTESIAN_POINT('Ctrl Pts',(-20.0438481628859,32.4026454109307,124.779365277945)) ;
#68363 = CARTESIAN_POINT('Ctrl Pts',(-19.9169195251314,32.2226563305678,124.50586072606)) ;
#68364 = CARTESIAN_POINT('Ctrl Pts',(-19.7979892008617,32.4125928040134,124.868183348147)) ;
#68365 = CARTESIAN_POINT('Ctrl Pts',(-19.7202316993048,32.2326037236505,124.576913031386)) ;
#68366 = CARTESIAN_POINT('Ctrl Pts',(-19.5415342218403,32.4225029500598,124.913581797367)) ;
#68367 = CARTESIAN_POINT('Ctrl Pts',(-19.515067529213,32.2425138696969,124.613229582587)) ;
#68368 = CARTESIAN_POINT('Ctrl Pts',(-19.277223918375,32.4325618639094,124.913465271175)) ;
#68369 = CARTESIAN_POINT('Ctrl Pts',(-19.3036192607228,32.2525727835465,124.613134137926)) ;
#68370 = CARTESIAN_POINT('Ctrl Pts',(-19.022469311543,32.4424026341987,124.868802452506)) ;
#68371 = CARTESIAN_POINT('Ctrl Pts',(-19.099816280715,32.2624135538358,124.577401773527)) ;
#68372 = CARTESIAN_POINT('Ctrl Pts',(-18.7738114256327,32.4524655037773,124.778908029314)) ;
#68373 = CARTESIAN_POINT('Ctrl Pts',(-18.9008906793119,32.2724764234145,124.505484170492)) ;
#68374 = CARTESIAN_POINT('Ctrl Pts',(-18.5484324346786,32.4623598269078,124.649195864268)) ;
#68375 = CARTESIAN_POINT('Ctrl Pts',(-18.7205888114285,32.2823707465449,124.401712667753)) ;
#68376 = CARTESIAN_POINT('Ctrl Pts',(-18.3476349380033,32.4723016340023,124.482101731582)) ;
#68377 = CARTESIAN_POINT('Ctrl Pts',(-18.5599523479521,32.2923125536394,124.268035850005)) ;
#68378 = CARTESIAN_POINT('Ctrl Pts',(-18.1777508202333,32.4823041449576,124.281474853431)) ;
#68379 = CARTESIAN_POINT('Ctrl Pts',(-18.4240467225334,32.3023150645948,124.10753302208)) ;
#68380 = CARTESIAN_POINT('Ctrl Pts',(-18.0452392633268,32.492338865776,124.053503454134)) ;
#68381 = CARTESIAN_POINT('Ctrl Pts',(-18.3180393459561,32.3123497854131,123.925154800795)) ;
#68382 = CARTESIAN_POINT('Ctrl Pts',(-17.9556292696089,32.5021840432817,123.810780412352)) ;
#68383 = CARTESIAN_POINT('Ctrl Pts',(-18.24635350555,32.3221949629189,123.73097605505)) ;
#68384 = CARTESIAN_POINT('Ctrl Pts',(-17.9083727783839,32.5121688036828,123.552719582534)) ;
#68385 = CARTESIAN_POINT('Ctrl Pts',(-18.2085503837353,32.3321797233199,123.524527146658)) ;
#68386 = CARTESIAN_POINT('Ctrl Pts',(-17.9065240318847,32.5221077099992,123.291502653985)) ;
#68387 = CARTESIAN_POINT('Ctrl Pts',(-18.2070734512826,32.3421186296363,123.315553837412)) ;
#68388 = CARTESIAN_POINT('Ctrl Pts',(-17.9505907657664,32.5321499376349,123.031335993592)) ;
#68389 = CARTESIAN_POINT('Ctrl Pts',(-18.242328891931,32.3521608572721,123.107420816645)) ;
#68390 = CARTESIAN_POINT('Ctrl Pts',(-18.0376192936705,32.5420351492193,122.786543593569)) ;
#68391 = CARTESIAN_POINT('Ctrl Pts',(-18.3119535058972,32.3620460688564,122.911587983726)) ;
#68392 = CARTESIAN_POINT('Ctrl Pts',(-18.1669767556182,32.5520340794212,122.557873550048)) ;
#68393 = CARTESIAN_POINT('Ctrl Pts',(-18.4154411876375,32.3720449990584,122.728653018332)) ;
#68394 = CARTESIAN_POINT('Ctrl Pts',(-18.3326104946629,32.5619515023317,122.356600741746)) ;
#68395 = CARTESIAN_POINT('Ctrl Pts',(-18.5479494908398,32.3819624219688,122.567636304059)) ;
#68396 = CARTESIAN_POINT('Ctrl Pts',(-18.5332526173871,32.5719994344104,122.185007966984)) ;
#68397 = CARTESIAN_POINT('Ctrl Pts',(-18.7084645480787,32.3920103540475,122.430363551794)) ;
#68398 = CARTESIAN_POINT('Ctrl Pts',(-18.7567232187338,32.5818768102198,122.052875232647)) ;
#68399 = CARTESIAN_POINT('Ctrl Pts',(-18.8872415842206,32.4018877298569,122.324659316094)) ;
#68400 = CARTESIAN_POINT('Ctrl Pts',(-19.0039525695959,32.5919307033877,121.95982536141)) ;
#68401 = CARTESIAN_POINT('Ctrl Pts',(-19.0850258485824,32.4119416230248,122.250221203348)) ;
#68402 = CARTESIAN_POINT('Ctrl Pts',(-19.2595182815849,32.601824326641,121.911755678648)) ;
#68403 = CARTESIAN_POINT('Ctrl Pts',(-19.2894783105699,32.4218352462781,122.211767438031)) ;
#68404 = CARTESIAN_POINT('Ctrl Pts',(-19.5238926627054,32.611886920264,121.908700188409)) ;
#68405 = CARTESIAN_POINT('Ctrl Pts',(-19.5009779851935,32.4318978399011,122.209324968628)) ;
#68406 = CARTESIAN_POINT('Ctrl Pts',(-19.7791709674073,32.6217294942531,121.950535647314)) ;
#68407 = CARTESIAN_POINT('Ctrl Pts',(-19.7051996362344,32.4417404138902,122.242795101324)) ;
#68408 = CARTESIAN_POINT('Ctrl Pts',(-20.0271280441419,32.631720251136,122.036735366636)) ;
#68409 = CARTESIAN_POINT('Ctrl Pts',(-19.9035645706121,32.4517311707731,122.311756541242)) ;
#68410 = CARTESIAN_POINT('Ctrl Pts',(-20.2549311093635,32.6416483128939,122.163938821337)) ;
#68411 = CARTESIAN_POINT('Ctrl Pts',(-20.0858057967329,32.4616592325311,122.413520699274)) ;
#68412 = CARTESIAN_POINT('Ctrl Pts',(-20.4586943445291,32.6516362887831,122.329402962598)) ;
#68413 = CARTESIAN_POINT('Ctrl Pts',(-20.2488151736051,32.4716472084202,122.545893272239)) ;
#68414 = CARTESIAN_POINT('Ctrl Pts',(-20.6311078851739,32.6616719531395,122.528955452347)) ;
#68415 = CARTESIAN_POINT('Ctrl Pts',(-20.3867446776176,32.4816828727767,122.705536503265)) ;
#68416 = CARTESIAN_POINT('Ctrl Pts',(-20.76419350534,32.6715278915592,122.751167847475)) ;
#68417 = CARTESIAN_POINT('Ctrl Pts',(-20.4932112993434,32.4915388111963,122.88330668774)) ;
#68418 = CARTESIAN_POINT('Ctrl Pts',(-20.8583709770248,32.6815233829561,122.99634558384)) ;
#68419 = CARTESIAN_POINT('Ctrl Pts',(-20.5685516696912,32.5015343025932,123.079449363677)) ;
#68420 = CARTESIAN_POINT('Ctrl Pts',(-20.9082019158921,32.6914331879096,123.251966021349)) ;
#68421 = CARTESIAN_POINT('Ctrl Pts',(-20.6084146932958,32.5114441075467,123.283945511149)) ;
#68422 = CARTESIAN_POINT('Ctrl Pts',(-20.913367466307,32.7014454101763,123.515032024856)) ;
#68423 = CARTESIAN_POINT('Ctrl Pts',(-20.6125455536325,32.5214563298134,123.494398306009)) ;
#68424 = CARTESIAN_POINT('Ctrl Pts',(-20.8722060909322,32.7114732908691,123.775321815842)) ;
#68425 = CARTESIAN_POINT('Ctrl Pts',(-20.5796147887184,32.5314842105063,123.702629927723)) ;
#68426 = CARTESIAN_POINT('Ctrl Pts',(-20.7883600167789,32.7213296868517,124.02038977865)) ;
#68427 = CARTESIAN_POINT('Ctrl Pts',(-20.5125366813953,32.5413406064889,123.898683026209)) ;
#68428 = CARTESIAN_POINT('Ctrl Pts',(-20.6615779007813,32.7313544840317,124.25132140461)) ;
#68429 = CARTESIAN_POINT('Ctrl Pts',(-20.4111096709629,32.5513654036688,124.083427628986)) ;
#68430 = CARTESIAN_POINT('Ctrl Pts',(-20.4960157375153,32.7413854140155,124.456454889738)) ;
#68431 = CARTESIAN_POINT('Ctrl Pts',(-20.2786586468199,32.5613963336526,124.247533447329)) ;
#68432 = CARTESIAN_POINT('Ctrl Pts',(-20.3013621684409,32.7512300165242,124.626844922445)) ;
#68433 = CARTESIAN_POINT('Ctrl Pts',(-20.1229354628895,32.5712409361613,124.38384373688)) ;
#68434 = CARTESIAN_POINT('Ctrl Pts',(-20.0771483650704,32.7612208677483,124.763458712167)) ;
#68435 = CARTESIAN_POINT('Ctrl Pts',(-19.9435638346434,32.5812317873854,124.493133506793)) ;
#68436 = CARTESIAN_POINT('Ctrl Pts',(-19.8312628601083,32.7712587007595,124.858962378708)) ;
#68437 = CARTESIAN_POINT('Ctrl Pts',(-19.7468547876405,32.5912696203966,124.569535079804)) ;
#68438 = CARTESIAN_POINT('Ctrl Pts',(-19.5775920832475,32.7811030892249,124.909777937782)) ;
#68439 = CARTESIAN_POINT('Ctrl Pts',(-19.5439188102841,32.6011140088621,124.610185961714)) ;
#68440 = CARTESIAN_POINT('Ctrl Pts',(-19.3153197757331,32.7910878935945,124.916379101424)) ;
#68441 = CARTESIAN_POINT('Ctrl Pts',(-19.3341011312526,32.6110988132316,124.615465586228)) ;
#68442 = CARTESIAN_POINT('Ctrl Pts',(-19.0569748481772,32.8010274130773,124.877619388893)) ;
#68443 = CARTESIAN_POINT('Ctrl Pts',(-19.1274258094831,32.6210383327145,124.584456619583)) ;
#68444 = CARTESIAN_POINT('Ctrl Pts',(-18.8068609697535,32.8110671440787,124.793713447214)) ;
#68445 = CARTESIAN_POINT('Ctrl Pts',(-18.9273350056697,32.6310780637158,124.517330604952)) ;
#68446 = CARTESIAN_POINT('Ctrl Pts',(-18.5785199696836,32.820955272325,124.669655218426)) ;
#68447 = CARTESIAN_POINT('Ctrl Pts',(-18.7446634574821,32.6409661919621,124.418083265181)) ;
#68448 = CARTESIAN_POINT('Ctrl Pts',(-18.3728153330768,32.8309449975335,124.506569798915)) ;
#68449 = CARTESIAN_POINT('Ctrl Pts',(-18.5801006004135,32.6509559171706,124.287614130099)) ;
#68450 = CARTESIAN_POINT('Ctrl Pts',(-18.1992468678326,32.840902762235,124.310742518053)) ;
#68451 = CARTESIAN_POINT('Ctrl Pts',(-18.4412469568537,32.6609136818721,124.130951769751)) ;
#68452 = CARTESIAN_POINT('Ctrl Pts',(-18.0625524288157,32.850805103647,124.089302873787)) ;
#68453 = CARTESIAN_POINT('Ctrl Pts',(-18.3318926747522,32.6708160232841,123.95380009295)) ;
#68454 = CARTESIAN_POINT('Ctrl Pts',(-17.9650377613778,32.8608492993534,123.844039624706)) ;
#68455 = CARTESIAN_POINT('Ctrl Pts',(-18.2538818733743,32.6808602189905,123.757588954974)) ;
#68456 = CARTESIAN_POINT('Ctrl Pts',(-17.9122844842802,32.8707567001127,123.58906943826)) ;
#68457 = CARTESIAN_POINT('Ctrl Pts',(-18.2116804247751,32.6907676197498,123.553613231978)) ;
#68458 = CARTESIAN_POINT('Ctrl Pts',(-17.9040614841339,32.880767299987,123.326126151249)) ;
#68459 = CARTESIAN_POINT('Ctrl Pts',(-18.2051029793148,32.7007782196241,123.34325861009)) ;
#68460 = CARTESIAN_POINT('Ctrl Pts',(-17.9421976273555,32.8907975958992,123.065306227518)) ;
#68461 = CARTESIAN_POINT('Ctrl Pts',(-18.2356129698765,32.7108085155363,123.134602745316)) ;
#68462 = CARTESIAN_POINT('Ctrl Pts',(-18.0232436735507,32.9006523755489,122.819357208247)) ;
#68463 = CARTESIAN_POINT('Ctrl Pts',(-18.3004504322419,32.720663295186,122.937844802407)) ;
#68464 = CARTESIAN_POINT('Ctrl Pts',(-18.1463463293519,32.9106097037664,122.588444800357)) ;
#68465 = CARTESIAN_POINT('Ctrl Pts',(-18.3989330865564,32.7306206234035,122.753115585193)) ;
#68466 = CARTESIAN_POINT('Ctrl Pts',(-18.3093474042476,32.9206487366733,122.381033273986)) ;
#68467 = CARTESIAN_POINT('Ctrl Pts',(-18.5293347464535,32.7406596563104,122.587186824327)) ;
#68468 = CARTESIAN_POINT('Ctrl Pts',(-18.5023603004912,32.9305218485626,122.207583253798)) ;
#68469 = CARTESIAN_POINT('Ctrl Pts',(-18.6837449255098,32.7505327681997,122.448428002608)) ;
#68470 = CARTESIAN_POINT('Ctrl Pts',(-18.7269817759468,32.9405951335897,122.067617063673)) ;
#68471 = CARTESIAN_POINT('Ctrl Pts',(-18.8634428286131,32.7606060532268,122.336455563458)) ;
#68472 = CARTESIAN_POINT('Ctrl Pts',(-18.9663055363985,32.9504154533265,121.970905134139)) ;
#68473 = CARTESIAN_POINT('Ctrl Pts',(-19.0549009577353,32.7704263729636,122.259087166004)) ;
#68474 = CARTESIAN_POINT('Ctrl Pts',(-19.2252558871534,32.9604941187049,121.915591458617)) ;
#68475 = CARTESIAN_POINT('Ctrl Pts',(-19.262061748827,32.780505038342,122.214836808385)) ;
#68476 = CARTESIAN_POINT('Ctrl Pts',(-19.4840372151867,32.9703457091887,121.906199287805)) ;
#68477 = CARTESIAN_POINT('Ctrl Pts',(-19.4690857796967,32.7903566288258,122.207323762619)) ;
#68478 = CARTESIAN_POINT('Ctrl Pts',(-19.7462073716882,32.9804188595076,121.942441422299)) ;
#68479 = CARTESIAN_POINT('Ctrl Pts',(-19.6788221704482,32.8004297791447,122.236318111422)) ;
#68480 = CARTESIAN_POINT('Ctrl Pts',(-19.9923907933803,32.9902612394826,122.021850824201)) ;
#68481 = CARTESIAN_POINT('Ctrl Pts',(-19.8757676411912,32.8102721591198,122.299845862724)) ;
#68482 = CARTESIAN_POINT('Ctrl Pts',(-20.2246277641436,33.0002422157257,122.143718242006)) ;
#68483 = CARTESIAN_POINT('Ctrl Pts',(-20.0615568191512,32.8202531353628,122.397340033153)) ;
#68484 = CARTESIAN_POINT('Ctrl Pts',(-20.4326666594073,33.010258544081,122.304997705767)) ;
#68485 = CARTESIAN_POINT('Ctrl Pts',(-20.2279876169795,32.8302694637181,122.52636399411)) ;
#68486 = CARTESIAN_POINT('Ctrl Pts',(-20.6076780088902,33.0201563410721,122.497403957948)) ;
#68487 = CARTESIAN_POINT('Ctrl Pts',(-20.3679958534134,32.8401672607093,122.680288693608)) ;
#68488 = CARTESIAN_POINT('Ctrl Pts',(-20.7486295700232,33.0301688978042,122.719608055138)) ;
#68489 = CARTESIAN_POINT('Ctrl Pts',(-20.4807568301996,32.8501798174413,122.858052122149)) ;
#68490 = CARTESIAN_POINT('Ctrl Pts',(-20.8484637130917,33.0402009326507,122.96359161389)) ;
#68491 = CARTESIAN_POINT('Ctrl Pts',(-20.5606237531606,32.8602118522878,123.053239243088)) ;
#68492 = CARTESIAN_POINT('Ctrl Pts',(-20.9039796443904,33.0500403334661,123.216152649294)) ;
#68493 = CARTESIAN_POINT('Ctrl Pts',(-20.6050359484339,32.8700512531033,123.255286987946)) ;
#68494 = CARTESIAN_POINT('Ctrl Pts',(-20.9152463774755,33.0601061191177,123.480399984258)) ;
#68495 = CARTESIAN_POINT('Ctrl Pts',(-20.6140490933859,32.8801170387548,123.466685170754)) ;
#68496 = CARTESIAN_POINT('Ctrl Pts',(-20.8809372575507,33.0699965742323,123.738064421165)) ;
#68497 = CARTESIAN_POINT('Ctrl Pts',(-20.5866016261539,32.8900074938694,123.672815854496)) ;
#68498 = CARTESIAN_POINT('Ctrl Pts',(-20.8021533889854,33.0799886928681,123.98853537261)) ;
#68499 = CARTESIAN_POINT('Ctrl Pts',(-20.523574446852,32.8999996125052,123.873192408795)) ;
#68500 = CARTESIAN_POINT('Ctrl Pts',(-20.6812106073249,33.0899515196311,124.220732031348)) ;
#68501 = CARTESIAN_POINT('Ctrl Pts',(-20.4268202076342,32.9099624392683,124.058949317243)) ;
#68502 = CARTESIAN_POINT('Ctrl Pts',(-20.5232306933288,33.099855802904,124.427605321835)) ;
#68503 = CARTESIAN_POINT('Ctrl Pts',(-20.3004367035077,32.9198667225411,124.22444733005)) ;
#68504 = CARTESIAN_POINT('Ctrl Pts',(-20.3285971107455,33.1099162368511,124.606480559927)) ;
#68505 = CARTESIAN_POINT('Ctrl Pts',(-20.1447295646736,32.9299271564882,124.36754764172)) ;
#68506 = CARTESIAN_POINT('Ctrl Pts',(-20.1108525131507,33.1197567895243,124.746047511506)) ;
#68507 = CARTESIAN_POINT('Ctrl Pts',(-19.970534871693,32.9397677091614,124.479200559667)) ;
#68508 = CARTESIAN_POINT('Ctrl Pts',(-19.8669950901314,33.12981900947,124.84821784105)) ;
#68509 = CARTESIAN_POINT('Ctrl Pts',(-19.7754486895611,32.9498299291071,124.560937006756)) ;
#68510 = CARTESIAN_POINT('Ctrl Pts',(-19.6132318493154,33.1397161487486,124.905283007203)) ;
#68511 = CARTESIAN_POINT('Ctrl Pts',(-19.5724388798712,32.9597270683857,124.606588967545)) ;
#68512 = CARTESIAN_POINT('Ctrl Pts',(-19.3525812289575,33.1496473408836,124.918328736674)) ;
#68513 = CARTESIAN_POINT('Ctrl Pts',(-19.3639189712111,32.9696582605208,124.617025749215)) ;
#68514 = CARTESIAN_POINT('Ctrl Pts',(-19.090770522027,33.1596894955287,124.885264797401)) ;
#68515 = CARTESIAN_POINT('Ctrl Pts',(-19.1544702195643,32.9797004151658,124.590574725584)) ;
#68516 = CARTESIAN_POINT('Ctrl Pts',(-18.842487870914,33.169576256548,124.808646986439)) ;
#68517 = CARTESIAN_POINT('Ctrl Pts',(-18.9558448766533,32.9895871761851,124.529280933374)) ;
#68518 = CARTESIAN_POINT('Ctrl Pts',(-18.6085457635101,33.1795755582652,124.689058201042)) ;
#68519 = CARTESIAN_POINT('Ctrl Pts',(-18.7686911704573,32.9995864779024,124.433610222531)) ;
#68520 = CARTESIAN_POINT('Ctrl Pts',(-18.4004044124469,33.189496356432,124.532007686267)) ;
#68521 = CARTESIAN_POINT('Ctrl Pts',(-18.6021783869313,33.0095072760691,124.307970451747)) ;
#68522 = CARTESIAN_POINT('Ctrl Pts',(-18.2206897370185,33.1995304100287,124.339091714962)) ;
#68523 = CARTESIAN_POINT('Ctrl Pts',(-18.4584063193687,33.0195413296658,124.153637825087)) ;
#68524 = CARTESIAN_POINT('Ctrl Pts',(-18.0786177880743,33.2094535275951,124.120374761366)) ;
#68525 = CARTESIAN_POINT('Ctrl Pts',(-18.344748777028,33.0294644472322,123.978664981646)) ;
#68526 = CARTESIAN_POINT('Ctrl Pts',(-17.9753934550452,33.2195096510942,123.87713368977)) ;
#68527 = CARTESIAN_POINT('Ctrl Pts',(-18.2621688831962,33.0395205707314,123.784072046529)) ;
#68528 = CARTESIAN_POINT('Ctrl Pts',(-17.9170984303965,33.2293550927491,123.625046988953)) ;
#68529 = CARTESIAN_POINT('Ctrl Pts',(-18.2155327344032,33.0493660123862,123.582403874291)) ;
#68530 = CARTESIAN_POINT('Ctrl Pts',(-17.9024396209619,33.2393173938732,123.363675275733)) ;
#68531 = CARTESIAN_POINT('Ctrl Pts',(-18.2038050999464,33.0593283135103,123.373306898927)) ;
#68532 = CARTESIAN_POINT('Ctrl Pts',(-17.9339408232565,33.2493458731483,123.102009100134)) ;
#68533 = CARTESIAN_POINT('Ctrl Pts',(-18.2290055541262,33.0693567927855,123.163973819942)) ;
#68534 = CARTESIAN_POINT('Ctrl Pts',(-18.009402919707,33.259256226658,122.852760854094)) ;
#68535 = CARTESIAN_POINT('Ctrl Pts',(-18.2893745088673,33.0792671462951,122.964575736527)) ;
#68536 = CARTESIAN_POINT('Ctrl Pts',(-18.1266871223674,33.2691910988352,122.61950036567)) ;
#68537 = CARTESIAN_POINT('Ctrl Pts',(-18.3832009980876,33.0892020184723,122.777967498192)) ;
#68538 = CARTESIAN_POINT('Ctrl Pts',(-18.2845465433898,33.2792322364209,122.40806845954)) ;
#68539 = CARTESIAN_POINT('Ctrl Pts',(-18.5094881032574,33.099243156058,122.608821464249)) ;
#68540 = CARTESIAN_POINT('Ctrl Pts',(-18.4736647676083,33.2891193856355,122.229881635933)) ;
#68541 = CARTESIAN_POINT('Ctrl Pts',(-18.6607816011752,33.1091303052726,122.466272069737)) ;
#68542 = CARTESIAN_POINT('Ctrl Pts',(-18.6928889148738,33.2991116203865,122.085373784708)) ;
#68543 = CARTESIAN_POINT('Ctrl Pts',(-18.8361603422665,33.1191225400237,122.350665209582)) ;
#68544 = CARTESIAN_POINT('Ctrl Pts',(-18.9328841091275,33.3090603259495,121.981637584403)) ;
#68545 = CARTESIAN_POINT('Ctrl Pts',(-19.0281557898517,33.1290712455866,122.267675703838)) ;
#68546 = CARTESIAN_POINT('Ctrl Pts',(-19.1868031331839,33.3189963943732,121.920862306553)) ;
#68547 = CARTESIAN_POINT('Ctrl Pts',(-19.2312903095408,33.1390073140103,122.219054752622)) ;
#68548 = CARTESIAN_POINT('Ctrl Pts',(-19.4487454010854,33.328982078589,121.90471788781)) ;
#68549 = CARTESIAN_POINT('Ctrl Pts',(-19.4408438645719,33.1489929982261,122.20613828772)) ;
#68550 = CARTESIAN_POINT('Ctrl Pts',(-19.7108540776556,33.3390225051576,121.934873930191)) ;
#68551 = CARTESIAN_POINT('Ctrl Pts',(-19.6505310372627,33.1590334247948,122.230262297346)) ;
#68552 = CARTESIAN_POINT('Ctrl Pts',(-19.9588162424853,33.3488616186214,122.008165761205)) ;
#68553 = CARTESIAN_POINT('Ctrl Pts',(-19.8488999925423,33.1688725382585,122.288894547529)) ;
#68554 = CARTESIAN_POINT('Ctrl Pts',(-20.1950323307625,33.3588913527972,122.125097981869)) ;
#68555 = CARTESIAN_POINT('Ctrl Pts',(-20.0378734209598,33.1789022724343,122.38243939003)) ;
#68556 = CARTESIAN_POINT('Ctrl Pts',(-20.406784218548,33.3689134523031,122.281698617158)) ;
#68557 = CARTESIAN_POINT('Ctrl Pts',(-20.2072754977896,33.1889243719402,122.507719170111)) ;
#68558 = CARTESIAN_POINT('Ctrl Pts',(-20.5858350552601,33.3787818921965,122.469326974363)) ;
#68559 = CARTESIAN_POINT('Ctrl Pts',(-20.350516319059,33.1987928118337,122.657820459907)) ;
#68560 = CARTESIAN_POINT('Ctrl Pts',(-20.732476955186,33.3888507568821,122.68954538537)) ;
#68561 = CARTESIAN_POINT('Ctrl Pts',(-20.4678308998726,33.2088616765193,122.833994843785)) ;
#68562 = CARTESIAN_POINT('Ctrl Pts',(-20.8362904559934,33.3986934299808,122.926463443138)) ;
#68563 = CARTESIAN_POINT('Ctrl Pts',(-20.5508822680002,33.2187043496179,123.023527908559)) ;
#68564 = CARTESIAN_POINT('Ctrl Pts',(-20.8990494415645,33.4086540641432,123.180578146984)) ;
#68565 = CARTESIAN_POINT('Ctrl Pts',(-20.6010906294462,33.2286649837803,123.226819047015)) ;
#68566 = CARTESIAN_POINT('Ctrl Pts',(-20.916351249052,33.4186919798213,123.443786581483)) ;
#68567 = CARTESIAN_POINT('Ctrl Pts',(-20.6149332528463,33.2387028994585,123.43738582393)) ;
#68568 = CARTESIAN_POINT('Ctrl Pts',(-20.8886281343362,33.4285662546808,123.701819630219)) ;
#68569 = CARTESIAN_POINT('Ctrl Pts',(-20.592756117805,33.2485771743179,123.643811594593)) ;
#68570 = CARTESIAN_POINT('Ctrl Pts',(-20.8151004364326,33.4386360050559,123.95598455471)) ;
#68571 = CARTESIAN_POINT('Ctrl Pts',(-20.5339351068565,33.258646924693,123.84714415652)) ;
#68572 = CARTESIAN_POINT('Ctrl Pts',(-20.7013946872375,33.4484693004304,124.188056231771)) ;
#68573 = CARTESIAN_POINT('Ctrl Pts',(-20.442972128081,33.2684802200675,124.03280115278)) ;
#68574 = CARTESIAN_POINT('Ctrl Pts',(-20.5466931297227,33.45849959791,124.401459336272)) ;
#68575 = CARTESIAN_POINT('Ctrl Pts',(-20.3192120229929,33.2785105175472,124.20352454908)) ;
#68576 = CARTESIAN_POINT('Ctrl Pts',(-20.3567007162318,33.4685316843515,124.58424663072)) ;
#68577 = CARTESIAN_POINT('Ctrl Pts',(-20.1672189437675,33.2885426039886,124.34975536662)) ;
#68578 = CARTESIAN_POINT('Ctrl Pts',(-20.1426457143214,33.4783596128404,124.728735741513)) ;
#68579 = CARTESIAN_POINT('Ctrl Pts',(-19.9959765796565,33.2983705324775,124.465347258471)) ;
#68580 = CARTESIAN_POINT('Ctrl Pts',(-19.9029989792466,33.4883556539512,124.836308043002)) ;
#68581 = CARTESIAN_POINT('Ctrl Pts',(-19.8042599394586,33.3083665735883,124.551406472735)) ;
#68582 = CARTESIAN_POINT('Ctrl Pts',(-19.6474220237301,33.4983814660524,124.900335793291)) ;
#68583 = CARTESIAN_POINT('Ctrl Pts',(-19.5997986983396,33.3183923856895,124.602630093288)) ;
#68584 = CARTESIAN_POINT('Ctrl Pts',(-19.3882695560054,33.5082687009472,124.919091810044)) ;
#68585 = CARTESIAN_POINT('Ctrl Pts',(-19.3924774972755,33.3282796205843,124.617636375343)) ;
#68586 = CARTESIAN_POINT('Ctrl Pts',(-19.1274334857693,33.5182455671582,124.892759807624)) ;
#68587 = CARTESIAN_POINT('Ctrl Pts',(-19.1838086836,33.3382564867954,124.596572391666)) ;
#68588 = CARTESIAN_POINT('Ctrl Pts',(-18.8746590268341,33.52823851103,124.821451907867)) ;
#68589 = CARTESIAN_POINT('Ctrl Pts',(-18.9815887977188,33.3482494306672,124.539527654376)) ;
#68590 = CARTESIAN_POINT('Ctrl Pts',(-18.6372374521722,33.5382764337014,124.706546424498)) ;
#68591 = CARTESIAN_POINT('Ctrl Pts',(-18.7916507985739,33.3582873533385,124.447604630339)) ;
#68592 = CARTESIAN_POINT('Ctrl Pts',(-18.4271493677989,33.5481248979631,124.555368999614)) ;
#68593 = CARTESIAN_POINT('Ctrl Pts',(-18.6235800486874,33.3681358176002,124.326664485506)) ;
#68594 = CARTESIAN_POINT('Ctrl Pts',(-18.2435773439465,33.5581167647071,124.367679767415)) ;
#68595 = CARTESIAN_POINT('Ctrl Pts',(-18.4767213025052,33.3781276843442,124.176514389402)) ;
#68596 = CARTESIAN_POINT('Ctrl Pts',(-18.096319636919,33.5680344967483,124.152599028164)) ;
#68597 = CARTESIAN_POINT('Ctrl Pts',(-18.3589139685211,33.3880454163854,124.004451152358)) ;
#68598 = CARTESIAN_POINT('Ctrl Pts',(-17.9874040348388,33.5780626816436,123.912652984584)) ;
#68599 = CARTESIAN_POINT('Ctrl Pts',(-18.271779888472,33.3980736012807,123.812495012593)) ;
#68600 = CARTESIAN_POINT('Ctrl Pts',(-17.9226291155959,33.5879478396924,123.661079753393)) ;
#68601 = CARTESIAN_POINT('Ctrl Pts',(-18.2199583955529,33.4079587593295,123.611237435979)) ;
#68602 = CARTESIAN_POINT('Ctrl Pts',(-17.9016709287819,33.5979372002341,123.399402541443)) ;
#68603 = CARTESIAN_POINT('Ctrl Pts',(-18.2031899993243,33.4179481198712,123.401895940217)) ;
#68604 = CARTESIAN_POINT('Ctrl Pts',(-17.9271501704679,33.6079783571685,123.1367648659)) ;
#68605 = CARTESIAN_POINT('Ctrl Pts',(-18.2235716341578,33.4279892768056,123.191785556007)) ;
#68606 = CARTESIAN_POINT('Ctrl Pts',(-17.9959631146861,33.6178109406236,122.887710030823)) ;
#68607 = CARTESIAN_POINT('Ctrl Pts',(-18.2786200105537,33.4378218602607,122.992541933455)) ;
#68608 = CARTESIAN_POINT('Ctrl Pts',(-18.1081263093149,33.6278051605856,122.650231330554)) ;
#68609 = CARTESIAN_POINT('Ctrl Pts',(-18.3683487586546,33.4478160802227,122.802558226559)) ;
#68610 = CARTESIAN_POINT('Ctrl Pts',(-18.2607792875272,33.6378332623729,122.435411305488)) ;
#68611 = CARTESIAN_POINT('Ctrl Pts',(-18.4904696240239,33.45784418201,122.630701109372)) ;
#68612 = CARTESIAN_POINT('Ctrl Pts',(-18.4453797141511,33.647713206996,122.252832221367)) ;
#68613 = CARTESIAN_POINT('Ctrl Pts',(-18.6381482311407,33.4677241266331,122.484636845497)) ;
#68614 = CARTESIAN_POINT('Ctrl Pts',(-18.6610157891126,33.657703533553,122.10310705135)) ;
#68615 = CARTESIAN_POINT('Ctrl Pts',(-18.8106558663145,33.4777144531901,122.364855145268)) ;
#68616 = CARTESIAN_POINT('Ctrl Pts',(-18.8982140305105,33.6676444652073,121.993631136502)) ;
#68617 = CARTESIAN_POINT('Ctrl Pts',(-19.0004133768427,33.4876553848444,122.277272732784)) ;
#68618 = CARTESIAN_POINT('Ctrl Pts',(-19.1519080089799,33.6776315837102,121.92632833614)) ;
#68619 = CARTESIAN_POINT('Ctrl Pts',(-19.2033679299254,33.4976425033473,122.223428561246)) ;
#68620 = CARTESIAN_POINT('Ctrl Pts',(-19.4146423301779,33.6876649166074,121.904411969349)) ;
#68621 = CARTESIAN_POINT('Ctrl Pts',(-19.4135552411739,33.5076758362445,122.20589349727)) ;
#68622 = CARTESIAN_POINT('Ctrl Pts',(-19.6729091690056,33.6975310210521,121.927545767156)) ;
#68623 = CARTESIAN_POINT('Ctrl Pts',(-19.6201683942856,33.5175419406893,122.224398461816)) ;
#68624 = CARTESIAN_POINT('Ctrl Pts',(-19.9282681240009,33.7075971349325,121.996466980296)) ;
#68625 = CARTESIAN_POINT('Ctrl Pts',(-19.8244562056054,33.5276080545696,122.279533486686)) ;
#68626 = CARTESIAN_POINT('Ctrl Pts',(-20.1628320829574,33.7174531467009,122.10634520991)) ;
#68627 = CARTESIAN_POINT('Ctrl Pts',(-20.0121077897334,33.537464066338,122.367434006079)) ;
#68628 = CARTESIAN_POINT('Ctrl Pts',(-20.3781604555604,33.7274478503322,122.256728476995)) ;
#68629 = CARTESIAN_POINT('Ctrl Pts',(-20.184371642184,33.5474587699693,122.487738827655)) ;
#68630 = CARTESIAN_POINT('Ctrl Pts',(-20.5643974693118,33.7374791860571,122.443302838799)) ;
#68631 = CARTESIAN_POINT('Ctrl Pts',(-20.3333627176559,33.5574901056942,122.636996853287)) ;
#68632 = CARTESIAN_POINT('Ctrl Pts',(-20.713269761922,33.7473457112607,122.655597325724)) ;
#68633 = CARTESIAN_POINT('Ctrl Pts',(-20.4524620449125,33.5673566308979,122.806830892729)) ;
#68634 = CARTESIAN_POINT('Ctrl Pts',(-20.8247303532555,33.7573331393065,122.893178808627)) ;
#68635 = CARTESIAN_POINT('Ctrl Pts',(-20.5416324255552,33.5773440589437,122.99689507574)) ;
#68636 = CARTESIAN_POINT('Ctrl Pts',(-20.8931087336896,33.767278068993,123.145457142139)) ;
#68637 = CARTESIAN_POINT('Ctrl Pts',(-20.5963371660383,33.5872889886301,123.198716996963)) ;
#68638 = CARTESIAN_POINT('Ctrl Pts',(-20.9167263518425,33.7773229871015,123.408343079754)) ;
#68639 = CARTESIAN_POINT('Ctrl Pts',(-20.6152334042726,33.5973339067386,123.409025569641)) ;
#68640 = CARTESIAN_POINT('Ctrl Pts',(-20.8949748056446,33.7871849567154,123.666612207482)) ;
#68641 = CARTESIAN_POINT('Ctrl Pts',(-20.5978343558141,33.6071958763525,123.61564071411)) ;
#68642 = CARTESIAN_POINT('Ctrl Pts',(-20.8283422293108,33.7971770247366,123.920571241178)) ;
#68643 = CARTESIAN_POINT('Ctrl Pts',(-20.5445304472365,33.6171879443737,123.818808427627)) ;
#68644 = CARTESIAN_POINT('Ctrl Pts',(-20.7192376865205,33.8071079501112,124.157662672187)) ;
#68645 = CARTESIAN_POINT('Ctrl Pts',(-20.4572488862588,33.6271188697483,124.008482329076)) ;
#68646 = CARTESIAN_POINT('Ctrl Pts',(-20.5707091129721,33.8170585783346,124.372854625881)) ;
#68647 = CARTESIAN_POINT('Ctrl Pts',(-20.3384279325118,33.6370694979717,124.180637052448)) ;
#68648 = CARTESIAN_POINT('Ctrl Pts',(-20.3862313186414,33.8270588173937,124.560056609312)) ;
#68649 = CARTESIAN_POINT('Ctrl Pts',(-20.1908473210986,33.6470697370308,124.330400159823)) ;
#68650 = CARTESIAN_POINT('Ctrl Pts',(-20.1712584195521,33.8370872727629,124.71248063517)) ;
#68651 = CARTESIAN_POINT('Ctrl Pts',(-20.0188703330059,33.6570981924,124.45234117015)) ;
#68652 = CARTESIAN_POINT('Ctrl Pts',(-19.9370901885251,33.8469533073462,124.823799494521)) ;
#68653 = CARTESIAN_POINT('Ctrl Pts',(-19.8315368156364,33.6669642269833,124.541398163761)) ;
#68654 = CARTESIAN_POINT('Ctrl Pts',(-19.6841021964421,33.8569456290936,124.894057284954)) ;
#68655 = CARTESIAN_POINT('Ctrl Pts',(-19.6291473694453,33.6769565487307,124.597606616661)) ;
#68656 = CARTESIAN_POINT('Ctrl Pts',(-19.424287490384,33.8668779187706,124.9192160717)) ;
#68657 = CARTESIAN_POINT('Ctrl Pts',(-19.4212948596349,33.6868888384077,124.617735604572)) ;
#68658 = CARTESIAN_POINT('Ctrl Pts',(-19.1622401128872,33.8768795637414,124.898995670993)) ;
#68659 = CARTESIAN_POINT('Ctrl Pts',(-19.2116608120875,33.6968904833785,124.60156252601)) ;
#68660 = CARTESIAN_POINT('Ctrl Pts',(-18.823429392135,33.8901921971574,124.811777112252)) ;
#68661 = CARTESIAN_POINT('Ctrl Pts',(-18.9405918138416,33.7102031167945,124.531785666973)) ;
#68662 = CARTESIAN_POINT('Ctrl Pts',(-18.5168908225473,33.903423946539,124.639429121269)) ;
#68663 = CARTESIAN_POINT('Ctrl Pts',(-18.6953483850143,33.7234348661761,124.393891756695)) ;
#68664 = CARTESIAN_POINT('Ctrl Pts',(-18.266416953034,33.916747211356,124.394788919274)) ;
#68665 = CARTESIAN_POINT('Ctrl Pts',(-18.4950002778242,33.7367581309931,124.198208384198)) ;
#68666 = CARTESIAN_POINT('Ctrl Pts',(-18.1147393757088,33.9266229175737,124.184190734435)) ;
#68667 = CARTESIAN_POINT('Ctrl Pts',(-18.3736497561591,33.7466338372108,124.029725816734)) ;
#68668 = CARTESIAN_POINT('Ctrl Pts',(-18.0003398463956,33.9366125086737,123.947943873737)) ;
#68669 = CARTESIAN_POINT('Ctrl Pts',(-18.2821299057794,33.7566234283109,123.840730774139)) ;
#68670 = CARTESIAN_POINT('Ctrl Pts',(-17.9289645288639,33.9465396051291,123.69699206503)) ;
#68671 = CARTESIAN_POINT('Ctrl Pts',(-18.2250270203462,33.7665505247663,123.639969543988)) ;
#68672 = CARTESIAN_POINT('Ctrl Pts',(-17.9019571311773,33.9565647536337,123.434953214904)) ;
#68673 = CARTESIAN_POINT('Ctrl Pts',(-18.2034190100901,33.7765756732709,123.430338874046)) ;
#68674 = CARTESIAN_POINT('Ctrl Pts',(-17.920456867938,33.9664604077804,123.175542057052)) ;
#68675 = CARTESIAN_POINT('Ctrl Pts',(-18.2182165454262,33.7864713274175,123.222809688118)) ;
#68676 = CARTESIAN_POINT('Ctrl Pts',(-17.9840343132116,33.9764639421586,122.920489516577)) ;
#68677 = CARTESIAN_POINT('Ctrl Pts',(-18.2690763509193,33.7964748617957,123.018767172028)) ;
#68678 = CARTESIAN_POINT('Ctrl Pts',(-18.0907856147797,33.9864490805987,122.680743142477)) ;
#68679 = CARTESIAN_POINT('Ctrl Pts',(-18.3544753559251,33.8064600002358,122.826969197833)) ;
#68680 = CARTESIAN_POINT('Ctrl Pts',(-18.2384789185145,33.996485005194,122.462260358717)) ;
#68681 = CARTESIAN_POINT('Ctrl Pts',(-18.4726280899805,33.8164959248312,122.652181813698)) ;
#68682 = CARTESIAN_POINT('Ctrl Pts',(-18.4182776203018,34.0063362806217,122.276005602402)) ;
#68683 = CARTESIAN_POINT('Ctrl Pts',(-18.6164655966101,33.8263472002588,122.503176330571)) ;
#68684 = CARTESIAN_POINT('Ctrl Pts',(-18.6302489538193,34.0163285417831,122.121008187001)) ;
#68685 = CARTESIAN_POINT('Ctrl Pts',(-18.7860413729788,33.8363394614202,122.379176658812)) ;
#68686 = CARTESIAN_POINT('Ctrl Pts',(-18.8673098715377,34.0263684258007,122.00522798075)) ;
#68687 = CARTESIAN_POINT('Ctrl Pts',(-18.9756890388998,33.8463793454378,122.2865505691)) ;
#68688 = CARTESIAN_POINT('Ctrl Pts',(-19.1155543481873,34.0362032003031,121.933213929773)) ;
#68689 = CARTESIAN_POINT('Ctrl Pts',(-19.1742842270233,33.8562141199402,122.228937167852)) ;
#68690 = CARTESIAN_POINT('Ctrl Pts',(-19.3787606441446,34.0462795813234,121.904625237353)) ;
#68691 = CARTESIAN_POINT('Ctrl Pts',(-19.3848492266586,33.8662905009605,122.20606409206)) ;
#68692 = CARTESIAN_POINT('Ctrl Pts',(-19.636979964933,34.056125854474,121.921704730838)) ;
#68693 = CARTESIAN_POINT('Ctrl Pts',(-19.591423616235,33.8761367741112,122.219725605663)) ;
#68694 = CARTESIAN_POINT('Ctrl Pts',(-19.9782262367002,34.0694903757593,122.004738916925)) ;
#68695 = CARTESIAN_POINT('Ctrl Pts',(-19.8644290060011,33.8895012953964,122.286150073343)) ;
#68696 = CARTESIAN_POINT('Ctrl Pts',(-20.2860725515586,34.0826966201937,122.173341752895)) ;
#68697 = CARTESIAN_POINT('Ctrl Pts',(-20.1107333615667,33.9027075398308,122.421054696917)) ;
#68698 = CARTESIAN_POINT('Ctrl Pts',(-20.5388137926812,34.0959615748709,122.413398914322)) ;
#68699 = CARTESIAN_POINT('Ctrl Pts',(-20.3128900569695,33.9159724945081,122.613069455434)) ;
#68700 = CARTESIAN_POINT('Ctrl Pts',(-20.6954462284396,34.1059938554226,122.625471146507)) ;
#68701 = CARTESIAN_POINT('Ctrl Pts',(-20.4382052101993,33.9260047750597,122.782731831385)) ;
#68702 = CARTESIAN_POINT('Ctrl Pts',(-20.8114438350329,34.1159025889405,122.858591933872)) ;
#68703 = CARTESIAN_POINT('Ctrl Pts',(-20.5310032327312,33.9359135085776,122.969226073235)) ;
#68704 = CARTESIAN_POINT('Ctrl Pts',(-20.8860726329882,34.125840139808,123.108858926557)) ;
#68705 = CARTESIAN_POINT('Ctrl Pts',(-20.5907085395253,33.9458510594451,123.169440598116)) ;
#68706 = CARTESIAN_POINT('Ctrl Pts',(-20.9161696354576,34.1358699874019,123.370684085346)) ;
#68707 = CARTESIAN_POINT('Ctrl Pts',(-20.6147885800743,33.9558809070391,123.37889723275)) ;
#68708 = CARTESIAN_POINT('Ctrl Pts',(-20.8957675550664,34.1491051273224,123.717974610671)) ;
#68709 = CARTESIAN_POINT('Ctrl Pts',(-20.5984660541345,33.9691160469595,123.656745092967)) ;
#68710 = CARTESIAN_POINT('Ctrl Pts',(-20.7562726268257,34.1657735916935,124.138314956001)) ;
#68711 = CARTESIAN_POINT('Ctrl Pts',(-20.4868736501461,33.9857845113307,123.993003032338)) ;
#68712 = CARTESIAN_POINT('Ctrl Pts',(-20.4290861791078,34.1856446035674,124.553127465598)) ;
#68713 = CARTESIAN_POINT('Ctrl Pts',(-20.2251415375173,34.0056555232046,124.32485414861)) ;
#68714 = CARTESIAN_POINT('Ctrl Pts',(-20.0516612997823,34.2023516879504,124.786832185012)) ;
#68715 = CARTESIAN_POINT('Ctrl Pts',(-19.9231542599151,34.0223626075875,124.511841034845)) ;
#68716 = CARTESIAN_POINT('Ctrl Pts',(-19.7200431655426,34.215528969261,124.88675620924)) ;
#68717 = CARTESIAN_POINT('Ctrl Pts',(-19.6579040689418,34.0355398888981,124.591763773494)) ;
#68718 = CARTESIAN_POINT('Ctrl Pts',(-19.3739840223207,34.2287964297751,124.92908813568)) ;
#68719 = CARTESIAN_POINT('Ctrl Pts',(-19.3810402452549,34.0488073494122,124.625633782971)) ;
#68720 = CARTESIAN_POINT('Ctrl Pts',(-18.936720024018,34.2454103204623,124.86755517988)) ;
#68721 = CARTESIAN_POINT('Ctrl Pts',(-19.0312400607427,34.0654212400994,124.576410349906)) ;
#68722 = CARTESIAN_POINT('Ctrl Pts',(-18.4683529488932,34.2653591198897,124.618947214226)) ;
#68723 = CARTESIAN_POINT('Ctrl Pts',(-18.6565409486287,34.0853700395268,124.377526283527)) ;
#68724 = CARTESIAN_POINT('Ctrl Pts',(-18.1135823385577,34.2852802314206,124.226010700003)) ;
#68725 = CARTESIAN_POINT('Ctrl Pts',(-18.3727229363681,34.1052911510577,124.063178594994)) ;
#68726 = CARTESIAN_POINT('Ctrl Pts',(-17.9136663305497,34.3051466795934,123.737213595555)) ;
#68727 = CARTESIAN_POINT('Ctrl Pts',(-18.2127872251194,34.1251575992306,123.672140797996)) ;
#68728 = CARTESIAN_POINT('Ctrl Pts',(-17.8927069831386,34.3251730262106,123.205416904764)) ;
#68729 = CARTESIAN_POINT('Ctrl Pts',(-18.1960174659992,34.1451839458477,123.246703802556)) ;
#68730 = CARTESIAN_POINT('Ctrl Pts',(-18.0532950837359,34.3450350706001,122.702439446676)) ;
#68731 = CARTESIAN_POINT('Ctrl Pts',(-18.3244861394055,34.1650459902372,122.844319988715)) ;
#68732 = CARTESIAN_POINT('Ctrl Pts',(-18.3764719974847,34.3649803732812,122.282323158732)) ;
#68733 = CARTESIAN_POINT('Ctrl Pts',(-18.5830265759983,34.1849912929184,122.50822539218)) ;
#68734 = CARTESIAN_POINT('Ctrl Pts',(-18.8226102498659,34.3848756803401,121.998446004947)) ;
#68735 = CARTESIAN_POINT('Ctrl Pts',(-18.9399371661432,34.2048865999772,122.281121677154)) ;
#68736 = CARTESIAN_POINT('Ctrl Pts',(-19.3385786404572,34.4047689505077,121.882935209767)) ;
#68737 = CARTESIAN_POINT('Ctrl Pts',(-19.3527127879478,34.2247798701449,122.188711677315)) ;
#68738 = CARTESIAN_POINT('Ctrl Pts',(-19.864843872694,34.4247345431882,121.950781567567)) ;
#68739 = CARTESIAN_POINT('Ctrl Pts',(-19.773725507496,34.2447454628253,122.242987830082)) ;
#68740 = CARTESIAN_POINT('Ctrl Pts',(-20.3344600160615,34.444609866873,122.192739799094)) ;
#68741 = CARTESIAN_POINT('Ctrl Pts',(-20.149420050782,34.2646207865101,122.436554544585)) ;
#68742 = CARTESIAN_POINT('Ctrl Pts',(-20.6955112754201,34.464584929448,122.582004291072)) ;
#68743 = CARTESIAN_POINT('Ctrl Pts',(-20.4382613889304,34.2845958490851,122.74796620737)) ;
#68744 = CARTESIAN_POINT('Ctrl Pts',(-20.9010681970121,34.4845373390791,123.070845431308)) ;
#68745 = CARTESIAN_POINT('Ctrl Pts',(-20.6027074986626,34.3045482587162,123.139039529433)) ;
#68746 = CARTESIAN_POINT('Ctrl Pts',(-20.9283379623324,34.5043733933152,123.597346656962)) ;
#68747 = CARTESIAN_POINT('Ctrl Pts',(-20.6245230859658,34.3243843129523,123.560242643287)) ;
#68748 = CARTESIAN_POINT('Ctrl Pts',(-20.7737648833637,34.5243513047327,124.105329355223)) ;
#68749 = CARTESIAN_POINT('Ctrl Pts',(-20.5008637718727,34.3443622243698,123.966628801619)) ;
#68750 = CARTESIAN_POINT('Ctrl Pts',(-20.4555977349369,34.5442693542362,124.528394482397)) ;
#68751 = CARTESIAN_POINT('Ctrl Pts',(-20.2463288803223,34.3642802738733,124.305081255519)) ;
#68752 = CARTESIAN_POINT('Ctrl Pts',(-20.0139097341758,34.5641374980043,124.818008765311)) ;
#68753 = CARTESIAN_POINT('Ctrl Pts',(-19.8929765031619,34.3841484176414,124.536772192443)) ;
#68754 = CARTESIAN_POINT('Ctrl Pts',(-19.4952245290992,34.5841883545916,124.939780508264)) ;
#68755 = CARTESIAN_POINT('Ctrl Pts',(-19.4780285056584,34.4041992742287,124.634188162972)) ;
#68756 = CARTESIAN_POINT('Ctrl Pts',(-18.9729159061863,34.6039687910475,124.878612004196)) ;
#68757 = CARTESIAN_POINT('Ctrl Pts',(-19.0601796451305,34.4239797106846,124.585251399659)) ;
#68758 = CARTESIAN_POINT('Ctrl Pts',(-18.496759486199,34.6239988467253,124.640786108479)) ;
#68759 = CARTESIAN_POINT('Ctrl Pts',(-18.6792557743103,34.4440097663624,124.394988854983)) ;
#68760 = CARTESIAN_POINT('Ctrl Pts',(-18.1335792137849,34.6438799519001,124.256847057463)) ;
#68761 = CARTESIAN_POINT('Ctrl Pts',(-18.3887122909116,34.4638908715372,124.087835457315)) ;
#68762 = CARTESIAN_POINT('Ctrl Pts',(-17.9219139096296,34.6637604142679,123.772762991353)) ;
#68763 = CARTESIAN_POINT('Ctrl Pts',(-18.2193820937176,34.483771333905,123.700566231009)) ;
#68764 = CARTESIAN_POINT('Ctrl Pts',(-17.8881094855176,34.6837455614122,123.242649910961)) ;
#68765 = CARTESIAN_POINT('Ctrl Pts',(-18.1923412744921,34.5037564810494,123.276475501805)) ;
#68766 = CARTESIAN_POINT('Ctrl Pts',(-18.0366497415648,34.7036361399486,122.735276316463)) ;
#68767 = CARTESIAN_POINT('Ctrl Pts',(-18.3111764212583,34.5236470595857,122.87057664201)) ;
#68768 = CARTESIAN_POINT('Ctrl Pts',(-18.3487015779653,34.723530159823,122.308436690887)) ;
#68769 = CARTESIAN_POINT('Ctrl Pts',(-18.5608208835814,34.5435410794601,122.529106268789)) ;
#68770 = CARTESIAN_POINT('Ctrl Pts',(-18.7881430602527,34.7434516045494,122.013226846896)) ;
#68771 = CARTESIAN_POINT('Ctrl Pts',(-18.9123763432651,34.5634625241865,122.292940896369)) ;
#68772 = CARTESIAN_POINT('Ctrl Pts',(-19.3013427498124,34.7633497426048,121.884875817397)) ;
#68773 = CARTESIAN_POINT('Ctrl Pts',(-19.3229374638322,34.583360662242,122.190263485441)) ;
#68774 = CARTESIAN_POINT('Ctrl Pts',(-19.8317538659919,34.7834204978209,121.940822959894)) ;
#68775 = CARTESIAN_POINT('Ctrl Pts',(-19.7472655742941,34.603431417458,122.235024637541)) ;
#68776 = CARTESIAN_POINT('Ctrl Pts',(-20.3047188071783,34.8032060478722,122.170959918835)) ;
#68777 = CARTESIAN_POINT('Ctrl Pts',(-20.1256368670043,34.6232169675093,122.419137989732)) ;
#68778 = CARTESIAN_POINT('Ctrl Pts',(-20.6751904640124,34.8231891227495,122.55139832022)) ;
#68779 = CARTESIAN_POINT('Ctrl Pts',(-20.4220114541107,34.6432000423866,122.72349136495)) ;
#68780 = CARTESIAN_POINT('Ctrl Pts',(-20.8920819873269,34.8430982053954,123.034062768714)) ;
#68781 = CARTESIAN_POINT('Ctrl Pts',(-20.5955208682009,34.6631091250326,123.109625335908)) ;
#68782 = CARTESIAN_POINT('Ctrl Pts',(-20.9326680570592,34.8629567645182,123.560377307948)) ;
#68783 = CARTESIAN_POINT('Ctrl Pts',(-20.6279870568241,34.6829676841553,123.53067592304)) ;
#68784 = CARTESIAN_POINT('Ctrl Pts',(-20.7893451366516,34.8830002083569,124.073345382285)) ;
#68785 = CARTESIAN_POINT('Ctrl Pts',(-20.5133192229244,34.703011127994,123.941055778839)) ;
#68786 = CARTESIAN_POINT('Ctrl Pts',(-20.5344079580577,34.8995002730861,124.43033347796)) ;
#68787 = CARTESIAN_POINT('Ctrl Pts',(-20.309383562949,34.7195111927232,124.226623694968)) ;
#68788 = CARTESIAN_POINT('Ctrl Pts',(-20.2630356079764,34.912890012935,124.654232063007)) ;
#68789 = CARTESIAN_POINT('Ctrl Pts',(-20.0922687245513,34.7329009325721,124.405758721467)) ;
#68790 = CARTESIAN_POINT('Ctrl Pts',(-20.0376601532639,34.9227469141434,124.781982024209)) ;
#68791 = CARTESIAN_POINT('Ctrl Pts',(-19.911970256192,34.7427578337805,124.507953327853)) ;
#68792 = CARTESIAN_POINT('Ctrl Pts',(-19.7904462531825,34.9327384399899,124.870322609915)) ;
#68793 = CARTESIAN_POINT('Ctrl Pts',(-19.7141969621559,34.752749359627,124.578624529211)) ;
#68794 = CARTESIAN_POINT('Ctrl Pts',(-19.5333148830126,34.9426631204409,124.914209741491)) ;
#68795 = CARTESIAN_POINT('Ctrl Pts',(-19.5084940323309,34.762674040078,124.613732529277)) ;
#68796 = CARTESIAN_POINT('Ctrl Pts',(-19.2702905171994,34.9526737104853,124.912873328828)) ;
#68797 = CARTESIAN_POINT('Ctrl Pts',(-19.2980655576572,34.7726846301224,124.61265864524)) ;
#68798 = CARTESIAN_POINT('Ctrl Pts',(-18.9272936377873,34.9659329711889,124.851006430555)) ;
#68799 = CARTESIAN_POINT('Ctrl Pts',(-19.0237133047444,34.7859438908261,124.563175229187)) ;
#68800 = CARTESIAN_POINT('Ctrl Pts',(-18.606436005865,34.9792840463392,124.69972105366)) ;
#68801 = CARTESIAN_POINT('Ctrl Pts',(-18.7669990812473,34.7992949659763,124.442141522519)) ;
#68802 = CARTESIAN_POINT('Ctrl Pts',(-18.3413122765646,34.992490355574,124.475665673841)) ;
#68803 = CARTESIAN_POINT('Ctrl Pts',(-18.5548921869106,34.8125012752111,124.262885113938)) ;
#68804 = CARTESIAN_POINT('Ctrl Pts',(-18.1729444100433,35.0024771891643,124.274406568228)) ;
#68805 = CARTESIAN_POINT('Ctrl Pts',(-18.4202016064083,34.8224881088014,124.101878384377)) ;
#68806 = CARTESIAN_POINT('Ctrl Pts',(-18.0423683362087,35.0124299166604,124.047733829672)) ;
#68807 = CARTESIAN_POINT('Ctrl Pts',(-18.3157421784876,34.8324408362975,123.920538559733)) ;
#68808 = CARTESIAN_POINT('Ctrl Pts',(-17.9525123755645,35.022478013502,123.799470169266)) ;
#68809 = CARTESIAN_POINT('Ctrl Pts',(-18.2438596889398,34.8424889331391,123.721927081998)) ;
#68810 = CARTESIAN_POINT('Ctrl Pts',(-17.9077516294115,35.0323194703738,123.544724476242)) ;
#68811 = CARTESIAN_POINT('Ctrl Pts',(-18.208053265257,34.8523303900109,123.518130066413)) ;
#68812 = CARTESIAN_POINT('Ctrl Pts',(-17.9073445683786,35.0423057372873,123.282339109367)) ;
#68813 = CARTESIAN_POINT('Ctrl Pts',(-18.2077298902901,34.8623166569244,123.308221845002)) ;
#68814 = CARTESIAN_POINT('Ctrl Pts',(-17.9521637827218,35.0522423381877,123.025046666914)) ;
#68815 = CARTESIAN_POINT('Ctrl Pts',(-18.2435874714704,34.8722532578248,123.10238833231)) ;
#68816 = CARTESIAN_POINT('Ctrl Pts',(-18.0420906679866,35.0622922809748,122.776754559742)) ;
#68817 = CARTESIAN_POINT('Ctrl Pts',(-18.3155310899466,34.8823032006119,122.903755461618)) ;
#68818 = CARTESIAN_POINT('Ctrl Pts',(-18.1709996406622,35.0721424806605,122.552262724124)) ;
#68819 = CARTESIAN_POINT('Ctrl Pts',(-18.4186601790438,34.8921534002976,122.724163199285)) ;
#68820 = CARTESIAN_POINT('Ctrl Pts',(-18.3384352196694,35.0821153855926,122.350682137594)) ;
#68821 = CARTESIAN_POINT('Ctrl Pts',(-18.5526103127129,34.9021263052297,122.562900239816)) ;
#68822 = CARTESIAN_POINT('Ctrl Pts',(-18.5389407429953,35.0921137600722,122.180827804113)) ;
#68823 = CARTESIAN_POINT('Ctrl Pts',(-18.7130161369838,34.9121246797094,122.427018525397)) ;
#68824 = CARTESIAN_POINT('Ctrl Pts',(-18.7664484679922,35.1021339339422,122.048263316574)) ;
#68825 = CARTESIAN_POINT('Ctrl Pts',(-18.8950234142683,34.9221448535794,122.320968904354)) ;
#68826 = CARTESIAN_POINT('Ctrl Pts',(-19.0105165623716,35.1120349778842,121.958081319082)) ;
#68827 = CARTESIAN_POINT('Ctrl Pts',(-19.0902785364057,34.9320458975213,122.24882546228)) ;
#68828 = CARTESIAN_POINT('Ctrl Pts',(-19.2687227454526,35.1220237816085,121.910830619248)) ;
#68829 = CARTESIAN_POINT('Ctrl Pts',(-19.2968438044793,34.9420347012456,122.211027113215)) ;
#68830 = CARTESIAN_POINT('Ctrl Pts',(-19.5305882706686,35.1319892484403,121.909321300949)) ;
#68831 = CARTESIAN_POINT('Ctrl Pts',(-19.5063361388599,34.9520001680775,122.209821901071)) ;
#68832 = CARTESIAN_POINT('Ctrl Pts',(-19.7872767838356,35.1418928107133,121.952415553993)) ;
#68833 = CARTESIAN_POINT('Ctrl Pts',(-19.7116863821234,34.9619037303504,122.244299447509)) ;
#68834 = CARTESIAN_POINT('Ctrl Pts',(-20.0363461469721,35.1519534885913,122.040990349835)) ;
#68835 = CARTESIAN_POINT('Ctrl Pts',(-19.9109411536517,34.9719644082284,122.315161388044)) ;
#68836 = CARTESIAN_POINT('Ctrl Pts',(-20.2614426416287,35.1617937865408,122.168353377903)) ;
#68837 = CARTESIAN_POINT('Ctrl Pts',(-20.0910169782063,34.9818047061779,122.417053562184)) ;
#68838 = CARTESIAN_POINT('Ctrl Pts',(-20.4656690482286,35.1718567814502,122.33629520841)) ;
#68839 = CARTESIAN_POINT('Ctrl Pts',(-20.2543967460004,34.9918677010873,122.551408735198)) ;
#68840 = CARTESIAN_POINT('Ctrl Pts',(-20.6346269466373,35.1817510755973,122.533966500745)) ;
#68841 = CARTESIAN_POINT('Ctrl Pts',(-20.389561223534,35.0017619952345,122.709546994155)) ;
#68842 = CARTESIAN_POINT('Ctrl Pts',(-20.7679099510609,35.1916928732942,122.758634465352)) ;
#68843 = CARTESIAN_POINT('Ctrl Pts',(-20.4961856757514,35.0117037929313,122.889282276775)) ;
#68844 = CARTESIAN_POINT('Ctrl Pts',(-20.8608365588192,35.2016954508233,123.004554830575)) ;
#68845 = CARTESIAN_POINT('Ctrl Pts',(-20.5705249456458,35.0217063704604,123.086019259422)) ;
#68846 = CARTESIAN_POINT('Ctrl Pts',(-20.9093992123313,35.2117299147444,123.263726218813)) ;
#68847 = CARTESIAN_POINT('Ctrl Pts',(-20.6093729389667,35.0317408343815,123.293356782246)) ;
#68848 = CARTESIAN_POINT('Ctrl Pts',(-20.912575954229,35.2215760532655,123.522461220006)) ;
#68849 = CARTESIAN_POINT('Ctrl Pts',(-20.6119121959131,35.0415869729026,123.500344358)) ;
#68850 = CARTESIAN_POINT('Ctrl Pts',(-20.8707879748683,35.2315572265025,123.781384610257)) ;
#68851 = CARTESIAN_POINT('Ctrl Pts',(-20.5784797854132,35.0515681461396,123.707482601004)) ;
#68852 = CARTESIAN_POINT('Ctrl Pts',(-20.7848581741263,35.2415095204597,124.028409346698)) ;
#68853 = CARTESIAN_POINT('Ctrl Pts',(-20.5097340530019,35.0615204400968,123.905101502577)) ;
#68854 = CARTESIAN_POINT('Ctrl Pts',(-20.6570382603351,35.2515083155943,124.258005618651)) ;
#68855 = CARTESIAN_POINT('Ctrl Pts',(-20.4074763796465,35.0715192352314,124.088777453895)) ;
#68856 = CARTESIAN_POINT('Ctrl Pts',(-20.4902556612724,35.2615474238551,124.462394870675)) ;
#68857 = CARTESIAN_POINT('Ctrl Pts',(-20.2740486420064,35.0815583434922,124.252287564926)) ;
#68858 = CARTESIAN_POINT('Ctrl Pts',(-20.2951179160963,35.2713723652943,124.631484396849)) ;
#68859 = CARTESIAN_POINT('Ctrl Pts',(-20.117937581225,35.0913832849314,124.387557244038)) ;
#68860 = CARTESIAN_POINT('Ctrl Pts',(-20.0686559821828,35.2814270523687,124.767580615175)) ;
#68861 = CARTESIAN_POINT('Ctrl Pts',(-19.9367669380912,35.1014379720058,124.496432562579)) ;
#68862 = CARTESIAN_POINT('Ctrl Pts',(-19.8245654449264,35.2913698573088,124.860825828368)) ;
#68863 = CARTESIAN_POINT('Ctrl Pts',(-19.74149402968,35.1113807769459,124.571026731217)) ;
#68864 = CARTESIAN_POINT('Ctrl Pts',(-19.5691531625667,35.3012736433053,124.910862029586)) ;
#68865 = CARTESIAN_POINT('Ctrl Pts',(-19.5371642509211,35.1212845629424,124.61105371151)) ;
#68866 = CARTESIAN_POINT('Ctrl Pts',(-19.3052006854437,35.3113204598701,124.915700617854)) ;
#68867 = CARTESIAN_POINT('Ctrl Pts',(-19.3260021502799,35.1313313795072,124.614922626619)) ;
#68868 = CARTESIAN_POINT('Ctrl Pts',(-19.0482438728121,35.3212159793488,124.875474923149)) ;
#68869 = CARTESIAN_POINT('Ctrl Pts',(-19.1204374586696,35.1412268989859,124.582740243431)) ;
#68870 = CARTESIAN_POINT('Ctrl Pts',(-18.7981091918514,35.3312780646732,124.789853312718)) ;
#68871 = CARTESIAN_POINT('Ctrl Pts',(-18.9203301991824,35.1512889843104,124.514241085553)) ;
#68872 = CARTESIAN_POINT('Ctrl Pts',(-18.571557569673,35.3411207756312,124.664983089902)) ;
#68873 = CARTESIAN_POINT('Ctrl Pts',(-18.7390904274587,35.1611316952683,124.4143435761)) ;
#68874 = CARTESIAN_POINT('Ctrl Pts',(-18.3667589020139,35.3511114929372,124.500756432804)) ;
#68875 = CARTESIAN_POINT('Ctrl Pts',(-18.5752527356648,35.1711224125743,124.282960925271)) ;
#68876 = CARTESIAN_POINT('Ctrl Pts',(-18.1946758847601,35.3610395760338,124.304637787655)) ;
#68877 = CARTESIAN_POINT('Ctrl Pts',(-18.4375879438694,35.1810504956709,124.126065105729)) ;
#68878 = CARTESIAN_POINT('Ctrl Pts',(-18.0580530664321,35.3710275061455,124.080513754998)) ;
#68879 = CARTESIAN_POINT('Ctrl Pts',(-18.3282912523427,35.1910384257827,123.946765097769)) ;
#68880 = CARTESIAN_POINT('Ctrl Pts',(-17.9623826480587,35.3810633322728,123.83475626619)) ;
#68881 = CARTESIAN_POINT('Ctrl Pts',(-18.2517565843422,35.20107425191,123.750158383688)) ;
#68882 = CARTESIAN_POINT('Ctrl Pts',(-17.9113535514333,35.3909186693864,123.580830234499)) ;
#68883 = CARTESIAN_POINT('Ctrl Pts',(-18.2109351630595,35.2109295890236,123.547017932825)) ;
#68884 = CARTESIAN_POINT('Ctrl Pts',(-17.9046862415223,35.4009164042366,123.318213209581)) ;
#68885 = CARTESIAN_POINT('Ctrl Pts',(-18.205602992744,35.2209273238737,123.336924392206)) ;
#68886 = CARTESIAN_POINT('Ctrl Pts',(-17.9432873405184,35.4108243082211,123.060708970242)) ;
#68887 = CARTESIAN_POINT('Ctrl Pts',(-18.2364854316828,35.2308352278582,123.130921769729)) ;
#68888 = CARTESIAN_POINT('Ctrl Pts',(-18.0264553068263,35.4208353827695,122.811112169827)) ;
#68889 = CARTESIAN_POINT('Ctrl Pts',(-18.3030212907696,35.2408463024066,122.931244865584)) ;
#68890 = CARTESIAN_POINT('Ctrl Pts',(-18.1523789389796,35.4308632383051,122.579621476818)) ;
#68891 = CARTESIAN_POINT('Ctrl Pts',(-18.403761694324,35.2508741579423,122.746053067434)) ;
#68892 = CARTESIAN_POINT('Ctrl Pts',(-18.3134289650525,35.4407208322104,122.376725539727)) ;
#68893 = CARTESIAN_POINT('Ctrl Pts',(-18.5326024658146,35.2607317518475,122.583737933796)) ;
#68894 = CARTESIAN_POINT('Ctrl Pts',(-18.5102358433116,35.4507475190485,122.201520587918)) ;
#68895 = CARTESIAN_POINT('Ctrl Pts',(-18.6900489765213,35.2707584386856,122.443575071446)) ;
#68896 = CARTESIAN_POINT('Ctrl Pts',(-18.7348673255698,35.4607761882022,122.063678979707)) ;
#68897 = CARTESIAN_POINT('Ctrl Pts',(-18.8697550564223,35.2807871078393,122.333303131403)) ;
#68898 = CARTESIAN_POINT('Ctrl Pts',(-18.9753389392073,35.4706213964836,121.968264330612)) ;
#68899 = CARTESIAN_POINT('Ctrl Pts',(-19.0621320757983,35.2906323161207,122.256973158654)) ;
#68900 = CARTESIAN_POINT('Ctrl Pts',(-19.232344395239,35.4806120854467,121.914585662056)) ;
#68901 = CARTESIAN_POINT('Ctrl Pts',(-19.2677365699942,35.3006230050839,122.214031608862)) ;
#68902 = CARTESIAN_POINT('Ctrl Pts',(-19.4960145845419,35.490649961729,121.906896220203)) ;
#68903 = CARTESIAN_POINT('Ctrl Pts',(-19.4786728720695,35.3106608813661,122.207881552385)) ;
#68904 = CARTESIAN_POINT('Ctrl Pts',(-19.7520613231325,35.5004943393712,121.943923950967)) ;
#68905 = CARTESIAN_POINT('Ctrl Pts',(-19.6835091319941,35.3205052590084,122.237504996433)) ;
#68906 = CARTESIAN_POINT('Ctrl Pts',(-20.0014137029836,35.5104791437627,122.025494346825)) ;
#68907 = CARTESIAN_POINT('Ctrl Pts',(-19.8829904412346,35.3304900633998,122.302762488264)) ;
#68908 = CARTESIAN_POINT('Ctrl Pts',(-20.2318815338735,35.5204186739812,122.148494733348)) ;
#68909 = CARTESIAN_POINT('Ctrl Pts',(-20.0673637209045,35.3404295936183,122.401163717447)) ;
#68910 = CARTESIAN_POINT('Ctrl Pts',(-20.4394809697131,35.5304583620181,122.311280393352)) ;
#68911 = CARTESIAN_POINT('Ctrl Pts',(-20.2334425657068,35.3504692816552,122.53139333392)) ;
#68912 = CARTESIAN_POINT('Ctrl Pts',(-20.6131244207075,35.5403466513864,122.504619288811)) ;
#68913 = CARTESIAN_POINT('Ctrl Pts',(-20.3723558935254,35.3603575710235,122.686064744329)) ;
#68914 = CARTESIAN_POINT('Ctrl Pts',(-20.7523694041922,35.5503357750712,122.72713725888)) ;
#68915 = CARTESIAN_POINT('Ctrl Pts',(-20.4837508097204,35.3703466947083,122.864079588493)) ;
#68916 = CARTESIAN_POINT('Ctrl Pts',(-20.8503882560538,35.5602957847458,122.969824688647)) ;
#68917 = CARTESIAN_POINT('Ctrl Pts',(-20.5621646481119,35.3803067043829,123.058229659203)) ;
#68918 = CARTESIAN_POINT('Ctrl Pts',(-20.9050630989688,35.57019621445,123.224196430447)) ;
#68919 = CARTESIAN_POINT('Ctrl Pts',(-20.6059033396929,35.3902071340872,123.261726591413)) ;
#68920 = CARTESIAN_POINT('Ctrl Pts',(-20.9148664709882,35.5802392958568,123.487924566708)) ;
#68921 = CARTESIAN_POINT('Ctrl Pts',(-20.6137449783066,35.4002502154939,123.472709296187)) ;
#68922 = CARTESIAN_POINT('Ctrl Pts',(-20.8792189654738,35.5901466897644,123.74584291802)) ;
#68923 = CARTESIAN_POINT('Ctrl Pts',(-20.5852260111583,35.4101576094016,123.679043182914)) ;
#68924 = CARTESIAN_POINT('Ctrl Pts',(-20.7989552795368,35.6001584207536,123.996400804876)) ;
#68925 = CARTESIAN_POINT('Ctrl Pts',(-20.5210141652758,35.4201693403907,123.879489165425)) ;
#68926 = CARTESIAN_POINT('Ctrl Pts',(-20.6756899073301,35.6101906384684,124.229454654533)) ;
#68927 = CARTESIAN_POINT('Ctrl Pts',(-20.4224008782605,35.4302015581055,124.065931815006)) ;
#68928 = CARTESIAN_POINT('Ctrl Pts',(-20.5170202759795,35.6200431477146,124.434034154075)) ;
#68929 = CARTESIAN_POINT('Ctrl Pts',(-20.2954650100176,35.4400540673517,124.229594006282)) ;
#68930 = CARTESIAN_POINT('Ctrl Pts',(-20.3237177193579,35.6300010842576,124.610433802406)) ;
#68931 = CARTESIAN_POINT('Ctrl Pts',(-20.1408227029007,35.4500120038947,124.370712879431)) ;
#68932 = CARTESIAN_POINT('Ctrl Pts',(-20.1006943914862,35.6400399542659,124.751315017522)) ;
#68933 = CARTESIAN_POINT('Ctrl Pts',(-19.9624034408403,35.460050873903,124.483417150071)) ;
#68934 = CARTESIAN_POINT('Ctrl Pts',(-19.8607559657353,35.6499131094241,124.850152762012)) ;
#68935 = CARTESIAN_POINT('Ctrl Pts',(-19.7704532300316,35.4699240290612,124.562486266306)) ;
#68936 = CARTESIAN_POINT('Ctrl Pts',(-19.6022411196816,35.6599863842738,124.906856510779)) ;
#68937 = CARTESIAN_POINT('Ctrl Pts',(-19.5636408438425,35.4799973039109,124.607848540031)) ;
#68938 = CARTESIAN_POINT('Ctrl Pts',(-19.3443505908473,35.6698067014512,124.917880380727)) ;
#68939 = CARTESIAN_POINT('Ctrl Pts',(-19.3573296329594,35.4898176210883,124.616666850261)) ;
#68940 = CARTESIAN_POINT('Ctrl Pts',(-19.0818227174019,35.6798853872447,124.883323751729)) ;
#68941 = CARTESIAN_POINT('Ctrl Pts',(-19.147307048226,35.4998963068818,124.589020826947)) ;
#68942 = CARTESIAN_POINT('Ctrl Pts',(-18.8348266453424,35.6897368986278,124.805553629414)) ;
#68943 = CARTESIAN_POINT('Ctrl Pts',(-18.9497113939592,35.5097478182649,124.526804423587)) ;
#68944 = CARTESIAN_POINT('Ctrl Pts',(-18.5999081950905,35.6998103449344,124.683638544709)) ;
#68945 = CARTESIAN_POINT('Ctrl Pts',(-18.7617765978972,35.5198212645716,124.429271661873)) ;
#68946 = CARTESIAN_POINT('Ctrl Pts',(-18.3945197612094,35.7096516200591,124.526430434708)) ;
#68947 = CARTESIAN_POINT('Ctrl Pts',(-18.5974671222276,35.5296625396963,124.303505384468)) ;
#68948 = CARTESIAN_POINT('Ctrl Pts',(-18.2164254320828,35.7196367197159,124.333759479541)) ;
#68949 = CARTESIAN_POINT('Ctrl Pts',(-18.4549921099954,35.539647639353,124.149368519473)) ;
#68950 = CARTESIAN_POINT('Ctrl Pts',(-18.0744564633631,35.7296441958502,124.112362113073)) ;
#68951 = CARTESIAN_POINT('Ctrl Pts',(-18.3414173794509,35.5496551154873,123.972250409102)) ;
#68952 = CARTESIAN_POINT('Ctrl Pts',(-17.9737377684653,35.7395667835592,123.871857563518)) ;
#68953 = CARTESIAN_POINT('Ctrl Pts',(-18.2608430645821,35.5595777031963,123.779847173338)) ;
#68954 = CARTESIAN_POINT('Ctrl Pts',(-17.915514233427,35.7495533878325,123.61593526692)) ;
#68955 = CARTESIAN_POINT('Ctrl Pts',(-18.2142645957526,35.5695643074696,123.575109448264)) ;
#68956 = CARTESIAN_POINT('Ctrl Pts',(-17.9030386020177,35.7595935161666,123.352407710946)) ;
#68957 = CARTESIAN_POINT('Ctrl Pts',(-18.2042845372192,35.5796044358037,123.364287232758)) ;
#68958 = CARTESIAN_POINT('Ctrl Pts',(-17.9352873093838,35.7694329507,123.095829361004)) ;
#68959 = CARTESIAN_POINT('Ctrl Pts',(-18.2300836623065,35.5894438703371,123.159025769629)) ;
#68960 = CARTESIAN_POINT('Ctrl Pts',(-18.0131110083021,35.779497005191,122.843100123072)) ;
#68961 = CARTESIAN_POINT('Ctrl Pts',(-18.2923429533616,35.5995079248281,122.956842160068)) ;
#68962 = CARTESIAN_POINT('Ctrl Pts',(-18.1316925352344,35.7893879244282,122.611771524711)) ;
#68963 = CARTESIAN_POINT('Ctrl Pts',(-18.3872080467958,35.6093988440653,122.771780155463)) ;
#68964 = CARTESIAN_POINT('Ctrl Pts',(-18.2897713917017,35.7993799177342,122.402124132987)) ;
#68965 = CARTESIAN_POINT('Ctrl Pts',(-18.5136711422251,35.6193908373713,122.604062465028)) ;
#68966 = CARTESIAN_POINT('Ctrl Pts',(-18.4814613118421,35.8093427816935,122.223804692162)) ;
#68967 = CARTESIAN_POINT('Ctrl Pts',(-18.6670229513666,35.6293537013306,122.461407311499)) ;
#68968 = CARTESIAN_POINT('Ctrl Pts',(-18.6995746479886,35.8192470415113,122.081746101379)) ;
#68969 = CARTESIAN_POINT('Ctrl Pts',(-18.8415130103748,35.6392579611484,122.347760879673)) ;
#68970 = CARTESIAN_POINT('Ctrl Pts',(-18.9428567780933,35.8293075320827,121.978340523878)) ;
#68971 = CARTESIAN_POINT('Ctrl Pts',(-19.0361390123414,35.6493184517198,122.265036395034)) ;
#68972 = CARTESIAN_POINT('Ctrl Pts',(-19.1947540652062,35.8391478817137,121.919707183759)) ;
#68973 = CARTESIAN_POINT('Ctrl Pts',(-19.2376556973774,35.6591588013508,122.218129998438)) ;
#68974 = CARTESIAN_POINT('Ctrl Pts',(-19.4587582959314,35.8492108572037,121.905070980687)) ;
#68975 = CARTESIAN_POINT('Ctrl Pts',(-19.448859376931,35.6692217768408,122.206420948279)) ;
#68976 = CARTESIAN_POINT('Ctrl Pts',(-19.716930430725,35.8591051773471,121.936190237955)) ;
#68977 = CARTESIAN_POINT('Ctrl Pts',(-19.6553962747645,35.6791160969842,122.231316240817)) ;
#68978 = CARTESIAN_POINT('Ctrl Pts',(-19.9671129941824,35.8690468904787,122.011332156098)) ;
#68979 = CARTESIAN_POINT('Ctrl Pts',(-19.8555418925478,35.6890578101158,122.291429441969)) ;
#68980 = CARTESIAN_POINT('Ctrl Pts',(-20.2020024297301,35.8790497802728,122.129427167199)) ;
#68981 = CARTESIAN_POINT('Ctrl Pts',(-20.0434534559638,35.69906069991,122.385905206129)) ;
#68982 = CARTESIAN_POINT('Ctrl Pts',(-20.4132559197395,35.8890896374333,122.28744132461)) ;
#68983 = CARTESIAN_POINT('Ctrl Pts',(-20.2124564260292,35.7091005570704,122.512316537818)) ;
#68984 = CARTESIAN_POINT('Ctrl Pts',(-20.5904446049363,35.8989138182709,122.475235422024)) ;
#68985 = CARTESIAN_POINT('Ctrl Pts',(-20.3542066813593,35.7189247379081,122.662550716544)) ;
#68986 = CARTESIAN_POINT('Ctrl Pts',(-20.7359772784035,35.9089707917741,122.695816923843)) ;
#68987 = CARTESIAN_POINT('Ctrl Pts',(-20.4706332561571,35.7289817114113,122.839015952767)) ;
#68988 = CARTESIAN_POINT('Ctrl Pts',(-20.8393638309279,35.9188989159612,122.935375322683)) ;
#68989 = CARTESIAN_POINT('Ctrl Pts',(-20.5533424999389,35.7389098355983,123.030662030176)) ;
#68990 = CARTESIAN_POINT('Ctrl Pts',(-20.9004170383969,35.9288526110346,123.189725205683)) ;
#68991 = CARTESIAN_POINT('Ctrl Pts',(-20.602185386523,35.7488635306717,123.234141416124)) ;
#68992 = CARTESIAN_POINT('Ctrl Pts',(-20.9161514803797,35.9388988046099,123.453256665995)) ;
#68993 = CARTESIAN_POINT('Ctrl Pts',(-20.6147732911417,35.758909724247,123.444966757205)) ;
#68994 = CARTESIAN_POINT('Ctrl Pts',(-20.8867329496708,35.9487469069698,123.710376268567)) ;
#68995 = CARTESIAN_POINT('Ctrl Pts',(-20.5912389928801,35.7687578266069,123.650661374287)) ;
#68996 = CARTESIAN_POINT('Ctrl Pts',(-20.813048468652,35.9587084951974,123.961560575043)) ;
#68997 = CARTESIAN_POINT('Ctrl Pts',(-20.5322920915651,35.7787194148345,123.851608640381)) ;
#68998 = CARTESIAN_POINT('Ctrl Pts',(-20.6957786698797,35.9687371653537,124.19759210035)) ;
#68999 = CARTESIAN_POINT('Ctrl Pts',(-20.4384766850489,35.7887480849908,124.04043416191)) ;
#69000 = CARTESIAN_POINT('Ctrl Pts',(-20.5412377893036,35.9786474682354,124.407201312219)) ;
#69001 = CARTESIAN_POINT('Ctrl Pts',(-20.3148448330596,35.7986583878725,124.208121289199)) ;
#69002 = CARTESIAN_POINT('Ctrl Pts',(-20.3526398125085,35.9885823520433,124.587747365873)) ;
#69003 = CARTESIAN_POINT('Ctrl Pts',(-20.1639673252218,35.8085932716804,124.352558280755)) ;
#69004 = CARTESIAN_POINT('Ctrl Pts',(-20.1331135059456,35.9986234937339,124.734141809642)) ;
#69005 = CARTESIAN_POINT('Ctrl Pts',(-19.9883465163358,35.8186344133711,124.469674459931)) ;
#69006 = CARTESIAN_POINT('Ctrl Pts',(-19.8952608881985,36.0085106148979,124.838745840386)) ;
#69007 = CARTESIAN_POINT('Ctrl Pts',(-19.7980654626942,35.828521534535,124.553357985807)) ;
#69008 = CARTESIAN_POINT('Ctrl Pts',(-19.6403085962477,36.0185029577464,124.901535971408)) ;
#69009 = CARTESIAN_POINT('Ctrl Pts',(-19.5941039789621,35.8385138773836,124.603590829665)) ;
#69010 = CARTESIAN_POINT('Ctrl Pts',(-19.3794454821469,36.0284512589704,124.918954868183)) ;
#69011 = CARTESIAN_POINT('Ctrl Pts',(-19.3854139711554,35.8484621786075,124.617526697189)) ;
#69012 = CARTESIAN_POINT('Ctrl Pts',(-19.1197882532334,36.0383888366525,124.8912260194)) ;
#69013 = CARTESIAN_POINT('Ctrl Pts',(-19.1776886066464,35.8583997562896,124.595344542413)) ;
#69014 = CARTESIAN_POINT('Ctrl Pts',(-18.8675463523897,36.0483754111031,124.818724120264)) ;
#69015 = CARTESIAN_POINT('Ctrl Pts',(-18.9758950062236,35.8683863307402,124.537343974835)) ;
#69016 = CARTESIAN_POINT('Ctrl Pts',(-18.6308789216368,36.0584042210115,124.702775017872)) ;
#69017 = CARTESIAN_POINT('Ctrl Pts',(-18.7865606156517,35.8784151406487,124.444585433762)) ;
#69018 = CARTESIAN_POINT('Ctrl Pts',(-18.4209855121877,36.0682825423183,124.550028242115)) ;
#69019 = CARTESIAN_POINT('Ctrl Pts',(-18.6186460335251,35.8882934619554,124.322389261554)) ;
#69020 = CARTESIAN_POINT('Ctrl Pts',(-18.2382837456184,36.0782741896657,124.361434085726)) ;
#69021 = CARTESIAN_POINT('Ctrl Pts',(-18.4724839618908,35.8982851093029,124.17151478619)) ;
#69022 = CARTESIAN_POINT('Ctrl Pts',(-18.0909304837619,36.0883087131035,124.142763989122)) ;
#69023 = CARTESIAN_POINT('Ctrl Pts',(-18.3546005264068,35.9083196327406,123.996579163665)) ;
#69024 = CARTESIAN_POINT('Ctrl Pts',(-17.9851026047473,36.0981720699821,123.906123266323)) ;
#69025 = CARTESIAN_POINT('Ctrl Pts',(-18.2699376258738,35.9181829896192,123.807267861114)) ;
#69026 = CARTESIAN_POINT('Ctrl Pts',(-17.9206102595099,36.1082422966624,123.649496524002)) ;
#69027 = CARTESIAN_POINT('Ctrl Pts',(-18.2183426310434,35.9282532162995,123.601966434206)) ;
#69028 = CARTESIAN_POINT('Ctrl Pts',(-17.9020958099089,36.1180846047971,123.391502808904)) ;
#69029 = CARTESIAN_POINT('Ctrl Pts',(-18.2035300751442,35.9380955244342,123.39557257472)) ;
#69030 = CARTESIAN_POINT('Ctrl Pts',(-17.9280157514707,36.1280453368205,123.131037798645)) ;
#69031 = CARTESIAN_POINT('Ctrl Pts',(-18.2242647137395,35.9480562564576,123.187200762251)) ;
#69032 = CARTESIAN_POINT('Ctrl Pts',(-17.999816726095,36.1380832260186,122.877221984986)) ;
#69033 = CARTESIAN_POINT('Ctrl Pts',(-18.2817043938246,35.9580941456557,122.984147689638)) ;
#69034 = CARTESIAN_POINT('Ctrl Pts',(-18.1123123668843,36.1479575089374,122.643353698666)) ;
#69035 = CARTESIAN_POINT('Ctrl Pts',(-18.3716994042814,35.9679684285746,122.797053236207)) ;
#69036 = CARTESIAN_POINT('Ctrl Pts',(-18.2666755578384,36.1580272535549,122.428462610188)) ;
#69037 = CARTESIAN_POINT('Ctrl Pts',(-18.4951890841048,35.978038173192,122.625139394901)) ;
#69038 = CARTESIAN_POINT('Ctrl Pts',(-18.4515040641022,36.1678605639005,122.247839904849)) ;
#69039 = CARTESIAN_POINT('Ctrl Pts',(-18.6430502466827,35.9878714835377,122.480641013743)) ;
#69040 = CARTESIAN_POINT('Ctrl Pts',(-18.6687131962433,36.1778908072532,122.098528505516)) ;
#69041 = CARTESIAN_POINT('Ctrl Pts',(-18.8168167817684,35.9979017268903,122.361190651918)) ;
#69042 = CARTESIAN_POINT('Ctrl Pts',(-18.9089342117129,36.1879230952316,121.98989079608)) ;
#69043 = CARTESIAN_POINT('Ctrl Pts',(-19.0089931242432,36.0079340148687,122.274279275505)) ;
#69044 = CARTESIAN_POINT('Ctrl Pts',(-19.1589917224903,36.1977502716997,121.925355327248)) ;
#69045 = CARTESIAN_POINT('Ctrl Pts',(-19.2090377774814,36.0177611913368,122.222649778263)) ;
#69046 = CARTESIAN_POINT('Ctrl Pts',(-19.4210472098018,36.2077556545666,121.904313326992)) ;
#69047 = CARTESIAN_POINT('Ctrl Pts',(-19.4186819756106,36.0277665742037,122.205814653997)) ;
#69048 = CARTESIAN_POINT('Ctrl Pts',(-19.6822546897857,36.2177382935593,121.929130110005)) ;
#69049 = CARTESIAN_POINT('Ctrl Pts',(-19.6276479311042,36.0377492131964,122.225666559862)) ;
#69050 = CARTESIAN_POINT('Ctrl Pts',(-19.9365810271852,36.2277823606959,121.999644910744)) ;
#69051 = CARTESIAN_POINT('Ctrl Pts',(-19.8311095076827,36.047793280333,122.282077034315)) ;
#69052 = CARTESIAN_POINT('Ctrl Pts',(-20.1697398906336,36.2376035794999,122.110337795579)) ;
#69053 = CARTESIAN_POINT('Ctrl Pts',(-20.0176363566891,36.057614499137,122.370629526365)) ;
#69054 = CARTESIAN_POINT('Ctrl Pts',(-20.3851350977547,36.247640418438,122.262557053081)) ;
#69055 = CARTESIAN_POINT('Ctrl Pts',(-20.1899535516625,36.0676513380751,122.492403621598)) ;
#69056 = CARTESIAN_POINT('Ctrl Pts',(-20.5700735002195,36.2576648305357,122.450169309994)) ;
#69057 = CARTESIAN_POINT('Ctrl Pts',(-20.3379053729967,36.0776757501728,122.64249237106)) ;
#69058 = CARTESIAN_POINT('Ctrl Pts',(-20.7175254012894,36.267516914941,122.662985785925)) ;
#69059 = CARTESIAN_POINT('Ctrl Pts',(-20.4558677751605,36.0875278345781,122.812743960038)) ;
#69060 = CARTESIAN_POINT('Ctrl Pts',(-20.827658912847,36.2775078116842,122.901285416374)) ;
#69061 = CARTESIAN_POINT('Ctrl Pts',(-20.5439760743343,36.0975187313213,123.003382825012)) ;
#69062 = CARTESIAN_POINT('Ctrl Pts',(-20.894433698142,36.2874258035851,123.153253367672)) ;
#69063 = CARTESIAN_POINT('Ctrl Pts',(-20.597397457909,36.1074367232222,123.204956301286)) ;
#69064 = CARTESIAN_POINT('Ctrl Pts',(-20.9167470714456,36.2974539190421,123.415814568147)) ;
#69065 = CARTESIAN_POINT('Ctrl Pts',(-20.6152498951296,36.1174648386792,123.415005141595)) ;
#69066 = CARTESIAN_POINT('Ctrl Pts',(-20.8935762347595,36.3073390949842,123.674557784478)) ;
#69067 = CARTESIAN_POINT('Ctrl Pts',(-20.5967150310461,36.1273500146213,123.621999285867)) ;
#69068 = CARTESIAN_POINT('Ctrl Pts',(-20.8257335492576,36.3173284533911,123.928155184694)) ;
#69069 = CARTESIAN_POINT('Ctrl Pts',(-20.5424427145472,36.1373393730282,123.824877566207)) ;
#69070 = CARTESIAN_POINT('Ctrl Pts',(-20.7138111338408,36.3273696009714,124.167113009814)) ;
#69071 = CARTESIAN_POINT('Ctrl Pts',(-20.4529063575782,36.1473805206085,124.016044644643)) ;
#69072 = CARTESIAN_POINT('Ctrl Pts',(-20.5656005075822,36.3372022239778,124.378768633685)) ;
#69073 = CARTESIAN_POINT('Ctrl Pts',(-20.334339803994,36.157213143615,124.185369574841)) ;
#69074 = CARTESIAN_POINT('Ctrl Pts',(-20.3804184420739,36.3471962950886,124.564996698335)) ;
#69075 = CARTESIAN_POINT('Ctrl Pts',(-20.1861956033881,36.1672072147257,124.334353335145)) ;
#69076 = CARTESIAN_POINT('Ctrl Pts',(-20.1646550508293,36.3572249527295,124.716351716207)) ;
#69077 = CARTESIAN_POINT('Ctrl Pts',(-20.013585958757,36.1772358723666,124.455438891468)) ;
#69078 = CARTESIAN_POINT('Ctrl Pts',(-19.9294697798766,36.3671092789223,124.82658534845)) ;
#69079 = CARTESIAN_POINT('Ctrl Pts',(-19.8254390212486,36.1871201985594,124.543627316612)) ;
#69080 = CARTESIAN_POINT('Ctrl Pts',(-19.6767994745705,36.3770750224129,124.895495364823)) ;
#69081 = CARTESIAN_POINT('Ctrl Pts',(-19.6233034862338,36.19708594205,124.598757213134)) ;
#69082 = CARTESIAN_POINT('Ctrl Pts',(-19.4143489319624,36.3871034015441,124.91925636217)) ;
#69083 = CARTESIAN_POINT('Ctrl Pts',(-19.4133432160735,36.2071143211812,124.617767958243)) ;
#69084 = CARTESIAN_POINT('Ctrl Pts',(-19.1550206095445,36.397004247751,124.897758003346)) ;
#69085 = CARTESIAN_POINT('Ctrl Pts',(-19.2058807986506,36.2170151673881,124.600571300824)) ;
#69086 = CARTESIAN_POINT('Ctrl Pts',(-18.8994442732755,36.4070629051681,124.830453416065)) ;
#69087 = CARTESIAN_POINT('Ctrl Pts',(-19.0014191286445,36.2270738248052,124.546729537339)) ;
#69088 = CARTESIAN_POINT('Ctrl Pts',(-18.6640416210879,36.41692046795,124.722218749263)) ;
#69089 = CARTESIAN_POINT('Ctrl Pts',(-18.8130966335472,36.2369313875871,124.460143863879)) ;
#69090 = CARTESIAN_POINT('Ctrl Pts',(-18.4464240794683,36.4269888705032,124.571792635111)) ;
#69091 = CARTESIAN_POINT('Ctrl Pts',(-18.6390013333269,36.2469997901403,124.339804589422)) ;
#69092 = CARTESIAN_POINT('Ctrl Pts',(-18.2621870024575,36.4368442692428,124.389737932051)) ;
#69093 = CARTESIAN_POINT('Ctrl Pts',(-18.4916105893428,36.2568551888799,124.194162632583)) ;
#69094 = CARTESIAN_POINT('Ctrl Pts',(-18.1096139658518,36.4468391363167,124.175952224907)) ;
#69095 = CARTESIAN_POINT('Ctrl Pts',(-18.3695504720034,36.2668500559538,124.023135369185)) ;
#69096 = CARTESIAN_POINT('Ctrl Pts',(-17.9965739248701,36.4568704313002,123.937801266144)) ;
#69097 = CARTESIAN_POINT('Ctrl Pts',(-18.2791165693549,36.2768813509373,123.832615491336)) ;
#69098 = CARTESIAN_POINT('Ctrl Pts',(-17.9273507223424,36.4667369560267,123.68792118455)) ;
#69099 = CARTESIAN_POINT('Ctrl Pts',(-18.2237360813941,36.2867478756638,123.632712386933)) ;
#69100 = CARTESIAN_POINT('Ctrl Pts',(-17.9018470654154,36.4767244267224,123.426734881173)) ;
#69101 = CARTESIAN_POINT('Ctrl Pts',(-18.2033310225224,36.2967353463596,123.423763651116)) ;
#69102 = CARTESIAN_POINT('Ctrl Pts',(-17.9218551058738,36.4866691862863,123.166123729046)) ;
#69103 = CARTESIAN_POINT('Ctrl Pts',(-18.2193352864995,36.3066801059234,123.215274750521)) ;
#69104 = CARTESIAN_POINT('Ctrl Pts',(-17.9876098911621,36.4967147422351,122.910487765929)) ;
#69105 = CARTESIAN_POINT('Ctrl Pts',(-18.2719370358106,36.3167256618723,123.010765429301)) ;
#69106 = CARTESIAN_POINT('Ctrl Pts',(-18.0945065089563,36.5065743306102,122.674433491217)) ;
#69107 = CARTESIAN_POINT('Ctrl Pts',(-18.3574522130804,36.3265852502474,122.821921426848)) ;
#69108 = CARTESIAN_POINT('Ctrl Pts',(-18.2424940102238,36.5165752857463,122.457296954355)) ;
#69109 = CARTESIAN_POINT('Ctrl Pts',(-18.4758403558108,36.3365862053834,122.648211013651)) ;
#69110 = CARTESIAN_POINT('Ctrl Pts',(-18.4240741922966,36.5264795130239,122.270772500049)) ;
#69111 = CARTESIAN_POINT('Ctrl Pts',(-18.6211027732019,36.346490432661,122.498990059894)) ;
#69112 = CARTESIAN_POINT('Ctrl Pts',(-18.6381179777294,36.536521589919,122.116476705951)) ;
#69113 = CARTESIAN_POINT('Ctrl Pts',(-18.7923365002083,36.3565325095561,122.375551632485)) ;
#69114 = CARTESIAN_POINT('Ctrl Pts',(-18.8725385168482,36.5464292026052,122.003075302597)) ;
#69115 = CARTESIAN_POINT('Ctrl Pts',(-18.979871801407,36.3664401222423,122.284828592145)) ;
#69116 = CARTESIAN_POINT('Ctrl Pts',(-19.1267156102874,36.5564837332209,121.931052177972)) ;
#69117 = CARTESIAN_POINT('Ctrl Pts',(-19.1832128661274,36.376494652858,122.227207955336)) ;
#69118 = CARTESIAN_POINT('Ctrl Pts',(-19.3845283469667,36.5663445197698,121.904614760594)) ;
#69119 = CARTESIAN_POINT('Ctrl Pts',(-19.3894626144026,36.3863554394069,122.206055828326)) ;
#69120 = CARTESIAN_POINT('Ctrl Pts',(-19.646459660601,36.5763382748409,121.923105823683)) ;
#69121 = CARTESIAN_POINT('Ctrl Pts',(-19.5990077631151,36.396349194478,122.220846431411)) ;
#69122 = CARTESIAN_POINT('Ctrl Pts',(-19.8995693751158,36.5862636350808,121.986256533974)) ;
#69123 = CARTESIAN_POINT('Ctrl Pts',(-19.8014959764349,36.406274554718,122.271364795615)) ;
#69124 = CARTESIAN_POINT('Ctrl Pts',(-20.1402663825485,36.5962915644761,122.093453651258)) ;
#69125 = CARTESIAN_POINT('Ctrl Pts',(-19.9940544515842,36.4163024841132,122.357120413461)) ;
#69126 = CARTESIAN_POINT('Ctrl Pts',(-20.3558196617263,36.6061778312754,122.23855197328)) ;
#69127 = CARTESIAN_POINT('Ctrl Pts',(-20.1664982539507,36.4261887509125,122.473197150911)) ;
#69128 = CARTESIAN_POINT('Ctrl Pts',(-20.5456928031172,36.6162096001737,122.421371062193)) ;
#69129 = CARTESIAN_POINT('Ctrl Pts',(-20.3183982921077,36.4362205198108,122.619450762827)) ;
#69130 = CARTESIAN_POINT('Ctrl Pts',(-20.6988722845905,36.6260911960173,122.631115950227)) ;
#69131 = CARTESIAN_POINT('Ctrl Pts',(-20.4409436684768,36.4461021156544,122.787245289088)) ;
#69132 = CARTESIAN_POINT('Ctrl Pts',(-20.815415738362,36.6361530814852,122.868418182703)) ;
#69133 = CARTESIAN_POINT('Ctrl Pts',(-20.5341804158425,36.4561640011224,122.97708607685)) ;
#69134 = CARTESIAN_POINT('Ctrl Pts',(-20.8875930298801,36.6460105155041,123.11723735423)) ;
#69135 = CARTESIAN_POINT('Ctrl Pts',(-20.5919244479909,36.4660214351412,123.176140562993)) ;
#69136 = CARTESIAN_POINT('Ctrl Pts',(-20.9163988743177,36.6560037585461,123.37823043788)) ;
#69137 = CARTESIAN_POINT('Ctrl Pts',(-20.6149712081136,36.4760146781832,123.384935555596)) ;
#69138 = CARTESIAN_POINT('Ctrl Pts',(-20.8995719078508,36.6659345194324,123.638673612031)) ;
#69139 = CARTESIAN_POINT('Ctrl Pts',(-20.6015124065235,36.4859454390695,123.593287223642)) ;
#69140 = CARTESIAN_POINT('Ctrl Pts',(-20.8168446966216,36.6792835116296,123.979609103864)) ;
#69141 = CARTESIAN_POINT('Ctrl Pts',(-20.535330876497,36.4992944312667,123.866051291918)) ;
#69142 = CARTESIAN_POINT('Ctrl Pts',(-20.6476556408436,36.692551884446,124.288994177467)) ;
#69143 = CARTESIAN_POINT('Ctrl Pts',(-20.3999608846557,36.5125628040832,124.113578703363)) ;
#69144 = CARTESIAN_POINT('Ctrl Pts',(-20.4070652076398,36.7058348258304,124.541941671544)) ;
#69145 = CARTESIAN_POINT('Ctrl Pts',(-20.2075187930554,36.5258457454675,124.31590241707)) ;
#69146 = CARTESIAN_POINT('Ctrl Pts',(-20.1946380684897,36.7158776116726,124.698516250031)) ;
#69147 = CARTESIAN_POINT('Ctrl Pts',(-20.0375727496872,36.5358885313097,124.441171067068)) ;
#69148 = CARTESIAN_POINT('Ctrl Pts',(-19.9628921814832,36.7257275542247,124.813842499232)) ;
#69149 = CARTESIAN_POINT('Ctrl Pts',(-19.8521787603597,36.5457384738618,124.53343231864)) ;
#69150 = CARTESIAN_POINT('Ctrl Pts',(-19.7111366687982,36.7357247871437,124.888900023742)) ;
#69151 = CARTESIAN_POINT('Ctrl Pts',(-19.6507730800588,36.5557357067808,124.593480421543)) ;
#69152 = CARTESIAN_POINT('Ctrl Pts',(-19.4496388355441,36.7457396824782,124.918754107173)) ;
#69153 = CARTESIAN_POINT('Ctrl Pts',(-19.4415808798337,36.5657506021153,124.617367625246)) ;
#69154 = CARTESIAN_POINT('Ctrl Pts',(-19.1023419164485,36.7589793591164,124.897941856105)) ;
#69155 = CARTESIAN_POINT('Ctrl Pts',(-19.163714991499,36.5789902787535,124.600711280948)) ;
#69156 = CARTESIAN_POINT('Ctrl Pts',(-18.6847931249913,36.7755265835217,124.759912521952)) ;
#69157 = CARTESIAN_POINT('Ctrl Pts',(-18.8297169408902,36.5955375031589,124.490312244877)) ;
#69158 = CARTESIAN_POINT('Ctrl Pts',(-18.3371603330514,36.7921740206528,124.486198909286)) ;
#69159 = CARTESIAN_POINT('Ctrl Pts',(-18.5515569759396,36.6121849402899,124.27129948126)) ;
#69160 = CARTESIAN_POINT('Ctrl Pts',(-18.1282776888068,36.805463518131,124.206288377136)) ;
#69161 = CARTESIAN_POINT('Ctrl Pts',(-18.3844875071243,36.6254744377682,124.047410080626)) ;
#69162 = CARTESIAN_POINT('Ctrl Pts',(-18.0108710102114,36.8153369259534,123.974907927257)) ;
#69163 = CARTESIAN_POINT('Ctrl Pts',(-18.2905523869042,36.6353478455905,123.86229865506)) ;
#69164 = CARTESIAN_POINT('Ctrl Pts',(-17.9340138084422,36.8253893035461,123.722181735766)) ;
#69165 = CARTESIAN_POINT('Ctrl Pts',(-18.2290667220401,36.6454002231832,123.660120782758)) ;
#69166 = CARTESIAN_POINT('Ctrl Pts',(-17.9027830695279,36.835292957087,123.463785283055)) ;
#69167 = CARTESIAN_POINT('Ctrl Pts',(-18.2040801107792,36.6553038767241,123.453402008484)) ;
#69168 = CARTESIAN_POINT('Ctrl Pts',(-17.9163185741068,36.8452372260823,123.20284412538)) ;
#69169 = CARTESIAN_POINT('Ctrl Pts',(-18.2149045717325,36.6652481457194,123.244652494399)) ;
#69170 = CARTESIAN_POINT('Ctrl Pts',(-17.9947816309639,36.858568234415,122.86134409118)) ;
#69171 = CARTESIAN_POINT('Ctrl Pts',(-18.2776833949051,36.6785791540521,122.971434015951)) ;
#69172 = CARTESIAN_POINT('Ctrl Pts',(-18.2021201495934,36.8751898149393,122.471324046481)) ;
#69173 = CARTESIAN_POINT('Ctrl Pts',(-18.4435276248863,36.6952007345764,122.65944458022)) ;
#69174 = CARTESIAN_POINT('Ctrl Pts',(-18.5280140338344,36.8917324856377,122.176159129624)) ;
#69175 = CARTESIAN_POINT('Ctrl Pts',(-18.7042903718315,36.7117434052748,122.423272175924)) ;
#69176 = CARTESIAN_POINT('Ctrl Pts',(-18.8400831149496,36.9050816452006,122.015936356967)) ;
#69177 = CARTESIAN_POINT('Ctrl Pts',(-18.9539021452591,36.7250925648377,122.295120890868)) ;
#69178 = CARTESIAN_POINT('Ctrl Pts',(-19.1721122727388,36.9183097953601,121.912858361427)) ;
#69179 = CARTESIAN_POINT('Ctrl Pts',(-19.2195445013812,36.7383207149972,122.212649893044)) ;
#69180 = CARTESIAN_POINT('Ctrl Pts',(-19.6137036972869,36.9349404724976,121.895030598863)) ;
#69181 = CARTESIAN_POINT('Ctrl Pts',(-19.5728023332913,36.7549513921347,122.198387296976)) ;
#69182 = CARTESIAN_POINT('Ctrl Pts',(-20.1178689307979,36.9548434117857,122.055389405996)) ;
#69183 = CARTESIAN_POINT('Ctrl Pts',(-19.9761410205625,36.7748543314228,122.326670629609)) ;
#69184 = CARTESIAN_POINT('Ctrl Pts',(-20.5372508618261,36.974746278389,122.377628584719)) ;
#69185 = CARTESIAN_POINT('Ctrl Pts',(-20.3116476493232,36.7947571980261,122.584460225814)) ;
#69186 = CARTESIAN_POINT('Ctrl Pts',(-20.8224429652518,36.9946594434938,122.823616943194)) ;
#69187 = CARTESIAN_POINT('Ctrl Pts',(-20.5398042577158,36.8146703631309,122.941249965246)) ;
#69188 = CARTESIAN_POINT('Ctrl Pts',(-20.9381837029395,37.0146952726351,123.343330198138)) ;
#69189 = CARTESIAN_POINT('Ctrl Pts',(-20.6323994047383,36.8347061922723,123.357019653058)) ;
#69190 = CARTESIAN_POINT('Ctrl Pts',(-20.870660430698,37.0345138475132,123.865857791706)) ;
#69191 = CARTESIAN_POINT('Ctrl Pts',(-20.5783831490658,36.8545247671503,123.775043510851)) ;
#69192 = CARTESIAN_POINT('Ctrl Pts',(-20.6279168053025,37.0544841485552,124.337676429547)) ;
#69193 = CARTESIAN_POINT('Ctrl Pts',(-20.3841900155139,36.8744950681923,124.152499694084)) ;
#69194 = CARTESIAN_POINT('Ctrl Pts',(-20.2401177850533,37.0743756809197,124.697290350133)) ;
#69195 = CARTESIAN_POINT('Ctrl Pts',(-20.0739513811675,36.8943866005569,124.440192902116)) ;
#69196 = CARTESIAN_POINT('Ctrl Pts',(-19.7497910668488,37.0943987787363,124.90385539926)) ;
#69197 = CARTESIAN_POINT('Ctrl Pts',(-19.6816909775682,36.9144096983734,124.60544662509)) ;
#69198 = CARTESIAN_POINT('Ctrl Pts',(-19.2242516782472,37.1141955316562,124.930779156354)) ;
#69199 = CARTESIAN_POINT('Ctrl Pts',(-19.2612574376801,36.9342064512933,124.626987358956)) ;
#69200 = CARTESIAN_POINT('Ctrl Pts',(-18.7165851062784,37.134156620145,124.77686253658)) ;
#69201 = CARTESIAN_POINT('Ctrl Pts',(-18.8551234525687,36.9541675397821,124.503854730213)) ;
#69202 = CARTESIAN_POINT('Ctrl Pts',(-18.2921431805836,37.1541348890772,124.457730120068)) ;
#69203 = CARTESIAN_POINT('Ctrl Pts',(-18.5155690830116,36.9741458087143,124.24854960687)) ;
#69204 = CARTESIAN_POINT('Ctrl Pts',(-18.0037890981737,37.1739549038682,124.016935959716)) ;
#69205 = CARTESIAN_POINT('Ctrl Pts',(-18.2848840606162,36.9939658235053,123.89591275192)) ;
#69206 = CARTESIAN_POINT('Ctrl Pts',(-17.8810922820256,37.19389331312,123.50137832524)) ;
#69207 = CARTESIAN_POINT('Ctrl Pts',(-18.1867266714987,37.0139042327571,123.483465809288)) ;
#69208 = CARTESIAN_POINT('Ctrl Pts',(-17.9432206011059,37.2139404305124,122.97212475137)) ;
#69209 = CARTESIAN_POINT('Ctrl Pts',(-18.2364291043745,37.0339513501496,123.06006363056)) ;
#69210 = CARTESIAN_POINT('Ctrl Pts',(-18.1799938362226,37.2337866763463,122.500836491877)) ;
#69211 = CARTESIAN_POINT('Ctrl Pts',(-18.4258485917207,37.0537975959834,122.683031144881)) ;
#69212 = CARTESIAN_POINT('Ctrl Pts',(-18.5620635941251,37.2536356448583,122.137020325925)) ;
#69213 = CARTESIAN_POINT('Ctrl Pts',(-18.7315064596815,37.0736465644954,122.391977845995)) ;
#69214 = CARTESIAN_POINT('Ctrl Pts',(-19.0504528465872,37.2736859471696,121.923931865139)) ;
#69215 = CARTESIAN_POINT('Ctrl Pts',(-19.1222177233639,37.0936968668067,122.221508236812)) ;
#69216 = CARTESIAN_POINT('Ctrl Pts',(-19.5767155011093,37.2935208696008,121.890757346003)) ;
#69217 = CARTESIAN_POINT('Ctrl Pts',(-19.5432297263916,37.113531789238,122.194969649968)) ;
#69218 = CARTESIAN_POINT('Ctrl Pts',(-20.08511494409,37.3134512708267,122.038788804448)) ;
#69219 = CARTESIAN_POINT('Ctrl Pts',(-19.9499495172448,37.1334621904638,122.313396725135)) ;
#69220 = CARTESIAN_POINT('Ctrl Pts',(-20.5122328950149,37.3333362161856,122.35040788788)) ;
#69221 = CARTESIAN_POINT('Ctrl Pts',(-20.2916434333738,37.1533471358227,122.562694298399)) ;
#69222 = CARTESIAN_POINT('Ctrl Pts',(-20.8092661802658,37.353408824337,122.793446550335)) ;
#69223 = CARTESIAN_POINT('Ctrl Pts',(-20.5292680326244,37.1734197439741,122.917125764005)) ;
#69224 = CARTESIAN_POINT('Ctrl Pts',(-20.9356180404718,37.3732001406651,123.304147384377)) ;
#69225 = CARTESIAN_POINT('Ctrl Pts',(-20.6303478832511,37.1932110603022,123.325688757585)) ;
#69226 = CARTESIAN_POINT('Ctrl Pts',(-20.8812658706226,37.3931649304323,123.8319433124)) ;
#69227 = CARTESIAN_POINT('Ctrl Pts',(-20.5868633031295,37.2131758500695,123.747925458238)) ;
#69228 = CARTESIAN_POINT('Ctrl Pts',(-20.6486375255731,37.4131478861826,124.309410738548)) ;
#69229 = CARTESIAN_POINT('Ctrl Pts',(-20.4007582836289,37.2331588058198,124.129898402551)) ;
#69230 = CARTESIAN_POINT('Ctrl Pts',(-20.2710983170399,37.4329564081588,124.676413569009)) ;
#69231 = CARTESIAN_POINT('Ctrl Pts',(-20.0987238439308,37.2529673277959,124.423499492388)) ;
#69232 = CARTESIAN_POINT('Ctrl Pts',(-19.7870846025984,37.4529419828946,124.894968051368)) ;
#69233 = CARTESIAN_POINT('Ctrl Pts',(-19.7115114515686,37.2729529025317,124.598340127017)) ;
#69234 = CARTESIAN_POINT('Ctrl Pts',(-19.2600251516879,37.472824622963,124.934935958172)) ;
#69235 = CARTESIAN_POINT('Ctrl Pts',(-19.2898629599609,37.2928355426001,124.630311187914)) ;
#69236 = CARTESIAN_POINT('Ctrl Pts',(-18.7492134555832,37.4927799350949,124.792594096249)) ;
#69237 = CARTESIAN_POINT('Ctrl Pts',(-18.8812143169606,37.312790854732,124.516434239319)) ;
#69238 = CARTESIAN_POINT('Ctrl Pts',(-18.319033254551,37.5126542917027,124.485894779788)) ;
#69239 = CARTESIAN_POINT('Ctrl Pts',(-18.5370718339478,37.3326652113398,124.27107140888)) ;
#69240 = CARTESIAN_POINT('Ctrl Pts',(-18.0175106060064,37.5326364985638,124.048765115388)) ;
#69241 = CARTESIAN_POINT('Ctrl Pts',(-18.2958567266438,37.3526474182009,123.921365577981)) ;
#69242 = CARTESIAN_POINT('Ctrl Pts',(-17.8838308617942,37.5525675765137,123.536059048149)) ;
#69243 = CARTESIAN_POINT('Ctrl Pts',(-18.1889170443655,37.3725784961509,123.5111991052)) ;
#69244 = CARTESIAN_POINT('Ctrl Pts',(-17.9330320754365,37.5724945513687,123.008830582015)) ;
#69245 = CARTESIAN_POINT('Ctrl Pts',(-18.2282802580598,37.3925054710058,123.089417886411)) ;
#69246 = CARTESIAN_POINT('Ctrl Pts',(-18.157254622848,37.5923270103176,122.531709623646)) ;
#69247 = CARTESIAN_POINT('Ctrl Pts',(-18.4076687041876,37.4123379299547,122.707716901662)) ;
#69248 = CARTESIAN_POINT('Ctrl Pts',(-18.4706659458096,37.6089846944928,122.219158784054)) ;
#69249 = CARTESIAN_POINT('Ctrl Pts',(-18.658380296989,37.4289956141299,122.457695891381)) ;
#69250 = CARTESIAN_POINT('Ctrl Pts',(-18.7724796762074,37.6222339183999,122.045392670349)) ;
#69251 = CARTESIAN_POINT('Ctrl Pts',(-18.8998510804845,37.442244838037,122.318670265349)) ;
#69252 = CARTESIAN_POINT('Ctrl Pts',(-19.0206690089167,37.6322829398511,121.955269929733)) ;
#69253 = CARTESIAN_POINT('Ctrl Pts',(-19.0983967704762,37.4522938594882,122.246576695617)) ;
#69254 = CARTESIAN_POINT('Ctrl Pts',(-19.2758657649021,37.6421429480816,121.910397904174)) ;
#69255 = CARTESIAN_POINT('Ctrl Pts',(-19.3025665790804,37.4621538677187,122.210682152963)) ;
#69256 = CARTESIAN_POINT('Ctrl Pts',(-19.6249794284296,37.6554264613062,121.909413584284)) ;
#69257 = CARTESIAN_POINT('Ctrl Pts',(-19.5818035064809,37.4754373809433,122.20988869481)) ;
#69258 = CARTESIAN_POINT('Ctrl Pts',(-20.0524638778648,37.672072380307,122.023188295616)) ;
#69259 = CARTESIAN_POINT('Ctrl Pts',(-19.9238581002366,37.4920832999442,122.300927565958)) ;
#69260 = CARTESIAN_POINT('Ctrl Pts',(-20.413880776944,37.6886263581231,122.274169668414)) ;
#69261 = CARTESIAN_POINT('Ctrl Pts',(-20.2129442060005,37.5086372777602,122.501691816295)) ;
#69262 = CARTESIAN_POINT('Ctrl Pts',(-20.6406243713132,37.7019860870947,122.542201540504)) ;
#69263 = CARTESIAN_POINT('Ctrl Pts',(-20.3943637147157,37.5219970067318,122.716138256514)) ;
#69264 = CARTESIAN_POINT('Ctrl Pts',(-20.771703979078,37.7118791388914,122.766737576687)) ;
#69265 = CARTESIAN_POINT('Ctrl Pts',(-20.4992200975137,37.5318900585285,122.895764440336)) ;
#69266 = CARTESIAN_POINT('Ctrl Pts',(-20.8630031282262,37.7218691041725,123.012844193469)) ;
#69267 = CARTESIAN_POINT('Ctrl Pts',(-20.5722587448008,37.5418800238096,123.092651501254)) ;
#69268 = CARTESIAN_POINT('Ctrl Pts',(-20.9101691765086,37.7318209850333,123.270122215449)) ;
#69269 = CARTESIAN_POINT('Ctrl Pts',(-20.609988980369,37.5518319046704,123.298474032624)) ;
#69270 = CARTESIAN_POINT('Ctrl Pts',(-20.9117400295103,37.7418693367251,123.534149528085)) ;
#69271 = CARTESIAN_POINT('Ctrl Pts',(-20.6112435209441,37.5618802563622,123.509695891286)) ;
#69272 = CARTESIAN_POINT('Ctrl Pts',(-20.8686496157947,37.7517106208313,123.789179451331)) ;
#69273 = CARTESIAN_POINT('Ctrl Pts',(-20.576768936994,37.5717215404684,123.713719468987)) ;
#69274 = CARTESIAN_POINT('Ctrl Pts',(-20.7811945958756,37.761697323957,124.0365703206)) ;
#69275 = CARTESIAN_POINT('Ctrl Pts',(-20.5068028158722,37.5817082435941,123.911631353683)) ;
#69276 = CARTESIAN_POINT('Ctrl Pts',(-20.6528738763807,37.7716323527744,124.263999794878)) ;
#69277 = CARTESIAN_POINT('Ctrl Pts',(-20.4041443030014,37.5916432724115,124.093573772257)) ;
#69278 = CARTESIAN_POINT('Ctrl Pts',(-20.4848851322175,37.7816881476813,124.467934944113)) ;
#69279 = CARTESIAN_POINT('Ctrl Pts',(-20.2697515895762,37.6016990673184,124.256720420404)) ;
#69280 = CARTESIAN_POINT('Ctrl Pts',(-20.2887835292672,37.7915165109706,124.636074676787)) ;
#69281 = CARTESIAN_POINT('Ctrl Pts',(-20.1128689225267,37.6115274306077,124.391230423038)) ;
#69282 = CARTESIAN_POINT('Ctrl Pts',(-20.0614584855971,37.8015774808685,124.771009318032)) ;
#69283 = CARTESIAN_POINT('Ctrl Pts',(-19.931007771351,37.6215884005056,124.49917617883)) ;
#69284 = CARTESIAN_POINT('Ctrl Pts',(-19.8176275658583,37.8114917597583,124.862882128275)) ;
#69285 = CARTESIAN_POINT('Ctrl Pts',(-19.735942339562,37.6315026793954,124.572672280903)) ;
#69286 = CARTESIAN_POINT('Ctrl Pts',(-19.5592226441299,37.8215007542265,124.911986102219)) ;
#69287 = CARTESIAN_POINT('Ctrl Pts',(-19.5292180435957,37.6415116738637,124.611953245993)) ;
#69288 = CARTESIAN_POINT('Ctrl Pts',(-19.2956698137528,37.8315305887903,124.914944725245)) ;
#69289 = CARTESIAN_POINT('Ctrl Pts',(-19.3183757846655,37.6515415084274,124.614317886194)) ;
#69290 = CARTESIAN_POINT('Ctrl Pts',(-19.0399553923332,37.8413888188625,124.873312424771)) ;
#69291 = CARTESIAN_POINT('Ctrl Pts',(-19.113804794043,37.6613997384997,124.581009863178)) ;
#69292 = CARTESIAN_POINT('Ctrl Pts',(-18.7918216048471,37.8513875246049,124.787014243601)) ;
#69293 = CARTESIAN_POINT('Ctrl Pts',(-18.915298566103,37.6713984442421,124.511969231989)) ;
#69294 = CARTESIAN_POINT('Ctrl Pts',(-18.5645984860679,37.8612821805237,124.660501733372)) ;
#69295 = CARTESIAN_POINT('Ctrl Pts',(-18.7335213311777,37.6812931001609,124.410757393858)) ;
#69296 = CARTESIAN_POINT('Ctrl Pts',(-18.3594834848053,37.8713452449077,124.493660346681)) ;
#69297 = CARTESIAN_POINT('Ctrl Pts',(-18.5694307097895,37.6913561645448,124.277282542542)) ;
#69298 = CARTESIAN_POINT('Ctrl Pts',(-18.1900212161876,37.8811849031876,124.298298757576)) ;
#69299 = CARTESIAN_POINT('Ctrl Pts',(-18.4338627738789,37.7011958228247,124.120992079632)) ;
#69300 = CARTESIAN_POINT('Ctrl Pts',(-18.0537869453756,37.8912480702694,124.071683477115)) ;
#69301 = CARTESIAN_POINT('Ctrl Pts',(-18.3248772081804,37.7112589899066,123.939698699603)) ;
#69302 = CARTESIAN_POINT('Ctrl Pts',(-17.9607436771395,37.9011423153965,123.828859729569)) ;
#69303 = CARTESIAN_POINT('Ctrl Pts',(-18.2504447386895,37.7211532350337,123.745439163456)) ;
#69304 = CARTESIAN_POINT('Ctrl Pts',(-17.9103527062584,37.9110841370011,123.572537760102)) ;
#69305 = CARTESIAN_POINT('Ctrl Pts',(-18.2101341056503,37.7310950566383,123.540381382668)) ;
#69306 = CARTESIAN_POINT('Ctrl Pts',(-17.9051034699468,37.9210866679192,123.309699103469)) ;
#69307 = CARTESIAN_POINT('Ctrl Pts',(-18.2059368477175,37.7410975875563,123.330110481641)) ;
#69308 = CARTESIAN_POINT('Ctrl Pts',(-17.946097783474,37.9311212943767,123.049219622139)) ;
#69309 = CARTESIAN_POINT('Ctrl Pts',(-18.238734443196,37.7511322140138,123.121727220956)) ;
#69310 = CARTESIAN_POINT('Ctrl Pts',(-18.0297012300919,37.9409668293631,122.804359246479)) ;
#69311 = CARTESIAN_POINT('Ctrl Pts',(-18.3056190713924,37.7609777490003,122.925840036189)) ;
#69312 = CARTESIAN_POINT('Ctrl Pts',(-18.1557855280744,37.9509502542022,122.574313582137)) ;
#69313 = CARTESIAN_POINT('Ctrl Pts',(-18.4064882631411,37.7709611738393,122.741804625682)) ;
#69314 = CARTESIAN_POINT('Ctrl Pts',(-18.3194140988036,37.9609006445672,122.370342409505)) ;
#69315 = CARTESIAN_POINT('Ctrl Pts',(-18.5373926050169,37.7809115642044,122.578629156935)) ;
#69316 = CARTESIAN_POINT('Ctrl Pts',(-18.5166838775539,37.9708982848643,122.196785487703)) ;
#69317 = CARTESIAN_POINT('Ctrl Pts',(-18.6952097128482,37.7909092045014,122.439785207195)) ;
#69318 = CARTESIAN_POINT('Ctrl Pts',(-18.7422660732146,37.9809373654275,122.060023983283)) ;
#69319 = CARTESIAN_POINT('Ctrl Pts',(-18.8756765999443,37.8009482850646,122.330377774988)) ;
#69320 = CARTESIAN_POINT('Ctrl Pts',(-18.9827700674646,37.9907635161966,121.965984935098)) ;
#69321 = CARTESIAN_POINT('Ctrl Pts',(-19.068079960445,37.8107744358337,122.255148655797)) ;
#69322 = CARTESIAN_POINT('Ctrl Pts',(-19.2417735141306,38.0008200911257,121.913534414804)) ;
#69323 = CARTESIAN_POINT('Ctrl Pts',(-19.2752831961908,37.8208310107629,122.213190167423)) ;
#69324 = CARTESIAN_POINT('Ctrl Pts',(-19.5029368385389,38.010760630506,121.907384733562)) ;
#69325 = CARTESIAN_POINT('Ctrl Pts',(-19.4842136365279,37.8307715501431,122.20827246862)) ;
#69326 = CARTESIAN_POINT('Ctrl Pts',(-19.7603796758828,38.0206650234824,121.94572645087)) ;
#69327 = CARTESIAN_POINT('Ctrl Pts',(-19.6901671990176,37.8406759431195,122.238947693233)) ;
#69328 = CARTESIAN_POINT('Ctrl Pts',(-20.0107210558662,38.0307116776873,122.029521129623)) ;
#69329 = CARTESIAN_POINT('Ctrl Pts',(-19.8904397605092,37.8507225973244,122.305985318718)) ;
#69330 = CARTESIAN_POINT('Ctrl Pts',(-20.2393912303446,38.0406072396257,122.153437722029)) ;
#69331 = CARTESIAN_POINT('Ctrl Pts',(-20.0733745736591,37.8606181592628,122.405120060761)) ;
#69332 = CARTESIAN_POINT('Ctrl Pts',(-20.4464358604614,38.0506693174713,122.317848314889)) ;
#69333 = CARTESIAN_POINT('Ctrl Pts',(-20.2390091946635,37.8706802371084,122.536650134307)) ;
#69334 = CARTESIAN_POINT('Ctrl Pts',(-20.6181207395519,38.060512015885,122.511348876402)) ;
#69335 = CARTESIAN_POINT('Ctrl Pts',(-20.3763552143861,37.8805229355222,122.691451327068)) ;
#69336 = CARTESIAN_POINT('Ctrl Pts',(-20.7561325943481,38.0705027908465,122.734655821582)) ;
#69337 = CARTESIAN_POINT('Ctrl Pts',(-20.4867630838622,37.8905137104836,122.870097716257)) ;
#69338 = CARTESIAN_POINT('Ctrl Pts',(-20.8526444302202,38.0804306558656,122.977057792993)) ;
#69339 = CARTESIAN_POINT('Ctrl Pts',(-20.5639707221755,37.9004415755027,123.064019601063)) ;
#69340 = CARTESIAN_POINT('Ctrl Pts',(-20.9063538531691,38.0904194006318,123.234003272381)) ;
#69341 = CARTESIAN_POINT('Ctrl Pts',(-20.6069365241512,37.9104303202689,123.269576200659)) ;
#69342 = CARTESIAN_POINT('Ctrl Pts',(-20.9142822162603,38.1004521862187,123.497539173054)) ;
#69343 = CARTESIAN_POINT('Ctrl Pts',(-20.6132774084487,37.9204631058559,123.480405034982)) ;
#69344 = CARTESIAN_POINT('Ctrl Pts',(-20.8772223147212,38.1103188708394,123.754154223928)) ;
#69345 = CARTESIAN_POINT('Ctrl Pts',(-20.5836278397377,37.9303297904765,123.685696137519)) ;
#69346 = CARTESIAN_POINT('Ctrl Pts',(-20.7960987290107,38.1202807630025,124.00306041153)) ;
#69347 = CARTESIAN_POINT('Ctrl Pts',(-20.5187275050565,37.9402916826396,123.884820316478)) ;
#69348 = CARTESIAN_POINT('Ctrl Pts',(-20.6717436692743,38.1303142399151,124.235550043403)) ;
#69349 = CARTESIAN_POINT('Ctrl Pts',(-20.4192419168591,37.9503251595522,124.070811279402)) ;
#69350 = CARTESIAN_POINT('Ctrl Pts',(-20.5116269403932,38.1401985811634,124.440122137364)) ;
#69351 = CARTESIAN_POINT('Ctrl Pts',(-20.291147641117,37.9602095008005,124.2344674478)) ;
#69352 = CARTESIAN_POINT('Ctrl Pts',(-20.3149827227567,38.1502615232845,124.616881340023)) ;
#69353 = CARTESIAN_POINT('Ctrl Pts',(-20.1338310207247,37.9702724429217,124.37587373082)) ;
#69354 = CARTESIAN_POINT('Ctrl Pts',(-20.0953938752767,38.1601119249041,124.75399118927)) ;
#69355 = CARTESIAN_POINT('Ctrl Pts',(-19.9581597997883,37.9801228445412,124.48555979968)) ;
#69356 = CARTESIAN_POINT('Ctrl Pts',(-19.8513087068426,38.1701388136938,124.853234002042)) ;
#69357 = CARTESIAN_POINT('Ctrl Pts',(-19.7628910767466,37.9901497333309,124.564952686841)) ;
#69358 = CARTESIAN_POINT('Ctrl Pts',(-19.593491376287,38.18016742865,124.907926696643)) ;
#69359 = CARTESIAN_POINT('Ctrl Pts',(-19.5566368221853,38.0001783482871,124.60870527169)) ;
#69360 = CARTESIAN_POINT('Ctrl Pts',(-19.3349545228551,38.19001265177,124.917345289566)) ;
#69361 = CARTESIAN_POINT('Ctrl Pts',(-19.3498081794795,38.0100235714072,124.616238591865)) ;
#69362 = CARTESIAN_POINT('Ctrl Pts',(-19.0748065717966,38.200003335576,124.88189910921)) ;
#69363 = CARTESIAN_POINT('Ctrl Pts',(-19.1416901604654,38.0200142552131,124.587880298934)) ;
#69364 = CARTESIAN_POINT('Ctrl Pts',(-18.8237728136893,38.2100412176484,124.80088615643)) ;
#69365 = CARTESIAN_POINT('Ctrl Pts',(-18.9408635131046,38.0300521372856,124.52306847567)) ;
#69366 = CARTESIAN_POINT('Ctrl Pts',(-18.5948907896328,38.2198855772873,124.680287851483)) ;
#69367 = CARTESIAN_POINT('Ctrl Pts',(-18.7577593811284,38.0398964969244,124.426589023562)) ;
#69368 = CARTESIAN_POINT('Ctrl Pts',(-18.3872272286847,38.229870447902,124.519955106578)) ;
#69369 = CARTESIAN_POINT('Ctrl Pts',(-18.5916294861403,38.0498813675391,124.298321919019)) ;
#69370 = CARTESIAN_POINT('Ctrl Pts',(-18.2112252563883,38.2398097312307,124.326911572828)) ;
#69371 = CARTESIAN_POINT('Ctrl Pts',(-18.4508291441772,38.0598206508678,124.143886556018)) ;
#69372 = CARTESIAN_POINT('Ctrl Pts',(-18.0700954992362,38.2498503406038,124.104002776353)) ;
#69373 = CARTESIAN_POINT('Ctrl Pts',(-18.3379263671355,38.0698612602409,123.9655587244)) ;
#69374 = CARTESIAN_POINT('Ctrl Pts',(-17.9711690914586,38.259735191517,123.863780801288)) ;
#69375 = CARTESIAN_POINT('Ctrl Pts',(-18.2587866856612,38.0797461111542,123.773381363225)) ;
#69376 = CARTESIAN_POINT('Ctrl Pts',(-17.9145022539865,38.2697371476858,123.607161518794)) ;
#69377 = CARTESIAN_POINT('Ctrl Pts',(-18.2134543961033,38.089748067323,123.568085793676)) ;
#69378 = CARTESIAN_POINT('Ctrl Pts',(-17.9031351939843,38.2796557444063,123.34671741945)) ;
#69379 = CARTESIAN_POINT('Ctrl Pts',(-18.2043619071338,38.0996666640434,123.359731038019)) ;
#69380 = CARTESIAN_POINT('Ctrl Pts',(-17.9376431227796,38.2897025664821,123.084999919376)) ;
#69381 = CARTESIAN_POINT('Ctrl Pts',(-18.2319694141101,38.1097134861192,123.150357019419)) ;
#69382 = CARTESIAN_POINT('Ctrl Pts',(-18.0154975116536,38.2995768475948,122.837421943665)) ;
#69383 = CARTESIAN_POINT('Ctrl Pts',(-18.2942537162335,38.1195877672319,122.95229576589)) ;
#69384 = CARTESIAN_POINT('Ctrl Pts',(-18.1371535108144,38.3096310476394,122.602934129142)) ;
#69385 = CARTESIAN_POINT('Ctrl Pts',(-18.391579553754,38.1296419672765,122.764705818433)) ;
#69386 = CARTESIAN_POINT('Ctrl Pts',(-18.2951140075871,38.3195264772746,122.396304412918)) ;
#69387 = CARTESIAN_POINT('Ctrl Pts',(-18.5179483256354,38.1395373969118,122.599403261707)) ;
#69388 = CARTESIAN_POINT('Ctrl Pts',(-18.489664634007,38.329588105592,122.217293421697)) ;
#69389 = CARTESIAN_POINT('Ctrl Pts',(-18.6735897116982,38.1495990252291,122.456195042217)) ;
#69390 = CARTESIAN_POINT('Ctrl Pts',(-18.7075571482892,38.3394327344219,122.077804596519)) ;
#69391 = CARTESIAN_POINT('Ctrl Pts',(-18.8479033795345,38.159443654059,122.344605407475)) ;
#69392 = CARTESIAN_POINT('Ctrl Pts',(-18.9487829946581,38.3493927820275,121.976237815657)) ;
#69393 = CARTESIAN_POINT('Ctrl Pts',(-19.0408840272685,38.1694037016646,122.26335285546)) ;
#69394 = CARTESIAN_POINT('Ctrl Pts',(-19.2060908983608,38.3594310882016,121.918149353435)) ;
#69395 = CARTESIAN_POINT('Ctrl Pts',(-19.2467306787397,38.1794420078387,122.216882950581)) ;
#69396 = CARTESIAN_POINT('Ctrl Pts',(-19.4652741750424,38.3693043876342,121.905324657195)) ;
#69397 = CARTESIAN_POINT('Ctrl Pts',(-19.4540764400432,38.1893153072714,122.206624032452)) ;
#69398 = CARTESIAN_POINT('Ctrl Pts',(-19.7278563927704,38.3793776492205,121.938426707961)) ;
#69399 = CARTESIAN_POINT('Ctrl Pts',(-19.6641424513348,38.1993885688576,122.233106527423)) ;
#69400 = CARTESIAN_POINT('Ctrl Pts',(-19.9745595742938,38.3891978751772,122.014360134831)) ;
#69401 = CARTESIAN_POINT('Ctrl Pts',(-19.8615035911148,38.2092087948143,122.293853602793)) ;
#69402 = CARTESIAN_POINT('Ctrl Pts',(-20.2103785146625,38.3992769391167,122.134809378916)) ;
#69403 = CARTESIAN_POINT('Ctrl Pts',(-20.0501587726125,38.2192878587538,122.390213775036)) ;
#69404 = CARTESIAN_POINT('Ctrl Pts',(-20.4170842341087,38.4091270291365,122.29073495999)) ;
#69405 = CARTESIAN_POINT('Ctrl Pts',(-20.2155221090438,38.2291379487737,122.514954115043)) ;
#69406 = CARTESIAN_POINT('Ctrl Pts',(-20.5976790049717,38.4192057827503,122.484385049267)) ;
#69407 = CARTESIAN_POINT('Ctrl Pts',(-20.359997738072,38.2392167023874,122.669874889421)) ;
#69408 = CARTESIAN_POINT('Ctrl Pts',(-20.7384592821363,38.4290272500098,122.700777392782)) ;
#69409 = CARTESIAN_POINT('Ctrl Pts',(-20.4726207917741,38.2490381696469,122.842988001983)) ;
#69410 = CARTESIAN_POINT('Ctrl Pts',(-20.8423676549778,38.4390928483674,122.943961403778)) ;
#69411 = CARTESIAN_POINT('Ctrl Pts',(-20.5557471819317,38.2591037680045,123.037535670951)) ;
#69412 = CARTESIAN_POINT('Ctrl Pts',(-20.9014598751906,38.4489955041421,123.197461404665)) ;
#69413 = CARTESIAN_POINT('Ctrl Pts',(-20.6030203204311,38.2690064237792,123.240335071546)) ;
#69414 = CARTESIAN_POINT('Ctrl Pts',(-20.9159258761711,38.4590463299717,123.461136272486)) ;
#69415 = CARTESIAN_POINT('Ctrl Pts',(-20.6145926705631,38.2790572496089,123.451275207691)) ;
#69416 = CARTESIAN_POINT('Ctrl Pts',(-20.8851806308957,38.4689205343106,123.718849938155)) ;
#69417 = CARTESIAN_POINT('Ctrl Pts',(-20.5899961850183,38.2889314539477,123.657445168674)) ;
#69418 = CARTESIAN_POINT('Ctrl Pts',(-20.808697747039,38.4789929843497,123.972194060034)) ;
#69419 = CARTESIAN_POINT('Ctrl Pts',(-20.5288093967578,38.2990039039868,123.860120677196)) ;
#69420 = CARTESIAN_POINT('Ctrl Pts',(-20.6924452330028,38.4888220011232,124.202906653744)) ;
#69421 = CARTESIAN_POINT('Ctrl Pts',(-20.4358076437675,38.3088329207603,124.044689498754)) ;
#69422 = CARTESIAN_POINT('Ctrl Pts',(-20.5345088117265,38.498888847038,124.415079071641)) ;
#69423 = CARTESIAN_POINT('Ctrl Pts',(-20.3094581203434,38.3188997666751,124.214427542869)) ;
#69424 = CARTESIAN_POINT('Ctrl Pts',(-20.3453362910282,38.5087790183398,124.593350718177)) ;
#69425 = CARTESIAN_POINT('Ctrl Pts',(-20.1581205171573,38.3287899379769,124.35704407548)) ;
#69426 = CARTESIAN_POINT('Ctrl Pts',(-20.1262004053155,38.5187712119636,124.737995435515)) ;
#69427 = CARTESIAN_POINT('Ctrl Pts',(-19.9828118735316,38.3387821316008,124.472759636862)) ;
#69428 = CARTESIAN_POINT('Ctrl Pts',(-19.8858793197356,38.5287340225871,124.841862120209)) ;
#69429 = CARTESIAN_POINT('Ctrl Pts',(-19.7905552583215,38.3487449422242,124.55585265074)) ;
#69430 = CARTESIAN_POINT('Ctrl Pts',(-19.6327966736522,38.5386382954305,124.9027167446)) ;
#69431 = CARTESIAN_POINT('Ctrl Pts',(-19.5880898637253,38.3586492150676,124.604536139099)) ;
#69432 = CARTESIAN_POINT('Ctrl Pts',(-19.3689353661875,38.5486987872351,124.918722771456)) ;
#69433 = CARTESIAN_POINT('Ctrl Pts',(-19.3770005294909,38.3687097068723,124.617340882227)) ;
#69434 = CARTESIAN_POINT('Ctrl Pts',(-19.1119433120646,38.5585391189074,124.8896559552)) ;
#69435 = CARTESIAN_POINT('Ctrl Pts',(-19.1714080569819,38.3785500385446,124.594087552618)) ;
#69436 = CARTESIAN_POINT('Ctrl Pts',(-18.858267179598,38.5686021649992,124.815076395297)) ;
#69437 = CARTESIAN_POINT('Ctrl Pts',(-18.9684668438895,38.3886130846363,124.534423889178)) ;
#69438 = CARTESIAN_POINT('Ctrl Pts',(-18.6254129262552,38.5784962206943,124.699336919331)) ;
#69439 = CARTESIAN_POINT('Ctrl Pts',(-18.782184165847,38.3985071403314,124.441832684119)) ;
#69440 = CARTESIAN_POINT('Ctrl Pts',(-18.4147842988255,38.5884389210173,124.544774213898)) ;
#69441 = CARTESIAN_POINT('Ctrl Pts',(-18.6136815630311,38.4084498406544,124.318182986908)) ;
#69442 = CARTESIAN_POINT('Ctrl Pts',(-18.2329705623296,38.5984446619449,124.354785151136)) ;
#69443 = CARTESIAN_POINT('Ctrl Pts',(-18.4682304676226,38.418455581582,124.166191932299)) ;
#69444 = CARTESIAN_POINT('Ctrl Pts',(-18.086951476104,38.6084655724604,124.135644682199)) ;
#69445 = CARTESIAN_POINT('Ctrl Pts',(-18.3514150709044,38.4284764920975,123.990879603999)) ;
#69446 = CARTESIAN_POINT('Ctrl Pts',(-17.9822934308915,38.6183563079104,123.897719206915)) ;
#69447 = CARTESIAN_POINT('Ctrl Pts',(-18.2676887771091,38.4383672275475,123.800540072914)) ;
#69448 = CARTESIAN_POINT('Ctrl Pts',(-17.9195346698227,38.6283478486392,123.642773296593)) ;
#69449 = CARTESIAN_POINT('Ctrl Pts',(-18.2174815116301,38.4483587682763,123.596583584727)) ;
#69450 = CARTESIAN_POINT('Ctrl Pts',(-17.9021467020347,38.6382957090609,123.381934725884)) ;
#69451 = CARTESIAN_POINT('Ctrl Pts',(-18.2035708827029,38.458306628698,123.387913220143)) ;
#69452 = CARTESIAN_POINT('Ctrl Pts',(-17.9297985346469,38.6482423782472,123.121998548221)) ;
#69453 = CARTESIAN_POINT('Ctrl Pts',(-18.225691882754,38.4682532978843,123.179964691049)) ;
#69454 = CARTESIAN_POINT('Ctrl Pts',(-18.0031723206151,38.6582904543828,122.868354913034)) ;
#69455 = CARTESIAN_POINT('Ctrl Pts',(-18.2843906358415,38.4783013740199,122.977049494518)) ;
#69456 = CARTESIAN_POINT('Ctrl Pts',(-18.1169630845849,38.6681380523884,122.635927730738)) ;
#69457 = CARTESIAN_POINT('Ctrl Pts',(-18.3754223953298,38.4881489720256,122.791108578199)) ;
#69458 = CARTESIAN_POINT('Ctrl Pts',(-18.2704754939803,38.6780997754729,122.423894509235)) ;
#69459 = CARTESIAN_POINT('Ctrl Pts',(-18.498231618631,38.49811069511,122.621481940386)) ;
#69460 = CARTESIAN_POINT('Ctrl Pts',(-18.459987920288,38.6881284105559,122.240733703719)) ;
#69461 = CARTESIAN_POINT('Ctrl Pts',(-18.6498412530283,38.508139330193,122.474952867454)) ;
#69462 = CARTESIAN_POINT('Ctrl Pts',(-18.6757765964958,38.6980387188739,122.094945578105)) ;
#69463 = CARTESIAN_POINT('Ctrl Pts',(-18.822471309607,38.5180496385111,122.358322309801)) ;
#69464 = CARTESIAN_POINT('Ctrl Pts',(-18.9139298646634,38.7079736160098,121.987944654687)) ;
#69465 = CARTESIAN_POINT('Ctrl Pts',(-19.0129931507068,38.5279845356469,122.272721138619)) ;
#69466 = CARTESIAN_POINT('Ctrl Pts',(-19.1697940908906,38.7180146989524,121.92347677505)) ;
#69467 = CARTESIAN_POINT('Ctrl Pts',(-19.2176845178362,38.5380256185895,122.221146167551)) ;
#69468 = CARTESIAN_POINT('Ctrl Pts',(-19.4289447281885,38.7279020417806,121.904527054462)) ;
#69469 = CARTESIAN_POINT('Ctrl Pts',(-19.4250041481742,38.5479129614178,122.20598575918)) ;
#69470 = CARTESIAN_POINT('Ctrl Pts',(-19.6901903067169,38.73789355672,121.930687744959)) ;
#69471 = CARTESIAN_POINT('Ctrl Pts',(-19.634000528053,38.5579044763571,122.226913496927)) ;
#69472 = CARTESIAN_POINT('Ctrl Pts',(-19.9419001392369,38.7478449479164,122.001637581168)) ;
#69473 = CARTESIAN_POINT('Ctrl Pts',(-19.8353681920912,38.5678558675536,122.283672501495)) ;
#69474 = CARTESIAN_POINT('Ctrl Pts',(-20.1772104092053,38.7577774812491,122.114589337141)) ;
#69475 = CARTESIAN_POINT('Ctrl Pts',(-20.0236163134936,38.5777884008862,122.374032878613)) ;
#69476 = CARTESIAN_POINT('Ctrl Pts',(-20.3907677132585,38.7677746391485,122.267583026891)) ;
#69477 = CARTESIAN_POINT('Ctrl Pts',(-20.1944625857522,38.5877855587856,122.496427023054)) ;
#69478 = CARTESIAN_POINT('Ctrl Pts',(-20.5743995160923,38.777759649312,122.455072551218)) ;
#69479 = CARTESIAN_POINT('Ctrl Pts',(-20.3413685642757,38.5977705689491,122.646417859673)) ;
#69480 = CARTESIAN_POINT('Ctrl Pts',(-20.7231828307075,38.7878024758818,122.673007430821)) ;
#69481 = CARTESIAN_POINT('Ctrl Pts',(-20.4603959891244,38.6078133955189,122.82076541107)) ;
#69482 = CARTESIAN_POINT('Ctrl Pts',(-20.8301369986688,38.7976327101868,122.908200598567)) ;
#69483 = CARTESIAN_POINT('Ctrl Pts',(-20.5459597363222,38.6176436298239,123.008918492089)) ;
#69484 = CARTESIAN_POINT('Ctrl Pts',(-20.8963322764258,38.8077087354214,123.164523836751)) ;
#69485 = CARTESIAN_POINT('Ctrl Pts',(-20.5989170207742,38.6277196550586,123.213977164575)) ;
#69486 = CARTESIAN_POINT('Ctrl Pts',(-20.9166999184839,38.8175609719123,123.422684680524)) ;
#69487 = CARTESIAN_POINT('Ctrl Pts',(-20.6152120890159,38.6375718915494,123.420504774744)) ;
#69488 = CARTESIAN_POINT('Ctrl Pts',(-20.8916094132905,38.8276341783464,123.686162896882)) ;
#69489 = CARTESIAN_POINT('Ctrl Pts',(-20.5951407373615,38.6476450979836,123.631287770219)) ;
#69490 = CARTESIAN_POINT('Ctrl Pts',(-20.8226867659829,38.8374756878536,123.935453060471)) ;
#69491 = CARTESIAN_POINT('Ctrl Pts',(-20.5400039281525,38.6574866074907,123.830719181644)) ;
#69492 = CARTESIAN_POINT('Ctrl Pts',(-20.711078874135,38.8474366346334,124.172221368131)) ;
#69493 = CARTESIAN_POINT('Ctrl Pts',(-20.4507189196892,38.6674475542705,124.020134084588)) ;
#69494 = CARTESIAN_POINT('Ctrl Pts',(-20.558458951886,38.8574744634334,124.387360046542)) ;
#69495 = CARTESIAN_POINT('Ctrl Pts',(-20.3286238767375,38.6774853830706,124.192245792429)) ;
#69496 = CARTESIAN_POINT('Ctrl Pts',(-20.3741695323438,38.8673487731879,124.570081720976)) ;
#69497 = CARTESIAN_POINT('Ctrl Pts',(-20.1811938154597,38.687359692825,124.338423469398)) ;
#69498 = CARTESIAN_POINT('Ctrl Pts',(-20.1567812055592,38.8774184708611,124.72090620419)) ;
#69499 = CARTESIAN_POINT('Ctrl Pts',(-20.0072836517336,38.6974293904982,124.459084262676)) ;
#69500 = CARTESIAN_POINT('Ctrl Pts',(-19.9221504638818,38.8872519421485,124.82924108008)) ;
#69501 = CARTESIAN_POINT('Ctrl Pts',(-19.8195805334962,38.7072628617856,124.545752917569)) ;
#69502 = CARTESIAN_POINT('Ctrl Pts',(-19.6675077755331,38.8972815886784,124.897233739368)) ;
#69503 = CARTESIAN_POINT('Ctrl Pts',(-19.615866693082,38.7172925083155,124.600148473551)) ;
#69504 = CARTESIAN_POINT('Ctrl Pts',(-19.4047212779265,38.9073161030058,124.919189865937)) ;
#69505 = CARTESIAN_POINT('Ctrl Pts',(-19.4056375333307,38.7273270226429,124.61771467157)) ;
#69506 = CARTESIAN_POINT('Ctrl Pts',(-19.1475370275011,38.9171413884767,124.896304082123)) ;
#69507 = CARTESIAN_POINT('Ctrl Pts',(-19.1998910344568,38.7371523081138,124.599407555355)) ;
#69508 = CARTESIAN_POINT('Ctrl Pts',(-18.8935792031542,38.9271456300252,124.828433457309)) ;
#69509 = CARTESIAN_POINT('Ctrl Pts',(-18.9967244455218,38.7471565496623,124.545112555679)) ;
#69510 = CARTESIAN_POINT('Ctrl Pts',(-18.6557514840931,38.9371282751043,124.717603510386)) ;
#69511 = CARTESIAN_POINT('Ctrl Pts',(-18.8064617880754,38.7571391947414,124.456450040447)) ;
#69512 = CARTESIAN_POINT('Ctrl Pts',(-18.439669749991,38.9471734721958,124.566019704998)) ;
#69513 = CARTESIAN_POINT('Ctrl Pts',(-18.633595466131,38.7671843918329,124.335184114137)) ;
#69514 = CARTESIAN_POINT('Ctrl Pts',(-18.2569780632649,38.9569965879559,124.383630345431)) ;
#69515 = CARTESIAN_POINT('Ctrl Pts',(-18.4874417365958,38.7770075075931,124.189274418743)) ;
#69516 = CARTESIAN_POINT('Ctrl Pts',(-18.1050023548241,38.9670311997562,124.168134092341)) ;
#69517 = CARTESIAN_POINT('Ctrl Pts',(-18.3658597612924,38.7870421193933,124.016878306509)) ;
#69518 = CARTESIAN_POINT('Ctrl Pts',(-17.9935211048472,38.9770562085294,123.929428614842)) ;
#69519 = CARTESIAN_POINT('Ctrl Pts',(-18.2766733718385,38.7970671281665,123.825914551769)) ;
#69520 = CARTESIAN_POINT('Ctrl Pts',(-17.9258146375031,38.9869081333709,123.679534933401)) ;
#69521 = CARTESIAN_POINT('Ctrl Pts',(-18.2225068346885,38.8069190530081,123.62600081153)) ;
#69522 = CARTESIAN_POINT('Ctrl Pts',(-17.9017999976252,38.9968990716936,123.418116000194)) ;
#69523 = CARTESIAN_POINT('Ctrl Pts',(-18.2032934378327,38.8169099913308,123.416865957209)) ;
#69524 = CARTESIAN_POINT('Ctrl Pts',(-17.9232192572526,39.0068170568401,123.158331775182)) ;
#69525 = CARTESIAN_POINT('Ctrl Pts',(-18.2204270837738,38.8268279764772,123.209038890302)) ;
#69526 = CARTESIAN_POINT('Ctrl Pts',(-17.9900801459671,39.0168451577356,122.903447812489)) ;
#69527 = CARTESIAN_POINT('Ctrl Pts',(-18.2739141162152,38.8368560773727,123.005131251338)) ;
#69528 = CARTESIAN_POINT('Ctrl Pts',(-18.0985256645866,39.0267303986782,122.66738650819)) ;
#69529 = CARTESIAN_POINT('Ctrl Pts',(-18.3606686866534,38.8467413183153,122.816282007666)) ;
#69530 = CARTESIAN_POINT('Ctrl Pts',(-18.2473354546933,39.0367195116448,122.451127866607)) ;
#69531 = CARTESIAN_POINT('Ctrl Pts',(-18.4797149123304,38.8567304312819,122.643274141846)) ;
#69532 = CARTESIAN_POINT('Ctrl Pts',(-18.4328121554963,39.0467615759856,122.263416874408)) ;
#69533 = CARTESIAN_POINT('Ctrl Pts',(-18.628095065177,38.8667724956227,122.49310404951)) ;
#69534 = CARTESIAN_POINT('Ctrl Pts',(-18.6432316642718,39.0565907773901,122.113588566168)) ;
#69535 = CARTESIAN_POINT('Ctrl Pts',(-18.7964289710917,38.8766016970272,122.373240345266)) ;
#69536 = CARTESIAN_POINT('Ctrl Pts',(-18.8804006960058,39.0665976181483,122.000064282247)) ;
#69537 = CARTESIAN_POINT('Ctrl Pts',(-18.986163304992,38.8866085377854,122.282419197407)) ;
#69538 = CARTESIAN_POINT('Ctrl Pts',(-19.1333031196278,39.0765851423402,121.929712194851)) ;
#69539 = CARTESIAN_POINT('Ctrl Pts',(-19.1884846090727,38.8965960619773,122.226135721828)) ;
#69540 = CARTESIAN_POINT('Ctrl Pts',(-19.3956318554856,39.0866147881488,121.90442252384)) ;
#69541 = CARTESIAN_POINT('Ctrl Pts',(-19.3983474399373,38.9066257077859,122.205902107864)) ;
#69542 = CARTESIAN_POINT('Ctrl Pts',(-19.6543650766534,39.0964888188876,121.924438378725)) ;
#69543 = CARTESIAN_POINT('Ctrl Pts',(-19.6053336278132,38.9164997385247,122.221912828069)) ;
#69544 = CARTESIAN_POINT('Ctrl Pts',(-19.9088952559089,39.1064881417517,121.989562946881)) ;
#69545 = CARTESIAN_POINT('Ctrl Pts',(-19.8089581746776,38.9264990613888,122.274010548606)) ;
#69546 = CARTESIAN_POINT('Ctrl Pts',(-20.1463184204116,39.1163989773273,122.096736593804)) ;
#69547 = CARTESIAN_POINT('Ctrl Pts',(-19.9988971842688,38.9364098969644,122.359747484487)) ;
#69548 = CARTESIAN_POINT('Ctrl Pts',(-20.3645137350782,39.1264532253013,122.245659936878)) ;
#69549 = CARTESIAN_POINT('Ctrl Pts',(-20.1734546335938,38.9464641449384,122.47888456104)) ;
#69550 = CARTESIAN_POINT('Ctrl Pts',(-20.5501363523251,39.136311969564,122.426460600573)) ;
#69551 = CARTESIAN_POINT('Ctrl Pts',(-20.3219537705766,38.9563228892011,122.623523276543)) ;
#69552 = CARTESIAN_POINT('Ctrl Pts',(-20.7048400636721,39.146380055637,122.641049209758)) ;
#69553 = CARTESIAN_POINT('Ctrl Pts',(-20.445718474219,38.9663909752741,122.795193064183)) ;
#69554 = CARTESIAN_POINT('Ctrl Pts',(-20.8175117263284,39.1562355388165,122.87427274074)) ;
#69555 = CARTESIAN_POINT('Ctrl Pts',(-20.5358574288074,38.9762464584537,122.981770549878)) ;
#69556 = CARTESIAN_POINT('Ctrl Pts',(-20.889721867706,39.1662303846107,123.126796707764)) ;
#69557 = CARTESIAN_POINT('Ctrl Pts',(-20.5936275684775,38.9862413042478,123.183789061337)) ;
#69558 = CARTESIAN_POINT('Ctrl Pts',(-20.9165245762999,39.1762616802733,123.389047651322)) ;
#69559 = CARTESIAN_POINT('Ctrl Pts',(-20.6150717949923,38.9962725999104,123.393589604221)) ;
#69560 = CARTESIAN_POINT('Ctrl Pts',(-20.8981112102425,39.1861282235631,123.647684462324)) ;
#69561 = CARTESIAN_POINT('Ctrl Pts',(-20.6003432386068,39.0061391432003,123.600498792257)) ;
#69562 = CARTESIAN_POINT('Ctrl Pts',(-20.8347179859735,39.1961156193265,123.902339731277)) ;
#69563 = CARTESIAN_POINT('Ctrl Pts',(-20.5496307722175,39.0161265389636,123.804223432309)) ;
#69564 = CARTESIAN_POINT('Ctrl Pts',(-20.728622932385,39.2060606600565,124.14122345198)) ;
#69565 = CARTESIAN_POINT('Ctrl Pts',(-20.4647567795798,39.0260715796936,123.9953311149)) ;
#69566 = CARTESIAN_POINT('Ctrl Pts',(-20.5811155220166,39.2161051662732,124.360088757602)) ;
#69567 = CARTESIAN_POINT('Ctrl Pts',(-20.3467526264366,39.0361160859103,124.170424573902)) ;
#69568 = CARTESIAN_POINT('Ctrl Pts',(-20.4012820501656,39.2259686724105,124.546795194446)) ;
#69569 = CARTESIAN_POINT('Ctrl Pts',(-20.2028876468785,39.0459795920477,124.319790982306)) ;
#69570 = CARTESIAN_POINT('Ctrl Pts',(-20.1893406639608,39.2359615332466,124.701780528445)) ;
#69571 = CARTESIAN_POINT('Ctrl Pts',(-20.033335900681,39.0559724528837,124.443780983451)) ;
#69572 = CARTESIAN_POINT('Ctrl Pts',(-19.9552664329016,39.2458877269655,124.816982053056)) ;
#69573 = CARTESIAN_POINT('Ctrl Pts',(-19.8460776484438,39.0658986466027,124.535944103352)) ;
#69574 = CARTESIAN_POINT('Ctrl Pts',(-19.7024842949339,39.2559066529981,124.890499840195)) ;
#69575 = CARTESIAN_POINT('Ctrl Pts',(-19.643852594965,39.0759175726352,124.594760445571)) ;
#69576 = CARTESIAN_POINT('Ctrl Pts',(-19.4434484431289,39.2658216523657,124.918965884066)) ;
#69577 = CARTESIAN_POINT('Ctrl Pts',(-19.4366243284276,39.0858325720028,124.61753546939)) ;
#69578 = CARTESIAN_POINT('Ctrl Pts',(-19.1798154010535,39.275876423923,124.901733325748)) ;
#69579 = CARTESIAN_POINT('Ctrl Pts',(-19.2257177564351,39.0958873435601,124.603751640336)) ;
#69580 = CARTESIAN_POINT('Ctrl Pts',(-18.9280744033614,39.2857353862206,124.840355827184)) ;
#69581 = CARTESIAN_POINT('Ctrl Pts',(-19.0243246392442,39.1057463058577,124.55465185544)) ;
#69582 = CARTESIAN_POINT('Ctrl Pts',(-18.6874294683808,39.2957296300584,124.735252472311)) ;
#69583 = CARTESIAN_POINT('Ctrl Pts',(-18.8318078469648,39.1157405496955,124.470571256637)) ;
#69584 = CARTESIAN_POINT('Ctrl Pts',(-18.4700628513266,39.3056548594826,124.591021419432)) ;
#69585 = CARTESIAN_POINT('Ctrl Pts',(-18.6579133993353,39.1256657791198,124.355188343277)) ;
#69586 = CARTESIAN_POINT('Ctrl Pts',(-18.2791321697973,39.3156828233741,124.409439034504)) ;
#69587 = CARTESIAN_POINT('Ctrl Pts',(-18.5051673400138,39.1356937430112,124.209924100878)) ;
#69588 = CARTESIAN_POINT('Ctrl Pts',(-18.1245827427517,39.3255690830045,124.200558385393)) ;
#69589 = CARTESIAN_POINT('Ctrl Pts',(-18.381526045183,39.1455800026416,124.042820995344)) ;
#69590 = CARTESIAN_POINT('Ctrl Pts',(-18.0068578913663,39.3356008460823,123.964729079241)) ;
#69591 = CARTESIAN_POINT('Ctrl Pts',(-18.2873441695228,39.1556117657195,123.854158607123)) ;
#69592 = CARTESIAN_POINT('Ctrl Pts',(-17.9327236697777,39.3454824723765,123.715808953631)) ;
#69593 = CARTESIAN_POINT('Ctrl Pts',(-18.2280346488682,39.1654933920136,123.65502319765)) ;
#69594 = CARTESIAN_POINT('Ctrl Pts',(-17.9023337792867,39.3555442418626,123.453187507275)) ;
#69595 = CARTESIAN_POINT('Ctrl Pts',(-18.2037205033373,39.1755551614998,123.444926368231)) ;
#69596 = CARTESIAN_POINT('Ctrl Pts',(-17.9176154685571,39.3654021093581,123.194552719115)) ;
#69597 = CARTESIAN_POINT('Ctrl Pts',(-18.2159436064791,39.1854130289952,123.238018412343)) ;
#69598 = CARTESIAN_POINT('Ctrl Pts',(-17.9778056084377,39.3753937344755,122.939007178567)) ;
#69599 = CARTESIAN_POINT('Ctrl Pts',(-18.2640935243759,39.1954046541126,123.033581500678)) ;
#69600 = CARTESIAN_POINT('Ctrl Pts',(-18.0809465923163,39.3853305335837,122.699093789421)) ;
#69601 = CARTESIAN_POINT('Ctrl Pts',(-18.3466042525769,39.2053414532208,122.841649902938)) ;
#69602 = CARTESIAN_POINT('Ctrl Pts',(-18.2246316582653,39.3953213631411,122.479348914402)) ;
#69603 = CARTESIAN_POINT('Ctrl Pts',(-18.4615504185501,39.2153322827782,122.66585281308)) ;
#69604 = CARTESIAN_POINT('Ctrl Pts',(-18.4050975254076,39.4053445988542,122.287476075996)) ;
#69605 = CARTESIAN_POINT('Ctrl Pts',(-18.6059214265816,39.2253555184914,122.512353066652)) ;
#69606 = CARTESIAN_POINT('Ctrl Pts',(-18.6133254066964,39.4152409468834,122.131679228761)) ;
#69607 = CARTESIAN_POINT('Ctrl Pts',(-18.7725024389883,39.2352518665205,122.387713758651)) ;
#69608 = CARTESIAN_POINT('Ctrl Pts',(-18.8473919143103,39.4252305093859,122.012791074316)) ;
#69609 = CARTESIAN_POINT('Ctrl Pts',(-18.9597546642961,39.245241429023,122.292601282324)) ;
#69610 = CARTESIAN_POINT('Ctrl Pts',(-19.0999512728563,39.4352708170704,121.936479082214)) ;
#69611 = CARTESIAN_POINT('Ctrl Pts',(-19.1618012471887,39.2552817367076,122.231549573829)) ;
#69612 = CARTESIAN_POINT('Ctrl Pts',(-19.3567329848095,39.4451131204176,121.905300141157)) ;
#69613 = CARTESIAN_POINT('Ctrl Pts',(-19.3672271092616,39.2651240400548,122.206604238954)) ;
#69614 = CARTESIAN_POINT('Ctrl Pts',(-19.6197445019835,39.4551368286967,121.919081532484)) ;
#69615 = CARTESIAN_POINT('Ctrl Pts',(-19.5776343212279,39.2751477483338,122.217627049978)) ;
#69616 = CARTESIAN_POINT('Ctrl Pts',(-19.9583923044283,39.4683590061644,121.997113385212)) ;
#69617 = CARTESIAN_POINT('Ctrl Pts',(-19.8485635151233,39.2883699258015,122.280050331721)) ;
#69618 = CARTESIAN_POINT('Ctrl Pts',(-20.2706261181306,39.4816515912237,122.162206025503)) ;
#69619 = CARTESIAN_POINT('Ctrl Pts',(-20.0983757918957,39.3016625108608,122.412145538287)) ;
#69620 = CARTESIAN_POINT('Ctrl Pts',(-20.5265366200315,39.4949364471453,122.399782063078)) ;
#69621 = CARTESIAN_POINT('Ctrl Pts',(-20.3030677424335,39.3149473667824,122.602175696939)) ;
#69622 = CARTESIAN_POINT('Ctrl Pts',(-20.6848475062148,39.5049086743181,122.608570519109)) ;
#69623 = CARTESIAN_POINT('Ctrl Pts',(-20.4297258566199,39.3249195939552,122.769211054602)) ;
#69624 = CARTESIAN_POINT('Ctrl Pts',(-20.8041722375231,39.5148172907571,122.840044926829)) ;
#69625 = CARTESIAN_POINT('Ctrl Pts',(-20.5251856336139,39.3348282103942,122.954388023249)) ;
#69626 = CARTESIAN_POINT('Ctrl Pts',(-20.8825021974907,39.5248704961408,123.09232602936)) ;
#69627 = CARTESIAN_POINT('Ctrl Pts',(-20.5878516382789,39.3448814157779,123.156213664846)) ;
#69628 = CARTESIAN_POINT('Ctrl Pts',(-20.9153854640603,39.5347356299011,123.349500706136)) ;
#69629 = CARTESIAN_POINT('Ctrl Pts',(-20.6141617865867,39.3547465495382,123.361949101435)) ;
#69630 = CARTESIAN_POINT('Ctrl Pts',(-20.8994475638338,39.5480746875274,123.699654940672)) ;
#69631 = CARTESIAN_POINT('Ctrl Pts',(-20.6014062025632,39.3680856071645,123.642094456117)) ;
#69632 = CARTESIAN_POINT('Ctrl Pts',(-20.7662626209752,39.5646438748606,124.119481950554)) ;
#69633 = CARTESIAN_POINT('Ctrl Pts',(-20.4948802699597,39.3846547944977,123.977922342078)) ;
#69634 = CARTESIAN_POINT('Ctrl Pts',(-20.4969232972869,39.5812890147116,124.470352991445)) ;
#69635 = CARTESIAN_POINT('Ctrl Pts',(-20.2793689415074,39.4012999343487,124.258669314264)) ;
#69636 = CARTESIAN_POINT('Ctrl Pts',(-20.2201055636797,39.594561317185,124.682635504472)) ;
#69637 = CARTESIAN_POINT('Ctrl Pts',(-20.0579520034563,39.4145722368221,124.428460073727)) ;
#69638 = CARTESIAN_POINT('Ctrl Pts',(-19.9875926506158,39.6045422806326,124.803956293346)) ;
#69639 = CARTESIAN_POINT('Ctrl Pts',(-19.8719346104858,39.4245532002698,124.525525821103)) ;
#69640 = CARTESIAN_POINT('Ctrl Pts',(-19.7385233068285,39.6144841127019,124.882919421765)) ;
#69641 = CARTESIAN_POINT('Ctrl Pts',(-19.6726839339702,39.4344950323391,124.588696443466)) ;
#69642 = CARTESIAN_POINT('Ctrl Pts',(-19.3916274184842,39.6278036819174,124.929289096296)) ;
#69643 = CARTESIAN_POINT('Ctrl Pts',(-19.3951539287029,39.4478146015545,124.625793702536)) ;
#69644 = CARTESIAN_POINT('Ctrl Pts',(-18.9557155359981,39.6443338368501,124.873608604834)) ;
#69645 = CARTESIAN_POINT('Ctrl Pts',(-19.0464382212822,39.4643447564872,124.581253473117)) ;
#69646 = CARTESIAN_POINT('Ctrl Pts',(-18.4827841914937,39.6643555623422,124.629948165702)) ;
#69647 = CARTESIAN_POINT('Ctrl Pts',(-18.6680869357579,39.4843664819793,124.386327764593)) ;
#69648 = CARTESIAN_POINT('Ctrl Pts',(-18.1247857375982,39.684166958949,124.243642886315)) ;
#69649 = CARTESIAN_POINT('Ctrl Pts',(-18.3816862675463,39.5041778785861,124.077284936914)) ;
#69650 = CARTESIAN_POINT('Ctrl Pts',(-17.9175888921553,39.7041522076579,123.754678947954)) ;
#69651 = CARTESIAN_POINT('Ctrl Pts',(-18.2159257535573,39.524163127295,123.686114759911)) ;
#69652 = CARTESIAN_POINT('Ctrl Pts',(-17.8901646194333,39.7240462702938,123.226554358752)) ;
#69653 = CARTESIAN_POINT('Ctrl Pts',(-18.1939835441653,39.5440571899309,123.263614485181)) ;
#69654 = CARTESIAN_POINT('Ctrl Pts',(-18.0441177194512,39.7439779494674,122.719677099901)) ;
#69655 = CARTESIAN_POINT('Ctrl Pts',(-18.3171437873971,39.5639888691045,122.858111428602)) ;
#69656 = CARTESIAN_POINT('Ctrl Pts',(-18.3626008286604,39.7639420039394,122.295272619757)) ;
#69657 = CARTESIAN_POINT('Ctrl Pts',(-18.5719284738746,39.5839529235765,122.518586147516)) ;
#69658 = CARTESIAN_POINT('Ctrl Pts',(-18.8047431638309,39.7838229057023,122.005888410444)) ;
#69659 = CARTESIAN_POINT('Ctrl Pts',(-18.9256420531025,39.6038338253394,122.287076349787)) ;
#69660 = CARTESIAN_POINT('Ctrl Pts',(-19.3204270314315,39.8037615673107,121.883932996576)) ;
#69661 = CARTESIAN_POINT('Ctrl Pts',(-19.3381893000524,39.6237724869478,122.189510074961)) ;
#69662 = CARTESIAN_POINT('Ctrl Pts',(-19.8456885699466,39.823658092566,121.945064977875)) ;
#69663 = CARTESIAN_POINT('Ctrl Pts',(-19.7583997745947,39.6436690122031,122.238414117191)) ;
#69664 = CARTESIAN_POINT('Ctrl Pts',(-20.3189371293568,39.8435531310203,122.180988955681)) ;
#69665 = CARTESIAN_POINT('Ctrl Pts',(-20.1370001890922,39.6635640506575,122.427152812222)) ;
#69666 = CARTESIAN_POINT('Ctrl Pts',(-20.684435302286,39.8635169543264,122.565581974928)) ;
#69667 = CARTESIAN_POINT('Ctrl Pts',(-20.4293997300506,39.6835278739635,122.734826840731)) ;
#69668 = CARTESIAN_POINT('Ctrl Pts',(-20.8961892011034,39.8833910784555,123.049543285432)) ;
#69669 = CARTESIAN_POINT('Ctrl Pts',(-20.5988040313383,39.7034019980926,123.121997016737)) ;
#69670 = CARTESIAN_POINT('Ctrl Pts',(-20.9307446999035,39.9033661541827,123.579345858903)) ;
#69671 = CARTESIAN_POINT('Ctrl Pts',(-20.6264486432097,39.7233770738199,123.54583933781)) ;
#69672 = CARTESIAN_POINT('Ctrl Pts',(-20.7818723368726,39.9233197235393,124.088346140046)) ;
#69673 = CARTESIAN_POINT('Ctrl Pts',(-20.5073509383854,39.7433306431764,123.953040241885)) ;
#69674 = CARTESIAN_POINT('Ctrl Pts',(-20.4708597448831,39.9431576337272,124.514109737929)) ;
#69675 = CARTESIAN_POINT('Ctrl Pts',(-20.2585393443571,39.7631685533643,124.293652633685)) ;
#69676 = CARTESIAN_POINT('Ctrl Pts',(-20.0304987770853,39.9631334622981,124.810695893572)) ;
#69677 = CARTESIAN_POINT('Ctrl Pts',(-19.9062499102217,39.7831443819352,124.53092102101)) ;
#69678 = CARTESIAN_POINT('Ctrl Pts',(-19.5167467254977,39.9830515070084,124.938262136295)) ;
#69679 = CARTESIAN_POINT('Ctrl Pts',(-19.4952471367361,39.8030624266455,124.632973548658)) ;
#69680 = CARTESIAN_POINT('Ctrl Pts',(-18.9912829799873,40.002921752796,124.884310017349)) ;
#69681 = CARTESIAN_POINT('Ctrl Pts',(-19.0748749155325,39.8229326724332,124.589810226705)) ;
#69682 = CARTESIAN_POINT('Ctrl Pts',(-18.512059067701,40.0229707558956,124.651607827821)) ;
#69683 = CARTESIAN_POINT('Ctrl Pts',(-18.691496813196,39.8429816755327,124.403647475634)) ;
#69684 = CARTESIAN_POINT('Ctrl Pts',(-18.1453823899898,40.0427499971364,124.274685535331)) ;
#69685 = CARTESIAN_POINT('Ctrl Pts',(-18.3981551846587,39.8627609167736,124.10210688277)) ;
#69686 = CARTESIAN_POINT('Ctrl Pts',(-17.9259795061986,40.0627800608453,123.789764142162)) ;
#69687 = CARTESIAN_POINT('Ctrl Pts',(-18.2226350126772,39.8827909804824,123.714169148054)) ;
#69688 = CARTESIAN_POINT('Ctrl Pts',(-17.8863640755832,40.0826623457473,123.26273048994)) ;
#69689 = CARTESIAN_POINT('Ctrl Pts',(-18.1909445989057,39.9026732653844,123.292541016045)) ;
#69690 = CARTESIAN_POINT('Ctrl Pts',(-18.0275270007879,40.1025446466403,122.753544083108)) ;
#69691 = CARTESIAN_POINT('Ctrl Pts',(-18.3038777717334,39.9225555662774,122.885191650426)) ;
#69692 = CARTESIAN_POINT('Ctrl Pts',(-18.3357032518353,40.1225277562586,122.320964219485)) ;
#69693 = CARTESIAN_POINT('Ctrl Pts',(-18.5504210502982,39.9425386758957,122.539129268786)) ;
#69694 = CARTESIAN_POINT('Ctrl Pts',(-18.7710249752049,40.1424181516365,122.020953450762)) ;
#69695 = CARTESIAN_POINT('Ctrl Pts',(-18.8986807002394,39.9624290712736,122.299122526392)) ;
#69696 = CARTESIAN_POINT('Ctrl Pts',(-19.2824556627369,40.1623149416708,121.886718883341)) ;
#69697 = CARTESIAN_POINT('Ctrl Pts',(-19.3078267411535,39.9823258613079,122.191737773976)) ;
#69698 = CARTESIAN_POINT('Ctrl Pts',(-19.809682792952,40.1822319956124,121.93454660401)) ;
#69699 = CARTESIAN_POINT('Ctrl Pts',(-19.7296086094093,40.0022429152495,122.230003389753)) ;
#69700 = CARTESIAN_POINT('Ctrl Pts',(-20.290985297749,40.2022355438159,122.160572440253)) ;
#69701 = CARTESIAN_POINT('Ctrl Pts',(-20.1146490294153,40.022246463453,122.410827178833)) ;
#69702 = CARTESIAN_POINT('Ctrl Pts',(-20.6644175476188,40.2221738374685,122.536530476513)) ;
#69703 = CARTESIAN_POINT('Ctrl Pts',(-20.4133927604481,40.0421847571056,122.711596130847)) ;
#69704 = CARTESIAN_POINT('Ctrl Pts',(-20.8870164933769,40.2419953249014,123.014022848812)) ;
#69705 = CARTESIAN_POINT('Ctrl Pts',(-20.591468541711,40.0620062445386,123.093592852938)) ;
#69706 = CARTESIAN_POINT('Ctrl Pts',(-20.9342078753314,40.2619737178923,123.54285440319)) ;
#69707 = CARTESIAN_POINT('Ctrl Pts',(-20.629219041352,40.0819846375294,123.51665686398)) ;
#69708 = CARTESIAN_POINT('Ctrl Pts',(-20.798306014332,40.281872099506,124.054044528013)) ;
#69709 = CARTESIAN_POINT('Ctrl Pts',(-20.5204887803847,40.1018830191431,123.925614389338)) ;
#69710 = CARTESIAN_POINT('Ctrl Pts',(-20.5470819880528,40.2984550302359,124.416062159147)) ;
#69711 = CARTESIAN_POINT('Ctrl Pts',(-20.319521718774,40.118465949873,124.215207873857)) ;
#69712 = CARTESIAN_POINT('Ctrl Pts',(-20.281028441282,40.3117292658247,124.641768863592)) ;
#69713 = CARTESIAN_POINT('Ctrl Pts',(-20.1066630077281,40.1317401854619,124.39578795603)) ;
#69714 = CARTESIAN_POINT('Ctrl Pts',(-20.0530654837522,40.3217756832809,124.774877815114)) ;
#69715 = CARTESIAN_POINT('Ctrl Pts',(-19.9242972790721,40.1417866029181,124.50226984556)) ;
#69716 = CARTESIAN_POINT('Ctrl Pts',(-19.810464403995,40.3316209085002,124.864833820521)) ;
#69717 = CARTESIAN_POINT('Ctrl Pts',(-19.7302036734289,40.1516318281373,124.574233889448)) ;
#69718 = CARTESIAN_POINT('Ctrl Pts',(-19.4658929191224,40.3449558795396,124.928504806225)) ;
#69719 = CARTESIAN_POINT('Ctrl Pts',(-19.4546005727731,40.1649667991767,124.625166764035)) ;
#69720 = CARTESIAN_POINT('Ctrl Pts',(-19.0264390688312,40.3615387363322,124.893652813554)) ;
#69721 = CARTESIAN_POINT('Ctrl Pts',(-19.1029686872478,40.1815496559694,124.597278988789)) ;
#69722 = CARTESIAN_POINT('Ctrl Pts',(-18.6239205040509,40.3781817386816,124.71045606654)) ;
#69723 = CARTESIAN_POINT('Ctrl Pts',(-18.7810022090588,40.1981926583188,124.450732338554)) ;
#69724 = CARTESIAN_POINT('Ctrl Pts',(-18.3550031410799,40.3914254697133,124.489405088402)) ;
#69725 = CARTESIAN_POINT('Ctrl Pts',(-18.5658419708258,40.2114363893504,124.273876441203)) ;
#69726 = CARTESIAN_POINT('Ctrl Pts',(-18.1831556506858,40.4014798643879,124.288773158582)) ;
#69727 = CARTESIAN_POINT('Ctrl Pts',(-18.4283713813035,40.221490784025,124.113372135424)) ;
#69728 = CARTESIAN_POINT('Ctrl Pts',(-18.0512693189918,40.4113209257765,124.066262657595)) ;
#69729 = CARTESIAN_POINT('Ctrl Pts',(-18.3228626055422,40.2313318454136,123.935361746005)) ;
#69730 = CARTESIAN_POINT('Ctrl Pts',(-17.9577246777451,40.421387150133,123.818872622899)) ;
#69731 = CARTESIAN_POINT('Ctrl Pts',(-18.2480294373586,40.2413980697701,123.737449245068)) ;
#69732 = CARTESIAN_POINT('Ctrl Pts',(-17.9095230457467,40.4312677630526,123.563691114021)) ;
#69733 = CARTESIAN_POINT('Ctrl Pts',(-18.2094701905773,40.2512786826897,123.533303479069)) ;
#69734 = CARTESIAN_POINT('Ctrl Pts',(-17.9058281378729,40.4412610562122,123.30114626875)) ;
#69735 = CARTESIAN_POINT('Ctrl Pts',(-18.2065165443278,40.2612719758493,123.323267634952)) ;
#69736 = CARTESIAN_POINT('Ctrl Pts',(-17.9475138799179,40.4512120644359,123.042941598617)) ;
#69737 = CARTESIAN_POINT('Ctrl Pts',(-18.2398673462306,40.271222984073,123.116704268342)) ;
#69738 = CARTESIAN_POINT('Ctrl Pts',(-18.0344070397604,40.4612605787978,122.793614478542)) ;
#69739 = CARTESIAN_POINT('Ctrl Pts',(-18.3093839709595,40.281271498435,122.917243386907)) ;
#69740 = CARTESIAN_POINT('Ctrl Pts',(-18.1603863836437,40.4711020848605,122.567719550063)) ;
#69741 = CARTESIAN_POINT('Ctrl Pts',(-18.4101694281105,40.2911130044976,122.736528509964)) ;
#69742 = CARTESIAN_POINT('Ctrl Pts',(-18.3255788630243,40.4810877374902,122.36388078949)) ;
#69743 = CARTESIAN_POINT('Ctrl Pts',(-18.5423251289196,40.3010986571273,122.573458977904)) ;
#69744 = CARTESIAN_POINT('Ctrl Pts',(-18.5227257140879,40.4910267463351,122.192496536557)) ;
#69745 = CARTESIAN_POINT('Ctrl Pts',(-18.7000440471516,40.3110376659722,122.436353315188)) ;
#69746 = CARTESIAN_POINT('Ctrl Pts',(-18.7489120153398,40.5010676716281,122.056659651422)) ;
#69747 = CARTESIAN_POINT('Ctrl Pts',(-18.8809942079959,40.3210785912652,122.327685771661)) ;
#69748 = CARTESIAN_POINT('Ctrl Pts',(-18.9915421154482,40.510957993383,121.963416273453)) ;
#69749 = CARTESIAN_POINT('Ctrl Pts',(-19.0750990226228,40.3309689130201,122.253093205079)) ;
#69750 = CARTESIAN_POINT('Ctrl Pts',(-19.249284101431,40.5209539667164,121.912814957505)) ;
#69751 = CARTESIAN_POINT('Ctrl Pts',(-19.2812929812387,40.3409648863536,122.212614377811)) ;
#69752 = CARTESIAN_POINT('Ctrl Pts',(-19.5102329048635,40.5308853662985,121.907746825893)) ;
#69753 = CARTESIAN_POINT('Ctrl Pts',(-19.4900519685887,40.3508962859356,122.208562125718)) ;
#69754 = CARTESIAN_POINT('Ctrl Pts',(-19.7700821945994,40.5408909067755,121.947997275359)) ;
#69755 = CARTESIAN_POINT('Ctrl Pts',(-19.697930995272,40.3609018264127,122.240764692487)) ;
#69756 = CARTESIAN_POINT('Ctrl Pts',(-20.0195011590798,40.5509238907068,122.033437044935)) ;
#69757 = CARTESIAN_POINT('Ctrl Pts',(-19.8974654062638,40.370934810344,122.30911863456)) ;
#69758 = CARTESIAN_POINT('Ctrl Pts',(-20.2464637604241,40.5607795215337,122.158246335581)) ;
#69759 = CARTESIAN_POINT('Ctrl Pts',(-20.0790342417892,40.3807904411708,122.408967940428)) ;
#69760 = CARTESIAN_POINT('Ctrl Pts',(-20.4514141919689,40.5707789237268,122.322629146748)) ;
#69761 = CARTESIAN_POINT('Ctrl Pts',(-20.2429931328991,40.390789843364,122.540475886912)) ;
#69762 = CARTESIAN_POINT('Ctrl Pts',(-20.623177160939,40.5806733930879,122.517901168788)) ;
#69763 = CARTESIAN_POINT('Ctrl Pts',(-20.3804017081287,40.400684312725,122.696694807102)) ;
#69764 = CARTESIAN_POINT('Ctrl Pts',(-20.7606139057598,40.5907365072521,122.743776897285)) ;
#69765 = CARTESIAN_POINT('Ctrl Pts',(-20.4903492208581,40.4107474268893,122.87739656958)) ;
#69766 = CARTESIAN_POINT('Ctrl Pts',(-20.8549063786372,40.6005761529685,122.984593090461)) ;
#69767 = CARTESIAN_POINT('Ctrl Pts',(-20.5657810296931,40.4205870726056,123.070050018048)) ;
#69768 = CARTESIAN_POINT('Ctrl Pts',(-20.9074265587478,40.6106393205242,123.243737629738)) ;
#69769 = CARTESIAN_POINT('Ctrl Pts',(-20.6077950427695,40.4306502401614,123.277366118892)) ;
#69770 = CARTESIAN_POINT('Ctrl Pts',(-20.9138213840196,40.6205335763191,123.50369845043)) ;
#69771 = CARTESIAN_POINT('Ctrl Pts',(-20.6129087015084,40.4405444959563,123.48533456448)) ;
#69772 = CARTESIAN_POINT('Ctrl Pts',(-20.8755072031584,40.6304753547788,123.762100783259)) ;
#69773 = CARTESIAN_POINT('Ctrl Pts',(-20.5822552681282,40.4504862744159,123.692055906574)) ;
#69774 = CARTESIAN_POINT('Ctrl Pts',(-20.7924699762297,40.640478047609,124.011537115954)) ;
#69775 = CARTESIAN_POINT('Ctrl Pts',(-20.5158234865121,40.4604889672461,123.891604236471)) ;
#69776 = CARTESIAN_POINT('Ctrl Pts',(-20.6666615752292,40.6505120695628,124.243257679907)) ;
#69777 = CARTESIAN_POINT('Ctrl Pts',(-20.4151748534295,40.4705229891999,124.076979664182)) ;
#69778 = CARTESIAN_POINT('Ctrl Pts',(-20.5058740591058,40.6603598606518,124.446047890609)) ;
#69779 = CARTESIAN_POINT('Ctrl Pts',(-20.2865434507489,40.480370780289,124.239210154722)) ;
#69780 = CARTESIAN_POINT('Ctrl Pts',(-20.3100969713907,40.6703413852009,124.620584309683)) ;
#69781 = CARTESIAN_POINT('Ctrl Pts',(-20.1299205038193,40.490352304838,124.378837647099)) ;
#69782 = CARTESIAN_POINT('Ctrl Pts',(-20.0876630799493,40.6802906086918,124.75801282759)) ;
#69783 = CARTESIAN_POINT('Ctrl Pts',(-19.9519724829499,40.5003015283289,124.488778579875)) ;
#69784 = CARTESIAN_POINT('Ctrl Pts',(-19.8436735816779,40.6902882649084,124.85551512015)) ;
#69785 = CARTESIAN_POINT('Ctrl Pts',(-19.7567802051122,40.5102991845455,124.566778487717)) ;
#69786 = CARTESIAN_POINT('Ctrl Pts',(-19.5853011891557,40.7003284779634,124.908895920478)) ;
#69787 = CARTESIAN_POINT('Ctrl Pts',(-19.5500818185997,40.5203393976006,124.609481080196)) ;
#69788 = CARTESIAN_POINT('Ctrl Pts',(-19.3271425182227,40.7101565252397,124.917006738006)) ;
#69789 = CARTESIAN_POINT('Ctrl Pts',(-19.3435554357432,40.5301674448768,124.615967681454)) ;
#69790 = CARTESIAN_POINT('Ctrl Pts',(-19.0655819825205,40.7202108722721,124.87973320103)) ;
#69791 = CARTESIAN_POINT('Ctrl Pts',(-19.1343072015728,40.5402217919092,124.58614687555)) ;
#69792 = CARTESIAN_POINT('Ctrl Pts',(-18.8174100404169,40.7301520086006,124.798108890604)) ;
#69793 = CARTESIAN_POINT('Ctrl Pts',(-18.9357705393896,40.5501629282377,124.520845572302)) ;
#69794 = CARTESIAN_POINT('Ctrl Pts',(-18.5876566119404,40.7400562416803,124.675804537039)) ;
#69795 = CARTESIAN_POINT('Ctrl Pts',(-18.7519690826901,40.5600671613174,124.423000582265)) ;
#69796 = CARTESIAN_POINT('Ctrl Pts',(-18.3798041844874,40.7501029385239,124.513046489696)) ;
#69797 = CARTESIAN_POINT('Ctrl Pts',(-18.5856882820567,40.5701138581611,124.292792552084)) ;
#69798 = CARTESIAN_POINT('Ctrl Pts',(-18.2058043531865,40.7599984898042,124.319735002295)) ;
#69799 = CARTESIAN_POINT('Ctrl Pts',(-18.4464901583571,40.5800094094413,124.138142422738)) ;
#69800 = CARTESIAN_POINT('Ctrl Pts',(-18.0657367626924,40.7700605676437,124.095504335531)) ;
#69801 = CARTESIAN_POINT('Ctrl Pts',(-18.3344376418936,40.5900714872808,123.958756744868)) ;
#69802 = CARTESIAN_POINT('Ctrl Pts',(-17.9687267603788,40.7799032767398,123.855697491767)) ;
#69803 = CARTESIAN_POINT('Ctrl Pts',(-18.2568316638286,40.5999141963769,123.766911199684)) ;
#69804 = CARTESIAN_POINT('Ctrl Pts',(-17.9134237543617,40.7898940089782,123.599076400319)) ;
#69805 = CARTESIAN_POINT('Ctrl Pts',(-18.2125910590899,40.6099049286153,123.561614081908)) ;
#69806 = CARTESIAN_POINT('Ctrl Pts',(-17.9036209757213,40.799822034207,123.33834843595)) ;
#69807 = CARTESIAN_POINT('Ctrl Pts',(-18.2047506639829,40.6198329538441,123.353032033196)) ;
#69808 = CARTESIAN_POINT('Ctrl Pts',(-17.9390103972283,40.8098101808575,123.07826099235)) ;
#69809 = CARTESIAN_POINT('Ctrl Pts',(-18.2330639096619,40.6298211004947,123.144962455833)) ;
#69810 = CARTESIAN_POINT('Ctrl Pts',(-18.0197805146774,40.8198451986975,122.827221506658)) ;
#69811 = CARTESIAN_POINT('Ctrl Pts',(-18.2976817439703,40.6398561183346,122.944131364963)) ;
#69812 = CARTESIAN_POINT('Ctrl Pts',(-18.1405769536225,40.8297099958027,122.597859805826)) ;
#69813 = CARTESIAN_POINT('Ctrl Pts',(-18.394320133305,40.6497209154398,122.76064343955)) ;
#69814 = CARTESIAN_POINT('Ctrl Pts',(-18.3003100262152,40.8396707281588,122.390481778754)) ;
#69815 = CARTESIAN_POINT('Ctrl Pts',(-18.5221077146717,40.6596816477959,122.594742235113)) ;
#69816 = CARTESIAN_POINT('Ctrl Pts',(-18.4953203364736,40.8497041905558,122.213037685501)) ;
#69817 = CARTESIAN_POINT('Ctrl Pts',(-18.6781171657498,40.6697151101929,122.452788175949)) ;
#69818 = CARTESIAN_POINT('Ctrl Pts',(-18.7146955767961,40.8595897247672,122.073836456238)) ;
#69819 = CARTESIAN_POINT('Ctrl Pts',(-18.8536176951084,40.6796006444043,122.341428911214)) ;
#69820 = CARTESIAN_POINT('Ctrl Pts',(-18.9592101605245,40.8696545654472,121.973078301155)) ;
#69821 = CARTESIAN_POINT('Ctrl Pts',(-19.0492301753213,40.6896654850843,122.260823821511)) ;
#69822 = CARTESIAN_POINT('Ctrl Pts',(-19.2119712899475,40.8795026971761,121.917403865115)) ;
#69823 = CARTESIAN_POINT('Ctrl Pts',(-19.2514386073647,40.6995136168132,122.216286026283)) ;
#69824 = CARTESIAN_POINT('Ctrl Pts',(-19.4752106016322,40.8895301941662,121.905583046178)) ;
#69825 = CARTESIAN_POINT('Ctrl Pts',(-19.4620301548535,40.7095411138033,122.206830852572)) ;
#69826 = CARTESIAN_POINT('Ctrl Pts',(-19.7364587404572,40.8995586462113,121.940346685251)) ;
#69827 = CARTESIAN_POINT('Ctrl Pts',(-19.6710285077072,40.7195695658484,122.234643374607)) ;
#69828 = CARTESIAN_POINT('Ctrl Pts',(-19.9832352577145,40.9094039127754,122.018011497405)) ;
#69829 = CARTESIAN_POINT('Ctrl Pts',(-19.8684484097077,40.7294148324125,122.296776407657)) ;
#69830 = CARTESIAN_POINT('Ctrl Pts',(-20.2165109099258,40.9193945857163,122.138492853158)) ;
#69831 = CARTESIAN_POINT('Ctrl Pts',(-20.0550681579274,40.7394055053534,122.393162648683)) ;
#69832 = CARTESIAN_POINT('Ctrl Pts',(-20.4259458604295,40.9294324678048,122.29886132802)) ;
#69833 = CARTESIAN_POINT('Ctrl Pts',(-20.2226152908657,40.7494433874419,122.521458685121)) ;
#69834 = CARTESIAN_POINT('Ctrl Pts',(-20.6012563123727,40.9392768382444,122.489117146691)) ;
#69835 = CARTESIAN_POINT('Ctrl Pts',(-20.3628619804321,40.7592877578816,122.67366360375)) ;
#69836 = CARTESIAN_POINT('Ctrl Pts',(-20.7432721400069,40.9492616656398,122.709711313099)) ;
#69837 = CARTESIAN_POINT('Ctrl Pts',(-20.4764734396498,40.7692725852769,122.850139473825)) ;
#69838 = CARTESIAN_POINT('Ctrl Pts',(-20.844502824681,40.9592011110451,122.950536538216)) ;
#69839 = CARTESIAN_POINT('Ctrl Pts',(-20.5574566433733,40.7792120306822,123.042799745308)) ;
#69840 = CARTESIAN_POINT('Ctrl Pts',(-20.9028785373405,40.969241115331,123.20781127082)) ;
#69841 = CARTESIAN_POINT('Ctrl Pts',(-20.6041559783071,40.7892520349681,123.24861993569)) ;
#69842 = CARTESIAN_POINT('Ctrl Pts',(-20.9156810985871,40.9791282245166,123.46734861019)) ;
#69843 = CARTESIAN_POINT('Ctrl Pts',(-20.6143967389084,40.7991391441538,123.456249117252)) ;
#69844 = CARTESIAN_POINT('Ctrl Pts',(-20.8831859202662,40.9891282844191,123.728082234662)) ;
#69845 = CARTESIAN_POINT('Ctrl Pts',(-20.5883994360712,40.8091392040562,123.664835757104)) ;
#69846 = CARTESIAN_POINT('Ctrl Pts',(-20.8067389220528,40.9990457003338,123.977282854265)) ;
#69847 = CARTESIAN_POINT('Ctrl Pts',(-20.5272409208135,40.8190566199709,123.864195371173)) ;
#69848 = CARTESIAN_POINT('Ctrl Pts',(-20.6866067690655,41.0090925150746,124.212346711425)) ;
#69849 = CARTESIAN_POINT('Ctrl Pts',(-20.4311340955001,40.8291034347117,124.052246084703)) ;
#69850 = CARTESIAN_POINT('Ctrl Pts',(-20.5303634279957,41.0189679922713,124.419613620439)) ;
#69851 = CARTESIAN_POINT('Ctrl Pts',(-20.3061390542249,40.8389789119084,124.218058285258)) ;
#69852 = CARTESIAN_POINT('Ctrl Pts',(-20.3371972791705,41.0290240879925,124.599886515678)) ;
#69853 = CARTESIAN_POINT('Ctrl Pts',(-20.1516052586008,40.8490350076296,124.362275967077)) ;
#69854 = CARTESIAN_POINT('Ctrl Pts',(-20.1192272911797,41.0389172500076,124.741681401867)) ;
#69855 = CARTESIAN_POINT('Ctrl Pts',(-19.9772293226388,40.8589281696447,124.475710604766)) ;
#69856 = CARTESIAN_POINT('Ctrl Pts',(-19.8759671921668,41.0489794860302,124.845254462117)) ;
#69857 = CARTESIAN_POINT('Ctrl Pts',(-19.7826206014674,40.8689904056673,124.558568216301)) ;
#69858 = CARTESIAN_POINT('Ctrl Pts',(-19.6239559484601,41.0588239516591,124.903758180381)) ;
#69859 = CARTESIAN_POINT('Ctrl Pts',(-19.5810124074109,40.8788348712962,124.605369962764)) ;
#69860 = CARTESIAN_POINT('Ctrl Pts',(-19.3626471098562,41.0687840443633,124.918720690763)) ;
#69861 = CARTESIAN_POINT('Ctrl Pts',(-19.3719656563023,40.8887949640004,124.61733915855)) ;
#69862 = CARTESIAN_POINT('Ctrl Pts',(-19.1007386053563,41.0788223333443,124.887329010187)) ;
#69863 = CARTESIAN_POINT('Ctrl Pts',(-19.16243883266,40.8988332529814,124.592224889164)) ;
#69864 = CARTESIAN_POINT('Ctrl Pts',(-18.8522137572535,41.0886956564505,124.812656518733)) ;
#69865 = CARTESIAN_POINT('Ctrl Pts',(-18.9636200453775,40.9087065760876,124.532486393259)) ;
#69866 = CARTESIAN_POINT('Ctrl Pts',(-18.6158596069558,41.0987688405356,124.693571352366)) ;
#69867 = CARTESIAN_POINT('Ctrl Pts',(-18.7745367877756,40.9187797601727,124.437217376295)) ;
#69868 = CARTESIAN_POINT('Ctrl Pts',(-18.4088042083935,41.1085893528235,124.539431437794)) ;
#69869 = CARTESIAN_POINT('Ctrl Pts',(-18.6088939047249,40.9286002724607,124.313905598339)) ;
#69870 = CARTESIAN_POINT('Ctrl Pts',(-18.2269108302998,41.1186673489393,124.347022071441)) ;
#69871 = CARTESIAN_POINT('Ctrl Pts',(-18.4633794360143,40.9386782685765,124.159977371275)) ;
#69872 = CARTESIAN_POINT('Ctrl Pts',(-18.0843084263497,41.1285214239226,124.130796993338)) ;
#69873 = CARTESIAN_POINT('Ctrl Pts',(-18.349298634213,40.9485323435597,123.986997811558)) ;
#69874 = CARTESIAN_POINT('Ctrl Pts',(-17.9790049811939,41.1385853055063,123.888252695276)) ;
#69875 = CARTESIAN_POINT('Ctrl Pts',(-18.2650563069979,40.9585962251434,123.792961884212)) ;
#69876 = CARTESIAN_POINT('Ctrl Pts',(-17.9185435301409,41.14846873148,123.63561553845)) ;
#69877 = CARTESIAN_POINT('Ctrl Pts',(-18.2166879295781,40.9684796511172,123.590852855347)) ;
#69878 = CARTESIAN_POINT('Ctrl Pts',(-17.9022681371798,41.1584693354011,123.37336067713)) ;
#69879 = CARTESIAN_POINT('Ctrl Pts',(-18.2036681214858,40.9784802550382,123.381049048255)) ;
#69880 = CARTESIAN_POINT('Ctrl Pts',(-17.931383888056,41.168389119739,123.114261971927)) ;
#69881 = CARTESIAN_POINT('Ctrl Pts',(-18.2269611056014,40.9884000393761,123.17377075239)) ;
#69882 = CARTESIAN_POINT('Ctrl Pts',(-18.0060263785442,41.1784364700958,122.861044240447)) ;
#69883 = CARTESIAN_POINT('Ctrl Pts',(-18.2866756080612,40.998447389733,122.971196520026)) ;
#69884 = CARTESIAN_POINT('Ctrl Pts',(-18.1212813811983,41.1883138123301,122.62841137183)) ;
#69885 = CARTESIAN_POINT('Ctrl Pts',(-18.3788795564563,41.0083247319672,122.785091229606)) ;
#69886 = CARTESIAN_POINT('Ctrl Pts',(-18.2781294851284,41.1983836934047,122.415344458296)) ;
#69887 = CARTESIAN_POINT('Ctrl Pts',(-18.504358563971,41.0183946130419,122.614637662932)) ;
#69888 = CARTESIAN_POINT('Ctrl Pts',(-18.4649093676713,41.2082133986064,122.236837854703)) ;
#69889 = CARTESIAN_POINT('Ctrl Pts',(-18.6537818070225,41.0282243182436,122.471833474203)) ;
#69890 = CARTESIAN_POINT('Ctrl Pts',(-18.684754038693,41.2182800597728,122.089775689271)) ;
#69891 = CARTESIAN_POINT('Ctrl Pts',(-18.829657944727,41.03829097941,122.354183767872)) ;
#69892 = CARTESIAN_POINT('Ctrl Pts',(-18.922687539533,41.2281702816401,121.985108837478)) ;
#69893 = CARTESIAN_POINT('Ctrl Pts',(-19.0200040932344,41.0481812012773,122.270450887395)) ;
#69894 = CARTESIAN_POINT('Ctrl Pts',(-19.1775992382533,41.2381624577503,121.922160157756)) ;
#69895 = CARTESIAN_POINT('Ctrl Pts',(-19.223933319871,41.0581733773874,122.22009212209)) ;
#69896 = CARTESIAN_POINT('Ctrl Pts',(-19.4388247420797,41.2481252878629,121.904728591906)) ;
#69897 = CARTESIAN_POINT('Ctrl Pts',(-19.4329133725897,41.0681362075001,122.206147099364)) ;
#69898 = CARTESIAN_POINT('Ctrl Pts',(-19.6976771545585,41.2580295002633,121.932097935364)) ;
#69899 = CARTESIAN_POINT('Ctrl Pts',(-19.6399945510564,41.0780404199004,122.228042530922)) ;
#69900 = CARTESIAN_POINT('Ctrl Pts',(-19.9516776747255,41.2680902143511,122.005343143406)) ;
#69901 = CARTESIAN_POINT('Ctrl Pts',(-19.8431952134582,41.0881011339882,122.286638869231)) ;
#69902 = CARTESIAN_POINT('Ctrl Pts',(-20.1841049252899,41.2779297173339,122.118737500505)) ;
#69903 = CARTESIAN_POINT('Ctrl Pts',(-20.0291359487438,41.097940636971,122.377353840953)) ;
#69904 = CARTESIAN_POINT('Ctrl Pts',(-20.3982213435744,41.2879958559003,122.273999666852)) ;
#69905 = CARTESIAN_POINT('Ctrl Pts',(-20.2004293795964,41.1080067755374,122.501563713022)) ;
#69906 = CARTESIAN_POINT('Ctrl Pts',(-20.5787589735412,41.2978783703863,122.460739928102)) ;
#69907 = CARTESIAN_POINT('Ctrl Pts',(-20.3448588816564,41.1178892900235,122.650955244937)) ;
#69908 = CARTESIAN_POINT('Ctrl Pts',(-20.7261276816334,41.3078706697419,122.678026456324)) ;
#69909 = CARTESIAN_POINT('Ctrl Pts',(-20.4627538900193,41.127881589379,122.82478422743)) ;
#69910 = CARTESIAN_POINT('Ctrl Pts',(-20.8332007283246,41.3178237366953,122.916705335846)) ;
#69911 = CARTESIAN_POINT('Ctrl Pts',(-20.5484123254759,41.1378346563324,123.01572688204)) ;
#69912 = CARTESIAN_POINT('Ctrl Pts',(-20.8976084793145,41.3278584449005,123.172399737523)) ;
#69913 = CARTESIAN_POINT('Ctrl Pts',(-20.5999387072137,41.1478693645376,123.220282482398)) ;
#69914 = CARTESIAN_POINT('Ctrl Pts',(-20.9165553817096,41.3377466658047,123.431576287923)) ;
#69915 = CARTESIAN_POINT('Ctrl Pts',(-20.6150963672015,41.1577575854418,123.427622853528)) ;
#69916 = CARTESIAN_POINT('Ctrl Pts',(-20.8903621464779,41.3477410888351,123.692895458737)) ;
#69917 = CARTESIAN_POINT('Ctrl Pts',(-20.5941421044658,41.1677520084722,123.636678055488)) ;
#69918 = CARTESIAN_POINT('Ctrl Pts',(-20.8194388311831,41.3576864282813,123.944442205965)) ;
#69919 = CARTESIAN_POINT('Ctrl Pts',(-20.5374038559839,41.1776973479184,123.837915073439)) ;
#69920 = CARTESIAN_POINT('Ctrl Pts',(-20.7063724848582,41.3676337728926,124.180145089931)) ;
#69921 = CARTESIAN_POINT('Ctrl Pts',(-20.446951356585,41.1876446925297,124.026477147799)) ;
#69922 = CARTESIAN_POINT('Ctrl Pts',(-20.5523289698857,41.3776816683036,124.394591659)) ;
#69923 = CARTESIAN_POINT('Ctrl Pts',(-20.3237167077923,41.1976925879407,124.198034766973)) ;
#69924 = CARTESIAN_POINT('Ctrl Pts',(-20.3673015896202,41.387529313783,124.575522794134)) ;
#69925 = CARTESIAN_POINT('Ctrl Pts',(-20.1756958838239,41.2075402334201,124.342779178533)) ;
#69926 = CARTESIAN_POINT('Ctrl Pts',(-20.1516704586702,41.397491027697,124.723938642442)) ;
#69927 = CARTESIAN_POINT('Ctrl Pts',(-20.0031916223503,41.2175019473341,124.461512149995)) ;
#69928 = CARTESIAN_POINT('Ctrl Pts',(-19.911780850099,41.4075196519879,124.833098044345)) ;
#69929 = CARTESIAN_POINT('Ctrl Pts',(-19.8112800810594,41.227530571625,124.548840178017)) ;
#69930 = CARTESIAN_POINT('Ctrl Pts',(-19.6596394073023,41.4174300126446,124.898243770015)) ;
#69931 = CARTESIAN_POINT('Ctrl Pts',(-19.6095677408918,41.2374409322817,124.600957108251)) ;
#69932 = CARTESIAN_POINT('Ctrl Pts',(-19.3994113076568,41.4273647112179,124.91935848404)) ;
#69933 = CARTESIAN_POINT('Ctrl Pts',(-19.4013858458597,41.247375630855,124.617849546606)) ;
#69934 = CARTESIAN_POINT('Ctrl Pts',(-19.1367143515178,41.4374065360721,124.894447395017)) ;
#69935 = CARTESIAN_POINT('Ctrl Pts',(-19.1912280682996,41.2574174557092,124.597921306122)) ;
#69936 = CARTESIAN_POINT('Ctrl Pts',(-18.8862194476765,41.4472911098165,124.825610729058)) ;
#69937 = CARTESIAN_POINT('Ctrl Pts',(-18.9908327711166,41.2673020294536,124.542852873517)) ;
#69938 = CARTESIAN_POINT('Ctrl Pts',(-18.6486170762246,41.4572929591797,124.713315149718)) ;
#69939 = CARTESIAN_POINT('Ctrl Pts',(-18.8007506471708,41.2773038788168,124.45301716696)) ;
#69940 = CARTESIAN_POINT('Ctrl Pts',(-18.4357242323319,41.4672122607537,124.562839022651)) ;
#69941 = CARTESIAN_POINT('Ctrl Pts',(-18.6304363934291,41.2872231803909,124.332637291821)) ;
#69942 = CARTESIAN_POINT('Ctrl Pts',(-18.2499195837942,41.477256369099,124.375398346987)) ;
#69943 = CARTESIAN_POINT('Ctrl Pts',(-18.4817919703577,41.2972672887361,124.182685211504)) ;
#69944 = CARTESIAN_POINT('Ctrl Pts',(-18.1017911287502,41.4871407925413,124.162007655832)) ;
#69945 = CARTESIAN_POINT('Ctrl Pts',(-18.3632889812558,41.3071517121784,124.011973815533)) ;
#69946 = CARTESIAN_POINT('Ctrl Pts',(-17.9909819762134,41.4971571544507,123.923238127084)) ;
#69947 = CARTESIAN_POINT('Ctrl Pts',(-18.27464077142,41.3171680740879,123.820958606205)) ;
#69948 = CARTESIAN_POINT('Ctrl Pts',(-17.9238542028585,41.5071938099561,123.66818572458)) ;
#69949 = CARTESIAN_POINT('Ctrl Pts',(-18.2209377383296,41.3272047295932,123.616916796119)) ;
#69950 = CARTESIAN_POINT('Ctrl Pts',(-17.9017753134138,41.5170239401454,123.410773438911)) ;
#69951 = CARTESIAN_POINT('Ctrl Pts',(-18.2032737428897,41.3370348597826,123.410988188349)) ;
#69952 = CARTESIAN_POINT('Ctrl Pts',(-17.9252038428856,41.5270999932353,123.147075094843)) ;
#69953 = CARTESIAN_POINT('Ctrl Pts',(-18.2220155951886,41.3471109128724,123.2000290831)) ;
#69954 = CARTESIAN_POINT('Ctrl Pts',(-17.9924242809587,41.5369522224211,122.896990000681)) ;
#69955 = CARTESIAN_POINT('Ctrl Pts',(-18.2757906890744,41.3569631420582,122.999961690913)) ;
#69956 = CARTESIAN_POINT('Ctrl Pts',(-18.1042623444851,41.5470254302204,122.657109249406)) ;
#69957 = CARTESIAN_POINT('Ctrl Pts',(-18.3652602896576,41.3670363498575,122.808056339764)) ;
#69958 = CARTESIAN_POINT('Ctrl Pts',(-18.2526543868681,41.5568669415718,122.445270485562)) ;
#69959 = CARTESIAN_POINT('Ctrl Pts',(-18.4839724495599,41.3768778612089,122.638585568541)) ;
#69960 = CARTESIAN_POINT('Ctrl Pts',(-18.4370777102109,41.5668278796093,122.259519138152)) ;
#69961 = CARTESIAN_POINT('Ctrl Pts',(-18.6315099644499,41.3868387992465,122.489983811783)) ;
#69962 = CARTESIAN_POINT('Ctrl Pts',(-18.6529080737898,41.5768657415343,122.107878162832)) ;
#69963 = CARTESIAN_POINT('Ctrl Pts',(-18.804173668292,41.3968766611714,122.368670011063)) ;
#69964 = CARTESIAN_POINT('Ctrl Pts',(-18.8877262423687,41.5867399275314,121.997383365689)) ;
#69965 = CARTESIAN_POINT('Ctrl Pts',(-18.9920269264179,41.4067508471685,122.280273361693)) ;
#69966 = CARTESIAN_POINT('Ctrl Pts',(-19.1430711045837,41.5968100871093,121.928030886543)) ;
#69967 = CARTESIAN_POINT('Ctrl Pts',(-19.1963027525332,41.4168210067464,122.22479007538)) ;
#69968 = CARTESIAN_POINT('Ctrl Pts',(-19.4003882644743,41.6066418345351,121.904466477439)) ;
#69969 = CARTESIAN_POINT('Ctrl Pts',(-19.4021553376179,41.4266527541722,122.205937341054)) ;
#69970 = CARTESIAN_POINT('Ctrl Pts',(-19.6632563157754,41.6166779146064,121.925697979521)) ;
#69971 = CARTESIAN_POINT('Ctrl Pts',(-19.6124499841248,41.4366888342435,122.222921102434)) ;
#69972 = CARTESIAN_POINT('Ctrl Pts',(-19.9178188413347,41.6266949614589,121.992773118902)) ;
#69973 = CARTESIAN_POINT('Ctrl Pts',(-19.8161003293912,41.446705881096,122.276579942071)) ;
#69974 = CARTESIAN_POINT('Ctrl Pts',(-20.1538480381938,41.6365772196255,122.10109797781)) ;
#69975 = CARTESIAN_POINT('Ctrl Pts',(-20.0049236160898,41.4565881392626,122.363238243392)) ;
#69976 = CARTESIAN_POINT('Ctrl Pts',(-20.3699075386073,41.6465649024218,122.250068895617)) ;
#69977 = CARTESIAN_POINT('Ctrl Pts',(-20.1777719215884,41.466575822059,122.482413671685)) ;
#69978 = CARTESIAN_POINT('Ctrl Pts',(-20.556247785553,41.6565115591386,122.433432011487)) ;
#69979 = CARTESIAN_POINT('Ctrl Pts',(-20.3268449195173,41.4765224787757,122.629102830338)) ;
#69980 = CARTESIAN_POINT('Ctrl Pts',(-20.7093408277522,41.6665686172188,122.648828544842)) ;
#69981 = CARTESIAN_POINT('Ctrl Pts',(-20.4493206451329,41.4865795368559,122.801419352681)) ;
#69982 = CARTESIAN_POINT('Ctrl Pts',(-20.8203574276063,41.6763867967682,122.881750559428)) ;
#69983 = CARTESIAN_POINT('Ctrl Pts',(-20.5381348730655,41.4963977164053,122.987755393131)) ;
#69984 = CARTESIAN_POINT('Ctrl Pts',(-20.8914554133569,41.6864227312072,123.135713115928)) ;
#69985 = CARTESIAN_POINT('Ctrl Pts',(-20.5950148896598,41.5064336508443,123.190925073507)) ;
#69986 = CARTESIAN_POINT('Ctrl Pts',(-20.9165972820437,41.6964473856362,123.397957733958)) ;
#69987 = CARTESIAN_POINT('Ctrl Pts',(-20.6151299031663,41.5164583052733,123.400720641268)) ;
#69988 = CARTESIAN_POINT('Ctrl Pts',(-20.8967522553727,41.7062994052157,123.656101312759)) ;
#69989 = CARTESIAN_POINT('Ctrl Pts',(-20.5992555699789,41.5263103248528,123.607234825418)) ;
#69990 = CARTESIAN_POINT('Ctrl Pts',(-20.8318758704315,41.7162903189306,123.910477841226)) ;
#69991 = CARTESIAN_POINT('Ctrl Pts',(-20.5473561475517,41.5363012385678,123.810736336764)) ;
#69992 = CARTESIAN_POINT('Ctrl Pts',(-20.7247343585358,41.7262083077702,124.148106422392)) ;
#69993 = CARTESIAN_POINT('Ctrl Pts',(-20.4616447029852,41.5462192274073,124.000839496386)) ;
#69994 = CARTESIAN_POINT('Ctrl Pts',(-20.5764123274112,41.736236418501,124.365906529172)) ;
#69995 = CARTESIAN_POINT('Ctrl Pts',(-20.3429885028579,41.5562473381381,124.175080585433)) ;
#69996 = CARTESIAN_POINT('Ctrl Pts',(-20.395206571467,41.7461216164094,124.552049981452)) ;
#69997 = CARTESIAN_POINT('Ctrl Pts',(-20.1980255691353,41.5661325360465,124.323996153329)) ;
#69998 = CARTESIAN_POINT('Ctrl Pts',(-20.1825881915492,41.7561108916774,124.706022484706)) ;
#69999 = CARTESIAN_POINT('Ctrl Pts',(-20.0279320600952,41.5761218113145,124.447175591284)) ;
#70000 = CARTESIAN_POINT('Ctrl Pts',(-19.944994054816,41.7661523498469,124.820818389465)) ;
#70001 = CARTESIAN_POINT('Ctrl Pts',(-19.837857454139,41.586163269484,124.539013942928)) ;
#70002 = CARTESIAN_POINT('Ctrl Pts',(-19.6965012965203,41.7759838136352,124.891575936423)) ;
#70003 = CARTESIAN_POINT('Ctrl Pts',(-19.6390644965111,41.5959947332723,124.595621546985)) ;
#70004 = CARTESIAN_POINT('Ctrl Pts',(-19.4350641759092,41.7859887459391,124.919157369809)) ;
#70005 = CARTESIAN_POINT('Ctrl Pts',(-19.4299150640357,41.6059996655762,124.61768861319)) ;
#70006 = CARTESIAN_POINT('Ctrl Pts',(-19.1732294916453,41.7959751098338,124.900811143185)) ;
#70007 = CARTESIAN_POINT('Ctrl Pts',(-19.2204473105258,41.615986029471,124.603013545684)) ;
#70008 = CARTESIAN_POINT('Ctrl Pts',(-18.9175714408772,41.8060047387197,124.836821562451)) ;
#70009 = CARTESIAN_POINT('Ctrl Pts',(-19.0159203902611,41.6260156583568,124.551823702806)) ;
#70010 = CARTESIAN_POINT('Ctrl Pts',(-18.6804315219461,41.8158799608281,124.731353527358)) ;
#70011 = CARTESIAN_POINT('Ctrl Pts',(-18.8262081643028,41.6358908804652,124.467451255553)) ;
#70012 = CARTESIAN_POINT('Ctrl Pts',(-18.4623421036418,41.8258811732252,124.584757637499)) ;
#70013 = CARTESIAN_POINT('Ctrl Pts',(-18.6517356019732,41.6458920928623,124.350176231393)) ;
#70014 = CARTESIAN_POINT('Ctrl Pts',(-18.2745387790295,41.8357897524607,124.404326737909)) ;
#70015 = CARTESIAN_POINT('Ctrl Pts',(-18.5014918287593,41.6558006720979,124.205833218676)) ;
#70016 = CARTESIAN_POINT('Ctrl Pts',(-18.1187665880947,41.8458446050167,124.190948411598)) ;
#70017 = CARTESIAN_POINT('Ctrl Pts',(-18.3768724125768,41.6658555246539,124.035131662587)) ;
#70018 = CARTESIAN_POINT('Ctrl Pts',(-18.0043751834666,41.8557031872915,123.958446111396)) ;
#70019 = CARTESIAN_POINT('Ctrl Pts',(-18.2853576981926,41.6757141069286,123.849131183936)) ;
#70020 = CARTESIAN_POINT('Ctrl Pts',(-17.93042449407,41.8657713167342,123.70445148532)) ;
#70021 = CARTESIAN_POINT('Ctrl Pts',(-18.2261951440607,41.6857822363713,123.645935938738)) ;
#70022 = CARTESIAN_POINT('Ctrl Pts',(-17.9023200741687,41.8756267884233,123.446967189866)) ;
#70023 = CARTESIAN_POINT('Ctrl Pts',(-18.2037096291495,41.6956377080604,123.439949220456)) ;
#70024 = CARTESIAN_POINT('Ctrl Pts',(-17.9188032302922,41.8856216368096,123.184839420313)) ;
#70025 = CARTESIAN_POINT('Ctrl Pts',(-18.2168940227441,41.7056325564467,123.23024695042)) ;
#70026 = CARTESIAN_POINT('Ctrl Pts',(-17.9813304619599,41.895652933594,122.928744998837)) ;
#70027 = CARTESIAN_POINT('Ctrl Pts',(-18.2669137962854,41.7156638532311,123.025370923546)) ;
#70028 = CARTESIAN_POINT('Ctrl Pts',(-18.0852555186611,41.9055194698041,122.691192079478)) ;
#70029 = CARTESIAN_POINT('Ctrl Pts',(-18.3500517412046,41.7255303894412,122.835328118647)) ;
#70030 = CARTESIAN_POINT('Ctrl Pts',(-18.2302333322929,41.9155068927649,122.472444933182)) ;
#70031 = CARTESIAN_POINT('Ctrl Pts',(-18.4660321429773,41.7355178124021,122.66032929391)) ;
#70032 = CARTESIAN_POINT('Ctrl Pts',(-18.4101690101242,41.9254518317847,122.282861709824)) ;
#70033 = CARTESIAN_POINT('Ctrl Pts',(-18.6099789904463,41.7454627514218,122.508661363733)) ;
#70034 = CARTESIAN_POINT('Ctrl Pts',(-18.6224325374237,41.9354967176447,122.125972345834)) ;
#70035 = CARTESIAN_POINT('Ctrl Pts',(-18.7797885429512,41.7555076372818,122.38314813357)) ;
#70036 = CARTESIAN_POINT('Ctrl Pts',(-18.8545248231622,41.9453652527309,122.010250360349)) ;
#70037 = CARTESIAN_POINT('Ctrl Pts',(-18.9654611095548,41.7653761723681,122.290568757108)) ;
#70038 = CARTESIAN_POINT('Ctrl Pts',(-19.1054113849967,41.9553311207376,121.935164518734)) ;
#70039 = CARTESIAN_POINT('Ctrl Pts',(-19.1661696157605,41.7753420403747,122.230497995113)) ;
#70040 = CARTESIAN_POINT('Ctrl Pts',(-19.3670697024523,41.9653537681901,121.904899528248)) ;
#70041 = CARTESIAN_POINT('Ctrl Pts',(-19.3754959860251,41.7853646878272,122.206283828786)) ;
#70042 = CARTESIAN_POINT('Ctrl Pts',(-19.6273839317657,41.9752774071977,121.920298317369)) ;
#70043 = CARTESIAN_POINT('Ctrl Pts',(-19.583747310097,41.7952883268348,122.218600653541)) ;
#70044 = CARTESIAN_POINT('Ctrl Pts',(-19.8817304496807,41.9852201322034,121.980174899417)) ;
#70045 = CARTESIAN_POINT('Ctrl Pts',(-19.7872249056599,41.8052310518406,122.266499716191)) ;
#70046 = CARTESIAN_POINT('Ctrl Pts',(-20.1241484576752,41.9952657382553,122.084651122132)) ;
#70047 = CARTESIAN_POINT('Ctrl Pts',(-19.9811601739826,41.8152766578924,122.350078652144)) ;
#70048 = CARTESIAN_POINT('Ctrl Pts',(-20.3408862916986,42.0051271607764,122.22675611249)) ;
#70049 = CARTESIAN_POINT('Ctrl Pts',(-20.1545514860313,41.8251380804135,122.463760663456)) ;
#70050 = CARTESIAN_POINT('Ctrl Pts',(-20.5324507967766,42.0151207292256,122.406346888385)) ;
#70051 = CARTESIAN_POINT('Ctrl Pts',(-20.3078045818973,41.8351316488627,122.607431606924)) ;
#70052 = CARTESIAN_POINT('Ctrl Pts',(-20.6890036597013,42.0250461999809,122.615019061482)) ;
#70053 = CARTESIAN_POINT('Ctrl Pts',(-20.4330486091548,41.845057119618,122.774367895725)) ;
#70054 = CARTESIAN_POINT('Ctrl Pts',(-20.808139363818,42.0350738739368,122.850031069966)) ;
#70055 = CARTESIAN_POINT('Ctrl Pts',(-20.528359143158,41.8550847935739,122.962376508046)) ;
#70056 = CARTESIAN_POINT('Ctrl Pts',(-20.8838479741626,42.0449610519785,123.098617303755)) ;
#70057 = CARTESIAN_POINT('Ctrl Pts',(-20.5889282071218,41.8649719716156,123.161244495286)) ;
#70058 = CARTESIAN_POINT('Ctrl Pts',(-20.9158670631571,42.0549894313466,123.360164459768)) ;
#70059 = CARTESIAN_POINT('Ctrl Pts',(-20.6145455234739,41.8750003509838,123.370482841574)) ;
#70060 = CARTESIAN_POINT('Ctrl Pts',(-20.9023097751863,42.0648836740681,123.619854631483)) ;
#70061 = CARTESIAN_POINT('Ctrl Pts',(-20.6037026459315,41.8848945937052,123.578231501373)) ;
#70062 = CARTESIAN_POINT('Ctrl Pts',(-20.8237470249053,42.078236590719,123.961816174747)) ;
#70063 = CARTESIAN_POINT('Ctrl Pts',(-20.540851905552,41.8982475103561,123.851818955548)) ;
#70064 = CARTESIAN_POINT('Ctrl Pts',(-20.6595997814835,42.0914391084657,124.272009590654)) ;
#70065 = CARTESIAN_POINT('Ctrl Pts',(-20.4095171791971,41.9114500281029,124.099990022592)) ;
#70066 = CARTESIAN_POINT('Ctrl Pts',(-20.4209837962718,42.1047950137467,124.529355053645)) ;
#70067 = CARTESIAN_POINT('Ctrl Pts',(-20.2186534466242,41.9248059333838,124.305833005313)) ;
#70068 = CARTESIAN_POINT('Ctrl Pts',(-20.2138409514704,42.1146916623845,124.686668820964)) ;
#70069 = CARTESIAN_POINT('Ctrl Pts',(-20.0529350989336,41.9347025820217,124.431692934571)) ;
#70070 = CARTESIAN_POINT('Ctrl Pts',(-19.9790784982733,42.124739800437,124.807498749042)) ;
#70071 = CARTESIAN_POINT('Ctrl Pts',(-19.8651277057987,41.9447507200741,124.528356915192)) ;
#70072 = CARTESIAN_POINT('Ctrl Pts',(-19.7308134332186,42.1346307606148,124.884508092935)) ;
#70073 = CARTESIAN_POINT('Ctrl Pts',(-19.6665158148451,41.9546416802519,124.589967046328)) ;
#70074 = CARTESIAN_POINT('Ctrl Pts',(-19.4703782998092,42.1446235964915,124.918232356421)) ;
#70075 = CARTESIAN_POINT('Ctrl Pts',(-19.4581682824578,41.9646345161287,124.616948547809)) ;
#70076 = CARTESIAN_POINT('Ctrl Pts',(-19.2068788945409,42.1546626914931,124.905562765929)) ;
#70077 = CARTESIAN_POINT('Ctrl Pts',(-19.2473681313206,41.9746736111302,124.606814984764)) ;
#70078 = CARTESIAN_POINT('Ctrl Pts',(-18.9545800921988,42.1645000473443,124.849083179674)) ;
#70079 = CARTESIAN_POINT('Ctrl Pts',(-19.0455306742898,41.9845109669814,124.56163402756)) ;
#70080 = CARTESIAN_POINT('Ctrl Pts',(-18.629663451881,42.177892995275,124.713940021359)) ;
#70081 = CARTESIAN_POINT('Ctrl Pts',(-18.7855850543186,41.9979039149121,124.453519158685)) ;
#70082 = CARTESIAN_POINT('Ctrl Pts',(-18.3520925365356,42.1910596717019,124.500678451702)) ;
#70083 = CARTESIAN_POINT('Ctrl Pts',(-18.5635083043611,42.0110705913391,124.282885722299)) ;
#70084 = CARTESIAN_POINT('Ctrl Pts',(-18.1378563760038,42.2044444531087,124.221781306289)) ;
#70085 = CARTESIAN_POINT('Ctrl Pts',(-18.3921499280378,42.0244553727458,124.059804293663)) ;
#70086 = CARTESIAN_POINT('Ctrl Pts',(-18.0179616237773,42.2143062357526,123.991978653527)) ;
#70087 = CARTESIAN_POINT('Ctrl Pts',(-18.2962255485433,42.0343171553897,123.875955881791)) ;
#70088 = CARTESIAN_POINT('Ctrl Pts',(-17.9383202716689,42.2243053837056,123.741625973935)) ;
#70089 = CARTESIAN_POINT('Ctrl Pts',(-18.2325120682241,42.0443163033428,123.675676550641)) ;
#70090 = CARTESIAN_POINT('Ctrl Pts',(-17.9034419632737,42.2342081763227,123.483683307464)) ;
#70091 = CARTESIAN_POINT('Ctrl Pts',(-18.2046075051605,42.0542190959598,123.469320792753)) ;
#70092 = CARTESIAN_POINT('Ctrl Pts',(-17.9141036164672,42.2442577562136,123.21987047093)) ;
#70093 = CARTESIAN_POINT('Ctrl Pts',(-18.2131325074826,42.0642686758508,123.258274986974)) ;
#70094 = CARTESIAN_POINT('Ctrl Pts',(-17.9873542558445,42.2574448300231,122.881031053165)) ;
#70095 = CARTESIAN_POINT('Ctrl Pts',(-18.2717422460334,42.0774557496602,122.987181397706)) ;
#70096 = CARTESIAN_POINT('Ctrl Pts',(-18.1910268972478,42.2741976199943,122.48527825742)) ;
#70097 = CARTESIAN_POINT('Ctrl Pts',(-18.4346521928802,42.0942085396314,122.670610268033)) ;
#70098 = CARTESIAN_POINT('Ctrl Pts',(-18.5127023287359,42.290686272089,122.187393477367)) ;
#70099 = CARTESIAN_POINT('Ctrl Pts',(-18.6920409981402,42.1106971917261,122.432258549758)) ;
#70100 = CARTESIAN_POINT('Ctrl Pts',(-18.8227825349679,42.3040430982724,122.023091316242)) ;
#70101 = CARTESIAN_POINT('Ctrl Pts',(-18.9400618893494,42.1240540179095,122.300845856215)) ;
#70102 = CARTESIAN_POINT('Ctrl Pts',(-19.0702507619016,42.3139394831503,121.942948929694)) ;
#70103 = CARTESIAN_POINT('Ctrl Pts',(-19.1380453748036,42.1339504027875,122.236723914257)) ;
#70104 = CARTESIAN_POINT('Ctrl Pts',(-19.3305991665012,42.3239459976708,121.906474651851)) ;
#70105 = CARTESIAN_POINT('Ctrl Pts',(-19.3463190360728,42.1439569173079,122.2075435789)) ;
#70106 = CARTESIAN_POINT('Ctrl Pts',(-19.6771578660426,42.3371361211872,121.917859655171)) ;
#70107 = CARTESIAN_POINT('Ctrl Pts',(-19.623580039702,42.1571470408243,122.216652401464)) ;
#70108 = CARTESIAN_POINT('Ctrl Pts',(-20.1032957575407,42.3539026823368,122.047670197675)) ;
#70109 = CARTESIAN_POINT('Ctrl Pts',(-19.9644762057803,42.1739136019739,122.320493865006)) ;
#70110 = CARTESIAN_POINT('Ctrl Pts',(-20.5238873611168,42.3736871710448,122.363526341007)) ;
#70111 = CARTESIAN_POINT('Ctrl Pts',(-20.3009572541404,42.1936980906819,122.573177890101)) ;
#70112 = CARTESIAN_POINT('Ctrl Pts',(-20.8150059840566,42.3936326186413,122.806396279347)) ;
#70113 = CARTESIAN_POINT('Ctrl Pts',(-20.5338537200683,42.2136435382784,122.927472140951)) ;
#70114 = CARTESIAN_POINT('Ctrl Pts',(-20.9368565339894,42.4135442807972,123.32140844695)) ;
#70115 = CARTESIAN_POINT('Ctrl Pts',(-20.6313376522247,42.2335552004343,123.33948182386)) ;
#70116 = CARTESIAN_POINT('Ctrl Pts',(-20.8768601174002,42.4334364728161,123.846776921239)) ;
#70117 = CARTESIAN_POINT('Ctrl Pts',(-20.583342978862,42.2534473924532,123.759777675271)) ;
#70118 = CARTESIAN_POINT('Ctrl Pts',(-20.6387749464663,42.4534776033707,124.323184054214)) ;
#70119 = CARTESIAN_POINT('Ctrl Pts',(-20.3928775130821,42.2734885230078,124.140904294275)) ;
#70120 = CARTESIAN_POINT('Ctrl Pts',(-20.2567515623942,42.4732959379863,124.686015098705)) ;
#70121 = CARTESIAN_POINT('Ctrl Pts',(-20.087259484934,42.2933068576234,124.431172000379)) ;
#70122 = CARTESIAN_POINT('Ctrl Pts',(-19.7707111217134,42.4932685032059,124.899002007876)) ;
#70123 = CARTESIAN_POINT('Ctrl Pts',(-19.6984277079127,42.313279422843,124.601563631414)) ;
#70124 = CARTESIAN_POINT('Ctrl Pts',(-19.2430064355605,42.5131577193775,124.933361056965)) ;
#70125 = CARTESIAN_POINT('Ctrl Pts',(-19.2762631018856,42.3331686390146,124.629052843148)) ;
#70126 = CARTESIAN_POINT('Ctrl Pts',(-18.7322443545962,42.5331812937002,124.784326245752)) ;
#70127 = CARTESIAN_POINT('Ctrl Pts',(-18.8676531273989,42.3531922133373,124.509826918718)) ;
#70128 = CARTESIAN_POINT('Ctrl Pts',(-18.3074466869106,42.5529784567885,124.473672881631)) ;
#70129 = CARTESIAN_POINT('Ctrl Pts',(-18.5278123342791,42.3729893764256,124.261304267751)) ;
#70130 = CARTESIAN_POINT('Ctrl Pts',(-18.0107152101051,42.5729439506122,124.03387590139)) ;
#70131 = CARTESIAN_POINT('Ctrl Pts',(-18.2904261458476,42.3929548702494,123.909466818997)) ;
#70132 = CARTESIAN_POINT('Ctrl Pts',(-17.8825244705871,42.5928976583536,123.51911914368)) ;
#70133 = CARTESIAN_POINT('Ctrl Pts',(-18.1878724815504,42.4129085779908,123.497661231514)) ;
#70134 = CARTESIAN_POINT('Ctrl Pts',(-17.9375074674537,42.6128050350802,122.992998485349)) ;
#70135 = CARTESIAN_POINT('Ctrl Pts',(-18.2318581752466,42.4328159547174,123.076763483073)) ;
#70136 = CARTESIAN_POINT('Ctrl Pts',(-18.1669062692067,42.6326572466288,122.517738273591)) ;
#70137 = CARTESIAN_POINT('Ctrl Pts',(-18.4153780968803,42.4526681662659,122.696553635092)) ;
#70138 = CARTESIAN_POINT('Ctrl Pts',(-18.5491943143349,42.6527296335745,122.145651577482)) ;
#70139 = CARTESIAN_POINT('Ctrl Pts',(-18.721207849793,42.4727405532116,122.398884952664)) ;
#70140 = CARTESIAN_POINT('Ctrl Pts',(-19.0301333322148,42.6725675032148,121.929544757103)) ;
#70141 = CARTESIAN_POINT('Ctrl Pts',(-19.1059609684924,42.4925784228519,122.225998529547)) ;
#70142 = CARTESIAN_POINT('Ctrl Pts',(-19.5561067931665,42.6924181577679,121.88822002276)) ;
#70143 = CARTESIAN_POINT('Ctrl Pts',(-19.5267415619836,42.5124290774051,122.19293977911)) ;
#70144 = CARTESIAN_POINT('Ctrl Pts',(-20.0695211678143,42.7124700921084,122.031029897398)) ;
#70145 = CARTESIAN_POINT('Ctrl Pts',(-19.9374722246251,42.5324810117455,122.307188485913)) ;
#70146 = CARTESIAN_POINT('Ctrl Pts',(-20.4987389792293,42.7323032796744,122.33724488066)) ;
#70147 = CARTESIAN_POINT('Ctrl Pts',(-20.2808472827428,42.5523141993116,122.552162457419)) ;
#70148 = CARTESIAN_POINT('Ctrl Pts',(-20.7998323714999,42.7522324919051,122.772792578482)) ;
#70149 = CARTESIAN_POINT('Ctrl Pts',(-20.5217209763658,42.5722434115422,122.900602245168)) ;
#70150 = CARTESIAN_POINT('Ctrl Pts',(-20.9346324231233,42.7721174571195,123.284031475315)) ;
#70151 = CARTESIAN_POINT('Ctrl Pts',(-20.6295592175581,42.5921283767566,123.309594871732)) ;
#70152 = CARTESIAN_POINT('Ctrl Pts',(-20.8856369561692,42.7921911982641,123.815196128951)) ;
#70153 = CARTESIAN_POINT('Ctrl Pts',(-20.5903609317186,42.6122021179012,123.734525730611)) ;
#70154 = CARTESIAN_POINT('Ctrl Pts',(-20.6614795251124,42.8119843800445,124.291210805294)) ;
#70155 = CARTESIAN_POINT('Ctrl Pts',(-20.4110322484531,42.6319952996816,124.115338243655)) ;
#70156 = CARTESIAN_POINT('Ctrl Pts',(-20.2863715695943,42.8319470880472,124.666388958395)) ;
#70157 = CARTESIAN_POINT('Ctrl Pts',(-20.1109437039454,42.6519580076843,124.415478939255)) ;
#70158 = CARTESIAN_POINT('Ctrl Pts',(-19.8046741907438,42.8519300397896,124.890126754003)) ;
#70159 = CARTESIAN_POINT('Ctrl Pts',(-19.7255846106919,42.6719409594268,124.594466924686)) ;
#70160 = CARTESIAN_POINT('Ctrl Pts',(-19.2801592562473,42.8717406595618,124.936699673532)) ;
#70161 = CARTESIAN_POINT('Ctrl Pts',(-19.3059710215937,42.6917515791989,124.631722408354)) ;
#70162 = CARTESIAN_POINT('Ctrl Pts',(-18.7667862152892,42.8917243755947,124.800954951219)) ;
#70163 = CARTESIAN_POINT('Ctrl Pts',(-18.8952733417193,42.7117352952318,124.523123451149)) ;
#70164 = CARTESIAN_POINT('Ctrl Pts',(-18.3326279856665,42.911605839492,124.499507379797)) ;
#70165 = CARTESIAN_POINT('Ctrl Pts',(-18.5479481189047,42.7316167591292,124.281962249473)) ;
#70166 = CARTESIAN_POINT('Ctrl Pts',(-18.0260984755986,42.9315611693364,124.066807185146)) ;
#70167 = CARTESIAN_POINT('Ctrl Pts',(-18.3027271574083,42.7515720889735,123.935799951114)) ;
#70168 = CARTESIAN_POINT('Ctrl Pts',(-17.8857662260403,42.9514366301419,123.557444062347)) ;
#70169 = CARTESIAN_POINT('Ctrl Pts',(-18.1904651245614,42.771447549779,123.528307551792)) ;
#70170 = CARTESIAN_POINT('Ctrl Pts',(-17.9275815086194,42.9714209501934,123.027999899649)) ;
#70171 = CARTESIAN_POINT('Ctrl Pts',(-18.2239197641623,42.7914318698305,123.104753757388)) ;
#70172 = CARTESIAN_POINT('Ctrl Pts',(-18.1472767537667,42.991348982983,122.545930346273)) ;
#70173 = CARTESIAN_POINT('Ctrl Pts',(-18.3996848299053,42.8113599026202,122.719094732473)) ;
#70174 = CARTESIAN_POINT('Ctrl Pts',(-18.4563016259536,43.0079577449228,122.230836526374)) ;
#70175 = CARTESIAN_POINT('Ctrl Pts',(-18.6468908763838,42.82796866456,122.467036542162)) ;
#70176 = CARTESIAN_POINT('Ctrl Pts',(-18.7544287787532,43.0211453836129,122.054087877132)) ;
#70177 = CARTESIAN_POINT('Ctrl Pts',(-18.8854094489693,42.84115630325,122.325626725663)) ;
#70178 = CARTESIAN_POINT('Ctrl Pts',(-18.9997521034799,43.031131817973,121.960916807132)) ;
#70179 = CARTESIAN_POINT('Ctrl Pts',(-19.0816631635093,42.8511427376102,122.251094035391)) ;
#70180 = CARTESIAN_POINT('Ctrl Pts',(-19.2581944108813,43.0411411919324,121.911902702877)) ;
#70181 = CARTESIAN_POINT('Ctrl Pts',(-19.2884287994832,42.8611521115695,122.211885725831)) ;
#70182 = CARTESIAN_POINT('Ctrl Pts',(-19.6074202778413,43.0544312254977,121.907165841963)) ;
#70183 = CARTESIAN_POINT('Ctrl Pts',(-19.5677560175321,42.8744421451348,122.208091120847)) ;
#70184 = CARTESIAN_POINT('Ctrl Pts',(-20.0350687767284,43.0710252131601,122.015093622791)) ;
#70185 = CARTESIAN_POINT('Ctrl Pts',(-19.9099409302065,42.8910361327973,122.294450399826)) ;
#70186 = CARTESIAN_POINT('Ctrl Pts',(-20.4010277793674,43.0876574684357,122.26302842487)) ;
#70187 = CARTESIAN_POINT('Ctrl Pts',(-20.2026637544341,42.9076683880728,122.492780756029)) ;
#70188 = CARTESIAN_POINT('Ctrl Pts',(-20.6289019817072,43.1008998521035,122.526052209373)) ;
#70189 = CARTESIAN_POINT('Ctrl Pts',(-20.3849854274242,42.9209107717406,122.70321807601)) ;
#70190 = CARTESIAN_POINT('Ctrl Pts',(-20.7634137015571,43.1108140603309,122.749188831555)) ;
#70191 = CARTESIAN_POINT('Ctrl Pts',(-20.49258810908,42.9308249799681,122.881725181544)) ;
#70192 = CARTESIAN_POINT('Ctrl Pts',(-20.8581936477321,43.1208706996026,122.995865179697)) ;
#70193 = CARTESIAN_POINT('Ctrl Pts',(-20.5684111153363,42.9408816192397,123.079068425544)) ;
#70194 = CARTESIAN_POINT('Ctrl Pts',(-20.9079570487934,43.1307165060227,123.249794573028)) ;
#70195 = CARTESIAN_POINT('Ctrl Pts',(-20.6082199684139,42.9507274256599,123.282209957339)) ;
#70196 = CARTESIAN_POINT('Ctrl Pts',(-20.9134264774939,43.1407615056559,123.513697714177)) ;
#70197 = CARTESIAN_POINT('Ctrl Pts',(-20.6125910612325,42.960772425293,123.493341293603)) ;
#70198 = CARTESIAN_POINT('Ctrl Pts',(-20.8594473356749,43.1540425280286,123.858497845333)) ;
#70199 = CARTESIAN_POINT('Ctrl Pts',(-20.569416250521,42.9740534476658,123.769136972112)) ;
#70200 = CARTESIAN_POINT('Ctrl Pts',(-20.718508196259,43.1672399745533,124.17971260659)) ;
#70201 = CARTESIAN_POINT('Ctrl Pts',(-20.4566616453272,42.9872508941904,124.026134275498)) ;
#70202 = CARTESIAN_POINT('Ctrl Pts',(-20.4978485962577,43.1806542723603,124.454637161235)) ;
#70203 = CARTESIAN_POINT('Ctrl Pts',(-20.2801208442663,43.0006651919974,124.246084216616)) ;
#70204 = CARTESIAN_POINT('Ctrl Pts',(-20.3035425807458,43.190493337763,124.625241624044)) ;
#70205 = CARTESIAN_POINT('Ctrl Pts',(-20.124676701218,43.0105042574002,124.382563655871)) ;
#70206 = CARTESIAN_POINT('Ctrl Pts',(-20.0797235876443,43.2004765440407,124.762051652017)) ;
#70207 = CARTESIAN_POINT('Ctrl Pts',(-19.9456197990869,43.0204874636778,124.492010372349)) ;
#70208 = CARTESIAN_POINT('Ctrl Pts',(-19.8362597616934,43.2104277789535,124.8575472145)) ;
#70209 = CARTESIAN_POINT('Ctrl Pts',(-19.7508481203091,43.0304386985906,124.568404524437)) ;
#70210 = CARTESIAN_POINT('Ctrl Pts',(-19.5786965198764,43.2204287786551,124.909888505183)) ;
#70211 = CARTESIAN_POINT('Ctrl Pts',(-19.544797096,43.0404396982923,124.610275379233)) ;
#70212 = CARTESIAN_POINT('Ctrl Pts',(-19.3151648430061,43.2304601244425,124.916319914135)) ;
#70213 = CARTESIAN_POINT('Ctrl Pts',(-19.3339717561267,43.0504710440796,124.615418233467)) ;
#70214 = CARTESIAN_POINT('Ctrl Pts',(-19.0590709276985,43.2403138891475,124.877945266862)) ;
#70215 = CARTESIAN_POINT('Ctrl Pts',(-19.1290970496758,43.0603248087846,124.584716300181)) ;
#70216 = CARTESIAN_POINT('Ctrl Pts',(-18.8104522663154,43.2502845428158,124.79531472401)) ;
#70217 = CARTESIAN_POINT('Ctrl Pts',(-18.9302029191281,43.0702954624529,124.518609759504)) ;
#70218 = CARTESIAN_POINT('Ctrl Pts',(-18.5792880259183,43.260281786473,124.670397983482)) ;
#70219 = CARTESIAN_POINT('Ctrl Pts',(-18.7452726496911,43.0802927061101,124.418674422827)) ;
#70220 = CARTESIAN_POINT('Ctrl Pts',(-18.3728375783555,43.2703152424172,124.506422572522)) ;
#70221 = CARTESIAN_POINT('Ctrl Pts',(-18.5801137193159,43.0903261620543,124.287492345244)) ;
#70222 = CARTESIAN_POINT('Ctrl Pts',(-18.2007504134058,43.2801707467176,124.31283503278)) ;
#70223 = CARTESIAN_POINT('Ctrl Pts',(-18.4424457883443,43.1001816663547,124.132620965001)) ;
#70224 = CARTESIAN_POINT('Ctrl Pts',(-18.0626456729148,43.2901701830037,124.089333194053)) ;
#70225 = CARTESIAN_POINT('Ctrl Pts',(-18.3319639343597,43.1101811026408,123.953818381161)) ;
#70226 = CARTESIAN_POINT('Ctrl Pts',(-17.9661552350075,43.3000646425196,123.847830753989)) ;
#70227 = CARTESIAN_POINT('Ctrl Pts',(-18.2547737161696,43.1200755621567,123.760615804186)) ;
#70228 = CARTESIAN_POINT('Ctrl Pts',(-17.9122545173091,43.3101277619712,123.588980661551)) ;
#70229 = CARTESIAN_POINT('Ctrl Pts',(-18.2116553113845,43.1301386816084,123.55353524895)) ;
#70230 = CARTESIAN_POINT('Ctrl Pts',(-17.9040100749574,43.3199673963832,123.330493713353)) ;
#70231 = CARTESIAN_POINT('Ctrl Pts',(-18.2050619671359,43.1399783160204,123.346745951152)) ;
#70232 = CARTESIAN_POINT('Ctrl Pts',(-17.9412644855324,43.330030603869,123.068717754911)) ;
#70233 = CARTESIAN_POINT('Ctrl Pts',(-18.2348676608804,43.1500415235061,123.137325455349)) ;
#70234 = CARTESIAN_POINT('Ctrl Pts',(-18.0222521551209,43.3399247112482,122.821614169064)) ;
#70235 = CARTESIAN_POINT('Ctrl Pts',(-18.2996598001454,43.1599356308853,122.939643522461)) ;
#70236 = CARTESIAN_POINT('Ctrl Pts',(-18.1448649357578,43.3498670434406,122.590937416187)) ;
#70237 = CARTESIAN_POINT('Ctrl Pts',(-18.3977518184139,43.1698779630777,122.755103312914)) ;
#70238 = CARTESIAN_POINT('Ctrl Pts',(-18.3065565946206,43.3598676697556,122.383706851709)) ;
#70239 = CARTESIAN_POINT('Ctrl Pts',(-18.5271067799686,43.1798785893927,122.589320225833)) ;
#70240 = CARTESIAN_POINT('Ctrl Pts',(-18.5028573530525,43.3699094040375,122.207385535582)) ;
#70241 = CARTESIAN_POINT('Ctrl Pts',(-18.6841488602168,43.1899203236746,122.448264772866)) ;
#70242 = CARTESIAN_POINT('Ctrl Pts',(-18.7217003533941,43.3797348299866,122.070323331608)) ;
#70243 = CARTESIAN_POINT('Ctrl Pts',(-18.8592239561885,43.1997457496237,122.338617074552)) ;
#70244 = CARTESIAN_POINT('Ctrl Pts',(-18.9664691272905,43.3897916565143,121.970708884775)) ;
#70245 = CARTESIAN_POINT('Ctrl Pts',(-19.0550398228914,43.2098025761514,122.258927422049)) ;
#70246 = CARTESIAN_POINT('Ctrl Pts',(-19.2216018609428,43.3997190896358,121.916174470016)) ;
#70247 = CARTESIAN_POINT('Ctrl Pts',(-19.2591461961739,43.219730009273,122.215302017841)) ;
#70248 = CARTESIAN_POINT('Ctrl Pts',(-19.4828888562582,43.4096690820421,121.905998966867)) ;
#70249 = CARTESIAN_POINT('Ctrl Pts',(-19.4681756430009,43.2296800016792,122.207163663939)) ;
#70250 = CARTESIAN_POINT('Ctrl Pts',(-19.7446216548047,43.4197242831161,121.942178613796)) ;
#70251 = CARTESIAN_POINT('Ctrl Pts',(-19.6775616803327,43.2397352027532,122.236109468103)) ;
#70252 = CARTESIAN_POINT('Ctrl Pts',(-19.9904509322207,43.4295465571684,122.02094445218)) ;
#70253 = CARTESIAN_POINT('Ctrl Pts',(-19.8742238828704,43.2495574768055,122.299123887706)) ;
#70254 = CARTESIAN_POINT('Ctrl Pts',(-20.2244870380784,43.4396024511276,122.143621831466)) ;
#70255 = CARTESIAN_POINT('Ctrl Pts',(-20.0614519256092,43.2596133707647,122.397267588395)) ;
#70256 = CARTESIAN_POINT('Ctrl Pts',(-20.4310096168158,43.4495431729727,122.303608199071)) ;
#70257 = CARTESIAN_POINT('Ctrl Pts',(-20.2266685268885,43.2695540926099,122.525258131967)) ;
#70258 = CARTESIAN_POINT('Ctrl Pts',(-20.6065731184016,43.4594475170593,122.495763120482)) ;
#70259 = CARTESIAN_POINT('Ctrl Pts',(-20.3671176119606,43.2794584366965,122.678983058845)) ;
#70260 = CARTESIAN_POINT('Ctrl Pts',(-20.7479541652507,43.4694941843588,122.718707024721)) ;
#70261 = CARTESIAN_POINT('Ctrl Pts',(-20.4802208409037,43.2895051039959,122.857339300646)) ;
#70262 = CARTESIAN_POINT('Ctrl Pts',(-20.8472092355886,43.4793897428087,122.95911028977)) ;
#70263 = CARTESIAN_POINT('Ctrl Pts',(-20.5596229418343,43.2994006624459,123.049662215042)) ;
#70264 = CARTESIAN_POINT('Ctrl Pts',(-20.904139618028,43.4894518215134,123.217291078424)) ;
#70265 = CARTESIAN_POINT('Ctrl Pts',(-20.6051653985535,43.3094627411505,123.256207403565)) ;
#70266 = CARTESIAN_POINT('Ctrl Pts',(-20.9152824166523,43.4992945199792,123.475736104278)) ;
#70267 = CARTESIAN_POINT('Ctrl Pts',(-20.6140777067984,43.3193054396163,123.462962813021)) ;
#70268 = CARTESIAN_POINT('Ctrl Pts',(-20.8814961280243,43.5092852938737,123.736067222342)) ;
#70269 = CARTESIAN_POINT('Ctrl Pts',(-20.5870468982505,43.3292962135108,123.671227335157)) ;
#70270 = CARTESIAN_POINT('Ctrl Pts',(-20.8034587033046,43.5192131631086,123.985028739388)) ;
#70271 = CARTESIAN_POINT('Ctrl Pts',(-20.5246153423973,43.3392240827457,123.870395633847)) ;
#70272 = CARTESIAN_POINT('Ctrl Pts',(-20.6830540646815,43.5292018920784,124.218293703487)) ;
#70273 = CARTESIAN_POINT('Ctrl Pts',(-20.4282901545074,43.3492128117156,124.057006673629)) ;
#70274 = CARTESIAN_POINT('Ctrl Pts',(-20.5227971110946,43.5392412940622,124.427851205494)) ;
#70275 = CARTESIAN_POINT('Ctrl Pts',(-20.3000830928166,43.3592522136993,124.224651637506)) ;
#70276 = CARTESIAN_POINT('Ctrl Pts',(-20.3327674227349,43.549081461799,124.603250592089)) ;
#70277 = CARTESIAN_POINT('Ctrl Pts',(-20.1480587518174,43.3690923814361,124.36496932946)) ;
#70278 = CARTESIAN_POINT('Ctrl Pts',(-20.1108004287422,43.5591296721735,124.746255706704)) ;
#70279 = CARTESIAN_POINT('Ctrl Pts',(-19.9704841479097,43.3791405918106,124.479372086508)) ;
#70280 = CARTESIAN_POINT('Ctrl Pts',(-19.8696476488821,43.5690768424612,124.84714360705)) ;
#70281 = CARTESIAN_POINT('Ctrl Pts',(-19.7775615548716,43.3890877620984,124.560080670385)) ;
#70282 = CARTESIAN_POINT('Ctrl Pts',(-19.6157403076391,43.5789876907163,124.905179129313)) ;
#70283 = CARTESIAN_POINT('Ctrl Pts',(-19.5744358437637,43.3989986103534,124.606507405916)) ;
#70284 = CARTESIAN_POINT('Ctrl Pts',(-19.3518069355752,43.5890440183941,124.91818859538)) ;
#70285 = CARTESIAN_POINT('Ctrl Pts',(-19.3632888855343,43.4090549380312,124.616913341816)) ;
#70286 = CARTESIAN_POINT('Ctrl Pts',(-19.0949363387433,43.5988944311626,124.886068138014)) ;
#70287 = CARTESIAN_POINT('Ctrl Pts',(-19.1577934324893,43.4189053507997,124.591215484819)) ;
#70288 = CARTESIAN_POINT('Ctrl Pts',(-18.8429401699179,43.6089213169963,124.809086046414)) ;
#70289 = CARTESIAN_POINT('Ctrl Pts',(-18.9561969026727,43.4289322366334,124.529628381766)) ;
#70290 = CARTESIAN_POINT('Ctrl Pts',(-18.608395133658,43.6189499326271,124.688881455388)) ;
#70291 = CARTESIAN_POINT('Ctrl Pts',(-18.7685615614303,43.4389608522643,124.433463244299)) ;
#70292 = CARTESIAN_POINT('Ctrl Pts',(-18.4018522456686,43.6287951560046,124.53309241998)) ;
#70293 = CARTESIAN_POINT('Ctrl Pts',(-18.6033288833992,43.4488060756417,124.308831339944)) ;
#70294 = CARTESIAN_POINT('Ctrl Pts',(-18.2223621198309,43.6387858381062,124.34147662207)) ;
#70295 = CARTESIAN_POINT('Ctrl Pts',(-18.4597378987131,43.4587967577433,124.15553787085)) ;
#70296 = CARTESIAN_POINT('Ctrl Pts',(-18.0786893213183,43.6488237267386,124.120254417819)) ;
#70297 = CARTESIAN_POINT('Ctrl Pts',(-18.344800860244,43.4688346463758,123.97855920037)) ;
#70298 = CARTESIAN_POINT('Ctrl Pts',(-17.977176387725,43.6586680618418,123.882292776737)) ;
#70299 = CARTESIAN_POINT('Ctrl Pts',(-18.2635921771929,43.4786789814789,123.788190198657)) ;
#70300 = CARTESIAN_POINT('Ctrl Pts',(-17.917193628408,43.6686530240393,123.626883148383)) ;
#70301 = CARTESIAN_POINT('Ctrl Pts',(-18.2156072828888,43.4886639436764,123.583862392775)) ;
#70302 = CARTESIAN_POINT('Ctrl Pts',(-17.9024116244684,43.6785919655727,123.366078461576)) ;
#70303 = CARTESIAN_POINT('Ctrl Pts',(-18.2037829771252,43.4986028852098,123.375219006614)) ;
#70304 = CARTESIAN_POINT('Ctrl Pts',(-17.9335320666697,43.6886338505441,123.104055220491)) ;
#70305 = CARTESIAN_POINT('Ctrl Pts',(-18.2286806289882,43.5086447701812,123.165600448032)) ;
#70306 = CARTESIAN_POINT('Ctrl Pts',(-18.008352723709,43.6985203984524,122.855226846736)) ;
#70307 = CARTESIAN_POINT('Ctrl Pts',(-18.2885381427592,43.5185313180895,122.966538824401)) ;
#70308 = CARTESIAN_POINT('Ctrl Pts',(-18.1261385188554,43.7085143239524,122.620528575572)) ;
#70309 = CARTESIAN_POINT('Ctrl Pts',(-18.3827677656657,43.5285252435895,122.778780862316)) ;
#70310 = CARTESIAN_POINT('Ctrl Pts',(-18.2819245676956,43.7184504150789,122.410933846051)) ;
#70311 = CARTESIAN_POINT('Ctrl Pts',(-18.5073972462572,43.538461334716,122.61110613432)) ;
#70312 = CARTESIAN_POINT('Ctrl Pts',(-18.4734970875813,43.7284796840588,122.229979319978)) ;
#70313 = CARTESIAN_POINT('Ctrl Pts',(-18.6606561040544,43.5484906036959,122.466343315554)) ;
#70314 = CARTESIAN_POINT('Ctrl Pts',(-18.6902358432055,43.7383620666181,122.086843147979)) ;
#70315 = CARTESIAN_POINT('Ctrl Pts',(-18.8340470312142,43.5583729862552,122.351835729643)) ;
#70316 = CARTESIAN_POINT('Ctrl Pts',(-18.9325293093004,43.748414583706,121.981687073779)) ;
#70317 = CARTESIAN_POINT('Ctrl Pts',(-19.0278824125168,43.5684255033431,122.267711767066)) ;
#70318 = CARTESIAN_POINT('Ctrl Pts',(-19.1854080916355,43.7583087045299,121.921017634688)) ;
#70319 = CARTESIAN_POINT('Ctrl Pts',(-19.2301849629632,43.578319624167,122.219177394001)) ;
#70320 = CARTESIAN_POINT('Ctrl Pts',(-19.4492993318414,43.7683706839503,121.904850471576)) ;
#70321 = CARTESIAN_POINT('Ctrl Pts',(-19.4412982796223,43.5883816035874,122.2062446672)) ;
#70322 = CARTESIAN_POINT('Ctrl Pts',(-19.7063573702631,43.7782152171792,121.934076663056)) ;
#70323 = CARTESIAN_POINT('Ctrl Pts',(-19.6469435446541,43.5982261368164,122.22962650948)) ;
#70324 = CARTESIAN_POINT('Ctrl Pts',(-19.9576002327423,43.7881752960855,122.007446102476)) ;
#70325 = CARTESIAN_POINT('Ctrl Pts',(-19.8479372613017,43.6081862157226,122.288322719679)) ;
#70326 = CARTESIAN_POINT('Ctrl Pts',(-20.1938925036668,43.7982135726581,122.124695495129)) ;
#70327 = CARTESIAN_POINT('Ctrl Pts',(-20.0369707873508,43.6182244922952,122.382123111982)) ;
#70328 = CARTESIAN_POINT('Ctrl Pts',(-20.403085266942,43.8080869591959,122.278251260109)) ;
#70329 = CARTESIAN_POINT('Ctrl Pts',(-20.2043238013652,43.6280978788331,122.504967832787)) ;
#70330 = CARTESIAN_POINT('Ctrl Pts',(-20.5859442921562,43.818159901963,122.469575837394)) ;
#70331 = CARTESIAN_POINT('Ctrl Pts',(-20.3506106669078,43.6381708216001,122.65802830527)) ;
#70332 = CARTESIAN_POINT('Ctrl Pts',(-20.7294563688574,43.8279813160913,122.684155238316)) ;
#70333 = CARTESIAN_POINT('Ctrl Pts',(-20.4654190257997,43.6479922357285,122.829691205274)) ;
#70334 = CARTESIAN_POINT('Ctrl Pts',(-20.8364643232835,43.8380559461636,122.926263897482)) ;
#70335 = CARTESIAN_POINT('Ctrl Pts',(-20.5510249269012,43.6580668658008,123.023378728422)) ;
#70336 = CARTESIAN_POINT('Ctrl Pts',(-20.8984148212984,43.8479225834805,123.178073112069)) ;
#70337 = CARTESIAN_POINT('Ctrl Pts',(-20.6005844237704,43.6679335031176,123.224825316576)) ;
#70338 = CARTESIAN_POINT('Ctrl Pts',(-20.9166483132866,43.8579461288523,123.440837266538)) ;
#70339 = CARTESIAN_POINT('Ctrl Pts',(-20.6151706983292,43.6779570484894,123.435036712492)) ;
#70340 = CARTESIAN_POINT('Ctrl Pts',(-20.8883395523817,43.8679718803695,123.702794177763)) ;
#70341 = CARTESIAN_POINT('Ctrl Pts',(-20.5925230028488,43.6879828000066,123.644602236926)) ;
#70342 = CARTESIAN_POINT('Ctrl Pts',(-20.8166599479504,43.8778254673789,123.951603594725)) ;
#70343 = CARTESIAN_POINT('Ctrl Pts',(-20.5351790633335,43.697836387016,123.843648589782)) ;
#70344 = CARTESIAN_POINT('Ctrl Pts',(-20.702060923653,43.8878024276068,124.187422142841)) ;
#70345 = CARTESIAN_POINT('Ctrl Pts',(-20.4434995981191,43.7078133472439,124.032303014082)) ;
#70346 = CARTESIAN_POINT('Ctrl Pts',(-20.5472263847729,43.8978235706353,124.400424003541)) ;
#70347 = CARTESIAN_POINT('Ctrl Pts',(-20.3196315437923,43.7178344902724,124.202704210316)) ;
#70348 = CARTESIAN_POINT('Ctrl Pts',(-20.3607073265626,43.9077061766552,124.581187205771)) ;
#70349 = CARTESIAN_POINT('Ctrl Pts',(-20.1704166645511,43.7277170962923,124.34731388807)) ;
#70350 = CARTESIAN_POINT('Ctrl Pts',(-20.141598516524,43.9177746472879,124.729426223139)) ;
#70351 = CARTESIAN_POINT('Ctrl Pts',(-19.9951291156329,43.737785566925,124.465904948293)) ;
#70352 = CARTESIAN_POINT('Ctrl Pts',(-19.9058383854937,43.9276047304716,124.835123522503)) ;
#70353 = CARTESIAN_POINT('Ctrl Pts',(-19.8065220003896,43.7476156501087,124.550461981873)) ;
#70354 = CARTESIAN_POINT('Ctrl Pts',(-19.6494502413749,43.937671290152,124.900110672069)) ;
#70355 = CARTESIAN_POINT('Ctrl Pts',(-19.6014111164167,43.7576822097891,124.602451541965)) ;
#70356 = CARTESIAN_POINT('Ctrl Pts',(-19.3902067493444,43.9475615399812,124.919096378298)) ;
#70357 = CARTESIAN_POINT('Ctrl Pts',(-19.3940171383949,43.7675724596183,124.617639759188)) ;
#70358 = CARTESIAN_POINT('Ctrl Pts',(-19.1289291993489,43.95755370573,124.893086593962)) ;
#70359 = CARTESIAN_POINT('Ctrl Pts',(-19.1849952828708,43.7775646253671,124.59683180778)) ;
#70360 = CARTESIAN_POINT('Ctrl Pts',(-18.8769378575391,43.9675165493261,124.822071866951)) ;
#70361 = CARTESIAN_POINT('Ctrl Pts',(-18.9834026165215,43.7875274689632,124.54001992677)) ;
#70362 = CARTESIAN_POINT('Ctrl Pts',(-18.6421796236828,43.9774207181539,124.709636238937)) ;
#70363 = CARTESIAN_POINT('Ctrl Pts',(-18.7955967231379,43.797431637791,124.450071716623)) ;
#70364 = CARTESIAN_POINT('Ctrl Pts',(-18.4273472596352,43.9874815930482,124.555590382771)) ;
#70365 = CARTESIAN_POINT('Ctrl Pts',(-18.6237306573745,43.8074925126853,124.32683478731)) ;
#70366 = CARTESIAN_POINT('Ctrl Pts',(-18.2462912417937,43.9973204963776,124.370950929424)) ;
#70367 = CARTESIAN_POINT('Ctrl Pts',(-18.4788866747654,43.8173314160147,124.179124065439)) ;
#70368 = CARTESIAN_POINT('Ctrl Pts',(-18.096473040413,44.0073888727515,124.152920066805)) ;
#70369 = CARTESIAN_POINT('Ctrl Pts',(-18.3590318811178,43.8273997923886,124.004699145389)) ;
#70370 = CARTESIAN_POINT('Ctrl Pts',(-17.9888795242822,44.0172694893841,123.916566377132)) ;
#70371 = CARTESIAN_POINT('Ctrl Pts',(-18.2729574087279,43.8372804090212,123.815617033052)) ;
#70372 = CARTESIAN_POINT('Ctrl Pts',(-17.9227396809683,44.0272606496131,123.662515814642)) ;
#70373 = CARTESIAN_POINT('Ctrl Pts',(-18.2200454142358,43.8472715692502,123.612376795175)) ;
#70374 = CARTESIAN_POINT('Ctrl Pts',(-17.9017478866056,44.0372137230452,123.40176367561)) ;
#70375 = CARTESIAN_POINT('Ctrl Pts',(-18.2032518302433,43.8572246426823,123.403775507638)) ;
#70376 = CARTESIAN_POINT('Ctrl Pts',(-17.9266347799871,44.0472495586578,123.139231148737)) ;
#70377 = CARTESIAN_POINT('Ctrl Pts',(-18.2231612008556,43.867260478295,123.193749351306)) ;
#70378 = CARTESIAN_POINT('Ctrl Pts',(-17.9955495886584,44.057139685388,122.888614558069)) ;
#70379 = CARTESIAN_POINT('Ctrl Pts',(-18.2782926266805,43.8771506050251,122.993256851643)) ;
#70380 = CARTESIAN_POINT('Ctrl Pts',(-18.1076878440328,44.0671318671573,122.651194666647)) ;
#70381 = CARTESIAN_POINT('Ctrl Pts',(-18.3680028793089,43.8871427867944,122.803320956342)) ;
#70382 = CARTESIAN_POINT('Ctrl Pts',(-18.2587247866769,44.0770778071318,122.437883820146)) ;
#70383 = CARTESIAN_POINT('Ctrl Pts',(-18.4888319257956,43.8970887267689,122.632672501952)) ;
#70384 = CARTESIAN_POINT('Ctrl Pts',(-18.4441648499972,44.0870249908912,122.253628827194)) ;
#70385 = CARTESIAN_POINT('Ctrl Pts',(-18.6371833541905,43.9070359105284,122.485268533601)) ;
#70386 = CARTESIAN_POINT('Ctrl Pts',(-18.6611045195494,44.0970729291816,122.103115117568)) ;
#70387 = CARTESIAN_POINT('Ctrl Pts',(-18.8107350578741,43.9170838488187,122.364857168353)) ;
#70388 = CARTESIAN_POINT('Ctrl Pts',(-18.8960216519544,44.1069205639951,121.9945561486)) ;
#70389 = CARTESIAN_POINT('Ctrl Pts',(-18.9986675796601,43.9269314836323,122.278010099489)) ;
#70390 = CARTESIAN_POINT('Ctrl Pts',(-19.1488932353645,44.1168822776931,121.926880369107)) ;
#70391 = CARTESIAN_POINT('Ctrl Pts',(-19.200964338225,43.9368931973302,122.223868984643)) ;
#70392 = CARTESIAN_POINT('Ctrl Pts',(-19.4114837782062,44.1269109135143,121.904316948058)) ;
#70393 = CARTESIAN_POINT('Ctrl Pts',(-19.4110368048726,43.9469218331514,122.205817721799)) ;
#70394 = CARTESIAN_POINT('Ctrl Pts',(-19.6708855677709,44.136821228266,121.927328148373)) ;
#70395 = CARTESIAN_POINT('Ctrl Pts',(-19.6185575864657,43.9568321479032,122.224226080018)) ;
#70396 = CARTESIAN_POINT('Ctrl Pts',(-19.923172854028,44.1467560989287,121.994541369525)) ;
#70397 = CARTESIAN_POINT('Ctrl Pts',(-19.8203870878445,43.9667670185658,122.277995832626)) ;
#70398 = CARTESIAN_POINT('Ctrl Pts',(-20.1623656622643,44.1567972813305,122.105936279633)) ;
#70399 = CARTESIAN_POINT('Ctrl Pts',(-20.011741745876,43.9768082009676,122.367111237361)) ;
#70400 = CARTESIAN_POINT('Ctrl Pts',(-20.3754115587803,44.1666842527952,122.254696080828)) ;
#70401 = CARTESIAN_POINT('Ctrl Pts',(-20.1821781748641,43.9866951724323,122.486118021261)) ;
#70402 = CARTESIAN_POINT('Ctrl Pts',(-20.5616797006254,44.1766836850578,122.439998156239)) ;
#70403 = CARTESIAN_POINT('Ctrl Pts',(-20.3311931547893,43.9966946046949,122.634359041277)) ;
#70404 = CARTESIAN_POINT('Ctrl Pts',(-20.7119248209942,44.1866037503144,122.653074790023)) ;
#70405 = CARTESIAN_POINT('Ctrl Pts',(-20.4513895765128,44.0066146699516,122.804819385592)) ;
#70406 = CARTESIAN_POINT('Ctrl Pts',(-20.8242248480084,44.1966406028986,122.89171516179)) ;
#70407 = CARTESIAN_POINT('Ctrl Pts',(-20.5412304078257,44.0166515225357,122.995731440884)) ;
#70408 = CARTESIAN_POINT('Ctrl Pts',(-20.8925256088344,44.2065532622386,123.143101297578)) ;
#70409 = CARTESIAN_POINT('Ctrl Pts',(-20.5958716458054,44.0265641818757,123.19683949956)) ;
#70410 = CARTESIAN_POINT('Ctrl Pts',(-20.9168966357386,44.2165444741535,123.404542148438)) ;
#70411 = CARTESIAN_POINT('Ctrl Pts',(-20.6153694127085,44.0365553937906,123.405991922717)) ;
#70412 = CARTESIAN_POINT('Ctrl Pts',(-20.8948063197256,44.2265861155566,123.667478543077)) ;
#70413 = CARTESIAN_POINT('Ctrl Pts',(-20.597697972569,44.0465970351937,123.616341249776)) ;
#70414 = CARTESIAN_POINT('Ctrl Pts',(-20.8294398407361,44.2364149097636,123.917397995982)) ;
#70415 = CARTESIAN_POINT('Ctrl Pts',(-20.5454060288172,44.0564258294008,123.816275945776)) ;
#70416 = CARTESIAN_POINT('Ctrl Pts',(-20.7190966284838,44.2464913208849,124.158051348321)) ;
#70417 = CARTESIAN_POINT('Ctrl Pts',(-20.45713223089,44.066502240522,124.008799361129)) ;
#70418 = CARTESIAN_POINT('Ctrl Pts',(-20.5720419186679,44.2563434539274,124.371206621261)) ;
#70419 = CARTESIAN_POINT('Ctrl Pts',(-20.3394898756421,44.0763543735645,124.179323355511)) ;
#70420 = CARTESIAN_POINT('Ctrl Pts',(-20.3863598082827,44.2664166882687,124.559814357932)) ;
#70421 = CARTESIAN_POINT('Ctrl Pts',(-20.1909447374728,44.0864276079058,124.330210536534)) ;
#70422 = CARTESIAN_POINT('Ctrl Pts',(-20.1756188492781,44.2762581895953,124.709761183194)) ;
#70423 = CARTESIAN_POINT('Ctrl Pts',(-20.0223534395185,44.0962691092324,124.450168264063)) ;
#70424 = CARTESIAN_POINT('Ctrl Pts',(-19.9396571120249,44.2862191411901,124.823064731638)) ;
#70425 = CARTESIAN_POINT('Ctrl Pts',(-19.833584900295,44.1062300608272,124.540812125368)) ;
#70426 = CARTESIAN_POINT('Ctrl Pts',(-19.6855192485354,44.2962569589108,124.893713217866)) ;
#70427 = CARTESIAN_POINT('Ctrl Pts',(-19.630274821082,44.1162678785479,124.597332072431)) ;
#70428 = CARTESIAN_POINT('Ctrl Pts',(-19.4272568805915,44.3061313081678,124.919231077549)) ;
#70429 = CARTESIAN_POINT('Ctrl Pts',(-19.4236658581151,44.1261422278049,124.617747552398)) ;
#70430 = CARTESIAN_POINT('Ctrl Pts',(-19.1634421663118,44.31620085891,124.899117334135)) ;
#70431 = CARTESIAN_POINT('Ctrl Pts',(-19.2126137105638,44.1362117785471,124.601657806731)) ;
#70432 = CARTESIAN_POINT('Ctrl Pts',(-18.9130262792897,44.3260348784186,124.835165719918)) ;
#70433 = CARTESIAN_POINT('Ctrl Pts',(-19.0122816736547,44.1460457980557,124.55049803559)) ;
#70434 = CARTESIAN_POINT('Ctrl Pts',(-18.6724761256092,44.3360690329981,124.727189304434)) ;
#70435 = CARTESIAN_POINT('Ctrl Pts',(-18.8198408751358,44.1560799526353,124.464118191425)) ;
#70436 = CARTESIAN_POINT('Ctrl Pts',(-18.4550666358706,44.3460849588206,124.578799029693)) ;
#70437 = CARTESIAN_POINT('Ctrl Pts',(-18.6459125515534,44.1660958784577,124.345407061156)) ;
#70438 = CARTESIAN_POINT('Ctrl Pts',(-18.2689206934433,44.3559672140149,124.397708730824)) ;
#70439 = CARTESIAN_POINT('Ctrl Pts',(-18.4969953334488,44.175978133652,124.200536340073)) ;
#70440 = CARTESIAN_POINT('Ctrl Pts',(-18.1151639542311,44.3659560205258,124.184994122571)) ;
#70441 = CARTESIAN_POINT('Ctrl Pts',(-18.3739888404937,44.1859669401629,124.030365648299)) ;
#70442 = CARTESIAN_POINT('Ctrl Pts',(-18.0009287364672,44.3759045877885,123.949788452977)) ;
#70443 = CARTESIAN_POINT('Ctrl Pts',(-18.2825994652639,44.1959155074256,123.842202101952)) ;
#70444 = CARTESIAN_POINT('Ctrl Pts',(-17.9287930124207,44.3859593930905,123.695625807384)) ;
#70445 = CARTESIAN_POINT('Ctrl Pts',(-18.2248894332105,44.2059703127276,123.638872216548)) ;
#70446 = CARTESIAN_POINT('Ctrl Pts',(-17.9021400804517,44.3957781763541,123.438965134921)) ;
#70447 = CARTESIAN_POINT('Ctrl Pts',(-18.2035656682634,44.2157890959912,123.433544841874)) ;
#70448 = CARTESIAN_POINT('Ctrl Pts',(-17.9201546965115,44.4058139487147,123.175857889878)) ;
#70449 = CARTESIAN_POINT('Ctrl Pts',(-18.2179757049312,44.2258248683518,123.223058844661)) ;
#70450 = CARTESIAN_POINT('Ctrl Pts',(-17.9842443392215,44.4158386477433,122.920324456169)) ;
#70451 = CARTESIAN_POINT('Ctrl Pts',(-18.2692459457446,44.2358495673804,123.018631708746)) ;
#70452 = CARTESIAN_POINT('Ctrl Pts',(-18.0893534627256,44.4256906510024,122.683715321304)) ;
#70453 = CARTESIAN_POINT('Ctrl Pts',(-18.3533314265156,44.2457015706395,122.8293444755)) ;
#70454 = CARTESIAN_POINT('Ctrl Pts',(-18.2356357013134,44.4356815853996,122.46572907487)) ;
#70455 = CARTESIAN_POINT('Ctrl Pts',(-18.4703557257671,44.2556925050367,122.654954642238)) ;
#70456 = CARTESIAN_POINT('Ctrl Pts',(-18.41613673709,44.4455995078307,122.277671975149)) ;
#70457 = CARTESIAN_POINT('Ctrl Pts',(-18.6147549895924,44.2656104274678,122.504508093951)) ;
#70458 = CARTESIAN_POINT('Ctrl Pts',(-18.6288136047377,44.455627863513,122.122084840499)) ;
#70459 = CARTESIAN_POINT('Ctrl Pts',(-18.7848954782,44.2756387831502,122.380036963716)) ;
#70460 = CARTESIAN_POINT('Ctrl Pts',(-18.8618504936233,44.4655121480236,122.007331995514)) ;
#70461 = CARTESIAN_POINT('Ctrl Pts',(-18.9713236802826,44.2855230676607,122.288233368328)) ;
#70462 = CARTESIAN_POINT('Ctrl Pts',(-19.1138322342733,44.4755048319315,121.933421901147)) ;
#70463 = CARTESIAN_POINT('Ctrl Pts',(-19.1729084429983,44.2955157515686,122.229103542104)) ;
#70464 = CARTESIAN_POINT('Ctrl Pts',(-19.3758137501504,44.4855335689392,121.904740742867)) ;
#70465 = CARTESIAN_POINT('Ctrl Pts',(-19.3824934791347,44.3055444885763,122.206156839405)) ;
#70466 = CARTESIAN_POINT('Ctrl Pts',(-19.6350667634332,44.4954189655681,121.921395206069)) ;
#70467 = CARTESIAN_POINT('Ctrl Pts',(-19.5898954555801,44.3154298852052,122.219478539478)) ;
#70468 = CARTESIAN_POINT('Ctrl Pts',(-19.8901602887943,44.505406850982,121.983076127047)) ;
#70469 = CARTESIAN_POINT('Ctrl Pts',(-19.7939705951904,44.3254177706191,122.268821404401)) ;
#70470 = CARTESIAN_POINT('Ctrl Pts',(-20.1298803582596,44.5153575536426,122.087637628189)) ;
#70471 = CARTESIAN_POINT('Ctrl Pts',(-19.9857471730679,44.3353684732797,122.35246874884)) ;
#70472 = CARTESIAN_POINT('Ctrl Pts',(-20.3496330623717,44.52539787174,122.233619868658)) ;
#70473 = CARTESIAN_POINT('Ctrl Pts',(-20.1615504313535,44.3454087913771,122.469252999656)) ;
#70474 = CARTESIAN_POINT('Ctrl Pts',(-20.5377640234238,44.5352724370732,122.412390214829)) ;
#70475 = CARTESIAN_POINT('Ctrl Pts',(-20.3120561285973,44.3552833567104,122.612267503124)) ;
#70476 = CARTESIAN_POINT('Ctrl Pts',(-20.6941762400211,44.5452720971343,122.62349750357)) ;
#70477 = CARTESIAN_POINT('Ctrl Pts',(-20.4371874373751,44.3652830167714,122.781152089198)) ;
#70478 = CARTESIAN_POINT('Ctrl Pts',(-20.8107568463258,44.555181092302,122.856392682696)) ;
#70479 = CARTESIAN_POINT('Ctrl Pts',(-20.5304535425006,44.3751920119392,122.967466996356)) ;
#70480 = CARTESIAN_POINT('Ctrl Pts',(-20.8861166779856,44.5652358334653,123.109601455861)) ;
#70481 = CARTESIAN_POINT('Ctrl Pts',(-20.5907433453259,44.3852467531024,123.170033530578)) ;
#70482 = CARTESIAN_POINT('Ctrl Pts',(-20.9160838152059,44.5750944453791,123.36698258296)) ;
#70483 = CARTESIAN_POINT('Ctrl Pts',(-20.6147190097219,44.3951053650162,123.375937681712)) ;
#70484 = CARTESIAN_POINT('Ctrl Pts',(-20.9007482951995,44.5851625676584,123.631078613714)) ;
#70485 = CARTESIAN_POINT('Ctrl Pts',(-20.6024526333435,44.4051734872955,123.587214747284)) ;
#70486 = CARTESIAN_POINT('Ctrl Pts',(-20.8410433869187,44.5950180383616,123.883116987979)) ;
#70487 = CARTESIAN_POINT('Ctrl Pts',(-20.5546908119095,44.4150289579987,123.788845432467)) ;
#70488 = CARTESIAN_POINT('Ctrl Pts',(-20.737768269546,44.605012897855,124.124606144448)) ;
#70489 = CARTESIAN_POINT('Ctrl Pts',(-20.4720727081621,44.4250238174921,123.982037522316)) ;
#70490 = CARTESIAN_POINT('Ctrl Pts',(-20.5931261612872,44.6150441511969,124.344997164701)) ;
#70491 = CARTESIAN_POINT('Ctrl Pts',(-20.3563607533755,44.435055070834,124.158351473366)) ;
#70492 = CARTESIAN_POINT('Ctrl Pts',(-20.4156755541826,44.62491085007,124.534060702266)) ;
#70493 = CARTESIAN_POINT('Ctrl Pts',(-20.2144020898501,44.4449217697071,124.309603448869)) ;
#70494 = CARTESIAN_POINT('Ctrl Pts',(-20.2058546846897,44.6348976658212,124.691655677439)) ;
#70495 = CARTESIAN_POINT('Ctrl Pts',(-20.0465467658949,44.4549085854583,124.435681091647)) ;
#70496 = CARTESIAN_POINT('Ctrl Pts',(-19.9727822075021,44.6448448710167,124.810089850081)) ;
#70497 = CARTESIAN_POINT('Ctrl Pts',(-19.8600899289393,44.4648557906538,124.530430271056)) ;
#70498 = CARTESIAN_POINT('Ctrl Pts',(-19.7202958616412,44.6548878591429,124.886862052342)) ;
#70499 = CARTESIAN_POINT('Ctrl Pts',(-19.6581014661053,44.4748987787801,124.591850096019)) ;
#70500 = CARTESIAN_POINT('Ctrl Pts',(-19.4628869098935,44.6647552137644,124.91822843966)) ;
#70501 = CARTESIAN_POINT('Ctrl Pts',(-19.4521748954927,44.4847661334015,124.616945312954)) ;
#70502 = CARTESIAN_POINT('Ctrl Pts',(-19.201339436511,44.6747211070625,124.904992081208)) ;
#70503 = CARTESIAN_POINT('Ctrl Pts',(-19.242936917876,44.4947320266996,124.606358443205)) ;
#70504 = CARTESIAN_POINT('Ctrl Pts',(-18.9446146117008,44.6847448844386,124.845931776589)) ;
#70505 = CARTESIAN_POINT('Ctrl Pts',(-19.0375565977731,44.5047558040757,124.559112343262)) ;
#70506 = CARTESIAN_POINT('Ctrl Pts',(-18.7044247703961,44.6946704323703,124.744265398415)) ;
#70507 = CARTESIAN_POINT('Ctrl Pts',(-18.8454040419128,44.5146813520074,124.477781340274)) ;
#70508 = CARTESIAN_POINT('Ctrl Pts',(-18.4848477732278,44.7046109087913,124.602728279973)) ;
#70509 = CARTESIAN_POINT('Ctrl Pts',(-18.6697413477393,44.5246218284284,124.364553593259)) ;
#70510 = CARTESIAN_POINT('Ctrl Pts',(-18.2913709521149,44.7146571184542,124.423127645142)) ;
#70511 = CARTESIAN_POINT('Ctrl Pts',(-18.5149583948213,44.5346680380913,124.220874721725)) ;
#70512 = CARTESIAN_POINT('Ctrl Pts',(-18.1347068986328,44.724518375116,124.216672914137)) ;
#70513 = CARTESIAN_POINT('Ctrl Pts',(-18.3896255050784,44.5445292947531,124.055712452699)) ;
#70514 = CARTESIAN_POINT('Ctrl Pts',(-18.0143070451238,44.7345120033913,123.983318570089)) ;
#70515 = CARTESIAN_POINT('Ctrl Pts',(-18.2933036525415,44.5545229230284,123.869030062897)) ;
#70516 = CARTESIAN_POINT('Ctrl Pts',(-17.936633762989,44.7444374007015,123.734282199344)) ;
#70517 = CARTESIAN_POINT('Ctrl Pts',(-18.2311629143838,44.5644483203386,123.669801734943)) ;
#70518 = CARTESIAN_POINT('Ctrl Pts',(-17.9030399617659,44.7544653086117,123.472943722699)) ;
#70519 = CARTESIAN_POINT('Ctrl Pts',(-18.2042856479589,44.5744762282489,123.46073129079)) ;
#70520 = CARTESIAN_POINT('Ctrl Pts',(-17.9148956263581,44.7643516242809,123.213374011942)) ;
#70521 = CARTESIAN_POINT('Ctrl Pts',(-18.2137679274287,44.584362543918,123.253075513145)) ;
#70522 = CARTESIAN_POINT('Ctrl Pts',(-17.9723197114155,44.7743832191847,122.95612772885)) ;
#70523 = CARTESIAN_POINT('Ctrl Pts',(-18.2597049813133,44.5943941388218,123.047278048275)) ;
#70524 = CARTESIAN_POINT('Ctrl Pts',(-18.0718425713874,44.7842654621364,122.716214046185)) ;
#70525 = CARTESIAN_POINT('Ctrl Pts',(-18.3393211701474,44.6042763817735,122.855346286345)) ;
#70526 = CARTESIAN_POINT('Ctrl Pts',(-18.2138824565932,44.7943249331663,122.493298818431)) ;
#70527 = CARTESIAN_POINT('Ctrl Pts',(-18.452951139445,44.6143358528034,122.677012948951)) ;
#70528 = CARTESIAN_POINT('Ctrl Pts',(-18.3890982744024,44.8041913778294,122.302163339125)) ;
#70529 = CARTESIAN_POINT('Ctrl Pts',(-18.5931221262605,44.6242022974665,122.524103052415)) ;
#70530 = CARTESIAN_POINT('Ctrl Pts',(-18.5963979569655,44.8141575022781,122.142117824611)) ;
#70531 = CARTESIAN_POINT('Ctrl Pts',(-18.7589604790486,44.6341684219152,122.396064874445)) ;
#70532 = CARTESIAN_POINT('Ctrl Pts',(-18.8300300927451,44.8241877456692,122.020087986119)) ;
#70533 = CARTESIAN_POINT('Ctrl Pts',(-18.9458651244295,44.6441986653064,122.298439056251)) ;
#70534 = CARTESIAN_POINT('Ctrl Pts',(-19.0777784031114,44.8340807806223,121.941205272921)) ;
#70535 = CARTESIAN_POINT('Ctrl Pts',(-19.1440629425059,44.6540917002594,122.235330716498)) ;
#70536 = CARTESIAN_POINT('Ctrl Pts',(-19.3395157430304,44.8441316948591,121.905920090679)) ;
#70537 = CARTESIAN_POINT('Ctrl Pts',(-19.3534531408236,44.6641426144963,122.207100459181)) ;
#70538 = CARTESIAN_POINT('Ctrl Pts',(-19.5992088007417,44.8540215210837,121.916417743617)) ;
#70539 = CARTESIAN_POINT('Ctrl Pts',(-19.561205041554,44.6740324407208,122.215496012711)) ;
#70540 = CARTESIAN_POINT('Ctrl Pts',(-19.9417558495349,44.8673563361306,121.990481112151)) ;
#70541 = CARTESIAN_POINT('Ctrl Pts',(-19.8352567550235,44.6873672557678,122.274745507017)) ;
#70542 = CARTESIAN_POINT('Ctrl Pts',(-20.2554040575952,44.8806334273021,122.152088557895)) ;
#70543 = CARTESIAN_POINT('Ctrl Pts',(-20.0861971038527,44.7006443469392,122.404050615546)) ;
#70544 = CARTESIAN_POINT('Ctrl Pts',(-20.5136611155883,44.8938817159004,122.385626670228)) ;
#70545 = CARTESIAN_POINT('Ctrl Pts',(-20.2927670421858,44.7138926355375,122.590851388565)) ;
#70546 = CARTESIAN_POINT('Ctrl Pts',(-20.6757307463464,44.9039365573945,122.59426491759)) ;
#70547 = CARTESIAN_POINT('Ctrl Pts',(-20.4224319383683,44.7239474770316,122.757766151545)) ;
#70548 = CARTESIAN_POINT('Ctrl Pts',(-20.7967932245961,44.913767546702,122.822543238522)) ;
#70549 = CARTESIAN_POINT('Ctrl Pts',(-20.5192820748052,44.7337784663392,122.940386237297)) ;
#70550 = CARTESIAN_POINT('Ctrl Pts',(-20.8785256178797,44.9238441110252,123.074368365477)) ;
#70551 = CARTESIAN_POINT('Ctrl Pts',(-20.5846700573935,44.7438550306624,123.141847246608)) ;
#70552 = CARTESIAN_POINT('Ctrl Pts',(-20.9144646604309,44.9336934361592,123.330718388823)) ;
#70553 = CARTESIAN_POINT('Ctrl Pts',(-20.6134249986564,44.7537043557963,123.346922032747)) ;
#70554 = CARTESIAN_POINT('Ctrl Pts',(-20.9029627808752,44.9470414357965,123.681317025944)) ;
#70555 = CARTESIAN_POINT('Ctrl Pts',(-20.60421795921,44.7670523554336,123.627426785072)) ;
#70556 = CARTESIAN_POINT('Ctrl Pts',(-20.7745082951822,44.963626195333,124.10295325502)) ;
#70557 = CARTESIAN_POINT('Ctrl Pts',(-20.5014772079403,44.7836371149701,123.964697051323)) ;
#70558 = CARTESIAN_POINT('Ctrl Pts',(-20.5110259009966,44.9801947466811,124.455768261803)) ;
#70559 = CARTESIAN_POINT('Ctrl Pts',(-20.2906509869384,44.8002056663183,124.247002496847)) ;
#70560 = CARTESIAN_POINT('Ctrl Pts',(-20.2351348038895,44.9935545715001,124.672943272086)) ;
#70561 = CARTESIAN_POINT('Ctrl Pts',(-20.0699761236227,44.8135654911373,124.420705379304)) ;
#70562 = CARTESIAN_POINT('Ctrl Pts',(-20.0058393288218,45.0034599803308,124.796167835363)) ;
#70563 = CARTESIAN_POINT('Ctrl Pts',(-19.8865323249825,44.8234708999679,124.519294746871)) ;
#70564 = CARTESIAN_POINT('Ctrl Pts',(-19.757418400852,45.0134200069148,124.878510971796)) ;
#70565 = CARTESIAN_POINT('Ctrl Pts',(-19.6878011258136,44.833430926552,124.585169321105)) ;
#70566 = CARTESIAN_POINT('Ctrl Pts',(-19.4127381950797,45.0266775911001,124.929494089017)) ;
#70567 = CARTESIAN_POINT('Ctrl Pts',(-19.4120406279165,44.8466885107373,124.62595768779)) ;
#70568 = CARTESIAN_POINT('Ctrl Pts',(-18.9730728854828,45.0433288025948,124.878933487773)) ;
#70569 = CARTESIAN_POINT('Ctrl Pts',(-19.0603260702002,44.8633397222319,124.585513496632)) ;
#70570 = CARTESIAN_POINT('Ctrl Pts',(-18.4995381186548,45.0632470167051,124.642306903848)) ;
#70571 = CARTESIAN_POINT('Ctrl Pts',(-18.6814904260909,44.8832579363422,124.396215029442)) ;
#70572 = CARTESIAN_POINT('Ctrl Pts',(-18.1350210819867,45.0831247799259,124.259778759138)) ;
#70573 = CARTESIAN_POINT('Ctrl Pts',(-18.3898754178223,44.9031356995631,124.090194473814)) ;
#70574 = CARTESIAN_POINT('Ctrl Pts',(-17.9219902774577,45.1031374477131,123.772503946077)) ;
#70575 = CARTESIAN_POINT('Ctrl Pts',(-18.219447255777,44.9231483673502,123.700376068826)) ;
#70576 = CARTESIAN_POINT('Ctrl Pts',(-17.8878614143457,45.1229499703797,123.246927329174)) ;
#70577 = CARTESIAN_POINT('Ctrl Pts',(-18.1921410117766,44.9429608900168,123.279913768998)) ;
#70578 = CARTESIAN_POINT('Ctrl Pts',(-18.0355408684965,45.1429332703796,122.736855760796)) ;
#70579 = CARTESIAN_POINT('Ctrl Pts',(-18.3102818169754,44.9629441900167,122.8718555916)) ;
#70580 = CARTESIAN_POINT('Ctrl Pts',(-18.3474404946756,45.1628275474809,122.309788228837)) ;
#70581 = CARTESIAN_POINT('Ctrl Pts',(-18.5597996758674,44.982838467118,122.530199273158)) ;
#70582 = CARTESIAN_POINT('Ctrl Pts',(-18.786662149823,45.1827603092387,122.0135853007)) ;
#70583 = CARTESIAN_POINT('Ctrl Pts',(-18.9111760676998,45.0027712288758,122.293234567284)) ;
#70584 = CARTESIAN_POINT('Ctrl Pts',(-19.3015601046736,45.2027263150034,121.885187082688)) ;
#70585 = CARTESIAN_POINT('Ctrl Pts',(-19.3230941010408,45.0227372346405,122.190513534484)) ;
#70586 = CARTESIAN_POINT('Ctrl Pts',(-19.8271247057948,45.2226048471683,121.939586650986)) ;
#70587 = CARTESIAN_POINT('Ctrl Pts',(-19.7435470906285,45.0426157668054,122.234031125667)) ;
#70588 = CARTESIAN_POINT('Ctrl Pts',(-20.3041812489775,45.2425445138286,122.170281678288)) ;
#70589 = CARTESIAN_POINT('Ctrl Pts',(-20.125193674908,45.0625554334657,122.418585724291)) ;
#70590 = CARTESIAN_POINT('Ctrl Pts',(-20.673234757221,45.262439388474,122.549040856896)) ;
#70591 = CARTESIAN_POINT('Ctrl Pts',(-20.4204384003569,45.0824503081111,122.721592696201)) ;
#70592 = CARTESIAN_POINT('Ctrl Pts',(-20.8914226002841,45.2823465277673,123.03092366853)) ;
#70593 = CARTESIAN_POINT('Ctrl Pts',(-20.5949902713448,45.1023574474044,123.107099401626)) ;
#70594 = CARTESIAN_POINT('Ctrl Pts',(-20.933006994823,45.3022570758458,123.558648564266)) ;
#70595 = CARTESIAN_POINT('Ctrl Pts',(-20.6282585345272,45.1222679954829,123.529280226432)) ;
#70596 = CARTESIAN_POINT('Ctrl Pts',(-20.7897928711044,45.322325661203,124.072332126759)) ;
#70597 = CARTESIAN_POINT('Ctrl Pts',(-20.513688465567,45.1423365808401,123.940226547894)) ;
#70598 = CARTESIAN_POINT('Ctrl Pts',(-20.4845776581537,45.3421074585177,124.500648372566)) ;
#70599 = CARTESIAN_POINT('Ctrl Pts',(-20.269515271003,45.1621183781549,124.282882031287)) ;
#70600 = CARTESIAN_POINT('Ctrl Pts',(-20.0473359397164,45.3621150054623,124.802932073758)) ;
#70601 = CARTESIAN_POINT('Ctrl Pts',(-19.9197218860292,45.1821259250994,124.524709061024)) ;
#70602 = CARTESIAN_POINT('Ctrl Pts',(-19.5376317009415,45.3819367437651,124.936721152217)) ;
#70603 = CARTESIAN_POINT('Ctrl Pts',(-19.5119562871531,45.2019476634022,124.631740691942)) ;
#70604 = CARTESIAN_POINT('Ctrl Pts',(-19.0088087615849,45.4019167636693,124.889143040385)) ;
#70605 = CARTESIAN_POINT('Ctrl Pts',(-19.0888977818351,45.2219276833064,124.593677332525)) ;
#70606 = CARTESIAN_POINT('Ctrl Pts',(-18.5296775435496,45.4218342149315,124.664000015216)) ;
#70607 = CARTESIAN_POINT('Ctrl Pts',(-18.7055922193586,45.2418451345686,124.413561830565)) ;
#70608 = CARTESIAN_POINT('Ctrl Pts',(-18.1560490205525,45.4417091361042,124.2905332235)) ;
#70609 = CARTESIAN_POINT('Ctrl Pts',(-18.4066894730446,45.2617200557413,124.114786420847)) ;
#70610 = CARTESIAN_POINT('Ctrl Pts',(-17.9309504550834,45.461733504655,123.80830220994)) ;
#70611 = CARTESIAN_POINT('Ctrl Pts',(-18.2266120673935,45.2817444242922,123.729001254374)) ;
#70612 = CARTESIAN_POINT('Ctrl Pts',(-17.8844372685422,45.4816001890285,123.282245957211)) ;
#70613 = CARTESIAN_POINT('Ctrl Pts',(-18.1894029640175,45.3016111086656,123.308154786778)) ;
#70614 = CARTESIAN_POINT('Ctrl Pts',(-18.0199005695342,45.5015440108747,122.769835234287)) ;
#70615 = CARTESIAN_POINT('Ctrl Pts',(-18.2977757249971,45.3215549305118,122.898226217715)) ;
#70616 = CARTESIAN_POINT('Ctrl Pts',(-18.3217175474885,45.5214513801262,122.335254029468)) ;
#70617 = CARTESIAN_POINT('Ctrl Pts',(-18.5392315505227,45.3414622997634,122.550561763219)) ;
#70618 = CARTESIAN_POINT('Ctrl Pts',(-18.7524316861596,45.5413260778729,122.029454998175)) ;
#70619 = CARTESIAN_POINT('Ctrl Pts',(-18.8838052127124,45.3613369975101,122.305924073514)) ;
#70620 = CARTESIAN_POINT('Ctrl Pts',(-19.2643939100382,45.5613080203947,121.888099189238)) ;
#70621 = CARTESIAN_POINT('Ctrl Pts',(-19.2933758171969,45.3813189400318,122.192842065019)) ;
#70622 = CARTESIAN_POINT('Ctrl Pts',(-19.7916381676523,45.5812106873055,121.930204794695)) ;
#70623 = CARTESIAN_POINT('Ctrl Pts',(-19.7151717616758,45.4012216069426,122.226529377587)) ;
#70624 = CARTESIAN_POINT('Ctrl Pts',(-20.2724895989063,45.6010660448442,122.147814462636)) ;
#70625 = CARTESIAN_POINT('Ctrl Pts',(-20.0998523930469,45.4210769644813,122.400620504394)) ;
#70626 = CARTESIAN_POINT('Ctrl Pts',(-20.6536580199716,45.6211300835602,122.520640262332)) ;
#70627 = CARTESIAN_POINT('Ctrl Pts',(-20.4047844905581,45.4411410031973,122.698883170157)) ;
#70628 = CARTESIAN_POINT('Ctrl Pts',(-20.8822424651067,45.6409852632853,122.996499598304)) ;
#70629 = CARTESIAN_POINT('Ctrl Pts',(-20.5876495721056,45.4609961829224,123.07957274604)) ;
#70630 = CARTESIAN_POINT('Ctrl Pts',(-20.9354305273725,45.6609653679497,123.524661889087)) ;
#70631 = CARTESIAN_POINT('Ctrl Pts',(-20.6301960379111,45.4809762875868,123.502103333297)) ;
#70632 = CARTESIAN_POINT('Ctrl Pts',(-20.8068347567717,45.6807744731195,124.035365380666)) ;
#70633 = CARTESIAN_POINT('Ctrl Pts',(-20.5273174457036,45.5007853927566,123.910665095287)) ;
#70634 = CARTESIAN_POINT('Ctrl Pts',(-20.5095739145416,45.7007670934602,124.475605981024)) ;
#70635 = CARTESIAN_POINT('Ctrl Pts',(-20.2894986134957,45.5207780130973,124.262859246648)) ;
#70636 = CARTESIAN_POINT('Ctrl Pts',(-20.1539637829234,45.7173065759643,124.734247767366)) ;
#70637 = CARTESIAN_POINT('Ctrl Pts',(-20.005029677627,45.5373174956014,124.469758245705)) ;
#70638 = CARTESIAN_POINT('Ctrl Pts',(-19.826276696828,45.7306708940285,124.860455779892)) ;
#70639 = CARTESIAN_POINT('Ctrl Pts',(-19.7428532302614,45.5506818136656,124.570733098296)) ;
#70640 = CARTESIAN_POINT('Ctrl Pts',(-19.4853999049105,45.74388849653,124.927543476285)) ;
#70641 = CARTESIAN_POINT('Ctrl Pts',(-19.4702042800056,45.5638994161671,124.624395485871)) ;
#70642 = CARTESIAN_POINT('Ctrl Pts',(-19.0437646821752,45.7605460908078,124.897999792884)) ;
#70643 = CARTESIAN_POINT('Ctrl Pts',(-19.1168393059101,45.5805570104449,124.60076273691)) ;
#70644 = CARTESIAN_POINT('Ctrl Pts',(-18.5604443553513,45.7804117928495,124.685196121248)) ;
#70645 = CARTESIAN_POINT('Ctrl Pts',(-18.7301974465919,45.6004227124867,124.430507595726)) ;
#70646 = CARTESIAN_POINT('Ctrl Pts',(-18.240630590451,45.7970415195396,124.380241225691)) ;
#70647 = CARTESIAN_POINT('Ctrl Pts',(-18.4743626408579,45.6170524391767,124.186562638723)) ;
#70648 = CARTESIAN_POINT('Ctrl Pts',(-18.0589348454478,45.8103306346774,124.081934291346)) ;
#70649 = CARTESIAN_POINT('Ctrl Pts',(-18.3289929495072,45.6303415543145,123.947896101221)) ;
#70650 = CARTESIAN_POINT('Ctrl Pts',(-17.9633418369383,45.8202949816545,123.838171148512)) ;
#70651 = CARTESIAN_POINT('Ctrl Pts',(-18.2525232679131,45.6403059012916,123.752891352259)) ;
#70652 = CARTESIAN_POINT('Ctrl Pts',(-17.9115389081574,45.830223349656,123.582470100099)) ;
#70653 = CARTESIAN_POINT('Ctrl Pts',(-18.2110838276306,45.6502342692931,123.548318177483)) ;
#70654 = CARTESIAN_POINT('Ctrl Pts',(-17.9020047414413,45.8435067827447,123.233481404821)) ;
#70655 = CARTESIAN_POINT('Ctrl Pts',(-18.2034517092472,45.6635177023819,123.269181304791)) ;
#70656 = CARTESIAN_POINT('Ctrl Pts',(-18.0050894429486,45.8601588604851,122.80309786385)) ;
#70657 = CARTESIAN_POINT('Ctrl Pts',(-18.2859374204291,45.6801697801222,122.924806771228)) ;
#70658 = CARTESIAN_POINT('Ctrl Pts',(-18.2472042450846,45.8767102297859,122.435821289861)) ;
#70659 = CARTESIAN_POINT('Ctrl Pts',(-18.4796083339964,45.696721149423,122.631034810004)) ;
#70660 = CARTESIAN_POINT('Ctrl Pts',(-18.5078328375495,45.8899976579349,122.203411111269)) ;
#70661 = CARTESIAN_POINT('Ctrl Pts',(-18.6881326846269,45.710008577572,122.445080306261)) ;
#70662 = CARTESIAN_POINT('Ctrl Pts',(-18.7324749007102,45.900042197635,122.064839904029)) ;
#70663 = CARTESIAN_POINT('Ctrl Pts',(-18.8678435288482,45.7200531172721,122.334231042964)) ;
#70664 = CARTESIAN_POINT('Ctrl Pts',(-18.9727512214166,45.9098850394588,121.969029204104)) ;
#70665 = CARTESIAN_POINT('Ctrl Pts',(-19.0600665012445,45.7298959590959,122.257583020281)) ;
#70666 = CARTESIAN_POINT('Ctrl Pts',(-19.2294892302823,45.9198693237057,121.91505230479)) ;
#70667 = CARTESIAN_POINT('Ctrl Pts',(-19.2654570275077,45.7398802433429,122.214404142504)) ;
#70668 = CARTESIAN_POINT('Ctrl Pts',(-19.4908293876516,45.9298189691049,121.906556619496)) ;
#70669 = CARTESIAN_POINT('Ctrl Pts',(-19.4745292486748,45.749829888742,122.207609741249)) ;
#70670 = CARTESIAN_POINT('Ctrl Pts',(-19.7510268140243,45.9398187307933,121.943434488528)) ;
#70671 = CARTESIAN_POINT('Ctrl Pts',(-19.6826867913636,45.7598296504304,122.23711429284)) ;
#70672 = CARTESIAN_POINT('Ctrl Pts',(-20.0015055166855,45.9498500767522,122.02559641534)) ;
#70673 = CARTESIAN_POINT('Ctrl Pts',(-19.8830690113146,45.7698609963893,122.302845959369)) ;
#70674 = CARTESIAN_POINT('Ctrl Pts',(-20.230012990869,45.9597050312293,122.147483174595)) ;
#70675 = CARTESIAN_POINT('Ctrl Pts',(-20.0658738423898,45.7797159508665,122.400357316511)) ;
#70676 = CARTESIAN_POINT('Ctrl Pts',(-20.4366698390954,45.9696775692299,122.308599139529)) ;
#70677 = CARTESIAN_POINT('Ctrl Pts',(-20.2311978645646,45.789688488867,122.529251805209)) ;
#70678 = CARTESIAN_POINT('Ctrl Pts',(-20.6126387229705,45.9796725629648,122.503651259972)) ;
#70679 = CARTESIAN_POINT('Ctrl Pts',(-20.3719712626983,45.7996834826019,122.685294957718)) ;
#70680 = CARTESIAN_POINT('Ctrl Pts',(-20.7523044634586,45.9897066217589,122.727282847818)) ;
#70681 = CARTESIAN_POINT('Ctrl Pts',(-20.4837019244027,45.809717541396,122.86420139806)) ;
#70682 = CARTESIAN_POINT('Ctrl Pts',(-20.8496612407523,45.9995619645819,122.967303410869)) ;
#70683 = CARTESIAN_POINT('Ctrl Pts',(-20.5615851977692,45.819572884219,123.056218516308)) ;
#70684 = CARTESIAN_POINT('Ctrl Pts',(-20.9049869101856,46.0095614439275,123.224140951696)) ;
#70685 = CARTESIAN_POINT('Ctrl Pts',(-20.6058435342198,45.8295723635646,123.261688948786)) ;
#70686 = CARTESIAN_POINT('Ctrl Pts',(-20.9150723248034,46.0194558926828,123.484010185289)) ;
#70687 = CARTESIAN_POINT('Ctrl Pts',(-20.6139096475916,45.8394668123199,123.469584210841)) ;
#70688 = CARTESIAN_POINT('Ctrl Pts',(-20.8792184641045,46.0295190121173,123.745970407933)) ;
#70689 = CARTESIAN_POINT('Ctrl Pts',(-20.5852243537012,45.8495299317544,123.67915211632)) ;
#70690 = CARTESIAN_POINT('Ctrl Pts',(-20.8004631964166,46.0393586573585,123.992305910844)) ;
#70691 = CARTESIAN_POINT('Ctrl Pts',(-20.5222181446683,45.8593695769957,123.876219533294)) ;
#70692 = CARTESIAN_POINT('Ctrl Pts',(-20.6777341782391,46.0494218215446,124.226510235197)) ;
#70693 = CARTESIAN_POINT('Ctrl Pts',(-20.4240329804487,45.8694327411817,124.063582012675)) ;
#70694 = CARTESIAN_POINT('Ctrl Pts',(-20.5187010120317,46.0593160912934,124.432251752361)) ;
#70695 = CARTESIAN_POINT('Ctrl Pts',(-20.2968048726953,45.8793270109305,124.228173673899)) ;
#70696 = CARTESIAN_POINT('Ctrl Pts',(-20.3259612493778,46.0692578173072,124.608573010416)) ;
#70697 = CARTESIAN_POINT('Ctrl Pts',(-20.1426117715884,45.8892687369444,124.369228956089)) ;
#70698 = CARTESIAN_POINT('Ctrl Pts',(-20.1041752620859,46.0792607059666,124.749748717296)) ;
#70699 = CARTESIAN_POINT('Ctrl Pts',(-19.965181898146,45.8992716256037,124.48216768824)) ;
#70700 = CARTESIAN_POINT('Ctrl Pts',(-19.8602243413917,46.0893005547606,124.850170623594)) ;
#70701 = CARTESIAN_POINT('Ctrl Pts',(-19.770020308728,45.9093114743977,124.562503212813)) ;
#70702 = CARTESIAN_POINT('Ctrl Pts',(-19.6081586045614,46.0991247702215,124.906078173757)) ;
#70703 = CARTESIAN_POINT('Ctrl Pts',(-19.5683677549541,45.9191356898586,124.607227074532)) ;
#70704 = CARTESIAN_POINT('Ctrl Pts',(-19.3441646598656,46.109181613715,124.918003343611)) ;
#70705 = CARTESIAN_POINT('Ctrl Pts',(-19.3571724382085,45.9291925333521,124.616765131644)) ;
#70706 = CARTESIAN_POINT('Ctrl Pts',(-19.0854647176779,46.119110223111,124.883999596897)) ;
#70707 = CARTESIAN_POINT('Ctrl Pts',(-19.150213020904,45.9391211427481,124.589560066791)) ;
#70708 = CARTESIAN_POINT('Ctrl Pts',(-18.8357963857665,46.1290621071489,124.806111234111)) ;
#70709 = CARTESIAN_POINT('Ctrl Pts',(-18.9504791821078,45.949073026786,124.527247495769)) ;
#70710 = CARTESIAN_POINT('Ctrl Pts',(-18.6013290923237,46.1391150599565,124.684426223968)) ;
#70711 = CARTESIAN_POINT('Ctrl Pts',(-18.7629062354974,45.9591259795936,124.429897589284)) ;
#70712 = CARTESIAN_POINT('Ctrl Pts',(-18.3960311454174,46.1489379364227,124.527912441961)) ;
#70713 = CARTESIAN_POINT('Ctrl Pts',(-18.5986696124886,45.9689488560598,124.304685323724)) ;
#70714 = CARTESIAN_POINT('Ctrl Pts',(-18.2165638688177,46.1589936689928,124.333973843009)) ;
#70715 = CARTESIAN_POINT('Ctrl Pts',(-18.455097186173,45.9790045886299,124.149533032839)) ;
#70716 = CARTESIAN_POINT('Ctrl Pts',(-18.0755063145666,46.1689344339805,124.114086515428)) ;
#70717 = CARTESIAN_POINT('Ctrl Pts',(-18.3422530053555,45.9889453536176,123.973622294175)) ;
#70718 = CARTESIAN_POINT('Ctrl Pts',(-17.9743911402895,46.1788387668861,123.874249737998)) ;
#70719 = CARTESIAN_POINT('Ctrl Pts',(-18.2613628144267,45.9988496865232,123.781752514046)) ;
#70720 = CARTESIAN_POINT('Ctrl Pts',(-17.9157922099519,46.1888854357668,123.616841983496)) ;
#70721 = CARTESIAN_POINT('Ctrl Pts',(-18.2144855602764,46.0088963554039,123.575825794976)) ;
#70722 = CARTESIAN_POINT('Ctrl Pts',(-17.9027335515217,46.1987809990726,123.357082770937)) ;
#70723 = CARTESIAN_POINT('Ctrl Pts',(-18.2040405772589,46.0187919187097,123.368018794538)) ;
#70724 = CARTESIAN_POINT('Ctrl Pts',(-17.9355083348723,46.2088430567729,123.094739738878)) ;
#70725 = CARTESIAN_POINT('Ctrl Pts',(-18.2302623332334,46.02885397641,123.158144462417)) ;
#70726 = CARTESIAN_POINT('Ctrl Pts',(-18.0115191596736,46.2186858344004,122.847471415839)) ;
#70727 = CARTESIAN_POINT('Ctrl Pts',(-18.2910726074192,46.0386967540375,122.960331026345)) ;
#70728 = CARTESIAN_POINT('Ctrl Pts',(-18.1304936326855,46.2286763126523,122.613475678947)) ;
#70729 = CARTESIAN_POINT('Ctrl Pts',(-18.3862537375702,46.0486872322894,122.773135382181)) ;
#70730 = CARTESIAN_POINT('Ctrl Pts',(-18.2873793152529,46.2386052852958,122.404966075839)) ;
#70731 = CARTESIAN_POINT('Ctrl Pts',(-18.5117634954812,46.0586162049329,122.60632910476)) ;
#70732 = CARTESIAN_POINT('Ctrl Pts',(-18.4789900283898,46.2485964221754,122.225460708948)) ;
#70733 = CARTESIAN_POINT('Ctrl Pts',(-18.6650531643566,46.0686073418125,122.462726177038)) ;
#70734 = CARTESIAN_POINT('Ctrl Pts',(-18.6997158872876,46.2586185396643,122.081771774985)) ;
#70735 = CARTESIAN_POINT('Ctrl Pts',(-18.8416348469598,46.0786294593014,122.347776532043)) ;
#70736 = CARTESIAN_POINT('Ctrl Pts',(-18.9390004515799,46.2685190500665,121.97961691748)) ;
#70737 = CARTESIAN_POINT('Ctrl Pts',(-19.0330627062083,46.0885299697036,122.266054470778)) ;
#70738 = CARTESIAN_POINT('Ctrl Pts',(-19.1945546489749,46.2785080428126,121.919635191703)) ;
#70739 = CARTESIAN_POINT('Ctrl Pts',(-19.2375063079573,46.0985189624497,122.218070771051)) ;
#70740 = CARTESIAN_POINT('Ctrl Pts',(-19.4560195398829,46.2884732868632,121.905154403475)) ;
#70741 = CARTESIAN_POINT('Ctrl Pts',(-19.4466780569291,46.1084842065003,122.206487877725)) ;
#70742 = CARTESIAN_POINT('Ctrl Pts',(-19.7145391120576,46.2983775513764,121.93549611882)) ;
#70743 = CARTESIAN_POINT('Ctrl Pts',(-19.653492980395,46.1183884710135,122.230762786779)) ;
#70744 = CARTESIAN_POINT('Ctrl Pts',(-19.9676465193919,46.3084356430746,122.011573715253)) ;
#70745 = CARTESIAN_POINT('Ctrl Pts',(-19.8559786088564,46.1284465627118,122.291626492136)) ;
#70746 = CARTESIAN_POINT('Ctrl Pts',(-20.1989353902242,46.318285583503,122.127826794879)) ;
#70747 = CARTESIAN_POINT('Ctrl Pts',(-20.0410082397393,46.1382965031402,122.384630018431)) ;
#70748 = CARTESIAN_POINT('Ctrl Pts',(-20.4106296400589,46.3283125946766,122.284718430549)) ;
#70749 = CARTESIAN_POINT('Ctrl Pts',(-20.2103627795123,46.1483235143137,122.510144538498)) ;
#70750 = CARTESIAN_POINT('Ctrl Pts',(-20.5914073282754,46.3383411812886,122.476498822217)) ;
#70751 = CARTESIAN_POINT('Ctrl Pts',(-20.3549837916193,46.1583521009257,122.663570001819)) ;
#70752 = CARTESIAN_POINT('Ctrl Pts',(-20.7338884447941,46.3481863954013,122.692436981991)) ;
#70753 = CARTESIAN_POINT('Ctrl Pts',(-20.4689669204349,46.1681973150384,122.836320620193)) ;
#70754 = CARTESIAN_POINT('Ctrl Pts',(-20.838883297733,46.3581771435809,122.933081577216)) ;
#70755 = CARTESIAN_POINT('Ctrl Pts',(-20.5529614728706,46.178188063218,123.028836705902)) ;
#70756 = CARTESIAN_POINT('Ctrl Pts',(-20.9002222159883,46.3682147771664,123.1896289369)) ;
#70757 = CARTESIAN_POINT('Ctrl Pts',(-20.6020311735636,46.1882256968035,123.234075045714)) ;
#70758 = CARTESIAN_POINT('Ctrl Pts',(-20.9162101455242,46.3780600663792,123.447862222641)) ;
#70759 = CARTESIAN_POINT('Ctrl Pts',(-20.614820050469,46.1980709860163,123.440660827507)) ;
#70760 = CARTESIAN_POINT('Ctrl Pts',(-20.8872976540046,46.3880414671851,123.708544539136)) ;
#70761 = CARTESIAN_POINT('Ctrl Pts',(-20.5916887966278,46.2080523868222,123.649206325939)) ;
#70762 = CARTESIAN_POINT('Ctrl Pts',(-20.8137082785738,46.397993700175,123.959520057968)) ;
#70763 = CARTESIAN_POINT('Ctrl Pts',(-20.5328161531047,46.2180046198121,123.849986010889)) ;
#70764 = CARTESIAN_POINT('Ctrl Pts',(-20.6974169783614,46.4079925116317,124.195165716517)) ;
#70765 = CARTESIAN_POINT('Ctrl Pts',(-20.4397820581274,46.2280034312688,124.038501896986)) ;
#70766 = CARTESIAN_POINT('Ctrl Pts',(-20.5409623495954,46.4180316155623,124.407564420263)) ;
#70767 = CARTESIAN_POINT('Ctrl Pts',(-20.3146171987756,46.2380425351995,124.208420165923)) ;
#70768 = CARTESIAN_POINT('Ctrl Pts',(-20.3544390959673,46.4278565579816,124.586111387913)) ;
#70769 = CARTESIAN_POINT('Ctrl Pts',(-20.1653985485672,46.2478674776188,124.351256099726)) ;
#70770 = CARTESIAN_POINT('Ctrl Pts',(-20.134995919871,46.4379112454576,124.733256870576)) ;
#70771 = CARTESIAN_POINT('Ctrl Pts',(-19.9898432095306,46.2579221650947,124.468971664984)) ;
#70772 = CARTESIAN_POINT('Ctrl Pts',(-19.8958234362632,46.4478540478144,124.838477290274)) ;
#70773 = CARTESIAN_POINT('Ctrl Pts',(-19.7985051353793,46.2678649674515,124.553146698639)) ;
#70774 = CARTESIAN_POINT('Ctrl Pts',(-19.6432030628621,46.4577578437542,124.901101950844)) ;
#70775 = CARTESIAN_POINT('Ctrl Pts',(-19.5964092448346,46.2777687633913,124.603245250316)) ;
#70776 = CARTESIAN_POINT('Ctrl Pts',(-19.3798141419767,46.4678046231292,124.919009575157)) ;
#70777 = CARTESIAN_POINT('Ctrl Pts',(-19.3856978663707,46.2878155427663,124.61757028202)) ;
#70778 = CARTESIAN_POINT('Ctrl Pts',(-19.1211811679258,46.4777002814238,124.891553789188)) ;
#70779 = CARTESIAN_POINT('Ctrl Pts',(-19.1787923210989,46.2977112010609,124.595604707242)) ;
#70780 = CARTESIAN_POINT('Ctrl Pts',(-18.8671103311317,46.4877618486744,124.818449852984)) ;
#70781 = CARTESIAN_POINT('Ctrl Pts',(-18.9755356841084,46.3077727683115,124.537120502504)) ;
#70782 = CARTESIAN_POINT('Ctrl Pts',(-18.6346615958398,46.4976064931117,124.704865605345)) ;
#70783 = CARTESIAN_POINT('Ctrl Pts',(-18.7895780913401,46.3176174127489,124.446252657151)) ;
#70784 = CARTESIAN_POINT('Ctrl Pts',(-18.4224718070244,46.5075665393544,124.551629282646)) ;
#70785 = CARTESIAN_POINT('Ctrl Pts',(-18.6198270211866,46.3275774589915,124.32366317014)) ;
#70786 = CARTESIAN_POINT('Ctrl Pts',(-18.2390573894743,46.5176048353728,124.362048863107)) ;
#70787 = CARTESIAN_POINT('Ctrl Pts',(-18.4730960549805,46.3376157550099,124.171998104319)) ;
#70788 = CARTESIAN_POINT('Ctrl Pts',(-18.0933321835797,46.5274781767911,124.147328823137)) ;
#70789 = CARTESIAN_POINT('Ctrl Pts',(-18.3565170542774,46.3474890964282,124.00022237033)) ;
#70790 = CARTESIAN_POINT('Ctrl Pts',(-17.9850644966569,46.5375512805904,123.905828159884)) ;
#70791 = CARTESIAN_POINT('Ctrl Pts',(-18.2699035102688,46.3575622002275,123.80702119456)) ;
#70792 = CARTESIAN_POINT('Ctrl Pts',(-17.9216561766812,46.5473720957093,123.655604769692)) ;
#70793 = CARTESIAN_POINT('Ctrl Pts',(-18.219177873809,46.3673830153464,123.606843503252)) ;
#70794 = CARTESIAN_POINT('Ctrl Pts',(-17.9018683250634,46.5574489607873,123.391584873684)) ;
#70795 = CARTESIAN_POINT('Ctrl Pts',(-18.2033482278461,46.3774598804244,123.395627180007)) ;
#70796 = CARTESIAN_POINT('Ctrl Pts',(-17.9277757499098,46.5673137004426,123.133615388447)) ;
#70797 = CARTESIAN_POINT('Ctrl Pts',(-18.2240747548872,46.3873246200797,123.189252631798)) ;
#70798 = CARTESIAN_POINT('Ctrl Pts',(-17.9985297244048,46.5773361036839,122.879929630516)) ;
#70799 = CARTESIAN_POINT('Ctrl Pts',(-18.2806784477161,46.397347023321,122.98630413088)) ;
#70800 = CARTESIAN_POINT('Ctrl Pts',(-18.1129004945136,46.5873618279724,122.642565399525)) ;
#70801 = CARTESIAN_POINT('Ctrl Pts',(-18.3721757093272,46.4073727476095,122.796412980426)) ;
#70802 = CARTESIAN_POINT('Ctrl Pts',(-18.2637366876288,46.5972166109937,122.432070963929)) ;
#70803 = CARTESIAN_POINT('Ctrl Pts',(-18.4928445100312,46.4172275306308,122.628018630033)) ;
#70804 = CARTESIAN_POINT('Ctrl Pts',(-18.4506972916997,46.607195454717,122.248181197861)) ;
#70805 = CARTESIAN_POINT('Ctrl Pts',(-18.6424130861803,46.4272063743541,122.48090728997)) ;
#70806 = CARTESIAN_POINT('Ctrl Pts',(-18.6678559884878,46.6172143469536,122.099336220667)) ;
#70807 = CARTESIAN_POINT('Ctrl Pts',(-18.8161403445689,46.4372252665907,122.361831725201)) ;
#70808 = CARTESIAN_POINT('Ctrl Pts',(-18.9041339832422,46.6270975559946,121.991423381431)) ;
#70809 = CARTESIAN_POINT('Ctrl Pts',(-19.0051620983221,46.4471084756317,122.275502163927)) ;
#70810 = CARTESIAN_POINT('Ctrl Pts',(-19.1602204279234,46.6371658653348,121.925081449906)) ;
#70811 = CARTESIAN_POINT('Ctrl Pts',(-19.2100316746212,46.4571767849719,122.222428931168)) ;
#70812 = CARTESIAN_POINT('Ctrl Pts',(-19.4177614318243,46.6469959906675,121.904397063364)) ;
#70813 = CARTESIAN_POINT('Ctrl Pts',(-19.4160632754822,46.4670069103046,122.205881850108)) ;
#70814 = CARTESIAN_POINT('Ctrl Pts',(-19.6811124793488,46.6570625430445,121.928980404509)) ;
#70815 = CARTESIAN_POINT('Ctrl Pts',(-19.6267444075026,46.4770734626816,122.22554879681)) ;
#70816 = CARTESIAN_POINT('Ctrl Pts',(-19.93175625164,46.6669527799382,121.997866497326)) ;
#70817 = CARTESIAN_POINT('Ctrl Pts',(-19.8272585403738,46.4869636995753,122.280657725669)) ;
#70818 = CARTESIAN_POINT('Ctrl Pts',(-20.1692553844016,46.6769450047322,122.109835361796)) ;
#70819 = CARTESIAN_POINT('Ctrl Pts',(-20.0172576312731,46.4969559243693,122.370232872609)) ;
#70820 = CARTESIAN_POINT('Ctrl Pts',(-20.3829389131417,46.6869076250832,122.261097188161)) ;
#70821 = CARTESIAN_POINT('Ctrl Pts',(-20.1882040373504,46.5069185447203,122.491242289893)) ;
#70822 = CARTESIAN_POINT('Ctrl Pts',(-20.5665204839457,46.6968126278463,122.445649602459)) ;
#70823 = CARTESIAN_POINT('Ctrl Pts',(-20.3350687382439,46.5168235474834,122.638883718221)) ;
#70824 = CARTESIAN_POINT('Ctrl Pts',(-20.7173901651887,46.7068703902444,122.662639131591)) ;
#70825 = CARTESIAN_POINT('Ctrl Pts',(-20.4557645655042,46.5268813098816,122.812475613443)) ;
#70826 = CARTESIAN_POINT('Ctrl Pts',(-20.8262181894773,46.7167209096232,122.89753556539)) ;
#70827 = CARTESIAN_POINT('Ctrl Pts',(-20.5428264841465,46.5367318292604,123.000391752439)) ;
#70828 = CARTESIAN_POINT('Ctrl Pts',(-20.8943773618054,46.7267524866214,123.15217347503)) ;
#70829 = CARTESIAN_POINT('Ctrl Pts',(-20.5973539588229,46.5467634062585,123.204102140928)) ;
#70830 = CARTESIAN_POINT('Ctrl Pts',(-20.9167369790523,46.7367622217263,123.414295804395)) ;
#70831 = CARTESIAN_POINT('Ctrl Pts',(-20.6152416326084,46.5567731413635,123.413799972381)) ;
#70832 = CARTESIAN_POINT('Ctrl Pts',(-20.8937123153054,46.7466717983526,123.673666920638)) ;
#70833 = CARTESIAN_POINT('Ctrl Pts',(-20.596822009193,46.5666827179897,123.621296152954)) ;
#70834 = CARTESIAN_POINT('Ctrl Pts',(-20.8265171674148,46.7565991842093,123.925758286608)) ;
#70835 = CARTESIAN_POINT('Ctrl Pts',(-20.5430662495124,46.5766101038464,123.822968723922)) ;
#70836 = CARTESIAN_POINT('Ctrl Pts',(-20.7150850922258,46.7666441186995,124.165042883978)) ;
#70837 = CARTESIAN_POINT('Ctrl Pts',(-20.4539206594605,46.5866550383367,124.014396623228)) ;
#70838 = CARTESIAN_POINT('Ctrl Pts',(-20.566303423748,46.7765300508875,124.378031588581)) ;
#70839 = CARTESIAN_POINT('Ctrl Pts',(-20.3348959856929,46.5965409705246,124.184786987194)) ;
#70840 = CARTESIAN_POINT('Ctrl Pts',(-20.3811494336437,46.7865233568405,124.56424680321)) ;
#70841 = CARTESIAN_POINT('Ctrl Pts',(-20.1867731294926,46.6065342764777,124.333759263123)) ;
#70842 = CARTESIAN_POINT('Ctrl Pts',(-20.167426750717,46.7964689946224,124.714688252167)) ;
#70843 = CARTESIAN_POINT('Ctrl Pts',(-20.0157955364757,46.6164799142595,124.454112381368)) ;
#70844 = CARTESIAN_POINT('Ctrl Pts',(-19.9310071201226,46.8064162629683,124.826243396208)) ;
#70845 = CARTESIAN_POINT('Ctrl Pts',(-19.8266604269535,46.6264271826054,124.543356680596)) ;
#70846 = CARTESIAN_POINT('Ctrl Pts',(-19.6762006528589,46.8164641651054,124.895457669008)) ;
#70847 = CARTESIAN_POINT('Ctrl Pts',(-19.6228151502625,46.6364750847425,124.598728484168)) ;
#70848 = CARTESIAN_POINT('Ctrl Pts',(-19.4184961828357,46.8263118599456,124.91911890289)) ;
#70849 = CARTESIAN_POINT('Ctrl Pts',(-19.4166527254704,46.6463227795827,124.617657767164)) ;
#70850 = CARTESIAN_POINT('Ctrl Pts',(-19.1575612607115,46.83627336969,124.898251094209)) ;
#70851 = CARTESIAN_POINT('Ctrl Pts',(-19.2079051028574,46.6562842893271,124.600964154411)) ;
#70852 = CARTESIAN_POINT('Ctrl Pts',(-18.902556312997,46.8463027612989,124.831598304346)) ;
#70853 = CARTESIAN_POINT('Ctrl Pts',(-19.0039009355955,46.666313680936,124.54764240293)) ;
#70854 = CARTESIAN_POINT('Ctrl Pts',(-18.6658571373904,46.8562102568536,124.723148671996)) ;
#70855 = CARTESIAN_POINT('Ctrl Pts',(-18.8145420155273,46.6762211764908,124.460883498429)) ;
#70856 = CARTESIAN_POINT('Ctrl Pts',(-18.4504873824993,46.8661556485166,124.575124657286)) ;
#70857 = CARTESIAN_POINT('Ctrl Pts',(-18.6422462094197,46.6861665681538,124.342465111585)) ;
#70858 = CARTESIAN_POINT('Ctrl Pts',(-18.262882041295,46.876157566114,124.390984128)) ;
#70859 = CARTESIAN_POINT('Ctrl Pts',(-18.4921615041804,46.6961684857511,124.195153273134)) ;
#70860 = CARTESIAN_POINT('Ctrl Pts',(-18.1099479381027,46.8861976336662,124.176016249327)) ;
#70861 = CARTESIAN_POINT('Ctrl Pts',(-18.3698136515618,46.7062085533033,124.023179206255)) ;
#70862 = CARTESIAN_POINT('Ctrl Pts',(-17.998547175216,46.896021945106,123.943090129844)) ;
#70863 = CARTESIAN_POINT('Ctrl Pts',(-18.280692897445,46.7160328647431,123.836839731432)) ;
#70864 = CARTESIAN_POINT('Ctrl Pts',(-17.9273097685191,46.9060781862621,123.688632681324)) ;
#70865 = CARTESIAN_POINT('Ctrl Pts',(-18.2237021026595,46.7260891058992,123.633273756565)) ;
#70866 = CARTESIAN_POINT('Ctrl Pts',(-17.9019600484687,46.9160091079977,123.4288626675)) ;
#70867 = CARTESIAN_POINT('Ctrl Pts',(-18.2034216287563,46.7360200276349,123.425458357104)) ;
#70868 = CARTESIAN_POINT('Ctrl Pts',(-17.9215882488076,46.925952344074,123.168336310537)) ;
#70869 = CARTESIAN_POINT('Ctrl Pts',(-18.2191232721713,46.7459632637111,123.217037686628)) ;
#70870 = CARTESIAN_POINT('Ctrl Pts',(-17.9861745623724,46.9359336280864,122.914073624315)) ;
#70871 = CARTESIAN_POINT('Ctrl Pts',(-18.2707913566683,46.7559445477236,123.01362751071)) ;
#70872 = CARTESIAN_POINT('Ctrl Pts',(-18.0949933336756,46.9459779297121,122.673631325158)) ;
#70873 = CARTESIAN_POINT('Ctrl Pts',(-18.3578456757999,46.7659888493492,122.821273187654)) ;
#70874 = CARTESIAN_POINT('Ctrl Pts',(-18.2402478329783,46.9558060109315,122.460027367171)) ;
#70875 = CARTESIAN_POINT('Ctrl Pts',(-18.474047818082,46.7758169305687,122.650390426094)) ;
#70876 = CARTESIAN_POINT('Ctrl Pts',(-18.4247793331419,46.9658826137807,122.270186990604)) ;
#70877 = CARTESIAN_POINT('Ctrl Pts',(-18.6216725361831,46.7858935334178,122.498517174402)) ;
#70878 = CARTESIAN_POINT('Ctrl Pts',(-18.6347009617729,46.9757346928992,122.118553078034)) ;
#70879 = CARTESIAN_POINT('Ctrl Pts',(-18.789608433041,46.7957456125364,122.377209782781)) ;
#70880 = CARTESIAN_POINT('Ctrl Pts',(-18.8728048873028,46.9858079512082,122.002979006205)) ;
#70881 = CARTESIAN_POINT('Ctrl Pts',(-18.9800913870549,46.8058188708453,122.28474940667)) ;
#70882 = CARTESIAN_POINT('Ctrl Pts',(-19.1215801045156,46.9956494105884,121.93222329205)) ;
#70883 = CARTESIAN_POINT('Ctrl Pts',(-19.1791102655951,46.8156603302256,122.228144091495)) ;
#70884 = CARTESIAN_POINT('Ctrl Pts',(-19.381859343394,47.0056105060008,121.904442012515)) ;
#70885 = CARTESIAN_POINT('Ctrl Pts',(-19.3873331982892,46.8256214256379,122.205917820199)) ;
#70886 = CARTESIAN_POINT('Ctrl Pts',(-19.6449738782894,47.0156477903975,121.922928491226)) ;
#70887 = CARTESIAN_POINT('Ctrl Pts',(-19.5978250114014,46.8356587100347,122.220705838776)) ;
#70888 = CARTESIAN_POINT('Ctrl Pts',(-19.8969217299239,47.0255241291328,121.985363214302)) ;
#70889 = CARTESIAN_POINT('Ctrl Pts',(-19.7993828256105,46.8455350487699,122.270652190592)) ;
#70890 = CARTESIAN_POINT('Ctrl Pts',(-20.1386279884017,47.0355862552861,122.092504779786)) ;
#70891 = CARTESIAN_POINT('Ctrl Pts',(-19.9927485620531,46.8555971749232,122.356364359904)) ;
#70892 = CARTESIAN_POINT('Ctrl Pts',(-20.3539188130597,47.0454544292626,122.237128270037)) ;
#70893 = CARTESIAN_POINT('Ctrl Pts',(-20.1649812567676,46.8654653488997,122.472061612692)) ;
#70894 = CARTESIAN_POINT('Ctrl Pts',(-20.5437493740665,47.0554599777664,122.419010050859)) ;
#70895 = CARTESIAN_POINT('Ctrl Pts',(-20.3168466298338,46.8754708974035,122.617565974457)) ;
#70896 = CARTESIAN_POINT('Ctrl Pts',(-20.6987362985448,47.065442609662,122.630724270001)) ;
#70897 = CARTESIAN_POINT('Ctrl Pts',(-20.440837183443,46.8854535292991,122.786936385641)) ;
#70898 = CARTESIAN_POINT('Ctrl Pts',(-20.8150425909332,47.0754865520838,122.867637130232)) ;
#70899 = CARTESIAN_POINT('Ctrl Pts',(-20.5338834673555,46.8954974717209,122.976466203145)) ;
#70900 = CARTESIAN_POINT('Ctrl Pts',(-20.8872078791894,47.0853147001109,123.115624213289)) ;
#70901 = CARTESIAN_POINT('Ctrl Pts',(-20.5916167561873,46.9053256197481,123.174854489363)) ;
#70902 = CARTESIAN_POINT('Ctrl Pts',(-20.9165166534759,47.0953045674853,123.37650718992)) ;
#70903 = CARTESIAN_POINT('Ctrl Pts',(-20.6150653220902,46.9153154871225,123.383560557976)) ;
#70904 = CARTESIAN_POINT('Ctrl Pts',(-20.8993091493922,47.1053483064408,123.639884268201)) ;
#70905 = CARTESIAN_POINT('Ctrl Pts',(-20.6013007427833,46.925359226078,123.594262430873)) ;
#70906 = CARTESIAN_POINT('Ctrl Pts',(-20.8385403650369,47.1151700549788,123.890732974447)) ;
#70907 = CARTESIAN_POINT('Ctrl Pts',(-20.5526874481851,46.9351809746159,123.794940790409)) ;
#70908 = CARTESIAN_POINT('Ctrl Pts',(-20.7334869965978,47.1252050325885,124.132613019297)) ;
#70909 = CARTESIAN_POINT('Ctrl Pts',(-20.4686462451259,46.9452159522256,123.988445566052)) ;
#70910 = CARTESIAN_POINT('Ctrl Pts',(-20.5875612969449,47.1352299453462,124.351957946675)) ;
#70911 = CARTESIAN_POINT('Ctrl Pts',(-20.3519069440029,46.9552408649833,124.163922368766)) ;
#70912 = CARTESIAN_POINT('Ctrl Pts',(-20.4093144805832,47.14508188844,124.539733165987)) ;
#70913 = CARTESIAN_POINT('Ctrl Pts',(-20.209311228941,46.9650928080772,124.314143082127)) ;
#70914 = CARTESIAN_POINT('Ctrl Pts',(-20.1985036701278,47.1550728497691,124.69617951058)) ;
#70915 = CARTESIAN_POINT('Ctrl Pts',(-20.0406637063053,46.9750837694063,124.439301445059)) ;
#70916 = CARTESIAN_POINT('Ctrl Pts',(-19.9654674976531,47.1649907246376,124.812968953075)) ;
#70917 = CARTESIAN_POINT('Ctrl Pts',(-19.8542359521288,46.9850016442747,124.532734341221)) ;
#70918 = CARTESIAN_POINT('Ctrl Pts',(-19.71297510293,47.1750192436388,124.88839013585)) ;
#70919 = CARTESIAN_POINT('Ctrl Pts',(-19.652242507693,46.9950301632759,124.593072964507)) ;
#70920 = CARTESIAN_POINT('Ctrl Pts',(-19.4549854354218,47.1849029224366,124.918522015687)) ;
#70921 = CARTESIAN_POINT('Ctrl Pts',(-19.4458515655707,47.0049138420738,124.617180149726)) ;
#70922 = CARTESIAN_POINT('Ctrl Pts',(-19.1927415406444,47.1948978658764,124.903808702217)) ;
#70923 = CARTESIAN_POINT('Ctrl Pts',(-19.2360564571309,47.0149087855135,124.605411359916)) ;
#70924 = CARTESIAN_POINT('Ctrl Pts',(-18.9363215273581,47.2049247196988,124.843152452533)) ;
#70925 = CARTESIAN_POINT('Ctrl Pts',(-19.0309200183396,47.0249356393359,124.55688809248)) ;
#70926 = CARTESIAN_POINT('Ctrl Pts',(-18.6976217950589,47.2148088840377,124.740702605869)) ;
#70927 = CARTESIAN_POINT('Ctrl Pts',(-18.8399600159307,47.0348198036749,124.47493012311)) ;
#70928 = CARTESIAN_POINT('Ctrl Pts',(-18.4778918251213,47.2247969820801,124.597178175501)) ;
#70929 = CARTESIAN_POINT('Ctrl Pts',(-18.6641751118157,47.0448079017172,124.360112235116)) ;
#70930 = CARTESIAN_POINT('Ctrl Pts',(-18.2869868870465,47.2347480885372,124.418412493407)) ;
#70931 = CARTESIAN_POINT('Ctrl Pts',(-18.511450049831,47.0547590081743,124.2171012666)) ;
#70932 = CARTESIAN_POINT('Ctrl Pts',(-18.1286864683151,47.2447931397053,124.207190353518)) ;
#70933 = CARTESIAN_POINT('Ctrl Pts',(-18.3848081587268,47.0648040593424,124.048124631986)) ;
#70934 = CARTESIAN_POINT('Ctrl Pts',(-18.0115053675036,47.2546549000636,123.976037450219)) ;
#70935 = CARTESIAN_POINT('Ctrl Pts',(-18.2910618397786,47.0746658197007,123.863203703224)) ;
#70936 = CARTESIAN_POINT('Ctrl Pts',(-17.9346962187188,47.264617716894,123.725744078448)) ;
#70937 = CARTESIAN_POINT('Ctrl Pts',(-18.2296126464617,47.0846286365312,123.662969789116)) ;
#70938 = CARTESIAN_POINT('Ctrl Pts',(-17.9027315659369,47.2746523981748,123.463999492697)) ;
#70939 = CARTESIAN_POINT('Ctrl Pts',(-18.2040389739103,47.0946633178119,123.453574331988)) ;
#70940 = CARTESIAN_POINT('Ctrl Pts',(-17.9160504867167,47.2845374279556,123.204536864795)) ;
#70941 = CARTESIAN_POINT('Ctrl Pts',(-18.214692073012,47.1045483475927,123.246004576489)) ;
#70942 = CARTESIAN_POINT('Ctrl Pts',(-17.9753215326006,47.2946030213536,122.946793722897)) ;
#70943 = CARTESIAN_POINT('Ctrl Pts',(-18.2621069751575,47.1146139409907,123.039809496486)) ;
#70944 = CARTESIAN_POINT('Ctrl Pts',(-18.0759175402315,47.3044421897151,122.708557598471)) ;
#70945 = CARTESIAN_POINT('Ctrl Pts',(-18.3425816822834,47.1244531093522,122.84922032325)) ;
#70946 = CARTESIAN_POINT('Ctrl Pts',(-18.2191949884316,47.3145047874566,122.486339905974)) ;
#70947 = CARTESIAN_POINT('Ctrl Pts',(-18.4572019469866,47.1345157070937,122.671444952012)) ;
#70948 = CARTESIAN_POINT('Ctrl Pts',(-18.396159615514,47.3244017998635,122.295722821703)) ;
#70949 = CARTESIAN_POINT('Ctrl Pts',(-18.5987718917569,47.1444127195006,122.518950162102)) ;
#70950 = CARTESIAN_POINT('Ctrl Pts',(-18.6037098264549,47.3343331216891,122.137504758704)) ;
#70951 = CARTESIAN_POINT('Ctrl Pts',(-18.7648105710639,47.1543440413262,122.392374154288)) ;
#70952 = CARTESIAN_POINT('Ctrl Pts',(-18.8382907890392,47.3443748844436,122.016648795488)) ;
#70953 = CARTESIAN_POINT('Ctrl Pts',(-18.9524743954627,47.1643858040807,122.295687495838)) ;
#70954 = CARTESIAN_POINT('Ctrl Pts',(-19.0864023365642,47.3542630833343,121.939374027969)) ;
#70955 = CARTESIAN_POINT('Ctrl Pts',(-19.1509626756622,47.1742740029714,122.233865749171)) ;
#70956 = CARTESIAN_POINT('Ctrl Pts',(-19.3468297085847,47.3642570219342,121.905591956175)) ;
#70957 = CARTESIAN_POINT('Ctrl Pts',(-19.3593042135663,47.1842679415713,122.206837953697)) ;
#70958 = CARTESIAN_POINT('Ctrl Pts',(-19.6078094898697,47.374197842971,121.917497147633)) ;
#70959 = CARTESIAN_POINT('Ctrl Pts',(-19.568087947677,47.1942087626082,122.216359938901)) ;
#70960 = CARTESIAN_POINT('Ctrl Pts',(-19.8632760200849,47.3841572252593,121.974310927408)) ;
#70961 = CARTESIAN_POINT('Ctrl Pts',(-19.772461509312,47.2041681448964,122.261808795976)) ;
#70962 = CARTESIAN_POINT('Ctrl Pts',(-20.1060266518377,47.3941549849116,122.074874782439)) ;
#70963 = CARTESIAN_POINT('Ctrl Pts',(-19.966662791665,47.2141659045487,122.342257824521)) ;
#70964 = CARTESIAN_POINT('Ctrl Pts',(-20.3282563986287,47.4041911211139,122.216891398893)) ;
#70965 = CARTESIAN_POINT('Ctrl Pts',(-20.1444477453573,47.224202040751,122.455869277174)) ;
#70966 = CARTESIAN_POINT('Ctrl Pts',(-20.5190751999569,47.4140419186048,122.391820347718)) ;
#70967 = CARTESIAN_POINT('Ctrl Pts',(-20.2971040399441,47.2340528382419,122.595810607946)) ;
#70968 = CARTESIAN_POINT('Ctrl Pts',(-20.6789956607079,47.4240027836811,122.599038839022)) ;
#70969 = CARTESIAN_POINT('Ctrl Pts',(-20.4250421187195,47.2440137033182,122.76158395382)) ;
#70970 = CARTESIAN_POINT('Ctrl Pts',(-20.8010651623618,47.4340316513115,122.832629226849)) ;
#70971 = CARTESIAN_POINT('Ctrl Pts',(-20.5226996700031,47.2540425709486,122.948455205887)) ;
#70972 = CARTESIAN_POINT('Ctrl Pts',(-20.8798481803655,47.4439418874479,123.080846336945)) ;
#70973 = CARTESIAN_POINT('Ctrl Pts',(-20.5857281550626,47.263952807085,123.147028060503)) ;
#70974 = CARTESIAN_POINT('Ctrl Pts',(-20.9151022554273,47.4538768407624,123.339542816455)) ;
#70975 = CARTESIAN_POINT('Ctrl Pts',(-20.6139336294218,47.2738877603996,123.353984836361)) ;
#70976 = CARTESIAN_POINT('Ctrl Pts',(-20.9045535939109,47.463917771172,123.603190649991)) ;
#70977 = CARTESIAN_POINT('Ctrl Pts',(-20.605496940888,47.2839286908091,123.564903155438)) ;
#70978 = CARTESIAN_POINT('Ctrl Pts',(-20.849402115707,47.4738056679536,123.857124325427)) ;
#70979 = CARTESIAN_POINT('Ctrl Pts',(-20.5613779800688,47.2938165875907,123.768050447587)) ;
#70980 = CARTESIAN_POINT('Ctrl Pts',(-20.750444918412,47.4837951196123,124.1002641636)) ;
#70981 = CARTESIAN_POINT('Ctrl Pts',(-20.4822143310711,47.3038060392494,123.962563117497)) ;
#70982 = CARTESIAN_POINT('Ctrl Pts',(-20.6110220669267,47.4937542099777,124.321740017003)) ;
#70983 = CARTESIAN_POINT('Ctrl Pts',(-20.3706779971095,47.3137651296148,124.13974493574)) ;
#70984 = CARTESIAN_POINT('Ctrl Pts',(-20.4368281965108,47.503651522284,124.514904688104)) ;
#70985 = CARTESIAN_POINT('Ctrl Pts',(-20.2313246021344,47.3236624419211,124.294278151825)) ;
#70986 = CARTESIAN_POINT('Ctrl Pts',(-20.2283967744204,47.5137079481842,124.677338457595)) ;
#70987 = CARTESIAN_POINT('Ctrl Pts',(-20.064580902708,47.3337188678213,124.424226901582)) ;
#70988 = CARTESIAN_POINT('Ctrl Pts',(-19.9992773799533,47.523577950774,124.798958001509)) ;
#70989 = CARTESIAN_POINT('Ctrl Pts',(-19.8812864635495,47.3435888704111,124.521524526354)) ;
#70990 = CARTESIAN_POINT('Ctrl Pts',(-19.7493845402161,47.5335818839512,124.880515352736)) ;
#70991 = CARTESIAN_POINT('Ctrl Pts',(-19.6813728797849,47.3535928035883,124.586772510695)) ;
#70992 = CARTESIAN_POINT('Ctrl Pts',(-19.4894723640348,47.5435691444151,124.917254732859)) ;
#70993 = CARTESIAN_POINT('Ctrl Pts',(-19.4734436940258,47.3635800640522,124.616166289918)) ;
#70994 = CARTESIAN_POINT('Ctrl Pts',(-19.2261503135035,47.5535961960008,124.908119289949)) ;
#70995 = CARTESIAN_POINT('Ctrl Pts',(-19.2627853251842,47.3736071156379,124.608859963816)) ;
#70996 = CARTESIAN_POINT('Ctrl Pts',(-18.9718149570964,47.5634872858269,124.854385043497)) ;
#70997 = CARTESIAN_POINT('Ctrl Pts',(-19.0593192486441,47.383498205464,124.565875589659)) ;
#70998 = CARTESIAN_POINT('Ctrl Pts',(-18.6475331408761,47.576785040608,124.724300286802)) ;
#70999 = CARTESIAN_POINT('Ctrl Pts',(-18.7998792298712,47.3967959602451,124.461806395647)) ;
#71000 = CARTESIAN_POINT('Ctrl Pts',(-18.3663382799237,47.5899831002161,124.51451143139)) ;
#71001 = CARTESIAN_POINT('Ctrl Pts',(-18.5749054443382,47.4099940198532,124.29395298759)) ;
#71002 = CARTESIAN_POINT('Ctrl Pts',(-18.1483991888473,47.6033798407853,124.238054641967)) ;
#71003 = CARTESIAN_POINT('Ctrl Pts',(-18.4005844644017,47.4233907604224,124.072822927662)) ;
#71004 = CARTESIAN_POINT('Ctrl Pts',(-18.025347143704,47.6132507528587,124.009644853001)) ;
#71005 = CARTESIAN_POINT('Ctrl Pts',(-18.3021342785884,47.4332616724959,123.890089214301)) ;
#71006 = CARTESIAN_POINT('Ctrl Pts',(-17.9421929511721,47.6233243146269,123.758382877817)) ;
#71007 = CARTESIAN_POINT('Ctrl Pts',(-18.2356106624253,47.443335234264,123.689082422527)) ;
#71008 = CARTESIAN_POINT('Ctrl Pts',(-17.9045616883877,47.6331457272152,123.502983370987)) ;
#71009 = CARTESIAN_POINT('Ctrl Pts',(-18.2055029686415,47.4531566468523,123.484761871704)) ;
#71010 = CARTESIAN_POINT('Ctrl Pts',(-17.911781843042,47.6432197444462,123.238412336144)) ;
#71011 = CARTESIAN_POINT('Ctrl Pts',(-18.2112771669349,47.4632306640834,123.273106890456)) ;
#71012 = CARTESIAN_POINT('Ctrl Pts',(-17.9808569614933,47.6563785314108,122.899509564629)) ;
#71013 = CARTESIAN_POINT('Ctrl Pts',(-18.2665340443339,47.4763894510479,123.001975913631)) ;
#71014 = CARTESIAN_POINT('Ctrl Pts',(-18.1386436633673,47.669744634505,122.581350825213)) ;
#71015 = CARTESIAN_POINT('Ctrl Pts',(-18.3927847615618,47.4897555541421,122.74742093734)) ;
#71016 = CARTESIAN_POINT('Ctrl Pts',(-18.370652315842,47.683058569394,122.319320691079)) ;
#71017 = CARTESIAN_POINT('Ctrl Pts',(-18.5783616726508,47.5030694890312,122.537834646464)) ;
#71018 = CARTESIAN_POINT('Ctrl Pts',(-18.5739282398627,47.6929586088415,122.157012936139)) ;
#71019 = CARTESIAN_POINT('Ctrl Pts',(-18.7409870352096,47.5129695284786,122.407978673393)) ;
#71020 = CARTESIAN_POINT('Ctrl Pts',(-18.8036181717246,47.702923011976,122.031241515346)) ;
#71021 = CARTESIAN_POINT('Ctrl Pts',(-18.9247363827808,47.5229339316132,122.307361838149)) ;
#71022 = CARTESIAN_POINT('Ctrl Pts',(-19.0533535758895,47.7129529790972,121.946938831321)) ;
#71023 = CARTESIAN_POINT('Ctrl Pts',(-19.1245251698578,47.5329638987343,122.239917409977)) ;
#71024 = CARTESIAN_POINT('Ctrl Pts',(-19.3105838879911,47.7228552557062,121.907675661922)) ;
#71025 = CARTESIAN_POINT('Ctrl Pts',(-19.3303061564412,47.5428661753434,122.208504383687)) ;
#71026 = CARTESIAN_POINT('Ctrl Pts',(-19.6591650885652,47.7361211848754,121.914819682812)) ;
#71027 = CARTESIAN_POINT('Ctrl Pts',(-19.609187461542,47.5561321045125,122.214219997551)) ;
#71028 = CARTESIAN_POINT('Ctrl Pts',(-20.0833550247634,47.7527427159818,122.037930509702)) ;
#71029 = CARTESIAN_POINT('Ctrl Pts',(-19.9485240134624,47.5727536356189,122.312705495618)) ;
#71030 = CARTESIAN_POINT('Ctrl Pts',(-20.510453729545,47.7726175446265,122.348898697034)) ;
#71031 = CARTESIAN_POINT('Ctrl Pts',(-20.2902038142842,47.5926284642636,122.561462978366)) ;
#71032 = CARTESIAN_POINT('Ctrl Pts',(-20.7582479358267,47.7892907527283,122.71623189636)) ;
#71033 = CARTESIAN_POINT('Ctrl Pts',(-20.4884640703777,47.6093016723655,122.855376229388)) ;
#71034 = CARTESIAN_POINT('Ctrl Pts',(-20.8714295868913,47.8025418777096,123.04557591284)) ;
#71035 = CARTESIAN_POINT('Ctrl Pts',(-20.5789911114765,47.6225527973467,123.118807090608)) ;
#71036 = CARTESIAN_POINT('Ctrl Pts',(-20.9269298434521,47.8157841965304,123.389178316211)) ;
#71037 = CARTESIAN_POINT('Ctrl Pts',(-20.6233964746189,47.6357951161676,123.393706836067)) ;
#71038 = CARTESIAN_POINT('Ctrl Pts',(-20.881145520325,47.8325174368699,123.831476120658)) ;
#71039 = CARTESIAN_POINT('Ctrl Pts',(-20.5867718080052,47.652528356507,123.747531615695)) ;
#71040 = CARTESIAN_POINT('Ctrl Pts',(-20.6511822086368,47.8523465850579,124.305796219641)) ;
#71041 = CARTESIAN_POINT('Ctrl Pts',(-20.4028036328943,47.672357504695,124.126994379831)) ;
#71042 = CARTESIAN_POINT('Ctrl Pts',(-20.2723934902227,47.8722712801585,124.675711001554)) ;
#71043 = CARTESIAN_POINT('Ctrl Pts',(-20.0997742015209,47.6922821997956,124.422927479501)) ;
#71044 = CARTESIAN_POINT('Ctrl Pts',(-19.7899432576281,47.8921945087419,124.89417687357)) ;
#71045 = CARTESIAN_POINT('Ctrl Pts',(-19.7138146109579,47.7122054283791,124.597703165401)) ;
#71046 = CARTESIAN_POINT('Ctrl Pts',(-19.2619554888101,47.912121647868,124.935052545408)) ;
#71047 = CARTESIAN_POINT('Ctrl Pts',(-19.2914239665457,47.7321325675052,124.630406187641)) ;
#71048 = CARTESIAN_POINT('Ctrl Pts',(-18.7527354696576,47.9319981104837,124.794293876189)) ;
#71049 = CARTESIAN_POINT('Ctrl Pts',(-18.8840463051201,47.7520090301208,124.51780103702)) ;
#71050 = CARTESIAN_POINT('Ctrl Pts',(-18.3198015893089,47.951975339089,124.486914551041)) ;
#71051 = CARTESIAN_POINT('Ctrl Pts',(-18.5376979391742,47.7719862587261,124.271898997653)) ;
#71052 = CARTESIAN_POINT('Ctrl Pts',(-18.0187050938315,47.9719101970627,124.050892286809)) ;
#71053 = CARTESIAN_POINT('Ctrl Pts',(-18.2968188352507,47.7919211166998,123.923081749406)) ;
#71054 = CARTESIAN_POINT('Ctrl Pts',(-17.8842318765923,47.9918066459935,123.539502996666)) ;
#71055 = CARTESIAN_POINT('Ctrl Pts',(-18.1892385060343,47.8118175656306,123.51396964369)) ;
#71056 = CARTESIAN_POINT('Ctrl Pts',(-17.9318165298211,48.0117279300601,123.012148120241)) ;
#71057 = CARTESIAN_POINT('Ctrl Pts',(-18.227305199235,47.8317388496972,123.092084787911)) ;
#71058 = CARTESIAN_POINT('Ctrl Pts',(-18.1570558911766,48.0316845797311,122.53190203543)) ;
#71059 = CARTESIAN_POINT('Ctrl Pts',(-18.4074959798686,47.8516954993682,122.7078870895)) ;
#71060 = CARTESIAN_POINT('Ctrl Pts',(-18.5309774065162,48.0515618728427,122.158784664484)) ;
#71061 = CARTESIAN_POINT('Ctrl Pts',(-18.7066337296029,47.8715727924798,122.409391583344)) ;
#71062 = CARTESIAN_POINT('Ctrl Pts',(-19.0095199143223,48.0714483450711,121.934235959805)) ;
#71063 = CARTESIAN_POINT('Ctrl Pts',(-19.0894691453368,47.8914592647082,122.229752104761)) ;
#71064 = CARTESIAN_POINT('Ctrl Pts',(-19.540633493891,48.0915099109951,121.886851609452)) ;
#71065 = CARTESIAN_POINT('Ctrl Pts',(-19.5143591422602,47.9115208306322,122.191844655207)) ;
#71066 = CARTESIAN_POINT('Ctrl Pts',(-20.0501821768271,48.1113503185359,122.022521216227)) ;
#71067 = CARTESIAN_POINT('Ctrl Pts',(-19.9220001526352,47.931361238173,122.300380806211)) ;
#71068 = CARTESIAN_POINT('Ctrl Pts',(-20.4843799802069,48.1312016425088,122.322303458234)) ;
#71069 = CARTESIAN_POINT('Ctrl Pts',(-20.2693591621974,47.9512125621459,122.540208559723)) ;
#71070 = CARTESIAN_POINT('Ctrl Pts',(-20.7926161664346,48.1512549124602,122.757030819445)) ;
#71071 = CARTESIAN_POINT('Ctrl Pts',(-20.5159469547042,47.9712658320974,122.887990515959)) ;
#71072 = CARTESIAN_POINT('Ctrl Pts',(-20.93252583496,48.1710755698436,123.265061844735)) ;
#71073 = CARTESIAN_POINT('Ctrl Pts',(-20.627874051427,47.9910864894807,123.294417505765)) ;
#71074 = CARTESIAN_POINT('Ctrl Pts',(-20.8912365983079,48.1910469911741,123.794086280571)) ;
#71075 = CARTESIAN_POINT('Ctrl Pts',(-20.5948408958009,48.0110579108112,123.717637230084)) ;
#71076 = CARTESIAN_POINT('Ctrl Pts',(-20.6727225902505,48.2109404835378,124.275764014104)) ;
#71077 = CARTESIAN_POINT('Ctrl Pts',(-20.4200275548019,48.0309514031749,124.102979505904)) ;
#71078 = CARTESIAN_POINT('Ctrl Pts',(-20.3004819424767,48.2309645697788,124.655976968053)) ;
#71079 = CARTESIAN_POINT('Ctrl Pts',(-20.1222337727236,48.050975489416,124.407148369197)) ;
#71080 = CARTESIAN_POINT('Ctrl Pts',(-19.8260643109497,48.2507694488917,124.884148701362)) ;
#71081 = CARTESIAN_POINT('Ctrl Pts',(-19.7426971430051,48.0707803685288,124.589684526452)) ;
#71082 = CARTESIAN_POINT('Ctrl Pts',(-19.298401689414,48.2707284645896,124.938563164576)) ;
#71083 = CARTESIAN_POINT('Ctrl Pts',(-19.3205664831375,48.0907393842267,124.633213331361)) ;
#71084 = CARTESIAN_POINT('Ctrl Pts',(-18.7834401752579,48.2907144882186,124.808270536172)) ;
#71085 = CARTESIAN_POINT('Ctrl Pts',(-18.9085977754014,48.1107254078558,124.528976723537)) ;
#71086 = CARTESIAN_POINT('Ctrl Pts',(-18.3471324483424,48.3105229839791,124.513544556307)) ;
#71087 = CARTESIAN_POINT('Ctrl Pts',(-18.5595521151312,48.1305339036163,124.29319269375)) ;
#71088 = CARTESIAN_POINT('Ctrl Pts',(-18.0344280932835,48.3305056230847,124.084394876722)) ;
#71089 = CARTESIAN_POINT('Ctrl Pts',(-18.3093912303342,48.1505165427219,123.949870956698)) ;
#71090 = CARTESIAN_POINT('Ctrl Pts',(-17.8877491679608,48.3503870708787,123.576606049549)) ;
#71091 = CARTESIAN_POINT('Ctrl Pts',(-18.1920510956395,48.1703979905159,123.543638317555)) ;
#71092 = CARTESIAN_POINT('Ctrl Pts',(-17.9228534217252,48.3703435376163,123.047472668677)) ;
#71093 = CARTESIAN_POINT('Ctrl Pts',(-18.2201380308155,48.1903544572534,123.120331605847)) ;
#71094 = CARTESIAN_POINT('Ctrl Pts',(-18.1353200268485,48.3902209345718,122.563676201082)) ;
#71095 = CARTESIAN_POINT('Ctrl Pts',(-18.3901149639764,48.210231854209,122.733295384716)) ;
#71096 = CARTESIAN_POINT('Ctrl Pts',(-18.5017348375152,48.4102028807471,122.179310317759)) ;
#71097 = CARTESIAN_POINT('Ctrl Pts',(-18.6832494823206,48.2302138003843,122.425805199473)) ;
#71098 = CARTESIAN_POINT('Ctrl Pts',(-18.9763255338847,48.4301319797839,121.943845821942)) ;
#71099 = CARTESIAN_POINT('Ctrl Pts',(-19.0629244628759,48.250142899421,122.237437292873)) ;
#71100 = CARTESIAN_POINT('Ctrl Pts',(-19.5025485758174,48.4500606029965,121.8844085627)) ;
#71101 = CARTESIAN_POINT('Ctrl Pts',(-19.4839018350502,48.2700715226336,122.189890020095)) ;
#71102 = CARTESIAN_POINT('Ctrl Pts',(-20.0154041734413,48.4698949271029,122.006602474331)) ;
#71103 = CARTESIAN_POINT('Ctrl Pts',(-19.8941925598735,48.28990584674,122.287654399379)) ;
#71104 = CARTESIAN_POINT('Ctrl Pts',(-20.3852740340378,48.4865472144863,122.249514009236)) ;
#71105 = CARTESIAN_POINT('Ctrl Pts',(-20.1900656488884,48.3065581341234,122.481970779686)) ;
#71106 = CARTESIAN_POINT('Ctrl Pts',(-20.6170557319961,48.4998077155085,122.509808729621)) ;
#71107 = CARTESIAN_POINT('Ctrl Pts',(-20.3755074720273,48.3198186351457,122.690222602484)) ;
#71108 = CARTESIAN_POINT('Ctrl Pts',(-20.7555225669231,48.5098091927098,122.73319887295)) ;
#71109 = CARTESIAN_POINT('Ctrl Pts',(-20.4862754159992,48.3298201123469,122.868932815288)) ;
#71110 = CARTESIAN_POINT('Ctrl Pts',(-20.8529891978789,48.5198412135693,122.978158629166)) ;
#71111 = CARTESIAN_POINT('Ctrl Pts',(-20.5642475521182,48.3398521332064,123.064902698722)) ;
#71112 = CARTESIAN_POINT('Ctrl Pts',(-20.9058519382839,48.5297047572949,123.231906669117)) ;
#71113 = CARTESIAN_POINT('Ctrl Pts',(-20.6065360580068,48.349715676932,123.267899228391)) ;
#71114 = CARTESIAN_POINT('Ctrl Pts',(-20.9146324101858,48.539673470965,123.493731289981)) ;
#71115 = CARTESIAN_POINT('Ctrl Pts',(-20.613556026208,48.3596843906021,123.477368180223)) ;
#71116 = CARTESIAN_POINT('Ctrl Pts',(-20.8648547231583,48.5530192183687,123.840870176946)) ;
#71117 = CARTESIAN_POINT('Ctrl Pts',(-20.5737423451447,48.3730301380058,123.755033409764)) ;
#71118 = CARTESIAN_POINT('Ctrl Pts',(-20.7281894338226,48.5661697734414,124.16259745941)) ;
#71119 = CARTESIAN_POINT('Ctrl Pts',(-20.4644056241511,48.3861806930785,124.012444016206)) ;
#71120 = CARTESIAN_POINT('Ctrl Pts',(-20.5118249048892,48.5795551539912,124.439903596676)) ;
#71121 = CARTESIAN_POINT('Ctrl Pts',(-20.2913023607941,48.3995660736284,124.234297052958)) ;
#71122 = CARTESIAN_POINT('Ctrl Pts',(-20.3188115906214,48.5894430899841,124.613917552832)) ;
#71123 = CARTESIAN_POINT('Ctrl Pts',(-20.1368920377986,48.4094540096212,124.373504600187)) ;
#71124 = CARTESIAN_POINT('Ctrl Pts',(-20.0965059871697,48.5994342797967,124.753554193822)) ;
#71125 = CARTESIAN_POINT('Ctrl Pts',(-19.9590458940921,48.4194451994339,124.485212524752)) ;
#71126 = CARTESIAN_POINT('Ctrl Pts',(-19.8542566549361,48.609386378335,124.852215716831)) ;
#71127 = CARTESIAN_POINT('Ctrl Pts',(-19.7652457303651,48.4293972979721,124.5641395104)) ;
#71128 = CARTESIAN_POINT('Ctrl Pts',(-19.5961577410576,48.6194326347855,124.907656726796)) ;
#71129 = CARTESIAN_POINT('Ctrl Pts',(-19.5587661686804,48.4394435544226,124.608490145194)) ;
#71130 = CARTESIAN_POINT('Ctrl Pts',(-19.337504837007,48.6292820821796,124.917439257159)) ;
#71131 = CARTESIAN_POINT('Ctrl Pts',(-19.3518437348216,48.4492930018168,124.616313910644)) ;
#71132 = CARTESIAN_POINT('Ctrl Pts',(-19.078037022272,48.6392447346748,124.882575057759)) ;
#71133 = CARTESIAN_POINT('Ctrl Pts',(-19.1442698490704,48.4592556543119,124.588420320008)) ;
#71134 = CARTESIAN_POINT('Ctrl Pts',(-18.8271502999389,48.6492678203169,124.802367820736)) ;
#71135 = CARTESIAN_POINT('Ctrl Pts',(-18.9435612086211,48.469278739954,124.524252395797)) ;
#71136 = CARTESIAN_POINT('Ctrl Pts',(-18.5961153422512,48.6591929360738,124.681264951306)) ;
#71137 = CARTESIAN_POINT('Ctrl Pts',(-18.7587343441336,48.479203855711,124.427368128863)) ;
#71138 = CARTESIAN_POINT('Ctrl Pts',(-18.3870750955819,48.6692454144736,124.519790373217)) ;
#71139 = CARTESIAN_POINT('Ctrl Pts',(-18.5915035653785,48.4892563341108,124.298186706336)) ;
#71140 = CARTESIAN_POINT('Ctrl Pts',(-18.2126444694148,48.6790969131764,124.328462267053)) ;
#71141 = CARTESIAN_POINT('Ctrl Pts',(-18.4519607973613,48.4991078328135,124.14512276976)) ;
#71142 = CARTESIAN_POINT('Ctrl Pts',(-18.0718445075732,48.6890686523789,124.107495060904)) ;
#71143 = CARTESIAN_POINT('Ctrl Pts',(-18.339322775097,48.509079572016,123.968347874547)) ;
#71144 = CARTESIAN_POINT('Ctrl Pts',(-17.9713155069276,48.6990638601446,123.86478462589)) ;
#71145 = CARTESIAN_POINT('Ctrl Pts',(-18.2589016723393,48.5190747797817,123.774178726449)) ;
#71146 = CARTESIAN_POINT('Ctrl Pts',(-17.9145635742469,48.7090978616136,123.607305099869)) ;
#71147 = CARTESIAN_POINT('Ctrl Pts',(-18.213502337176,48.5291087812508,123.568194649321)) ;
#71148 = CARTESIAN_POINT('Ctrl Pts',(-17.9031654069168,48.718953219706,123.348541528174)) ;
#71149 = CARTESIAN_POINT('Ctrl Pts',(-18.2043860513762,48.5389641393431,123.361183881843)) ;
#71150 = CARTESIAN_POINT('Ctrl Pts',(-17.937003026666,48.7289526952993,123.088000944887)) ;
#71151 = CARTESIAN_POINT('Ctrl Pts',(-18.231458353244,48.5489636149364,123.152751774568)) ;
#71152 = CARTESIAN_POINT('Ctrl Pts',(-18.0144858731634,48.7388471437944,122.839746756377)) ;
#71153 = CARTESIAN_POINT('Ctrl Pts',(-18.29344667902,48.5588580634315,122.954149283923)) ;
#71154 = CARTESIAN_POINT('Ctrl Pts',(-18.1359580112243,48.7489102680221,122.604899456879)) ;
#71155 = CARTESIAN_POINT('Ctrl Pts',(-18.3906263763058,48.5689211876593,122.766272439426)) ;
#71156 = CARTESIAN_POINT('Ctrl Pts',(-18.2926260056632,48.7587498943507,122.399136493447)) ;
#71157 = CARTESIAN_POINT('Ctrl Pts',(-18.5159623218924,48.5787608139879,122.601663664949)) ;
#71158 = CARTESIAN_POINT('Ctrl Pts',(-18.4866726839865,48.7688131293937,122.219522458127)) ;
#71159 = CARTESIAN_POINT('Ctrl Pts',(-18.6712011734618,48.5888240490308,122.457974012859)) ;
#71160 = CARTESIAN_POINT('Ctrl Pts',(-18.7053931823134,48.7787071346277,122.078888414331)) ;
#71161 = CARTESIAN_POINT('Ctrl Pts',(-18.8461785372344,48.5987180542649,122.345468767959)) ;
#71162 = CARTESIAN_POINT('Ctrl Pts',(-18.9460602718396,48.7886498478435,121.977234200229)) ;
#71163 = CARTESIAN_POINT('Ctrl Pts',(-19.038712845065,48.6086607674806,122.264147453385)) ;
#71164 = CARTESIAN_POINT('Ctrl Pts',(-19.2023805082056,48.7986555876417,121.918479266341)) ;
#71165 = CARTESIAN_POINT('Ctrl Pts',(-19.2437694535632,48.6186665072788,122.217145598752)) ;
#71166 = CARTESIAN_POINT('Ctrl Pts',(-19.4653884139487,48.8086764897881,121.905400360003)) ;
#71167 = CARTESIAN_POINT('Ctrl Pts',(-19.4541758671944,48.6286874094252,122.206684634383)) ;
#71168 = CARTESIAN_POINT('Ctrl Pts',(-19.7233301714243,48.818567259837,121.937466358609)) ;
#71169 = CARTESIAN_POINT('Ctrl Pts',(-19.660528678975,48.6385781794741,122.232339509988)) ;
#71170 = CARTESIAN_POINT('Ctrl Pts',(-19.9744129235702,48.8285586706167,122.014229612701)) ;
#71171 = CARTESIAN_POINT('Ctrl Pts',(-19.8613941678022,48.6485695902538,122.29375209031)) ;
#71172 = CARTESIAN_POINT('Ctrl Pts',(-20.2073088426993,48.8385070162812,122.13298779378)) ;
#71173 = CARTESIAN_POINT('Ctrl Pts',(-20.0477097505346,48.6585179359183,122.388760413796)) ;
#71174 = CARTESIAN_POINT('Ctrl Pts',(-20.4163278633967,48.8484518743424,122.289901832939)) ;
#71175 = CARTESIAN_POINT('Ctrl Pts',(-20.2149235466463,48.6684627939795,122.514293137704)) ;
#71176 = CARTESIAN_POINT('Ctrl Pts',(-20.5965846062851,48.8585067097353,122.483065165235)) ;
#71177 = CARTESIAN_POINT('Ctrl Pts',(-20.3591274717753,48.6785176293724,122.66882529591)) ;
#71178 = CARTESIAN_POINT('Ctrl Pts',(-20.7376368968491,48.8683290818368,122.699266149593)) ;
#71179 = CARTESIAN_POINT('Ctrl Pts',(-20.4719672538664,48.6883400014739,122.841786671009)) ;
#71180 = CARTESIAN_POINT('Ctrl Pts',(-20.8418372689003,48.8783849492805,122.942091527948)) ;
#71181 = CARTESIAN_POINT('Ctrl Pts',(-20.555325764693,48.6983958689176,123.036047837099)) ;
#71182 = CARTESIAN_POINT('Ctrl Pts',(-20.9011534756052,48.8883256791384,123.196510502706)) ;
#71183 = CARTESIAN_POINT('Ctrl Pts',(-20.6027766814318,48.7083365987755,123.239583219455)) ;
#71184 = CARTESIAN_POINT('Ctrl Pts',(-20.9161549876618,48.8982300176895,123.456358415646)) ;
#71185 = CARTESIAN_POINT('Ctrl Pts',(-20.6147759351108,48.7182409373267,123.447461235112)) ;
#71186 = CARTESIAN_POINT('Ctrl Pts',(-20.8852105592629,48.908276699118,123.718532273713)) ;
#71187 = CARTESIAN_POINT('Ctrl Pts',(-20.5900184387417,48.7282876187551,123.657200174612)) ;
#71188 = CARTESIAN_POINT('Ctrl Pts',(-20.810567540589,48.9181722065873,123.967677397249)) ;
#71189 = CARTESIAN_POINT('Ctrl Pts',(-20.530302315986,48.7381831262244,123.856515274534)) ;
#71190 = CARTESIAN_POINT('Ctrl Pts',(-20.6918640066937,48.9282344750859,124.203918318717)) ;
#71191 = CARTESIAN_POINT('Ctrl Pts',(-20.4353377019454,48.748245394723,124.045507277748)) ;
#71192 = CARTESIAN_POINT('Ctrl Pts',(-20.5374874732684,48.9380764653565,124.4114706526)) ;
#71193 = CARTESIAN_POINT('Ctrl Pts',(-20.3118353640093,48.7580873849936,124.211547452761)) ;
#71194 = CARTESIAN_POINT('Ctrl Pts',(-20.346982966348,48.9480698822375,124.59217583248)) ;
#71195 = CARTESIAN_POINT('Ctrl Pts',(-20.1594306094742,48.7680808018746,124.356110185967)) ;
#71196 = CARTESIAN_POINT('Ctrl Pts',(-20.1294622771985,48.9579943700896,124.736115686117)) ;
#71197 = CARTESIAN_POINT('Ctrl Pts',(-19.9854133980772,48.7780052897268,124.471260339818)) ;
#71198 = CARTESIAN_POINT('Ctrl Pts',(-19.8885974147487,48.9679940039981,124.841121711921)) ;
#71199 = CARTESIAN_POINT('Ctrl Pts',(-19.7927208876813,48.7880049236352,124.555263504968)) ;
#71200 = CARTESIAN_POINT('Ctrl Pts',(-19.6334469697658,48.9779801142549,124.9026502756)) ;
#71201 = CARTESIAN_POINT('Ctrl Pts',(-19.5886002554755,48.797991033892,124.604484611095)) ;
#71202 = CARTESIAN_POINT('Ctrl Pts',(-19.3702291570135,48.988016065442,124.918743054803)) ;
#71203 = CARTESIAN_POINT('Ctrl Pts',(-19.3780258273931,48.8080269850791,124.617357030523)) ;
#71204 = CARTESIAN_POINT('Ctrl Pts',(-19.1128025382839,48.9978727037768,124.889803469788)) ;
#71205 = CARTESIAN_POINT('Ctrl Pts',(-19.1720854580198,48.8178836234139,124.594203711341)) ;
#71206 = CARTESIAN_POINT('Ctrl Pts',(-18.8606911455665,49.0078716638548,124.815911669425)) ;
#71207 = CARTESIAN_POINT('Ctrl Pts',(-18.9703969207896,48.8278825834919,124.535088685264)) ;
#71208 = CARTESIAN_POINT('Ctrl Pts',(-18.6274774420179,49.0177668941686,124.700789980476)) ;
#71209 = CARTESIAN_POINT('Ctrl Pts',(-18.7838272068471,48.8377778138057,124.442990132716)) ;
#71210 = CARTESIAN_POINT('Ctrl Pts',(-18.4143731818113,49.0278274066372,124.544376734575)) ;
#71211 = CARTESIAN_POINT('Ctrl Pts',(-18.6133446125383,48.8478383262744,124.317858101007)) ;
#71212 = CARTESIAN_POINT('Ctrl Pts',(-18.2353571530203,49.0376766981834,124.357410469631)) ;
#71213 = CARTESIAN_POINT('Ctrl Pts',(-18.4701335294732,48.8576876178205,124.168284578467)) ;
#71214 = CARTESIAN_POINT('Ctrl Pts',(-18.0883869155088,49.0477038841156,124.13870846236)) ;
#71215 = CARTESIAN_POINT('Ctrl Pts',(-18.3525585546623,48.8677148037527,123.993322118891)) ;
#71216 = CARTESIAN_POINT('Ctrl Pts',(-17.9822338382996,49.0577324205749,123.89747926818)) ;
#71217 = CARTESIAN_POINT('Ctrl Pts',(-18.2676375508408,48.8777433402121,123.800338060987)) ;
#71218 = CARTESIAN_POINT('Ctrl Pts',(-17.9202532459207,49.0675776605399,123.646304603655)) ;
#71219 = CARTESIAN_POINT('Ctrl Pts',(-18.2180547698184,48.887588580177,123.599398834632)) ;
#71220 = CARTESIAN_POINT('Ctrl Pts',(-17.9018658552473,49.0775683554631,123.384397836007)) ;
#71221 = CARTESIAN_POINT('Ctrl Pts',(-18.2033462475352,48.8975792751002,123.389873479783)) ;
#71222 = CARTESIAN_POINT('Ctrl Pts',(-17.9299430170255,49.0876061762217,123.122114050778)) ;
#71223 = CARTESIAN_POINT('Ctrl Pts',(-18.2258094796159,48.9076170958588,123.180046505559)) ;
#71224 = CARTESIAN_POINT('Ctrl Pts',(-18.0013047262961,49.0974507699987,122.873439403411)) ;
#71225 = CARTESIAN_POINT('Ctrl Pts',(-18.2828999451431,48.9174616896358,122.981108076686)) ;
#71226 = CARTESIAN_POINT('Ctrl Pts',(-18.1158511804771,49.1074347653747,122.637421711162)) ;
#71227 = CARTESIAN_POINT('Ctrl Pts',(-18.3745381797035,48.9274456850118,122.792294678741)) ;
#71228 = CARTESIAN_POINT('Ctrl Pts',(-18.2691440175312,49.1173838139361,122.425609469171)) ;
#71229 = CARTESIAN_POINT('Ctrl Pts',(-18.4971732750292,48.9373947335732,122.622845958059)) ;
#71230 = CARTESIAN_POINT('Ctrl Pts',(-18.4576938725769,49.1273862529106,122.242453382412)) ;
#71231 = CARTESIAN_POINT('Ctrl Pts',(-18.6480139645982,48.9473971725478,122.476322036241)) ;
#71232 = CARTESIAN_POINT('Ctrl Pts',(-18.6757844901155,49.137407494207,122.094840814009)) ;
#71233 = CARTESIAN_POINT('Ctrl Pts',(-18.8224872183678,48.9574184138441,122.358233056651)) ;
#71234 = CARTESIAN_POINT('Ctrl Pts',(-18.912980073684,49.1473001726465,121.988431832938)) ;
#71235 = CARTESIAN_POINT('Ctrl Pts',(-19.0122435443815,48.9673110922836,122.273107306657)) ;
#71236 = CARTESIAN_POINT('Ctrl Pts',(-19.1674232251513,49.1572902265941,121.923790931797)) ;
#71237 = CARTESIAN_POINT('Ctrl Pts',(-19.2157981795932,48.9773011462313,122.221395753359)) ;
#71238 = CARTESIAN_POINT('Ctrl Pts',(-19.4284019621495,49.1672485877426,121.904559887262)) ;
#71239 = CARTESIAN_POINT('Ctrl Pts',(-19.4245809128314,48.9872595073797,122.206012139739)) ;
#71240 = CARTESIAN_POINT('Ctrl Pts',(-19.6873094646854,49.1771482146274,121.930145178779)) ;
#71241 = CARTESIAN_POINT('Ctrl Pts',(-19.6317061102632,48.9971591342646,122.226481354379)) ;
#71242 = CARTESIAN_POINT('Ctrl Pts',(-19.941526102593,49.1871961114308,122.001425268329)) ;
#71243 = CARTESIAN_POINT('Ctrl Pts',(-19.8350792979722,49.0072070310679,122.283506510641)) ;
#71244 = CARTESIAN_POINT('Ctrl Pts',(-20.1760417540059,49.1970914690668,122.113872563223)) ;
#71245 = CARTESIAN_POINT('Ctrl Pts',(-20.022690714718,49.0171023887039,122.373464959482)) ;
#71246 = CARTESIAN_POINT('Ctrl Pts',(-20.3909878097268,49.2071531215235,122.267804384145)) ;
#71247 = CARTESIAN_POINT('Ctrl Pts',(-20.1946471758079,49.0271640411606,122.496611400077)) ;
#71248 = CARTESIAN_POINT('Ctrl Pts',(-20.5720068053571,49.2169977257954,122.452644101985)) ;
#71249 = CARTESIAN_POINT('Ctrl Pts',(-20.3394609075565,49.0370086454325,122.644483128646)) ;
#71250 = CARTESIAN_POINT('Ctrl Pts',(-20.7206623097227,49.2269578474934,122.668068984939)) ;
#71251 = CARTESIAN_POINT('Ctrl Pts',(-20.4583844503407,49.0469687671305,122.816823184735)) ;
#71252 = CARTESIAN_POINT('Ctrl Pts',(-20.8300406886576,49.2369958818559,122.90810181371)) ;
#71253 = CARTESIAN_POINT('Ctrl Pts',(-20.5458863746886,49.0570068014931,123.008849944546)) ;
#71254 = CARTESIAN_POINT('Ctrl Pts',(-20.895474107219,49.2468701944424,123.15923667191)) ;
#71255 = CARTESIAN_POINT('Ctrl Pts',(-20.5982321097899,49.0668811140795,123.209757165169)) ;
#71256 = CARTESIAN_POINT('Ctrl Pts',(-20.9167021696326,49.2569396752251,123.422962968094)) ;
#71257 = CARTESIAN_POINT('Ctrl Pts',(-20.6152137829838,49.0769505948622,123.420738590608)) ;
#71258 = CARTESIAN_POINT('Ctrl Pts',(-20.8925309748415,49.2667740112422,123.680288852952)) ;
#71259 = CARTESIAN_POINT('Ctrl Pts',(-20.5958761715019,49.0867849308793,123.626598057855)) ;
#71260 = CARTESIAN_POINT('Ctrl Pts',(-20.8233682239885,49.2768069689704,123.934702843844)) ;
#71261 = CARTESIAN_POINT('Ctrl Pts',(-20.5405453724813,49.0968178886076,123.830129187291)) ;
#71262 = CARTESIAN_POINT('Ctrl Pts',(-20.7105597644519,49.2868273675456,124.172644633411)) ;
#71263 = CARTESIAN_POINT('Ctrl Pts',(-20.4502978908563,49.1068382871827,124.020482314942)) ;
#71264 = CARTESIAN_POINT('Ctrl Pts',(-20.5610300420917,49.2966929413168,124.38445939655)) ;
#71265 = CARTESIAN_POINT('Ctrl Pts',(-20.3306741735145,49.116703860954,124.189932981708)) ;
#71266 = CARTESIAN_POINT('Ctrl Pts',(-20.3732384290242,49.3067618159729,124.570826297004)) ;
#71267 = CARTESIAN_POINT('Ctrl Pts',(-20.1804402169388,49.12677273561,124.33902629884)) ;
#71268 = CARTESIAN_POINT('Ctrl Pts',(-20.1607506292362,49.3166072468784,124.718462326025)) ;
#71269 = CARTESIAN_POINT('Ctrl Pts',(-20.0104505595802,49.1366181665155,124.457133981811)) ;
#71270 = CARTESIAN_POINT('Ctrl Pts',(-19.9230300882037,49.3265868717491,124.829197136237)) ;
#71271 = CARTESIAN_POINT('Ctrl Pts',(-19.820274187598,49.1465977913862,124.545721370372)) ;
#71272 = CARTESIAN_POINT('Ctrl Pts',(-19.6685730451368,49.3366055546632,124.896756529863)) ;
#71273 = CARTESIAN_POINT('Ctrl Pts',(-19.6167084117739,49.1566164743003,124.599768387045)) ;
#71274 = CARTESIAN_POINT('Ctrl Pts',(-19.4098038796016,49.346488819847,124.919356964503)) ;
#71275 = CARTESIAN_POINT('Ctrl Pts',(-19.4096939213468,49.1664997394842,124.617848281741)) ;
#71276 = CARTESIAN_POINT('Ctrl Pts',(-19.1462832607712,49.3565571139384,124.89615090551)) ;
#71277 = CARTESIAN_POINT('Ctrl Pts',(-19.1988771347697,49.1765680335755,124.599282999011)) ;
#71278 = CARTESIAN_POINT('Ctrl Pts',(-18.8966752356581,49.3663872441237,124.829435060277)) ;
#71279 = CARTESIAN_POINT('Ctrl Pts',(-18.999191990857,49.1863981637609,124.545910321874)) ;
#71280 = CARTESIAN_POINT('Ctrl Pts',(-18.656744831752,49.3764537923389,124.718117896912)) ;
#71281 = CARTESIAN_POINT('Ctrl Pts',(-18.8072474823496,49.196464711976,124.456856234754)) ;
#71282 = CARTESIAN_POINT('Ctrl Pts',(-18.4436181844938,49.3863440410275,124.569306863408)) ;
#71283 = CARTESIAN_POINT('Ctrl Pts',(-18.6367470167291,49.2063549606646,124.337807652728)) ;
#71284 = CARTESIAN_POINT('Ctrl Pts',(-18.2572992166369,49.3963362228035,124.384299698902)) ;
#71285 = CARTESIAN_POINT('Ctrl Pts',(-18.4876920638657,49.2163471424406,124.189801941018)) ;
#71286 = CARTESIAN_POINT('Ctrl Pts',(-18.1065741069592,49.4062990034313,124.170232758712)) ;
#71287 = CARTESIAN_POINT('Ctrl Pts',(-18.3671123543255,49.2263099230684,124.018548569717)) ;
#71288 = CARTESIAN_POINT('Ctrl Pts',(-17.9953598077173,49.4162034081051,123.934891647468)) ;
#71289 = CARTESIAN_POINT('Ctrl Pts',(-18.2781412702089,49.2362143277422,123.830276340777)) ;
#71290 = CARTESIAN_POINT('Ctrl Pts',(-17.9258209627765,49.4262634025841,123.679859999836)) ;
#71291 = CARTESIAN_POINT('Ctrl Pts',(-18.2225102077793,49.2462743222212,123.626250739129)) ;
#71292 = CARTESIAN_POINT('Ctrl Pts',(-17.9019035489539,49.4361120245539,123.422136143483)) ;
#71293 = CARTESIAN_POINT('Ctrl Pts',(-18.2033764111946,49.256122944191,123.42007277146)) ;
#71294 = CARTESIAN_POINT('Ctrl Pts',(-17.9228967151139,49.4461424639657,123.159399391363)) ;
#71295 = CARTESIAN_POINT('Ctrl Pts',(-18.2201708355214,49.2661533836029,123.209883266575)) ;
#71296 = CARTESIAN_POINT('Ctrl Pts',(-17.9895783325629,49.4561521796005,122.90491683128)) ;
#71297 = CARTESIAN_POINT('Ctrl Pts',(-18.2735161375883,49.2761630992376,123.006297255522)) ;
#71298 = CARTESIAN_POINT('Ctrl Pts',(-18.0980952655541,49.4660629322931,122.668183285469)) ;
#71299 = CARTESIAN_POINT('Ctrl Pts',(-18.3603293441848,49.2860738519302,122.816911054056)) ;
#71300 = CARTESIAN_POINT('Ctrl Pts',(-18.245826326081,49.4759922052395,122.453085432562)) ;
#71301 = CARTESIAN_POINT('Ctrl Pts',(-18.4785136798849,49.2960031248766,122.644833143533)) ;
#71302 = CARTESIAN_POINT('Ctrl Pts',(-18.4308927790873,49.4860348966322,122.264952869192)) ;
#71303 = CARTESIAN_POINT('Ctrl Pts',(-18.6265668504671,49.3060458162693,122.494326860631)) ;
#71304 = CARTESIAN_POINT('Ctrl Pts',(-18.6423948660931,49.4959214298497,122.114039679069)) ;
#71305 = CARTESIAN_POINT('Ctrl Pts',(-18.7957676964125,49.3159323494868,122.373596652419)) ;
#71306 = CARTESIAN_POINT('Ctrl Pts',(-18.8791977037883,49.5059145747817,122.000547015104)) ;
#71307 = CARTESIAN_POINT('Ctrl Pts',(-18.9852096849577,49.3259254944189,122.282802310595)) ;
#71308 = CARTESIAN_POINT('Ctrl Pts',(-19.1309496466814,49.5158602556182,121.930322869947)) ;
#71309 = CARTESIAN_POINT('Ctrl Pts',(-19.1866107041673,49.3358711752553,122.226622847818)) ;
#71310 = CARTESIAN_POINT('Ctrl Pts',(-19.3910719340289,49.5258075127667,121.904340399635)) ;
#71311 = CARTESIAN_POINT('Ctrl Pts',(-19.3947080350026,49.3458184324039,122.205836499033)) ;
#71312 = CARTESIAN_POINT('Ctrl Pts',(-19.6543477211243,49.5358554166387,121.924410607122)) ;
#71313 = CARTESIAN_POINT('Ctrl Pts',(-19.605328890607,49.3558663362759,122.221892336368)) ;
#71314 = CARTESIAN_POINT('Ctrl Pts',(-19.9051063909627,49.5457031157367,121.988376325681)) ;
#71315 = CARTESIAN_POINT('Ctrl Pts',(-19.8059348407056,49.3657140353738,122.273064246999)) ;
#71316 = CARTESIAN_POINT('Ctrl Pts',(-20.1440032593785,49.5556646067154,122.095383178499)) ;
#71317 = CARTESIAN_POINT('Ctrl Pts',(-19.9970522508123,49.3756755263525,122.358669026334)) ;
#71318 = CARTESIAN_POINT('Ctrl Pts',(-20.3619888762732,49.5656940691293,122.243550726972)) ;
#71319 = CARTESIAN_POINT('Ctrl Pts',(-20.1714411021644,49.3857049887665,122.47720268182)) ;
#71320 = CARTESIAN_POINT('Ctrl Pts',(-20.5487252565727,49.5756013002292,122.424969613015)) ;
#71321 = CARTESIAN_POINT('Ctrl Pts',(-20.3208300784889,49.3956122198664,122.622336896963)) ;
#71322 = CARTESIAN_POINT('Ctrl Pts',(-20.7021484057419,49.5855476789066,122.636565942067)) ;
#71323 = CARTESIAN_POINT('Ctrl Pts',(-20.4435688760117,49.4055585985438,122.791613175442)) ;
#71324 = CARTESIAN_POINT('Ctrl Pts',(-20.817273052069,49.5955524477155,122.872960551607)) ;
#71325 = CARTESIAN_POINT('Ctrl Pts',(-20.5356691966512,49.4155633673526,122.980728486746)) ;
#71326 = CARTESIAN_POINT('Ctrl Pts',(-20.8894241945035,49.6055735687357,123.126222955828)) ;
#71327 = CARTESIAN_POINT('Ctrl Pts',(-20.5933907246933,49.4255844883728,123.183338265928)) ;
#71328 = CARTESIAN_POINT('Ctrl Pts',(-20.9164510303163,49.6154644345883,123.384745011977)) ;
#71329 = CARTESIAN_POINT('Ctrl Pts',(-20.6150128120107,49.4354753542255,123.390155041313)) ;
#71330 = CARTESIAN_POINT('Ctrl Pts',(-20.8983831554368,49.6254552433476,123.64665553533)) ;
#71331 = CARTESIAN_POINT('Ctrl Pts',(-20.6005593184925,49.4454661629847,123.599683344797)) ;
#71332 = CARTESIAN_POINT('Ctrl Pts',(-20.8353127628865,49.6354059015279,123.900441641724)) ;
#71333 = CARTESIAN_POINT('Ctrl Pts',(-20.550103868979,49.4554168211651,123.802711999998)) ;
#71334 = CARTESIAN_POINT('Ctrl Pts',(-20.7296226128942,49.64534211117,124.139186358957)) ;
#71335 = CARTESIAN_POINT('Ctrl Pts',(-20.4655527511557,49.4653530308072,123.993707659371)) ;
#71336 = CARTESIAN_POINT('Ctrl Pts',(-20.5836489640743,49.6553252778949,124.357211327668)) ;
#71337 = CARTESIAN_POINT('Ctrl Pts',(-20.3487747338897,49.475336197532,124.168127991278)) ;
#71338 = CARTESIAN_POINT('Ctrl Pts',(-20.4006247563479,49.6653690751052,124.547345114736)) ;
#71339 = CARTESIAN_POINT('Ctrl Pts',(-20.2023558633861,49.4853799947423,124.320235708206)) ;
#71340 = CARTESIAN_POINT('Ctrl Pts',(-20.1922492122206,49.6751972912734,124.70000920038)) ;
#71341 = CARTESIAN_POINT('Ctrl Pts',(-20.0356569367093,49.4952082109106,124.442367083583)) ;
#71342 = CARTESIAN_POINT('Ctrl Pts',(-19.9548171286621,49.6852738587427,124.817128808093)) ;
#71343 = CARTESIAN_POINT('Ctrl Pts',(-19.84571140594,49.5052847783798,124.536063826559)) ;
#71344 = CARTESIAN_POINT('Ctrl Pts',(-19.706248503042,49.6951259444321,124.889748332412)) ;
#71345 = CARTESIAN_POINT('Ctrl Pts',(-19.646857742828,49.5151368640692,124.594160163181)) ;
#71346 = CARTESIAN_POINT('Ctrl Pts',(-19.4431934347657,49.7051992118375,124.918954084388)) ;
#71347 = CARTESIAN_POINT('Ctrl Pts',(-19.436413489415,49.5252101314746,124.617525881266)) ;
#71348 = CARTESIAN_POINT('Ctrl Pts',(-19.1850858539182,49.7150406282611,124.902355961624)) ;
#71349 = CARTESIAN_POINT('Ctrl Pts',(-19.2299283962633,49.5350515478982,124.604248517549)) ;
#71350 = CARTESIAN_POINT('Ctrl Pts',(-18.93051882681,49.7250018864038,124.841407931651)) ;
#71351 = CARTESIAN_POINT('Ctrl Pts',(-19.0262747888918,49.545012806041,124.555491422723)) ;
#71352 = CARTESIAN_POINT('Ctrl Pts',(-18.6887821551517,49.7350385628358,124.735926054212)) ;
#71353 = CARTESIAN_POINT('Ctrl Pts',(-18.8328848873509,49.5550494824729,124.471106955947)) ;
#71354 = CARTESIAN_POINT('Ctrl Pts',(-18.472223638631,49.7449171706996,124.592716974689)) ;
#71355 = CARTESIAN_POINT('Ctrl Pts',(-18.6596380365307,49.5649280903367,124.356541193233)) ;
#71356 = CARTESIAN_POINT('Ctrl Pts',(-18.2803615486336,49.7549773993384,124.410883615209)) ;
#71357 = CARTESIAN_POINT('Ctrl Pts',(-18.5061473145343,49.5749883189755,124.211075281749)) ;
#71358 = CARTESIAN_POINT('Ctrl Pts',(-18.1259078276829,49.7648443834992,124.2025693445)) ;
#71359 = CARTESIAN_POINT('Ctrl Pts',(-18.3825837898089,49.5848553031363,124.044425304176)) ;
#71360 = CARTESIAN_POINT('Ctrl Pts',(-18.007919160607,49.7748499497519,123.967632043592)) ;
#71361 = CARTESIAN_POINT('Ctrl Pts',(-18.2881916293145,49.594860869389,123.856476155528)) ;
#71362 = CARTESIAN_POINT('Ctrl Pts',(-17.9327202356782,49.7848337381665,123.716228002346)) ;
#71363 = CARTESIAN_POINT('Ctrl Pts',(-18.2280312110072,49.6048446578036,123.655353491718)) ;
#71364 = CARTESIAN_POINT('Ctrl Pts',(-17.9024202751919,49.7948795949691,123.453999545748)) ;
#71365 = CARTESIAN_POINT('Ctrl Pts',(-18.2037899069106,49.6148905146063,123.445570751579)) ;
#71366 = CARTESIAN_POINT('Ctrl Pts',(-17.9174338428605,49.8047054721851,123.196221483282)) ;
#71367 = CARTESIAN_POINT('Ctrl Pts',(-18.2157993021619,49.6247163918222,123.23934924798)) ;
#71368 = CARTESIAN_POINT('Ctrl Pts',(-17.9771398351836,49.8146959480264,122.940561425494)) ;
#71369 = CARTESIAN_POINT('Ctrl Pts',(-18.2635625340082,49.6347068676635,123.034820978752)) ;
#71370 = CARTESIAN_POINT('Ctrl Pts',(-18.0815158765867,49.8247395239252,122.698141841169)) ;
#71371 = CARTESIAN_POINT('Ctrl Pts',(-18.3470620957204,49.6447504435623,122.840884636504)) ;
#71372 = CARTESIAN_POINT('Ctrl Pts',(-18.2227460406671,49.8345613162232,122.482103844544)) ;
#71373 = CARTESIAN_POINT('Ctrl Pts',(-18.4600443913908,49.6545722358604,122.668054229687)) ;
#71374 = CARTESIAN_POINT('Ctrl Pts',(-18.4027042307795,49.8445962818491,122.289342033901)) ;
#71375 = CARTESIAN_POINT('Ctrl Pts',(-18.6040097854602,49.6646072014862,122.513843584762)) ;
#71376 = CARTESIAN_POINT('Ctrl Pts',(-18.6136336981396,49.8546211987822,122.131496311253)) ;
#71377 = CARTESIAN_POINT('Ctrl Pts',(-18.772752461505,49.6746321184193,122.38756577421)) ;
#71378 = CARTESIAN_POINT('Ctrl Pts',(-18.844452425863,49.8644731371583,122.014217927815)) ;
#71379 = CARTESIAN_POINT('Ctrl Pts',(-18.9574059859319,49.6844840567954,122.293741978756)) ;
#71380 = CARTESIAN_POINT('Ctrl Pts',(-19.0954698169911,49.8744641131831,121.937362207403)) ;
#71381 = CARTESIAN_POINT('Ctrl Pts',(-19.1582192690863,49.6944750328202,122.232255812791)) ;
#71382 = CARTESIAN_POINT('Ctrl Pts',(-19.3541562238253,49.8843819339867,121.905312031361)) ;
#71383 = CARTESIAN_POINT('Ctrl Pts',(-19.3651677277275,49.7043928536238,122.206614010283)) ;
#71384 = CARTESIAN_POINT('Ctrl Pts',(-19.6173285205986,49.8944106545513,121.918768394832)) ;
#71385 = CARTESIAN_POINT('Ctrl Pts',(-19.5757056845183,49.7144215741884,122.217377365489)) ;
#71386 = CARTESIAN_POINT('Ctrl Pts',(-19.8705237928236,49.9042935811605,121.976696588945)) ;
#71387 = CARTESIAN_POINT('Ctrl Pts',(-19.7782617108459,49.7243045007976,122.263718061929)) ;
#71388 = CARTESIAN_POINT('Ctrl Pts',(-20.1128653758692,49.91429786628,122.078541501099)) ;
#71389 = CARTESIAN_POINT('Ctrl Pts',(-19.9721356237173,49.7343087859171,122.345192269613)) ;
#71390 = CARTESIAN_POINT('Ctrl Pts',(-20.3334334359267,49.9242815474878,122.22068996082)) ;
#71391 = CARTESIAN_POINT('Ctrl Pts',(-20.1485909406997,49.7442924671249,122.458909422584)) ;
#71392 = CARTESIAN_POINT('Ctrl Pts',(-20.5268216963565,49.9343225462177,122.400179102875)) ;
#71393 = CARTESIAN_POINT('Ctrl Pts',(-20.3033028181441,49.7543334658549,122.602499480691)) ;
#71394 = CARTESIAN_POINT('Ctrl Pts',(-20.683102613612,49.9441549910849,122.605949735523)) ;
#71395 = CARTESIAN_POINT('Ctrl Pts',(-20.4283285548429,49.764165910722,122.767114266815)) ;
#71396 = CARTESIAN_POINT('Ctrl Pts',(-20.8039177883312,49.9541499895152,122.839164524174)) ;
#71397 = CARTESIAN_POINT('Ctrl Pts',(-20.5249823843959,49.7741609091523,122.953685109195)) ;
#71398 = CARTESIAN_POINT('Ctrl Pts',(-20.8821585762413,49.9641815382648,123.090919199762)) ;
#71399 = CARTESIAN_POINT('Ctrl Pts',(-20.5875768107398,49.7841924579019,123.155088321944)) ;
#71400 = CARTESIAN_POINT('Ctrl Pts',(-20.9152659613685,49.9740469165703,123.348034537658)) ;
#71401 = CARTESIAN_POINT('Ctrl Pts',(-20.6140645490356,49.7940578362074,123.3607797692)) ;
#71402 = CARTESIAN_POINT('Ctrl Pts',(-20.9038469302478,49.9840087640306,123.609580354995)) ;
#71403 = CARTESIAN_POINT('Ctrl Pts',(-20.6049313502839,49.8040196836677,123.57001630993)) ;
#71404 = CARTESIAN_POINT('Ctrl Pts',(-20.8463577366402,49.9940437048448,123.8669305923)) ;
#71405 = CARTESIAN_POINT('Ctrl Pts',(-20.5589419045982,49.814054624482,123.77589695398)) ;
#71406 = CARTESIAN_POINT('Ctrl Pts',(-20.7469555508652,50.003928665862,124.106966043971)) ;
#71407 = CARTESIAN_POINT('Ctrl Pts',(-20.4794221918956,49.8239395854991,123.967925670353)) ;
#71408 = CARTESIAN_POINT('Ctrl Pts',(-20.6048292012254,50.0139942747808,124.330001338928)) ;
#71409 = CARTESIAN_POINT('Ctrl Pts',(-20.3657227455692,49.8340051944179,124.146355087729)) ;
#71410 = CARTESIAN_POINT('Ctrl Pts',(-20.4302906277304,50.0238334498225,124.520821628096)) ;
#71411 = CARTESIAN_POINT('Ctrl Pts',(-20.2260937730439,49.8438443694597,124.299012279554)) ;
#71412 = CARTESIAN_POINT('Ctrl Pts',(-20.2208961768224,50.0338960053224,124.682260919657)) ;
#71413 = CARTESIAN_POINT('Ctrl Pts',(-20.0585794010133,49.8539069249596,124.42816542681)) ;
#71414 = CARTESIAN_POINT('Ctrl Pts',(-19.990330202873,50.0437931800154,124.802645968509)) ;
#71415 = CARTESIAN_POINT('Ctrl Pts',(-19.8741279016726,49.8638040996525,124.524475111746)) ;
#71416 = CARTESIAN_POINT('Ctrl Pts',(-19.7418079589796,50.0537238949387,124.882264366511)) ;
#71417 = CARTESIAN_POINT('Ctrl Pts',(-19.6753109887391,49.8737348145758,124.588171796186)) ;
#71418 = CARTESIAN_POINT('Ctrl Pts',(-19.4802461248259,50.0637679230163,124.91762289268)) ;
#71419 = CARTESIAN_POINT('Ctrl Pts',(-19.4660617807019,49.8837788426534,124.616460713011)) ;
#71420 = CARTESIAN_POINT('Ctrl Pts',(-19.2206304688887,50.0736541248696,124.907397165842)) ;
#71421 = CARTESIAN_POINT('Ctrl Pts',(-19.2583695113846,49.8936650445067,124.608282273323)) ;
#71422 = CARTESIAN_POINT('Ctrl Pts',(-18.9639476699514,50.0836472913365,124.852050273482)) ;
#71423 = CARTESIAN_POINT('Ctrl Pts',(-19.0530228963227,49.9036582109736,124.564006892753)) ;
#71424 = CARTESIAN_POINT('Ctrl Pts',(-18.7219951492464,50.0935867623236,124.753556604735)) ;
#71425 = CARTESIAN_POINT('Ctrl Pts',(-18.8594602370748,49.9135976819608,124.485214036914)) ;
#71426 = CARTESIAN_POINT('Ctrl Pts',(-18.4991286839628,50.1036032766778,124.613546547454)) ;
#71427 = CARTESIAN_POINT('Ctrl Pts',(-18.6811659438584,49.9236141963149,124.37320785353)) ;
#71428 = CARTESIAN_POINT('Ctrl Pts',(-18.305447857855,50.1135333031546,124.438612238836)) ;
#71429 = CARTESIAN_POINT('Ctrl Pts',(-18.5262199636435,49.9335442227918,124.233262162402)) ;
#71430 = CARTESIAN_POINT('Ctrl Pts',(-18.1432330982203,50.1235858386641,124.23014085339)) ;
#71431 = CARTESIAN_POINT('Ctrl Pts',(-18.396446423529,49.9435967583012,124.066486379902)) ;
#71432 = CARTESIAN_POINT('Ctrl Pts',(-18.0220679537995,50.1334322418838,124.001499451881)) ;
#71433 = CARTESIAN_POINT('Ctrl Pts',(-18.2995125219658,49.9534431615209,123.883574567668)) ;
#71434 = CARTESIAN_POINT('Ctrl Pts',(-17.9407108291128,50.1433942847378,123.752685556883)) ;
#71435 = CARTESIAN_POINT('Ctrl Pts',(-18.2344247243619,49.963405204375,123.684524241367)) ;
#71436 = CARTESIAN_POINT('Ctrl Pts',(-17.903879790198,50.1534228355285,123.491714650898)) ;
#71437 = CARTESIAN_POINT('Ctrl Pts',(-18.2049577020538,49.9734337551656,123.475747861428)) ;
#71438 = CARTESIAN_POINT('Ctrl Pts',(-17.9127260347505,50.1633331612461,123.23144379837)) ;
#71439 = CARTESIAN_POINT('Ctrl Pts',(-18.212032467387,49.9833440808833,123.267531271564)) ;
#71440 = CARTESIAN_POINT('Ctrl Pts',(-17.9660995838745,50.1732680730757,122.975870378448)) ;
#71441 = CARTESIAN_POINT('Ctrl Pts',(-18.2547290835788,49.9932789927128,123.063072178671)) ;
#71442 = CARTESIAN_POINT('Ctrl Pts',(-18.0642927488552,50.1833090798438,122.730962183356)) ;
#71443 = CARTESIAN_POINT('Ctrl Pts',(-18.3332815219319,50.0033199994809,122.867144823383)) ;
#71444 = CARTESIAN_POINT('Ctrl Pts',(-18.201255664043,50.193196712676,122.510138724716)) ;
#71445 = CARTESIAN_POINT('Ctrl Pts',(-18.4428498771025,50.0132076323131,122.690484981077)) ;
#71446 = CARTESIAN_POINT('Ctrl Pts',(-18.3759163267486,50.203187143774,122.314146410369)) ;
#71447 = CARTESIAN_POINT('Ctrl Pts',(-18.5825766919906,50.0231980634112,122.533689671197)) ;
#71448 = CARTESIAN_POINT('Ctrl Pts',(-18.5813368510253,50.2131425803313,122.152125343484)) ;
#71449 = CARTESIAN_POINT('Ctrl Pts',(-18.7469116404268,50.0331534999684,122.404071093068)) ;
#71450 = CARTESIAN_POINT('Ctrl Pts',(-18.8104932141694,50.2230535284306,122.028377092564)) ;
#71451 = CARTESIAN_POINT('Ctrl Pts',(-18.9302356832612,50.0430644480677,122.305070539431)) ;
#71452 = CARTESIAN_POINT('Ctrl Pts',(-19.0601191774314,50.2330656045283,121.945157820195)) ;
#71453 = CARTESIAN_POINT('Ctrl Pts',(-19.1299354530242,50.0530765241654,122.238492965492)) ;
#71454 = CARTESIAN_POINT('Ctrl Pts',(-19.3208286510922,50.2430929266033,121.907019503274)) ;
#71455 = CARTESIAN_POINT('Ctrl Pts',(-19.3385035281413,50.0631038462404,122.207980229758)) ;
#71456 = CARTESIAN_POINT('Ctrl Pts',(-19.5798646279409,50.2529517015574,121.913948569486)) ;
#71457 = CARTESIAN_POINT('Ctrl Pts',(-19.5457290400626,50.0729626211945,122.213520711451)) ;
#71458 = CARTESIAN_POINT('Ctrl Pts',(-19.9254133373517,50.2663778943698,121.984759551957)) ;
#71459 = CARTESIAN_POINT('Ctrl Pts',(-19.8221850711281,50.086388814007,122.270169142813)) ;
#71460 = CARTESIAN_POINT('Ctrl Pts',(-20.2369013110527,50.2794619101513,122.13968280904)) ;
#71461 = CARTESIAN_POINT('Ctrl Pts',(-20.0713939474092,50.0994728297884,122.394125151919)) ;
#71462 = CARTESIAN_POINT('Ctrl Pts',(-20.5024950621529,50.2929353589065,122.373723117195)) ;
#71463 = CARTESIAN_POINT('Ctrl Pts',(-20.2838339357162,50.1129462785436,122.581328603426)) ;
#71464 = CARTESIAN_POINT('Ctrl Pts',(-20.6634968410946,50.3027683167123,122.575877232274)) ;
#71465 = CARTESIAN_POINT('Ctrl Pts',(-20.4126446009124,50.1227792363495,122.743055923512)) ;
#71466 = CARTESIAN_POINT('Ctrl Pts',(-20.7895391335986,50.312731590163,122.805346777483)) ;
#71467 = CARTESIAN_POINT('Ctrl Pts',(-20.5134783878091,50.1327425098001,122.926629108663)) ;
#71468 = CARTESIAN_POINT('Ctrl Pts',(-20.8739118055342,50.322768663981,123.05524832364)) ;
#71469 = CARTESIAN_POINT('Ctrl Pts',(-20.5809791128739,50.1427795836181,123.126549935224)) ;
#71470 = CARTESIAN_POINT('Ctrl Pts',(-20.9134611751376,50.3326436669926,123.311752830501)) ;
#71471 = CARTESIAN_POINT('Ctrl Pts',(-20.6126206731099,50.1526545866297,123.331753172435)) ;
#71472 = CARTESIAN_POINT('Ctrl Pts',(-20.9077542261225,50.3427113466188,123.576222416539)) ;
#71473 = CARTESIAN_POINT('Ctrl Pts',(-20.6080572696327,50.1627222662559,123.543329200487)) ;
#71474 = CARTESIAN_POINT('Ctrl Pts',(-20.857508009601,50.3525521968365,123.829932935511)) ;
#71475 = CARTESIAN_POINT('Ctrl Pts',(-20.5678626302659,50.1725631164736,123.746296581769)) ;
#71476 = CARTESIAN_POINT('Ctrl Pts',(-20.7314548291478,50.3658883953125,124.156910684336)) ;
#71477 = CARTESIAN_POINT('Ctrl Pts',(-20.4670213805127,50.1858993149496,124.00788851066)) ;
#71478 = CARTESIAN_POINT('Ctrl Pts',(-20.524653068368,50.3791059191269,124.440925618285)) ;
#71479 = CARTESIAN_POINT('Ctrl Pts',(-20.3015547453208,50.199116838764,124.235123745287)) ;
#71480 = CARTESIAN_POINT('Ctrl Pts',(-20.252395006723,50.3924408456182,124.66151880778)) ;
#71481 = CARTESIAN_POINT('Ctrl Pts',(-20.0837839668042,50.2124517652553,124.411566257854)) ;
#71482 = CARTESIAN_POINT('Ctrl Pts',(-20.0229851842833,50.4024239462128,124.788869046757)) ;
#71483 = CARTESIAN_POINT('Ctrl Pts',(-19.9002502106648,50.2224348658499,124.513455083149)) ;
#71484 = CARTESIAN_POINT('Ctrl Pts',(-19.7733522297728,50.4124687221124,124.874590001612)) ;
#71485 = CARTESIAN_POINT('Ctrl Pts',(-19.7005468471622,50.2324796417495,124.582032094973)) ;
#71486 = CARTESIAN_POINT('Ctrl Pts',(-19.5185568926512,50.4222866452983,124.915250650633)) ;
#71487 = CARTESIAN_POINT('Ctrl Pts',(-19.4967086995116,50.2422975649354,124.614562632195)) ;
#71488 = CARTESIAN_POINT('Ctrl Pts',(-19.2545052235582,50.4323359592536,124.911493375565)) ;
#71489 = CARTESIAN_POINT('Ctrl Pts',(-19.2854717860523,50.2523468788908,124.611560855551)) ;
#71490 = CARTESIAN_POINT('Ctrl Pts',(-18.9112636456039,50.4456396998762,124.845209773811)) ;
#71491 = CARTESIAN_POINT('Ctrl Pts',(-19.0108574254215,50.2656506195133,124.558525723013)) ;
#71492 = CARTESIAN_POINT('Ctrl Pts',(-18.5163636183236,50.4621298953529,124.654888417403)) ;
#71493 = CARTESIAN_POINT('Ctrl Pts',(-18.6949672451094,50.28214081499,124.406294866323)) ;
#71494 = CARTESIAN_POINT('Ctrl Pts',(-18.2061311342259,50.4788490602775,124.336917792434)) ;
#71495 = CARTESIAN_POINT('Ctrl Pts',(-18.4467378517919,50.2988599799146,124.151872297986)) ;
#71496 = CARTESIAN_POINT('Ctrl Pts',(-18.0368827272804,50.4920100539476,124.035219084609)) ;
#71497 = CARTESIAN_POINT('Ctrl Pts',(-18.311368220634,50.3120209735847,123.910554390484)) ;
#71498 = CARTESIAN_POINT('Ctrl Pts',(-17.9492027072533,50.5020062760529,123.787616040863)) ;
#71499 = CARTESIAN_POINT('Ctrl Pts',(-18.2412163833771,50.32201719569,123.712463854449)) ;
#71500 = CARTESIAN_POINT('Ctrl Pts',(-17.9063100733637,50.5120301155866,123.527712476807)) ;
#71501 = CARTESIAN_POINT('Ctrl Pts',(-18.2069016114084,50.3320410352238,123.504545668271)) ;
#71502 = CARTESIAN_POINT('Ctrl Pts',(-17.9093431973629,50.5252234375799,123.180991999699)) ;
#71503 = CARTESIAN_POINT('Ctrl Pts',(-18.2093282776367,50.345234357217,123.227157652856)) ;
#71504 = CARTESIAN_POINT('Ctrl Pts',(-18.027118283777,50.5418826093572,122.754212984447)) ;
#71505 = CARTESIAN_POINT('Ctrl Pts',(-18.3035426189576,50.3618935289943,122.885745424795)) ;
#71506 = CARTESIAN_POINT('Ctrl Pts',(-18.333937561739,50.5617927848429,122.323039035125)) ;
#71507 = CARTESIAN_POINT('Ctrl Pts',(-18.5489966706976,50.38180370448,122.540800132755)) ;
#71508 = CARTESIAN_POINT('Ctrl Pts',(-18.7684393921744,50.5816827726873,122.021820822919)) ;
#71509 = CARTESIAN_POINT('Ctrl Pts',(-18.8965968570353,50.4016936923244,122.299823770032)) ;
#71510 = CARTESIAN_POINT('Ctrl Pts',(-19.2825937715403,50.6016882207021,121.886677539595)) ;
#71511 = CARTESIAN_POINT('Ctrl Pts',(-19.307919625913,50.4216991403392,122.191706067227)) ;
#71512 = CARTESIAN_POINT('Ctrl Pts',(-19.8078113963263,50.6215246147294,121.934169205366)) ;
#71513 = CARTESIAN_POINT('Ctrl Pts',(-19.7280952319297,50.4415355343665,122.229696987763)) ;
#71514 = CARTESIAN_POINT('Ctrl Pts',(-20.2892513212485,50.6415324086261,122.159662815759)) ;
#71515 = CARTESIAN_POINT('Ctrl Pts',(-20.1132481557937,50.4615433282632,122.410089630547)) ;
#71516 = CARTESIAN_POINT('Ctrl Pts',(-20.6617398847741,50.66135904492,122.532541564671)) ;
#71517 = CARTESIAN_POINT('Ctrl Pts',(-20.4112416638867,50.4813699645572,122.708392168977)) ;
#71518 = CARTESIAN_POINT('Ctrl Pts',(-20.8871620269531,50.6813379878739,123.013304098428)) ;
#71519 = CARTESIAN_POINT('Ctrl Pts',(-20.5915810553221,50.501348907511,123.093001677507)) ;
#71520 = CARTESIAN_POINT('Ctrl Pts',(-20.9339369378857,50.701269789743,123.540918150504)) ;
#71521 = CARTESIAN_POINT('Ctrl Pts',(-20.6290028531258,50.5212807093801,123.515093416669)) ;
#71522 = CARTESIAN_POINT('Ctrl Pts',(-20.8002489892957,50.7210940902405,124.050742162796)) ;
#71523 = CARTESIAN_POINT('Ctrl Pts',(-20.5220534268662,50.5411050098776,123.922954725086)) ;
#71524 = CARTESIAN_POINT('Ctrl Pts',(-20.4959470937685,50.7411900915803,124.489434446394)) ;
#71525 = CARTESIAN_POINT('Ctrl Pts',(-20.2786119963971,50.5612010112175,124.273908331322)) ;
#71526 = CARTESIAN_POINT('Ctrl Pts',(-20.0674250455001,50.7609485076843,124.793529199864)) ;
#71527 = CARTESIAN_POINT('Ctrl Pts',(-19.9357982255067,50.5809594273214,124.517186790158)) ;
#71528 = CARTESIAN_POINT('Ctrl Pts',(-19.5529196248031,50.7810422005684,124.935512899744)) ;
#71529 = CARTESIAN_POINT('Ctrl Pts',(-19.524171586782,50.6010531202055,124.630773511285)) ;
#71530 = CARTESIAN_POINT('Ctrl Pts',(-19.2053312341041,50.7941531664751,124.907880339345)) ;
#71531 = CARTESIAN_POINT('Ctrl Pts',(-19.2461441930599,50.6141640861122,124.608669210494)) ;
#71532 = CARTESIAN_POINT('Ctrl Pts',(-19.035117438896,50.8008665412629,124.864312062334)) ;
#71533 = CARTESIAN_POINT('Ctrl Pts',(-19.1099467513572,50.6208774609001,124.573813086965)) ;
#71534 = CARTESIAN_POINT('',(-20.6544117723369,12.0237783230283,123.301689203239)) ;
#71535 = CARTESIAN_POINT('Ctrl Pts',(-20.6544115797749,12.0237782093581,123.301688455234)) ;
#71536 = CARTESIAN_POINT('Ctrl Pts',(-20.6751132995434,12.0362928130092,123.293550512105)) ;
#71537 = CARTESIAN_POINT('Ctrl Pts',(-20.6957063040839,12.0487910861619,123.284611049605)) ;
#71538 = CARTESIAN_POINT('Ctrl Pts',(-20.7158767772876,12.0611019792037,123.274999238965)) ;
#71539 = CARTESIAN_POINT('Ctrl Pts',(-20.7358112078758,12.0732688054522,123.26549990942)) ;
#71540 = CARTESIAN_POINT('Ctrl Pts',(-20.7553325868204,12.0852526121581,123.255343873335)) ;
#71541 = CARTESIAN_POINT('Ctrl Pts',(-20.774148982094,12.0968882682071,123.24470604279)) ;
#71542 = CARTESIAN_POINT('Ctrl Pts',(-20.7790756776112,12.0999348312529,123.24192074033)) ;
#71543 = CARTESIAN_POINT('Ctrl Pts',(-20.7839541174359,12.102957526743,123.239102676279)) ;
#71544 = CARTESIAN_POINT('Ctrl Pts',(-20.788779231699,12.1059533903454,123.236255555915)) ;
#71545 = CARTESIAN_POINT('Ctrl Pts',(-20.808608031553,12.1182648873431,123.224555319035)) ;
#71546 = CARTESIAN_POINT('Ctrl Pts',(-20.8282355576711,12.1305576883349,123.211948910434)) ;
#71547 = CARTESIAN_POINT('Ctrl Pts',(-20.8472694739559,12.1426194691851,123.198544107178)) ;
#71548 = CARTESIAN_POINT('Ctrl Pts',(-20.8615954260223,12.1516978160533,123.188454929207)) ;
#71549 = CARTESIAN_POINT('Ctrl Pts',(-20.8755851620327,12.1606452915608,123.177914421792)) ;
#71550 = CARTESIAN_POINT('Ctrl Pts',(-20.8890752031254,12.1693713464509,123.166987767337)) ;
#71551 = CARTESIAN_POINT('',(-18.3268339991922,12.1788250889762,124.036972600407)) ;
#71552 = CARTESIAN_POINT('Ctrl Pts',(-18.1733332732719,12.2002112739617,123.598774336477)) ;
#71553 = CARTESIAN_POINT('Ctrl Pts',(-18.1437739434563,12.2192124780422,123.626890688012)) ;
#71554 = CARTESIAN_POINT('Ctrl Pts',(-18.1155519840929,12.2380735843825,123.659034167815)) ;
#71555 = CARTESIAN_POINT('Ctrl Pts',(-18.0788950768115,12.264782265653,123.716747867416)) ;
#71556 = CARTESIAN_POINT('Ctrl Pts',(-18.0663998540908,12.2745789428676,123.741420731664)) ;
#71557 = CARTESIAN_POINT('Ctrl Pts',(-18.0527323281464,12.2874752510621,123.784178421799)) ;
#71558 = CARTESIAN_POINT('Ctrl Pts',(-18.049031605284,12.2917819347337,123.8016488575)) ;
#71559 = CARTESIAN_POINT('Ctrl Pts',(-18.0469608922576,12.2970228146757,123.831943690158)) ;
#71560 = CARTESIAN_POINT('Ctrl Pts',(-18.0473135809881,12.2985681111668,123.844453983307)) ;
#71561 = CARTESIAN_POINT('Ctrl Pts',(-18.0497385762831,12.2996578525868,123.861380043343)) ;
#71562 = CARTESIAN_POINT('Ctrl Pts',(-18.0505576652496,12.2998485070101,123.865811638863)) ;
#71563 = CARTESIAN_POINT('Ctrl Pts',(-18.0527703707483,12.3000477727242,123.875497560335)) ;
#71564 = CARTESIAN_POINT('Ctrl Pts',(-18.0542408074423,12.300011368751,123.880712238468)) ;
#71565 = CARTESIAN_POINT('Ctrl Pts',(-18.0561492734575,12.2998090598907,123.886360179938)) ;
#71566 = CARTESIAN_POINT('Ctrl Pts',(-18.0563249547583,12.2997892478978,123.886871506831)) ;
#71567 = CARTESIAN_POINT('Ctrl Pts',(-18.0565108989679,12.2997670567988,123.887403881291)) ;
#71568 = CARTESIAN_POINT('Ctrl Pts',(-18.0565185857082,12.2997661372984,123.887425873618)) ;
#71569 = CARTESIAN_POINT('Ctrl Pts',(-18.0565331994726,12.2997643851054,123.887467655272)) ;
#71570 = CARTESIAN_POINT('Ctrl Pts',(-18.0565401250457,12.2997635529941,123.887487443392)) ;
#71571 = CARTESIAN_POINT('Ctrl Pts',(-18.0565502565831,12.2997623331508,123.887516373468)) ;
#71572 = CARTESIAN_POINT('Ctrl Pts',(-18.0565534594976,12.2997619471482,123.887525516553)) ;
#71573 = CARTESIAN_POINT('Ctrl Pts',(-18.0565590575015,12.2997612718528,123.887541492028)) ;
#71574 = CARTESIAN_POINT('Ctrl Pts',(-18.0565614522309,12.2997609827666,123.88754832457)) ;
#71575 = CARTESIAN_POINT('Ctrl Pts',(-18.0565663690132,12.2997603888004,123.887562349868)) ;
#71576 = CARTESIAN_POINT('Ctrl Pts',(-18.0565688910754,12.2997600838969,123.887569542489)) ;
#71577 = CARTESIAN_POINT('Ctrl Pts',(-18.0565752815213,12.2997593107477,123.887587763097)) ;
#71578 = CARTESIAN_POINT('Ctrl Pts',(-18.0565791506111,12.2997588421077,123.887598790867)) ;
#71579 = CARTESIAN_POINT('Ctrl Pts',(-18.0565942212527,12.2997570145979,123.887641730451)) ;
#71580 = CARTESIAN_POINT('Ctrl Pts',(-18.0566054316885,12.2997556506893,123.887673638972)) ;
#71581 = CARTESIAN_POINT('Ctrl Pts',(-18.0590015798815,12.2994631655,123.894486919769)) ;
#71582 = CARTESIAN_POINT('Ctrl Pts',(-18.061830203414,12.298915038444,123.901065001398)) ;
#71583 = CARTESIAN_POINT('Ctrl Pts',(-18.0701064049968,12.2968881910932,123.917270600894)) ;
#71584 = CARTESIAN_POINT('Ctrl Pts',(-18.0760644154365,12.2950839853311,123.926456828537)) ;
#71585 = CARTESIAN_POINT('Ctrl Pts',(-18.0926654304272,12.2894248879463,123.947565980743)) ;
#71586 = CARTESIAN_POINT('Ctrl Pts',(-18.1040515527384,12.285054139982,123.958571881896)) ;
#71587 = CARTESIAN_POINT('Ctrl Pts',(-18.1349180947271,12.2723955189041,123.982828648664)) ;
#71588 = CARTESIAN_POINT('Ctrl Pts',(-18.155694410254,12.26318030131,123.994378655851)) ;
#71589 = CARTESIAN_POINT('Ctrl Pts',(-18.2194310980166,12.2336621656688,124.021802848732)) ;
#71590 = CARTESIAN_POINT('Ctrl Pts',(-18.2704827038226,12.2083681409552,124.033080779891)) ;
#71591 = CARTESIAN_POINT('Ctrl Pts',(-18.3268339991922,12.1788250889762,124.036972600407)) ;
#71592 = CARTESIAN_POINT('Ctrl Pts',(-18.3268329934248,12.1788261493768,124.036974575079)) ;
#71593 = CARTESIAN_POINT('Ctrl Pts',(-18.3309561086821,12.1784521366068,124.044113579922)) ;
#71594 = CARTESIAN_POINT('Ctrl Pts',(-18.335149729096,12.1780774444603,124.051211586361)) ;
#71595 = CARTESIAN_POINT('Ctrl Pts',(-18.3423169557771,12.1774461337977,124.063073113184)) ;
#71596 = CARTESIAN_POINT('Ctrl Pts',(-18.3452530035821,12.1771899809839,124.06785902791)) ;
#71597 = CARTESIAN_POINT('Ctrl Pts',(-18.3498365787837,12.1767937826142,124.075218787483)) ;
#71598 = CARTESIAN_POINT('Ctrl Pts',(-18.3514614724111,12.1766540296321,124.077806653189)) ;
#71599 = CARTESIAN_POINT('Ctrl Pts',(-18.3547371233891,12.1763736859824,124.082981345011)) ;
#71600 = CARTESIAN_POINT('Ctrl Pts',(-18.3563879496659,12.1762330952556,124.085568102145)) ;
#71601 = CARTESIAN_POINT('Ctrl Pts',(-18.359959596429,12.1759303975391,124.091119499098)) ;
#71602 = CARTESIAN_POINT('Ctrl Pts',(-18.3618834914386,12.175768251981,124.094082126548)) ;
#71603 = CARTESIAN_POINT('Ctrl Pts',(-18.3670623375374,12.1753341801676,124.101983558783)) ;
#71604 = CARTESIAN_POINT('Ctrl Pts',(-18.3703398205182,12.175061972512,124.106907469637)) ;
#71605 = CARTESIAN_POINT('Ctrl Pts',(-18.3847847100382,12.1738731097679,124.128278263932)) ;
#71606 = CARTESIAN_POINT('Ctrl Pts',(-18.3963085270288,12.1729521993781,124.144480537417)) ;
#71607 = CARTESIAN_POINT('Ctrl Pts',(-18.4232925461838,12.1708620966218,124.18056531699)) ;
#71608 = CARTESIAN_POINT('Ctrl Pts',(-18.4389773134463,12.1696945627848,124.200269661361)) ;
#71609 = CARTESIAN_POINT('Ctrl Pts',(-18.4678172941385,12.1676312235368,124.23433555177)) ;
#71610 = CARTESIAN_POINT('Ctrl Pts',(-18.4807330953577,12.1667338677983,124.248888783628)) ;
#71611 = CARTESIAN_POINT('Ctrl Pts',(-18.4982848415437,12.1655482404027,124.267759375193)) ;
#71612 = CARTESIAN_POINT('Ctrl Pts',(-18.5026213166717,12.1652579317476,124.272351409021)) ;
#71613 = CARTESIAN_POINT('Ctrl Pts',(-18.5107463421741,12.1647187963383,124.280825666637)) ;
#71614 = CARTESIAN_POINT('Ctrl Pts',(-18.5145257195718,12.1644699057803,124.284716476236)) ;
#71615 = CARTESIAN_POINT('Ctrl Pts',(-18.5222714957369,12.1639636048236,124.292587469649)) ;
#71616 = CARTESIAN_POINT('Ctrl Pts',(-18.526239649542,12.1637062151148,124.296565757538)) ;
#71617 = CARTESIAN_POINT('Ctrl Pts',(-18.5354269798619,12.1631147968241,124.305653171346)) ;
#71618 = CARTESIAN_POINT('Ctrl Pts',(-18.5406643862709,12.1627809370258,124.310743587654)) ;
#71619 = CARTESIAN_POINT('Ctrl Pts',(-18.5568490594105,12.1617591296451,124.326200513915)) ;
#71620 = CARTESIAN_POINT('Ctrl Pts',(-18.5679395411594,12.1610726680707,124.336415145548)) ;
#71621 = CARTESIAN_POINT('Ctrl Pts',(-18.5833701166089,12.160135177217,124.350119548717)) ;
#71622 = CARTESIAN_POINT('Ctrl Pts',(-18.5875526761695,12.1598827561002,124.353784584154)) ;
#71623 = CARTESIAN_POINT('Ctrl Pts',(-18.5987779267441,12.1592095596942,124.363489231507)) ;
#71624 = CARTESIAN_POINT('Ctrl Pts',(-18.605863636986,12.1587890311453,124.369478554744)) ;
#71625 = CARTESIAN_POINT('Ctrl Pts',(-18.6339450219884,12.1571381352803,124.392683823556)) ;
#71626 = CARTESIAN_POINT('Ctrl Pts',(-18.6554325503652,12.1559086064401,124.409292637778)) ;
#71627 = CARTESIAN_POINT('Ctrl Pts',(-18.6866563009285,12.1541580311278,124.431841495251)) ;
#71628 = CARTESIAN_POINT('Ctrl Pts',(-18.6959590741923,12.1536408492618,124.438368536798)) ;
#71629 = CARTESIAN_POINT('Ctrl Pts',(-18.7110045839349,12.1528107345973,124.448621541144)) ;
#71630 = CARTESIAN_POINT('Ctrl Pts',(-18.7166911876344,12.1524984057569,124.452428763065)) ;
#71631 = CARTESIAN_POINT('Ctrl Pts',(-18.7276119130962,12.1519011693592,124.459611096525)) ;
#71632 = CARTESIAN_POINT('Ctrl Pts',(-18.7328405599809,12.1516163314452,124.462994165875)) ;
#71633 = CARTESIAN_POINT('Ctrl Pts',(-18.7416520111582,12.1511380934684,124.468602434594)) ;
#71634 = CARTESIAN_POINT('Ctrl Pts',(-18.745221195541,12.150944861499,124.470848832909)) ;
#71635 = CARTESIAN_POINT('Ctrl Pts',(-18.7531205419484,12.150518239497,124.475764944144)) ;
#71636 = CARTESIAN_POINT('Ctrl Pts',(-18.7574557686962,12.1502847897276,124.478426371889)) ;
#71637 = CARTESIAN_POINT('Ctrl Pts',(-18.769540168913,12.1496358997812,124.485743884565)) ;
#71638 = CARTESIAN_POINT('Ctrl Pts',(-18.7773237713421,12.1492200402206,124.490342467398)) ;
#71639 = CARTESIAN_POINT('Ctrl Pts',(-18.8214619475145,12.1468732364854,124.515777614443)) ;
#71640 = CARTESIAN_POINT('Ctrl Pts',(-18.8587960674524,12.1449299126189,124.53486009634)) ;
#71641 = CARTESIAN_POINT('Ctrl Pts',(-18.9139729955992,12.1421242821054,124.559648928632)) ;
#71642 = CARTESIAN_POINT('Ctrl Pts',(-18.9310965056275,12.1412627503848,124.566887306796)) ;
#71643 = CARTESIAN_POINT('Ctrl Pts',(-18.9564533001242,12.1400023439097,124.576945490497)) ;
#71644 = CARTESIAN_POINT('Ctrl Pts',(-18.9645646880267,12.1396013872073,124.580065504982)) ;
#71645 = CARTESIAN_POINT('Ctrl Pts',(-18.9791159272324,12.1388860855064,124.585489072915)) ;
#71646 = CARTESIAN_POINT('Ctrl Pts',(-18.9855433853753,12.1385715029736,124.587824837599)) ;
#71647 = CARTESIAN_POINT('Ctrl Pts',(-18.995936113443,12.1380650310906,124.591505333423)) ;
#71648 = CARTESIAN_POINT('Ctrl Pts',(-18.9998895246317,12.1378728744833,124.592883087366)) ;
#71649 = CARTESIAN_POINT('Ctrl Pts',(-19.0076657347591,12.1374958891479,124.595549341794)) ;
#71650 = CARTESIAN_POINT('Ctrl Pts',(-19.0114879973792,12.1373110507774,124.596839249442)) ;
#71651 = CARTESIAN_POINT('Ctrl Pts',(-19.0203630306894,12.1368829207235,124.599786549263)) ;
#71652 = CARTESIAN_POINT('Ctrl Pts',(-19.0254202715219,12.1366397478072,124.601430248465)) ;
#71653 = CARTESIAN_POINT('Ctrl Pts',(-19.0407068717453,12.1359070071212,124.606291055064)) ;
#71654 = CARTESIAN_POINT('Ctrl Pts',(-19.0509673168084,12.1354182904964,124.609408861383)) ;
#71655 = CARTESIAN_POINT('Ctrl Pts',(-19.0983481678484,12.1331745141152,124.62314289154)) ;
#71656 = CARTESIAN_POINT('Ctrl Pts',(-19.135907308955,12.1314352924154,124.63216766381)) ;
#71657 = CARTESIAN_POINT('Ctrl Pts',(-19.185832039001,12.12913802557,124.641742810519)) ;
#71658 = CARTESIAN_POINT('Ctrl Pts',(-19.1978732237918,12.1285845297001,124.643869541303)) ;
#71659 = CARTESIAN_POINT('Ctrl Pts',(-19.2155834909889,12.1277695243768,124.646730277972)) ;
#71660 = CARTESIAN_POINT('Ctrl Pts',(-19.2212295206173,12.1275095723486,124.64760260689)) ;
#71661 = CARTESIAN_POINT('Ctrl Pts',(-19.2303371967085,12.1270899040682,124.648945909585)) ;
#71662 = CARTESIAN_POINT('Ctrl Pts',(-19.2337951920354,12.1269304872354,124.649441131769)) ;
#71663 = CARTESIAN_POINT('Ctrl Pts',(-19.2404037493357,12.1266256527697,124.650359294679)) ;
#71664 = CARTESIAN_POINT('Ctrl Pts',(-19.243553938108,12.1264802680291,124.650784725532)) ;
#71665 = CARTESIAN_POINT('Ctrl Pts',(-19.2491898898548,12.1262200146339,124.651523977672)) ;
#71666 = CARTESIAN_POINT('Ctrl Pts',(-19.2516750402328,12.1261052056308,124.651842350628)) ;
#71667 = CARTESIAN_POINT('Ctrl Pts',(-19.2567554186499,12.1258703922224,124.652477679522)) ;
#71668 = CARTESIAN_POINT('Ctrl Pts',(-19.259350716869,12.1257503797777,124.652793969034)) ;
#71669 = CARTESIAN_POINT('Ctrl Pts',(-19.2666646898003,12.1254119951527,124.653662045682)) ;
#71670 = CARTESIAN_POINT('Ctrl Pts',(-19.2713855323837,12.1251933830539,124.654195075941)) ;
#71671 = CARTESIAN_POINT('Ctrl Pts',(-19.2980125716004,12.123959212496,124.657047898168)) ;
#71672 = CARTESIAN_POINT('Ctrl Pts',(-19.3199737148664,12.1229365148661,124.65881517204)) ;
#71673 = CARTESIAN_POINT('Ctrl Pts',(-19.3583755690349,12.1211461929445,124.66088580607)) ;
#71674 = CARTESIAN_POINT('Ctrl Pts',(-19.3747972379329,12.1203803250949,124.661446876312)) ;
#71675 = CARTESIAN_POINT('Ctrl Pts',(-19.4025984884849,12.1190879848973,124.661848301862)) ;
#71676 = CARTESIAN_POINT('Ctrl Pts',(-19.4139735268802,12.1185603883619,124.661857277545)) ;
#71677 = CARTESIAN_POINT('Ctrl Pts',(-19.4308582588047,12.1177796885816,124.661640122708)) ;
#71678 = CARTESIAN_POINT('Ctrl Pts',(-19.4363688273304,12.1175252776935,124.661532795761)) ;
#71679 = CARTESIAN_POINT('Ctrl Pts',(-19.4463925817608,12.1170632365372,124.661271236795)) ;
#71680 = CARTESIAN_POINT('Ctrl Pts',(-19.4509059776786,12.1168554636031,124.661128987644)) ;
#71681 = CARTESIAN_POINT('Ctrl Pts',(-19.4581089955715,12.1165243081718,124.660862892255)) ;
#71682 = CARTESIAN_POINT('Ctrl Pts',(-19.4607991489641,12.1164007259829,124.660754807863)) ;
#71683 = CARTESIAN_POINT('Ctrl Pts',(-19.4660166369468,12.1161612255412,124.660528294707)) ;
#71684 = CARTESIAN_POINT('Ctrl Pts',(-19.4685440016305,12.1160452947918,124.660410882346)) ;
#71685 = CARTESIAN_POINT('Ctrl Pts',(-19.4744209069952,12.1157759099962,124.660119978235)) ;
#71686 = CARTESIAN_POINT('Ctrl Pts',(-19.4777701431751,12.1156225319265,124.659940676791)) ;
#71687 = CARTESIAN_POINT('Ctrl Pts',(-19.4879808771949,12.1151553471206,124.659352821464)) ;
#71688 = CARTESIAN_POINT('Ctrl Pts',(-19.4948397796812,12.1148420982047,124.658901149022)) ;
#71689 = CARTESIAN_POINT('Ctrl Pts',(-19.5395975418219,12.1128010645601,124.655582770018)) ;
#71690 = CARTESIAN_POINT('Ctrl Pts',(-19.5773517629285,12.1110970236261,124.651045488828)) ;
#71691 = CARTESIAN_POINT('Ctrl Pts',(-19.6243814208216,12.1089411400518,124.643204471514)) ;
#71692 = CARTESIAN_POINT('Ctrl Pts',(-19.6339031091612,12.1085028465813,124.641503156803)) ;
#71693 = CARTESIAN_POINT('Ctrl Pts',(-19.6482180187781,12.1078404098274,124.638773587489)) ;
#71694 = CARTESIAN_POINT('Ctrl Pts',(-19.6530265275211,12.1076172964537,124.637827360772)) ;
#71695 = CARTESIAN_POINT('Ctrl Pts',(-19.6609096731925,12.1072504731384,124.636227891222)) ;
#71696 = CARTESIAN_POINT('Ctrl Pts',(-19.6639876373078,12.1071069848894,124.635591283902)) ;
#71697 = CARTESIAN_POINT('Ctrl Pts',(-19.6696692547856,12.1068416198828,124.634393806143)) ;
#71698 = CARTESIAN_POINT('Ctrl Pts',(-19.6722735808662,12.1067197881108,124.633836210074)) ;
#71699 = CARTESIAN_POINT('Ctrl Pts',(-19.6772531681451,12.1064864619113,124.632753405863)) ;
#71700 = CARTESIAN_POINT('Ctrl Pts',(-19.679628717628,12.1063749867977,124.632229578891)) ;
#71701 = CARTESIAN_POINT('Ctrl Pts',(-19.684523120746,12.1061449682624,124.631135333513)) ;
#71702 = CARTESIAN_POINT('Ctrl Pts',(-19.6870417652005,12.1060264134561,124.630564036756)) ;
#71703 = CARTESIAN_POINT('Ctrl Pts',(-19.6942618608993,12.1056860159488,124.628902779674)) ;
#71704 = CARTESIAN_POINT('Ctrl Pts',(-19.698958780763,12.1054639154586,124.627793394794)) ;
#71705 = CARTESIAN_POINT('Ctrl Pts',(-19.7311424377226,12.103937583566,124.619994749598)) ;
#71706 = CARTESIAN_POINT('Ctrl Pts',(-19.7584012552096,12.1026208615476,124.612401345337)) ;
#71707 = CARTESIAN_POINT('Ctrl Pts',(-19.8078142985598,12.100211998718,124.596811287358)) ;
#71708 = CARTESIAN_POINT('Ctrl Pts',(-19.830046894039,12.0991213656254,124.589100324975)) ;
#71709 = CARTESIAN_POINT('Ctrl Pts',(-19.8577117655564,12.0977581546964,124.578621401988)) ;
#71710 = CARTESIAN_POINT('Ctrl Pts',(-19.863359027879,12.0974795315819,124.576435272909)) ;
#71711 = CARTESIAN_POINT('Ctrl Pts',(-19.872219293051,12.0970418066097,124.572931105043)) ;
#71712 = CARTESIAN_POINT('Ctrl Pts',(-19.8754430554125,12.0968824207354,124.571640571314)) ;
#71713 = CARTESIAN_POINT('Ctrl Pts',(-19.8819030589345,12.0965627736227,124.569023223501)) ;
#71714 = CARTESIAN_POINT('Ctrl Pts',(-19.885139192205,12.0964025158514,124.567696226204)) ;
#71715 = CARTESIAN_POINT('Ctrl Pts',(-19.8883899053704,12.0962413949055,124.56634728485)) ;
#71716 = CARTESIAN_POINT('Ctrl Pts',(-19.8884100912478,12.096240394391,124.56633890774)) ;
#71717 = CARTESIAN_POINT('Ctrl Pts',(-19.8884505059743,12.0962383912212,124.566322134444)) ;
#71718 = CARTESIAN_POINT('Ctrl Pts',(-19.8884707355008,12.0962373885322,124.566313737975)) ;
#71719 = CARTESIAN_POINT('Ctrl Pts',(-19.8885112400915,12.0962353808862,124.566296924886)) ;
#71720 = CARTESIAN_POINT('Ctrl Pts',(-19.8885315141901,12.0962343759769,124.566288508666)) ;
#71721 = CARTESIAN_POINT('Ctrl Pts',(-19.8885721091959,12.096232363827,124.56627165554)) ;
#71722 = CARTESIAN_POINT('Ctrl Pts',(-19.8885924305321,12.0962313565652,124.566263218454)) ;
#71723 = CARTESIAN_POINT('Ctrl Pts',(-19.8886331225267,12.0962293395857,124.566246322543)) ;
#71724 = CARTESIAN_POINT('Ctrl Pts',(-19.8886534916079,12.0962283299461,124.566237864371)) ;
#71725 = CARTESIAN_POINT('Ctrl Pts',(-19.8886942795243,12.0962263081895,124.566220926102)) ;
#71726 = CARTESIAN_POINT('Ctrl Pts',(-19.8887146995792,12.0962252960121,124.566212445494)) ;
#71727 = CARTESIAN_POINT('Ctrl Pts',(-19.8887555907354,12.0962232691156,124.566195461807)) ;
#71728 = CARTESIAN_POINT('Ctrl Pts',(-19.8887760621694,12.0962222543801,124.566186958586)) ;
#71729 = CARTESIAN_POINT('Ctrl Pts',(-19.8888170578738,12.0962202222786,124.566169928919)) ;
#71730 = CARTESIAN_POINT('Ctrl Pts',(-19.8888375826562,12.0962192048873,124.566161402256)) ;
#71731 = CARTESIAN_POINT('Ctrl Pts',(-19.8888786872779,12.0962171673641,124.566144324774)) ;
#71732 = CARTESIAN_POINT('Ctrl Pts',(-19.8888992666296,12.0962161472564,124.566135774153)) ;
#71733 = CARTESIAN_POINT('Ctrl Pts',(-19.8889404823842,12.0962141042014,124.566118647913)) ;
#71734 = CARTESIAN_POINT('Ctrl Pts',(-19.8889611182149,12.0962130812825,124.566110072529)) ;
#71735 = CARTESIAN_POINT('Ctrl Pts',(-19.8890024476845,12.0962110325677,124.566092896439)) ;
#71736 = CARTESIAN_POINT('Ctrl Pts',(-19.8890231420417,12.096210006736,124.566084295431)) ;
#71737 = CARTESIAN_POINT('Ctrl Pts',(-19.8890645907982,12.0962079520848,124.566067067152)) ;
#71738 = CARTESIAN_POINT('Ctrl Pts',(-19.8890853443253,12.0962069233084,124.56605844024)) ;
#71739 = CARTESIAN_POINT('Ctrl Pts',(-19.8891269129884,12.0962048626899,124.566041159492)) ;
#71740 = CARTESIAN_POINT('Ctrl Pts',(-19.8891477280691,12.0962038308505,124.566032505674)) ;
#71741 = CARTESIAN_POINT('Ctrl Pts',(-19.8891894207076,12.0962017640628,124.566015170742)) ;
#71742 = CARTESIAN_POINT('Ctrl Pts',(-19.8892102988711,12.0962007290844,124.566006489371)) ;
#71743 = CARTESIAN_POINT('Ctrl Pts',(-19.889252119754,12.0961986559157,124.565989098456)) ;
#71744 = CARTESIAN_POINT('Ctrl Pts',(-19.8892730620161,12.0961976177479,124.565980389097)) ;
#71745 = CARTESIAN_POINT('Ctrl Pts',(-19.8893150125022,12.0961955381305,124.565962941608)) ;
#71746 = CARTESIAN_POINT('Ctrl Pts',(-19.8893360210389,12.0961944966653,124.565954203344)) ;
#71747 = CARTESIAN_POINT('Ctrl Pts',(-19.8893781051252,12.0961924104008,124.565936697595)) ;
#71748 = CARTESIAN_POINT('Ctrl Pts',(-19.8893991813962,12.0961913655658,124.565927929805)) ;
#71749 = CARTESIAN_POINT('Ctrl Pts',(-19.8894414030598,12.0961892724569,124.565910364114)) ;
#71750 = CARTESIAN_POINT('Ctrl Pts',(-19.8894625481686,12.0961882241971,124.565901566326)) ;
#71751 = CARTESIAN_POINT('Ctrl Pts',(-19.8895049100727,12.0961861241116,124.565883939559)) ;
#71752 = CARTESIAN_POINT('Ctrl Pts',(-19.8895261255919,12.096185072349,124.565875111105)) ;
#71753 = CARTESIAN_POINT('Ctrl Pts',(-19.8895686279618,12.0961829652752,124.56585742314)) ;
#71754 = CARTESIAN_POINT('Ctrl Pts',(-19.8895899168957,12.0961819098608,124.565848562757)) ;
#71755 = CARTESIAN_POINT('Ctrl Pts',(-19.8896325689494,12.0961797953417,124.565830809729)) ;
#71756 = CARTESIAN_POINT('Ctrl Pts',(-19.8896539305731,12.0961787363111,124.565821917703)) ;
#71757 = CARTESIAN_POINT('Ctrl Pts',(-19.8896967300142,12.0961766144602,124.56580410054)) ;
#71758 = CARTESIAN_POINT('Ctrl Pts',(-19.8897181674514,12.0961755516586,124.565795175556)) ;
#71759 = CARTESIAN_POINT('Ctrl Pts',(-19.8897611191027,12.0961734222365,124.56577729222)) ;
#71760 = CARTESIAN_POINT('Ctrl Pts',(-19.8897826338468,12.0961723555896,124.565768333642)) ;
#71761 = CARTESIAN_POINT('Ctrl Pts',(-19.8898257416592,12.0961702184002,124.565750382458)) ;
#71762 = CARTESIAN_POINT('Ctrl Pts',(-19.8898473348348,12.0961691478522,124.565741389802)) ;
#71763 = CARTESIAN_POINT('Ctrl Pts',(-19.8898906012064,12.0961670027762,124.565723369739)) ;
#71764 = CARTESIAN_POINT('Ctrl Pts',(-19.8899122745324,12.0961659282417,124.565714342273)) ;
#71765 = CARTESIAN_POINT('Ctrl Pts',(-19.8899557030499,12.096163775101,124.565696251807)) ;
#71766 = CARTESIAN_POINT('Ctrl Pts',(-19.8899774579468,12.0961626965094,124.565687188923)) ;
#71767 = CARTESIAN_POINT('Ctrl Pts',(-19.8900132216144,12.0961609233627,124.565672288932)) ;
#71768 = CARTESIAN_POINT('Ctrl Pts',(-19.8900272315851,12.0961602287519,124.565666451747)) ;
#71769 = CARTESIAN_POINT('Ctrl Pts',(-19.8900553823775,12.0961588330374,124.565654722257)) ;
#71770 = CARTESIAN_POINT('Ctrl Pts',(-19.8900695230093,12.096158131943,124.565648830025)) ;
#71771 = CARTESIAN_POINT('Ctrl Pts',(-19.8900979393219,12.096156723053,124.565636988675)) ;
#71772 = CARTESIAN_POINT('Ctrl Pts',(-19.890112213525,12.0961560153306,124.565631040167)) ;
#71773 = CARTESIAN_POINT('Ctrl Pts',(-19.8901408985717,12.0961545931055,124.565619085583)) ;
#71774 = CARTESIAN_POINT('Ctrl Pts',(-19.8901553106431,12.0961538785419,124.56561307899)) ;
#71775 = CARTESIAN_POINT('Ctrl Pts',(-19.8901842732507,12.0961524425436,124.565601007459)) ;
#71776 = CARTESIAN_POINT('Ctrl Pts',(-19.8901988254819,12.096151721025,124.565594941808)) ;
#71777 = CARTESIAN_POINT('Ctrl Pts',(-19.8902280740247,12.0961502708381,124.5655827498)) ;
#71778 = CARTESIAN_POINT('Ctrl Pts',(-19.890242768038,12.0961495422838,124.565576624395)) ;
#71779 = CARTESIAN_POINT('Ctrl Pts',(-19.8902723027371,12.0961480778969,124.565564311781)) ;
#71780 = CARTESIAN_POINT('Ctrl Pts',(-19.8902871439326,12.0961473420391,124.565558124353)) ;
#71781 = CARTESIAN_POINT('Ctrl Pts',(-19.8903169751637,12.0961458629374,124.565545686767)) ;
#71782 = CARTESIAN_POINT('Ctrl Pts',(-19.890331965887,12.0961451196595,124.565539436317)) ;
#71783 = CARTESIAN_POINT('Ctrl Pts',(-19.8903621001897,12.0961436255185,124.565526870992)) ;
#71784 = CARTESIAN_POINT('Ctrl Pts',(-19.8903772432713,12.0961428746801,124.565520556319)) ;
#71785 = CARTESIAN_POINT('Ctrl Pts',(-19.8904076862415,12.0961413652218,124.56550786088)) ;
#71786 = CARTESIAN_POINT('Ctrl Pts',(-19.8904229853098,12.0961406066427,124.565501480449)) ;
#71787 = CARTESIAN_POINT('Ctrl Pts',(-19.8904537435082,12.0961390815415,124.565488652116)) ;
#71788 = CARTESIAN_POINT('Ctrl Pts',(-19.8904692022185,12.0961383150403,124.565482204381)) ;
#71789 = CARTESIAN_POINT('Ctrl Pts',(-19.8905002824576,12.096136773958,124.565469240268)) ;
#71790 = CARTESIAN_POINT('Ctrl Pts',(-19.8905159044465,12.0961359993541,124.565462723689)) ;
#71791 = CARTESIAN_POINT('Ctrl Pts',(-19.8905473146054,12.0961344418996,124.565449620462)) ;
#71792 = CARTESIAN_POINT('Ctrl Pts',(-19.8905631030922,12.0961336590332,124.565443033674)) ;
#71793 = CARTESIAN_POINT('Ctrl Pts',(-19.8905948499206,12.0961320848713,124.56542978847)) ;
#71794 = CARTESIAN_POINT('Ctrl Pts',(-19.8906108085725,12.0961312935604,124.565423129917)) ;
#71795 = CARTESIAN_POINT('Ctrl Pts',(-19.8906428998161,12.0961297023067,124.565409739454)) ;
#71796 = CARTESIAN_POINT('Ctrl Pts',(-19.8906590321436,12.0961289023769,124.565403007647)) ;
#71797 = CARTESIAN_POINT('Ctrl Pts',(-19.8906914750132,12.0961272936733,124.565389468866)) ;
#71798 = CARTESIAN_POINT('Ctrl Pts',(-19.8907077848372,12.096126484935,124.565382662184)) ;
#71799 = CARTESIAN_POINT('Ctrl Pts',(-19.8907405852627,12.096124858487,124.565368972558)) ;
#71800 = CARTESIAN_POINT('Ctrl Pts',(-19.8907570772909,12.0961240407065,124.565362089009)) ;
#71801 = CARTESIAN_POINT('Ctrl Pts',(-19.8907902471995,12.0961223959221,124.565348243504)) ;
#71802 = CARTESIAN_POINT('Ctrl Pts',(-19.8908069237545,12.0961215689839,124.565341282092)) ;
#71803 = CARTESIAN_POINT('Ctrl Pts',(-19.8908404664989,12.0961199056965,124.565327279253)) ;
#71804 = CARTESIAN_POINT('Ctrl Pts',(-19.8908573330806,12.0961190693277,124.565320237652)) ;
#71805 = CARTESIAN_POINT('Ctrl Pts',(-19.8908912602615,12.0961173869614,124.565306072578)) ;
#71806 = CARTESIAN_POINT('Ctrl Pts',(-19.8909083199804,12.0961165410075,124.565298949461)) ;
#71807 = CARTESIAN_POINT('Ctrl Pts',(-19.8909426362466,12.0961148393312,124.56528462015)) ;
#71808 = CARTESIAN_POINT('Ctrl Pts',(-19.8909598946158,12.0961139835185,124.565277413184)) ;
#71809 = CARTESIAN_POINT('Ctrl Pts',(-19.8909946128312,12.0961122618939,124.565262914202)) ;
#71810 = CARTESIAN_POINT('Ctrl Pts',(-19.8910120725937,12.096111396086,124.565255622211)) ;
#71811 = CARTESIAN_POINT('Ctrl Pts',(-19.8932200461518,12.0960019048985,124.564333413046)) ;
#71812 = CARTESIAN_POINT('Ctrl Pts',(-19.8954079518662,12.095893342643,124.563412256993)) ;
#71813 = CARTESIAN_POINT('Ctrl Pts',(-19.9018327066309,12.0955743452035,124.560685722707)) ;
#71814 = CARTESIAN_POINT('Ctrl Pts',(-19.9060622234605,12.095364080751,124.558863153119)) ;
#71815 = CARTESIAN_POINT('Ctrl Pts',(-19.9172083501097,12.0948091825736,124.553986887343)) ;
#71816 = CARTESIAN_POINT('Ctrl Pts',(-19.9241075017011,12.0944649162962,124.55089373742)) ;
#71817 = CARTESIAN_POINT('Ctrl Pts',(-19.947189550004,12.0933098005277,124.540292637351)) ;
#71818 = CARTESIAN_POINT('Ctrl Pts',(-19.9632397016889,12.0925011604031,124.532500894411)) ;
#71819 = CARTESIAN_POINT('Ctrl Pts',(-19.9997021501647,12.0906432498922,124.513824984359)) ;
#71820 = CARTESIAN_POINT('Ctrl Pts',(-20.0199899485757,12.0895932315963,124.502712505895)) ;
#71821 = CARTESIAN_POINT('Ctrl Pts',(-20.0451574487418,12.0882630667123,124.488004994032)) ;
#71822 = CARTESIAN_POINT('Ctrl Pts',(-20.0503351268551,12.0879879339241,124.484928824601)) ;
#71823 = CARTESIAN_POINT('Ctrl Pts',(-20.0592641580973,12.087510822128,124.479536211108)) ;
#71824 = CARTESIAN_POINT('Ctrl Pts',(-20.0630258648687,12.0873090005106,124.47723711304)) ;
#71825 = CARTESIAN_POINT('Ctrl Pts',(-20.0707724660396,12.0868916700692,124.472446034137)) ;
#71826 = CARTESIAN_POINT('Ctrl Pts',(-20.0747556264624,12.0866761410594,124.469951382956)) ;
#71827 = CARTESIAN_POINT('Ctrl Pts',(-20.0829831587476,12.0862289818328,124.464733651904)) ;
#71828 = CARTESIAN_POINT('Ctrl Pts',(-20.0872253118421,12.0859973280671,124.462007232492)) ;
#71829 = CARTESIAN_POINT('Ctrl Pts',(-20.0977563432511,12.0854195367764,124.455148569015)) ;
#71830 = CARTESIAN_POINT('Ctrl Pts',(-20.1040246172856,12.0850731844949,124.450985070618)) ;
#71831 = CARTESIAN_POINT('Ctrl Pts',(-20.1253685275516,12.083885700615,124.436528624841)) ;
#71832 = CARTESIAN_POINT('Ctrl Pts',(-20.1402560706855,12.0830432374429,124.425962206619)) ;
#71833 = CARTESIAN_POINT('Ctrl Pts',(-20.1608000932679,12.0818640137746,124.410693635432)) ;
#71834 = CARTESIAN_POINT('Ctrl Pts',(-20.1666546517558,12.0815260381859,124.406261847004)) ;
#71835 = CARTESIAN_POINT('Ctrl Pts',(-20.1766176495245,12.0809479577298,124.398581028828)) ;
#71836 = CARTESIAN_POINT('Ctrl Pts',(-20.1807453202545,12.0807075591967,124.395357304067)) ;
#71837 = CARTESIAN_POINT('Ctrl Pts',(-20.1890187257961,12.0802237303642,124.388811619601)) ;
#71838 = CARTESIAN_POINT('Ctrl Pts',(-20.1931637870648,12.0799803109458,124.385488982202)) ;
#71839 = CARTESIAN_POINT('Ctrl Pts',(-20.1980454916039,12.0796923303333,124.381524480264)) ;
#71840 = CARTESIAN_POINT('Ctrl Pts',(-20.1988027142953,12.0796476230646,124.380908055126)) ;
#71841 = CARTESIAN_POINT('Ctrl Pts',(-20.2005462007064,12.0795445984949,124.379485351754)) ;
#71842 = CARTESIAN_POINT('Ctrl Pts',(-20.2015319558203,12.0794862846559,124.378678451714)) ;
#71843 = CARTESIAN_POINT('Ctrl Pts',(-20.2033067724417,12.0793811744691,124.377221120535)) ;
#71844 = CARTESIAN_POINT('Ctrl Pts',(-20.2040962724662,12.0793343755022,124.376571225431)) ;
#71845 = CARTESIAN_POINT('Ctrl Pts',(-20.2070796773395,12.0791573668663,124.374109219249)) ;
#71846 = CARTESIAN_POINT('Ctrl Pts',(-20.2092681907218,12.0790271876121,124.372290586679)) ;
#71847 = CARTESIAN_POINT('Ctrl Pts',(-20.2227467037841,12.0782233181007,124.361012050794)) ;
#71848 = CARTESIAN_POINT('Ctrl Pts',(-20.2338749828313,12.0775503409761,124.351360674119)) ;
#71849 = CARTESIAN_POINT('Ctrl Pts',(-20.2557121074218,12.0762081999463,124.331734804513)) ;
#71850 = CARTESIAN_POINT('Ctrl Pts',(-20.2664215418767,12.075539144723,124.321764438779)) ;
#71851 = CARTESIAN_POINT('Ctrl Pts',(-20.279945206364,12.0746787217884,124.308723421208)) ;
#71852 = CARTESIAN_POINT('Ctrl Pts',(-20.2829225436843,12.0744883010146,124.305823546296)) ;
#71853 = CARTESIAN_POINT('Ctrl Pts',(-20.2911382071323,12.0739600312075,124.297741397543)) ;
#71854 = CARTESIAN_POINT('Ctrl Pts',(-20.296345248864,12.0736220001745,124.292527580215)) ;
#71855 = CARTESIAN_POINT('Ctrl Pts',(-20.3085062999761,12.0728246403682,124.280133436177)) ;
#71856 = CARTESIAN_POINT('Ctrl Pts',(-20.3154208739859,12.0723650571799,124.272915146482)) ;
#71857 = CARTESIAN_POINT('Ctrl Pts',(-20.3298226096132,12.0713941369018,124.257515249955)) ;
#71858 = CARTESIAN_POINT('Ctrl Pts',(-20.337288955113,12.070882556332,124.249315376395)) ;
#71859 = CARTESIAN_POINT('Ctrl Pts',(-20.3604436677817,12.0692712293282,124.223195965355)) ;
#71860 = CARTESIAN_POINT('Ctrl Pts',(-20.3757297246262,12.0681712569354,124.20492667103)) ;
#71861 = CARTESIAN_POINT('Ctrl Pts',(-20.3937476135386,12.0668338044131,124.182097412825)) ;
#71862 = CARTESIAN_POINT('Ctrl Pts',(-20.3969844870212,12.0665918185485,124.177942456214)) ;
#71863 = CARTESIAN_POINT('Ctrl Pts',(-20.4028076011051,12.0661533702789,124.170369472117)) ;
#71864 = CARTESIAN_POINT('Ctrl Pts',(-20.4054027039292,12.0659568257136,124.166958366656)) ;
#71865 = CARTESIAN_POINT('Ctrl Pts',(-20.4104438072535,12.0655727692254,124.160260935774)) ;
#71866 = CARTESIAN_POINT('Ctrl Pts',(-20.412891297502,12.0653852443372,124.156975799786)) ;
#71867 = CARTESIAN_POINT('Ctrl Pts',(-20.4153869236975,12.0651929285345,124.153591453652)) ;
#71868 = CARTESIAN_POINT('Ctrl Pts',(-20.4154512373072,12.0651879716971,124.153504213507)) ;
#71869 = CARTESIAN_POINT('Ctrl Pts',(-20.4155837796079,12.065177754714,124.153324373518)) ;
#71870 = CARTESIAN_POINT('Ctrl Pts',(-20.4156520067771,12.06517249459,124.153231772741)) ;
#71871 = CARTESIAN_POINT('Ctrl Pts',(-20.4157927131427,12.0651616447619,124.15304074495)) ;
#71872 = CARTESIAN_POINT('Ctrl Pts',(-20.4158651907121,12.0651560550728,124.152942316683)) ;
#71873 = CARTESIAN_POINT('Ctrl Pts',(-20.41601476633,12.0651445173581,124.152739122883)) ;
#71874 = CARTESIAN_POINT('Ctrl Pts',(-20.4160918624688,12.0651385693522,124.15263435594)) ;
#71875 = CARTESIAN_POINT('Ctrl Pts',(-20.41625107805,12.065126283532,124.152417925061)) ;
#71876 = CARTESIAN_POINT('Ctrl Pts',(-20.4163331952535,12.0651199457425,124.152306259526)) ;
#71877 = CARTESIAN_POINT('Ctrl Pts',(-20.4165028930751,12.0651068459312,124.152075418696)) ;
#71878 = CARTESIAN_POINT('Ctrl Pts',(-20.4165904711245,12.0651000839356,124.151956241505)) ;
#71879 = CARTESIAN_POINT('Ctrl Pts',(-20.4167715711197,12.0650860980831,124.151709706921)) ;
#71880 = CARTESIAN_POINT('Ctrl Pts',(-20.4168650901363,12.0650788742523,124.151582347246)) ;
#71881 = CARTESIAN_POINT('Ctrl Pts',(-20.4170585962738,12.0650639236198,124.151318714486)) ;
#71882 = CARTESIAN_POINT('Ctrl Pts',(-20.4171585798546,12.0650561968585,124.151182438921)) ;
#71883 = CARTESIAN_POINT('Ctrl Pts',(-20.4173655861165,12.0650401955187,124.150900173625)) ;
#71884 = CARTESIAN_POINT('Ctrl Pts',(-20.4174726047053,12.0650319209845,124.150754180954)) ;
#71885 = CARTESIAN_POINT('Ctrl Pts',(-20.4176943019083,12.0650147752497,124.150451608138)) ;
#71886 = CARTESIAN_POINT('Ctrl Pts',(-20.4178089758365,12.0650059040936,124.150295024435)) ;
#71887 = CARTESIAN_POINT('Ctrl Pts',(-20.4180466577821,12.0649875119879,124.149970318471)) ;
#71888 = CARTESIAN_POINT('Ctrl Pts',(-20.4181696602443,12.0649779910963,124.149802192162)) ;
#71889 = CARTESIAN_POINT('Ctrl Pts',(-20.4184247291509,12.0649582418742,124.14945336746)) ;
#71890 = CARTESIAN_POINT('Ctrl Pts',(-20.4185567891168,12.0649480136099,124.14927266431)) ;
#71891 = CARTESIAN_POINT('Ctrl Pts',(-20.4188307611062,12.0649267872597,124.148897565596)) ;
#71892 = CARTESIAN_POINT('Ctrl Pts',(-20.418972665493,12.0649157892556,124.148703164546)) ;
#71893 = CARTESIAN_POINT('Ctrl Pts',(-20.422192437283,12.0646661618952,124.144289581556)) ;
#71894 = CARTESIAN_POINT('Ctrl Pts',(-20.4252438958259,12.0644278074472,124.140051183426)) ;
#71895 = CARTESIAN_POINT('Ctrl Pts',(-20.4331073680391,12.0638088571386,124.128983395644)) ;
#71896 = CARTESIAN_POINT('Ctrl Pts',(-20.4378776439048,12.0634286941462,124.122124657684)) ;
#71897 = CARTESIAN_POINT('Ctrl Pts',(-20.4528336824315,12.062221153675,124.100154114118)) ;
#71898 = CARTESIAN_POINT('Ctrl Pts',(-20.4627578372336,12.0613965442986,124.084867254394)) ;
#71899 = CARTESIAN_POINT('Ctrl Pts',(-20.4727813146158,12.0605343833122,124.068662240816)) ;
#71900 = CARTESIAN_POINT('Ctrl Pts',(-20.4732176477929,12.0604967910872,124.067955243916)) ;
#71901 = CARTESIAN_POINT('Ctrl Pts',(-20.4738579534048,12.0604415344476,124.066915429489)) ;
#71902 = CARTESIAN_POINT('Ctrl Pts',(-20.47406247534,12.0604238710399,124.066582950534)) ;
#71903 = CARTESIAN_POINT('Ctrl Pts',(-20.4843179391799,12.0595374725998,124.049893750197)) ;
#71904 = CARTESIAN_POINT('Ctrl Pts',(-20.4939908272755,12.0586677426322,124.033307837398)) ;
#71905 = CARTESIAN_POINT('Ctrl Pts',(-20.5059948635859,12.0575370041652,124.011590177861)) ;
#71906 = CARTESIAN_POINT('Ctrl Pts',(-20.5086787182254,12.0572806733436,124.00665630531)) ;
#71907 = CARTESIAN_POINT('Ctrl Pts',(-20.512853324228,12.056876255664,123.998857135199)) ;
#71908 = CARTESIAN_POINT('Ctrl Pts',(-20.5143663828104,12.0567284643461,123.996003853889)) ;
#71909 = CARTESIAN_POINT('Ctrl Pts',(-20.517005735188,12.0564685004419,123.990979693407)) ;
#71910 = CARTESIAN_POINT('Ctrl Pts',(-20.5181367485304,12.05635639112,123.988811310969)) ;
#71911 = CARTESIAN_POINT('Ctrl Pts',(-20.5205349422282,12.0561171488925,123.984180392362)) ;
#71912 = CARTESIAN_POINT('Ctrl Pts',(-20.521800316381,12.0559899929009,123.98171693723)) ;
#71913 = CARTESIAN_POINT('Ctrl Pts',(-20.5246253246488,12.0557040202269,123.976171891689)) ;
#71914 = CARTESIAN_POINT('Ctrl Pts',(-20.5261803932535,12.0555451455551,123.973088004535)) ;
#71915 = CARTESIAN_POINT('Ctrl Pts',(-20.5301083198074,12.0551401077827,123.965217488337)) ;
#71916 = CARTESIAN_POINT('Ctrl Pts',(-20.5324633030709,12.0548937254411,123.96042203006)) ;
#71917 = CARTESIAN_POINT('Ctrl Pts',(-20.5394434255522,12.054152739411,123.945975039241)) ;
#71918 = CARTESIAN_POINT('Ctrl Pts',(-20.5439754046794,12.0536571107952,123.936279101889)) ;
#71919 = CARTESIAN_POINT('Ctrl Pts',(-20.5620006759575,12.0516265810683,123.896387329024)) ;
#71920 = CARTESIAN_POINT('Ctrl Pts',(-20.5744178530992,12.0500879661591,123.865719170608)) ;
#71921 = CARTESIAN_POINT('Ctrl Pts',(-20.5880790005414,12.0482251157667,123.827708763827)) ;
#71922 = CARTESIAN_POINT('Ctrl Pts',(-20.5904932724967,12.0478882184446,123.820801409786)) ;
#71923 = CARTESIAN_POINT('Ctrl Pts',(-20.5942155879645,12.0473563127395,123.809843716294)) ;
#71924 = CARTESIAN_POINT('Ctrl Pts',(-20.5955638247531,12.0471609157256,123.805807230995)) ;
#71925 = CARTESIAN_POINT('Ctrl Pts',(-20.59804666127,12.0467958645489,123.798245575422)) ;
#71926 = CARTESIAN_POINT('Ctrl Pts',(-20.5991862591325,12.0466261635597,123.794722098284)) ;
#71927 = CARTESIAN_POINT('Ctrl Pts',(-20.6016697257812,12.0462515135264,123.786925406358)) ;
#71928 = CARTESIAN_POINT('Ctrl Pts',(-20.6030063164397,12.0460466360809,123.782649924706)) ;
#71929 = CARTESIAN_POINT('Ctrl Pts',(-20.6071630785038,12.0453989591058,123.769097916851)) ;
#71930 = CARTESIAN_POINT('Ctrl Pts',(-20.6098983232399,12.0449569452473,123.759795696497)) ;
#71931 = CARTESIAN_POINT('Ctrl Pts',(-20.6165612161888,12.0438375928716,123.736121732893)) ;
#71932 = CARTESIAN_POINT('Ctrl Pts',(-20.6203406615935,12.0431613709553,123.721709865636)) ;
#71933 = CARTESIAN_POINT('Ctrl Pts',(-20.6297784283664,12.0413493131084,123.682907377856)) ;
#71934 = CARTESIAN_POINT('Ctrl Pts',(-20.6349630441291,12.0402131776064,123.658408815265)) ;
#71935 = CARTESIAN_POINT('Ctrl Pts',(-20.6406211340074,12.0387595178698,123.627050353775)) ;
#71936 = CARTESIAN_POINT('Ctrl Pts',(-20.6417786739652,12.0384476006976,123.620319807053)) ;
#71937 = CARTESIAN_POINT('Ctrl Pts',(-20.6436637759499,12.0379135113278,123.608794173082)) ;
#71938 = CARTESIAN_POINT('Ctrl Pts',(-20.6444186943254,12.0376915400198,123.604003711717)) ;
#71939 = CARTESIAN_POINT('Ctrl Pts',(-20.6458999344702,12.037238901197,123.594234885875)) ;
#71940 = CARTESIAN_POINT('Ctrl Pts',(-20.6466241161967,12.0370082231259,123.589256286303)) ;
#71941 = CARTESIAN_POINT('Ctrl Pts',(-20.6480658827345,12.0365286695965,123.578906160684)) ;
#71942 = CARTESIAN_POINT('Ctrl Pts',(-20.6487786317843,12.0362797683314,123.573534066836)) ;
#71943 = CARTESIAN_POINT('Ctrl Pts',(-20.650463700079,12.035660496697,123.560167347254)) ;
#71944 = CARTESIAN_POINT('Ctrl Pts',(-20.6513937331328,12.0352899070978,123.552167646638)) ;
#71945 = CARTESIAN_POINT('Ctrl Pts',(-20.6544396878819,12.0339650937015,123.523560307749)) ;
#71946 = CARTESIAN_POINT('Ctrl Pts',(-20.6561205682173,12.0330093666764,123.502909777888)) ;
#71947 = CARTESIAN_POINT('Ctrl Pts',(-20.6576438143366,12.0317651851348,123.475911306821)) ;
#71948 = CARTESIAN_POINT('Ctrl Pts',(-20.657952198977,12.0314744462619,123.469592960766)) ;
#71949 = CARTESIAN_POINT('Ctrl Pts',(-20.6584354889974,12.0309355557161,123.457863030485)) ;
#71950 = CARTESIAN_POINT('Ctrl Pts',(-20.6586232206058,12.0306872812204,123.452452151454)) ;
#71951 = CARTESIAN_POINT('Ctrl Pts',(-20.659418912749,12.0293933844223,123.424227986118)) ;
#71952 = CARTESIAN_POINT('Ctrl Pts',(-20.6594371880276,12.028350724203,123.40140236518)) ;
#71953 = CARTESIAN_POINT('Ctrl Pts',(-20.6584226153015,12.0266050694688,123.363245728406)) ;
#71954 = CARTESIAN_POINT('Ctrl Pts',(-20.657732078491,12.0259028403014,123.347911293571)) ;
#71955 = CARTESIAN_POINT('Ctrl Pts',(-20.6564251327272,12.0249580295856,123.327330883274)) ;
#71956 = CARTESIAN_POINT('Ctrl Pts',(-20.656057636337,12.024716329629,123.322070441065)) ;
#71957 = CARTESIAN_POINT('Ctrl Pts',(-20.6552721826119,12.024242401614,123.311765619155)) ;
#71958 = CARTESIAN_POINT('Ctrl Pts',(-20.6548576526987,12.0240106250304,123.306730645549)) ;
#71959 = CARTESIAN_POINT('Ctrl Pts',(-20.6544117326069,12.0237782986488,123.30168882934)) ;
#71960 = CARTESIAN_POINT('Origin',(-19.4092722359532,16.5113612779716,123.411814366564)) ;
#71961 = CARTESIAN_POINT('',(-20.5919049252751,11.7,123.006993514553)) ;
#71962 = CARTESIAN_POINT('',(-20.5919021064381,16.5113612779716,123.006985279772)) ;
#71963 = CARTESIAN_POINT('Ctrl Pts',(-20.6544117668603,12.0237783015714,123.301689216628)) ;
#71964 = CARTESIAN_POINT('Ctrl Pts',(-20.6544694561418,12.0157819840134,123.302341485478)) ;
#71965 = CARTESIAN_POINT('Ctrl Pts',(-20.6544970374151,12.0078383226351,123.302657626506)) ;
#71966 = CARTESIAN_POINT('Ctrl Pts',(-20.6544970374151,11.9621695797156,123.302657626506)) ;
#71967 = CARTESIAN_POINT('Ctrl Pts',(-20.6538866180435,11.9219235159018,123.294843389787)) ;
#71968 = CARTESIAN_POINT('Ctrl Pts',(-20.6505510417636,11.8480564696761,123.263577766805)) ;
#71969 = CARTESIAN_POINT('Ctrl Pts',(-20.6477244677879,11.8144220247008,123.24016910469)) ;
#71970 = CARTESIAN_POINT('Ctrl Pts',(-20.6391780918807,11.761317155029,123.186964545377)) ;
#71971 = CARTESIAN_POINT('Ctrl Pts',(-20.6328682032119,11.7382522587826,123.15357258444)) ;
#71972 = CARTESIAN_POINT('Ctrl Pts',(-20.6154021887202,11.7075896772133,123.081471444624)) ;
#71973 = CARTESIAN_POINT('Ctrl Pts',(-20.6041551258135,11.7,123.042780919119)) ;
#71974 = CARTESIAN_POINT('Ctrl Pts',(-20.5919049252751,11.7,123.006993514553)) ;
#71975 = CARTESIAN_POINT('Ctrl Pts',(-18.3268334740834,12.1788217328616,124.036975407319)) ;
#71976 = CARTESIAN_POINT('Ctrl Pts',(-18.3340422145277,12.1597692257128,124.049457023371)) ;
#71977 = CARTESIAN_POINT('Ctrl Pts',(-18.3403342428411,12.139044727822,124.059859793497)) ;
#71978 = CARTESIAN_POINT('Ctrl Pts',(-18.3453503566598,12.1170531743812,124.067992874926)) ;
#71979 = CARTESIAN_POINT('',(-18.2266508223232,11.7,123.81666815758)) ;
#71980 = CARTESIAN_POINT('Ctrl Pts',(-18.3583806245238,12.,124.088665030377)) ;
#71981 = CARTESIAN_POINT('Ctrl Pts',(-18.3583806245238,11.9621695797156,124.088665030377)) ;
#71982 = CARTESIAN_POINT('Ctrl Pts',(-18.3540742080748,11.9219235159018,124.082116008719)) ;
#71983 = CARTESIAN_POINT('Ctrl Pts',(-18.3375495990129,11.8480564696761,124.055365260225)) ;
#71984 = CARTESIAN_POINT('Ctrl Pts',(-18.3254377303918,11.8144220247008,124.035135143544)) ;
#71985 = CARTESIAN_POINT('Ctrl Pts',(-18.2995859960063,11.761317155029,123.987854560826)) ;
#71986 = CARTESIAN_POINT('Ctrl Pts',(-18.2841086594605,11.7382522587826,123.957600803974)) ;
#71987 = CARTESIAN_POINT('Ctrl Pts',(-18.2537250256192,11.7075896772133,123.889921628303)) ;
#71988 = CARTESIAN_POINT('Ctrl Pts',(-18.2389020196221,11.7,123.852455220934)) ;
#71989 = CARTESIAN_POINT('Ctrl Pts',(-18.2266508223232,11.7,123.81666815758)) ;
#71990 = CARTESIAN_POINT('Ctrl Pts',(-18.2266508223232,11.7,123.81666815758)) ;
#71991 = CARTESIAN_POINT('Ctrl Pts',(-18.2143996574381,11.7,123.78088118891)) ;
#71992 = CARTESIAN_POINT('Ctrl Pts',(-18.2031515402731,11.7075896412593,123.742191073382)) ;
#71993 = CARTESIAN_POINT('Ctrl Pts',(-18.1856835511285,11.7382521626639,123.670090636116)) ;
#71994 = CARTESIAN_POINT('Ctrl Pts',(-18.1793727421956,11.7613170365764,123.636698971197)) ;
#71995 = CARTESIAN_POINT('Ctrl Pts',(-18.1708248842569,11.8144219229966,123.583494827023)) ;
#71996 = CARTESIAN_POINT('Ctrl Pts',(-18.1679976569785,11.8480564142548,123.560086346945)) ;
#71997 = CARTESIAN_POINT('Ctrl Pts',(-18.1646612055237,11.9219235188396,123.528820989278)) ;
#71998 = CARTESIAN_POINT('Ctrl Pts',(-18.1640505668151,11.9621695923928,123.521006833268)) ;
#71999 = CARTESIAN_POINT('Ctrl Pts',(-18.1640505668151,12.,123.521006833268)) ;
#72000 = CARTESIAN_POINT('Ctrl Pts',(-20.5919021064174,11.7000000001262,123.006985279712)) ;
#72001 = CARTESIAN_POINT('Ctrl Pts',(-20.579651689103,11.7000010975739,122.971198055147)) ;
#72002 = CARTESIAN_POINT('Ctrl Pts',(-20.5648328354892,11.7075896412593,122.933739475197)) ;
#72003 = CARTESIAN_POINT('Ctrl Pts',(-20.5344511925933,11.7382521626639,122.86605964457)) ;
#72004 = CARTESIAN_POINT('Ctrl Pts',(-20.5189747646632,11.7613170365764,122.835805557673)) ;
#72005 = CARTESIAN_POINT('Ctrl Pts',(-20.4931244558125,11.8144219229966,122.788524394775)) ;
#72006 = CARTESIAN_POINT('Ctrl Pts',(-20.4810132149992,11.8480564142548,122.76829402158)) ;
#72007 = CARTESIAN_POINT('Ctrl Pts',(-20.4644894601081,11.9219235188396,122.741542946412)) ;
#72008 = CARTESIAN_POINT('Ctrl Pts',(-20.4601832664426,11.9621695923928,122.734993854115)) ;
#72009 = CARTESIAN_POINT('Ctrl Pts',(-20.4601832664426,12.,122.734993854115)) ;
#72010 = CARTESIAN_POINT('Ctrl Pts',(-17.9901976316281,-10.0000000000559,
123.897592500191)) ;
#72011 = CARTESIAN_POINT('Ctrl Pts',(-18.2740109056134,-9.82001091963712,
123.800437437226)) ;
#72012 = CARTESIAN_POINT('Ctrl Pts',(-18.0463587734038,-10.006626850874,124.061733136848)) ;
#72013 = CARTESIAN_POINT('Ctrl Pts',(-18.318952820002,-9.82663777045524,123.931772257896)) ;
#72014 = CARTESIAN_POINT('Ctrl Pts',(-18.215820208241,-10.019857477355,124.369865791256)) ;
#72015 = CARTESIAN_POINT('Ctrl Pts',(-18.4544999964107,-9.83986839693625,
124.178242269465)) ;
#72016 = CARTESIAN_POINT('Ctrl Pts',(-18.6148367044591,-10.0398330986136,
124.720100586831)) ;
#72017 = CARTESIAN_POINT('Ctrl Pts',(-18.7737259547846,-9.85984401819488,
124.458448709452)) ;
#72018 = CARTESIAN_POINT('Ctrl Pts',(-19.1081207670021,-10.0597504335156,
124.912141899957)) ;
#72019 = CARTESIAN_POINT('Ctrl Pts',(-19.1683517739458,-9.87976135309682,
124.612076728176)) ;
#72020 = CARTESIAN_POINT('Ctrl Pts',(-19.6362061149481,-10.0796237102316,
124.925498515574)) ;
#72021 = CARTESIAN_POINT('Ctrl Pts',(-19.5908222086086,-9.89963462981282,
124.622761886445)) ;
#72022 = CARTESIAN_POINT('Ctrl Pts',(-20.1407529320643,-10.0996482003955,
124.756244590418)) ;
#72023 = CARTESIAN_POINT('Ctrl Pts',(-19.994458721673,-9.91965911997678,124.487357109044)) ;
#72024 = CARTESIAN_POINT('Ctrl Pts',(-20.5540202996666,-10.1195160415463,
124.427406225496)) ;
#72025 = CARTESIAN_POINT('Ctrl Pts',(-20.3250727353524,-9.9395269611275,124.224284451464)) ;
#72026 = CARTESIAN_POINT('Ctrl Pts',(-20.8319818408465,-10.1394616924258,
123.976064807466)) ;
#72027 = CARTESIAN_POINT('Ctrl Pts',(-20.547440485577,-9.95947261200706,123.863209762279)) ;
#72028 = CARTESIAN_POINT('Ctrl Pts',(-20.9388342401899,-10.1593670930428,
123.457915382838)) ;
#72029 = CARTESIAN_POINT('Ctrl Pts',(-20.6329204948871,-9.97937801262402,
123.448688955287)) ;
#72030 = CARTESIAN_POINT('Ctrl Pts',(-20.8636098403204,-10.1792413208591,
122.935072644698)) ;
#72031 = CARTESIAN_POINT('Ctrl Pts',(-20.5727382379585,-9.99925224044038,
123.03041411648)) ;
#72032 = CARTESIAN_POINT('Ctrl Pts',(-20.6131115834828,-10.1992271117367,
122.466642059168)) ;
#72033 = CARTESIAN_POINT('Ctrl Pts',(-20.3723371633396,-10.019238031318,122.655670872381)) ;
#72034 = CARTESIAN_POINT('Ctrl Pts',(-20.2194466572393,-10.2191213543965,
122.113692749269)) ;
#72035 = CARTESIAN_POINT('Ctrl Pts',(-20.0574027588299,-10.0391322739778,
122.373312971228)) ;
#72036 = CARTESIAN_POINT('Ctrl Pts',(-19.7297807740129,-10.2390000704686,
121.915093775285)) ;
#72037 = CARTESIAN_POINT('Ctrl Pts',(-19.6656681100072,-10.0590109900498,
122.21443654672)) ;
#72038 = CARTESIAN_POINT('Ctrl Pts',(-19.1975679684638,-10.2590395203132,
121.895998337722)) ;
#72039 = CARTESIAN_POINT('Ctrl Pts',(-19.2398980466007,-10.0790504398944,
122.199163431724)) ;
#72040 = CARTESIAN_POINT('Ctrl Pts',(-18.6950312339479,-10.278902681851,122.058270950154)) ;
#72041 = CARTESIAN_POINT('Ctrl Pts',(-18.837868920824,-10.0989136014323,122.328984924085)) ;
#72042 = CARTESIAN_POINT('Ctrl Pts',(-18.2756669291074,-10.2988820498653,
122.383749835499)) ;
#72043 = CARTESIAN_POINT('Ctrl Pts',(-18.5023795133954,-10.1188929694465,
122.589370885141)) ;
#72044 = CARTESIAN_POINT('Ctrl Pts',(-17.9943038604906,-10.3186926303881,
122.828930487525)) ;
#72045 = CARTESIAN_POINT('Ctrl Pts',(-18.2772917344201,-10.1387035499693,
122.945518187819)) ;
#72046 = CARTESIAN_POINT('Ctrl Pts',(-17.8800540060949,-10.3386735586737,
123.347451469639)) ;
#72047 = CARTESIAN_POINT('Ctrl Pts',(-18.1858955346146,-10.1586844782549,
123.360335798021)) ;
#72048 = CARTESIAN_POINT('Ctrl Pts',(-17.9496636135844,-10.3585662305431,
123.871624239551)) ;
#72049 = CARTESIAN_POINT('Ctrl Pts',(-18.2415877728661,-10.1785771501243,
123.779674103343)) ;
#72050 = CARTESIAN_POINT('Ctrl Pts',(-18.1935384904097,-10.3784925608302,
124.341742095298)) ;
#72051 = CARTESIAN_POINT('Ctrl Pts',(-18.4366892418074,-10.1985034804115,
124.155765909524)) ;
#72052 = CARTESIAN_POINT('Ctrl Pts',(-18.5843830565522,-10.3984631149225,
124.700856014359)) ;
#72053 = CARTESIAN_POINT('Ctrl Pts',(-18.7493759717748,-10.2184740345037,
124.44305681766)) ;
#72054 = CARTESIAN_POINT('Ctrl Pts',(-18.9897866675732,-10.4149949540101,
124.87030674843)) ;
#72055 = CARTESIAN_POINT('Ctrl Pts',(-19.0736749228579,-10.2350058735914,
124.578605598989)) ;
#72056 = CARTESIAN_POINT('Ctrl Pts',(-19.3371420473562,-10.4283346928377,
124.91771178987)) ;
#72057 = CARTESIAN_POINT('Ctrl Pts',(-19.3515822796175,-10.2483456124189,
124.6165344309)) ;
#72058 = CARTESIAN_POINT('Ctrl Pts',(-19.600556266745,-10.4383669350563,124.907063768875)) ;
#72059 = CARTESIAN_POINT('Ctrl Pts',(-19.5623087731277,-10.2583778546375,
124.608012505296)) ;
#72060 = CARTESIAN_POINT('Ctrl Pts',(-19.8537397871011,-10.4482246356997,
124.852203726836)) ;
#72061 = CARTESIAN_POINT('Ctrl Pts',(-19.7648571225557,-10.268235555281,124.564122220758)) ;
#72062 = CARTESIAN_POINT('Ctrl Pts',(-20.0969735540212,-10.458216500339,124.753332920167)) ;
#72063 = CARTESIAN_POINT('Ctrl Pts',(-19.9594412734619,-10.2782274199202,
124.485025314983)) ;
#72064 = CARTESIAN_POINT('Ctrl Pts',(-20.3177787346959,-10.4681390500991,
124.61465218344)) ;
#72065 = CARTESIAN_POINT('Ctrl Pts',(-20.1360907041886,-10.2881499696804,
124.374071880139)) ;
#72066 = CARTESIAN_POINT('Ctrl Pts',(-20.5771970982088,-10.4814168235926,
124.381203458951)) ;
#72067 = CARTESIAN_POINT('Ctrl Pts',(-20.3435922192053,-10.3014277431738,
124.18734533642)) ;
#72068 = CARTESIAN_POINT('Ctrl Pts',(-20.7701003709019,-10.4947641625332,
124.083584310499)) ;
#72069 = CARTESIAN_POINT('Ctrl Pts',(-20.4979358992389,-10.3147750821144,
123.949230612993)) ;
#72070 = CARTESIAN_POINT('Ctrl Pts',(-20.8774553694635,-10.5079713943264,
123.753475217075)) ;
#72071 = CARTESIAN_POINT('Ctrl Pts',(-20.5838202404129,-10.3279823139076,
123.685128879657)) ;
#72072 = CARTESIAN_POINT('Ctrl Pts',(-20.914528239215,-10.5179585104161,123.493699384281)) ;
#72073 = CARTESIAN_POINT('Ctrl Pts',(-20.6134756829108,-10.3379694299973,
123.477310647391)) ;
#72074 = CARTESIAN_POINT('Ctrl Pts',(-20.9061303770652,-10.5279094159958,
123.232285620256)) ;
#72075 = CARTESIAN_POINT('Ctrl Pts',(-20.6067552793287,-10.3479203355771,
123.268178977505)) ;
#72076 = CARTESIAN_POINT('Ctrl Pts',(-20.8516285273061,-10.5379645180033,
122.97376743032)) ;
#72077 = CARTESIAN_POINT('Ctrl Pts',(-20.5631517097427,-10.3579754375845,
123.061365248372)) ;
#72078 = CARTESIAN_POINT('Ctrl Pts',(-20.7557521455566,-10.5477861913244,
122.73410076229)) ;
#72079 = CARTESIAN_POINT('Ctrl Pts',(-20.4864480022253,-10.3677971109056,
122.869632334128)) ;
#72080 = CARTESIAN_POINT('Ctrl Pts',(-20.6168357131279,-10.5578446623993,
122.509252277658)) ;
#72081 = CARTESIAN_POINT('Ctrl Pts',(-20.3753148734437,-10.3778555819805,
122.689756047917)) ;
#72082 = CARTESIAN_POINT('Ctrl Pts',(-20.443040351458,-10.5677692735758,122.314768071388)) ;
#72083 = CARTESIAN_POINT('Ctrl Pts',(-20.2362698376991,-10.387780193157,122.534165626482)) ;
#72084 = CARTESIAN_POINT('Ctrl Pts',(-20.1694406713465,-10.5810466124762,
122.098190251823)) ;
#72085 = CARTESIAN_POINT('Ctrl Pts',(-20.0174235370575,-10.4010575320574,
122.360928563111)) ;
#72086 = CARTESIAN_POINT('Ctrl Pts',(-19.8449850135089,-10.5943454917138,
121.958111265245)) ;
#72087 = CARTESIAN_POINT('Ctrl Pts',(-19.7578454755217,-10.414356411295,122.248851541412)) ;
#72088 = CARTESIAN_POINT('Ctrl Pts',(-19.5008057716398,-10.6075843638845,
121.907157355555)) ;
#72089 = CARTESIAN_POINT('Ctrl Pts',(-19.4824812721784,-10.4275952834657,
122.208088431707)) ;
#72090 = CARTESIAN_POINT('Ctrl Pts',(-19.2379220825766,-10.6175909820211,
121.913944971311)) ;
#72091 = CARTESIAN_POINT('Ctrl Pts',(-19.2721785612158,-10.4376019016023,
122.213521362329)) ;
#72092 = CARTESIAN_POINT('Ctrl Pts',(-18.9796997397217,-10.6276219270826,
121.966900411334)) ;
#72093 = CARTESIAN_POINT('Ctrl Pts',(-19.0656000663898,-10.4476328466638,
122.255887759951)) ;
#72094 = CARTESIAN_POINT('Ctrl Pts',(-18.7386663423007,-10.6374781004344,
122.061762842518)) ;
#72095 = CARTESIAN_POINT('Ctrl Pts',(-18.8727746408769,-10.4574890200157,
122.33177976469)) ;
#72096 = CARTESIAN_POINT('Ctrl Pts',(-18.5144394578207,-10.6474773713973,
122.198683103342)) ;
#72097 = CARTESIAN_POINT('Ctrl Pts',(-18.6933942799492,-10.4674882909785,
122.44131783091)) ;
#72098 = CARTESIAN_POINT('Ctrl Pts',(-18.319187379609,-10.6573718231546,122.370468477367)) ;
#72099 = CARTESIAN_POINT('Ctrl Pts',(-18.5371942578644,-10.4773827427359,
122.578747654411)) ;
#72100 = CARTESIAN_POINT('Ctrl Pts',(-18.1540827676739,-10.667435138964,122.576990252215)) ;
#72101 = CARTESIAN_POINT('Ctrl Pts',(-18.4051122800728,-10.4874460585452,
122.743966484082)) ;
#72102 = CARTESIAN_POINT('Ctrl Pts',(-18.0298636946178,-10.6772739957036,
122.803803190582)) ;
#72103 = CARTESIAN_POINT('Ctrl Pts',(-18.3057391118683,-10.4972849152848,
122.925417599334)) ;
#72104 = CARTESIAN_POINT('Ctrl Pts',(-17.9447485717296,-10.6873401175212,
123.054218033079)) ;
#72105 = CARTESIAN_POINT('Ctrl Pts',(-18.2376490673584,-10.5073510371024,
123.125750218179)) ;
#72106 = CARTESIAN_POINT('Ctrl Pts',(-17.9052474070553,-10.6972233452454,
123.310952604461)) ;
#72107 = CARTESIAN_POINT('Ctrl Pts',(-18.2060503446323,-10.5172342648267,
123.331137917859)) ;
#72108 = CARTESIAN_POINT('Ctrl Pts',(-17.9104088182972,-10.7072128065242,
123.573388107822)) ;
#72109 = CARTESIAN_POINT('Ctrl Pts',(-18.2101816191011,-10.5272237261055,
123.541086174157)) ;
#72110 = CARTESIAN_POINT('Ctrl Pts',(-17.9610292609966,-10.7171765169507,
123.830297050008)) ;
#72111 = CARTESIAN_POINT('Ctrl Pts',(-18.2506800579227,-10.5371874365319,
123.746612765702)) ;
#72112 = CARTESIAN_POINT('Ctrl Pts',(-18.055529675123,-10.7271715196816,124.07538741282)) ;
#72113 = CARTESIAN_POINT('Ctrl Pts',(-18.3262823460712,-10.5471824392628,
123.942684211435)) ;
#72114 = CARTESIAN_POINT('Ctrl Pts',(-18.1920485022638,-10.7372078506919,
124.301034603995)) ;
#72115 = CARTESIAN_POINT('Ctrl Pts',(-18.4354992728269,-10.5572187702731,
124.12320085702)) ;
#72116 = CARTESIAN_POINT('Ctrl Pts',(-18.3620830673666,-10.7470540800342,
124.496092551294)) ;
#72117 = CARTESIAN_POINT('Ctrl Pts',(-18.5715282310147,-10.5670649996154,
124.279245472498)) ;
#72118 = CARTESIAN_POINT('Ctrl Pts',(-18.5658978745398,-10.7570395783094,
124.661307440014)) ;
#72119 = CARTESIAN_POINT('Ctrl Pts',(-18.7345812884953,-10.5770504978907,
124.411415684018)) ;
#72120 = CARTESIAN_POINT('Ctrl Pts',(-18.7941275674309,-10.7669744812924,
124.788187738313)) ;
#72121 = CARTESIAN_POINT('Ctrl Pts',(-18.9171658133098,-10.5869854008736,
124.51291799715)) ;
#72122 = CARTESIAN_POINT('Ctrl Pts',(-19.0439620659732,-10.7770319843876,
124.87431287249)) ;
#72123 = CARTESIAN_POINT('Ctrl Pts',(-19.1170341816332,-10.5970429039689,
124.58181616074)) ;
#72124 = CARTESIAN_POINT('Ctrl Pts',(-19.2988377714731,-10.7868536407581,
124.915180256281)) ;
#72125 = CARTESIAN_POINT('Ctrl Pts',(-19.3209344474807,-10.6068645603394,
124.614507954235)) ;
#72126 = CARTESIAN_POINT('Ctrl Pts',(-19.5630543230719,-10.7969097034233,
124.911570311864)) ;
#72127 = CARTESIAN_POINT('Ctrl Pts',(-19.5323077507347,-10.6169206230045,
124.611618015563)) ;
#72128 = CARTESIAN_POINT('Ctrl Pts',(-19.8195954463674,-10.8068503681265,
124.862237558384)) ;
#72129 = CARTESIAN_POINT('Ctrl Pts',(-19.7375400007717,-10.6268612877077,
124.572149858921)) ;
#72130 = CARTESIAN_POINT('Ctrl Pts',(-20.0630665620779,-10.816754772075,124.770214821725)) ;
#72131 = CARTESIAN_POINT('Ctrl Pts',(-19.9323158100592,-10.6367656916563,
124.498530010754)) ;
#72132 = CARTESIAN_POINT('Ctrl Pts',(-20.2899670416391,-10.8268012570685,
124.635280761844)) ;
#72133 = CARTESIAN_POINT('Ctrl Pts',(-20.1138352645202,-10.6468121766498,
124.390581038644)) ;
#72134 = CARTESIAN_POINT('Ctrl Pts',(-20.4871895042014,-10.8366974848803,
124.465706330273)) ;
#72135 = CARTESIAN_POINT('Ctrl Pts',(-20.2716116273665,-10.6567084044615,
124.254920337405)) ;
#72136 = CARTESIAN_POINT('Ctrl Pts',(-20.6546848716755,-10.8467570684437,
124.261221540579)) ;
#72137 = CARTESIAN_POINT('Ctrl Pts',(-20.4056065232405,-10.666767988025,124.091331180759)) ;
#72138 = CARTESIAN_POINT('Ctrl Pts',(-20.7815048415896,-10.8566090781126,
124.035494716852)) ;
#72139 = CARTESIAN_POINT('Ctrl Pts',(-20.5070605035221,-10.6766199976938,
123.910749362364)) ;
#72140 = CARTESIAN_POINT('Ctrl Pts',(-20.8689878383844,-10.8665716095522,
123.788751735719)) ;
#72141 = CARTESIAN_POINT('Ctrl Pts',(-20.5770451355397,-10.6865825291334,
123.713354624159)) ;
#72142 = CARTESIAN_POINT('Ctrl Pts',(-20.9122007989983,-10.8766031577915,
123.528690516738)) ;
#72143 = CARTESIAN_POINT('Ctrl Pts',(-20.6116136920761,-10.6966140773728,
123.505305293071)) ;
#72144 = CARTESIAN_POINT('Ctrl Pts',(-20.9098873496379,-10.8864945690046,
123.268764662033)) ;
#72145 = CARTESIAN_POINT('Ctrl Pts',(-20.6097611319996,-10.7065054885858,
123.297365172637)) ;
#72146 = CARTESIAN_POINT('Ctrl Pts',(-20.8623452480794,-10.8965108227126,
123.009867420376)) ;
#72147 = CARTESIAN_POINT('Ctrl Pts',(-20.5717257539026,-10.7165217422938,
123.090247714627)) ;
#72148 = CARTESIAN_POINT('Ctrl Pts',(-20.7699148714446,-10.9065409255573,
122.763029266293)) ;
#72149 = CARTESIAN_POINT('Ctrl Pts',(-20.4977797294624,-10.7265518451385,
122.89277779572)) ;
#72150 = CARTESIAN_POINT('Ctrl Pts',(-20.6387642262215,-10.916397374511,122.53965056504)) ;
#72151 = CARTESIAN_POINT('Ctrl Pts',(-20.3928580826567,-10.7364082940922,
122.714076343171)) ;
#72152 = CARTESIAN_POINT('Ctrl Pts',(-20.4686808694509,-10.9263963852833,
122.339414946331)) ;
#72153 = CARTESIAN_POINT('Ctrl Pts',(-20.2567901831118,-10.7464073048645,
122.553889022845)) ;
#72154 = CARTESIAN_POINT('Ctrl Pts',(-20.2686322562865,-10.9362916022013,
122.173218025973)) ;
#72155 = CARTESIAN_POINT('Ctrl Pts',(-20.0967507033617,-10.7563025217825,
122.420933115589)) ;
#72156 = CARTESIAN_POINT('Ctrl Pts',(-20.0390441622035,-10.9463521175586,
122.042191046902)) ;
#72157 = CARTESIAN_POINT('Ctrl Pts',(-19.9130792483847,-10.7663630371399,
122.316112859812)) ;
#72158 = CARTESIAN_POINT('Ctrl Pts',(-19.7954165502378,-10.9562014109456,
121.954734482414)) ;
#72159 = CARTESIAN_POINT('Ctrl Pts',(-19.7181774003615,-10.7762123305269,
122.246149405366)) ;
#72160 = CARTESIAN_POINT('Ctrl Pts',(-19.5358374377784,-10.9662285866257,
121.909463378903)) ;
#72161 = CARTESIAN_POINT('Ctrl Pts',(-19.5105138249597,-10.7862395062069,
122.209933979971)) ;
#72162 = CARTESIAN_POINT('Ctrl Pts',(-19.2722869357708,-10.9762571622528,
121.910644966018)) ;
#72163 = CARTESIAN_POINT('Ctrl Pts',(-19.2996733747243,-10.7962680818341,
122.210880867466)) ;
#72164 = CARTESIAN_POINT('Ctrl Pts',(-19.0176264126099,-10.9861022557987,
121.956219772802)) ;
#72165 = CARTESIAN_POINT('Ctrl Pts',(-19.0959461067893,-10.80611317538,122.247342053206)) ;
#72166 = CARTESIAN_POINT('Ctrl Pts',(-18.7708903038196,-10.9960934972305,
122.045998590388)) ;
#72167 = CARTESIAN_POINT('Ctrl Pts',(-18.8985578386737,-10.8161044168118,
122.319166355093)) ;
#72168 = CARTESIAN_POINT('Ctrl Pts',(-18.542748292224,-11.0061292783738,122.178316885935)) ;
#72169 = CARTESIAN_POINT('Ctrl Pts',(-18.7160448934344,-10.826140197955,122.425022334904)) ;
#72170 = CARTESIAN_POINT('Ctrl Pts',(-18.344525155925,-11.0159814841035,122.344856285558)) ;
#72171 = CARTESIAN_POINT('Ctrl Pts',(-18.5574679962225,-10.8359924036847,
122.558254360555)) ;
#72172 = CARTESIAN_POINT('Ctrl Pts',(-18.175788051193,-11.0259435782205,122.545009574779)) ;
#72173 = CARTESIAN_POINT('Ctrl Pts',(-18.422479486084,-10.8459544978017,122.718377561325)) ;
#72174 = CARTESIAN_POINT('Ctrl Pts',(-18.0438458205834,-11.0359661390476,
122.77296014226)) ;
#72175 = CARTESIAN_POINT('Ctrl Pts',(-18.3169268399301,-10.8559770586288,
122.900738711909)) ;
#72176 = CARTESIAN_POINT('Ctrl Pts',(-17.9540915965204,-11.0458939106991,
123.017952668902)) ;
#72177 = CARTESIAN_POINT('Ctrl Pts',(-18.245124831637,-10.8659048302804,123.096732704545)) ;
#72178 = CARTESIAN_POINT('Ctrl Pts',(-17.9077456059783,-11.055936294824,123.27773445602)) ;
#72179 = CARTESIAN_POINT('Ctrl Pts',(-18.2080492829974,-10.8759472144052,
123.304558492291)) ;
#72180 = CARTESIAN_POINT('Ctrl Pts',(-17.9071113955482,-11.0658255188946,
123.537627775345)) ;
#72181 = CARTESIAN_POINT('Ctrl Pts',(-18.2075431810581,-10.8858364384758,
123.512472408022)) ;
#72182 = CARTESIAN_POINT('Ctrl Pts',(-17.9515732677146,-11.0758147670619,
123.796333212576)) ;
#72183 = CARTESIAN_POINT('Ctrl Pts',(-18.2431137880875,-10.8958256866432,
123.719436394321)) ;
#72184 = CARTESIAN_POINT('Ctrl Pts',(-18.0401957306553,-11.0857733441039,
124.042564530885)) ;
#72185 = CARTESIAN_POINT('Ctrl Pts',(-18.3140127714057,-10.9057842636851,
123.916420715581)) ;
#72186 = CARTESIAN_POINT('Ctrl Pts',(-18.1689090611489,-11.0956729131951,
124.26866068517)) ;
#72187 = CARTESIAN_POINT('Ctrl Pts',(-18.4169840046767,-10.9156838327764,
124.097296505228)) ;
#72188 = CARTESIAN_POINT('Ctrl Pts',(-18.3374567294345,-11.1057208252791,
124.471882073848)) ;
#72189 = CARTESIAN_POINT('Ctrl Pts',(-18.5518230802635,-10.9257317448604,
124.259873062704)) ;
#72190 = CARTESIAN_POINT('Ctrl Pts',(-18.5355938113499,-11.1156161795864,
124.640356432231)) ;
#72191 = CARTESIAN_POINT('Ctrl Pts',(-18.7103328563198,-10.9356270991676,
124.394651291218)) ;
#72192 = CARTESIAN_POINT('Ctrl Pts',(-18.7636640135748,-11.1256778300776,
124.77407551391)) ;
#72193 = CARTESIAN_POINT('Ctrl Pts',(-18.8927897608012,-10.9456887496588,
124.50162580593)) ;
#72194 = CARTESIAN_POINT('Ctrl Pts',(-19.0061643664109,-11.13552244554,124.864226909318)) ;
#72195 = CARTESIAN_POINT('Ctrl Pts',(-19.0867894053353,-10.9555333651213,
124.573745602818)) ;
#72196 = CARTESIAN_POINT('Ctrl Pts',(-19.263434682644,-11.1454825244414,124.912371167805)) ;
#72197 = CARTESIAN_POINT('Ctrl Pts',(-19.2926054448866,-10.9654934440227,
124.612260162443)) ;
#72198 = CARTESIAN_POINT('Ctrl Pts',(-19.5272078042054,-11.1555207187998,
124.914621442869)) ;
#72199 = CARTESIAN_POINT('Ctrl Pts',(-19.5036240790433,-10.9755316383811,
124.614059468937)) ;
#72200 = CARTESIAN_POINT('Ctrl Pts',(-19.7832249578814,-11.1653944341994,
124.872221302239)) ;
#72201 = CARTESIAN_POINT('Ctrl Pts',(-19.7084367869545,-10.9854053537807,
124.580138714143)) ;
#72202 = CARTESIAN_POINT('Ctrl Pts',(-20.0328232712433,-11.1754661437337,
124.784280775652)) ;
#72203 = CARTESIAN_POINT('Ctrl Pts',(-19.9081154761896,-10.9954770633149,
124.509785425241)) ;
#72204 = CARTESIAN_POINT('Ctrl Pts',(-20.2580073160993,-11.1852985841862,
124.657525797666)) ;
#72205 = CARTESIAN_POINT('Ctrl Pts',(-20.0882613121544,-11.0053095037674,
124.408381348776)) ;
#72206 = CARTESIAN_POINT('Ctrl Pts',(-20.4622563154496,-11.1953304051116,
124.490859965115)) ;
#72207 = CARTESIAN_POINT('Ctrl Pts',(-20.2516602105671,-11.0153413246928,
124.275048161913)) ;
#72208 = CARTESIAN_POINT('Ctrl Pts',(-20.6337047073231,-11.2053507749972,
124.29099219891)) ;
#72209 = CARTESIAN_POINT('Ctrl Pts',(-20.388818355727,-11.0253616945784,124.115153420591)) ;
#72210 = CARTESIAN_POINT('Ctrl Pts',(-20.7663802889298,-11.2152175461309,
124.068198059757)) ;
#72211 = CARTESIAN_POINT('Ctrl Pts',(-20.4949578009106,-11.0352284657122,
123.936918629634)) ;
#72212 = CARTESIAN_POINT('Ctrl Pts',(-20.8602333251002,-11.2252883173203,
123.820777914733)) ;
#72213 = CARTESIAN_POINT('Ctrl Pts',(-20.5700397729981,-11.0452992369015,
123.738981987884)) ;
#72214 = CARTESIAN_POINT('Ctrl Pts',(-20.9086197172396,-11.2351314778419,
123.566660443402)) ;
#72215 = CARTESIAN_POINT('Ctrl Pts',(-20.608748082228,-11.0551423974231,123.535689006923)) ;
#72216 = CARTESIAN_POINT('Ctrl Pts',(-20.9130575838385,-11.2451117110283,
123.3044363292)) ;
#72217 = CARTESIAN_POINT('Ctrl Pts',(-20.6122979803846,-11.0651226306096,
123.325909958137)) ;
#72218 = CARTESIAN_POINT('Ctrl Pts',(-20.8712385789228,-11.2551302310635,
123.044509679232)) ;
#72219 = CARTESIAN_POINT('Ctrl Pts',(-20.5788422638188,-11.0751411506447,
123.117968711757)) ;
#72220 = CARTESIAN_POINT('Ctrl Pts',(-20.7865977119189,-11.2650135394472,
122.798931493941)) ;
#72221 = CARTESIAN_POINT('Ctrl Pts',(-20.5111294989851,-11.0850244590284,
122.921507117009)) ;
#72222 = CARTESIAN_POINT('Ctrl Pts',(-20.6581795185129,-11.275081823618,122.567651782583)) ;
#72223 = CARTESIAN_POINT('Ctrl Pts',(-20.4083944277967,-11.0950927431992,
122.736483258853)) ;
#72224 = CARTESIAN_POINT('Ctrl Pts',(-20.4956768374631,-11.2849119502856,
122.366783576228)) ;
#72225 = CARTESIAN_POINT('Ctrl Pts',(-20.278392801361,-11.1049228698669,122.575789859925)) ;
#72226 = CARTESIAN_POINT('Ctrl Pts',(-20.2963683002657,-11.2949785224922,
122.192903170053)) ;
#72227 = CARTESIAN_POINT('Ctrl Pts',(-20.1189455705143,-11.1149894420734,
122.436685510706)) ;
#72228 = CARTESIAN_POINT('Ctrl Pts',(-20.0737183941144,-11.3048686787329,
122.058761956698)) ;
#72229 = CARTESIAN_POINT('Ctrl Pts',(-19.9408262162374,-11.1248795983141,
122.329373218762)) ;
#72230 = CARTESIAN_POINT('Ctrl Pts',(-19.8289002832295,-11.3148612063093,
121.963839656231)) ;
#72231 = CARTESIAN_POINT('Ctrl Pts',(-19.7449718346838,-11.1348721258905,
122.253435573056)) ;
#72232 = CARTESIAN_POINT('Ctrl Pts',(-19.5720596013039,-11.3248226961836,
121.913243324942)) ;
#72233 = CARTESIAN_POINT('Ctrl Pts',(-19.53949961243,-11.1448336157648,122.212958778088)) ;
#72234 = CARTESIAN_POINT('Ctrl Pts',(-19.3117087063704,-11.3347319180708,
121.907440658288)) ;
#72235 = CARTESIAN_POINT('Ctrl Pts',(-19.3312196283681,-11.154742837652,122.208316707602)) ;
#72236 = CARTESIAN_POINT('Ctrl Pts',(-19.0507261790617,-11.3447804978811,
121.947576761834)) ;
#72237 = CARTESIAN_POINT('Ctrl Pts',(-19.1224334112309,-11.1647914174624,
122.240425692634)) ;
#72238 = CARTESIAN_POINT('Ctrl Pts',(-18.804739750581,-11.3546634723512,122.030941792097)) ;
#72239 = CARTESIAN_POINT('Ctrl Pts',(-18.9256451263576,-11.1746743919324,
122.307117480373)) ;
#72240 = CARTESIAN_POINT('Ctrl Pts',(-18.5741327464294,-11.3646583834939,
122.156656021999)) ;
#72241 = CARTESIAN_POINT('Ctrl Pts',(-18.7411596022947,-11.1846693030751,
122.407688711713)) ;
#72242 = CARTESIAN_POINT('Ctrl Pts',(-18.3685394795341,-11.3746787700675,
122.321218804794)) ;
#72243 = CARTESIAN_POINT('Ctrl Pts',(-18.5766849675727,-11.1946896896487,
122.539338955783)) ;
#72244 = CARTESIAN_POINT('Ctrl Pts',(-18.1964679002399,-11.3845888739245,
122.516679816492)) ;
#72245 = CARTESIAN_POINT('Ctrl Pts',(-18.4390281618024,-11.2045997935058,
122.69570718939)) ;
#72246 = CARTESIAN_POINT('Ctrl Pts',(-18.0601098923841,-11.3945165861344,
122.739110167185)) ;
#72247 = CARTESIAN_POINT('Ctrl Pts',(-18.3299418822673,-11.2145275057157,
122.873650852243)) ;
#72248 = CARTESIAN_POINT('Ctrl Pts',(-17.9635464110785,-11.4045596959017,
122.984721718115)) ;
#72249 = CARTESIAN_POINT('Ctrl Pts',(-18.2526908895868,-11.2245706154829,
123.070140194401)) ;
#72250 = CARTESIAN_POINT('Ctrl Pts',(-17.9117458664218,-11.4144461163572,
123.239325516357)) ;
#72251 = CARTESIAN_POINT('Ctrl Pts',(-18.2112504325607,-11.2344570359385,
123.273822340803)) ;
#72252 = CARTESIAN_POINT('Ctrl Pts',(-17.9044206321702,-11.4244392939629,
123.501819128655)) ;
#72253 = CARTESIAN_POINT('Ctrl Pts',(-18.2053899382535,-11.2444502135441,
123.483817059054)) ;
#72254 = CARTESIAN_POINT('Ctrl Pts',(-17.9427031377014,-11.4343849568668,
123.760362733603)) ;
#72255 = CARTESIAN_POINT('Ctrl Pts',(-18.2360155909013,-11.254395876448,123.690651513861)) ;
#72256 = CARTESIAN_POINT('Ctrl Pts',(-18.0248064636778,-11.444332253072,124.008552115049)) ;
#72257 = CARTESIAN_POINT('Ctrl Pts',(-18.3016977085877,-11.2643431726532,
123.889202714741)) ;
#72258 = CARTESIAN_POINT('Ctrl Pts',(-18.1502567639507,-11.4543800186499,
124.240883955194)) ;
#72259 = CARTESIAN_POINT('Ctrl Pts',(-18.402057739547,-11.2743909382311,124.075068526834)) ;
#72260 = CARTESIAN_POINT('Ctrl Pts',(-18.3107289743718,-11.4642282318675,
124.443923603777)) ;
#72261 = CARTESIAN_POINT('Ctrl Pts',(-18.5304345036023,-11.2842391514487,
124.237499615883)) ;
#72262 = CARTESIAN_POINT('Ctrl Pts',(-18.505629079582,-11.4741878046616,124.618608196074)) ;
#72263 = CARTESIAN_POINT('Ctrl Pts',(-18.6863538979281,-11.2941987242428,
124.377247496808)) ;
#72264 = CARTESIAN_POINT('Ctrl Pts',(-18.7298566496117,-11.4842244256941,
124.7574702214)) ;
#72265 = CARTESIAN_POINT('Ctrl Pts',(-18.8657357990191,-11.3042353452753,
124.488337605862)) ;
#72266 = CARTESIAN_POINT('Ctrl Pts',(-18.9708633136345,-11.4941049405044,
124.854157638522)) ;
#72267 = CARTESIAN_POINT('Ctrl Pts',(-19.0585400766373,-11.3141158600857,
124.565687764043)) ;
#72268 = CARTESIAN_POINT('Ctrl Pts',(-19.2293390121341,-11.5041575918115,
124.908543575082)) ;
#72269 = CARTESIAN_POINT('Ctrl Pts',(-19.265320722865,-11.3241685113927,124.609197170298)) ;
#72270 = CARTESIAN_POINT('Ctrl Pts',(-19.4892814881004,-11.5140529900915,
124.917196362608)) ;
#72271 = CARTESIAN_POINT('Ctrl Pts',(-19.4732739141341,-11.3340639096727,
124.61612002099)) ;
#72272 = CARTESIAN_POINT('Ctrl Pts',(-19.7507413265395,-11.5241031117976,
124.880139860479)) ;
#72273 = CARTESIAN_POINT('Ctrl Pts',(-19.6824420883012,-11.3441140313788,
124.586475461409)) ;
#72274 = CARTESIAN_POINT('Ctrl Pts',(-19.9977235239071,-11.5339873913395,
124.799620909401)) ;
#72275 = CARTESIAN_POINT('Ctrl Pts',(-19.8800272541223,-11.3539983109207,
124.522061213482)) ;
#72276 = CARTESIAN_POINT('Ctrl Pts',(-20.2297217101935,-11.5439821726314,
124.676533838813)) ;
#72277 = CARTESIAN_POINT('Ctrl Pts',(-20.0656260392352,-11.3639930922127,
124.423592342302)) ;
#72278 = CARTESIAN_POINT('Ctrl Pts',(-20.4358226950953,-11.5539300178182,
124.51568737912)) ;
#72279 = CARTESIAN_POINT('Ctrl Pts',(-20.2305069652934,-11.3739409373994,
124.294916057216)) ;
#72280 = CARTESIAN_POINT('Ctrl Pts',(-20.6109276227869,-11.5638669812056,
124.321995034951)) ;
#72281 = CARTESIAN_POINT('Ctrl Pts',(-20.37059121164,-11.3838779007868,124.139963144074)) ;
#72282 = CARTESIAN_POINT('Ctrl Pts',(-20.7506923360164,-11.5738499459428,
124.099943607962)) ;
#72283 = CARTESIAN_POINT('Ctrl Pts',(-20.482403674932,-11.3938608655241,123.962322680992)) ;
#72284 = CARTESIAN_POINT('Ctrl Pts',(-20.849910076086,-11.5838937973584,123.855392878885)) ;
#72285 = CARTESIAN_POINT('Ctrl Pts',(-20.561778696542,-11.4039047169397,123.766682270914)) ;
#72286 = CARTESIAN_POINT('Ctrl Pts',(-20.9045834154324,-11.5937219986932,
123.602930177821)) ;
#72287 = CARTESIAN_POINT('Ctrl Pts',(-20.6055180794411,-11.4137329182744,
123.5647134447)) ;
#72288 = CARTESIAN_POINT('Ctrl Pts',(-20.9149654650687,-11.6037985712912,
123.338386769832)) ;
#72289 = CARTESIAN_POINT('Ctrl Pts',(-20.6138247398722,-11.4238094908725,
123.353078412637)) ;
#72290 = CARTESIAN_POINT('Ctrl Pts',(-20.8801663078721,-11.6136506512988,
123.081776137411)) ;
#72291 = CARTESIAN_POINT('Ctrl Pts',(-20.5859865727851,-11.43366157088,123.147790745259)) ;
#72292 = CARTESIAN_POINT('Ctrl Pts',(-20.7998144513112,-11.6237239363029,
122.82959680017)) ;
#72293 = CARTESIAN_POINT('Ctrl Pts',(-20.5217060262302,-11.4437348558841,
122.946046639568)) ;
#72294 = CARTESIAN_POINT('Ctrl Pts',(-20.6796373591694,-11.6335652880134,
122.600571403719)) ;
#72295 = CARTESIAN_POINT('Ctrl Pts',(-20.4255657854105,-11.4535762075946,
122.762826748449)) ;
#72296 = CARTESIAN_POINT('Ctrl Pts',(-20.5203770952536,-11.6435267874099,
122.392832222546)) ;
#72297 = CARTESIAN_POINT('Ctrl Pts',(-20.2981587895807,-11.4635377069911,
122.59663487523)) ;
#72298 = CARTESIAN_POINT('Ctrl Pts',(-20.3256964581536,-11.6535625635399,
122.214906329216)) ;
#72299 = CARTESIAN_POINT('Ctrl Pts',(-20.1424150134632,-11.4735734831211,
122.454293226116)) ;
#72300 = CARTESIAN_POINT('Ctrl Pts',(-20.1065035193334,-11.6634509901774,
122.075338994237)) ;
#72301 = CARTESIAN_POINT('Ctrl Pts',(-19.9670619537043,-11.4834619097587,
122.34263870474)) ;
#72302 = CARTESIAN_POINT('Ctrl Pts',(-19.863504629617,-11.6734663122523,121.97420927489)) ;
#72303 = CARTESIAN_POINT('Ctrl Pts',(-19.7726633636097,-11.4934772318336,
122.261733686333)) ;
#72304 = CARTESIAN_POINT('Ctrl Pts',(-19.6061275734834,-11.6834966611526,
121.917323321507)) ;
#72305 = CARTESIAN_POINT('Ctrl Pts',(-19.5667619143694,-11.5035075807338,
122.216223718493)) ;
#72306 = CARTESIAN_POINT('Ctrl Pts',(-19.3477206075202,-11.6933400367592,
121.905682077729)) ;
#72307 = CARTESIAN_POINT('Ctrl Pts',(-19.3600373704475,-11.5133509563405,
122.206909440148)) ;
#72308 = CARTESIAN_POINT('Ctrl Pts',(-19.0862848802526,-11.7033694736564,
121.939135039811)) ;
#72309 = CARTESIAN_POINT('Ctrl Pts',(-19.1508885485966,-11.5233803932376,
122.233670378294)) ;
#72310 = CARTESIAN_POINT('Ctrl Pts',(-18.8347782583874,-11.7134013515893,
122.018183059093)) ;
#72311 = CARTESIAN_POINT('Ctrl Pts',(-18.9496827948867,-11.5334122711706,
122.296907572202)) ;
#72312 = CARTESIAN_POINT('Ctrl Pts',(-18.605313347461,-11.7232309746948,122.136772150878)) ;
#72313 = CARTESIAN_POINT('Ctrl Pts',(-18.7661111198526,-11.543241894276,122.391777125529)) ;
#72314 = CARTESIAN_POINT('Ctrl Pts',(-18.3960907644608,-11.7332204458479,
122.295336373502)) ;
#72315 = CARTESIAN_POINT('Ctrl Pts',(-18.5987322188273,-11.5532313654291,
122.518627168111)) ;
#72316 = CARTESIAN_POINT('Ctrl Pts',(-18.2171052462607,-11.7432642946103,
122.489315907986)) ;
#72317 = CARTESIAN_POINT('Ctrl Pts',(-18.4555426693397,-11.5632752141915,
122.673809908671)) ;
#72318 = CARTESIAN_POINT('Ctrl Pts',(-18.0772224087979,-11.753086000142,122.706227559869)) ;
#72319 = CARTESIAN_POINT('Ctrl Pts',(-18.3436356441143,-11.5730969197232,
122.847337557249)) ;
#72320 = CARTESIAN_POINT('Ctrl Pts',(-17.9743582755339,-11.7631210399698,
122.949047320003)) ;
#72321 = CARTESIAN_POINT('Ctrl Pts',(-18.2613427735164,-11.583131959551,123.041592794472)) ;
#72322 = CARTESIAN_POINT('Ctrl Pts',(-17.9159869175349,-11.7731457468612,
123.20594742871)) ;
#72323 = CARTESIAN_POINT('Ctrl Pts',(-18.2146441954026,-11.5931566664425,
123.247112562016)) ;
#72324 = CARTESIAN_POINT('Ctrl Pts',(-17.9027824759829,-11.782998451202,123.464529062488)) ;
#72325 = CARTESIAN_POINT('Ctrl Pts',(-18.2040790568452,-11.6030093707832,
123.453976982937)) ;
#72326 = CARTESIAN_POINT('Ctrl Pts',(-17.9346582754265,-11.7929865734097,
123.725044751909)) ;
#72327 = CARTESIAN_POINT('Ctrl Pts',(-18.2295779793896,-11.6129974929909,
123.662389596345)) ;
#72328 = CARTESIAN_POINT('Ctrl Pts',(-18.0108208429798,-11.802915043517,123.97459768502)) ;
#72329 = CARTESIAN_POINT('Ctrl Pts',(-18.290506276576,-11.6229259630982,123.862032045727)) ;
#72330 = CARTESIAN_POINT('Ctrl Pts',(-18.1294925171115,-11.8129040206842,
124.208755459199)) ;
#72331 = CARTESIAN_POINT('Ctrl Pts',(-18.3854419582014,-11.6329149402654,
124.049358946099)) ;
#72332 = CARTESIAN_POINT('Ctrl Pts',(-18.2881378410589,-11.8229418279639,
124.419490767669)) ;
#72333 = CARTESIAN_POINT('Ctrl Pts',(-18.5123568914905,-11.6429527475451,
124.217948275703)) ;
#72334 = CARTESIAN_POINT('Ctrl Pts',(-18.4770035096393,-11.8327881288271,
124.596360779288)) ;
#72335 = CARTESIAN_POINT('Ctrl Pts',(-18.6634476664908,-11.6527990484084,
124.359445074232)) ;
#72336 = CARTESIAN_POINT('Ctrl Pts',(-18.6973386410896,-11.8428138722065,
124.740820127124)) ;
#72337 = CARTESIAN_POINT('Ctrl Pts',(-18.8397147708248,-11.6628247917877,
124.47501413786)) ;
#72338 = CARTESIAN_POINT('Ctrl Pts',(-18.9398076656902,-11.8528447386455,
124.84425093062)) ;
#72339 = CARTESIAN_POINT('Ctrl Pts',(-19.0336893273778,-11.6728556582267,
124.557760414888)) ;
#72340 = CARTESIAN_POINT('Ctrl Pts',(-19.1914647637009,-11.8626820974443,
124.903358127401)) ;
#72341 = CARTESIAN_POINT('Ctrl Pts',(-19.2350138511474,-11.6826930170255,
124.605047798239)) ;
#72342 = CARTESIAN_POINT('Ctrl Pts',(-19.4535879451871,-11.872674058378,124.918802859936)) ;
#72343 = CARTESIAN_POINT('Ctrl Pts',(-19.4447121787566,-11.6926849779593,
124.617405527106)) ;
#72344 = CARTESIAN_POINT('Ctrl Pts',(-19.7154151681475,-11.8827064209346,
124.887849956771)) ;
#72345 = CARTESIAN_POINT('Ctrl Pts',(-19.6541742063547,-11.7027173405158,
124.592645060716)) ;
#72346 = CARTESIAN_POINT('Ctrl Pts',(-19.963751398213,-11.892571581509,124.813477415183)) ;
#72347 = CARTESIAN_POINT('Ctrl Pts',(-19.8528431830511,-11.7125825010902,
124.533149033972)) ;
#72348 = CARTESIAN_POINT('Ctrl Pts',(-20.1980246865073,-11.9025334860867,
124.696630723428)) ;
#72349 = CARTESIAN_POINT('Ctrl Pts',(-20.0402625347496,-11.7225444056679,
124.439673577518)) ;
#72350 = CARTESIAN_POINT('Ctrl Pts',(-20.4097188088808,-11.9125684161624,
124.539405883201)) ;
#72351 = CARTESIAN_POINT('Ctrl Pts',(-20.2096190243359,-11.7325793357437,
124.313895264542)) ;
#72352 = CARTESIAN_POINT('Ctrl Pts',(-20.5885436051697,-11.922453363016,124.350939834782)) ;
#72353 = CARTESIAN_POINT('Ctrl Pts',(-20.3526800140608,-11.7424642825973,
124.163124141174)) ;
#72354 = CARTESIAN_POINT('Ctrl Pts',(-20.7344544462776,-11.9325190393275,
124.13036082964)) ;
#72355 = CARTESIAN_POINT('Ctrl Pts',(-20.4694104306545,-11.7525299589087,
123.986661948345)) ;
#72356 = CARTESIAN_POINT('Ctrl Pts',(-20.8377538536608,-11.9423579589624,
123.89328858745)) ;
#72357 = CARTESIAN_POINT('Ctrl Pts',(-20.5520516016734,-11.7623688785436,
123.797005487303)) ;
#72358 = CARTESIAN_POINT('Ctrl Pts',(-20.9000168314442,-11.9524214686968,
123.636302931603)) ;
#72359 = CARTESIAN_POINT('Ctrl Pts',(-20.6018640323336,-11.7724323882781,
123.591417349548)) ;
#72360 = CARTESIAN_POINT('Ctrl Pts',(-20.9162207082288,-11.9623150818586,
123.376783859033)) ;
#72361 = CARTESIAN_POINT('Ctrl Pts',(-20.6148291614224,-11.7823260014398,
123.383802596767)) ;
#72362 = CARTESIAN_POINT('Ctrl Pts',(-20.887664564412,-11.972259088672,123.117066234083)) ;
#72363 = CARTESIAN_POINT('Ctrl Pts',(-20.5919863882844,-11.7922700082532,
123.176028481019)) ;
#72364 = CARTESIAN_POINT('Ctrl Pts',(-20.8141243156859,-11.9822600430263,
122.864708641766)) ;
#72365 = CARTESIAN_POINT('Ctrl Pts',(-20.5331562591136,-11.8022709626075,
122.974141872013)) ;
#72366 = CARTESIAN_POINT('Ctrl Pts',(-20.697050499779,-11.9922988007186,122.628327620954)) ;
#72367 = CARTESIAN_POINT('Ctrl Pts',(-20.4394990793776,-11.8123097202998,
122.78503611631)) ;
#72368 = CARTESIAN_POINT('Ctrl Pts',(-20.5444825752597,-12.0021229848886,
122.420035360942)) ;
#72369 = CARTESIAN_POINT('Ctrl Pts',(-20.3174467467038,-11.8221339044698,
122.618401417283)) ;
#72370 = CARTESIAN_POINT('Ctrl Pts',(-20.3539293396122,-12.012181050488,122.236896566253)) ;
#72371 = CARTESIAN_POINT('Ctrl Pts',(-20.1650056265507,-11.8321919700692,
122.471888771544)) ;
#72372 = CARTESIAN_POINT('Ctrl Pts',(-20.1370409747598,-12.0221110972627,
122.09176436793)) ;
#72373 = CARTESIAN_POINT('Ctrl Pts',(-19.9914963147766,-11.8421220168439,
122.355781349936)) ;
#72374 = CARTESIAN_POINT('Ctrl Pts',(-19.8980237231971,-12.0320625395998,
121.98564356461)) ;
#72375 = CARTESIAN_POINT('Ctrl Pts',(-19.8002835442428,-11.8520734591811,
122.270882756195)) ;
#72376 = CARTESIAN_POINT('Ctrl Pts',(-19.6416983085851,-12.0421093367791,
121.922384338885)) ;
#72377 = CARTESIAN_POINT('Ctrl Pts',(-19.5952237285874,-11.8621202563603,
122.220273262082)) ;
#72378 = CARTESIAN_POINT('Ctrl Pts',(-19.3835093232659,-12.0519572774592,
121.904703348249)) ;
#72379 = CARTESIAN_POINT('Ctrl Pts',(-19.3886730067727,-11.8719681970404,
122.206126303218)) ;
#72380 = CARTESIAN_POINT('Ctrl Pts',(-19.1231275997135,-12.0619189088018,
121.931627958195)) ;
#72381 = CARTESIAN_POINT('Ctrl Pts',(-19.1803674964563,-11.881929828383,122.227663754114)) ;
#72382 = CARTESIAN_POINT('Ctrl Pts',(-18.869747044229,-12.0719475681777,122.00416367076)) ;
#72383 = CARTESIAN_POINT('Ctrl Pts',(-18.9776624753786,-11.8919584877589,
122.28569018209)) ;
#72384 = CARTESIAN_POINT('Ctrl Pts',(-18.6355935849855,-12.0818578710659,
122.118142693062)) ;
#72385 = CARTESIAN_POINT('Ctrl Pts',(-18.7903388847647,-11.9018687906471,
122.376871325098)) ;
#72386 = CARTESIAN_POINT('Ctrl Pts',(-18.4238474019215,-12.0917927656281,
122.270883952983)) ;
#72387 = CARTESIAN_POINT('Ctrl Pts',(-18.6209407077585,-11.9118036852093,
122.49906244756)) ;
#72388 = CARTESIAN_POINT('Ctrl Pts',(-18.2400799717169,-12.101833864295,122.46023114314)) ;
#72389 = CARTESIAN_POINT('Ctrl Pts',(-18.4739251815215,-11.9218447838762,
122.650538612055)) ;
#72390 = CARTESIAN_POINT('Ctrl Pts',(-18.0940875092482,-12.1117211467993,
122.675182672161)) ;
#72391 = CARTESIAN_POINT('Ctrl Pts',(-18.3571294254557,-11.9317320663806,
122.822498468009)) ;
#72392 = CARTESIAN_POINT('Ctrl Pts',(-17.9861176822328,-12.1217128873099,
122.914511116788)) ;
#72393 = CARTESIAN_POINT('Ctrl Pts',(-18.2707515313325,-11.9417238068911,
123.013960245955)) ;
#72394 = CARTESIAN_POINT('Ctrl Pts',(-17.9216897295086,-12.1316634365453,
123.167952928715)) ;
#72395 = CARTESIAN_POINT('Ctrl Pts',(-18.2192070041483,-11.9516743561265,
123.216713069332)) ;
#72396 = CARTESIAN_POINT('Ctrl Pts',(-17.9018892647571,-12.1415991141801,
123.428284203219)) ;
#72397 = CARTESIAN_POINT('Ctrl Pts',(-18.203364387403,-11.9616100337613,123.424977867107)) ;
#72398 = CARTESIAN_POINT('Ctrl Pts',(-17.9274444397156,-12.1515845319728,
123.689463440896)) ;
#72399 = CARTESIAN_POINT('Ctrl Pts',(-18.2238062820509,-11.9715954515541,
123.633921427947)) ;
#72400 = CARTESIAN_POINT('Ctrl Pts',(-17.9985764204831,-12.1616133248434,
123.94322681677)) ;
#72401 = CARTESIAN_POINT('Ctrl Pts',(-18.2807096769127,-11.9816242444246,
123.836932670854)) ;
#72402 = CARTESIAN_POINT('Ctrl Pts',(-18.1107411249802,-12.1714928360713,
124.177366527425)) ;
#72403 = CARTESIAN_POINT('Ctrl Pts',(-18.3704394042732,-11.9915037556526,
124.024245403531)) ;
#72404 = CARTESIAN_POINT('Ctrl Pts',(-18.2631174664648,-12.1814863727443,
124.391272663534)) ;
#72405 = CARTESIAN_POINT('Ctrl Pts',(-18.4923386313118,-12.0014972923255,
124.195371583237)) ;
#72406 = CARTESIAN_POINT('Ctrl Pts',(-18.4514152852982,-12.1915186410081,
124.575779592077)) ;
#72407 = CARTESIAN_POINT('Ctrl Pts',(-18.6429752478029,-12.0115295605894,
124.342978676221)) ;
#72408 = CARTESIAN_POINT('Ctrl Pts',(-18.6649582254525,-12.201382603014,124.722768521375)) ;
#72409 = CARTESIAN_POINT('Ctrl Pts',(-18.813808386405,-12.0213935225952,124.460571699597)) ;
#72410 = CARTESIAN_POINT('Ctrl Pts',(-18.9056381213236,-12.2114526643589,
124.83271375166)) ;
#72411 = CARTESIAN_POINT('Ctrl Pts',(-19.0063512619196,-12.0314635839401,
124.548529868389)) ;
#72412 = CARTESIAN_POINT('Ctrl Pts',(-19.1560012005584,-12.2212950287076,
124.897694900667)) ;
#72413 = CARTESIAN_POINT('Ctrl Pts',(-19.2066412928752,-12.0413059482889,
124.600516988053)) ;
#72414 = CARTESIAN_POINT('Ctrl Pts',(-19.4168488001021,-12.2312557012101,
124.919426126798)) ;
#72415 = CARTESIAN_POINT('Ctrl Pts',(-19.4153192326186,-12.0512666207913,
124.617904150398)) ;
#72416 = CARTESIAN_POINT('Ctrl Pts',(-19.6794781670502,-12.2412937722779,
124.894826056508)) ;
#72417 = CARTESIAN_POINT('Ctrl Pts',(-19.6254228033852,-12.0613046918591,
124.598226319022)) ;
#72418 = CARTESIAN_POINT('Ctrl Pts',(-19.9298584470628,-12.2511673872383,
124.826609084819)) ;
#72419 = CARTESIAN_POINT('Ctrl Pts',(-19.82572781557,-12.0711783068196,124.543654773306)) ;
#72420 = CARTESIAN_POINT('Ctrl Pts',(-20.1692027686012,-12.2612396218196,
124.713703674944)) ;
#72421 = CARTESIAN_POINT('Ctrl Pts',(-20.0172039403952,-12.0812505414008,
124.45333259084)) ;
#72422 = CARTESIAN_POINT('Ctrl Pts',(-20.3802336085162,-12.2710636402683,
124.564901741631)) ;
#72423 = CARTESIAN_POINT('Ctrl Pts',(-20.1860304834579,-12.0910745598496,
124.334292311524)) ;
#72424 = CARTESIAN_POINT('Ctrl Pts',(-20.5668505339753,-12.2811285612444,
124.37754684746)) ;
#72425 = CARTESIAN_POINT('Ctrl Pts',(-20.3353241585353,-12.1011394808256,
124.184411132778)) ;
#72426 = CARTESIAN_POINT('Ctrl Pts',(-20.7654710389229,-12.2943388595391,
124.09273138074)) ;
#72427 = CARTESIAN_POINT('Ctrl Pts',(-20.4942292379436,-12.1143497791204,
123.9565547192)) ;
#72428 = CARTESIAN_POINT('Ctrl Pts',(-20.8864681735863,-12.3076543062711,
123.760293059353)) ;
#72429 = CARTESIAN_POINT('Ctrl Pts',(-20.5910323501045,-12.1276652258523,
123.690569694297)) ;
#72430 = CARTESIAN_POINT('Ctrl Pts',(-20.9168412403421,-12.3209445515383,
123.412248798329)) ;
#72431 = CARTESIAN_POINT('Ctrl Pts',(-20.6153241110925,-12.1409554711196,
123.412181858016)) ;
#72432 = CARTESIAN_POINT('Ctrl Pts',(-20.8936136565225,-12.3309953011455,
123.149204261567)) ;
#72433 = CARTESIAN_POINT('Ctrl Pts',(-20.5967459980804,-12.1510062207267,
123.20173670269)) ;
#72434 = CARTESIAN_POINT('Ctrl Pts',(-20.8271599101353,-12.3408079081277,
122.900008574074)) ;
#72435 = CARTESIAN_POINT('Ctrl Pts',(-20.5435845615401,-12.160818827709,123.002381693859)) ;
#72436 = CARTESIAN_POINT('Ctrl Pts',(-20.7159339873303,-12.350879006122,122.659895486388)) ;
#72437 = CARTESIAN_POINT('Ctrl Pts',(-20.4546048866285,-12.1708899257032,
122.810289464688)) ;
#72438 = CARTESIAN_POINT('Ctrl Pts',(-20.567182547186,-12.3607685788968,122.446765213272)) ;
#72439 = CARTESIAN_POINT('Ctrl Pts',(-20.3356088789073,-12.1807794984781,
122.639785845869)) ;
#72440 = CARTESIAN_POINT('Ctrl Pts',(-20.3217335958412,-12.3740386857001,
122.1990367701)) ;
#72441 = CARTESIAN_POINT('Ctrl Pts',(-20.1392327070889,-12.1940496052814,
122.441591581826)) ;
#72442 = CARTESIAN_POINT('Ctrl Pts',(-19.9402799223617,-12.3906553726226,
121.976489963094)) ;
#72443 = CARTESIAN_POINT('Ctrl Pts',(-19.8341061887492,-12.2106662922039,
122.263562894215)) ;
#72444 = CARTESIAN_POINT('Ctrl Pts',(-19.5069560654144,-12.4072294159389,
121.897341845793)) ;
#72445 = CARTESIAN_POINT('Ctrl Pts',(-19.4873858330109,-12.2272403355201,
122.200234744545)) ;
#72446 = CARTESIAN_POINT('Ctrl Pts',(-19.1586250795986,-12.4205259833707,
121.925240968609)) ;
#72447 = CARTESIAN_POINT('Ctrl Pts',(-19.2087707820573,-12.2405369029519,
122.222555129474)) ;
#72448 = CARTESIAN_POINT('Ctrl Pts',(-18.903549791528,-12.4305560469481,121.991664800818)) ;
#72449 = CARTESIAN_POINT('Ctrl Pts',(-19.0046999503751,-12.2505669665293,
122.275692101065)) ;
#72450 = CARTESIAN_POINT('Ctrl Pts',(-18.6671468528591,-12.4404499387973,
122.099840645891)) ;
#72451 = CARTESIAN_POINT('Ctrl Pts',(-18.8155801630729,-12.2604608583786,
122.362230133135)) ;
#72452 = CARTESIAN_POINT('Ctrl Pts',(-18.3796682060552,-12.4537026945829,
122.296549637397)) ;
#72453 = CARTESIAN_POINT('Ctrl Pts',(-18.5855889437377,-12.2737136141641,
122.519603145883)) ;
#72454 = CARTESIAN_POINT('Ctrl Pts',(-18.0908280312836,-12.4704307995753,
122.63446210067)) ;
#72455 = CARTESIAN_POINT('Ctrl Pts',(-18.3545219823308,-12.2904417191566,
122.789922698833)) ;
#72456 = CARTESIAN_POINT('Ctrl Pts',(-17.9056069776855,-12.4902616360538,
123.128014485506)) ;
#72457 = CARTESIAN_POINT('Ctrl Pts',(-18.2063394436304,-12.3102725556351,
123.184767136768)) ;
#72458 = CARTESIAN_POINT('Ctrl Pts',(-17.8986058473091,-12.5101870279439,
123.657435239685)) ;
#72459 = CARTESIAN_POINT('Ctrl Pts',(-18.2007363231524,-12.3301979475252,
123.608303576448)) ;
#72460 = CARTESIAN_POINT('Ctrl Pts',(-18.0728134811667,-12.530112241296,124.157630024476)) ;
#72461 = CARTESIAN_POINT('Ctrl Pts',(-18.3400999156776,-12.3501231608772,
124.00846101179)) ;
#72462 = CARTESIAN_POINT('Ctrl Pts',(-18.407056128328,-12.5500372547811,124.568319257419)) ;
#72463 = CARTESIAN_POINT('Ctrl Pts',(-18.6074925126866,-12.3700481743623,
124.337014427016)) ;
#72464 = CARTESIAN_POINT('Ctrl Pts',(-18.8599799730915,-12.5699137264811,
124.840308097054)) ;
#72465 = CARTESIAN_POINT('Ctrl Pts',(-18.9698314340081,-12.3899246460623,
124.554607919997)) ;
#72466 = CARTESIAN_POINT('Ctrl Pts',(-19.3811313633276,-12.5898930443899,
124.94215813979)) ;
#72467 = CARTESIAN_POINT('Ctrl Pts',(-19.3867523851537,-12.4099039639712,
124.636089848104)) ;
#72468 = CARTESIAN_POINT('Ctrl Pts',(-19.904526260355,-12.6098260479659,124.859844414559)) ;
#72469 = CARTESIAN_POINT('Ctrl Pts',(-19.8054692095567,-12.4298369675472,
124.570240637955)) ;
#72470 = CARTESIAN_POINT('Ctrl Pts',(-20.3677432424787,-12.6297213179936,
124.604878989374)) ;
#72471 = CARTESIAN_POINT('Ctrl Pts',(-20.1760444928505,-12.4497322375749,
124.366269105617)) ;
#72472 = CARTESIAN_POINT('Ctrl Pts',(-20.7170498596776,-12.6496426558995,
124.206944794336)) ;
#72473 = CARTESIAN_POINT('Ctrl Pts',(-20.4554911883008,-12.4696535754807,
124.047921837557)) ;
#72474 = CARTESIAN_POINT('Ctrl Pts',(-20.9098403566524,-12.6696002791656,
123.71275120436)) ;
#72475 = CARTESIAN_POINT('Ctrl Pts',(-20.6097246738742,-12.4896111987469,
123.652566906432)) ;
#72476 = CARTESIAN_POINT('Ctrl Pts',(-20.922485985097,-12.6894801111229,123.184612097155)) ;
#72477 = CARTESIAN_POINT('Ctrl Pts',(-20.6198419805455,-12.5094910307041,
123.230054122359)) ;
#72478 = CARTESIAN_POINT('Ctrl Pts',(-20.7554545445887,-12.7093619624198,
122.683172172791)) ;
#72479 = CARTESIAN_POINT('Ctrl Pts',(-20.4862161995466,-12.529372882001,122.828900805559)) ;
#72480 = CARTESIAN_POINT('Ctrl Pts',(-20.4235254244921,-12.7294329795236,
122.265649140975)) ;
#72481 = CARTESIAN_POINT('Ctrl Pts',(-20.2206735911977,-12.5494438991048,
122.494883034392)) ;
#72482 = CARTESIAN_POINT('Ctrl Pts',(-19.9749237655552,-12.7492402032767,
121.989968961394)) ;
#72483 = CARTESIAN_POINT('Ctrl Pts',(-19.8617900839095,-12.5692511228579,
122.274337697005)) ;
#72484 = CARTESIAN_POINT('Ctrl Pts',(-19.4550399386811,-12.7692213388454,
121.881799009458)) ;
#72485 = CARTESIAN_POINT('Ctrl Pts',(-19.4458826423283,-12.5892322584267,
122.18780260183)) ;
#72486 = CARTESIAN_POINT('Ctrl Pts',(-18.9310095255379,-12.7891488321847,
121.958350587215)) ;
#72487 = CARTESIAN_POINT('Ctrl Pts',(-19.0266575304228,-12.6091597517659,
122.24904461452)) ;
#72488 = CARTESIAN_POINT('Ctrl Pts',(-18.4660378435097,-12.8089694935425,
122.206286369138)) ;
#72489 = CARTESIAN_POINT('Ctrl Pts',(-18.6546792788745,-12.6289804131237,
122.447395528075)) ;
#72490 = CARTESIAN_POINT('Ctrl Pts',(-18.1095237057662,-12.8290666827643,
122.603786127355)) ;
#72491 = CARTESIAN_POINT('Ctrl Pts',(-18.3694696834846,-12.6490776023455,
122.765395547961)) ;
#72492 = CARTESIAN_POINT('Ctrl Pts',(-17.9128685241176,-12.8488303617726,
123.091145395857)) ;
#72493 = CARTESIAN_POINT('Ctrl Pts',(-18.212146236786,-12.6688412813539,123.155285756016)) ;
#72494 = CARTESIAN_POINT('Ctrl Pts',(-17.8934532249177,-12.8688876404457,
123.623648070247)) ;
#72495 = CARTESIAN_POINT('Ctrl Pts',(-18.1966161448372,-12.6888985600269,
123.581287459871)) ;
#72496 = CARTESIAN_POINT('Ctrl Pts',(-18.0551868057906,-12.8886830641931,
124.124451004265)) ;
#72497 = CARTESIAN_POINT('Ctrl Pts',(-18.3260055893083,-12.7086939837743,
123.981930874229)) ;
#72498 = CARTESIAN_POINT('Ctrl Pts',(-18.379428806349,-12.9086467089207,124.544379679897)) ;
#72499 = CARTESIAN_POINT('Ctrl Pts',(-18.5854015952883,-12.7286576285019,
124.317872293328)) ;
#72500 = CARTESIAN_POINT('Ctrl Pts',(-18.8287006511191,-12.9286302001948,
124.827680379783)) ;
#72501 = CARTESIAN_POINT('Ctrl Pts',(-18.9448205353017,-12.748641119776,124.544510768176)) ;
#72502 = CARTESIAN_POINT('Ctrl Pts',(-19.342918686626,-12.9484376953441,124.940731620075)) ;
#72503 = CARTESIAN_POINT('Ctrl Pts',(-19.3561969576373,-12.7684486149253,
124.634949144309)) ;
#72504 = CARTESIAN_POINT('Ctrl Pts',(-19.8693844497471,-12.9684202860642,
124.871533418485)) ;
#72505 = CARTESIAN_POINT('Ctrl Pts',(-19.7773692207012,-12.7884312056454,
124.579587326227)) ;
#72506 = CARTESIAN_POINT('Ctrl Pts',(-20.3384447755248,-12.9883029400554,
124.627871581424)) ;
#72507 = CARTESIAN_POINT('Ctrl Pts',(-20.1526165530644,-12.8083138596367,
124.384654591439)) ;
#72508 = CARTESIAN_POINT('Ctrl Pts',(-20.6976976848922,-13.0082611849185,
124.237731507695)) ;
#72509 = CARTESIAN_POINT('Ctrl Pts',(-20.4400164509615,-12.8282721044997,
124.072539967842)) ;
#72510 = CARTESIAN_POINT('Ctrl Pts',(-20.9017768870184,-13.0281367719601,
123.750397269465)) ;
#72511 = CARTESIAN_POINT('Ctrl Pts',(-20.6032766081325,-12.8481476915413,
123.682670590867)) ;
#72512 = CARTESIAN_POINT('Ctrl Pts',(-20.9278087944924,-13.0481176600953,
123.220011471914)) ;
#72513 = CARTESIAN_POINT('Ctrl Pts',(-20.6240984650254,-12.8681285796766,
123.258361753543)) ;
#72514 = CARTESIAN_POINT('Ctrl Pts',(-20.7712144054665,-13.0680528012063,
122.713763278184)) ;
#72515 = CARTESIAN_POINT('Ctrl Pts',(-20.4988186174616,-12.8880637207876,
122.853363994619)) ;
#72516 = CARTESIAN_POINT('Ctrl Pts',(-20.4520106816662,-13.0879648192174,
122.291696114203)) ;
#72517 = CARTESIAN_POINT('Ctrl Pts',(-20.2434545045575,-12.9079757387987,
122.515712746724)) ;
#72518 = CARTESIAN_POINT('Ctrl Pts',(-20.0087285877689,-13.107853037461,122.003722192622)) ;
#72519 = CARTESIAN_POINT('Ctrl Pts',(-19.8888179313836,-12.9278639570422,
122.285335578687)) ;
#72520 = CARTESIAN_POINT('Ctrl Pts',(-19.5791090604669,-13.1244513413079,
121.903703056127)) ;
#72521 = CARTESIAN_POINT('Ctrl Pts',(-19.5451473403849,-12.9444622608891,
122.20532771232)) ;
#72522 = CARTESIAN_POINT('Ctrl Pts',(-19.2304680801344,-13.1377239312107,
121.914976366531)) ;
#72523 = CARTESIAN_POINT('Ctrl Pts',(-19.2662110826215,-12.957734850792,122.214345972793)) ;
#72524 = CARTESIAN_POINT('Ctrl Pts',(-18.9730360739055,-13.1477313461616,
121.968723010313)) ;
#72525 = CARTESIAN_POINT('Ctrl Pts',(-19.0602727214037,-12.9677422657428,
122.25734421058)) ;
#72526 = CARTESIAN_POINT('Ctrl Pts',(-18.728923774741,-13.1577386928942,122.066570256233)) ;
#72527 = CARTESIAN_POINT('Ctrl Pts',(-18.8649743141328,-12.9777496124754,
122.335631001214)) ;
#72528 = CARTESIAN_POINT('Ctrl Pts',(-18.4326373531088,-13.1710050526958,
122.250316913769)) ;
#72529 = CARTESIAN_POINT('Ctrl Pts',(-18.6279877739114,-12.991015972277,122.482594753417)) ;
#72530 = CARTESIAN_POINT('Ctrl Pts',(-18.1316373287042,-13.1875197103187,
122.569692622232)) ;
#72531 = CARTESIAN_POINT('Ctrl Pts',(-18.3871406493088,-13.0075306299,122.738147077933)) ;
#72532 = CARTESIAN_POINT('Ctrl Pts',(-17.9558681006143,-13.2041171435614,
122.974265631464)) ;
#72533 = CARTESIAN_POINT('Ctrl Pts',(-18.2465546550527,-13.0241280631426,
123.061762709622)) ;
#72534 = CARTESIAN_POINT('Ctrl Pts',(-17.9045373895887,-13.2174651407064,
123.321302564887)) ;
#72535 = CARTESIAN_POINT('Ctrl Pts',(-18.20548016203,-13.0374760602876,123.339423056025)) ;
#72536 = CARTESIAN_POINT('Ctrl Pts',(-17.9113737957026,-13.227360895058,123.581262925392)) ;
#72537 = CARTESIAN_POINT('Ctrl Pts',(-18.2109541050246,-13.0473718146392,
123.547385244145)) ;
#72538 = CARTESIAN_POINT('Ctrl Pts',(-17.9634088820115,-13.2373488489893,
123.838506352565)) ;
#72539 = CARTESIAN_POINT('Ctrl Pts',(-18.2525836755494,-13.0573597685706,
123.753181135679)) ;
#72540 = CARTESIAN_POINT('Ctrl Pts',(-18.0589349738846,-13.2473060726941,
124.082144873692)) ;
#72541 = CARTESIAN_POINT('Ctrl Pts',(-18.3290068212281,-13.0673169922753,
123.948090676495)) ;
#72542 = CARTESIAN_POINT('Ctrl Pts',(-18.1964661585353,-13.2573416192507,
124.307146372521)) ;
#72543 = CARTESIAN_POINT('Ctrl Pts',(-18.4390335973166,-13.077352538832,124.128090758229)) ;
#72544 = CARTESIAN_POINT('Ctrl Pts',(-18.368270053298,-13.2672287305268,124.502082982774)) ;
#72545 = CARTESIAN_POINT('Ctrl Pts',(-18.576478424902,-13.0872396501081,124.284038539208)) ;
#72546 = CARTESIAN_POINT('Ctrl Pts',(-18.5731686000291,-13.2772201356277,
124.66624633591)) ;
#72547 = CARTESIAN_POINT('Ctrl Pts',(-18.7403986257916,-13.0972310552089,
124.415367430382)) ;
#72548 = CARTESIAN_POINT('Ctrl Pts',(-18.8024527486547,-13.2871657568424,
124.791696662214)) ;
#72549 = CARTESIAN_POINT('Ctrl Pts',(-18.9238269941468,-13.1071766764237,
124.515725689855)) ;
#72550 = CARTESIAN_POINT('Ctrl Pts',(-19.0499707909239,-13.2971150051108,
124.875968223261)) ;
#72551 = CARTESIAN_POINT('Ctrl Pts',(-19.1218420945713,-13.117125924692,124.58314078008)) ;
#72552 = CARTESIAN_POINT('Ctrl Pts',(-19.3109074952324,-13.3071615002794,
124.916064204563)) ;
#72553 = CARTESIAN_POINT('Ctrl Pts',(-19.3305917563602,-13.1271724198607,
124.615215324585)) ;
#72554 = CARTESIAN_POINT('Ctrl Pts',(-19.5697458477352,-13.3170128430709,
124.910614060222)) ;
#72555 = CARTESIAN_POINT('Ctrl Pts',(-19.5376622956873,-13.1370237626522,
124.610852953311)) ;
#72556 = CARTESIAN_POINT('Ctrl Pts',(-19.8268961278623,-13.3269846231983,
124.86034740177)) ;
#72557 = CARTESIAN_POINT('Ctrl Pts',(-19.7433819968767,-13.1469955427795,
124.570637436565)) ;
#72558 = CARTESIAN_POINT('Ctrl Pts',(-20.0720441859134,-13.336979823176,124.76592134673)) ;
#72559 = CARTESIAN_POINT('Ctrl Pts',(-19.9394995773028,-13.1569907427572,
124.495094521128)) ;
#72560 = CARTESIAN_POINT('Ctrl Pts',(-20.2977248332658,-13.347013814872,124.629595035423)) ;
#72561 = CARTESIAN_POINT('Ctrl Pts',(-20.1200429020722,-13.1670247344533,
124.386031555564)) ;
#72562 = CARTESIAN_POINT('Ctrl Pts',(-20.4930785404937,-13.3568692198445,
124.459519571189)) ;
#72563 = CARTESIAN_POINT('Ctrl Pts',(-20.2763242533844,-13.1768801394258,
124.2499696171)) ;
#72564 = CARTESIAN_POINT('Ctrl Pts',(-20.6585461152762,-13.3668685176903,
124.255447402395)) ;
#72565 = CARTESIAN_POINT('Ctrl Pts',(-20.4086965325383,-13.1868794372715,
124.086710531574)) ;
#72566 = CARTESIAN_POINT('Ctrl Pts',(-20.7850259764522,-13.3767636302955,
124.028196369729)) ;
#72567 = CARTESIAN_POINT('Ctrl Pts',(-20.509878386038,-13.1967745498767,123.904908812571)) ;
#72568 = CARTESIAN_POINT('Ctrl Pts',(-20.8714967333463,-13.3868242758305,
123.778389961142)) ;
#72569 = CARTESIAN_POINT('Ctrl Pts',(-20.5790529024792,-13.2068351954117,
123.705062936695)) ;
#72570 = CARTESIAN_POINT('Ctrl Pts',(-20.9125557495548,-13.3966731528197,
123.522828864948)) ;
#72571 = CARTESIAN_POINT('Ctrl Pts',(-20.6118978858686,-13.2166840724009,
123.500614018673)) ;
#72572 = CARTESIAN_POINT('Ctrl Pts',(-20.9092102412474,-13.4067018639133,
123.259309807955)) ;
#72573 = CARTESIAN_POINT('Ctrl Pts',(-20.60921931471,-13.2267127834945,123.289798833326)) ;
#72574 = CARTESIAN_POINT('Ctrl Pts',(-20.8594509751279,-13.4167312651694,
123.000482346254)) ;
#72575 = CARTESIAN_POINT('Ctrl Pts',(-20.5694097280133,-13.2367421847506,
123.082737285215)) ;
#72576 = CARTESIAN_POINT('Ctrl Pts',(-20.7678172836453,-13.4265714569654,
122.758667592134)) ;
#72577 = CARTESIAN_POINT('Ctrl Pts',(-20.4961008807738,-13.2465823765466,
122.889286615854)) ;
#72578 = CARTESIAN_POINT('Ctrl Pts',(-20.6338292437807,-13.4365748861584,
122.532528062979)) ;
#72579 = CARTESIAN_POINT('Ctrl Pts',(-20.3889086516706,-13.2565858057396,
122.708376145626)) ;
#72580 = CARTESIAN_POINT('Ctrl Pts',(-20.4628072718296,-13.4465603986246,
122.333446821081)) ;
#72581 = CARTESIAN_POINT('Ctrl Pts',(-20.2520895182278,-13.2665713182058,
122.549112622993)) ;
#72582 = CARTESIAN_POINT('Ctrl Pts',(-20.2585721952877,-13.4566014950085,
122.166409914503)) ;
#72583 = CARTESIAN_POINT('Ctrl Pts',(-20.0887000684384,-13.2766124145898,
122.415484760473)) ;
#72584 = CARTESIAN_POINT('Ctrl Pts',(-20.0331061121513,-13.4664446909596,
122.039577187864)) ;
#72585 = CARTESIAN_POINT('Ctrl Pts',(-19.9083265551085,-13.2864556105408,
122.314020659262)) ;
#72586 = CARTESIAN_POINT('Ctrl Pts',(-19.7857320971706,-13.476431002014,121.952101012355)) ;
#72587 = CARTESIAN_POINT('Ctrl Pts',(-19.7104267699532,-13.2964419215952,
122.2440417256)) ;
#72588 = CARTESIAN_POINT('Ctrl Pts',(-19.5282010411942,-13.4863656872717,
121.908939846923)) ;
#72589 = CARTESIAN_POINT('Ctrl Pts',(-19.5044018436985,-13.3063766068529,
122.209514865674)) ;
#72590 = CARTESIAN_POINT('Ctrl Pts',(-19.2639488168524,-13.4964232484887,
121.911409438733)) ;
#72591 = CARTESIAN_POINT('Ctrl Pts',(-19.2929999897462,-13.31643416807,122.211492628297)) ;
#72592 = CARTESIAN_POINT('Ctrl Pts',(-19.010096667528,-13.5062448900973,121.958214888059)) ;
#72593 = CARTESIAN_POINT('Ctrl Pts',(-19.0899192590891,-13.3262558096786,
122.248938879444)) ;
#72594 = CARTESIAN_POINT('Ctrl Pts',(-18.7623301681883,-13.5163009536883,
122.050058119872)) ;
#72595 = CARTESIAN_POINT('Ctrl Pts',(-18.8917066650352,-13.3363118732695,
122.322415354375)) ;
#72596 = CARTESIAN_POINT('Ctrl Pts',(-18.5371012425421,-13.5262416294501,
122.182417857211)) ;
#72597 = CARTESIAN_POINT('Ctrl Pts',(-18.7115247897244,-13.3462525490313,
122.428304768289)) ;
#72598 = CARTESIAN_POINT('Ctrl Pts',(-18.3384782455445,-13.5361459882384,
122.350628473845)) ;
#72599 = CARTESIAN_POINT('Ctrl Pts',(-18.5526279681694,-13.3561569078197,
122.562874462125)) ;
#72600 = CARTESIAN_POINT('Ctrl Pts',(-18.1698329825616,-13.5461926428142,
122.553733855512)) ;
#72601 = CARTESIAN_POINT('Ctrl Pts',(-18.4177132105659,-13.3662035623955,
122.725360081205)) ;
#72602 = CARTESIAN_POINT('Ctrl Pts',(-18.0407519035807,-13.5560882374571,
122.779526388137)) ;
#72603 = CARTESIAN_POINT('Ctrl Pts',(-18.314450248629,-13.3760991570383,122.905994658498)) ;
#72604 = CARTESIAN_POINT('Ctrl Pts',(-17.9513576420596,-13.5661501841139,
123.028342279831)) ;
#72605 = CARTESIAN_POINT('Ctrl Pts',(-18.2429366010411,-13.3861611036952,
123.105048152778)) ;
#72606 = CARTESIAN_POINT('Ctrl Pts',(-17.9074152112643,-13.5759998080461,
123.283436990163)) ;
#72607 = CARTESIAN_POINT('Ctrl Pts',(-18.2077846559609,-13.3960107276274,
123.30912358981)) ;
#72608 = CARTESIAN_POINT('Ctrl Pts',(-17.9075794489119,-13.5859630470759,
123.545245160126)) ;
#72609 = CARTESIAN_POINT('Ctrl Pts',(-18.2079178311045,-13.4059739666572,
123.518569875125)) ;
#72610 = CARTESIAN_POINT('Ctrl Pts',(-17.953843845115,-13.5959876218518,123.804601716879)) ;
#72611 = CARTESIAN_POINT('Ctrl Pts',(-18.2449311618866,-13.415998541433,123.726054822038)) ;
#72612 = CARTESIAN_POINT('Ctrl Pts',(-18.0433151853354,-13.6059061845395,
124.049406829339)) ;
#72613 = CARTESIAN_POINT('Ctrl Pts',(-18.3165097898856,-13.4259171041207,
123.921897880132)) ;
#72614 = CARTESIAN_POINT('Ctrl Pts',(-18.1745142882444,-13.6158983712635,
124.276882942857)) ;
#72615 = CARTESIAN_POINT('Ctrl Pts',(-18.4214705117975,-13.4359092908447,
124.103877785203)) ;
#72616 = CARTESIAN_POINT('Ctrl Pts',(-18.3442843563145,-13.6259331698477,
124.478655912782)) ;
#72617 = CARTESIAN_POINT('Ctrl Pts',(-18.5572880000568,-13.4459440894289,
124.265295042287)) ;
#72618 = CARTESIAN_POINT('Ctrl Pts',(-18.542628717793,-13.6357883605213,124.645217964086)) ;
#72619 = CARTESIAN_POINT('Ctrl Pts',(-18.7159640464026,-13.4557992801026,
124.398542876088)) ;
#72620 = CARTESIAN_POINT('Ctrl Pts',(-18.7699291705577,-13.6457877086743,
124.776978497938)) ;
#72621 = CARTESIAN_POINT('Ctrl Pts',(-18.8978051604027,-13.4657986282556,
124.503949791851)) ;
#72622 = CARTESIAN_POINT('Ctrl Pts',(-19.0140681533334,-13.6556828343495,
124.86662328355)) ;
#72623 = CARTESIAN_POINT('Ctrl Pts',(-19.0931163563245,-13.4756937539307,
124.57566388753)) ;
#72624 = CARTESIAN_POINT('Ctrl Pts',(-19.2742712713138,-13.6657433772976,
124.913241818075)) ;
#72625 = CARTESIAN_POINT('Ctrl Pts',(-19.3012793296211,-13.4857542968788,
124.612957136434)) ;
#72626 = CARTESIAN_POINT('Ctrl Pts',(-19.5331191648045,-13.6755926515645,
124.914103544995)) ;
#72627 = CARTESIAN_POINT('Ctrl Pts',(-19.5083568152058,-13.4956035711457,
124.613644905364)) ;
#72628 = CARTESIAN_POINT('Ctrl Pts',(-19.7928781485179,-13.6856198761344,
124.869872597729)) ;
#72629 = CARTESIAN_POINT('Ctrl Pts',(-19.7161637833577,-13.5056307957156,
124.578258678487)) ;
#72630 = CARTESIAN_POINT('Ctrl Pts',(-20.0408282969086,-13.6956482753222,
124.780544744238)) ;
#72631 = CARTESIAN_POINT('Ctrl Pts',(-19.9145234061736,-13.5156591949034,
124.506794855646)) ;
#72632 = CARTESIAN_POINT('Ctrl Pts',(-20.2655486147192,-13.7054940257356,
124.652339842783)) ;
#72633 = CARTESIAN_POINT('Ctrl Pts',(-20.0942981282645,-13.5255049453169,
124.404230053982)) ;
#72634 = CARTESIAN_POINT('Ctrl Pts',(-20.4679785319136,-13.7154828161364,
124.485209945388)) ;
#72635 = CARTESIAN_POINT('Ctrl Pts',(-20.2562410584806,-13.5354937357177,
124.270525177274)) ;
#72636 = CARTESIAN_POINT('Ctrl Pts',(-20.6387470355723,-13.7255277445361,
124.283933112309)) ;
#72637 = CARTESIAN_POINT('Ctrl Pts',(-20.3928547958644,-13.5455386641174,
124.109502630356)) ;
#72638 = CARTESIAN_POINT('Ctrl Pts',(-20.7695822851755,-13.7353522293251,
124.061344007619)) ;
#72639 = CARTESIAN_POINT('Ctrl Pts',(-20.4975212694255,-13.5553631489063,
123.931431547031)) ;
#72640 = CARTESIAN_POINT('Ctrl Pts',(-20.8622650302476,-13.7454096268663,
123.813853115584)) ;
#72641 = CARTESIAN_POINT('Ctrl Pts',(-20.5716663117887,-13.5654205464475,
123.733438175729)) ;
#72642 = CARTESIAN_POINT('Ctrl Pts',(-20.9096073545619,-13.7553357184525,
123.557318498513)) ;
#72643 = CARTESIAN_POINT('Ctrl Pts',(-20.6095387227254,-13.5753466380337,
123.528210720789)) ;
#72644 = CARTESIAN_POINT('Ctrl Pts',(-20.9123708211663,-13.765290503597,123.295734355716)) ;
#72645 = CARTESIAN_POINT('Ctrl Pts',(-20.6117482517937,-13.5853014231783,
123.318943754624)) ;
#72646 = CARTESIAN_POINT('Ctrl Pts',(-20.8690285857303,-13.7753278732547,
123.035549479077)) ;
#72647 = CARTESIAN_POINT('Ctrl Pts',(-20.5770731610732,-13.5953387928359,
123.110795969221)) ;
#72648 = CARTESIAN_POINT('Ctrl Pts',(-20.7826546062724,-13.7852166833763,
122.790448432896)) ;
#72649 = CARTESIAN_POINT('Ctrl Pts',(-20.5079730348007,-13.6052276029575,
122.914716243319)) ;
#72650 = CARTESIAN_POINT('Ctrl Pts',(-20.6541544833678,-13.7952060424273,
122.561546360063)) ;
#72651 = CARTESIAN_POINT('Ctrl Pts',(-20.4051720120301,-13.6152169620086,
122.731595301545)) ;
#72652 = CARTESIAN_POINT('Ctrl Pts',(-20.4882245282182,-13.8051645898834,
122.359184923962)) ;
#72653 = CARTESIAN_POINT('Ctrl Pts',(-20.2724273390847,-13.6251755094647,
122.569707182105)) ;
#72654 = CARTESIAN_POINT('Ctrl Pts',(-20.2912542116433,-13.8150641664345,
122.189215690087)) ;
#72655 = CARTESIAN_POINT('Ctrl Pts',(-20.1148509292206,-13.6350750860157,
122.433733053993)) ;
#72656 = CARTESIAN_POINT('Ctrl Pts',(-20.0644048945388,-13.8251120782652,
122.054135819841)) ;
#72657 = CARTESIAN_POINT('Ctrl Pts',(-19.9333707741338,-13.6451229978464,
122.325669994257)) ;
#72658 = CARTESIAN_POINT('Ctrl Pts',(-19.8213040212545,-13.8350074261257,
121.961702812334)) ;
#72659 = CARTESIAN_POINT('Ctrl Pts',(-19.7388903925254,-13.655018345707,122.251724810852)) ;
#72660 = CARTESIAN_POINT('Ctrl Pts',(-19.5616299166023,-13.8450691026569,
121.912040392366)) ;
#72661 = CARTESIAN_POINT('Ctrl Pts',(-19.5311506601532,-13.6650800222382,
122.211995830886)) ;
#72662 = CARTESIAN_POINT('Ctrl Pts',(-19.3029437659874,-13.8549136204061,
121.908260248707)) ;
#72663 = CARTESIAN_POINT('Ctrl Pts',(-19.3242027824673,-13.6749245399873,
122.208972745531)) ;
#72664 = CARTESIAN_POINT('Ctrl Pts',(-19.0443926106545,-13.8648740641208,
121.949016797518)) ;
#72665 = CARTESIAN_POINT('Ctrl Pts',(-19.1173623421421,-13.6848849837021,
122.241578712485)) ;
#72666 = CARTESIAN_POINT('Ctrl Pts',(-18.7951065532915,-13.8749108969391,
122.035163624188)) ;
#72667 = CARTESIAN_POINT('Ctrl Pts',(-18.9179336758563,-13.6949218165203,
122.310497076572)) ;
#72668 = CARTESIAN_POINT('Ctrl Pts',(-18.5679607592285,-13.8847896936859,
122.160911880391)) ;
#72669 = CARTESIAN_POINT('Ctrl Pts',(-18.7362182015604,-13.7048006132671,
122.411095961693)) ;
#72670 = CARTESIAN_POINT('Ctrl Pts',(-18.3623992980215,-13.8948490098142,
122.327074678638)) ;
#72671 = CARTESIAN_POINT('Ctrl Pts',(-18.5717693261378,-13.7148599293955,
122.544026976484)) ;
#72672 = CARTESIAN_POINT('Ctrl Pts',(-18.1920392190739,-13.9047194565674,
122.522692233417)) ;
#72673 = CARTESIAN_POINT('Ctrl Pts',(-18.4354824658003,-13.7247303761487,
122.700520842774)) ;
#72674 = CARTESIAN_POINT('Ctrl Pts',(-18.0559754686605,-13.9147120948255,
122.747289602254)) ;
#72675 = CARTESIAN_POINT('Ctrl Pts',(-18.3266320713964,-13.7347230144067,
122.880198925302)) ;
#72676 = CARTESIAN_POINT('Ctrl Pts',(-17.9611352242736,-13.9247441103734,
122.99326074619)) ;
#72677 = CARTESIAN_POINT('Ctrl Pts',(-18.2507605487093,-13.7447550299547,
123.076976202334)) ;
#72678 = CARTESIAN_POINT('Ctrl Pts',(-17.9107237977274,-13.93460996668,123.247603809018)) ;
#72679 = CARTESIAN_POINT('Ctrl Pts',(-18.210432205314,-13.7546208862612,123.280449806178)) ;
#72680 = CARTESIAN_POINT('Ctrl Pts',(-17.905103874463,-13.9446792561491,123.512124786774)) ;
#72681 = CARTESIAN_POINT('Ctrl Pts',(-18.2059368701527,-13.7646901757304,
123.492066934925)) ;
#72682 = CARTESIAN_POINT('Ctrl Pts',(-17.9445700337425,-13.9545228137004,
123.767790797014)) ;
#72683 = CARTESIAN_POINT('Ctrl Pts',(-18.2375102230327,-13.7745337332817,
123.696598534101)) ;
#72684 = CARTESIAN_POINT('Ctrl Pts',(-18.0281629109246,-13.9645029404882,
124.016370584135)) ;
#72685 = CARTESIAN_POINT('Ctrl Pts',(-18.3043848156925,-13.7845138600695,
123.895462003248)) ;
#72686 = CARTESIAN_POINT('Ctrl Pts',(-18.1545752562792,-13.9745214890882,
124.247305606064)) ;
#72687 = CARTESIAN_POINT('Ctrl Pts',(-18.4055151504625,-13.7945324086694,
124.080209779767)) ;
#72688 = CARTESIAN_POINT('Ctrl Pts',(-18.316536321276,-13.9844047896114,124.450385028018)) ;
#72689 = CARTESIAN_POINT('Ctrl Pts',(-18.535083750399,-13.8044157091926,124.242672395031)) ;
#72690 = CARTESIAN_POINT('Ctrl Pts',(-18.5149631926706,-13.9944730766595,
124.62533735748)) ;
#72691 = CARTESIAN_POINT('Ctrl Pts',(-18.6938257640231,-13.8144839962408,
124.382634169633)) ;
#72692 = CARTESIAN_POINT('Ctrl Pts',(-18.7353286473333,-14.0043031996781,
124.760223493751)) ;
#72693 = CARTESIAN_POINT('Ctrl Pts',(-18.8701172488312,-13.8243141192594,
124.49054215336)) ;
#72694 = CARTESIAN_POINT('Ctrl Pts',(-18.9813430292537,-14.0143697836035,
124.857357794723)) ;
#72695 = CARTESIAN_POINT('Ctrl Pts',(-19.0669291407156,-13.8343807031847,
124.568249482507)) ;
#72696 = CARTESIAN_POINT('Ctrl Pts',(-19.2360505050049,-14.0242598966179,
124.909235187394)) ;
#72697 = CARTESIAN_POINT('Ctrl Pts',(-19.2706943553894,-13.8442708161992,
124.60975094901)) ;
#72698 = CARTESIAN_POINT('Ctrl Pts',(-19.4985188781197,-14.0342525853805,
124.916724579576)) ;
#72699 = CARTESIAN_POINT('Ctrl Pts',(-19.4806688914999,-13.8542635049618,
124.615742311681)) ;
#72700 = CARTESIAN_POINT('Ctrl Pts',(-19.7574815058641,-14.0442134737363,
124.878462065185)) ;
#72701 = CARTESIAN_POINT('Ctrl Pts',(-19.6878385846522,-13.8642243933176,
124.585132166976)) ;
#72702 = CARTESIAN_POINT('Ctrl Pts',(-20.0049101277861,-14.0541314186163,
124.796606975599)) ;
#72703 = CARTESIAN_POINT('Ctrl Pts',(-19.8857808233358,-13.8741423381976,
124.519648232361)) ;
#72704 = CARTESIAN_POINT('Ctrl Pts',(-20.2366270329028,-14.0641391717125,
124.672163407171)) ;
#72705 = CARTESIAN_POINT('Ctrl Pts',(-20.0711543039772,-13.8841500912938,
124.420093397815)) ;
#72706 = CARTESIAN_POINT('Ctrl Pts',(-20.4433359396019,-14.0741702656716,
124.508602153835)) ;
#72707 = CARTESIAN_POINT('Ctrl Pts',(-20.2365214217928,-13.8941811852529,
124.289244226254)) ;
#72708 = CARTESIAN_POINT('Ctrl Pts',(-20.6157637308893,-14.0840182336996,
124.315591986934)) ;
#72709 = CARTESIAN_POINT('Ctrl Pts',(-20.3744629095565,-13.9040291532808,
124.134836941808)) ;
#72710 = CARTESIAN_POINT('Ctrl Pts',(-20.7551952257983,-14.0940801898254,
124.090948557005)) ;
#72711 = CARTESIAN_POINT('Ctrl Pts',(-20.4860083127366,-13.9140911094067,
123.955121992217)) ;
#72712 = CARTESIAN_POINT('Ctrl Pts',(-20.8516795937115,-14.1039774014266,
123.849406694899)) ;
#72713 = CARTESIAN_POINT('Ctrl Pts',(-20.5631955167448,-13.9239883210078,
123.761889246969)) ;
#72714 = CARTESIAN_POINT('Ctrl Pts',(-20.905779742348,-14.1139085680912,123.594099508429)) ;
#72715 = CARTESIAN_POINT('Ctrl Pts',(-20.6064757368551,-13.9339194876725,
123.557644109238)) ;
#72716 = CARTESIAN_POINT('Ctrl Pts',(-20.9145419979697,-14.1239507522954,
123.330350913862)) ;
#72717 = CARTESIAN_POINT('Ctrl Pts',(-20.6134856993466,-13.9439616718766,
123.346645072015)) ;
#72718 = CARTESIAN_POINT('Ctrl Pts',(-20.8781348522192,-14.1338374205485,
123.073090399085)) ;
#72719 = CARTESIAN_POINT('Ctrl Pts',(-20.5843603024591,-13.9538483401298,
123.140837492851)) ;
#72720 = CARTESIAN_POINT('Ctrl Pts',(-20.7971713176932,-14.1438305325268,
122.823288399599)) ;
#72721 = CARTESIAN_POINT('Ctrl Pts',(-20.5195898212087,-13.963841452108,122.940995952471)) ;
#72722 = CARTESIAN_POINT('Ctrl Pts',(-20.6745548236783,-14.1537762101426,
122.5924733342)) ;
#72723 = CARTESIAN_POINT('Ctrl Pts',(-20.4214971012033,-13.9737871297239,
122.756344186729)) ;
#72724 = CARTESIAN_POINT('Ctrl Pts',(-20.514110475055,-14.1637235131276,122.386083823483)) ;
#72725 = CARTESIAN_POINT('Ctrl Pts',(-20.2931422359031,-13.9837344327088,
122.591232683106)) ;
#72726 = CARTESIAN_POINT('Ctrl Pts',(-20.318129265181,-14.1737712368743,122.209146648003)) ;
#72727 = CARTESIAN_POINT('Ctrl Pts',(-20.1363573513922,-13.9937821564556,
122.449682552309)) ;
#72728 = CARTESIAN_POINT('Ctrl Pts',(-20.0989460634278,-14.1836196106369,
122.071534647431)) ;
#72729 = CARTESIAN_POINT('Ctrl Pts',(-19.961011947168,-14.0036305302181,122.339593209163)) ;
#72730 = CARTESIAN_POINT('Ctrl Pts',(-19.8568324061837,-14.1935785830826,
121.972166958838)) ;
#72731 = CARTESIAN_POINT('Ctrl Pts',(-19.767321602057,-14.0135895026638,122.260098632269)) ;
#72732 = CARTESIAN_POINT('Ctrl Pts',(-19.5989991593739,-14.2036174449637,
121.916368996526)) ;
#72733 = CARTESIAN_POINT('Ctrl Pts',(-19.5610549871586,-14.023628364545,122.215459749838)) ;
#72734 = CARTESIAN_POINT('Ctrl Pts',(-19.3395819370227,-14.2134960491355,
121.905934350628)) ;
#72735 = CARTESIAN_POINT('Ctrl Pts',(-19.3535221269257,-14.0335069687168,
122.207111469005)) ;
#72736 = CARTESIAN_POINT('Ctrl Pts',(-19.077837641455,-14.2235475903388,121.94118979378)) ;
#72737 = CARTESIAN_POINT('Ctrl Pts',(-19.1441263879232,-14.0435585099201,
122.235315233814)) ;
#72738 = CARTESIAN_POINT('Ctrl Pts',(-18.8299973984086,-14.2334429883192,
122.020057862205)) ;
#72739 = CARTESIAN_POINT('Ctrl Pts',(-18.9458547296678,-14.0534539079004,
122.298408839437)) ;
#72740 = CARTESIAN_POINT('Ctrl Pts',(-18.5959941771807,-14.2434942208645,
122.142497342956)) ;
#72741 = CARTESIAN_POINT('Ctrl Pts',(-18.7586516520923,-14.0635051404457,
122.396359920337)) ;
#72742 = CARTESIAN_POINT('Ctrl Pts',(-18.3901717061781,-14.2533804114888,
122.301075810724)) ;
#72743 = CARTESIAN_POINT('Ctrl Pts',(-18.5939939275408,-14.07339133107,122.523221635957)) ;
#72744 = CARTESIAN_POINT('Ctrl Pts',(-18.2128046216458,-14.2633729508045,
122.494683384624)) ;
#72745 = CARTESIAN_POINT('Ctrl Pts',(-18.4520997745653,-14.0833838703858,
122.678107034334)) ;
#72746 = CARTESIAN_POINT('Ctrl Pts',(-18.0724208013344,-14.2733213966993,
122.715249428743)) ;
#72747 = CARTESIAN_POINT('Ctrl Pts',(-18.339792292697,-14.0933323162805,122.854559084059)) ;
#72748 = CARTESIAN_POINT('Ctrl Pts',(-17.9722554346234,-14.2832581992312,
122.956378922637)) ;
#72749 = CARTESIAN_POINT('Ctrl Pts',(-18.2596593906044,-14.1032691188124,
123.047461874324)) ;
#72750 = CARTESIAN_POINT('Ctrl Pts',(-17.9148800449504,-14.2932412066825,
123.21240535779)) ;
#72751 = CARTESIAN_POINT('Ctrl Pts',(-18.2137581989984,-14.1132521262637,
123.252282614946)) ;
#72752 = CARTESIAN_POINT('Ctrl Pts',(-17.9032450353391,-14.3032850480973,
123.47605995493)) ;
#72753 = CARTESIAN_POINT('Ctrl Pts',(-18.2044493516429,-14.1232959676785,
123.463206407145)) ;
#72754 = CARTESIAN_POINT('Ctrl Pts',(-17.9362327115269,-14.3131132467212,
123.732259863048)) ;
#72755 = CARTESIAN_POINT('Ctrl Pts',(-18.2308383754507,-14.1331241663024,
123.668165314127)) ;
#72756 = CARTESIAN_POINT('Ctrl Pts',(-18.0150012318199,-14.3231898401634,
123.985018013465)) ;
#72757 = CARTESIAN_POINT('Ctrl Pts',(-18.2938523322178,-14.1432007597447,
123.870372464175)) ;
#72758 = CARTESIAN_POINT('Ctrl Pts',(-18.133686667507,-14.333041839505,124.215176688649)) ;
#72759 = CARTESIAN_POINT('Ctrl Pts',(-18.3887993080397,-14.1530527590862,
124.054499001948)) ;
#72760 = CARTESIAN_POINT('Ctrl Pts',(-18.2938233161028,-14.3431154263288,
124.425914521009)) ;
#72761 = CARTESIAN_POINT('Ctrl Pts',(-18.5169079559941,-14.1631263459101,
124.223090181388)) ;
#72762 = CARTESIAN_POINT('Ctrl Pts',(-18.4837016928437,-14.3529556514263,
124.601492972283)) ;
#72763 = CARTESIAN_POINT('Ctrl Pts',(-18.6688091616826,-14.1729665710076,
124.363553020106)) ;
#72764 = CARTESIAN_POINT('Ctrl Pts',(-18.7034169617972,-14.362921355455,124.743969337095)) ;
#72765 = CARTESIAN_POINT('Ctrl Pts',(-18.844580419153,-14.1829322750362,124.47753501832)) ;
#72766 = CARTESIAN_POINT('Ctrl Pts',(-18.9461903268553,-14.3729479887616,
124.846418837686)) ;
#72767 = CARTESIAN_POINT('Ctrl Pts',(-19.0387986926441,-14.1929589083428,
124.559495739056)) ;
#72768 = CARTESIAN_POINT('Ctrl Pts',(-19.2001264119719,-14.3828622844734,
124.9046678972)) ;
#72769 = CARTESIAN_POINT('Ctrl Pts',(-19.2419467128813,-14.2028732040546,
124.60609605546)) ;
#72770 = CARTESIAN_POINT('Ctrl Pts',(-19.4622585244001,-14.3928505731658,
124.918515058878)) ;
#72771 = CARTESIAN_POINT('Ctrl Pts',(-19.4516521770258,-14.2128614927471,
124.617175109609)) ;
#72772 = CARTESIAN_POINT('Ctrl Pts',(-19.7240472766197,-14.4028893063242,
124.886002641522)) ;
#72773 = CARTESIAN_POINT('Ctrl Pts',(-19.6610834379714,-14.2229002259054,
124.591166382665)) ;
#72774 = CARTESIAN_POINT('Ctrl Pts',(-19.971442278505,-14.4127326381517,124.81045280007)) ;
#72775 = CARTESIAN_POINT('Ctrl Pts',(-19.8589988887457,-14.232743557733,124.530728061937)) ;
#72776 = CARTESIAN_POINT('Ctrl Pts',(-20.2065561511299,-14.4227603640313,
124.691438006589)) ;
#72777 = CARTESIAN_POINT('Ctrl Pts',(-20.0470906952005,-14.2427712836126,
124.435517495806)) ;
#72778 = CARTESIAN_POINT('Ctrl Pts',(-20.4171057819687,-14.4327927004199,
124.532757562432)) ;
#72779 = CARTESIAN_POINT('Ctrl Pts',(-20.2155312378511,-14.2528036200011,
124.308574138805)) ;
#72780 = CARTESIAN_POINT('Ctrl Pts',(-20.5936350311629,-14.4426222007205,
124.344201635608)) ;
#72781 = CARTESIAN_POINT('Ctrl Pts',(-20.3567549741227,-14.2626331203018,
124.15773110315)) ;
#72782 = CARTESIAN_POINT('Ctrl Pts',(-20.7377126083649,-14.4526117046373,
124.124750610615)) ;
#72783 = CARTESIAN_POINT('Ctrl Pts',(-20.4720182693449,-14.2726226242185,
123.982171262254)) ;
#72784 = CARTESIAN_POINT('Ctrl Pts',(-20.8414417059571,-14.4626555451497,
123.882049023588)) ;
#72785 = CARTESIAN_POINT('Ctrl Pts',(-20.5550029138087,-14.2826664647309,
123.788010448594)) ;
#72786 = CARTESIAN_POINT('Ctrl Pts',(-20.9006480360546,-14.4724772509177,
123.630827043124)) ;
#72787 = CARTESIAN_POINT('Ctrl Pts',(-20.602369249548,-14.292488170499,123.587034187836)) ;
#72788 = CARTESIAN_POINT('Ctrl Pts',(-20.9162986355371,-14.4825122980501,
123.367582647656)) ;
#72789 = CARTESIAN_POINT('Ctrl Pts',(-20.6148913940102,-14.3025232176314,
123.376438685901)) ;
#72790 = CARTESIAN_POINT('Ctrl Pts',(-20.8853105896396,-14.492536975487,123.105964149148)) ;
#72791 = CARTESIAN_POINT('Ctrl Pts',(-20.5901024698145,-14.3125478950683,
123.167143688753)) ;
#72792 = CARTESIAN_POINT('Ctrl Pts',(-20.8111959912493,-14.5023897903414,
122.857876731646)) ;
#72793 = CARTESIAN_POINT('Ctrl Pts',(-20.5308125817991,-14.3224007099227,
122.96867405913)) ;
#72794 = CARTESIAN_POINT('Ctrl Pts',(-20.6939628549343,-14.512377499949,122.623068574737)) ;
#72795 = CARTESIAN_POINT('Ctrl Pts',(-20.4370276691554,-14.3323884195303,
122.780826900379)) ;
#72796 = CARTESIAN_POINT('Ctrl Pts',(-20.5386353139863,-14.5223075099431,
122.413370344801)) ;
#72797 = CARTESIAN_POINT('Ctrl Pts',(-20.3127672606121,-14.3423184295243,
122.613067632083)) ;
#72798 = CARTESIAN_POINT('Ctrl Pts',(-20.3483991860462,-14.5322972651622,
122.232456679558)) ;
#72799 = CARTESIAN_POINT('Ctrl Pts',(-20.1605796814699,-14.3523081847435,
122.468335499922)) ;
#72800 = CARTESIAN_POINT('Ctrl Pts',(-20.1286457022136,-14.5423238738451,
122.087070807821)) ;
#72801 = CARTESIAN_POINT('Ctrl Pts',(-19.9847778210034,-14.3623347934264,
122.352025351931)) ;
#72802 = CARTESIAN_POINT('Ctrl Pts',(-19.8905327192544,-14.552207813867,121.983318872827)) ;
#72803 = CARTESIAN_POINT('Ctrl Pts',(-19.7942886798817,-14.3722187334482,
122.269022420981)) ;
#72804 = CARTESIAN_POINT('Ctrl Pts',(-19.635462587823,-14.5621970414055,121.921242080252)) ;
#72805 = CARTESIAN_POINT('Ctrl Pts',(-19.5902331362649,-14.3822079609867,
122.219359208042)) ;
#72806 = CARTESIAN_POINT('Ctrl Pts',(-19.3720577988272,-14.5722399119292,
121.904853032936)) ;
#72807 = CARTESIAN_POINT('Ctrl Pts',(-19.3795093430328,-14.3922508315104,
122.206246194466)) ;
#72808 = CARTESIAN_POINT('Ctrl Pts',(-19.1152596800148,-14.5820722986846,
121.933419317755)) ;
#72809 = CARTESIAN_POINT('Ctrl Pts',(-19.1740714024378,-14.4020832182658,
122.229097307701)) ;
#72810 = CARTESIAN_POINT('Ctrl Pts',(-18.8630536664774,-14.5920655918562,
122.006599511794)) ;
#72811 = CARTESIAN_POINT('Ctrl Pts',(-18.9723061434464,-14.4120765114374,
122.287639558264)) ;
#72812 = CARTESIAN_POINT('Ctrl Pts',(-18.626700387474,-14.6020975975046,122.123410637896)) ;
#72813 = CARTESIAN_POINT('Ctrl Pts',(-18.7832226648472,-14.4221085170859,
122.38108679379)) ;
#72814 = CARTESIAN_POINT('Ctrl Pts',(-18.4175822404047,-14.6119628534736,
122.276618419856)) ;
#72815 = CARTESIAN_POINT('Ctrl Pts',(-18.61592748227,-14.4319737730548,122.503651126042)) ;
#72816 = CARTESIAN_POINT('Ctrl Pts',(-18.2359363519332,-14.6219247333811,
122.46514351394)) ;
#72817 = CARTESIAN_POINT('Ctrl Pts',(-18.4706094571108,-14.4419356529623,
122.654469655171)) ;
#72818 = CARTESIAN_POINT('Ctrl Pts',(-18.0890820795263,-14.631959666743,122.684159241036)) ;
#72819 = CARTESIAN_POINT('Ctrl Pts',(-18.3531243943116,-14.4519705863242,
122.829681166478)) ;
#72820 = CARTESIAN_POINT('Ctrl Pts',(-17.9836588830018,-14.6418446251222,
122.921611991618)) ;
#72821 = CARTESIAN_POINT('Ctrl Pts',(-18.2687841767101,-14.4618555447035,
123.019642136378)) ;
#72822 = CARTESIAN_POINT('Ctrl Pts',(-17.9199993003975,-14.6519102520449,
123.178306439061)) ;
#72823 = CARTESIAN_POINT('Ctrl Pts',(-18.217854528994,-14.4719211716262,123.224997325049)) ;
#72824 = CARTESIAN_POINT('Ctrl Pts',(-17.902016923723,-14.6617493577093,123.436284553321)) ;
#72825 = CARTESIAN_POINT('Ctrl Pts',(-18.2034666313559,-14.4817602772905,
123.431379111336)) ;
#72826 = CARTESIAN_POINT('Ctrl Pts',(-17.9293579839906,-14.6718121727146,
123.699271479255)) ;
#72827 = CARTESIAN_POINT('Ctrl Pts',(-18.2253374197392,-14.4918230922959,
123.641768973016)) ;
#72828 = CARTESIAN_POINT('Ctrl Pts',(-18.0009916818358,-14.6817083787633,
123.949301618016)) ;
#72829 = CARTESIAN_POINT('Ctrl Pts',(-18.2826422983745,-14.5017192983446,
123.841793287146)) ;
#72830 = CARTESIAN_POINT('Ctrl Pts',(-18.1147854787737,-14.6916492017886,
124.184415931293)) ;
#72831 = CARTESIAN_POINT('Ctrl Pts',(-18.3736753208548,-14.5116601213698,
124.029885468125)) ;
#72832 = CARTESIAN_POINT('Ctrl Pts',(-18.268637847317,-14.7016537847672,124.397645063543)) ;
#72833 = CARTESIAN_POINT('Ctrl Pts',(-18.4967554534644,-14.5216647043485,
124.200469975829)) ;
#72834 = CARTESIAN_POINT('Ctrl Pts',(-18.4576820791723,-14.711674679212,124.580965224255)) ;
#72835 = CARTESIAN_POINT('Ctrl Pts',(-18.6479893550732,-14.5316855987932,
124.347127597631)) ;
#72836 = CARTESIAN_POINT('Ctrl Pts',(-18.6727084409686,-14.7215665998014,
124.727050531071)) ;
#72837 = CARTESIAN_POINT('Ctrl Pts',(-18.8200089755962,-14.5415775193826,
124.463997424165)) ;
#72838 = CARTESIAN_POINT('Ctrl Pts',(-18.9120984381153,-14.7315600321468,
124.835009694334)) ;
#72839 = CARTESIAN_POINT('Ctrl Pts',(-19.0115200042416,-14.551570951728,124.55036669427)) ;
#72840 = CARTESIAN_POINT('Ctrl Pts',(-19.1654082296923,-14.7415056370466,
124.899373825314)) ;
#72841 = CARTESIAN_POINT('Ctrl Pts',(-19.2141671271123,-14.5615165566279,
124.601860046211)) ;
#72842 = CARTESIAN_POINT('Ctrl Pts',(-19.4260649276636,-14.7514529105282,
124.919311654111)) ;
#72843 = CARTESIAN_POINT('Ctrl Pts',(-19.4226921583559,-14.5714638301094,
124.617812487927)) ;
#72844 = CARTESIAN_POINT('Ctrl Pts',(-19.688803998052,-14.7615008250045,124.893135998559)) ;
#72845 = CARTESIAN_POINT('Ctrl Pts',(-19.6328836382695,-14.5815117445858,
124.596874129132)) ;
#72846 = CARTESIAN_POINT('Ctrl Pts',(-19.9380105597633,-14.7713484653519,
124.823369065501)) ;
#72847 = CARTESIAN_POINT('Ctrl Pts',(-19.8322491726103,-14.5913593849331,
124.541062779856)) ;
#72848 = CARTESIAN_POINT('Ctrl Pts',(-20.1743610166354,-14.7813101807285,
124.710840541203)) ;
#72849 = CARTESIAN_POINT('Ctrl Pts',(-20.0213304109851,-14.6013211003097,
124.451042024514)) ;
#72850 = CARTESIAN_POINT('Ctrl Pts',(-20.3888445239837,-14.7913388043013,
124.557674697963)) ;
#72851 = CARTESIAN_POINT('Ctrl Pts',(-20.1929184772654,-14.6113497238825,
124.32851117537)) ;
#72852 = CARTESIAN_POINT('Ctrl Pts',(-20.5713377847483,-14.8012491663677,
124.37189085968)) ;
#72853 = CARTESIAN_POINT('Ctrl Pts',(-20.3389145561169,-14.6212600859489,
124.179885784323)) ;
#72854 = CARTESIAN_POINT('Ctrl Pts',(-20.7197431782127,-14.8111838600201,
124.157087470511)) ;
#72855 = CARTESIAN_POINT('Ctrl Pts',(-20.457640661641,-14.6311947796013,124.008044437838)) ;
#72856 = CARTESIAN_POINT('Ctrl Pts',(-20.8295234845985,-14.821225703148,123.917131743873)) ;
#72857 = CARTESIAN_POINT('Ctrl Pts',(-20.5454669287708,-14.6412366227292,
123.816080822821)) ;
#72858 = CARTESIAN_POINT('Ctrl Pts',(-20.895164226046,-14.8311102087184,123.665780824493)) ;
#72859 = CARTESIAN_POINT('Ctrl Pts',(-20.5979816634709,-14.6511211282996,
123.615000778527)) ;
#72860 = CARTESIAN_POINT('Ctrl Pts',(-20.9167156315003,-14.8411123125036,
123.403859517349)) ;
#72861 = CARTESIAN_POINT('Ctrl Pts',(-20.6152250273271,-14.6611232320848,
123.405463971272)) ;
#72862 = CARTESIAN_POINT('Ctrl Pts',(-20.892871759179,-14.8510306639186,123.144264974581)) ;
#72863 = CARTESIAN_POINT('Ctrl Pts',(-20.5961521920614,-14.6710415834998,
123.197788211826)) ;
#72864 = CARTESIAN_POINT('Ctrl Pts',(-20.8233784417563,-14.8610783199395,
122.889574983723)) ;
#72865 = CARTESIAN_POINT('Ctrl Pts',(-20.5405596778779,-14.6810892395207,
122.994035641784)) ;
#72866 = CARTESIAN_POINT('Ctrl Pts',(-20.7129195792961,-14.8709495129677,
122.654803032933)) ;
#72867 = CARTESIAN_POINT('Ctrl Pts',(-20.4521948362717,-14.6909604325489,
122.806217311393)) ;
#72868 = CARTESIAN_POINT('Ctrl Pts',(-20.5605298604952,-14.8810152261112,
122.438669790552)) ;
#72869 = CARTESIAN_POINT('Ctrl Pts',(-20.330284230218,-14.7010261456924,122.633308925959)) ;
#72870 = CARTESIAN_POINT('Ctrl Pts',(-20.3770184511799,-14.8908676866838,
122.255919658945)) ;
#72871 = CARTESIAN_POINT('Ctrl Pts',(-20.1834793625096,-14.7108786062651,
122.487109277975)) ;
#72872 = CARTESIAN_POINT('Ctrl Pts',(-20.0875427687652,-14.9042961494064,
122.05428711409)) ;
#72873 = CARTESIAN_POINT('Ctrl Pts',(-19.9518873140162,-14.7243070689876,
122.325790630287)) ;
#72874 = CARTESIAN_POINT('Ctrl Pts',(-19.7606733441764,-14.9173770969235,
121.935403530438)) ;
#72875 = CARTESIAN_POINT('Ctrl Pts',(-19.6903664132712,-14.7373880165047,
122.230682365548)) ;
#72876 = CARTESIAN_POINT('Ctrl Pts',(-19.4080294143568,-14.930851595158,121.904239537991)) ;
#72877 = CARTESIAN_POINT('Ctrl Pts',(-19.408296278235,-14.7508625147393,122.205756669958)) ;
#72878 = CARTESIAN_POINT('Ctrl Pts',(-19.1506048229963,-14.9406836987675,
121.926886772549)) ;
#72879 = CARTESIAN_POINT('Ctrl Pts',(-19.2023472618255,-14.7606946183488,
122.223870633588)) ;
#72880 = CARTESIAN_POINT('Ctrl Pts',(-18.8974267386833,-14.9506496018942,
121.993755117911)) ;
#72881 = CARTESIAN_POINT('Ctrl Pts',(-18.9998068131851,-14.7706605214754,
122.277363288063)) ;
#72882 = CARTESIAN_POINT('Ctrl Pts',(-18.658349854463,-14.9606770112044,122.104643278286)) ;
#72883 = CARTESIAN_POINT('Ctrl Pts',(-18.8085430338256,-14.7806879307857,
122.366073028994)) ;
#72884 = CARTESIAN_POINT('Ctrl Pts',(-18.4446798400925,-14.970588042571,122.253516252919)) ;
#72885 = CARTESIAN_POINT('Ctrl Pts',(-18.6376088003778,-14.7905989621522,
122.485164544284)) ;
#72886 = CARTESIAN_POINT('Ctrl Pts',(-18.1971580267573,-14.983832350192,122.498300087687)) ;
#72887 = CARTESIAN_POINT('Ctrl Pts',(-18.4395744217537,-14.8038432697733,
122.681015310389)) ;
#72888 = CARTESIAN_POINT('Ctrl Pts',(-17.9735883959182,-15.0005328328632,
122.881645823223)) ;
#72889 = CARTESIAN_POINT('Ctrl Pts',(-18.2607334713096,-14.8205437524445,
122.987646040595)) ;
#72890 = CARTESIAN_POINT('Ctrl Pts',(-17.8949212634125,-15.017039662019,123.313331293307)) ;
#72891 = CARTESIAN_POINT('Ctrl Pts',(-18.197786980337,-14.8370505816002,123.333061833224)) ;
#72892 = CARTESIAN_POINT('Ctrl Pts',(-17.9226408362243,-15.0303502902566,
123.66198197427)) ;
#72893 = CARTESIAN_POINT('Ctrl Pts',(-18.2199642568686,-14.8503612098378,
123.611928568434)) ;
#72894 = CARTESIAN_POINT('Ctrl Pts',(-17.9885443791132,-15.0403428537967,
123.916213406508)) ;
#72895 = CARTESIAN_POINT('Ctrl Pts',(-18.2726848749169,-14.8603537733779,
123.815325758311)) ;
#72896 = CARTESIAN_POINT('Ctrl Pts',(-18.0982567044604,-15.0503729367982,
124.155839488602)) ;
#72897 = CARTESIAN_POINT('Ctrl Pts',(-18.3604503472436,-14.8703838563795,
124.007021726878)) ;
#72898 = CARTESIAN_POINT('Ctrl Pts',(-18.2942816287218,-15.063546540796,124.44126177794)) ;
#72899 = CARTESIAN_POINT('Ctrl Pts',(-18.5172815099474,-14.8835574603772,
124.235376257215)) ;
#72900 = CARTESIAN_POINT('Ctrl Pts',(-18.6299004804295,-15.0801842460274,
124.728937538232)) ;
#72901 = CARTESIAN_POINT('Ctrl Pts',(-18.785763290496,-14.9001951656086,124.465502997211)) ;
#72902 = CARTESIAN_POINT('Ctrl Pts',(-19.1244402676939,-15.1000660085948,
124.915683237947)) ;
#72903 = CARTESIAN_POINT('Ctrl Pts',(-19.1813811513845,-14.9200769281761,
124.614910725455)) ;
#72904 = CARTESIAN_POINT('Ctrl Pts',(-19.5680268436955,-15.1167623608113,
124.921075710922)) ;
#72905 = CARTESIAN_POINT('Ctrl Pts',(-19.5363048231766,-14.9367732803926,
124.619219761806)) ;
#72906 = CARTESIAN_POINT('Ctrl Pts',(-19.9032277012464,-15.1299193886004,
124.836006277043)) ;
#72907 = CARTESIAN_POINT('Ctrl Pts',(-19.804416663056,-14.9499303081817,124.551173733196)) ;
#72908 = CARTESIAN_POINT('Ctrl Pts',(-20.2240299228252,-15.1432967432439,
124.69232618413)) ;
#72909 = CARTESIAN_POINT('Ctrl Pts',(-20.0610789329257,-14.9633076628252,
124.436222806107)) ;
#72910 = CARTESIAN_POINT('Ctrl Pts',(-20.5648835408939,-15.1598275775027,
124.415004995523)) ;
#72911 = CARTESIAN_POINT('Ctrl Pts',(-20.33374952369,-14.979838497084,124.214377150155)) ;
#72912 = CARTESIAN_POINT('Ctrl Pts',(-20.8382356611217,-15.1797922672458,
123.96026126481)) ;
#72913 = CARTESIAN_POINT('Ctrl Pts',(-20.5524388724161,-14.9998031868271,
123.850580630537)) ;
#72914 = CARTESIAN_POINT('Ctrl Pts',(-20.9392779040773,-15.1997087606695,
123.440635012869)) ;
#72915 = CARTESIAN_POINT('Ctrl Pts',(-20.6332747129782,-15.0197196802507,
123.434880576487)) ;
#72916 = CARTESIAN_POINT('Ctrl Pts',(-20.8580805310066,-15.219598480019,122.918218801413)) ;
#72917 = CARTESIAN_POINT('Ctrl Pts',(-20.5683198928512,-15.0396093996003,
123.016946176903)) ;
#72918 = CARTESIAN_POINT('Ctrl Pts',(-20.6016712396936,-15.2396052096669,
122.452465436921)) ;
#72919 = CARTESIAN_POINT('Ctrl Pts',(-20.363194945236,-15.0596161292481,122.644342199294)) ;
#72920 = CARTESIAN_POINT('Ctrl Pts',(-20.2052118910456,-15.2594432633138,
122.104699832053)) ;
#72921 = CARTESIAN_POINT('Ctrl Pts',(-20.0460282780659,-15.079454182895,122.366126875178)) ;
#72922 = CARTESIAN_POINT('Ctrl Pts',(-19.7104197648693,-15.2794366015274,
121.91117270604)) ;
#72923 = CARTESIAN_POINT('Ctrl Pts',(-19.6501953671741,-15.0994475211086,
122.211302958785)) ;
#72924 = CARTESIAN_POINT('Ctrl Pts',(-19.1820210308672,-15.299319400934,121.898505004047)) ;
#72925 = CARTESIAN_POINT('Ctrl Pts',(-19.2274754164287,-15.1193303205152,
122.201166461084)) ;
#72926 = CARTESIAN_POINT('Ctrl Pts',(-18.6807320925473,-15.3192115818527,
122.066058969387)) ;
#72927 = CARTESIAN_POINT('Ctrl Pts',(-18.8264426177306,-15.1392225014339,
122.335208221256)) ;
#72928 = CARTESIAN_POINT('Ctrl Pts',(-18.2657076845976,-15.3391137603478,
122.394277865581)) ;
#72929 = CARTESIAN_POINT('Ctrl Pts',(-18.494421510302,-15.159124679929,122.597782896425)) ;
#72930 = CARTESIAN_POINT('Ctrl Pts',(-17.9866547280491,-15.3591510715515,
122.847707709336)) ;
#72931 = CARTESIAN_POINT('Ctrl Pts',(-18.2711780423566,-15.1791619911328,
122.960525608524)) ;
#72932 = CARTESIAN_POINT('Ctrl Pts',(-17.8794922156579,-15.3789635130924,
123.363506708321)) ;
#72933 = CARTESIAN_POINT('Ctrl Pts',(-18.1854465971545,-15.1989744326736,
123.373166586324)) ;
#72934 = CARTESIAN_POINT('Ctrl Pts',(-17.9558345969628,-15.3990287538273,
123.891058298173)) ;
#72935 = CARTESIAN_POINT('Ctrl Pts',(-18.2465194339574,-15.2190396734085,
123.795207317988)) ;
#72936 = CARTESIAN_POINT('Ctrl Pts',(-18.2036257716966,-15.4187859586831,
124.354317293428)) ;
#72937 = CARTESIAN_POINT('Ctrl Pts',(-18.444753257949,-15.2387968782644,124.165817334642)) ;
#72938 = CARTESIAN_POINT('Ctrl Pts',(-18.5991767272992,-15.4388192313288,
124.71034908512)) ;
#72939 = CARTESIAN_POINT('Ctrl Pts',(-18.7611938046602,-15.2588301509101,
124.450642577608)) ;
#72940 = CARTESIAN_POINT('Ctrl Pts',(-19.0875441523819,-15.4586321397826,
124.907957059545)) ;
#72941 = CARTESIAN_POINT('Ctrl Pts',(-19.1518899723408,-15.2786430593639,
124.608729644721)) ;
#72942 = CARTESIAN_POINT('Ctrl Pts',(-19.6183970906438,-15.4786282859101,
124.927914166539)) ;
#72943 = CARTESIAN_POINT('Ctrl Pts',(-19.576572466702,-15.2986392054913,124.62469458261)) ;
#72944 = CARTESIAN_POINT('Ctrl Pts',(-20.1213238856108,-15.4984900391326,
124.766723103291)) ;
#72945 = CARTESIAN_POINT('Ctrl Pts',(-19.9789150179613,-15.3185009587138,
124.495740310664)) ;
#72946 = CARTESIAN_POINT('Ctrl Pts',(-20.5429196526886,-15.5185585562607,
124.440174246475)) ;
#72947 = CARTESIAN_POINT('Ctrl Pts',(-20.3161903555175,-15.3385694758419,
124.234500854143)) ;
#72948 = CARTESIAN_POINT('Ctrl Pts',(-20.8242320696913,-15.5383894292575,
123.994315885948)) ;
#72949 = CARTESIAN_POINT('Ctrl Pts',(-20.5412403549953,-15.3584003488387,
123.877812029321)) ;
#72950 = CARTESIAN_POINT('Ctrl Pts',(-20.9383743236611,-15.5583113400742,
123.477399544048)) ;
#72951 = CARTESIAN_POINT('Ctrl Pts',(-20.6325525210197,-15.3783222596554,
123.464277746288)) ;
#72952 = CARTESIAN_POINT('Ctrl Pts',(-20.8690610708311,-15.5782407835095,
122.952175131988)) ;
#72953 = CARTESIAN_POINT('Ctrl Pts',(-20.5770999180587,-15.3982517030907,
123.044097841455)) ;
#72954 = CARTESIAN_POINT('Ctrl Pts',(-20.6251692263839,-15.5981504536259,
122.482655310881)) ;
#72955 = CARTESIAN_POINT('Ctrl Pts',(-20.3819841289406,-15.4181613732071,
122.668482232618)) ;
#72956 = CARTESIAN_POINT('Ctrl Pts',(-20.236940502455,-15.6180238108887,122.124408327006)) ;
#72957 = CARTESIAN_POINT('Ctrl Pts',(-20.0713986144983,-15.43803473047,122.381885868014)) ;
#72958 = CARTESIAN_POINT('Ctrl Pts',(-19.7469529682566,-15.6380153455067,
121.919076471778)) ;
#72959 = CARTESIAN_POINT('Ctrl Pts',(-19.6794074858345,-15.4580262650879,
122.217622870441)) ;
#72960 = CARTESIAN_POINT('Ctrl Pts',(-19.2195107524765,-15.6578809629174,
121.893213319222)) ;
#72961 = CARTESIAN_POINT('Ctrl Pts',(-19.257452611772,-15.4778918824987,122.196935186946)) ;
#72962 = CARTESIAN_POINT('Ctrl Pts',(-18.7119132759881,-15.6778618927456,
122.049260143558)) ;
#72963 = CARTESIAN_POINT('Ctrl Pts',(-18.8513754816871,-15.4978728123269,
122.321775691797)) ;
#72964 = CARTESIAN_POINT('Ctrl Pts',(-18.2892684219138,-15.6978003548287,
122.368964780191)) ;
#72965 = CARTESIAN_POINT('Ctrl Pts',(-18.513261161945,-15.51781127441,122.577542114275)) ;
#72966 = CARTESIAN_POINT('Ctrl Pts',(-18.0010412602358,-15.7176925480505,
122.812265657364)) ;
#72967 = CARTESIAN_POINT('Ctrl Pts',(-18.2826819358055,-15.5377034676318,
122.932185207393)) ;
#72968 = CARTESIAN_POINT('Ctrl Pts',(-17.8812058282244,-15.7376632630859,
123.329230583629)) ;
#72969 = CARTESIAN_POINT('Ctrl Pts',(-18.1868169736697,-15.5576741826671,
123.345758094485)) ;
#72970 = CARTESIAN_POINT('Ctrl Pts',(-17.9435942351176,-15.757472934752,123.852155946801)) ;
#72971 = CARTESIAN_POINT('Ctrl Pts',(-18.236731360586,-15.5774838543332,123.764098868335)) ;
#72972 = CARTESIAN_POINT('Ctrl Pts',(-18.182383268691,-15.7774661514431,124.326648974565)) ;
#72973 = CARTESIAN_POINT('Ctrl Pts',(-18.4277666392234,-15.5974770710244,
124.143691534973)) ;
#72974 = CARTESIAN_POINT('Ctrl Pts',(-18.566008687816,-15.7973170636395,124.689180060731)) ;
#72975 = CARTESIAN_POINT('Ctrl Pts',(-18.7346680390251,-15.6173279832208,
124.433713872996)) ;
#72976 = CARTESIAN_POINT('Ctrl Pts',(-19.0555605459816,-15.8173916699585,
124.900980308336)) ;
#72977 = CARTESIAN_POINT('Ctrl Pts',(-19.126318602416,-15.6374025895398,124.603150145415)) ;
#72978 = CARTESIAN_POINT('Ctrl Pts',(-19.4939341246382,-15.8339083018419,
124.927054797018)) ;
#72979 = CARTESIAN_POINT('Ctrl Pts',(-19.4769939508857,-15.6539192214231,
124.62400662122)) ;
#72980 = CARTESIAN_POINT('Ctrl Pts',(-19.8373421472815,-15.847247009536,124.85716735999)) ;
#72981 = CARTESIAN_POINT('Ctrl Pts',(-19.7517415685983,-15.6672579291172,
124.568093350014)) ;
#72982 = CARTESIAN_POINT('Ctrl Pts',(-20.0781804979538,-15.8570893838442,
124.762739875936)) ;
#72983 = CARTESIAN_POINT('Ctrl Pts',(-19.9444057990373,-15.6771003034255,
124.492551480651)) ;
#72984 = CARTESIAN_POINT('Ctrl Pts',(-20.3037960538785,-15.867144403827,124.625272793308)) ;
#72985 = CARTESIAN_POINT('Ctrl Pts',(-20.1249049700663,-15.6871553234083,
124.38256759213)) ;
#72986 = CARTESIAN_POINT('Ctrl Pts',(-20.5648469001971,-15.8803765604846,
124.395495442163)) ;
#72987 = CARTESIAN_POINT('Ctrl Pts',(-20.333709310747,-15.7003874800658,124.198785755722)) ;
#72988 = CARTESIAN_POINT('Ctrl Pts',(-20.8101326080118,-15.8969915278297,
124.028323713328)) ;
#72989 = CARTESIAN_POINT('Ctrl Pts',(-20.5299755608498,-15.717002447411,123.904990049025)) ;
#72990 = CARTESIAN_POINT('Ctrl Pts',(-20.9150857052234,-15.9135861148409,
123.59995181053)) ;
#72991 = CARTESIAN_POINT('Ctrl Pts',(-20.6139164049773,-15.7335970344222,
123.562338490809)) ;
#72992 = CARTESIAN_POINT('Ctrl Pts',(-20.9083137994438,-15.9268196831963,
123.252228775186)) ;
#72993 = CARTESIAN_POINT('Ctrl Pts',(-20.6085033810929,-15.7468306027775,
123.28412879026)) ;
#72994 = CARTESIAN_POINT('Ctrl Pts',(-20.8574915954294,-15.9368633010049,
122.993254896147)) ;
#72995 = CARTESIAN_POINT('Ctrl Pts',(-20.5678420886449,-15.7568742205862,
123.076956586024)) ;
#72996 = CARTESIAN_POINT('Ctrl Pts',(-20.7640240611452,-15.9467502252398,
122.75080795887)) ;
#72997 = CARTESIAN_POINT('Ctrl Pts',(-20.4930658151328,-15.766761144821,122.88299771998)) ;
#72998 = CARTESIAN_POINT('Ctrl Pts',(-20.6288932482248,-15.9567408796866,
122.525730668333)) ;
#72999 = CARTESIAN_POINT('Ctrl Pts',(-20.3849611673798,-15.7767517992678,
122.702938858516)) ;
#73000 = CARTESIAN_POINT('Ctrl Pts',(-20.4571800170239,-15.9667026381405,
122.328129169737)) ;
#73001 = CARTESIAN_POINT('Ctrl Pts',(-20.2475814010665,-15.7867135577218,
122.544854090362)) ;
#73002 = CARTESIAN_POINT('Ctrl Pts',(-20.184971644941,-15.9800425032078,122.107130949317)) ;
#73003 = CARTESIAN_POINT('Ctrl Pts',(-20.0298503330428,-15.800053422789,122.368082503893)) ;
#73004 = CARTESIAN_POINT('Ctrl Pts',(-19.8618390549688,-15.9933512861211,
121.963354375923)) ;
#73005 = CARTESIAN_POINT('Ctrl Pts',(-19.7713258119905,-15.8133622057023,
122.25304504801)) ;
#73006 = CARTESIAN_POINT('Ctrl Pts',(-19.5194352460045,-16.0065470435651,
121.908483591858)) ;
#73007 = CARTESIAN_POINT('Ctrl Pts',(-19.4973853555819,-15.8265579631464,
122.209149363533)) ;
#73008 = CARTESIAN_POINT('Ctrl Pts',(-19.2576646411424,-16.0165089272416,
121.911843868046)) ;
#73009 = CARTESIAN_POINT('Ctrl Pts',(-19.2879723775728,-15.8365198468229,
122.211840251455)) ;
#73010 = CARTESIAN_POINT('Ctrl Pts',(-18.998445535369,-16.0265520367563,121.96142659732)) ;
#73011 = CARTESIAN_POINT('Ctrl Pts',(-19.0805966476983,-15.8465629563375,
122.251508536236)) ;
#73012 = CARTESIAN_POINT('Ctrl Pts',(-18.7563398526898,-16.0364042867555,
122.053197919768)) ;
#73013 = CARTESIAN_POINT('Ctrl Pts',(-18.8869132360213,-15.8564152063368,
122.324927701526)) ;
#73014 = CARTESIAN_POINT('Ctrl Pts',(-18.5308557512997,-16.046375823706,122.186642824453)) ;
#73015 = CARTESIAN_POINT('Ctrl Pts',(-18.7065271150843,-15.8663867432872,
122.431685506008)) ;
#73016 = CARTESIAN_POINT('Ctrl Pts',(-18.3314551896141,-16.0563710891835,
122.357680218338)) ;
#73017 = CARTESIAN_POINT('Ctrl Pts',(-18.5470081927436,-15.8763820087648,
122.568517085258)) ;
#73018 = CARTESIAN_POINT('Ctrl Pts',(-18.1644264951237,-16.0664050620571,
122.561684900295)) ;
#73019 = CARTESIAN_POINT('Ctrl Pts',(-18.4133869982469,-15.8864159816384,
122.731722236848)) ;
#73020 = CARTESIAN_POINT('Ctrl Pts',(-18.0372716142788,-16.0762604768195,
122.787340539606)) ;
#73021 = CARTESIAN_POINT('Ctrl Pts',(-18.3116651407134,-15.8962713964007,
122.912247684701)) ;
#73022 = CARTESIAN_POINT('Ctrl Pts',(-17.9496588451068,-16.0862597543283,
123.035027131231)) ;
#73023 = CARTESIAN_POINT('Ctrl Pts',(-18.2415770550694,-15.9062706739096,
123.110397634539)) ;
#73024 = CARTESIAN_POINT('Ctrl Pts',(-17.9065430994012,-16.0961549384913,
123.291508010333)) ;
#73025 = CARTESIAN_POINT('Ctrl Pts',(-18.2070866753849,-15.9161658580725,
123.315582497717)) ;
#73026 = CARTESIAN_POINT('Ctrl Pts',(-17.9086795502078,-16.1062153181321,
123.555839709395)) ;
#73027 = CARTESIAN_POINT('Ctrl Pts',(-18.2087980556812,-15.9262262377133,
123.527047864045)) ;
#73028 = CARTESIAN_POINT('Ctrl Pts',(-17.9555303865302,-16.1160651871402,
123.810434776877)) ;
#73029 = CARTESIAN_POINT('Ctrl Pts',(-18.246280837973,-15.9360761067214,123.730723208321)) ;
#73030 = CARTESIAN_POINT('Ctrl Pts',(-18.0469625662497,-16.1260967483481,
124.057672087737)) ;
#73031 = CARTESIAN_POINT('Ctrl Pts',(-18.3194286080762,-15.9461076679293,
123.928512283029)) ;
#73032 = CARTESIAN_POINT('Ctrl Pts',(-18.180132940785,-16.1361071972304,124.284566442488)) ;
#73033 = CARTESIAN_POINT('Ctrl Pts',(-18.4259667878995,-15.9561181168116,
124.110026615654)) ;
#73034 = CARTESIAN_POINT('Ctrl Pts',(-18.3486698657814,-16.1460139366474,
124.482977937595)) ;
#73035 = CARTESIAN_POINT('Ctrl Pts',(-18.560797834217,-15.9660248562286,124.26875420935)) ;
#73036 = CARTESIAN_POINT('Ctrl Pts',(-18.549400664436,-16.1559519527158,124.650023534737)) ;
#73037 = CARTESIAN_POINT('Ctrl Pts',(-18.7213836797502,-15.9759628722971,
124.402388898548)) ;
#73038 = CARTESIAN_POINT('Ctrl Pts',(-18.7775718600951,-16.1659571991669,
124.780727182759)) ;
#73039 = CARTESIAN_POINT('Ctrl Pts',(-18.9039216373305,-15.9859681187482,
124.506949936595)) ;
#73040 = CARTESIAN_POINT('Ctrl Pts',(-19.0257972538553,-16.1759912602232,
124.869646857072)) ;
#73041 = CARTESIAN_POINT('Ctrl Pts',(-19.1025026967416,-15.9960021798045,
124.578083637669)) ;
#73042 = CARTESIAN_POINT('Ctrl Pts',(-19.2807496064562,-16.1858363412814,
124.913723831304)) ;
#73043 = CARTESIAN_POINT('Ctrl Pts',(-19.3064644940587,-16.0058472608626,
124.613343042249)) ;
#73044 = CARTESIAN_POINT('Ctrl Pts',(-19.543124427014,-16.1958221472349,124.913341409627)) ;
#73045 = CARTESIAN_POINT('Ctrl Pts',(-19.5163642183528,-16.0158330668161,
124.61303502158)) ;
#73046 = CARTESIAN_POINT('Ctrl Pts',(-19.8002495182359,-16.205756967789,124.86781116903)) ;
#73047 = CARTESIAN_POINT('Ctrl Pts',(-19.7220636745429,-16.0257678873703,
124.576608849091)) ;
#73048 = CARTESIAN_POINT('Ctrl Pts',(-20.0484305675954,-16.2158144929213,
124.777029790911)) ;
#73049 = CARTESIAN_POINT('Ctrl Pts',(-19.9206078848616,-16.0358254125025,
124.503981752975)) ;
#73050 = CARTESIAN_POINT('Ctrl Pts',(-20.2719717473582,-16.2256361435726,
124.647952173839)) ;
#73051 = CARTESIAN_POINT('Ctrl Pts',(-20.0994392637093,-16.0456470631539,
124.40071820774)) ;
#73052 = CARTESIAN_POINT('Ctrl Pts',(-20.4747026404971,-16.2356922070774,
124.478471590781)) ;
#73053 = CARTESIAN_POINT('Ctrl Pts',(-20.2616227752683,-16.0557031266586,
124.265132163495)) ;
#73054 = CARTESIAN_POINT('Ctrl Pts',(-20.6426334923553,-16.2456328741413,
124.278356285855)) ;
#73055 = CARTESIAN_POINT('Ctrl Pts',(-20.395965720866,-16.0656437937226,124.105038812576)) ;
#73056 = CARTESIAN_POINT('Ctrl Pts',(-20.7734945782826,-16.2555372678073,
124.053362462527)) ;
#73057 = CARTESIAN_POINT('Ctrl Pts',(-20.5006527028132,-16.0755481873885,
123.925043150666)) ;
#73058 = CARTESIAN_POINT('Ctrl Pts',(-20.864420115776,-16.2655837915703,123.805527276514)) ;
#73059 = CARTESIAN_POINT('Ctrl Pts',(-20.5733913233788,-16.0855947111516,
123.726774248411)) ;
#73060 = CARTESIAN_POINT('Ctrl Pts',(-20.9104948422774,-16.2754798745867,
123.549534920309)) ;
#73061 = CARTESIAN_POINT('Ctrl Pts',(-20.6102491311177,-16.0954907941679,
123.521980487086)) ;
#73062 = CARTESIAN_POINT('Ctrl Pts',(-20.9113721563936,-16.2855465738167,
123.285041710429)) ;
#73063 = CARTESIAN_POINT('Ctrl Pts',(-20.6109490499967,-16.105557493398,123.310385748136)) ;
#73064 = CARTESIAN_POINT('Ctrl Pts',(-20.8676796983875,-16.2953701842178,
123.030571216655)) ;
#73065 = CARTESIAN_POINT('Ctrl Pts',(-20.5759933528988,-16.115381103799,123.106810427065)) ;
#73066 = CARTESIAN_POINT('Ctrl Pts',(-20.7788672823149,-16.3054260443953,
122.781720920191)) ;
#73067 = CARTESIAN_POINT('Ctrl Pts',(-20.5049416634882,-16.1254369639765,
122.907730678547)) ;
#73068 = CARTESIAN_POINT('Ctrl Pts',(-20.6494650622141,-16.3153591907002,
122.554983567627)) ;
#73069 = CARTESIAN_POINT('Ctrl Pts',(-20.4014184363261,-16.1353701102815,
122.726342029914)) ;
#73070 = CARTESIAN_POINT('Ctrl Pts',(-20.4829072058007,-16.3253044464708,
122.353620794858)) ;
#73071 = CARTESIAN_POINT('Ctrl Pts',(-20.2681709878727,-16.1453153660521,
122.565253212726)) ;
#73072 = CARTESIAN_POINT('Ctrl Pts',(-20.2832435138197,-16.3352877449093,
122.183387066511)) ;
#73073 = CARTESIAN_POINT('Ctrl Pts',(-20.1084390193321,-16.1552986644905,
122.42906766522)) ;
#73074 = CARTESIAN_POINT('Ctrl Pts',(-20.0556974557649,-16.3453249250559,
122.050026596334)) ;
#73075 = CARTESIAN_POINT('Ctrl Pts',(-19.9264011931984,-16.1653358446372,
122.322380816789)) ;
#73076 = CARTESIAN_POINT('Ctrl Pts',(-19.8130492091126,-16.3551794777654,
121.959479734129)) ;
#73077 = CARTESIAN_POINT('Ctrl Pts',(-19.7322826766303,-16.1751903973466,
122.249945218267)) ;
#73078 = CARTESIAN_POINT('Ctrl Pts',(-19.5547543717507,-16.3651789962127,
121.911400782511)) ;
#73079 = CARTESIAN_POINT('Ctrl Pts',(-19.5256466039838,-16.185189915794,122.211483732283)) ;
#73080 = CARTESIAN_POINT('Ctrl Pts',(-19.294692522933,-16.3750740786748,121.908649507672)) ;
#73081 = CARTESIAN_POINT('Ctrl Pts',(-19.3175976958741,-16.195084998256,122.209284348646)) ;
#73082 = CARTESIAN_POINT('Ctrl Pts',(-19.0338948184635,-16.3851346241809,
121.951817978814)) ;
#73083 = CARTESIAN_POINT('Ctrl Pts',(-19.1089596094464,-16.2051455437621,
122.243820773441)) ;
#73084 = CARTESIAN_POINT('Ctrl Pts',(-18.7896903909364,-16.3949839314289,
122.03765160035)) ;
#73085 = CARTESIAN_POINT('Ctrl Pts',(-18.9135973885813,-16.2149948510101,
122.312488912832)) ;
#73086 = CARTESIAN_POINT('Ctrl Pts',(-18.5597221685073,-16.4050110215162,
122.166277137807)) ;
#73087 = CARTESIAN_POINT('Ctrl Pts',(-18.729623508621,-16.2250219410975,122.415390653368)) ;
#73088 = CARTESIAN_POINT('Ctrl Pts',(-18.355973838298,-16.4150399256532,122.33346171739)) ;
#73089 = CARTESIAN_POINT('Ctrl Pts',(-18.5666258270769,-16.2350508452344,
122.549139604119)) ;
#73090 = CARTESIAN_POINT('Ctrl Pts',(-18.1871403034402,-16.4248837907525,
122.529443722456)) ;
#73091 = CARTESIAN_POINT('Ctrl Pts',(-18.4315607383292,-16.2448947103337,
122.705925518047)) ;
#73092 = CARTESIAN_POINT('Ctrl Pts',(-18.0522973395216,-16.4348796174609,
122.754872248867)) ;
#73093 = CARTESIAN_POINT('Ctrl Pts',(-18.3236876314131,-16.2548905370421,
122.886268932754)) ;
#73094 = CARTESIAN_POINT('Ctrl Pts',(-17.9588203685042,-16.4449048341099,
123.001188739192)) ;
#73095 = CARTESIAN_POINT('Ctrl Pts',(-18.2489074300727,-16.2649157536911,
123.083322689755)) ;
#73096 = CARTESIAN_POINT('Ctrl Pts',(-17.909853990808,-16.4547946662675,123.256433493452)) ;
#73097 = CARTESIAN_POINT('Ctrl Pts',(-18.2097358498301,-16.2748055858487,
123.287518087541)) ;
#73098 = CARTESIAN_POINT('Ctrl Pts',(-17.9055514640211,-16.4647855223522,
123.518938743182)) ;
#73099 = CARTESIAN_POINT('Ctrl Pts',(-18.2062951731,-16.2847964419335,123.497522159626)) ;
#73100 = CARTESIAN_POINT('Ctrl Pts',(-17.9467544396273,-16.4747306169451,
123.777016725477)) ;
#73101 = CARTESIAN_POINT('Ctrl Pts',(-18.2392588287559,-16.2947415365263,
123.70398393257)) ;
#73102 = CARTESIAN_POINT('Ctrl Pts',(-18.0317409621934,-16.4846825207132,
124.024359260658)) ;
#73103 = CARTESIAN_POINT('Ctrl Pts',(-18.3072491056377,-16.3046934402944,
123.901857190127)) ;
#73104 = CARTESIAN_POINT('Ctrl Pts',(-18.159652183143,-16.4947189201826,124.255004194038)) ;
#73105 = CARTESIAN_POINT('Ctrl Pts',(-18.4095792698802,-16.3147298397639,
124.086372598792)) ;
#73106 = CARTESIAN_POINT('Ctrl Pts',(-18.3230928106585,-16.5046079902713,
124.457060170945)) ;
#73107 = CARTESIAN_POINT('Ctrl Pts',(-18.5403322885734,-16.3246189098525,
124.248016015903)) ;
#73108 = CARTESIAN_POINT('Ctrl Pts',(-18.5207993714394,-16.5145972796422,
124.629742950596)) ;
#73109 = CARTESIAN_POINT('Ctrl Pts',(-18.6984981684148,-16.3346081992234,
124.386161255533)) ;
#73110 = CARTESIAN_POINT('Ctrl Pts',(-18.7448946531259,-16.5245558458519,
124.76488924082)) ;
#73111 = CARTESIAN_POINT('Ctrl Pts',(-18.8777747171326,-16.3445667654331,
124.494277080252)) ;
#73112 = CARTESIAN_POINT('Ctrl Pts',(-18.987396430641,-16.5344554170687,124.859121187933)) ;
#73113 = CARTESIAN_POINT('Ctrl Pts',(-19.0717758652844,-16.3544663366499,
124.569661399205)) ;
#73114 = CARTESIAN_POINT('Ctrl Pts',(-19.2463751320927,-16.5445033314829,
124.910475054145)) ;
#73115 = CARTESIAN_POINT('Ctrl Pts',(-19.2789592074066,-16.3645142510642,
124.610743469147)) ;
#73116 = CARTESIAN_POINT('Ctrl Pts',(-19.5063926931737,-16.5543986743435,
124.91620248226)) ;
#73117 = CARTESIAN_POINT('Ctrl Pts',(-19.4869725482659,-16.3744095939248,
124.615324365784)) ;
#73118 = CARTESIAN_POINT('Ctrl Pts',(-19.7677103786789,-16.5644603682909,
124.876078188776)) ;
#73119 = CARTESIAN_POINT('Ctrl Pts',(-19.696026799547,-16.3844712878722,124.583223879591)) ;
#73120 = CARTESIAN_POINT('Ctrl Pts',(-20.0127402827486,-16.5743048213751,
124.793052261211)) ;
#73121 = CARTESIAN_POINT('Ctrl Pts',(-19.8920493950965,-16.3943157409564,
124.516802517793)) ;
#73122 = CARTESIAN_POINT('Ctrl Pts',(-20.2427297442012,-16.5842655063335,
124.6680922279)) ;
#73123 = CARTESIAN_POINT('Ctrl Pts',(-20.0760402661694,-16.4042764259148,
124.416833962095)) ;
#73124 = CARTESIAN_POINT('Ctrl Pts',(-20.4488151080384,-16.5943014388421,
124.503505578235)) ;
#73125 = CARTESIAN_POINT('Ctrl Pts',(-20.2409080798894,-16.4143123584233,
124.285163870932)) ;
#73126 = CARTESIAN_POINT('Ctrl Pts',(-20.6208188760599,-16.6041900545301,
124.308721850991)) ;
#73127 = CARTESIAN_POINT('Ctrl Pts',(-20.3785099279013,-16.4242009741114,
124.129336942414)) ;
#73128 = CARTESIAN_POINT('Ctrl Pts',(-20.7585722335936,-16.6142044636726,
124.084465548674)) ;
#73129 = CARTESIAN_POINT('Ctrl Pts',(-20.4887119985352,-16.4342153832538,
123.949931533889)) ;
#73130 = CARTESIAN_POINT('Ctrl Pts',(-20.8548321533235,-16.6242382726304,
123.839003471663)) ;
#73131 = CARTESIAN_POINT('Ctrl Pts',(-20.5657191556869,-16.4442491922116,
123.753561447325)) ;
#73132 = CARTESIAN_POINT('Ctrl Pts',(-20.9066678160013,-16.6340687268866,
123.585891332057)) ;
#73133 = CARTESIAN_POINT('Ctrl Pts',(-20.6071867566373,-16.4540796464678,
123.551072756513)) ;
#73134 = CARTESIAN_POINT('Ctrl Pts',(-20.9140293673925,-16.6441463944648,
123.321214560577)) ;
#73135 = CARTESIAN_POINT('Ctrl Pts',(-20.6130753215692,-16.464157314046,123.33933095717)) ;
#73136 = CARTESIAN_POINT('Ctrl Pts',(-20.8763072381655,-16.653998262587,123.065023312854)) ;
#73137 = CARTESIAN_POINT('Ctrl Pts',(-20.5828971286681,-16.4740091821683,
123.134379095039)) ;
#73138 = CARTESIAN_POINT('Ctrl Pts',(-20.7930831563035,-16.6640713001524,
122.813785638033)) ;
#73139 = CARTESIAN_POINT('Ctrl Pts',(-20.5163171841745,-16.4840822197336,
122.933388811495)) ;
#73140 = CARTESIAN_POINT('Ctrl Pts',(-20.6703077317906,-16.6739138535032,
122.586104119097)) ;
#73141 = CARTESIAN_POINT('Ctrl Pts',(-20.4180968468373,-16.4939247730845,
122.751244883158)) ;
#73142 = CARTESIAN_POINT('Ctrl Pts',(-20.5083311851296,-16.6838942489967,
122.379838432736)) ;
#73143 = CARTESIAN_POINT('Ctrl Pts',(-20.288515456469,-16.5039051685779,122.586232769824)) ;
#73144 = CARTESIAN_POINT('Ctrl Pts',(-20.3119093380156,-16.6939127269745,
122.204541346701)) ;
#73145 = CARTESIAN_POINT('Ctrl Pts',(-20.1313776273068,-16.5139236465557,
122.445995481957)) ;
#73146 = CARTESIAN_POINT('Ctrl Pts',(-20.0913143431078,-16.7037960412805,
122.067389838538)) ;
#73147 = CARTESIAN_POINT('Ctrl Pts',(-19.9549021776647,-16.5238069608618,
122.336275060039)) ;
#73148 = CARTESIAN_POINT('Ctrl Pts',(-19.8457714437435,-16.7138643438193,
121.968950139482)) ;
#73149 = CARTESIAN_POINT('Ctrl Pts',(-19.7584674011895,-16.5338752634005,
122.25752355759)) ;
#73150 = CARTESIAN_POINT('Ctrl Pts',(-19.5929691002769,-16.7236943910927,
121.91560728989)) ;
#73151 = CARTESIAN_POINT('Ctrl Pts',(-19.5562266645258,-16.543705310674,122.214849855465)) ;
#73152 = CARTESIAN_POINT('Ctrl Pts',(-19.3286263043333,-16.7337612625082,
121.906429428232)) ;
#73153 = CARTESIAN_POINT('Ctrl Pts',(-19.3447521004645,-16.5537721820895,
122.207507801228)) ;
#73154 = CARTESIAN_POINT('Ctrl Pts',(-19.0712701351288,-16.7436503013073,
121.942787563533)) ;
#73155 = CARTESIAN_POINT('Ctrl Pts',(-19.1388680389634,-16.5636612208885,
122.236594472759)) ;
#73156 = CARTESIAN_POINT('Ctrl Pts',(-18.8213494437406,-16.7536469994414,
122.02364571564)) ;
#73157 = CARTESIAN_POINT('Ctrl Pts',(-18.9389316809213,-16.5736579190226,
122.301281090436)) ;
#73158 = CARTESIAN_POINT('Ctrl Pts',(-18.5903042632467,-16.7635994251533,
122.146243992594)) ;
#73159 = CARTESIAN_POINT('Ctrl Pts',(-18.7540959986369,-16.5836103447346,
122.399359670759)) ;
#73160 = CARTESIAN_POINT('Ctrl Pts',(-18.3840928903676,-16.7735407273863,
122.306608387352)) ;
#73161 = CARTESIAN_POINT('Ctrl Pts',(-18.5891273551198,-16.5935516469676,
122.52765094837)) ;
#73162 = CARTESIAN_POINT('Ctrl Pts',(-18.2078769998156,-16.7835239664702,
122.501007316715)) ;
#73163 = CARTESIAN_POINT('Ctrl Pts',(-18.4481547970743,-16.6035348860515,
122.683169946801)) ;
#73164 = CARTESIAN_POINT('Ctrl Pts',(-18.067689740485,-16.7935627680388,122.724459360855)) ;
#73165 = CARTESIAN_POINT('Ctrl Pts',(-18.3360050210743,-16.6135736876201,
122.861931768501)) ;
#73166 = CARTESIAN_POINT('Ctrl Pts',(-17.969830608219,-16.8034108741604,122.964068373375)) ;
#73167 = CARTESIAN_POINT('Ctrl Pts',(-18.2577181420015,-16.6234217937417,
123.053617920861)) ;
#73168 = CARTESIAN_POINT('Ctrl Pts',(-17.9136507970271,-16.8134710697358,
123.222378870913)) ;
#73169 = CARTESIAN_POINT('Ctrl Pts',(-18.2127741641893,-16.633481989317,123.260266584404)) ;
#73170 = CARTESIAN_POINT('Ctrl Pts',(-17.9035805405926,-16.8233687530472,
123.482295776235)) ;
#73171 = CARTESIAN_POINT('Ctrl Pts',(-18.2047179840723,-16.6433796726285,
123.468199309359)) ;
#73172 = CARTESIAN_POINT('Ctrl Pts',(-17.9380616314296,-16.8332997934212,
123.740980891364)) ;
#73173 = CARTESIAN_POINT('Ctrl Pts',(-18.2323025565366,-16.6533107130024,
123.675146859333)) ;
#73174 = CARTESIAN_POINT('Ctrl Pts',(-18.0180896345586,-16.8433420110778,
123.992448629451)) ;
#73175 = CARTESIAN_POINT('Ctrl Pts',(-18.2963248642871,-16.6633529306591,
123.876321254892)) ;
#73176 = CARTESIAN_POINT('Ctrl Pts',(-18.1385099720365,-16.8532286718118,
124.222681786381)) ;
#73177 = CARTESIAN_POINT('Ctrl Pts',(-18.3926605542748,-16.673239591393,124.06050710284)) ;
#73178 = CARTESIAN_POINT('Ctrl Pts',(-18.2984195186838,-16.8632217804142,
124.43097259022)) ;
#73179 = CARTESIAN_POINT('Ctrl Pts',(-18.5205878453715,-16.6832326999955,
124.227139806063)) ;
#73180 = CARTESIAN_POINT('Ctrl Pts',(-18.4912243940238,-16.8731674790525,
124.607428923771)) ;
#73181 = CARTESIAN_POINT('Ctrl Pts',(-18.6748312019824,-16.6931783986337,
124.368304761902)) ;
#73182 = CARTESIAN_POINT('Ctrl Pts',(-18.711496354762,-16.8831147013235,124.748207213419)) ;
#73183 = CARTESIAN_POINT('Ctrl Pts',(-18.8510481570175,-16.7031256209048,
124.480927500203)) ;
#73184 = CARTESIAN_POINT('Ctrl Pts',(-18.9554062189345,-16.8931627269037,
124.849334419994)) ;
#73185 = CARTESIAN_POINT('Ctrl Pts',(-19.0461761012947,-16.7131736464849,
124.561829660936)) ;
#73186 = CARTESIAN_POINT('Ctrl Pts',(-19.2079801341347,-16.9030099740466,
124.905647600028)) ;
#73187 = CARTESIAN_POINT('Ctrl Pts',(-19.2482340537887,-16.7230208936278,
124.606880351078)) ;
#73188 = CARTESIAN_POINT('Ctrl Pts',(-19.4694948938872,-16.9129731511373,
124.918213293094)) ;
#73189 = CARTESIAN_POINT('Ctrl Pts',(-19.4574454686167,-16.7329840707186,
124.616933496724)) ;
#73190 = CARTESIAN_POINT('Ctrl Pts',(-19.7309060814747,-16.9230028721707,
124.884564981869)) ;
#73191 = CARTESIAN_POINT('Ctrl Pts',(-19.6665745634729,-16.743013791752,124.590015342495)) ;
#73192 = CARTESIAN_POINT('Ctrl Pts',(-19.9794823375519,-16.9329073397036,
124.807315147006)) ;
#73193 = CARTESIAN_POINT('Ctrl Pts',(-19.8654350540059,-16.7529182592849,
124.528216247189)) ;
#73194 = CARTESIAN_POINT('Ctrl Pts',(-20.2136657522084,-16.9429318255334,
124.686737651445)) ;
#73195 = CARTESIAN_POINT('Ctrl Pts',(-20.0527821064406,-16.7629427451146,
124.431754771356)) ;
#73196 = CARTESIAN_POINT('Ctrl Pts',(-20.4210159639658,-16.9528356606573,
124.529379524856)) ;
#73197 = CARTESIAN_POINT('Ctrl Pts',(-20.2186620983548,-16.7728465802385,
124.305869231909)) ;
#73198 = CARTESIAN_POINT('Ctrl Pts',(-20.6005228715883,-16.9628868513673,
124.33565635499)) ;
#73199 = CARTESIAN_POINT('Ctrl Pts',(-20.3622682531827,-16.7828977709485,
124.150891007985)) ;
#73200 = CARTESIAN_POINT('Ctrl Pts',(-20.7413629699218,-16.9727712940256,
124.117369250325)) ;
#73201 = CARTESIAN_POINT('Ctrl Pts',(-20.4749404514896,-16.7927822136068,
123.976262404854)) ;
#73202 = CARTESIAN_POINT('Ctrl Pts',(-20.8436992077545,-16.9827643018774,
123.875549411245)) ;
#73203 = CARTESIAN_POINT('Ctrl Pts',(-20.5568101194757,-16.8027752214587,
123.782806994121)) ;
#73204 = CARTESIAN_POINT('Ctrl Pts',(-20.9021522988049,-16.9927126215937,
123.620718922293)) ;
#73205 = CARTESIAN_POINT('Ctrl Pts',(-20.6035732565573,-16.812723541175,123.578943200647)) ;
#73206 = CARTESIAN_POINT('Ctrl Pts',(-20.91582621704,-17.0026494603032,123.359970070183)) ;
#73207 = CARTESIAN_POINT('Ctrl Pts',(-20.6145132340894,-16.8226603798844,
123.370344673644)) ;
#73208 = CARTESIAN_POINT('Ctrl Pts',(-20.8841917166136,-17.0126324492228,
123.099507780377)) ;
#73209 = CARTESIAN_POINT('Ctrl Pts',(-20.5892065993372,-16.832643368804,123.161974931273)) ;
#73210 = CARTESIAN_POINT('Ctrl Pts',(-20.8069010685589,-17.0226763285869,
122.847167752355)) ;
#73211 = CARTESIAN_POINT('Ctrl Pts',(-20.5273748335759,-16.8426872481681,
122.960102519886)) ;
#73212 = CARTESIAN_POINT('Ctrl Pts',(-20.6900614937302,-17.0325043939453,
122.616789554245)) ;
#73213 = CARTESIAN_POINT('Ctrl Pts',(-20.4339045684967,-16.8525153135265,
122.775800548252)) ;
#73214 = CARTESIAN_POINT('Ctrl Pts',(-20.5312178370852,-17.0425814825002,
122.404977089985)) ;
#73215 = CARTESIAN_POINT('Ctrl Pts',(-20.306830239219,-16.8625924020815,122.606349695402)) ;
#73216 = CARTESIAN_POINT('Ctrl Pts',(-20.3423853677135,-17.0524316346565,
122.227828485148)) ;
#73217 = CARTESIAN_POINT('Ctrl Pts',(-20.1557657033809,-16.8724425542378,
122.464630732549)) ;
#73218 = CARTESIAN_POINT('Ctrl Pts',(-20.1207672096657,-17.0625121151088,
122.082830799822)) ;
#73219 = CARTESIAN_POINT('Ctrl Pts',(-19.9784714607027,-16.8825230346901,
122.348631493821)) ;
#73220 = CARTESIAN_POINT('Ctrl Pts',(-19.8837370347765,-17.0723266128777,
121.981011738128)) ;
#73221 = CARTESIAN_POINT('Ctrl Pts',(-19.7888488634291,-16.8923375324589,
122.267175689381)) ;
#73222 = CARTESIAN_POINT('Ctrl Pts',(-19.6263495978727,-17.0823949088978,
121.919989507311)) ;
#73223 = CARTESIAN_POINT('Ctrl Pts',(-19.5829389187349,-16.9024058284791,
122.218356659132)) ;
#73224 = CARTESIAN_POINT('Ctrl Pts',(-19.3665898868757,-17.0922937413806,
121.904909547318)) ;
#73225 = CARTESIAN_POINT('Ctrl Pts',(-19.3751318865944,-16.9123046609618,
122.206291541471)) ;
#73226 = CARTESIAN_POINT('Ctrl Pts',(-19.1042454569166,-17.1023466213951,
121.935528536151)) ;
#73227 = CARTESIAN_POINT('Ctrl Pts',(-19.1652560101051,-16.9223575409764,
122.230785548798)) ;
#73228 = CARTESIAN_POINT('Ctrl Pts',(-18.8556383074816,-17.1122164368913,
122.00965239921)) ;
#73229 = CARTESIAN_POINT('Ctrl Pts',(-18.9663707255866,-16.9322273564725,
122.29008319219)) ;
#73230 = CARTESIAN_POINT('Ctrl Pts',(-18.618966820546,-17.1222891179741,122.128093849662)) ;
#73231 = CARTESIAN_POINT('Ctrl Pts',(-18.7770327094499,-16.9423000375553,
122.384835334691)) ;
#73232 = CARTESIAN_POINT('Ctrl Pts',(-18.4114058096266,-17.132121596545,122.282028735427)) ;
#73233 = CARTESIAN_POINT('Ctrl Pts',(-18.6109839479363,-16.9521325161263,
122.507981587497)) ;
#73234 = CARTESIAN_POINT('Ctrl Pts',(-18.2296195608036,-17.1421522305311,
122.472896223361)) ;
#73235 = CARTESIAN_POINT('Ctrl Pts',(-18.4655538438899,-16.9621631501124,
122.660674621782)) ;
#73236 = CARTESIAN_POINT('Ctrl Pts',(-18.0843508673433,-17.1521837877503,
122.692895741851)) ;
#73237 = CARTESIAN_POINT('Ctrl Pts',(-18.3493377687508,-16.9721947073315,
122.836673575722)) ;
#73238 = CARTESIAN_POINT('Ctrl Pts',(-17.9811153911421,-17.162013496622,122.92966578501)) ;
#73239 = CARTESIAN_POINT('Ctrl Pts',(-18.2667484984008,-16.9820244162032,
123.026088115789)) ;
#73240 = CARTESIAN_POINT('Ctrl Pts',(-17.9188078333547,-17.1720029454241,
123.184684449021)) ;
#73241 = CARTESIAN_POINT('Ctrl Pts',(-18.2169009623757,-16.9920138650053,
123.230102537214)) ;
#73242 = CARTESIAN_POINT('Ctrl Pts',(-17.9023020184727,-17.1820467978241,
123.448106892892)) ;
#73243 = CARTESIAN_POINT('Ctrl Pts',(-18.2036948702119,-17.0020577174053,
123.440840520039)) ;
#73244 = CARTESIAN_POINT('Ctrl Pts',(-17.93060345216,-17.1918685111562,123.704655127939)) ;
#73245 = CARTESIAN_POINT('Ctrl Pts',(-18.2263343758186,-17.0118794307374,
123.646078286481)) ;
#73246 = CARTESIAN_POINT('Ctrl Pts',(-18.0039709951869,-17.2019035161449,
123.957951976988)) ;
#73247 = CARTESIAN_POINT('Ctrl Pts',(-18.2850268365724,-17.0219144357261,
123.848716309395)) ;
#73248 = CARTESIAN_POINT('Ctrl Pts',(-18.1207470222398,-17.2119283545925,
124.194108297282)) ;
#73249 = CARTESIAN_POINT('Ctrl Pts',(-18.3784462993163,-17.0319392741737,
124.03764205884)) ;
#73250 = CARTESIAN_POINT('Ctrl Pts',(-18.273615812405,-17.2217805675477,124.403066982292)) ;
#73251 = CARTESIAN_POINT('Ctrl Pts',(-18.5007395422443,-17.0417914871289,
124.204809319358)) ;
#73252 = CARTESIAN_POINT('Ctrl Pts',(-18.4627330156094,-17.2317705237415,
124.585121418579)) ;
#73253 = CARTESIAN_POINT('Ctrl Pts',(-18.6520320121567,-17.0517814433227,
124.350453999726)) ;
#73254 = CARTESIAN_POINT('Ctrl Pts',(-18.6792511906534,-17.2416986340247,
124.730700896736)) ;
#73255 = CARTESIAN_POINT('Ctrl Pts',(-18.8252452509934,-17.061709553606,124.466918770551)) ;
#73256 = CARTESIAN_POINT('Ctrl Pts',(-18.9190395513251,-17.2516872341043,
124.837500135921)) ;
#73257 = CARTESIAN_POINT('Ctrl Pts',(-19.0170750943207,-17.0716981536855,
124.552359735373)) ;
#73258 = CARTESIAN_POINT('Ctrl Pts',(-19.1747837504995,-17.2617138260318,
124.900929840518)) ;
#73259 = CARTESIAN_POINT('Ctrl Pts',(-19.2216700660752,-17.081724745613,124.603105176145)) ;
#73260 = CARTESIAN_POINT('Ctrl Pts',(-19.433918408786,-17.271598954096,124.919007255926)) ;
#73261 = CARTESIAN_POINT('Ctrl Pts',(-19.4289770822547,-17.0916098736772,
124.617568828664)) ;
#73262 = CARTESIAN_POINT('Ctrl Pts',(-19.6951036459839,-17.2815900715695,
124.892117022708)) ;
#73263 = CARTESIAN_POINT('Ctrl Pts',(-19.6379253382598,-17.1016009911507,
124.596058506662)) ;
#73264 = CARTESIAN_POINT('Ctrl Pts',(-19.948740310072,-17.2916306874213,124.81939696296)) ;
#73265 = CARTESIAN_POINT('Ctrl Pts',(-19.8408352281527,-17.1116416070025,
124.537884144439)) ;
#73266 = CARTESIAN_POINT('Ctrl Pts',(-20.1811784262564,-17.301463678275,124.706518373468)) ;
#73267 = CARTESIAN_POINT('Ctrl Pts',(-20.0267858395131,-17.1214745978562,
124.447583262725)) ;
#73268 = CARTESIAN_POINT('Ctrl Pts',(-20.394335547211,-17.3114568097253,124.553138757131)) ;
#73269 = CARTESIAN_POINT('Ctrl Pts',(-20.1973125961385,-17.1314677293065,
124.324881214405)) ;
#73270 = CARTESIAN_POINT('Ctrl Pts',(-20.5779551583713,-17.3214888581607,
124.363950983879)) ;
#73271 = CARTESIAN_POINT('Ctrl Pts',(-20.3442096485662,-17.1414997777419,
124.17353227877)) ;
#73272 = CARTESIAN_POINT('Ctrl Pts',(-20.723726125488,-17.3313541047031,124.149582721449)) ;
#73273 = CARTESIAN_POINT('Ctrl Pts',(-20.4608276825751,-17.1513650242843,
124.002039230348)) ;
#73274 = CARTESIAN_POINT('Ctrl Pts',(-20.8317883621743,-17.3413159795299,
123.911130472927)) ;
#73275 = CARTESIAN_POINT('Ctrl Pts',(-20.5472792280348,-17.1613268991111,
123.811278448521)) ;
#73276 = CARTESIAN_POINT('Ctrl Pts',(-20.8968589918671,-17.3513509426412,
123.655591647124)) ;
#73277 = CARTESIAN_POINT('Ctrl Pts',(-20.5993376400282,-17.1713618622224,
123.606847845879)) ;
#73278 = CARTESIAN_POINT('Ctrl Pts',(-20.9167197830602,-17.3612357871036,
123.396550342785)) ;
#73279 = CARTESIAN_POINT('Ctrl Pts',(-20.6152282496205,-17.1812467066848,
123.399615406321)) ;
#73280 = CARTESIAN_POINT('Ctrl Pts',(-20.8907754477055,-17.3713018399443,
123.133346946216)) ;
#73281 = CARTESIAN_POINT('Ctrl Pts',(-20.5944747717883,-17.1913127595256,
123.189052373295)) ;
#73282 = CARTESIAN_POINT('Ctrl Pts',(-20.8213961193657,-17.3811393558533,
122.884260853047)) ;
#73283 = CARTESIAN_POINT('Ctrl Pts',(-20.5389734280671,-17.2011502754345,
122.989783496606)) ;
#73284 = CARTESIAN_POINT('Ctrl Pts',(-20.707493461148,-17.3912081039621,122.645486865897)) ;
#73285 = CARTESIAN_POINT('Ctrl Pts',(-20.4478531284103,-17.2112190235434,
122.798763308908)) ;
#73286 = CARTESIAN_POINT('Ctrl Pts',(-20.5566061674154,-17.4010886209932,
122.434129920222)) ;
#73287 = CARTESIAN_POINT('Ctrl Pts',(-20.3271452112243,-17.2210995405744,
122.629676886925)) ;
#73288 = CARTESIAN_POINT('Ctrl Pts',(-20.3696663137134,-17.4110798079276,
122.24982053188)) ;
#73289 = CARTESIAN_POINT('Ctrl Pts',(-20.1775948836073,-17.2310907275089,
122.482227931951)) ;
#73290 = CARTESIAN_POINT('Ctrl Pts',(-20.1543475644232,-17.4210328742026,
122.101259878742)) ;
#73291 = CARTESIAN_POINT('Ctrl Pts',(-20.0053412412653,-17.2410437937838,
122.363377768744)) ;
#73292 = CARTESIAN_POINT('Ctrl Pts',(-19.914546699615,-17.4310687117352,121.991540433693)) ;
#73293 = CARTESIAN_POINT('Ctrl Pts',(-19.8135014215866,-17.2510796313164,
122.275600286841)) ;
#73294 = CARTESIAN_POINT('Ctrl Pts',(-19.6630503154199,-17.4409588379466,
121.925907930573)) ;
#73295 = CARTESIAN_POINT('Ctrl Pts',(-19.6123051763993,-17.2609697575279,
122.223092308256)) ;
#73296 = CARTESIAN_POINT('Ctrl Pts',(-19.401369792171,-17.4509510198546,121.904306259292)) ;
#73297 = CARTESIAN_POINT('Ctrl Pts',(-19.4029610196723,-17.2709619394358,
122.205808818119)) ;
#73298 = CARTESIAN_POINT('Ctrl Pts',(-19.1411178680635,-17.4608969597931,
121.928446401785)) ;
#73299 = CARTESIAN_POINT('Ctrl Pts',(-19.1947594651076,-17.2809078793744,
122.22511876556)) ;
#73300 = CARTESIAN_POINT('Ctrl Pts',(-18.8888264116577,-17.4708441435572,
121.996908692717)) ;
#73301 = CARTESIAN_POINT('Ctrl Pts',(-18.9929258788226,-17.2908550631385,
122.279886435726)) ;
#73302 = CARTESIAN_POINT('Ctrl Pts',(-18.6500049664058,-17.4808920818647,
122.109521528278)) ;
#73303 = CARTESIAN_POINT('Ctrl Pts',(-18.8018677870459,-17.300903001446,122.369974738324)) ;
#73304 = CARTESIAN_POINT('Ctrl Pts',(-18.4385276907315,-17.490739716605,122.258681232151)) ;
#73305 = CARTESIAN_POINT('Ctrl Pts',(-18.6326849625005,-17.3107506361862,
122.489300526383)) ;
#73306 = CARTESIAN_POINT('Ctrl Pts',(-18.2534782916125,-17.5007014305788,
122.443832320231)) ;
#73307 = CARTESIAN_POINT('Ctrl Pts',(-18.4846439297647,-17.3207123501601,
122.637419744003)) ;
#73308 = CARTESIAN_POINT('Ctrl Pts',(-18.102637182743,-17.5107300653696,122.659957308394)) ;
#73309 = CARTESIAN_POINT('Ctrl Pts',(-18.3639692439427,-17.3307409849509,
122.810318436287)) ;
#73310 = CARTESIAN_POINT('Ctrl Pts',(-17.9928588042653,-17.5206403839668,
122.896109111967)) ;
#73311 = CARTESIAN_POINT('Ctrl Pts',(-18.2761445935121,-17.340651303548,122.999238788582)) ;
#73312 = CARTESIAN_POINT('Ctrl Pts',(-17.9249170447075,-17.5305752402783,
123.148201377901)) ;
#73313 = CARTESIAN_POINT('Ctrl Pts',(-18.2217890416061,-17.3505861598595,
123.200911914671)) ;
#73314 = CARTESIAN_POINT('Ctrl Pts',(-17.9017863180656,-17.540616476239,123.411046406639)) ;
#73315 = CARTESIAN_POINT('Ctrl Pts',(-18.2032822312824,-17.3606273958202,
123.411187703811)) ;
#73316 = CARTESIAN_POINT('Ctrl Pts',(-17.9240826084137,-17.550503247819,123.669927416852)) ;
#73317 = CARTESIAN_POINT('Ctrl Pts',(-18.221117014871,-17.3705141674002,123.618292577988)) ;
#73318 = CARTESIAN_POINT('Ctrl Pts',(-17.991434789248,-17.5605034265252,123.923904178017)) ;
#73319 = CARTESIAN_POINT('Ctrl Pts',(-18.274996565428,-17.3805143461064,123.821474510317)) ;
#73320 = CARTESIAN_POINT('Ctrl Pts',(-18.1007768932727,-17.5704207047348,
124.160520976259)) ;
#73321 = CARTESIAN_POINT('Ctrl Pts',(-18.3624681751621,-17.390431624316,124.010768829435)) ;
#73322 = CARTESIAN_POINT('Ctrl Pts',(-18.2515125585138,-17.5804679511484,
124.377250917373)) ;
#73323 = CARTESIAN_POINT('Ctrl Pts',(-18.4830548228013,-17.4004788707297,
124.184154022707)) ;
#73324 = CARTESIAN_POINT('Ctrl Pts',(-18.4342365121669,-17.5903418401297,
124.561534748414)) ;
#73325 = CARTESIAN_POINT('Ctrl Pts',(-18.6292323540018,-17.410352759711,124.331582640151)) ;
#73326 = CARTESIAN_POINT('Ctrl Pts',(-18.650076844133,-17.6004038577103,124.714221581085)) ;
#73327 = CARTESIAN_POINT('Ctrl Pts',(-18.8019032612626,-17.4204147772915,
124.453733907963)) ;
#73328 = CARTESIAN_POINT('Ctrl Pts',(-18.8846741124993,-17.6102749194446,
124.824958215728)) ;
#73329 = CARTESIAN_POINT('Ctrl Pts',(-18.9895801047362,-17.4302858390258,
124.542325248395)) ;
#73330 = CARTESIAN_POINT('Ctrl Pts',(-19.1378416764561,-17.6202689828049,
124.894832090655)) ;
#73331 = CARTESIAN_POINT('Ctrl Pts',(-19.1921135246435,-17.4402799023861,
124.598226499213)) ;
#73332 = CARTESIAN_POINT('Ctrl Pts',(-19.4003404043873,-17.6303011408383,
124.919197850821)) ;
#73333 = CARTESIAN_POINT('Ctrl Pts',(-19.4021122156701,-17.4503120604195,
124.617721341599)) ;
#73334 = CARTESIAN_POINT('Ctrl Pts',(-19.6587556166612,-17.6401650170784,
124.898540308971)) ;
#73335 = CARTESIAN_POINT('Ctrl Pts',(-19.6088446217045,-17.4601759366597,
124.601197540958)) ;
#73336 = CARTESIAN_POINT('Ctrl Pts',(-19.9148657636386,-17.6502355317167,
124.83200511838)) ;
#73337 = CARTESIAN_POINT('Ctrl Pts',(-19.8137332138143,-17.470246451298,124.54797155282)) ;
#73338 = CARTESIAN_POINT('Ctrl Pts',(-20.15009547768,-17.6600761686577,124.72452389288)) ;
#73339 = CARTESIAN_POINT('Ctrl Pts',(-20.0019179240621,-17.4800870882389,
124.461988673264)) ;
#73340 = CARTESIAN_POINT('Ctrl Pts',(-20.36628172174,-17.6700432974979,124.576684081939)) ;
#73341 = CARTESIAN_POINT('Ctrl Pts',(-20.1748686108959,-17.4900542170791,
124.343718154926)) ;
#73342 = CARTESIAN_POINT('Ctrl Pts',(-20.5542290543872,-17.6800572706224,
124.392466662708)) ;
#73343 = CARTESIAN_POINT('Ctrl Pts',(-20.3252263581462,-17.5000681902037,
124.196347578167)) ;
#73344 = CARTESIAN_POINT('Ctrl Pts',(-20.7574242466008,-17.6933420044857,
124.108563216876)) ;
#73345 = CARTESIAN_POINT('Ctrl Pts',(-20.487792909875,-17.5133529240669,123.969217895372)) ;
#73346 = CARTESIAN_POINT('Ctrl Pts',(-20.8815792328833,-17.7065672692004,
123.77977638725)) ;
#73347 = CARTESIAN_POINT('Ctrl Pts',(-20.5871211385938,-17.5265781887817,
123.706157444669)) ;
#73348 = CARTESIAN_POINT('Ctrl Pts',(-20.916715626838,-17.7198777917553,123.431719811704)) ;
#73349 = CARTESIAN_POINT('Ctrl Pts',(-20.6152233992077,-17.5398887113366,
123.427758937628)) ;
#73350 = CARTESIAN_POINT('Ctrl Pts',(-20.8970403046857,-17.7299064366575,
123.168922156218)) ;
#73351 = CARTESIAN_POINT('Ctrl Pts',(-20.599487173877,-17.5499173562387,123.217511388876)) ;
#73352 = CARTESIAN_POINT('Ctrl Pts',(-20.8332113375224,-17.7397874690114,
122.91722016416)) ;
#73353 = CARTESIAN_POINT('Ctrl Pts',(-20.5484257925112,-17.5597983885926,
123.016151680332)) ;
#73354 = CARTESIAN_POINT('Ctrl Pts',(-20.7260717927745,-17.7497684416915,
122.677813694356)) ;
#73355 = CARTESIAN_POINT('Ctrl Pts',(-20.4627150058846,-17.5697793612727,
122.824624299976)) ;
#73356 = CARTESIAN_POINT('Ctrl Pts',(-20.5788081877932,-17.7597495692775,
122.460780265019)) ;
#73357 = CARTESIAN_POINT('Ctrl Pts',(-20.3449101987234,-17.5797604888587,
122.650998991699)) ;
#73358 = CARTESIAN_POINT('Ctrl Pts',(-20.3368568947964,-17.7729927595389,
122.210535455746)) ;
#73359 = CARTESIAN_POINT('Ctrl Pts',(-20.1513291199415,-17.5930036791201,
122.450788794857)) ;
#73360 = CARTESIAN_POINT('Ctrl Pts',(-19.9569936985666,-17.7896607548997,
121.982786748416)) ;
#73361 = CARTESIAN_POINT('Ctrl Pts',(-19.8474794990023,-17.6096716744809,
122.26860190868)) ;
#73362 = CARTESIAN_POINT('Ctrl Pts',(-19.5259606159714,-17.8061812549117,
121.898720902047)) ;
#73363 = CARTESIAN_POINT('Ctrl Pts',(-19.5025885463891,-17.626192174493,122.201337274905)) ;
#73364 = CARTESIAN_POINT('Ctrl Pts',(-19.1769501917538,-17.8194942712277,
121.922374301819)) ;
#73365 = CARTESIAN_POINT('Ctrl Pts',(-19.2234321602598,-17.639505190809,122.220261939682)) ;
#73366 = CARTESIAN_POINT('Ctrl Pts',(-18.923841446365,-17.8294108294607,121.984571342108)) ;
#73367 = CARTESIAN_POINT('Ctrl Pts',(-19.0209334397387,-17.649421749042,122.270017435273)) ;
#73368 = CARTESIAN_POINT('Ctrl Pts',(-18.6828367950718,-17.8394384977636,
122.090994480647)) ;
#73369 = CARTESIAN_POINT('Ctrl Pts',(-18.8281336451652,-17.6594494173448,
122.355152451845)) ;
#73370 = CARTESIAN_POINT('Ctrl Pts',(-18.39451589716,-17.8526190875082,122.283176068352)) ;
#73371 = CARTESIAN_POINT('Ctrl Pts',(-18.5974653676165,-17.6726300070895,
122.50890583314)) ;
#73372 = CARTESIAN_POINT('Ctrl Pts',(-18.10101635581,-17.8693672266276,122.617564692497)) ;
#73373 = CARTESIAN_POINT('Ctrl Pts',(-18.3626740164398,-17.6893781462089,
122.776403445059)) ;
#73374 = CARTESIAN_POINT('Ctrl Pts',(-17.9093611844789,-17.8891619691382,
123.107788785558)) ;
#73375 = CARTESIAN_POINT('Ctrl Pts',(-18.2093429356618,-17.7091728887194,
123.168586034307)) ;
#73376 = CARTESIAN_POINT('Ctrl Pts',(-17.8958042830231,-17.909206361947,123.640179567823)) ;
#73377 = CARTESIAN_POINT('Ctrl Pts',(-18.198495043607,-17.7292172815282,123.594497346099)) ;
#73378 = CARTESIAN_POINT('Ctrl Pts',(-18.0635490482138,-17.9290455442457,
124.140228438877)) ;
#73379 = CARTESIAN_POINT('Ctrl Pts',(-18.3326878464618,-17.7490564638269,
123.994538700796)) ;
#73380 = CARTESIAN_POINT('Ctrl Pts',(-18.3920994919376,-17.9489708679386,
124.555410464729)) ;
#73381 = CARTESIAN_POINT('Ctrl Pts',(-18.5955264281991,-17.7689817875198,
124.3266864764)) ;
#73382 = CARTESIAN_POINT('Ctrl Pts',(-18.8427886963338,-17.9688945059901,
124.833584548263)) ;
#73383 = CARTESIAN_POINT('Ctrl Pts',(-18.9560768416233,-17.7889054255713,
124.549228339882)) ;
#73384 = CARTESIAN_POINT('Ctrl Pts',(-19.3612051307103,-17.9888193794556,
124.941403037261)) ;
#73385 = CARTESIAN_POINT('Ctrl Pts',(-19.3708100925674,-17.8088302990368,
124.635485728076)) ;
#73386 = CARTESIAN_POINT('Ctrl Pts',(-19.8842672961532,-18.0086979865345,
124.866686275116)) ;
#73387 = CARTESIAN_POINT('Ctrl Pts',(-19.7892612316858,-17.8287089061158,
124.575714277679)) ;
#73388 = CARTESIAN_POINT('Ctrl Pts',(-20.3528378763399,-18.0286754293665,
124.61697267285)) ;
#73389 = CARTESIAN_POINT('Ctrl Pts',(-20.1641187657695,-17.8486863489478,
124.375944971353)) ;
#73390 = CARTESIAN_POINT('Ctrl Pts',(-20.7070199752572,-18.0486072774512,
124.222957551438)) ;
#73391 = CARTESIAN_POINT('Ctrl Pts',(-20.4474662649599,-17.8686181970324,
124.060733674475)) ;
#73392 = CARTESIAN_POINT('Ctrl Pts',(-20.9055702119304,-18.0685025457937,
123.732901280478)) ;
#73393 = CARTESIAN_POINT('Ctrl Pts',(-20.6063082810486,-17.888513465375,123.668688213802)) ;
#73394 = CARTESIAN_POINT('Ctrl Pts',(-20.9255908589507,-18.0884250442059,
123.203759760793)) ;
#73395 = CARTESIAN_POINT('Ctrl Pts',(-20.622325941902,-17.9084359637871,123.245374181992)) ;
#73396 = CARTESIAN_POINT('Ctrl Pts',(-20.7634037511699,-18.1083845260819,
122.698638234476)) ;
#73397 = CARTESIAN_POINT('Ctrl Pts',(-20.4925770626071,-17.9283954456631,
122.84127622867)) ;
#73398 = CARTESIAN_POINT('Ctrl Pts',(-20.4400561873838,-18.1282622785412,
122.280931726658)) ;
#73399 = CARTESIAN_POINT('Ctrl Pts',(-20.2338986900793,-17.9482731981225,
122.507109352624)) ;
#73400 = CARTESIAN_POINT('Ctrl Pts',(-19.9941357017642,-18.1481440692758,
121.997211525616)) ;
#73401 = CARTESIAN_POINT('Ctrl Pts',(-19.8771609449229,-17.9681549888571,
122.280132520306)) ;
#73402 = CARTESIAN_POINT('Ctrl Pts',(-19.473136676443,-18.1682174081268,121.882665391147)) ;
#73403 = CARTESIAN_POINT('Ctrl Pts',(-19.4603626713499,-17.988228327708,122.188495684092)) ;
#73404 = CARTESIAN_POINT('Ctrl Pts',(-18.9512092801741,-18.1880218753626,
121.951729931277)) ;
#73405 = CARTESIAN_POINT('Ctrl Pts',(-19.0428183076886,-18.0080327949438,
122.243747774639)) ;
#73406 = CARTESIAN_POINT('Ctrl Pts',(-18.4795781027721,-18.2080052157704,
122.195819043175)) ;
#73407 = CARTESIAN_POINT('Ctrl Pts',(-18.665513625463,-18.0280161353516,122.43901994105)) ;
#73408 = CARTESIAN_POINT('Ctrl Pts',(-18.1213593078201,-18.2279201803684,
122.58549305673)) ;
#73409 = CARTESIAN_POINT('Ctrl Pts',(-18.3789384269809,-18.0479310999496,
122.750760357878)) ;
#73410 = CARTESIAN_POINT('Ctrl Pts',(-17.9166900270901,-18.2477887150847,
123.07239884694)) ;
#73411 = CARTESIAN_POINT('Ctrl Pts',(-18.2152038535447,-18.067799634666,123.140286849332)) ;
#73412 = CARTESIAN_POINT('Ctrl Pts',(-17.8910961295318,-18.2678410992965,
123.604588275997)) ;
#73413 = CARTESIAN_POINT('Ctrl Pts',(-18.1947300898754,-18.0878520188777,
123.566037963837)) ;
#73414 = CARTESIAN_POINT('Ctrl Pts',(-18.0458895721148,-18.2876150630857,
124.107054946162)) ;
#73415 = CARTESIAN_POINT('Ctrl Pts',(-18.3185671783008,-18.1076259826669,
123.968012895512)) ;
#73416 = CARTESIAN_POINT('Ctrl Pts',(-18.3667637787931,-18.307669442107,124.53239666569)) ;
#73417 = CARTESIAN_POINT('Ctrl Pts',(-18.5752679245152,-18.1276803616883,
124.308284615384)) ;
#73418 = CARTESIAN_POINT('Ctrl Pts',(-18.8082021318199,-18.3274661796803,
124.819004328832)) ;
#73419 = CARTESIAN_POINT('Ctrl Pts',(-18.9284212935939,-18.1474770992615,
124.537569929665)) ;
#73420 = CARTESIAN_POINT('Ctrl Pts',(-19.3247749684694,-18.3474339920317,
124.940168786591)) ;
#73421 = CARTESIAN_POINT('Ctrl Pts',(-19.3416804332519,-18.167444911613,124.634498827263)) ;
#73422 = CARTESIAN_POINT('Ctrl Pts',(-19.8515753100057,-18.3673929680968,
124.876958419537)) ;
#73423 = CARTESIAN_POINT('Ctrl Pts',(-19.7631206608013,-18.187403887678,124.583927892231)) ;
#73424 = CARTESIAN_POINT('Ctrl Pts',(-20.3237057375478,-18.3872878863742,
124.638896796403)) ;
#73425 = CARTESIAN_POINT('Ctrl Pts',(-20.140824401647,-18.2072988059554,124.393475677266)) ;
#73426 = CARTESIAN_POINT('Ctrl Pts',(-20.6867396805828,-18.4071841988245,
124.254454113003)) ;
#73427 = CARTESIAN_POINT('Ctrl Pts',(-20.4312497270068,-18.2271951184057,
124.085918852288)) ;
#73428 = CARTESIAN_POINT('Ctrl Pts',(-20.8974889910518,-18.4270921321986,
123.769075405449)) ;
#73429 = CARTESIAN_POINT('Ctrl Pts',(-20.5998462757639,-18.2471030517799,
123.697614033343)) ;
#73430 = CARTESIAN_POINT('Ctrl Pts',(-20.9299591275566,-18.4470420224871,
123.239880881326)) ;
#73431 = CARTESIAN_POINT('Ctrl Pts',(-20.6258188645366,-18.2670529420683,
123.274257946613)) ;
#73432 = CARTESIAN_POINT('Ctrl Pts',(-20.7809301919125,-18.4669192529884,
122.732978965345)) ;
#73433 = CARTESIAN_POINT('Ctrl Pts',(-20.5065921666265,-18.2869301725696,
122.868736840689)) ;
#73434 = CARTESIAN_POINT('Ctrl Pts',(-20.4664719535543,-18.4869019218594,
122.305004321839)) ;
#73435 = CARTESIAN_POINT('Ctrl Pts',(-20.2550218602243,-18.3069128414406,
122.526359509871)) ;
#73436 = CARTESIAN_POINT('Ctrl Pts',(-20.0256670326503,-18.5068348084397,
122.011010323999)) ;
#73437 = CARTESIAN_POINT('Ctrl Pts',(-19.9023778434081,-18.326845728021,122.291166823134)) ;
#73438 = CARTESIAN_POINT('Ctrl Pts',(-19.5117084694472,-18.5267475544577,
121.884894904179)) ;
#73439 = CARTESIAN_POINT('Ctrl Pts',(-19.4912012916676,-18.3467584740389,
122.190280271835)) ;
#73440 = CARTESIAN_POINT('Ctrl Pts',(-19.073811833589,-18.5433172757995,121.931691304988)) ;
#73441 = CARTESIAN_POINT('Ctrl Pts',(-19.140910274212,-18.3633281953808,122.227714621675)) ;
#73442 = CARTESIAN_POINT('Ctrl Pts',(-18.7476501459948,-18.5566172871045,
122.057314468822)) ;
#73443 = CARTESIAN_POINT('Ctrl Pts',(-18.8799531105504,-18.3766282066857,
122.32822609425)) ;
#73444 = CARTESIAN_POINT('Ctrl Pts',(-18.4486656985439,-18.5698874748544,
122.236842368707)) ;
#73445 = CARTESIAN_POINT('Ctrl Pts',(-18.6408115504094,-18.3898983944356,
122.471815668889)) ;
#73446 = CARTESIAN_POINT('Ctrl Pts',(-18.1413722272559,-18.5865148572198,
122.554451895043)) ;
#73447 = CARTESIAN_POINT('Ctrl Pts',(-18.3949285205775,-18.406525776801,122.72595265338)) ;
#73448 = CARTESIAN_POINT('Ctrl Pts',(-17.9611265355319,-18.603137146965,122.957810899834)) ;
#73449 = CARTESIAN_POINT('Ctrl Pts',(-18.2507608262965,-18.4231480665462,
123.048601618741)) ;
#73450 = CARTESIAN_POINT('Ctrl Pts',(-17.9059528960428,-18.6163823613595,
123.301475150402)) ;
#73451 = CARTESIAN_POINT('Ctrl Pts',(-18.2066124741129,-18.4363932809408,
123.323560293853)) ;
#73452 = CARTESIAN_POINT('Ctrl Pts',(-17.9091768533096,-18.6262943263202,
123.56194849763)) ;
#73453 = CARTESIAN_POINT('Ctrl Pts',(-18.2091963170387,-18.4463052459014,
123.53193369723)) ;
#73454 = CARTESIAN_POINT('Ctrl Pts',(-17.9585883654437,-18.6363529494846,
123.821589557135)) ;
#73455 = CARTESIAN_POINT('Ctrl Pts',(-18.2487269958253,-18.4563638690659,
123.739647432984)) ;
#73456 = CARTESIAN_POINT('Ctrl Pts',(-18.049960971692,-18.6461930636004,124.063536985051)) ;
#73457 = CARTESIAN_POINT('Ctrl Pts',(-18.3218274009337,-18.4662039831817,
123.933204397028)) ;
#73458 = CARTESIAN_POINT('Ctrl Pts',(-18.1847150492147,-18.6562588485581,
124.291112489649)) ;
#73459 = CARTESIAN_POINT('Ctrl Pts',(-18.4296324649852,-18.4762697681393,
124.11526364337)) ;
#73460 = CARTESIAN_POINT('Ctrl Pts',(-18.3539469882503,-18.666142166346,124.488176476343)) ;
#73461 = CARTESIAN_POINT('Ctrl Pts',(-18.5650197804419,-18.4861530859272,
124.272913430482)) ;
#73462 = CARTESIAN_POINT('Ctrl Pts',(-18.5565725703679,-18.6761316042045,
124.655035297665)) ;
#73463 = CARTESIAN_POINT('Ctrl Pts',(-18.7271216359093,-18.4961425237858,
124.406398725453)) ;
#73464 = CARTESIAN_POINT('Ctrl Pts',(-18.7845837389878,-18.6860953182573,
124.783781642354)) ;
#73465 = CARTESIAN_POINT('Ctrl Pts',(-18.9095316568693,-18.5061062378385,
124.509393835218)) ;
#73466 = CARTESIAN_POINT('Ctrl Pts',(-19.0321760408451,-18.6960903299165,
124.871518685356)) ;
#73467 = CARTESIAN_POINT('Ctrl Pts',(-19.1076061994151,-18.5161012494978,
124.579581328801)) ;
#73468 = CARTESIAN_POINT('Ctrl Pts',(-19.2923475774085,-18.7061266216107,
124.914699798587)) ;
#73469 = CARTESIAN_POINT('Ctrl Pts',(-19.3157437283926,-18.526137541192,124.614123995732)) ;
#73470 = CARTESIAN_POINT('Ctrl Pts',(-19.5511061455459,-18.7159729993042,
124.912522869841)) ;
#73471 = CARTESIAN_POINT('Ctrl Pts',(-19.5227505956409,-18.5359839188854,
124.612380200103)) ;
#73472 = CARTESIAN_POINT('Ctrl Pts',(-19.8091754394453,-18.7259579434549,
124.865290742825)) ;
#73473 = CARTESIAN_POINT('Ctrl Pts',(-19.7292055595761,-18.5459688630361,
124.574592283995)) ;
#73474 = CARTESIAN_POINT('Ctrl Pts',(-20.0540693302902,-18.7358949145848,
124.774521245397)) ;
#73475 = CARTESIAN_POINT('Ctrl Pts',(-19.9251198339151,-18.5559058341661,
124.50197459087)) ;
#73476 = CARTESIAN_POINT('Ctrl Pts',(-20.2819125649474,-18.7459446992166,
124.641024555296)) ;
#73477 = CARTESIAN_POINT('Ctrl Pts',(-20.1073932380398,-18.5659556187978,
124.395175312067)) ;
#73478 = CARTESIAN_POINT('Ctrl Pts',(-20.4792864442307,-18.755795161294,124.473508135912)) ;
#73479 = CARTESIAN_POINT('Ctrl Pts',(-20.2652908081466,-18.5758060808753,
124.261160516284)) ;
#73480 = CARTESIAN_POINT('Ctrl Pts',(-20.6471074504363,-18.7657671748145,
124.272284173906)) ;
#73481 = CARTESIAN_POINT('Ctrl Pts',(-20.3995458257233,-18.5857780943957,
124.100179977328)) ;
#73482 = CARTESIAN_POINT('Ctrl Pts',(-20.7777500987277,-18.7757623219339,
124.044367513395)) ;
#73483 = CARTESIAN_POINT('Ctrl Pts',(-20.5040579656922,-18.5957732415151,
123.917845587999)) ;
#73484 = CARTESIAN_POINT('Ctrl Pts',(-20.8668580982505,-18.78579629167,123.796222100958)) ;
#73485 = CARTESIAN_POINT('Ctrl Pts',(-20.5753422305749,-18.6058072112512,
123.719328523745)) ;
#73486 = CARTESIAN_POINT('Ctrl Pts',(-20.9111412971534,-18.7956518373406,
123.541018035023)) ;
#73487 = CARTESIAN_POINT('Ctrl Pts',(-20.6107665482665,-18.6156627569218,
123.515165073301)) ;
#73488 = CARTESIAN_POINT('Ctrl Pts',(-20.9107995972863,-18.8056505943538,
123.278303845411)) ;
#73489 = CARTESIAN_POINT('Ctrl Pts',(-20.6104909554121,-18.6256615139351,
123.304993798075)) ;
#73490 = CARTESIAN_POINT('Ctrl Pts',(-20.8655454312837,-18.815547729591,123.02214521666)) ;
#73491 = CARTESIAN_POINT('Ctrl Pts',(-20.5742854776814,-18.6355586491722,
123.100067482626)) ;
#73492 = CARTESIAN_POINT('Ctrl Pts',(-20.775165350312,-18.8256008254306,122.773930212828)) ;
#73493 = CARTESIAN_POINT('Ctrl Pts',(-20.5019793282326,-18.6456117450119,
122.901496230122)) ;
#73494 = CARTESIAN_POINT('Ctrl Pts',(-20.6452882014152,-18.8354843341612,
122.548985779886)) ;
#73495 = CARTESIAN_POINT('Ctrl Pts',(-20.3980758193706,-18.6554952537425,
122.72154200763)) ;
#73496 = CARTESIAN_POINT('Ctrl Pts',(-20.4769328739759,-18.8454792068073,
122.347392525911)) ;
#73497 = CARTESIAN_POINT('Ctrl Pts',(-20.2633899435099,-18.6654901263886,
122.56026886385)) ;
#73498 = CARTESIAN_POINT('Ctrl Pts',(-20.2753461931263,-18.855499168443,122.177967546798)) ;
#73499 = CARTESIAN_POINT('Ctrl Pts',(-20.1021192027833,-18.6755100880243,
122.424730580812)) ;
#73500 = CARTESIAN_POINT('Ctrl Pts',(-20.0501362495911,-18.8654045322428,
122.047445707161)) ;
#73501 = CARTESIAN_POINT('Ctrl Pts',(-19.9219503672684,-18.6854154518241,
122.320315127144)) ;
#73502 = CARTESIAN_POINT('Ctrl Pts',(-19.8050116122457,-18.8753451198504,
121.957195984755)) ;
#73503 = CARTESIAN_POINT('Ctrl Pts',(-19.7258501182768,-18.6953560394316,
122.248117437871)) ;
#73504 = CARTESIAN_POINT('Ctrl Pts',(-19.546310543461,-18.885347937951,121.91043255485)) ;
#73505 = CARTESIAN_POINT('Ctrl Pts',(-19.5188889496675,-18.7053588575323,
122.21070880072)) ;
#73506 = CARTESIAN_POINT('Ctrl Pts',(-19.2826245313338,-18.8953826496752,
121.909724812261)) ;
#73507 = CARTESIAN_POINT('Ctrl Pts',(-19.307940120733,-18.7153935692564,122.21014477667)) ;
#73508 = CARTESIAN_POINT('Ctrl Pts',(-19.0276297317508,-18.9052275564125,
121.953532899853)) ;
#73509 = CARTESIAN_POINT('Ctrl Pts',(-19.1039450889391,-18.7252384759937,
122.245193267705)) ;
#73510 = CARTESIAN_POINT('Ctrl Pts',(-18.7805173028943,-18.9152134089815,
122.041718001938)) ;
#73511 = CARTESIAN_POINT('Ctrl Pts',(-18.906255967733,-18.7352243285627,122.315743268288)) ;
#73512 = CARTESIAN_POINT('Ctrl Pts',(-18.5534655976855,-18.9251482173945,
122.170689853557)) ;
#73513 = CARTESIAN_POINT('Ctrl Pts',(-18.7246158475465,-18.7451591369758,
122.418922408914)) ;
#73514 = CARTESIAN_POINT('Ctrl Pts',(-18.3499886137343,-18.9352057444756,
122.339308389703)) ;
#73515 = CARTESIAN_POINT('Ctrl Pts',(-18.5618355205911,-18.7552166640568,
122.553818905849)) ;
#73516 = CARTESIAN_POINT('Ctrl Pts',(-18.1825491267015,-18.9450273994727,
122.535766487473)) ;
#73517 = CARTESIAN_POINT('Ctrl Pts',(-18.4278858915271,-18.7650383190539,
122.710986228041)) ;
#73518 = CARTESIAN_POINT('Ctrl Pts',(-18.0482437941304,-18.9550834436457,
122.76333018738)) ;
#73519 = CARTESIAN_POINT('Ctrl Pts',(-18.3204432872126,-18.775094363227,122.893038272163)) ;
#73520 = CARTESIAN_POINT('Ctrl Pts',(-17.956984649217,-18.9650241836909,123.008115620712)) ;
#73521 = CARTESIAN_POINT('Ctrl Pts',(-18.2474379774065,-18.7850351032721,
123.08886708059)) ;
#73522 = CARTESIAN_POINT('Ctrl Pts',(-17.9089873947582,-18.9749283047637,
123.263925149261)) ;
#73523 = CARTESIAN_POINT('Ctrl Pts',(-18.2090421543443,-18.794939224345,123.293514641434)) ;
#73524 = CARTESIAN_POINT('Ctrl Pts',(-17.9062567713338,-18.984975845918,123.527931134954)) ;
#73525 = CARTESIAN_POINT('Ctrl Pts',(-18.2068596105166,-18.8049867654992,
123.504719530089)) ;
#73526 = CARTESIAN_POINT('Ctrl Pts',(-17.9485884795038,-18.9948745975184,
123.784627499335)) ;
#73527 = CARTESIAN_POINT('Ctrl Pts',(-18.2407268052107,-18.8148855170996,
123.710075859708)) ;
#73528 = CARTESIAN_POINT('Ctrl Pts',(-18.0360231030446,-19.0049230764842,
124.033764662954)) ;
#73529 = CARTESIAN_POINT('Ctrl Pts',(-18.3106763436582,-18.8249339960654,
123.909385048735)) ;
#73530 = CARTESIAN_POINT('Ctrl Pts',(-18.1633256706867,-19.0148105735679,
124.260307326512)) ;
#73531 = CARTESIAN_POINT('Ctrl Pts',(-18.4125198128121,-18.8348214931492,
124.09061779922)) ;
#73532 = CARTESIAN_POINT('Ctrl Pts',(-18.3293793931131,-19.024803663866,124.463720725773)) ;
#73533 = CARTESIAN_POINT('Ctrl Pts',(-18.5453641388487,-18.8448145834472,
124.253347258974)) ;
#73534 = CARTESIAN_POINT('Ctrl Pts',(-18.5275042406055,-19.0347558339263,
124.634466519948)) ;
#73535 = CARTESIAN_POINT('Ctrl Pts',(-18.7038650100524,-18.8547667535075,
124.389942302569)) ;
#73536 = CARTESIAN_POINT('Ctrl Pts',(-18.7517438317054,-19.0446942538408,
124.768323296915)) ;
#73537 = CARTESIAN_POINT('Ctrl Pts',(-18.8832572996416,-18.864705173422,124.497025999753)) ;
#73538 = CARTESIAN_POINT('Ctrl Pts',(-18.9969024435073,-19.0546793839264,
124.861939962905)) ;
#73539 = CARTESIAN_POINT('Ctrl Pts',(-19.079384667915,-18.8746903035076,124.571917644386)) ;
#73540 = CARTESIAN_POINT('Ctrl Pts',(-19.2559540582283,-19.0647160733405,
124.911430511903)) ;
#73541 = CARTESIAN_POINT('Ctrl Pts',(-19.286626370737,-18.8847269929217,124.611508315008)) ;
#73542 = CARTESIAN_POINT('Ctrl Pts',(-19.5149158429189,-19.074570757333,124.915534596045)) ;
#73543 = CARTESIAN_POINT('Ctrl Pts',(-19.4937950895379,-18.8945816769142,
124.614789827494)) ;
#73544 = CARTESIAN_POINT('Ctrl Pts',(-19.7744035154706,-19.0845702413808,
124.874379795797)) ;
#73545 = CARTESIAN_POINT('Ctrl Pts',(-19.7013848578054,-18.9045811609621,
124.581864340682)) ;
#73546 = CARTESIAN_POINT('Ctrl Pts',(-20.0203843648942,-19.0944653301577,
124.789921645729)) ;
#73547 = CARTESIAN_POINT('Ctrl Pts',(-19.898168451651,-18.914476249739,124.514296469915)) ;
#73548 = CARTESIAN_POINT('Ctrl Pts',(-20.2516876995476,-19.1045258848039,
124.661945764437)) ;
#73549 = CARTESIAN_POINT('Ctrl Pts',(-20.0832104950723,-18.9245368043851,
124.41191423788)) ;
#73550 = CARTESIAN_POINT('Ctrl Pts',(-20.4530733453764,-19.1143751491768,
124.49932172969)) ;
#73551 = CARTESIAN_POINT('Ctrl Pts',(-20.2443173510078,-18.934386068758,124.281814281811)) ;
#73552 = CARTESIAN_POINT('Ctrl Pts',(-20.6267212720939,-19.1244024016246,
124.301134264947)) ;
#73553 = CARTESIAN_POINT('Ctrl Pts',(-20.3832345959501,-18.9444133212059,
124.123263308682)) ;
#73554 = CARTESIAN_POINT('Ctrl Pts',(-20.7627508778344,-19.1344306991948,
124.075408616425)) ;
#73555 = CARTESIAN_POINT('Ctrl Pts',(-20.4920569238612,-18.954441618776,123.942681905956)) ;
#73556 = CARTESIAN_POINT('Ctrl Pts',(-20.8562554222548,-19.1442768282008,
123.834159661691)) ;
#73557 = CARTESIAN_POINT('Ctrl Pts',(-20.5668588165386,-18.964287747782,123.749683032266)) ;
#73558 = CARTESIAN_POINT('Ctrl Pts',(-20.9078510941578,-19.1542707335628,
123.576649296548)) ;
#73559 = CARTESIAN_POINT('Ctrl Pts',(-20.6081339643689,-18.9742816531441,
123.543674604084)) ;
#73560 = CARTESIAN_POINT('Ctrl Pts',(-20.9134974108288,-19.1642948312459,
123.313280162655)) ;
#73561 = CARTESIAN_POINT('Ctrl Pts',(-20.6126495326501,-18.9843057508271,
123.332979224958)) ;
#73562 = CARTESIAN_POINT('Ctrl Pts',(-20.8741896283394,-19.1741846590999,
123.056370784483)) ;
#73563 = CARTESIAN_POINT('Ctrl Pts',(-20.5812020083466,-18.9941955786812,
123.127452614158)) ;
#73564 = CARTESIAN_POINT('Ctrl Pts',(-20.7903778747914,-19.1841766405303,
122.807538053467)) ;
#73565 = CARTESIAN_POINT('Ctrl Pts',(-20.5141513809669,-19.0041875601116,
122.928386999942)) ;
#73566 = CARTESIAN_POINT('Ctrl Pts',(-20.665139925764,-19.1941236452962,122.578095153236)) ;
#73567 = CARTESIAN_POINT('Ctrl Pts',(-20.41396002509,-19.0141345648774,122.744833684279)) ;
#73568 = CARTESIAN_POINT('Ctrl Pts',(-20.5022911488211,-19.204073296686,122.373520731225)) ;
#73569 = CARTESIAN_POINT('Ctrl Pts',(-20.2836802639546,-19.0240842162672,
122.581175227014)) ;
#73570 = CARTESIAN_POINT('Ctrl Pts',(-20.304546822287,-19.2141102996634,122.19898292141)) ;
#73571 = CARTESIAN_POINT('Ctrl Pts',(-20.125483863784,-19.0341212192446,122.441545883708)) ;
#73572 = CARTESIAN_POINT('Ctrl Pts',(-20.0829020054006,-19.2239992080984,
122.063295386289)) ;
#73573 = CARTESIAN_POINT('Ctrl Pts',(-19.9481679801292,-19.0440101276797,
122.332997314253)) ;
#73574 = CARTESIAN_POINT('Ctrl Pts',(-19.838797485772,-19.2339885405759,121.966751761761)) ;
#73575 = CARTESIAN_POINT('Ctrl Pts',(-19.7528840990243,-19.0539994601571,
122.255763553244)) ;
#73576 = CARTESIAN_POINT('Ctrl Pts',(-19.5823918613862,-19.243947096013,121.914413714457)) ;
#73577 = CARTESIAN_POINT('Ctrl Pts',(-19.547759698978,-19.0639580155942,122.213894361448)) ;
#73578 = CARTESIAN_POINT('Ctrl Pts',(-19.3223367513851,-19.2538466672135,
121.906790613273)) ;
#73579 = CARTESIAN_POINT('Ctrl Pts',(-19.3397162836837,-19.0738575867947,
122.20779695611)) ;
#73580 = CARTESIAN_POINT('Ctrl Pts',(-19.0611077173771,-19.2638945924655,
121.945087876707)) ;
#73581 = CARTESIAN_POINT('Ctrl Pts',(-19.1307330399337,-19.0839055120467,
122.23843585839)) ;
#73582 = CARTESIAN_POINT('Ctrl Pts',(-18.814173133089,-19.2737898919915,122.026726024973)) ;
#73583 = CARTESIAN_POINT('Ctrl Pts',(-18.9331863897438,-19.0938008115727,
122.303747125533)) ;
#73584 = CARTESIAN_POINT('Ctrl Pts',(-18.5813585769852,-19.2838517484394,
122.152010675361)) ;
#73585 = CARTESIAN_POINT('Ctrl Pts',(-18.7469349998699,-19.1038626680207,
122.403975871039)) ;
#73586 = CARTESIAN_POINT('Ctrl Pts',(-18.3782635158702,-19.2936955948561,
122.312252866395)) ;
#73587 = CARTESIAN_POINT('Ctrl Pts',(-18.5844604094953,-19.1137065144373,
122.53216976341)) ;
#73588 = CARTESIAN_POINT('Ctrl Pts',(-18.2033377996741,-19.3036585439841,
122.507039819568)) ;
#73589 = CARTESIAN_POINT('Ctrl Pts',(-18.4445206716217,-19.1236694635654,
122.687999590902)) ;
#73590 = CARTESIAN_POINT('Ctrl Pts',(-18.0642605165133,-19.3136925804121,
122.731072713043)) ;
#73591 = CARTESIAN_POINT('Ctrl Pts',(-18.3332595529383,-19.1337034999934,
122.867226472839)) ;
#73592 = CARTESIAN_POINT('Ctrl Pts',(-17.9673787965976,-19.3235800073702,
122.972163161429)) ;
#73593 = CARTESIAN_POINT('Ctrl Pts',(-18.2557552582931,-19.1435909269514,
123.060098390728)) ;
#73594 = CARTESIAN_POINT('Ctrl Pts',(-17.9126484520126,-19.3335944417065,
123.229596243484)) ;
#73595 = CARTESIAN_POINT('Ctrl Pts',(-18.2119716852264,-19.1536053612878,
123.266044996015)) ;
#73596 = CARTESIAN_POINT('Ctrl Pts',(-17.9040917215466,-19.3436293863415,
123.493147352363)) ;
#73597 = CARTESIAN_POINT('Ctrl Pts',(-18.2051271768608,-19.1636403059227,
123.476886022838)) ;
#73598 = CARTESIAN_POINT('Ctrl Pts',(-17.9399787130292,-19.3534617363725,
123.749059430695)) ;
#73599 = CARTESIAN_POINT('Ctrl Pts',(-18.2338373040545,-19.1734726559537,
123.681614412356)) ;
#73600 = CARTESIAN_POINT('Ctrl Pts',(-18.0216292179886,-19.3635371754897,
124.00087385618)) ;
#73601 = CARTESIAN_POINT('Ctrl Pts',(-18.2991584729874,-19.183548095071,123.883066086777)) ;
#73602 = CARTESIAN_POINT('Ctrl Pts',(-18.1429328956013,-19.3733896407243,
124.229675102656)) ;
#73603 = CARTESIAN_POINT('Ctrl Pts',(-18.396201496122,-19.1934005603056,124.066105849519)) ;
#73604 = CARTESIAN_POINT('Ctrl Pts',(-18.3054527183703,-19.3834625183012,
124.43855780688)) ;
#73605 = CARTESIAN_POINT('Ctrl Pts',(-18.5262180422587,-19.2034734378824,
124.23321192103)) ;
#73606 = CARTESIAN_POINT('Ctrl Pts',(-18.4973580639054,-19.3933051144937,
124.612009431565)) ;
#73607 = CARTESIAN_POINT('Ctrl Pts',(-18.6797418858111,-19.2133160340749,
124.371972008953)) ;
#73608 = CARTESIAN_POINT('Ctrl Pts',(-18.7190343990378,-19.403285498609,124.752157350423)) ;
#73609 = CARTESIAN_POINT('Ctrl Pts',(-18.8570829522641,-19.2232964181902,
124.4840898822)) ;
#73610 = CARTESIAN_POINT('Ctrl Pts',(-18.9628028394589,-19.4133039792578,
124.851593566048)) ;
#73611 = CARTESIAN_POINT('Ctrl Pts',(-19.0520979082859,-19.233314898839,124.56363837805)) ;
#73612 = CARTESIAN_POINT('Ctrl Pts',(-19.2165815610818,-19.4231872942581,
124.906993129044)) ;
#73613 = CARTESIAN_POINT('Ctrl Pts',(-19.2551201081469,-19.2431982138394,
124.607957472016)) ;
#73614 = CARTESIAN_POINT('Ctrl Pts',(-19.4809103809745,-19.4332555913486,
124.917562972761)) ;
#73615 = CARTESIAN_POINT('Ctrl Pts',(-19.4665835088432,-19.2532665109298,
124.616412951815)) ;
#73616 = CARTESIAN_POINT('Ctrl Pts',(-19.736986666509,-19.4430856597209,124.883208337383)) ;
#73617 = CARTESIAN_POINT('Ctrl Pts',(-19.6714432710506,-19.2630965793021,
124.588929081079)) ;
#73618 = CARTESIAN_POINT('Ctrl Pts',(-19.9891462344599,-19.4531524521893,
124.803370269059)) ;
#73619 = CARTESIAN_POINT('Ctrl Pts',(-19.8731711567886,-19.2731633717705,
124.525058292213)) ;
#73620 = CARTESIAN_POINT('Ctrl Pts',(-20.2195097660889,-19.4630417856778,
124.682973671284)) ;
#73621 = CARTESIAN_POINT('Ctrl Pts',(-20.0574610978455,-19.2830527052591,
124.428741164273)) ;
#73622 = CARTESIAN_POINT('Ctrl Pts',(-20.4279957456454,-19.4730439170939,
124.522983695166)) ;
#73623 = CARTESIAN_POINT('Ctrl Pts',(-20.2242496883146,-19.2930548366751,
124.300749114728)) ;
#73624 = CARTESIAN_POINT('Ctrl Pts',(-20.6043330328565,-19.4829677867149,
124.330784900603)) ;
#73625 = CARTESIAN_POINT('Ctrl Pts',(-20.3653190116598,-19.3029787062961,
124.146990434962)) ;
#73626 = CARTESIAN_POINT('Ctrl Pts',(-20.7461987471793,-19.4930113022321,
124.108267757286)) ;
#73627 = CARTESIAN_POINT('Ctrl Pts',(-20.4788115505222,-19.3130222218133,
123.968976491356)) ;
#73628 = CARTESIAN_POINT('Ctrl Pts',(-20.8459623354037,-19.5028935151204,
123.868447779217)) ;
#73629 = CARTESIAN_POINT('Ctrl Pts',(-20.5586220080263,-19.3229044347016,
123.77712130273)) ;
#73630 = CARTESIAN_POINT('Ctrl Pts',(-20.9036081810683,-19.5129615923398,
123.610275746696)) ;
#73631 = CARTESIAN_POINT('Ctrl Pts',(-20.6047386771519,-19.332972511921,123.570583349477)) ;
#73632 = CARTESIAN_POINT('Ctrl Pts',(-20.915515712549,-19.522800097074,123.351961006774)) ;
#73633 = CARTESIAN_POINT('Ctrl Pts',(-20.6142646315837,-19.3428110166552,
123.363932740499)) ;
#73634 = CARTESIAN_POINT('Ctrl Pts',(-20.8820171906125,-19.5328628655034,
123.089685129355)) ;
#73635 = CARTESIAN_POINT('Ctrl Pts',(-20.5874658526555,-19.3528737850846,
123.154111733586)) ;
#73636 = CARTESIAN_POINT('Ctrl Pts',(-20.8044967774728,-19.5427598587861,
122.841407511861)) ;
#73637 = CARTESIAN_POINT('Ctrl Pts',(-20.5254497644867,-19.3627707783674,
122.955490404283)) ;
#73638 = CARTESIAN_POINT('Ctrl Pts',(-20.6854165301344,-19.5526910864209,
122.60918260394)) ;
#73639 = CARTESIAN_POINT('Ctrl Pts',(-20.4301860313907,-19.3727020060021,
122.769710887484)) ;
#73640 = CARTESIAN_POINT('Ctrl Pts',(-20.5258305092585,-19.562733245063,122.39901017829)) ;
#73641 = CARTESIAN_POINT('Ctrl Pts',(-20.3025172352716,-19.3827441646443,
122.601572722186)) ;
#73642 = CARTESIAN_POINT('Ctrl Pts',(-20.3352897321576,-19.5726199545941,
122.222366967622)) ;
#73643 = CARTESIAN_POINT('Ctrl Pts',(-20.1500853867411,-19.3926308741753,
122.460258598056)) ;
#73644 = CARTESIAN_POINT('Ctrl Pts',(-20.1148863727612,-19.5826129270227,
122.079617245424)) ;
#73645 = CARTESIAN_POINT('Ctrl Pts',(-19.9737630061899,-19.4026238466039,
122.346058647369)) ;
#73646 = CARTESIAN_POINT('Ctrl Pts',(-19.874126422685,-19.5925591215593,121.977883229097)) ;
#73647 = CARTESIAN_POINT('Ctrl Pts',(-19.7811555923769,-19.4125700411405,
122.264671358312)) ;
#73648 = CARTESIAN_POINT('Ctrl Pts',(-19.6194821905601,-19.6025044964108,
121.91893843079)) ;
#73649 = CARTESIAN_POINT('Ctrl Pts',(-19.5774407611386,-19.422515415992,122.217515208665)) ;
#73650 = CARTESIAN_POINT('Ctrl Pts',(-19.3556280435148,-19.6125594157707,
121.905362356755)) ;
#73651 = CARTESIAN_POINT('Ctrl Pts',(-19.3663572165396,-19.4325703353519,
122.206654013868)) ;
#73652 = CARTESIAN_POINT('Ctrl Pts',(-19.0993869104876,-19.6223809352142,
121.936569596332)) ;
#73653 = CARTESIAN_POINT('Ctrl Pts',(-19.1613655396477,-19.4423918547954,
122.231619200685)) ;
#73654 = CARTESIAN_POINT('Ctrl Pts',(-18.8463008166407,-19.6324467039811,
122.01333370423)) ;
#73655 = CARTESIAN_POINT('Ctrl Pts',(-18.9588962140942,-19.4524576235623,
122.29303006788)) ;
#73656 = CARTESIAN_POINT('Ctrl Pts',(-18.614184741333,-19.6423486256361,122.131051371053)) ;
#73657 = CARTESIAN_POINT('Ctrl Pts',(-18.7732037818426,-19.4623595452174,
122.387203418498)) ;
#73658 = CARTESIAN_POINT('Ctrl Pts',(-18.4029852172984,-19.6523916844572,
122.289280682559)) ;
#73659 = CARTESIAN_POINT('Ctrl Pts',(-18.604243687009,-19.4724026040384,122.513786518166)) ;
#73660 = CARTESIAN_POINT('Ctrl Pts',(-18.2250106931332,-19.6622976784999,
122.479267826247)) ;
#73661 = CARTESIAN_POINT('Ctrl Pts',(-18.4618641781161,-19.4823085980811,
122.665775345268)) ;
#73662 = CARTESIAN_POINT('Ctrl Pts',(-18.0816334127858,-19.6722354515817,
122.697543077619)) ;
#73663 = CARTESIAN_POINT('Ctrl Pts',(-18.3471620419146,-19.4922463711629,
122.840394715573)) ;
#73664 = CARTESIAN_POINT('Ctrl Pts',(-17.9775290975299,-19.682275815314,122.939982086289)) ;
#73665 = CARTESIAN_POINT('Ctrl Pts',(-18.2638779349782,-19.5022867348952,
123.034345802999)) ;
#73666 = CARTESIAN_POINT('Ctrl Pts',(-17.9178270663796,-19.6921631590375,
123.192873036783)) ;
#73667 = CARTESIAN_POINT('Ctrl Pts',(-18.2161158243129,-19.5121740786187,
123.236657594822)) ;
#73668 = CARTESIAN_POINT('Ctrl Pts',(-17.9023535730021,-19.7021553896062,
123.454984271161)) ;
#73669 = CARTESIAN_POINT('Ctrl Pts',(-18.2037362398585,-19.5221663091874,
123.446346372631)) ;
#73670 = CARTESIAN_POINT('Ctrl Pts',(-17.9325684279104,-19.7121039173898,
123.714684335716)) ;
#73671 = CARTESIAN_POINT('Ctrl Pts',(-18.2279072969856,-19.532114836971,123.654106084101)) ;
#73672 = CARTESIAN_POINT('Ctrl Pts',(-18.0069653212784,-19.7220407011131,
123.964967568123)) ;
#73673 = CARTESIAN_POINT('Ctrl Pts',(-18.2874238319089,-19.5420516206943,
123.854332429313)) ;
#73674 = CARTESIAN_POINT('Ctrl Pts',(-18.1239596003207,-19.73202370191,124.199815869737)) ;
#73675 = CARTESIAN_POINT('Ctrl Pts',(-18.3810183152476,-19.5520346214913,
124.042211309555)) ;
#73676 = CARTESIAN_POINT('Ctrl Pts',(-18.2812582376319,-19.7420675887508,
124.411727571311)) ;
#73677 = CARTESIAN_POINT('Ctrl Pts',(-18.5068566460487,-19.562078508332,124.21174128928)) ;
#73678 = CARTESIAN_POINT('Ctrl Pts',(-18.4684715102888,-19.7518956123253,
124.58970605599)) ;
#73679 = CARTESIAN_POINT('Ctrl Pts',(-18.6566257534126,-19.5719065319066,
124.3541239909)) ;
#73680 = CARTESIAN_POINT('Ctrl Pts',(-18.689056614064,-19.761972860539,124.736130030158)) ;
#73681 = CARTESIAN_POINT('Ctrl Pts',(-18.8330935698082,-19.5819837801202,
124.471264200358)) ;
#73682 = CARTESIAN_POINT('Ctrl Pts',(-18.9262775518946,-19.7718224158442,
124.839850242378)) ;
#73683 = CARTESIAN_POINT('Ctrl Pts',(-19.0228689899652,-19.5918333354255,
124.554240926399)) ;
#73684 = CARTESIAN_POINT('Ctrl Pts',(-19.1837052991542,-19.781905124042,124.902304787764)) ;
#73685 = CARTESIAN_POINT('Ctrl Pts',(-19.2288112851542,-19.6019160436232,
124.604205685487)) ;
#73686 = CARTESIAN_POINT('Ctrl Pts',(-19.4410933758814,-19.7917177169684,
124.918904855349)) ;
#73687 = CARTESIAN_POINT('Ctrl Pts',(-19.434720478767,-19.6117286365497,124.61748677879)) ;
#73688 = CARTESIAN_POINT('Ctrl Pts',(-19.7040333399978,-19.8017849092264,
124.890266579445)) ;
#73689 = CARTESIAN_POINT('Ctrl Pts',(-19.6450728626718,-19.6217958288076,
124.594577333264)) ;
#73690 = CARTESIAN_POINT('Ctrl Pts',(-19.953852926939,-19.811683738689,124.817515981113)) ;
#73691 = CARTESIAN_POINT('Ctrl Pts',(-19.8449282229179,-19.6316946582702,
124.536378184494)) ;
#73692 = CARTESIAN_POINT('Ctrl Pts',(-20.1908446169336,-19.8217377298791,
124.700847328408)) ;
#73693 = CARTESIAN_POINT('Ctrl Pts',(-20.0345222842642,-19.6417486494604,
124.443044266715)) ;
#73694 = CARTESIAN_POINT('Ctrl Pts',(-20.4003396793583,-19.8316094546624,
124.547752149645)) ;
#73695 = CARTESIAN_POINT('Ctrl Pts',(-20.2021184087781,-19.6516203742436,
124.32056963313)) ;
#73696 = CARTESIAN_POINT('Ctrl Pts',(-20.5836646743315,-19.8416798967926,
124.356956666515)) ;
#73697 = CARTESIAN_POINT('Ctrl Pts',(-20.3487795243232,-19.6616908163738,
124.167933928758)) ;
#73698 = CARTESIAN_POINT('Ctrl Pts',(-20.7277380469085,-19.8515129752229,
124.142415105661)) ;
#73699 = CARTESIAN_POINT('Ctrl Pts',(-20.4640387321514,-19.6715238948041,
123.996302256258)) ;
#73700 = CARTESIAN_POINT('Ctrl Pts',(-20.8351448172692,-19.8615434487242,
123.901710971188)) ;
#73701 = CARTESIAN_POINT('Ctrl Pts',(-20.5499655097051,-19.6815543683055,
123.803739479692)) ;
#73702 = CARTESIAN_POINT('Ctrl Pts',(-20.8983935515043,-19.8715750480229,
123.645775745963)) ;
#73703 = CARTESIAN_POINT('Ctrl Pts',(-20.6005657740463,-19.6915859676042,
123.598991547224)) ;
#73704 = CARTESIAN_POINT('Ctrl Pts',(-20.9164189115972,-19.8814047490611,
123.388108112837)) ;
#73705 = CARTESIAN_POINT('Ctrl Pts',(-20.6149874004344,-19.7014156686424,
123.392858551262)) ;
#73706 = CARTESIAN_POINT('Ctrl Pts',(-20.8897697071989,-19.8913941871176,
123.126944309957)) ;
#73707 = CARTESIAN_POINT('Ctrl Pts',(-20.5936696114577,-19.7114051066988,
123.183927490661)) ;
#73708 = CARTESIAN_POINT('Ctrl Pts',(-20.8171461451354,-19.9014380903337,
122.873192498231)) ;
#73709 = CARTESIAN_POINT('Ctrl Pts',(-20.5355721095239,-19.7214490099149,
122.980925533021)) ;
#73710 = CARTESIAN_POINT('Ctrl Pts',(-20.7046073618449,-19.9112596111472,
122.640918152615)) ;
#73711 = CARTESIAN_POINT('Ctrl Pts',(-20.4455429052235,-19.7312705307284,
122.795106281435)) ;
#73712 = CARTESIAN_POINT('Ctrl Pts',(-20.5506673334874,-19.9212953353943,
122.426787436371)) ;
#73713 = CARTESIAN_POINT('Ctrl Pts',(-20.3223921809841,-19.7413062549755,
122.623800668938)) ;
#73714 = CARTESIAN_POINT('Ctrl Pts',(-20.361646906176,-19.9313174893268,122.243358309502)) ;
#73715 = CARTESIAN_POINT('Ctrl Pts',(-20.1711768967696,-19.751328408908,122.477056260967)) ;
#73716 = CARTESIAN_POINT('Ctrl Pts',(-20.147396817326,-19.9411797210841,122.097565987391)) ;
#73717 = CARTESIAN_POINT('Ctrl Pts',(-19.9997783728668,-19.7611906406653,
122.360421503876)) ;
#73718 = CARTESIAN_POINT('Ctrl Pts',(-19.9090443946138,-19.951138791542,121.989462309711)) ;
#73719 = CARTESIAN_POINT('Ctrl Pts',(-19.8090974023785,-19.7711497111232,
122.273937084454)) ;
#73720 = CARTESIAN_POINT('Ctrl Pts',(-19.6535218175542,-19.9611739639181,
121.924289992002)) ;
#73721 = CARTESIAN_POINT('Ctrl Pts',(-19.6046796893941,-19.7811848834994,
122.221797596013)) ;
#73722 = CARTESIAN_POINT('Ctrl Pts',(-19.3946113132466,-19.9710543490764,
121.904388967415)) ;
#73723 = CARTESIAN_POINT('Ctrl Pts',(-19.397552035366,-19.7910652686577,122.205875089908)) ;
#73724 = CARTESIAN_POINT('Ctrl Pts',(-19.1316102592224,-19.9811110636703,
121.930090607189)) ;
#73725 = CARTESIAN_POINT('Ctrl Pts',(-19.1871508676461,-19.8011219832516,
122.226434670213)) ;
#73726 = CARTESIAN_POINT('Ctrl Pts',(-18.8815248170263,-19.9909903322424,
121.999843995955)) ;
#73727 = CARTESIAN_POINT('Ctrl Pts',(-18.9870826419165,-19.8110012518237,
122.282235527794)) ;
#73728 = CARTESIAN_POINT('Ctrl Pts',(-18.6444106248793,-20.0009812897281,
122.112585153764)) ;
#73729 = CARTESIAN_POINT('Ctrl Pts',(-18.7973905924176,-19.8209922093093,
122.372426718099)) ;
#73730 = CARTESIAN_POINT('Ctrl Pts',(-18.4297462675424,-20.0110219483633,
122.266017180275)) ;
#73731 = CARTESIAN_POINT('Ctrl Pts',(-18.6256580184065,-19.8310328679445,
122.495170938252)) ;
#73732 = CARTESIAN_POINT('Ctrl Pts',(-18.2485010034017,-20.0208549280713,
122.450186849487)) ;
#73733 = CARTESIAN_POINT('Ctrl Pts',(-18.4806610287741,-19.8408658476525,
122.642504838089)) ;
#73734 = CARTESIAN_POINT('Ctrl Pts',(-18.0989811417454,-20.030848061321,122.6660694596)) ;
#73735 = CARTESIAN_POINT('Ctrl Pts',(-18.361043590352,-19.8508589809022,122.815209731099)) ;
#73736 = CARTESIAN_POINT('Ctrl Pts',(-17.9892812123843,-20.0408801137044,
122.905806909228)) ;
#73737 = CARTESIAN_POINT('Ctrl Pts',(-18.2732819325311,-19.8608910332856,
123.006998938251)) ;
#73738 = CARTESIAN_POINT('Ctrl Pts',(-17.9236747634942,-20.0507453426556,
123.156602970164)) ;
#73739 = CARTESIAN_POINT('Ctrl Pts',(-18.2207950630936,-19.8707562622369,
123.207634737405)) ;
#73740 = CARTESIAN_POINT('Ctrl Pts',(-17.901665291667,-20.0607072838989,123.417472522822)) ;
#73741 = CARTESIAN_POINT('Ctrl Pts',(-18.2031854905323,-19.8807182034801,
123.416330009112)) ;
#73742 = CARTESIAN_POINT('Ctrl Pts',(-17.9258798987478,-20.0707419989356,
123.680047914993)) ;
#73743 = CARTESIAN_POINT('Ctrl Pts',(-18.2225552242478,-19.8907529185169,
123.626390529728)) ;
#73744 = CARTESIAN_POINT('Ctrl Pts',(-17.9938945220798,-20.0806277692797,
123.930807070513)) ;
#73745 = CARTESIAN_POINT('Ctrl Pts',(-18.2769648599555,-19.9006386888609,
123.82699794779)) ;
#73746 = CARTESIAN_POINT('Ctrl Pts',(-18.1063688770827,-20.0906903666684,
124.170094182597)) ;
#73747 = CARTESIAN_POINT('Ctrl Pts',(-18.3669425672961,-19.9107012862497,
124.018428597259)) ;
#73748 = CARTESIAN_POINT('Ctrl Pts',(-18.2554062654067,-20.1005407785037,
124.381769206432)) ;
#73749 = CARTESIAN_POINT('Ctrl Pts',(-18.4861705070814,-19.9205516980849,
124.187769342642)) ;
#73750 = CARTESIAN_POINT('Ctrl Pts',(-18.4417280628566,-20.1105679477896,
124.568087270984)) ;
#73751 = CARTESIAN_POINT('Ctrl Pts',(-18.635226462847,-19.9305788673709,124.336825291195)) ;
#73752 = CARTESIAN_POINT('Ctrl Pts',(-18.6579883240509,-20.1205954285038,
124.718674943171)) ;
#73753 = CARTESIAN_POINT('Ctrl Pts',(-18.808233509183,-19.940606348085,124.457297090605)) ;
#73754 = CARTESIAN_POINT('Ctrl Pts',(-18.8924830332927,-20.1304384810831,
124.827831022271)) ;
#73755 = CARTESIAN_POINT('Ctrl Pts',(-18.9958279396515,-19.9504494006643,
124.544623631068)) ;
#73756 = CARTESIAN_POINT('Ctrl Pts',(-19.1460332396002,-20.1404323845217,
124.89628582595)) ;
#73757 = CARTESIAN_POINT('Ctrl Pts',(-19.1986674699778,-19.9604433041029,
124.599389529279)) ;
#73758 = CARTESIAN_POINT('Ctrl Pts',(-19.408537282864,-20.1504595072981,124.919271899811)) ;
#73759 = CARTESIAN_POINT('Ctrl Pts',(-19.408670501884,-19.9704704268793,124.617780480819)) ;
#73760 = CARTESIAN_POINT('Ctrl Pts',(-19.6674999586664,-20.1603502121901,
124.896966576187)) ;
#73761 = CARTESIAN_POINT('Ctrl Pts',(-19.6158404984156,-19.9803611317714,
124.599938376062)) ;
#73762 = CARTESIAN_POINT('Ctrl Pts',(-19.9213144643945,-20.1703422390405,
124.829720703275)) ;
#73763 = CARTESIAN_POINT('Ctrl Pts',(-19.8188925751091,-19.9903531586217,
124.546143793371)) ;
#73764 = CARTESIAN_POINT('Ctrl Pts',(-20.1584732283506,-20.180288220529,124.719860821127)) ;
#73765 = CARTESIAN_POINT('Ctrl Pts',(-20.0086203263769,-20.0002991401102,
124.458257924358)) ;
#73766 = CARTESIAN_POINT('Ctrl Pts',(-20.3732942471525,-20.1902353931509,
124.57089728247)) ;
#73767 = CARTESIAN_POINT('Ctrl Pts',(-20.1804782620418,-20.0102463127322,
124.339088990223)) ;
#73768 = CARTESIAN_POINT('Ctrl Pts',(-20.56064383046,-20.2002833344771,124.384839709402)) ;
#73769 = CARTESIAN_POINT('Ctrl Pts',(-20.3303594683394,-20.0202942540583,
124.19024447105)) ;
#73770 = CARTESIAN_POINT('Ctrl Pts',(-20.7099931678072,-20.2101309682848,
124.173496321027)) ;
#73771 = CARTESIAN_POINT('Ctrl Pts',(-20.4498405454841,-20.0301418878661,
124.021171285439)) ;
#73772 = CARTESIAN_POINT('Ctrl Pts',(-20.8223918371463,-20.2200926829699,
123.937083946807)) ;
#73773 = CARTESIAN_POINT('Ctrl Pts',(-20.5397614600564,-20.0401036025511,
123.832042436741)) ;
#73774 = CARTESIAN_POINT('Ctrl Pts',(-20.8921871413326,-20.2301213158484,
123.682935524395)) ;
#73775 = CARTESIAN_POINT('Ctrl Pts',(-20.5955998340411,-20.0501322354297,
123.628724320913)) ;
#73776 = CARTESIAN_POINT('Ctrl Pts',(-20.916586665412,-20.2400316413835,123.423658765385)) ;
#73777 = CARTESIAN_POINT('Ctrl Pts',(-20.6151216495105,-20.0600425609648,
123.421303286286)) ;
#73778 = CARTESIAN_POINT('Ctrl Pts',(-20.8962205047592,-20.2499664718553,
123.163371888253)) ;
#73779 = CARTESIAN_POINT('Ctrl Pts',(-20.5988309868347,-20.0699773914365,
123.213073725564)) ;
#73780 = CARTESIAN_POINT('Ctrl Pts',(-20.8300540057816,-20.2600078042372,
122.907927043683)) ;
#73781 = CARTESIAN_POINT('Ctrl Pts',(-20.545899908751,-20.0800187238185,123.008717280529)) ;
#73782 = CARTESIAN_POINT('Ctrl Pts',(-20.72224421422,-20.2699006776761,122.671362855086)) ;
#73783 = CARTESIAN_POINT('Ctrl Pts',(-20.4596543888742,-20.0899115972573,
122.819465277106)) ;
#73784 = CARTESIAN_POINT('Ctrl Pts',(-20.5744033926093,-20.279869843494,122.455071839391)) ;
#73785 = CARTESIAN_POINT('Ctrl Pts',(-20.3413828139098,-20.0998807630752,
122.646430631496)) ;
#73786 = CARTESIAN_POINT('Ctrl Pts',(-20.3898674157818,-20.2898985772105,
122.266945763592)) ;
#73787 = CARTESIAN_POINT('Ctrl Pts',(-20.1937587117748,-20.1099094967917,
122.495930505573)) ;
#73788 = CARTESIAN_POINT('Ctrl Pts',(-20.1081899355574,-20.3030910959816,
122.064717611269)) ;
#73789 = CARTESIAN_POINT('Ctrl Pts',(-19.9684034754264,-20.1231020155629,
122.334134312511)) ;
#73790 = CARTESIAN_POINT('Ctrl Pts',(-19.7762004294478,-20.3164509640243,
121.939098029962)) ;
#73791 = CARTESIAN_POINT('Ctrl Pts',(-19.70278986189,-20.1364618836056,122.233638111856)) ;
#73792 = CARTESIAN_POINT('Ctrl Pts',(-19.4302944299189,-20.3296763011732,
121.904585070765)) ;
#73793 = CARTESIAN_POINT('Ctrl Pts',(-19.4261079855339,-20.1496872207544,
122.206033326473)) ;
#73794 = CARTESIAN_POINT('Ctrl Pts',(-19.16869005573,-20.3396575270138,121.923502397356)) ;
#73795 = CARTESIAN_POINT('Ctrl Pts',(-19.2168157977084,-20.1596684465951,
122.221163228254)) ;
#73796 = CARTESIAN_POINT('Ctrl Pts',(-18.9130849261676,-20.3496930939967,
121.988403504239)) ;
#73797 = CARTESIAN_POINT('Ctrl Pts',(-19.0123335164269,-20.1697040135779,
122.273082369404)) ;
#73798 = CARTESIAN_POINT('Ctrl Pts',(-18.676515944024,-20.3595561719588,122.094373600207)) ;
#73799 = CARTESIAN_POINT('Ctrl Pts',(-18.8230767411481,-20.17956709154,122.357856308508)) ;
#73800 = CARTESIAN_POINT('Ctrl Pts',(-18.4574468061026,-20.3696264707599,
122.242786566427)) ;
#73801 = CARTESIAN_POINT('Ctrl Pts',(-18.6478204417451,-20.1896373903411,
122.476584793139)) ;
#73802 = CARTESIAN_POINT('Ctrl Pts',(-18.2717579004932,-20.3794687693277,
122.422851075658)) ;
#73803 = CARTESIAN_POINT('Ctrl Pts',(-18.4992676185254,-20.1994796889089,
122.620634878705)) ;
#73804 = CARTESIAN_POINT('Ctrl Pts',(-18.117558664648,-20.3894294674975,122.634360678024)) ;
#73805 = CARTESIAN_POINT('Ctrl Pts',(-18.3759064506187,-20.2094403870787,
122.78984130679)) ;
#73806 = CARTESIAN_POINT('Ctrl Pts',(-18.0020059071283,-20.3994675016769,
122.871483585748)) ;
#73807 = CARTESIAN_POINT('Ctrl Pts',(-18.2834623026179,-20.2194784212582,
122.97953855026)) ;
#73808 = CARTESIAN_POINT('Ctrl Pts',(-17.9300887192863,-20.4093412385234,
123.120824683892)) ;
#73809 = CARTESIAN_POINT('Ctrl Pts',(-18.2259264014613,-20.2293521581047,
123.179011012652)) ;
#73810 = CARTESIAN_POINT('Ctrl Pts',(-17.9020448473122,-20.4194130224487,
123.383973224124)) ;
#73811 = CARTESIAN_POINT('Ctrl Pts',(-18.2034891482727,-20.2394239420299,
123.389529423009)) ;
#73812 = CARTESIAN_POINT('Ctrl Pts',(-17.9195350318856,-20.4292451436499,
123.641783391203)) ;
#73813 = CARTESIAN_POINT('Ctrl Pts',(-18.2174791482912,-20.2492560632311,
123.595778035105)) ;
#73814 = CARTESIAN_POINT('Ctrl Pts',(-17.9820931575839,-20.4392781676753,
123.897898640815)) ;
#73815 = CARTESIAN_POINT('Ctrl Pts',(-18.2675235858112,-20.2592890872566,
123.8006706467)) ;
#73816 = CARTESIAN_POINT('Ctrl Pts',(-18.0886185613689,-20.449294047872,124.138604141892)) ;
#73817 = CARTESIAN_POINT('Ctrl Pts',(-18.3527418295689,-20.2693049674532,
123.993235758513)) ;
#73818 = CARTESIAN_POINT('Ctrl Pts',(-18.2329706507944,-20.4591775669661,
124.354523331937)) ;
#73819 = CARTESIAN_POINT('Ctrl Pts',(-18.4682220840992,-20.2791884865474,
124.165972815499)) ;
#73820 = CARTESIAN_POINT('Ctrl Pts',(-18.4143074090764,-20.4691679793298,
124.54434899159)) ;
#73821 = CARTESIAN_POINT('Ctrl Pts',(-18.6132892508366,-20.2891788989111,
124.31783370646)) ;
#73822 = CARTESIAN_POINT('Ctrl Pts',(-18.6951170309622,-20.4824311425333,
124.750853866848)) ;
#73823 = CARTESIAN_POINT('Ctrl Pts',(-18.8379390825619,-20.3024420621145,
124.483045334698)) ;
#73824 = CARTESIAN_POINT('Ctrl Pts',(-19.0235816254363,-20.4957087127844,
124.879780338538)) ;
#73825 = CARTESIAN_POINT('Ctrl Pts',(-19.1007466138958,-20.3157196323657,
124.586193622694)) ;
#73826 = CARTESIAN_POINT('Ctrl Pts',(-19.3717460245755,-20.5090390152911,
124.918788838363)) ;
#73827 = CARTESIAN_POINT('Ctrl Pts',(-19.3792305302181,-20.3290499348723,
124.617392368579)) ;
#73828 = CARTESIAN_POINT('Ctrl Pts',(-19.6313783521578,-20.5189376971075,
124.902811153658)) ;
#73829 = CARTESIAN_POINT('Ctrl Pts',(-19.586946416879,-20.3389486166887,124.604614298726)) ;
#73830 = CARTESIAN_POINT('Ctrl Pts',(-19.8866819313856,-20.528927212155,124.841743662591)) ;
#73831 = CARTESIAN_POINT('Ctrl Pts',(-19.7911870921237,-20.3489381317363,
124.555761778186)) ;
#73832 = CARTESIAN_POINT('Ctrl Pts',(-20.126518376041,-20.53887526393,124.73768939616)) ;
#73833 = CARTESIAN_POINT('Ctrl Pts',(-19.9830583085483,-20.3588861835113,
124.472519572636)) ;
#73834 = CARTESIAN_POINT('Ctrl Pts',(-20.3446556457817,-20.5488166672085,
124.593959706051)) ;
#73835 = CARTESIAN_POINT('Ctrl Pts',(-20.1575676024382,-20.3688275867898,
124.357539619825)) ;
#73836 = CARTESIAN_POINT('Ctrl Pts',(-20.5987445476816,-20.5621033319895,
124.35442785802)) ;
#73837 = CARTESIAN_POINT('Ctrl Pts',(-20.3608485152388,-20.3821142515707,
124.165903776339)) ;
#73838 = CARTESIAN_POINT('Ctrl Pts',(-20.8307521720985,-20.5787137536443,
123.978870507215)) ;
#73839 = CARTESIAN_POINT('Ctrl Pts',(-20.5464484061325,-20.3987246732255,
123.865472812429)) ;
#73840 = CARTESIAN_POINT('Ctrl Pts',(-20.9389514261438,-20.5986250158951,
123.46082131634)) ;
#73841 = CARTESIAN_POINT('Ctrl Pts',(-20.6330141894971,-20.4186359354763,
123.451029346131)) ;
#73842 = CARTESIAN_POINT('Ctrl Pts',(-20.8639502682869,-20.6185691450599,
122.936042849581)) ;
#73843 = CARTESIAN_POINT('Ctrl Pts',(-20.5730157436839,-20.4385800646412,
123.031206971255)) ;
#73844 = CARTESIAN_POINT('Ctrl Pts',(-20.6146112119338,-20.6384923076651,
122.46895137449)) ;
#73845 = CARTESIAN_POINT('Ctrl Pts',(-20.373547351219,-20.4585032272464,122.657531515704)) ;
#73846 = CARTESIAN_POINT('Ctrl Pts',(-20.2219924331612,-20.6583824300717,
122.114827126847)) ;
#73847 = CARTESIAN_POINT('Ctrl Pts',(-20.0594536357031,-20.4783933496529,
122.374229525961)) ;
#73848 = CARTESIAN_POINT('Ctrl Pts',(-19.7292685932823,-20.6783873836718,
121.915230361475)) ;
#73849 = CARTESIAN_POINT('Ctrl Pts',(-19.6652757291056,-20.498398303253,122.2145494258)) ;
#73850 = CARTESIAN_POINT('Ctrl Pts',(-19.2022698837566,-20.6982256406874,
121.895490958109)) ;
#73851 = CARTESIAN_POINT('Ctrl Pts',(-19.2436755852947,-20.5182365602686,
122.198755216504)) ;
#73852 = CARTESIAN_POINT('Ctrl Pts',(-18.696210882358,-20.7182199414739,122.057473862863)) ;
#73853 = CARTESIAN_POINT('Ctrl Pts',(-18.8388276085648,-20.5382308610552,
122.328339327978)) ;
#73854 = CARTESIAN_POINT('Ctrl Pts',(-18.2783285951909,-20.7381051835183,
122.38107556081)) ;
#73855 = CARTESIAN_POINT('Ctrl Pts',(-18.5045195347661,-20.5581161030996,
122.587219431288)) ;
#73856 = CARTESIAN_POINT('Ctrl Pts',(-17.9948546692312,-20.7579801299943,
122.826813664097)) ;
#73857 = CARTESIAN_POINT('Ctrl Pts',(-18.2777383070033,-20.5779910495756,
122.943810054151)) ;
#73858 = CARTESIAN_POINT('Ctrl Pts',(-17.8799919147253,-20.7780131999354,
123.346775629794)) ;
#73859 = CARTESIAN_POINT('Ctrl Pts',(-18.1858465680844,-20.5980241195166,
123.359778876185)) ;
#73860 = CARTESIAN_POINT('Ctrl Pts',(-17.9496011377498,-20.7979017068358,
123.870729922715)) ;
#73861 = CARTESIAN_POINT('Ctrl Pts',(-18.2415323136978,-20.617912626417,123.778943688252)) ;
#73862 = CARTESIAN_POINT('Ctrl Pts',(-18.1918462218339,-20.8177565666171,
124.339642131858)) ;
#73863 = CARTESIAN_POINT('Ctrl Pts',(-18.4353283966454,-20.6377674861983,
124.15407531908)) ;
#73864 = CARTESIAN_POINT('Ctrl Pts',(-18.5838321067755,-20.8378074004048,
124.700496054213)) ;
#73865 = CARTESIAN_POINT('Ctrl Pts',(-18.7489159490425,-20.657818319986,124.442758816039)) ;
#73866 = CARTESIAN_POINT('Ctrl Pts',(-19.0684642768098,-20.857573342294,124.903648311974)) ;
#73867 = CARTESIAN_POINT('Ctrl Pts',(-19.1366240867067,-20.6775842618753,
124.605282256728)) ;
#73868 = CARTESIAN_POINT('Ctrl Pts',(-19.5995315082767,-20.8775860737534,
124.930591112263)) ;
#73869 = CARTESIAN_POINT('Ctrl Pts',(-19.5614778234741,-20.6975969933346,
124.626836366824)) ;
#73870 = CARTESIAN_POINT('Ctrl Pts',(-20.1049415619747,-20.8974789086969,
124.774856355386)) ;
#73871 = CARTESIAN_POINT('Ctrl Pts',(-19.9658071300402,-20.7174898282782,
124.502248164714)) ;
#73872 = CARTESIAN_POINT('Ctrl Pts',(-20.5274834956849,-20.9173859320365,
124.456638371379)) ;
#73873 = CARTESIAN_POINT('Ctrl Pts',(-20.3038412440261,-20.7373968516177,
124.247672563111)) ;
#73874 = CARTESIAN_POINT('Ctrl Pts',(-20.8168305785184,-20.9373011969372,
124.013259477113)) ;
#73875 = CARTESIAN_POINT('Ctrl Pts',(-20.5353184953281,-20.7573121165184,
123.892968103574)) ;
#73876 = CARTESIAN_POINT('Ctrl Pts',(-20.9375148305264,-20.9573328890969,
123.494752291653)) ;
#73877 = CARTESIAN_POINT('Ctrl Pts',(-20.6318648818766,-20.7773438086781,
123.47816249865)) ;
#73878 = CARTESIAN_POINT('Ctrl Pts',(-20.8746353857485,-20.9771759356699,
122.971063764424)) ;
#73879 = CARTESIAN_POINT('Ctrl Pts',(-20.5815599743237,-20.7971868552511,
123.059210077434)) ;
#73880 = CARTESIAN_POINT('Ctrl Pts',(-20.6370889547926,-20.9970924835697,
122.498095047668)) ;
#73881 = CARTESIAN_POINT('Ctrl Pts',(-20.3915208071778,-20.8171034031509,
122.680835172587)) ;
#73882 = CARTESIAN_POINT('Ctrl Pts',(-20.2519449229786,-21.017024726561,122.134274226636)) ;
#73883 = CARTESIAN_POINT('Ctrl Pts',(-20.0834038045587,-20.8370356461422,
122.389779490593)) ;
#73884 = CARTESIAN_POINT('Ctrl Pts',(-19.7666424548866,-21.0369285613703,
121.923791010099)) ;
#73885 = CARTESIAN_POINT('Ctrl Pts',(-19.6951601330397,-20.8569394809515,
122.221394579836)) ;
#73886 = CARTESIAN_POINT('Ctrl Pts',(-19.2387517746191,-21.0568289615578,
121.890890792303)) ;
#73887 = CARTESIAN_POINT('Ctrl Pts',(-19.2728466143262,-20.876839881139,122.195076908479)) ;
#73888 = CARTESIAN_POINT('Ctrl Pts',(-18.7299794806425,-21.0767786379371,
122.04027094574)) ;
#73889 = CARTESIAN_POINT('Ctrl Pts',(-18.8658292110054,-20.8967895575183,
122.314583763135)) ;
#73890 = CARTESIAN_POINT('Ctrl Pts',(-18.3031667102184,-21.0967111621575,
122.354115893624)) ;
#73891 = CARTESIAN_POINT('Ctrl Pts',(-18.5243802930808,-20.9167220817387,
122.565662292929)) ;
#73892 = CARTESIAN_POINT('Ctrl Pts',(-18.0088633208664,-21.1166311711436,
122.794268679496)) ;
#73893 = CARTESIAN_POINT('Ctrl Pts',(-18.2889398325272,-20.9366420907249,
122.917786669233)) ;
#73894 = CARTESIAN_POINT('Ctrl Pts',(-17.8822937307216,-21.1365880773198,
123.309313272759)) ;
#73895 = CARTESIAN_POINT('Ctrl Pts',(-18.1876872095001,-20.9565989969011,
123.329823376665)) ;
#73896 = CARTESIAN_POINT('Ctrl Pts',(-17.9384143245851,-21.1564739168213,
123.834958994837)) ;
#73897 = CARTESIAN_POINT('Ctrl Pts',(-18.2325869694415,-20.9764848364026,
123.750340253762)) ;
#73898 = CARTESIAN_POINT('Ctrl Pts',(-18.1714993858974,-21.1764450889572,
124.311714842716)) ;
#73899 = CARTESIAN_POINT('Ctrl Pts',(-18.4190587792687,-20.9964560085384,
124.131743525052)) ;
#73900 = CARTESIAN_POINT('Ctrl Pts',(-18.5499193846683,-21.1962592859416,
124.678080172015)) ;
#73901 = CARTESIAN_POINT('Ctrl Pts',(-18.7217959353721,-21.0162702055228,
124.424833857205)) ;
#73902 = CARTESIAN_POINT('Ctrl Pts',(-19.0342352621691,-21.2162404719098,
124.895714964022)) ;
#73903 = CARTESIAN_POINT('Ctrl Pts',(-19.1092580929924,-21.0362513914911,
124.598937764021)) ;
#73904 = CARTESIAN_POINT('Ctrl Pts',(-19.4736619237812,-21.2328159772991,
124.928069751283)) ;
#73905 = CARTESIAN_POINT('Ctrl Pts',(-19.4607756982869,-21.0528268968803,
124.624819424069)) ;
#73906 = CARTESIAN_POINT('Ctrl Pts',(-19.8173383619341,-21.2461254251627,
124.863112509731)) ;
#73907 = CARTESIAN_POINT('Ctrl Pts',(-19.7357439277155,-21.0661363447439,
124.572846691441)) ;
#73908 = CARTESIAN_POINT('Ctrl Pts',(-20.1458733463393,-21.2594931229393,
124.73871434374)) ;
#73909 = CARTESIAN_POINT('Ctrl Pts',(-19.998523136109,-21.0795040425205,124.473349266923)) ;
#73910 = CARTESIAN_POINT('Ctrl Pts',(-20.5018728442844,-21.2759836946052,
124.483060829729)) ;
#73911 = CARTESIAN_POINT('Ctrl Pts',(-20.2833722640373,-21.0959946141864,
124.268798320229)) ;
#73912 = CARTESIAN_POINT('Ctrl Pts',(-20.801833760268,-21.295903966938,124.046874735379)) ;
#73913 = CARTESIAN_POINT('Ctrl Pts',(-20.5233223409627,-21.1159148865192,
123.919846740881)) ;
#73914 = CARTESIAN_POINT('Ctrl Pts',(-20.9126872838241,-21.312521002659,123.619326861725)) ;
#73915 = CARTESIAN_POINT('Ctrl Pts',(-20.6120012338397,-21.1325319222402,
123.57783290666)) ;
#73916 = CARTESIAN_POINT('Ctrl Pts',(-20.9100801365058,-21.3258118529401,
123.270041130559)) ;
#73917 = CARTESIAN_POINT('Ctrl Pts',(-20.6099160373388,-21.1458227725213,
123.298380131864)) ;
#73918 = CARTESIAN_POINT('Ctrl Pts',(-20.8627908877949,-21.3357808980945,
123.012396956915)) ;
#73919 = CARTESIAN_POINT('Ctrl Pts',(-20.572081952972,-21.1557918176758,123.092270099761)) ;
#73920 = CARTESIAN_POINT('Ctrl Pts',(-20.7725483588054,-21.3456842887281,
122.768260657571)) ;
#73921 = CARTESIAN_POINT('Ctrl Pts',(-20.499885452573,-21.1656952083094,122.896960032138)) ;
#73922 = CARTESIAN_POINT('Ctrl Pts',(-20.639146259406,-21.3557420748408,122.540122041368)) ;
#73923 = CARTESIAN_POINT('Ctrl Pts',(-20.3931639432043,-21.1757529944221,
122.714452096665)) ;
#73924 = CARTESIAN_POINT('Ctrl Pts',(-20.4717962813349,-21.3655941114906,
122.342544854359)) ;
#73925 = CARTESIAN_POINT('Ctrl Pts',(-20.2592745302504,-21.1856050310718,
122.556386398767)) ;
#73926 = CARTESIAN_POINT('Ctrl Pts',(-20.2020865685042,-21.3789592356338,
122.117585029571)) ;
#73927 = CARTESIAN_POINT('Ctrl Pts',(-20.0435429434541,-21.198970155215,122.376446523523)) ;
#73928 = CARTESIAN_POINT('Ctrl Pts',(-19.8829746643163,-21.3921852985968,
121.970083355977)) ;
#73929 = CARTESIAN_POINT('Ctrl Pts',(-19.7882331633885,-21.2121962181781,
122.25842782825)) ;
#73930 = CARTESIAN_POINT('Ctrl Pts',(-19.5386166648349,-21.4054889468791,
121.909867161764)) ;
#73931 = CARTESIAN_POINT('Ctrl Pts',(-19.5127307955836,-21.2254998664603,
122.210256068313)) ;
#73932 = CARTESIAN_POINT('Ctrl Pts',(-19.2760167649112,-21.4154804780421,
121.910107183549)) ;
#73933 = CARTESIAN_POINT('Ctrl Pts',(-19.302654042271,-21.2354913976233,122.210450691306)) ;
#73934 = CARTESIAN_POINT('Ctrl Pts',(-19.0163207496218,-21.4255199258414,
121.956500605388)) ;
#73935 = CARTESIAN_POINT('Ctrl Pts',(-19.0948968590476,-21.2455308454226,
122.247567530299)) ;
#73936 = CARTESIAN_POINT('Ctrl Pts',(-18.7732843138924,-21.4353637013552,
122.045159677544)) ;
#73937 = CARTESIAN_POINT('Ctrl Pts',(-18.9004686755779,-21.2553746209365,
122.318496939825)) ;
#73938 = CARTESIAN_POINT('Ctrl Pts',(-18.5458944196666,-21.4453493427429,
122.176053036264)) ;
#73939 = CARTESIAN_POINT('Ctrl Pts',(-18.7185578856858,-21.2653602623241,
122.42321354917)) ;
#73940 = CARTESIAN_POINT('Ctrl Pts',(-18.3455158402241,-21.4552861271047,
122.343559635679)) ;
#73941 = CARTESIAN_POINT('Ctrl Pts',(-18.5582565294496,-21.2752970466859,
122.557220524187)) ;
#73942 = CARTESIAN_POINT('Ctrl Pts',(-18.1755004123223,-21.465335961572,122.545621877057)) ;
#73943 = CARTESIAN_POINT('Ctrl Pts',(-18.4222459430947,-21.2853468811533,
122.718871736199)) ;
#73944 = CARTESIAN_POINT('Ctrl Pts',(-18.0455857951016,-21.4751864110752,
122.769542152849)) ;
#73945 = CARTESIAN_POINT('Ctrl Pts',(-18.3183162510833,-21.2951973306564,
122.898009008209)) ;
#73946 = CARTESIAN_POINT('Ctrl Pts',(-17.9548017336223,-21.4851584250573,
123.015333175411)) ;
#73947 = CARTESIAN_POINT('Ctrl Pts',(-18.2456911442363,-21.3051693446385,
123.094642518288)) ;
#73948 = CARTESIAN_POINT('Ctrl Pts',(-17.9079865988999,-21.4951535829044,
123.273832595295)) ;
#73949 = CARTESIAN_POINT('Ctrl Pts',(-18.2082412561885,-21.3151645024856,
123.3014423916)) ;
#73950 = CARTESIAN_POINT('Ctrl Pts',(-17.9070803717474,-21.5051875092681,
123.537489745396)) ;
#73951 = CARTESIAN_POINT('Ctrl Pts',(-18.2075185318219,-21.3251984288494,
123.512368089065)) ;
#73952 = CARTESIAN_POINT('Ctrl Pts',(-17.9507793757721,-21.5150432177005,
123.792798278257)) ;
#73953 = CARTESIAN_POINT('Ctrl Pts',(-18.2424799133806,-21.3350541372817,
123.716614351345)) ;
#73954 = CARTESIAN_POINT('Ctrl Pts',(-18.0390300007286,-21.5250413670391,
124.040230621181)) ;
#73955 = CARTESIAN_POINT('Ctrl Pts',(-18.3130824917955,-21.3450522866204,
123.914559406275)) ;
#73956 = CARTESIAN_POINT('Ctrl Pts',(-18.1674560177498,-21.5349407702127,
124.266510551669)) ;
#73957 = CARTESIAN_POINT('Ctrl Pts',(-18.4158251303191,-21.354951689794,124.095582078707)) ;
#73958 = CARTESIAN_POINT('Ctrl Pts',(-18.3356760699682,-21.5449919671012,
124.470114255053)) ;
#73959 = CARTESIAN_POINT('Ctrl Pts',(-18.5504028849582,-21.3650028866824,
124.258463636638)) ;
#73960 = CARTESIAN_POINT('Ctrl Pts',(-18.5333267196621,-21.554874290914,124.638598756926)) ;
#73961 = CARTESIAN_POINT('Ctrl Pts',(-18.7085246479764,-21.3748852104953,
124.393249391773)) ;
#73962 = CARTESIAN_POINT('Ctrl Pts',(-18.759456001813,-21.5648691865706,124.772199668069)) ;
#73963 = CARTESIAN_POINT('Ctrl Pts',(-18.8894291059458,-21.3848801061519,
124.500128205226)) ;
#73964 = CARTESIAN_POINT('Ctrl Pts',(-19.0061476935315,-21.5748902859531,
124.864395292347)) ;
#73965 = CARTESIAN_POINT('Ctrl Pts',(-19.0867832058502,-21.3949012055344,
124.573882634977)) ;
#73966 = CARTESIAN_POINT('Ctrl Pts',(-19.2621059878514,-21.5847975538152,
124.912011501675)) ;
#73967 = CARTESIAN_POINT('Ctrl Pts',(-19.2915499957338,-21.4048084733965,
124.611973405595)) ;
#73968 = CARTESIAN_POINT('Ctrl Pts',(-19.5232414618361,-21.5947358976405,
124.914993347276)) ;
#73969 = CARTESIAN_POINT('Ctrl Pts',(-19.5004581837589,-21.4147468172218,
124.61435673395)) ;
#73970 = CARTESIAN_POINT('Ctrl Pts',(-19.7826877608884,-21.604739316941,124.872466522389)) ;
#73971 = CARTESIAN_POINT('Ctrl Pts',(-19.7080148132996,-21.4247502365222,
124.580333183701)) ;
#73972 = CARTESIAN_POINT('Ctrl Pts',(-20.0313953526549,-21.6147738676481,
124.784868563524)) ;
#73973 = CARTESIAN_POINT('Ctrl Pts',(-19.9069801784579,-21.4347847872293,
124.510252765367)) ;
#73974 = CARTESIAN_POINT('Ctrl Pts',(-20.2570175361581,-21.6246188172537,
124.658232944554)) ;
#73975 = CARTESIAN_POINT('Ctrl Pts',(-20.0874764875126,-21.4446297368349,
124.408942636223)) ;
#73976 = CARTESIAN_POINT('Ctrl Pts',(-20.4603562192265,-21.6346046593666,
124.492418457944)) ;
#73977 = CARTESIAN_POINT('Ctrl Pts',(-20.2501460171759,-21.4546155789478,
124.276289513827)) ;
#73978 = CARTESIAN_POINT('Ctrl Pts',(-20.6311392302461,-21.6445394667356,
124.294885221569)) ;
#73979 = CARTESIAN_POINT('Ctrl Pts',(-20.3867706983452,-21.4645503863169,
124.118261777518)) ;
#73980 = CARTESIAN_POINT('Ctrl Pts',(-20.7664361278029,-21.6545970084489,
124.067883129718)) ;
#73981 = CARTESIAN_POINT('Ctrl Pts',(-20.4950064705292,-21.4746079280302,
123.936658954064)) ;
#73982 = CARTESIAN_POINT('Ctrl Pts',(-20.8584564949469,-21.6644186059611,
123.826712005203)) ;
#73983 = CARTESIAN_POINT('Ctrl Pts',(-20.5686206343265,-21.4844295255424,
123.743721915454)) ;
#73984 = CARTESIAN_POINT('Ctrl Pts',(-20.9088388979674,-21.6744748654416,
123.567314526494)) ;
#73985 = CARTESIAN_POINT('Ctrl Pts',(-20.6089246277522,-21.4944857850228,
123.536203466964)) ;
#73986 = CARTESIAN_POINT('Ctrl Pts',(-20.9129054422664,-21.684414801742,123.306120784311)) ;
#73987 = CARTESIAN_POINT('Ctrl Pts',(-20.61217581895,-21.5044257213232,123.327248710015)) ;
#73988 = CARTESIAN_POINT('Ctrl Pts',(-20.8724715626847,-21.6943219224864,
123.048933898894)) ;
#73989 = CARTESIAN_POINT('Ctrl Pts',(-20.5798268670816,-21.5143328420676,
123.121499921516)) ;
#73990 = CARTESIAN_POINT('Ctrl Pts',(-20.786747108785,-21.7043648284116,122.79933394968)) ;
#73991 = CARTESIAN_POINT('Ctrl Pts',(-20.5112454371669,-21.5243757479929,
122.921820528242)) ;
#73992 = CARTESIAN_POINT('Ctrl Pts',(-20.6607421011446,-21.7142726095109,
122.571477249556)) ;
#73993 = CARTESIAN_POINT('Ctrl Pts',(-20.4104399317555,-21.5342835290921,
122.739536474708)) ;
#73994 = CARTESIAN_POINT('Ctrl Pts',(-20.495754325636,-21.7242829785133,122.366574426268)) ;
#73995 = CARTESIAN_POINT('Ctrl Pts',(-20.2784482779818,-21.5442938980945,
122.575615429182)) ;
#73996 = CARTESIAN_POINT('Ctrl Pts',(-20.2969450012805,-21.7343138170821,
122.193488770764)) ;
#73997 = CARTESIAN_POINT('Ctrl Pts',(-20.1193995041773,-21.5543247366633,
122.437148355907)) ;
#73998 = CARTESIAN_POINT('Ctrl Pts',(-20.0753430040867,-21.7441666567218,
122.05956218883)) ;
#73999 = CARTESIAN_POINT('Ctrl Pts',(-19.9421175002561,-21.564177576303,122.330009052223)) ;
#74000 = CARTESIAN_POINT('Ctrl Pts',(-19.8307389892277,-21.7541546578867,
121.964427436331)) ;
#74001 = CARTESIAN_POINT('Ctrl Pts',(-19.7464337668386,-21.574165577468,122.253902995604)) ;
#74002 = CARTESIAN_POINT('Ctrl Pts',(-19.5748309877836,-21.7640834768659,
121.913501885796)) ;
#74003 = CARTESIAN_POINT('Ctrl Pts',(-19.5417073934896,-21.5840943964472,
122.213164409837)) ;
#74004 = CARTESIAN_POINT('Ctrl Pts',(-19.3124241042383,-21.7740711795882,
121.907308023962)) ;
#74005 = CARTESIAN_POINT('Ctrl Pts',(-19.3317819920219,-21.5940820991695,
122.208211065179)) ;
#74006 = CARTESIAN_POINT('Ctrl Pts',(-19.0517647367199,-21.7841071793909,
121.947395957951)) ;
#74007 = CARTESIAN_POINT('Ctrl Pts',(-19.1232547049505,-21.6041180989721,
122.240283218186)) ;
#74008 = CARTESIAN_POINT('Ctrl Pts',(-18.8063639186808,-21.7939620491923,
122.030208537062)) ;
#74009 = CARTESIAN_POINT('Ctrl Pts',(-18.9269353053611,-21.6139729687736,
122.306534697317)) ;
#74010 = CARTESIAN_POINT('Ctrl Pts',(-18.575622053571,-21.8039614796158,122.155848712775)) ;
#74011 = CARTESIAN_POINT('Ctrl Pts',(-18.7423427130502,-21.6239723991971,
122.407048265854)) ;
#74012 = CARTESIAN_POINT('Ctrl Pts',(-18.3721015981849,-21.8138565970811,
122.317772569595)) ;
#74013 = CARTESIAN_POINT('Ctrl Pts',(-18.5795278239004,-21.6338675166624,
122.536588260672)) ;
#74014 = CARTESIAN_POINT('Ctrl Pts',(-18.1969788650004,-21.8239170905981,
122.515789157029)) ;
#74015 = CARTESIAN_POINT('Ctrl Pts',(-18.4394307367387,-21.6439280101794,
122.695002760507)) ;
#74016 = CARTESIAN_POINT('Ctrl Pts',(-18.0616465448308,-21.8337665707993,
122.736447563601)) ;
#74017 = CARTESIAN_POINT('Ctrl Pts',(-18.3311666894869,-21.6537774903805,
122.871529616356)) ;
#74018 = CARTESIAN_POINT('Ctrl Pts',(-17.9643529996744,-21.8437930210631,
122.981307539536)) ;
#74019 = CARTESIAN_POINT('Ctrl Pts',(-18.2533332210301,-21.6638039406443,
123.067418172796)) ;
#74020 = CARTESIAN_POINT('Ctrl Pts',(-17.91173712929,-21.8538243115412,123.239620782811)) ;
#74021 = CARTESIAN_POINT('Ctrl Pts',(-18.2112421016013,-21.6738352311224,
123.274069149451)) ;
#74022 = CARTESIAN_POINT('Ctrl Pts',(-17.904341497502,-21.863665699193,123.498138969841)) ;
#74023 = CARTESIAN_POINT('Ctrl Pts',(-18.2053271327317,-21.6836766187742,
123.480882829659)) ;
#74024 = CARTESIAN_POINT('Ctrl Pts',(-17.9420552179328,-21.8736691000842,
123.758271923729)) ;
#74025 = CARTESIAN_POINT('Ctrl Pts',(-18.2354994952421,-21.6936800196655,
123.688988903637)) ;
#74026 = CARTESIAN_POINT('Ctrl Pts',(-18.0243333211888,-21.8836534828754,
124.007465107882)) ;
#74027 = CARTESIAN_POINT('Ctrl Pts',(-18.3013232846925,-21.7036644024566,
123.888342843706)) ;
#74028 = CARTESIAN_POINT('Ctrl Pts',(-18.1494974494825,-21.8936925728888,
124.239670692919)) ;
#74029 = CARTESIAN_POINT('Ctrl Pts',(-18.4014559474029,-21.71370349247,124.074106700481)) ;
#74030 = CARTESIAN_POINT('Ctrl Pts',(-18.30967337421,-21.9035383817979,124.442892027239)) ;
#74031 = CARTESIAN_POINT('Ctrl Pts',(-18.5295972153698,-21.7235493013792,
124.236682156643)) ;
#74032 = CARTESIAN_POINT('Ctrl Pts',(-18.5050211084765,-21.9135228046169,
124.618000034217)) ;
#74033 = CARTESIAN_POINT('Ctrl Pts',(-18.6858761220133,-21.7335337241982,
124.376767460048)) ;
#74034 = CARTESIAN_POINT('Ctrl Pts',(-18.7268105926393,-21.9234624298581,
124.756042327735)) ;
#74035 = CARTESIAN_POINT('Ctrl Pts',(-18.8633080134688,-21.7434733494394,
124.487199981582)) ;
#74036 = CARTESIAN_POINT('Ctrl Pts',(-18.97160932172,-21.9335021193768,124.854379340685)) ;
#74037 = CARTESIAN_POINT('Ctrl Pts',(-19.0591475870826,-21.7535130389581,
124.565868438061)) ;
#74038 = CARTESIAN_POINT('Ctrl Pts',(-19.2258769015524,-21.9433903077954,
124.908032136416)) ;
#74039 = CARTESIAN_POINT('Ctrl Pts',(-19.2625611888641,-21.7634012273766,
124.608789286634)) ;
#74040 = CARTESIAN_POINT('Ctrl Pts',(-19.4882188467812,-21.9533798337974,
124.917301153526)) ;
#74041 = CARTESIAN_POINT('Ctrl Pts',(-19.4724346146083,-21.7733907533787,
124.616203339472)) ;
#74042 = CARTESIAN_POINT('Ctrl Pts',(-19.7473517520532,-21.9633383351526,
124.880791790101)) ;
#74043 = CARTESIAN_POINT('Ctrl Pts',(-19.679740427849,-21.7833492547339,124.586994707607)) ;
#74044 = CARTESIAN_POINT('Ctrl Pts',(-19.9949571853536,-21.9732379291563,
124.800926502681)) ;
#74045 = CARTESIAN_POINT('Ctrl Pts',(-19.8778237805908,-21.7932488487375,
124.523101689369)) ;
#74046 = CARTESIAN_POINT('Ctrl Pts',(-20.2282969935453,-21.9832858172776,
124.677397513658)) ;
#74047 = CARTESIAN_POINT('Ctrl Pts',(-20.0644952773521,-21.8032967368588,
124.424277463967)) ;
#74048 = CARTESIAN_POINT('Ctrl Pts',(-20.4336615726101,-21.9931812425231,
124.517808969279)) ;
#74049 = CARTESIAN_POINT('Ctrl Pts',(-20.2287857314875,-21.8131921621044,
124.296606263855)) ;
#74050 = CARTESIAN_POINT('Ctrl Pts',(-20.6111028162001,-22.0032426332237,
124.321832201038)) ;
#74051 = CARTESIAN_POINT('Ctrl Pts',(-20.3707381429069,-21.8232535528049,
124.139823967692)) ;
#74052 = CARTESIAN_POINT('Ctrl Pts',(-20.7488672564471,-22.0130882169104,
124.102810049115)) ;
#74053 = CARTESIAN_POINT('Ctrl Pts',(-20.4809482739668,-21.8330991364916,
123.964606606129)) ;
#74054 = CARTESIAN_POINT('Ctrl Pts',(-20.8484784323002,-22.0230511902195,
123.860702848392)) ;
#74055 = CARTESIAN_POINT('Ctrl Pts',(-20.5606363386565,-21.8430621098008,
123.770920863267)) ;
#74056 = CARTESIAN_POINT('Ctrl Pts',(-20.9045567468612,-22.0330768570453,
123.603259320316)) ;
#74057 = CARTESIAN_POINT('Ctrl Pts',(-20.6054981356393,-21.8530877766266,
123.564965788728)) ;
#74058 = CARTESIAN_POINT('Ctrl Pts',(-20.9151055479369,-22.0429913349116,
123.342939247582)) ;
#74059 = CARTESIAN_POINT('Ctrl Pts',(-20.6139362973576,-21.8630022544929,
123.356710337489)) ;
#74060 = CARTESIAN_POINT('Ctrl Pts',(-20.8805485314069,-22.0529798495866,
123.082714706922)) ;
#74061 = CARTESIAN_POINT('Ctrl Pts',(-20.586289982988,-21.8729907691679,123.148530979108)) ;
#74062 = CARTESIAN_POINT('Ctrl Pts',(-20.8003679518877,-22.0630239605021,
122.831264561831)) ;
#74063 = CARTESIAN_POINT('Ctrl Pts',(-20.5221446448977,-21.8830348800833,
122.947370978964)) ;
#74064 = CARTESIAN_POINT('Ctrl Pts',(-20.6809098953826,-22.0728520980966,
122.602235481597)) ;
#74065 = CARTESIAN_POINT('Ctrl Pts',(-20.4265781234052,-21.8928630176779,
122.76414910543)) ;
#74066 = CARTESIAN_POINT('Ctrl Pts',(-20.5196736796147,-22.0829286661556,
122.392249516392)) ;
#74067 = CARTESIAN_POINT('Ctrl Pts',(-20.2975883848863,-21.9029395857368,
122.596160459755)) ;
#74068 = CARTESIAN_POINT('Ctrl Pts',(-20.3287820284441,-22.0927808280597,
122.217258955723)) ;
#74069 = CARTESIAN_POINT('Ctrl Pts',(-20.1448754008448,-21.912791747641,122.456169202449)) ;
#74070 = CARTESIAN_POINT('Ctrl Pts',(-20.1057172726031,-22.1028537900166,
122.074824536905)) ;
#74071 = CARTESIAN_POINT('Ctrl Pts',(-19.9664229786563,-21.9228647095978,
122.342221984015)) ;
#74072 = CARTESIAN_POINT('Ctrl Pts',(-19.8668228113682,-22.1126963520195,
121.97561587134)) ;
#74073 = CARTESIAN_POINT('Ctrl Pts',(-19.7753082232677,-21.9327072716007,
122.262856048578)) ;
#74074 = CARTESIAN_POINT('Ctrl Pts',(-19.6110214816257,-22.1226767885133,
121.917755554063)) ;
#74075 = CARTESIAN_POINT('Ctrl Pts',(-19.5706673154193,-21.9426877080945,
122.216568229645)) ;
#74076 = CARTESIAN_POINT('Ctrl Pts',(-19.3480335183773,-22.1326950938377,
121.905648968593)) ;
#74077 = CARTESIAN_POINT('Ctrl Pts',(-19.3602769131939,-21.9527060134189,
122.206883477632)) ;
#74078 = CARTESIAN_POINT('Ctrl Pts',(-19.0903400797142,-22.1425790577571,
121.938406487009)) ;
#74079 = CARTESIAN_POINT('Ctrl Pts',(-19.1541230782783,-21.9625899773384,
122.233089760099)) ;
#74080 = CARTESIAN_POINT('Ctrl Pts',(-18.8377600204404,-22.1526449344956,
122.016875429342)) ;
#74081 = CARTESIAN_POINT('Ctrl Pts',(-18.9520588488056,-21.9726558540769,
122.295865388187)) ;
#74082 = CARTESIAN_POINT('Ctrl Pts',(-18.6078114381679,-22.1624840353566,
122.135152615133)) ;
#74083 = CARTESIAN_POINT('Ctrl Pts',(-18.7681011911182,-21.9824949549378,
122.390486916667)) ;
#74084 = CARTESIAN_POINT('Ctrl Pts',(-18.3974600457077,-22.1725171182223,
122.294091316756)) ;
#74085 = CARTESIAN_POINT('Ctrl Pts',(-18.5998201180981,-21.9925280378036,
122.517638081399)) ;
#74086 = CARTESIAN_POINT('Ctrl Pts',(-18.2185627412926,-22.1825388034977,
122.487389938075)) ;
#74087 = CARTESIAN_POINT('Ctrl Pts',(-18.4567025086376,-22.002549723079,122.67227724618)) ;
#74088 = CARTESIAN_POINT('Ctrl Pts',(-18.0778211453225,-22.1924054985962,
122.705132096636)) ;
#74089 = CARTESIAN_POINT('Ctrl Pts',(-18.3441099857594,-22.0124164181775,
122.846470267623)) ;
#74090 = CARTESIAN_POINT('Ctrl Pts',(-17.9754225073383,-22.2023653883308,
122.946017980741)) ;
#74091 = CARTESIAN_POINT('Ctrl Pts',(-18.2621912862455,-22.0223763079121,
123.039178659271)) ;
#74092 = CARTESIAN_POINT('Ctrl Pts',(-17.9163607641115,-22.2124003761563,
123.203010659021)) ;
#74093 = CARTESIAN_POINT('Ctrl Pts',(-18.2149420385229,-22.0324112957375,
123.244772955829)) ;
#74094 = CARTESIAN_POINT('Ctrl Pts',(-17.9025839573901,-22.2222870802306,
123.462494584698)) ;
#74095 = CARTESIAN_POINT('Ctrl Pts',(-18.2039207061201,-22.0422979998118,
123.452359223595)) ;
#74096 = CARTESIAN_POINT('Ctrl Pts',(-17.9346959979923,-22.2323522244635,
123.724996117173)) ;
#74097 = CARTESIAN_POINT('Ctrl Pts',(-18.2296104579225,-22.0523631440447,
123.662360751984)) ;
#74098 = CARTESIAN_POINT('Ctrl Pts',(-18.009937769105,-22.242191515192,123.972415043897)) ;
#74099 = CARTESIAN_POINT('Ctrl Pts',(-18.2898035447589,-22.0622024347733,
123.860294755891)) ;
#74100 = CARTESIAN_POINT('Ctrl Pts',(-18.1292969690011,-22.2522540726305,
124.208342841521)) ;
#74101 = CARTESIAN_POINT('Ctrl Pts',(-18.3852909705668,-22.0722649922117,
124.049037294054)) ;
#74102 = CARTESIAN_POINT('Ctrl Pts',(-18.285451684864,-22.2621511238826,124.416351010889)) ;
#74103 = CARTESIAN_POINT('Ctrl Pts',(-18.5102142588833,-22.0821620434638,
124.215443190149)) ;
#74104 = CARTESIAN_POINT('Ctrl Pts',(-18.4753956189542,-22.2720823306308,
124.595319409297)) ;
#74105 = CARTESIAN_POINT('Ctrl Pts',(-18.6621688310842,-22.0920932502121,
124.358617678543)) ;
#74106 = CARTESIAN_POINT('Ctrl Pts',(-18.6961275310964,-22.2821245148496,
124.739948983668)) ;
#74107 = CARTESIAN_POINT('Ctrl Pts',(-18.8387544167778,-22.1021354344309,
124.47432155666)) ;
#74108 = CARTESIAN_POINT('Ctrl Pts',(-18.9348029986471,-22.2920111429606,
124.842623278205)) ;
#74109 = CARTESIAN_POINT('Ctrl Pts',(-19.0296939129993,-22.1120220625418,
124.556460832634)) ;
#74110 = CARTESIAN_POINT('Ctrl Pts',(-19.1902815584454,-22.302004415493,124.90335805786)) ;
#74111 = CARTESIAN_POINT('Ctrl Pts',(-19.2340765313827,-22.1220153350742,
124.605048920887)) ;
#74112 = CARTESIAN_POINT('Ctrl Pts',(-19.4511817330622,-22.3119494910344,
124.918648968618)) ;
#74113 = CARTESIAN_POINT('Ctrl Pts',(-19.442796174619,-22.1319604106157,124.61728190834)) ;
#74114 = CARTESIAN_POINT('Ctrl Pts',(-19.7109595708838,-22.3218990417627,
124.888897659264)) ;
#74115 = CARTESIAN_POINT('Ctrl Pts',(-19.6506180532169,-22.141909961344,124.593481323135)) ;
#74116 = CARTESIAN_POINT('Ctrl Pts',(-19.9637921602484,-22.3319383766107,
124.813587576236)) ;
#74117 = CARTESIAN_POINT('Ctrl Pts',(-19.8528843512006,-22.1519492961919,
124.533233558072)) ;
#74118 = CARTESIAN_POINT('Ctrl Pts',(-20.1962451731138,-22.3418245155546,
124.697521392909)) ;
#74119 = CARTESIAN_POINT('Ctrl Pts',(-20.0388461770694,-22.1618354351359,
124.440381365318)) ;
#74120 = CARTESIAN_POINT('Ctrl Pts',(-20.4075357060936,-22.3518226285283,
124.541405526239)) ;
#74121 = CARTESIAN_POINT('Ctrl Pts',(-20.2078787966008,-22.1718335481096,
124.315489143515)) ;
#74122 = CARTESIAN_POINT('Ctrl Pts',(-20.5872481935433,-22.3617423908807,
124.352530361832)) ;
#74123 = CARTESIAN_POINT('Ctrl Pts',(-20.3516487449868,-22.181753310462,124.164389831893)) ;
#74124 = CARTESIAN_POINT('Ctrl Pts',(-20.7332188477084,-22.3717817864934,
124.132782767691)) ;
#74125 = CARTESIAN_POINT('Ctrl Pts',(-20.4684258066509,-22.1917927060747,
123.988591943343)) ;
#74126 = CARTESIAN_POINT('Ctrl Pts',(-20.8373803849402,-22.3816909722817,
123.894117096674)) ;
#74127 = CARTESIAN_POINT('Ctrl Pts',(-20.5517552368214,-22.2017018918629,
123.797660275818)) ;
#74128 = CARTESIAN_POINT('Ctrl Pts',(-20.8993918233242,-22.3916261564392,
123.640499494835)) ;
#74129 = CARTESIAN_POINT('Ctrl Pts',(-20.6013649575712,-22.2116370760204,
123.594766873805)) ;
#74130 = CARTESIAN_POINT('Ctrl Pts',(-20.9163470244169,-22.4016672138251,
123.377183112357)) ;
#74131 = CARTESIAN_POINT('Ctrl Pts',(-20.6149297759424,-22.2216781334063,
123.38411366101)) ;
#74132 = CARTESIAN_POINT('Ctrl Pts',(-20.8879521472954,-22.4115543718584,
123.118900643928)) ;
#74133 = CARTESIAN_POINT('Ctrl Pts',(-20.5922146560384,-22.2315652914396,
123.177488436444)) ;
#74134 = CARTESIAN_POINT('Ctrl Pts',(-20.8147966667285,-22.4215466515343,
122.866729097608)) ;
#74135 = CARTESIAN_POINT('Ctrl Pts',(-20.5336910860111,-22.2415575711155,
122.97575113261)) ;
#74136 = CARTESIAN_POINT('Ctrl Pts',(-20.6993946933996,-22.4314951685793,
122.63212443824)) ;
#74137 = CARTESIAN_POINT('Ctrl Pts',(-20.4413704002996,-22.2515060881606,
122.788067448919)) ;
#74138 = CARTESIAN_POINT('Ctrl Pts',(-20.5455120187873,-22.4414319461497,
122.421182047668)) ;
#74139 = CARTESIAN_POINT('Ctrl Pts',(-20.3182652644741,-22.261442865731,122.619313435312)) ;
#74140 = CARTESIAN_POINT('Ctrl Pts',(-20.3566546113956,-22.4514149822967,
122.239043334133)) ;
#74141 = CARTESIAN_POINT('Ctrl Pts',(-20.1671801441174,-22.2714259018779,
122.473601924756)) ;
#74142 = CARTESIAN_POINT('Ctrl Pts',(-20.1374997937771,-22.4614587338904,
122.092007982377)) ;
#74143 = CARTESIAN_POINT('Ctrl Pts',(-19.9918566291476,-22.2814696534717,
122.355972866551)) ;
#74144 = CARTESIAN_POINT('Ctrl Pts',(-19.9014984820175,-22.471287263103,121.986966332281)) ;
#74145 = CARTESIAN_POINT('Ctrl Pts',(-19.803057030311,-22.2912981826842,122.27193912262)) ;
#74146 = CARTESIAN_POINT('Ctrl Pts',(-19.6446726698096,-22.4813626240117,
121.922812414337)) ;
#74147 = CARTESIAN_POINT('Ctrl Pts',(-19.5975962939444,-22.3013735435929,
122.220614925738)) ;
#74148 = CARTESIAN_POINT('Ctrl Pts',(-19.3862413607604,-22.4912192228988,
121.904531259499)) ;
#74149 = CARTESIAN_POINT('Ctrl Pts',(-19.3908522878681,-22.3112301424801,
122.205989042091)) ;
#74150 = CARTESIAN_POINT('Ctrl Pts',(-19.1232446772994,-22.5012822169167,
121.931678446554)) ;
#74151 = CARTESIAN_POINT('Ctrl Pts',(-19.1804545703553,-22.321293136498,122.227705729695)) ;
#74152 = CARTESIAN_POINT('Ctrl Pts',(-18.8735448281445,-22.5111601512062,
122.002791143802)) ;
#74153 = CARTESIAN_POINT('Ctrl Pts',(-18.9806951761436,-22.3311710707875,
122.284594621574)) ;
#74154 = CARTESIAN_POINT('Ctrl Pts',(-18.6369922199402,-22.5211607987643,
122.117182285991)) ;
#74155 = CARTESIAN_POINT('Ctrl Pts',(-18.7914526693458,-22.3411717183456,
122.376106428338)) ;
#74156 = CARTESIAN_POINT('Ctrl Pts',(-18.4254683343304,-22.5310786452023,
122.269531684406)) ;
#74157 = CARTESIAN_POINT('Ctrl Pts',(-18.6222333099972,-22.3510895647836,
122.497984627214)) ;
#74158 = CARTESIAN_POINT('Ctrl Pts',(-18.2412825268734,-22.541129762208,122.458791235511)) ;
#74159 = CARTESIAN_POINT('Ctrl Pts',(-18.4748836852717,-22.3611406817893,
122.649391549011)) ;
#74160 = CARTESIAN_POINT('Ctrl Pts',(-18.0951286475946,-22.5510004975186,
122.673148447067)) ;
#74161 = CARTESIAN_POINT('Ctrl Pts',(-18.3579599995673,-22.3710114170999,
122.820875923692)) ;
#74162 = CARTESIAN_POINT('Ctrl Pts',(-17.9862416101576,-22.5610712047616,
122.914310640387)) ;
#74163 = CARTESIAN_POINT('Ctrl Pts',(-18.270849088114,-22.3810821243429,123.013805409563)) ;
#74164 = CARTESIAN_POINT('Ctrl Pts',(-17.9222939723837,-22.5709042122135,
123.164699747297)) ;
#74165 = CARTESIAN_POINT('Ctrl Pts',(-18.2196899694515,-22.3909151317947,
123.214115380671)) ;
#74166 = CARTESIAN_POINT('Ctrl Pts',(-17.9016542678297,-22.5809347045157,
123.427471548307)) ;
#74167 = CARTESIAN_POINT('Ctrl Pts',(-18.2031767454531,-22.400945624097,123.424332776703)) ;
#74168 = CARTESIAN_POINT('Ctrl Pts',(-17.9277238840771,-22.5909662995892,
123.689813957219)) ;
#74169 = CARTESIAN_POINT('Ctrl Pts',(-18.2240311522087,-22.4109772191704,
123.634206897862)) ;
#74170 = CARTESIAN_POINT('Ctrl Pts',(-17.996987812227,-22.6007959987274,123.938651312462)) ;
#74171 = CARTESIAN_POINT('Ctrl Pts',(-18.2794406618939,-22.4208069183087,
123.833276183553)) ;
#74172 = CARTESIAN_POINT('Ctrl Pts',(-18.1095198728437,-22.610785448609,124.175829192036)) ;
#74173 = CARTESIAN_POINT('Ctrl Pts',(-18.3694648327991,-22.4307963681902,
124.023019031505)) ;
#74174 = CARTESIAN_POINT('Ctrl Pts',(-18.2628916856932,-22.6208293064246,
124.390633246443)) ;
#74175 = CARTESIAN_POINT('Ctrl Pts',(-18.4921611832323,-22.4408402260059,
124.194863205091)) ;
#74176 = CARTESIAN_POINT('Ctrl Pts',(-18.4466924342053,-22.6306509970149,
124.571839161865)) ;
#74177 = CARTESIAN_POINT('Ctrl Pts',(-18.6391999895716,-22.4506619165961,
124.339828335497)) ;
#74178 = CARTESIAN_POINT('Ctrl Pts',(-18.663412437741,-22.6406860875553,124.722085054517)) ;
#74179 = CARTESIAN_POINT('Ctrl Pts',(-18.8125751167322,-22.4606970071365,
124.460026463756)) ;
#74180 = CARTESIAN_POINT('Ctrl Pts',(-18.9029886662183,-22.650710606538,124.831675526104)) ;
#74181 = CARTESIAN_POINT('Ctrl Pts',(-19.0042354735576,-22.4707215261192,
124.547700237809)) ;
#74182 = CARTESIAN_POINT('Ctrl Pts',(-19.1536198777415,-22.6605704519482,
124.897332264214)) ;
#74183 = CARTESIAN_POINT('Ctrl Pts',(-19.204739284053,-22.4805813715294,124.600226994176)) ;
#74184 = CARTESIAN_POINT('Ctrl Pts',(-19.4144244913006,-22.6705302282638,
124.919409093061)) ;
#74185 = CARTESIAN_POINT('Ctrl Pts',(-19.4133825651792,-22.4905411478451,
124.617890170222)) ;
#74186 = CARTESIAN_POINT('Ctrl Pts',(-19.6768496651458,-22.6805584255785,
124.895342097737)) ;
#74187 = CARTESIAN_POINT('Ctrl Pts',(-19.6233228939347,-22.5005693451597,
124.598638241263)) ;
#74188 = CARTESIAN_POINT('Ctrl Pts',(-19.9281559636439,-22.6904659678688,
124.827199647071)) ;
#74189 = CARTESIAN_POINT('Ctrl Pts',(-19.8243678986999,-22.51047688745,124.544126081424)) ;
#74190 = CARTESIAN_POINT('Ctrl Pts',(-20.1667897462468,-22.7004986184326,
124.715157775164)) ;
#74191 = CARTESIAN_POINT('Ctrl Pts',(-20.0152757027157,-22.5205095380139,
124.454494146685)) ;
#74192 = CARTESIAN_POINT('Ctrl Pts',(-20.3792168210654,-22.7103825748593,
124.565679509322)) ;
#74193 = CARTESIAN_POINT('Ctrl Pts',(-20.1852178909652,-22.5303934944406,
124.334913312455)) ;
#74194 = CARTESIAN_POINT('Ctrl Pts',(-20.5648833310454,-22.7203722762211,
124.380082284129)) ;
#74195 = CARTESIAN_POINT('Ctrl Pts',(-20.333752327996,-22.5403831958024,124.18643693813)) ;
#74196 = CARTESIAN_POINT('Ctrl Pts',(-20.7158142404303,-22.7304132714972,
124.163643559997)) ;
#74197 = CARTESIAN_POINT('Ctrl Pts',(-20.454498551908,-22.5504241910784,124.013286914038)) ;
#74198 = CARTESIAN_POINT('Ctrl Pts',(-20.8249543880197,-22.7402461607655,
123.929430163596)) ;
#74199 = CARTESIAN_POINT('Ctrl Pts',(-20.5418120172613,-22.5602570803468,
123.825917666245)) ;
#74200 = CARTESIAN_POINT('Ctrl Pts',(-20.8935867560127,-22.750239319133,123.675951817859)) ;
#74201 = CARTESIAN_POINT('Ctrl Pts',(-20.5967197715693,-22.5702502387142,
123.623135597207)) ;
#74202 = CARTESIAN_POINT('Ctrl Pts',(-20.9167106283964,-22.7602713614851,
123.413324039136)) ;
#74203 = CARTESIAN_POINT('Ctrl Pts',(-20.6152207367782,-22.5802822810663,
123.413033509542)) ;
#74204 = CARTESIAN_POINT('Ctrl Pts',(-20.8945827854885,-22.7701366054435,
123.155034786076)) ;
#74205 = CARTESIAN_POINT('Ctrl Pts',(-20.5975204254551,-22.5901475250248,
123.206402523635)) ;
#74206 = CARTESIAN_POINT('Ctrl Pts',(-20.8280023409781,-22.7800984966895,
122.901847296209)) ;
#74207 = CARTESIAN_POINT('Ctrl Pts',(-20.5442580738547,-22.6001094162708,
123.003852212977)) ;
#74208 = CARTESIAN_POINT('Ctrl Pts',(-20.7172881604763,-22.790133396708,122.66252192034)) ;
#74209 = CARTESIAN_POINT('Ctrl Pts',(-20.4556884995148,-22.6101443162892,
122.812391063934)) ;
#74210 = CARTESIAN_POINT('Ctrl Pts',(-20.5692752425529,-22.8000184771226,
122.449004039162)) ;
#74211 = CARTESIAN_POINT('Ctrl Pts',(-20.3372800779245,-22.6200293967038,
122.641575980296)) ;
#74212 = CARTESIAN_POINT('Ctrl Pts',(-20.3831352081332,-22.8100836492474,
122.261135086184)) ;
#74213 = CARTESIAN_POINT('Ctrl Pts',(-20.1883694027549,-22.6300945688287,
122.491279318454)) ;
#74214 = CARTESIAN_POINT('Ctrl Pts',(-20.1719153766464,-22.8199308839709,
122.111588554408)) ;
#74215 = CARTESIAN_POINT('Ctrl Pts',(-20.0193951546591,-22.6399418035521,
122.37164074922)) ;
#74216 = CARTESIAN_POINT('Ctrl Pts',(-19.9338810020047,-22.8299616952886,
121.998385955135)) ;
#74217 = CARTESIAN_POINT('Ctrl Pts',(-19.8289685381442,-22.6499726148699,
122.281076763213)) ;
#74218 = CARTESIAN_POINT('Ctrl Pts',(-19.6801542546411,-22.8399713112021,
121.92888895062)) ;
#74219 = CARTESIAN_POINT('Ctrl Pts',(-19.6259877257716,-22.6599822307834,
122.225477204985)) ;
#74220 = CARTESIAN_POINT('Ctrl Pts',(-19.4208786354204,-22.8498820906059,
121.904493618339)) ;
#74221 = CARTESIAN_POINT('Ctrl Pts',(-19.4185677565269,-22.6698930101871,
122.20595890965)) ;
#74222 = CARTESIAN_POINT('Ctrl Pts',(-19.1607322268199,-22.8598113563949,
121.924877430806)) ;
#74223 = CARTESIAN_POINT('Ctrl Pts',(-19.2104507120868,-22.6798222759761,
122.222263811396)) ;
#74224 = CARTESIAN_POINT('Ctrl Pts',(-18.9052696005904,-22.8698540497075,
121.991077325564)) ;
#74225 = CARTESIAN_POINT('Ctrl Pts',(-19.0060800555527,-22.6898649692887,
122.275221687729)) ;
#74226 = CARTESIAN_POINT('Ctrl Pts',(-18.6688210508007,-22.8797405824022,
122.098781259465)) ;
#74227 = CARTESIAN_POINT('Ctrl Pts',(-18.8169206428243,-22.6997515019835,
122.361382756701)) ;
#74228 = CARTESIAN_POINT('Ctrl Pts',(-18.4521283292077,-22.8897337275055,
122.247107144914)) ;
#74229 = CARTESIAN_POINT('Ctrl Pts',(-18.6435653091888,-22.7097446470868,
122.480041629506)) ;
#74230 = CARTESIAN_POINT('Ctrl Pts',(-18.2654318575566,-22.8996794081796,
122.430014319168)) ;
#74231 = CARTESIAN_POINT('Ctrl Pts',(-18.4942067535944,-22.7196903277608,
122.626365697427)) ;
#74232 = CARTESIAN_POINT('Ctrl Pts',(-18.1128639587461,-22.9096266658063,
122.642292140938)) ;
#74233 = CARTESIAN_POINT('Ctrl Pts',(-18.372150743422,-22.7296375853876,122.796186542585)) ;
#74234 = CARTESIAN_POINT('Ctrl Pts',(-17.9986015571631,-22.9196745679278,
122.8803282538)) ;
#74235 = CARTESIAN_POINT('Ctrl Pts',(-18.280738856107,-22.739685487509,122.986614497746)) ;
#74236 = CARTESIAN_POINT('Ctrl Pts',(-17.9286121290648,-22.9295222735495,
123.129473138902)) ;
#74237 = CARTESIAN_POINT('Ctrl Pts',(-18.2247452886835,-22.7495331931307,
123.18592950677)) ;
#74238 = CARTESIAN_POINT('Ctrl Pts',(-17.9018275041775,-22.9394837401836,
123.389866644)) ;
#74239 = CARTESIAN_POINT('Ctrl Pts',(-18.2033153717119,-22.7594946597648,
123.394243983057)) ;
#74240 = CARTESIAN_POINT('Ctrl Pts',(-17.9211473398124,-22.9495132934518,
123.652733485391)) ;
#74241 = CARTESIAN_POINT('Ctrl Pts',(-18.2187690258878,-22.769524213033,123.604537583863)) ;
#74242 = CARTESIAN_POINT('Ctrl Pts',(-17.9848788716588,-22.9594201854792,
123.905158576433)) ;
#74243 = CARTESIAN_POINT('Ctrl Pts',(-18.2697520510413,-22.7794311050604,
123.806478038071)) ;
#74244 = CARTESIAN_POINT('Ctrl Pts',(-18.0914378077315,-22.9693678295922,
124.143845240082)) ;
#74245 = CARTESIAN_POINT('Ctrl Pts',(-18.3549971072633,-22.7893787491735,
123.997428193049)) ;
#74246 = CARTESIAN_POINT('Ctrl Pts',(-18.2384883381668,-22.9793678726211,
124.361682579481)) ;
#74247 = CARTESIAN_POINT('Ctrl Pts',(-18.4726356373326,-22.7993787922023,
124.17169927459)) ;
#74248 = CARTESIAN_POINT('Ctrl Pts',(-18.4221353270863,-22.9894066386151,
124.551044334178)) ;
#74249 = CARTESIAN_POINT('Ctrl Pts',(-18.6195515901072,-22.8094175581963,
124.323190202852)) ;
#74250 = CARTESIAN_POINT('Ctrl Pts',(-18.6310313254935,-22.9992317006373,
124.702816918831)) ;
#74251 = CARTESIAN_POINT('Ctrl Pts',(-18.7866669492004,-22.8192426202186,
124.444610004211)) ;
#74252 = CARTESIAN_POINT('Ctrl Pts',(-18.8683046803301,-23.0092862479637,
124.819034540498)) ;
#74253 = CARTESIAN_POINT('Ctrl Pts',(-18.9764846127344,-22.8292971675449,
124.537586113637)) ;
#74254 = CARTESIAN_POINT('Ctrl Pts',(-19.1194917233143,-23.0192294914129,
124.89104987129)) ;
#74255 = CARTESIAN_POINT('Ctrl Pts',(-19.1774335457929,-22.8392404109942,
124.59520052088)) ;
#74256 = CARTESIAN_POINT('Ctrl Pts',(-19.3782034066458,-23.0291316630208,
124.919048155832)) ;
#74257 = CARTESIAN_POINT('Ctrl Pts',(-19.3844026140547,-22.849142582602,124.617601382244)) ;
#74258 = CARTESIAN_POINT('Ctrl Pts',(-19.6417720055684,-23.039184498631,124.901274622892)) ;
#74259 = CARTESIAN_POINT('Ctrl Pts',(-19.5952575647132,-22.8591954182122,
124.603384820688)) ;
#74260 = CARTESIAN_POINT('Ctrl Pts',(-19.8937094830224,-23.0490575563165,
124.839234191548)) ;
#74261 = CARTESIAN_POINT('Ctrl Pts',(-19.7968081119254,-22.8690684758978,
124.553754624461)) ;
#74262 = CARTESIAN_POINT('Ctrl Pts',(-20.1342348698511,-23.0590528178422,
124.733693798466)) ;
#74263 = CARTESIAN_POINT('Ctrl Pts',(-19.9892291535961,-22.8790637374234,
124.469324531308)) ;
#74264 = CARTESIAN_POINT('Ctrl Pts',(-20.3531841876224,-23.0690781872627,
124.587158170205)) ;
#74265 = CARTESIAN_POINT('Ctrl Pts',(-20.1643902941915,-22.8890891068439,
124.352097370289)) ;
#74266 = CARTESIAN_POINT('Ctrl Pts',(-20.5410358789156,-23.0789680197893,
124.407538040027)) ;
#74267 = CARTESIAN_POINT('Ctrl Pts',(-20.3146713621505,-22.8989789393705,
124.208404998467)) ;
#74268 = CARTESIAN_POINT('Ctrl Pts',(-20.7481493171931,-23.0922659905986,
124.126127329807)) ;
#74269 = CARTESIAN_POINT('Ctrl Pts',(-20.4803737638767,-22.9122769101799,
123.98326757738)) ;
#74270 = CARTESIAN_POINT('Ctrl Pts',(-20.8766367896411,-23.1054643857078,
123.799667857757)) ;
#74271 = CARTESIAN_POINT('Ctrl Pts',(-20.58316718686,-22.9254753052891,123.722071594726)) ;
#74272 = CARTESIAN_POINT('Ctrl Pts',(-20.9162580762145,-23.1188598279873,
123.449902418925)) ;
#74273 = CARTESIAN_POINT('Ctrl Pts',(-20.6148571213026,-22.9388707475686,
123.442305273441)) ;
#74274 = CARTESIAN_POINT('Ctrl Pts',(-20.9004717404035,-23.1287356662262,
123.190816756854)) ;
#74275 = CARTESIAN_POINT('Ctrl Pts',(-20.6022321474832,-22.9487465858075,
123.235027218103)) ;
#74276 = CARTESIAN_POINT('Ctrl Pts',(-20.8389416667209,-23.138797068824,122.933714939008)) ;
#74277 = CARTESIAN_POINT('Ctrl Pts',(-20.5530100608366,-22.9588079884053,
123.029348080478)) ;
#74278 = CARTESIAN_POINT('Ctrl Pts',(-20.7357971607968,-23.1486621257591,
122.695832837335)) ;
#74279 = CARTESIAN_POINT('Ctrl Pts',(-20.4704951899831,-22.9686730453404,
122.839039863601)) ;
#74280 = CARTESIAN_POINT('Ctrl Pts',(-20.5912157870912,-23.1586742217079,
122.476050346829)) ;
#74281 = CARTESIAN_POINT('Ctrl Pts',(-20.3548367390331,-22.9786851412892,
122.663215848403)) ;
#74282 = CARTESIAN_POINT('Ctrl Pts',(-20.3516936594629,-23.1719515308534,
122.222286259343)) ;
#74283 = CARTESIAN_POINT('Ctrl Pts',(-20.1631968596537,-22.9919624504346,
122.460187975031)) ;
#74284 = CARTESIAN_POINT('Ctrl Pts',(-19.976439806796,-23.1885505563607,121.990323874567)) ;
#74285 = CARTESIAN_POINT('Ctrl Pts',(-19.8630376390117,-23.0085614759419,
122.27463286839)) ;
#74286 = CARTESIAN_POINT('Ctrl Pts',(-19.5445846288345,-23.2051496043937,
121.900290049197)) ;
#74287 = CARTESIAN_POINT('Ctrl Pts',(-19.5174874237851,-23.025160523975,122.202591932357)) ;
#74288 = CARTESIAN_POINT('Ctrl Pts',(-19.1970504323598,-23.2183930164246,
121.919316506813)) ;
#74289 = CARTESIAN_POINT('Ctrl Pts',(-19.2395130687559,-23.0384039360059,
122.217815974426)) ;
#74290 = CARTESIAN_POINT('Ctrl Pts',(-18.9401631490869,-23.2284304441131,
121.979134289614)) ;
#74291 = CARTESIAN_POINT('Ctrl Pts',(-19.0339916375281,-23.0484413636943,
122.26566763804)) ;
#74292 = CARTESIAN_POINT('Ctrl Pts',(-18.7007825062175,-23.2383347460687,
122.081317818178)) ;
#74293 = CARTESIAN_POINT('Ctrl Pts',(-18.8424912391791,-23.0583456656499,
122.347410849636)) ;
#74294 = CARTESIAN_POINT('Ctrl Pts',(-18.4082618728007,-23.2516015860438,
122.27103030745)) ;
#74295 = CARTESIAN_POINT('Ctrl Pts',(-18.60846034993,-23.0716125056251,122.499189722715)) ;
#74296 = CARTESIAN_POINT('Ctrl Pts',(-18.1123399886893,-23.2682277841338,
122.599191193704)) ;
#74297 = CARTESIAN_POINT('Ctrl Pts',(-18.37173453001,-23.088238703715,122.761707661206)) ;
#74298 = CARTESIAN_POINT('Ctrl Pts',(-17.9131297580703,-23.2881468995172,
123.089717711768)) ;
#74299 = CARTESIAN_POINT('Ctrl Pts',(-18.2123565653371,-23.1081578190985,
123.154114524712)) ;
#74300 = CARTESIAN_POINT('Ctrl Pts',(-17.8962057486873,-23.3047533226514,
123.530754190473)) ;
#74301 = CARTESIAN_POINT('Ctrl Pts',(-18.1988208182487,-23.1247642422327,
123.506996945006)) ;
#74302 = CARTESIAN_POINT('Ctrl Pts',(-17.9736383079811,-23.3180495431471,
123.871481315113)) ;
#74303 = CARTESIAN_POINT('Ctrl Pts',(-18.260758884604,-23.1380604627284,123.779530840826)) ;
#74304 = CARTESIAN_POINT('Ctrl Pts',(-18.1080876894243,-23.3313183754886,
124.193291225487)) ;
#74305 = CARTESIAN_POINT('Ctrl Pts',(-18.3683238288418,-23.1513292950698,
124.03699746914)) ;
#74306 = CARTESIAN_POINT('Ctrl Pts',(-18.3795904845169,-23.3480096235217,
124.544002089699)) ;
#74307 = CARTESIAN_POINT('Ctrl Pts',(-18.5855160258156,-23.1680205431029,
124.317555357592)) ;
#74308 = CARTESIAN_POINT('Ctrl Pts',(-18.8243580038421,-23.3678193551945,
124.825895671642)) ;
#74309 = CARTESIAN_POINT('Ctrl Pts',(-18.9413318339364,-23.1878302747757,
124.543077599675)) ;
#74310 = CARTESIAN_POINT('Ctrl Pts',(-19.342669247738,-23.387796962523,124.941057197764)) ;
#74311 = CARTESIAN_POINT('Ctrl Pts',(-19.3559797197809,-23.2078078821043,
124.635208534349)) ;
#74312 = CARTESIAN_POINT('Ctrl Pts',(-19.8676443126911,-23.4077232715809,
124.871649885316)) ;
#74313 = CARTESIAN_POINT('Ctrl Pts',(-19.7759608640312,-23.2277341911621,
124.579685870567)) ;
#74314 = CARTESIAN_POINT('Ctrl Pts',(-20.3358743902142,-23.4275401317456,
124.63015528066)) ;
#74315 = CARTESIAN_POINT('Ctrl Pts',(-20.1505472945724,-23.2475510513268,
124.386491407269)) ;
#74316 = CARTESIAN_POINT('Ctrl Pts',(-20.6978674016967,-23.4476399473396,
124.237525821814)) ;
#74317 = CARTESIAN_POINT('Ctrl Pts',(-20.4401428874829,-23.2676508669208,
124.072390151263)) ;
#74318 = CARTESIAN_POINT('Ctrl Pts',(-20.9010174942789,-23.4673969112221,
123.753071870138)) ;
#74319 = CARTESIAN_POINT('Ctrl Pts',(-20.6026658029561,-23.2874078308034,
123.684825804928)) ;
#74320 = CARTESIAN_POINT('Ctrl Pts',(-20.9280426936551,-23.4874338372916,
123.221391133702)) ;
#74321 = CARTESIAN_POINT('Ctrl Pts',(-20.6242875973045,-23.3074447568728,
123.259481619139)) ;
#74322 = CARTESIAN_POINT('Ctrl Pts',(-20.7724260968496,-23.5073034196731,
122.716597558735)) ;
#74323 = CARTESIAN_POINT('Ctrl Pts',(-20.4997956703775,-23.3273143392544,
122.855645015619)) ;
#74324 = CARTESIAN_POINT('Ctrl Pts',(-20.4545393934254,-23.5272079914263,
122.293853597021)) ;
#74325 = CARTESIAN_POINT('Ctrl Pts',(-20.245486515064,-23.3472189110075,122.517448272747)) ;
#74326 = CARTESIAN_POINT('Ctrl Pts',(-20.010214950493,-23.5471605936248,122.004204373884)) ;
#74327 = CARTESIAN_POINT('Ctrl Pts',(-19.8900270498159,-23.367171513206,122.28572785493)) ;
#74328 = CARTESIAN_POINT('Ctrl Pts',(-19.4949902616996,-23.567070084595,121.884042017119)) ;
#74329 = CARTESIAN_POINT('Ctrl Pts',(-19.477846400596,-23.3870810041763,122.189596888272)) ;
#74330 = CARTESIAN_POINT('Ctrl Pts',(-18.9708122647387,-23.5869214532945,
121.945279500549)) ;
#74331 = CARTESIAN_POINT('Ctrl Pts',(-19.0585021151188,-23.4069323728757,
122.23858718962)) ;
#74332 = CARTESIAN_POINT('Ctrl Pts',(-18.4941229339975,-23.6070016494305,
122.185035924268)) ;
#74333 = CARTESIAN_POINT('Ctrl Pts',(-18.6771515404996,-23.4270125690117,
122.43039179208)) ;
#74334 = CARTESIAN_POINT('Ctrl Pts',(-18.1327837984762,-23.6268025930059,
122.567847534535)) ;
#74335 = CARTESIAN_POINT('Ctrl Pts',(-18.3880785930256,-23.4468135125871,
122.736642978161)) ;
#74336 = CARTESIAN_POINT('Ctrl Pts',(-17.9208269263131,-23.6467865695154,
123.054772698346)) ;
#74337 = CARTESIAN_POINT('Ctrl Pts',(-18.2185138580659,-23.4667974890966,
123.126183626084)) ;
#74338 = CARTESIAN_POINT('Ctrl Pts',(-17.8886839109788,-23.666702532491,123.583127051777)) ;
#74339 = CARTESIAN_POINT('Ctrl Pts',(-18.1928000784033,-23.4867134520722,
123.548868146991)) ;
#74340 = CARTESIAN_POINT('Ctrl Pts',(-18.0370543005805,-23.6865729673129,
124.090087584565)) ;
#74341 = CARTESIAN_POINT('Ctrl Pts',(-18.3114982241245,-23.5065838868942,
123.954437479053)) ;
#74342 = CARTESIAN_POINT('Ctrl Pts',(-18.3529120735645,-23.706623252546,124.519105466841)) ;
#74343 = CARTESIAN_POINT('Ctrl Pts',(-18.5641852225777,-23.5266341721272,
124.297650597675)) ;
#74344 = CARTESIAN_POINT('Ctrl Pts',(-18.7899845412355,-23.7263972213053,
124.811340607941)) ;
#74345 = CARTESIAN_POINT('Ctrl Pts',(-18.9138460145566,-23.5464081408865,
124.531438476037)) ;
#74346 = CARTESIAN_POINT('Ctrl Pts',(-19.3073372095551,-23.7464536794248,
124.938934907385)) ;
#74347 = CARTESIAN_POINT('Ctrl Pts',(-19.3277281762554,-23.5664645990061,
124.633511759487)) ;
#74348 = CARTESIAN_POINT('Ctrl Pts',(-19.8306051755305,-23.7662485624158,
124.882843707618)) ;
#74349 = CARTESIAN_POINT('Ctrl Pts',(-19.7463441186502,-23.5862594819971,
124.588636471734)) ;
#74350 = CARTESIAN_POINT('Ctrl Pts',(-20.3078444225555,-23.7862152177182,
124.651011447799)) ;
#74351 = CARTESIAN_POINT('Ctrl Pts',(-20.1281345081567,-23.6062261372994,
124.40316804433)) ;
#74352 = CARTESIAN_POINT('Ctrl Pts',(-20.6767016462669,-23.8061741877947,
124.269621393415)) ;
#74353 = CARTESIAN_POINT('Ctrl Pts',(-20.4232185854534,-23.6261851073759,
124.09805398004)) ;
#74354 = CARTESIAN_POINT('Ctrl Pts',(-20.8928840688212,-23.8260702753848,
123.787054530336)) ;
#74355 = CARTESIAN_POINT('Ctrl Pts',(-20.5961622166163,-23.6460811949661,
123.711998606436)) ;
#74356 = CARTESIAN_POINT('Ctrl Pts',(-20.9320464015032,-23.8459684452964,
123.25969081321)) ;
#74357 = CARTESIAN_POINT('Ctrl Pts',(-20.6274889756677,-23.6659793648776,
123.290106706066)) ;
#74358 = CARTESIAN_POINT('Ctrl Pts',(-20.7893616369833,-23.8658742806635,
122.750190072166)) ;
#74359 = CARTESIAN_POINT('Ctrl Pts',(-20.5133377383693,-23.6858852002447,
122.882506513553)) ;
#74360 = CARTESIAN_POINT('Ctrl Pts',(-20.4807327589257,-23.8858242056014,
122.319088447616)) ;
#74361 = CARTESIAN_POINT('Ctrl Pts',(-20.2664316366618,-23.7058351251827,
122.537627039628)) ;
#74362 = CARTESIAN_POINT('Ctrl Pts',(-20.0452649316596,-23.9057033955118,
122.019778092152)) ;
#74363 = CARTESIAN_POINT('Ctrl Pts',(-19.9180547884745,-23.725714315093,122.298181446568)) ;
#74364 = CARTESIAN_POINT('Ctrl Pts',(-19.5313379425043,-23.9256847197924,
121.886108845962)) ;
#74365 = CARTESIAN_POINT('Ctrl Pts',(-19.5069121971362,-23.7456956393736,
122.191249793125)) ;
#74366 = CARTESIAN_POINT('Ctrl Pts',(-19.0038793189926,-23.9456145040007,
121.936000230765)) ;
#74367 = CARTESIAN_POINT('Ctrl Pts',(-19.084945405429,-23.765625423582,122.231166579714)) ;
#74368 = CARTESIAN_POINT('Ctrl Pts',(-18.5255093850122,-23.9655344933915,
122.162577000596)) ;
#74369 = CARTESIAN_POINT('Ctrl Pts',(-18.70225086222,-23.7855454129728,122.412432333271)) ;
#74370 = CARTESIAN_POINT('Ctrl Pts',(-18.1533588422932,-23.9853896887455,
122.536910497514)) ;
#74371 = CARTESIAN_POINT('Ctrl Pts',(-18.4045331019949,-23.8054006083268,
122.711900044301)) ;
#74372 = CARTESIAN_POINT('Ctrl Pts',(-17.9297252154946,-24.0054356904049,
123.020349675074)) ;
#74373 = CARTESIAN_POINT('Ctrl Pts',(-18.225629991919,-23.8254466099861,123.098661705087)) ;
#74374 = CARTESIAN_POINT('Ctrl Pts',(-17.8922881636494,-24.0219354376147,
123.457418896115)) ;
#74375 = CARTESIAN_POINT('Ctrl Pts',(-18.1956840852011,-23.8419463571959,
123.448290621712)) ;
#74376 = CARTESIAN_POINT('Ctrl Pts',(-17.9536182368234,-24.0353240420628,
123.80382318546)) ;
#74377 = CARTESIAN_POINT('Ctrl Pts',(-18.2447511118131,-23.855334961644,123.725437823404)) ;
#74378 = CARTESIAN_POINT('Ctrl Pts',(-18.0424306541701,-24.0451858703977,
124.047300970895)) ;
#74379 = CARTESIAN_POINT('Ctrl Pts',(-18.3158010379649,-23.8651967899789,
123.920212948107)) ;
#74380 = CARTESIAN_POINT('Ctrl Pts',(-18.1728224347277,-24.0551520131552,
124.274441107763)) ;
#74381 = CARTESIAN_POINT('Ctrl Pts',(-18.4201247042669,-23.8751629327365,
124.101932317986)) ;
#74382 = CARTESIAN_POINT('Ctrl Pts',(-18.3983154769493,-24.0685137592802,
124.543527593451)) ;
#74383 = CARTESIAN_POINT('Ctrl Pts',(-18.600479724246,-23.8885246788614,124.317163946771)) ;
#74384 = CARTESIAN_POINT('Ctrl Pts',(-18.7557534013745,-24.0849680882353,
124.79576607839)) ;
#74385 = CARTESIAN_POINT('Ctrl Pts',(-18.8864880582342,-23.9049790078165,
124.518993913012)) ;
#74386 = CARTESIAN_POINT('Ctrl Pts',(-19.1855079887592,-24.1017353332835,
124.913045707108)) ;
#74387 = CARTESIAN_POINT('Ctrl Pts',(-19.2302449597953,-23.9217462528648,
124.61279458323)) ;
#74388 = CARTESIAN_POINT('Ctrl Pts',(-19.5321625871977,-24.1149218985576,
124.914163508208)) ;
#74389 = CARTESIAN_POINT('Ctrl Pts',(-19.5076007478974,-23.9349328181389,
124.613694249745)) ;
#74390 = CARTESIAN_POINT('Ctrl Pts',(-19.7909027433504,-24.1249113573022,
124.870218955384)) ;
#74391 = CARTESIAN_POINT('Ctrl Pts',(-19.7145860227272,-23.9449222768835,
124.578534711631)) ;
#74392 = CARTESIAN_POINT('Ctrl Pts',(-20.0373293988203,-24.1348651297833,
124.782335916203)) ;
#74393 = CARTESIAN_POINT('Ctrl Pts',(-19.9117282978741,-23.9548760493646,
124.508226619746)) ;
#74394 = CARTESIAN_POINT('Ctrl Pts',(-20.2667248445259,-24.144912946316,124.651640371328)) ;
#74395 = CARTESIAN_POINT('Ctrl Pts',(-20.0952430132553,-23.9649238658972,
124.403668150689)) ;
#74396 = CARTESIAN_POINT('Ctrl Pts',(-20.4660081192489,-24.1547544794385,
124.486757064538)) ;
#74397 = CARTESIAN_POINT('Ctrl Pts',(-20.2546683482556,-23.9747653990197,
124.27175978153)) ;
#74398 = CARTESIAN_POINT('Ctrl Pts',(-20.636481553147,-24.1647407216582,124.287296273897)) ;
#74399 = CARTESIAN_POINT('Ctrl Pts',(-20.3910452989074,-23.9847516412394,
124.112189719401)) ;
#74400 = CARTESIAN_POINT('Ctrl Pts',(-20.7692271457761,-24.1746773450831,
124.06238042497)) ;
#74401 = CARTESIAN_POINT('Ctrl Pts',(-20.497239809877,-23.9946882646643,123.932255945756)) ;
#74402 = CARTESIAN_POINT('Ctrl Pts',(-20.8617993883926,-24.184727222466,123.815064619608)) ;
#74403 = CARTESIAN_POINT('Ctrl Pts',(-20.5712954677108,-24.0047381420473,
123.734402552555)) ;
#74404 = CARTESIAN_POINT('Ctrl Pts',(-20.9092661001648,-24.1945776612436,
123.560575071868)) ;
#74405 = CARTESIAN_POINT('Ctrl Pts',(-20.6092666006814,-24.0145885808249,
123.53081059359)) ;
#74406 = CARTESIAN_POINT('Ctrl Pts',(-20.9125392724031,-24.2045496752123,
123.298574461712)) ;
#74407 = CARTESIAN_POINT('Ctrl Pts',(-20.6118828876205,-24.0245605947936,
123.3212101705)) ;
#74408 = CARTESIAN_POINT('Ctrl Pts',(-20.8701252718286,-24.2145448438384,
123.039316830686)) ;
#74409 = CARTESIAN_POINT('Ctrl Pts',(-20.5779494825875,-24.0345557634197,
123.113804490714)) ;
#74410 = CARTESIAN_POINT('Ctrl Pts',(-20.78272672112,-24.2245787270997,122.790564493775)) ;
#74411 = CARTESIAN_POINT('Ctrl Pts',(-20.5080285227167,-24.0445896466809,
122.914803398227)) ;
#74412 = CARTESIAN_POINT('Ctrl Pts',(-20.6560814228893,-24.234434597163,122.564616215092)) ;
#74413 = CARTESIAN_POINT('Ctrl Pts',(-20.4067104191487,-24.0544455167443,
122.734046035466)) ;
#74414 = CARTESIAN_POINT('Ctrl Pts',(-20.4901252099173,-24.2444321430802,
122.360979293834)) ;
#74415 = CARTESIAN_POINT('Ctrl Pts',(-20.2739437686294,-24.0644430626614,
122.571137967992)) ;
#74416 = CARTESIAN_POINT('Ctrl Pts',(-20.2931350357888,-24.2543402699794,
122.190698398453)) ;
#74417 = CARTESIAN_POINT('Ctrl Pts',(-20.1163503191905,-24.0743511895607,
122.434915056073)) ;
#74418 = CARTESIAN_POINT('Ctrl Pts',(-20.0674961654785,-24.2643506415016,
122.055437128111)) ;
#74419 = CARTESIAN_POINT('Ctrl Pts',(-19.9358381408742,-24.0843615610829,
122.326707954225)) ;
#74420 = CARTESIAN_POINT('Ctrl Pts',(-19.8211172047511,-24.274381084249,121.961778537645)) ;
#74421 = CARTESIAN_POINT('Ctrl Pts',(-19.7387341883922,-24.0943920038303,
122.251783172163)) ;
#74422 = CARTESIAN_POINT('Ctrl Pts',(-19.567014787891,-24.2842290368023,121.912623318363)) ;
#74423 = CARTESIAN_POINT('Ctrl Pts',(-19.5354521536671,-24.1042399563836,
122.212461213181)) ;
#74424 = CARTESIAN_POINT('Ctrl Pts',(-19.3026436245722,-24.2942917058233,
121.908036630915)) ;
#74425 = CARTESIAN_POINT('Ctrl Pts',(-19.3239551506336,-24.1143026254045,
122.208794046212)) ;
#74426 = CARTESIAN_POINT('Ctrl Pts',(-19.0458393133489,-24.3041860812872,
121.948921771781)) ;
#74427 = CARTESIAN_POINT('Ctrl Pts',(-19.1185123080235,-24.1241970008685,
122.24150428493)) ;
#74428 = CARTESIAN_POINT('Ctrl Pts',(-18.7986820358378,-24.3141278796054,
122.033501629757)) ;
#74429 = CARTESIAN_POINT('Ctrl Pts',(-18.9207873807656,-24.1341387991866,
122.309170130401)) ;
#74430 = CARTESIAN_POINT('Ctrl Pts',(-18.568460887549,-24.3241303733327,122.160425707842)) ;
#74431 = CARTESIAN_POINT('Ctrl Pts',(-18.7366115490919,-24.1441412929139,
122.410711225786)) ;
#74432 = CARTESIAN_POINT('Ctrl Pts',(-18.3634159134579,-24.3341651718396,
122.32621930411)) ;
#74433 = CARTESIAN_POINT('Ctrl Pts',(-18.572576923515,-24.1541760914208,122.543347798557)) ;
#74434 = CARTESIAN_POINT('Ctrl Pts',(-18.1931997743441,-24.3440100558189,
122.521073096118)) ;
#74435 = CARTESIAN_POINT('Ctrl Pts',(-18.4364059140593,-24.1640209754002,
122.699231890635)) ;
#74436 = CARTESIAN_POINT('Ctrl Pts',(-18.0570939033418,-24.353995912637,122.74538606812)) ;
#74437 = CARTESIAN_POINT('Ctrl Pts',(-18.3275230654761,-24.1740068322182,
122.878683238655)) ;
#74438 = CARTESIAN_POINT('Ctrl Pts',(-17.9622837120141,-24.3639307268117,
122.988691099176)) ;
#74439 = CARTESIAN_POINT('Ctrl Pts',(-18.2516769244132,-24.183941646393,123.07332776623)) ;
#74440 = CARTESIAN_POINT('Ctrl Pts',(-17.9107758865764,-24.3739882265971,
123.247885387994)) ;
#74441 = CARTESIAN_POINT('Ctrl Pts',(-18.2104726941361,-24.1939991461783,
123.28068369653)) ;
#74442 = CARTESIAN_POINT('Ctrl Pts',(-17.9047935451196,-24.3838099850154,
123.505950068635)) ;
#74443 = CARTESIAN_POINT('Ctrl Pts',(-18.2056888745737,-24.2038209045966,
123.487134859051)) ;
#74444 = CARTESIAN_POINT('Ctrl Pts',(-17.9441385894984,-24.3938656427994,
123.767234420937)) ;
#74445 = CARTESIAN_POINT('Ctrl Pts',(-18.2371668835213,-24.2138765623806,
123.696162133941)) ;
#74446 = CARTESIAN_POINT('Ctrl Pts',(-18.0277646257666,-24.4038078249794,
124.014774122517)) ;
#74447 = CARTESIAN_POINT('Ctrl Pts',(-18.3040695599417,-24.2238187445607,
123.894192987516)) ;
#74448 = CARTESIAN_POINT('Ctrl Pts',(-18.1519307758805,-24.4137130336741,
124.243545142384)) ;
#74449 = CARTESIAN_POINT('Ctrl Pts',(-18.4034039803286,-24.2337239532553,
124.077208506641)) ;
#74450 = CARTESIAN_POINT('Ctrl Pts',(-18.3162322484319,-24.4237548246365,
124.450038000941)) ;
#74451 = CARTESIAN_POINT('Ctrl Pts',(-18.5348467279855,-24.2437657442178,
124.242401635478)) ;
#74452 = CARTESIAN_POINT('Ctrl Pts',(-18.5112465950809,-24.4336625991088,
124.622564118238)) ;
#74453 = CARTESIAN_POINT('Ctrl Pts',(-18.6908591806819,-24.25367351869,124.380420796196)) ;
#74454 = CARTESIAN_POINT('Ctrl Pts',(-18.7353216882154,-24.4436740993364,
124.760445262969)) ;
#74455 = CARTESIAN_POINT('Ctrl Pts',(-18.8701201999352,-24.2636850189176,
124.490724088854)) ;
#74456 = CARTESIAN_POINT('Ctrl Pts',(-18.9806475911466,-24.4537068597291,
124.857016709401)) ;
#74457 = CARTESIAN_POINT('Ctrl Pts',(-19.0663816751917,-24.2737177793103,
124.567979438308)) ;
#74458 = CARTESIAN_POINT('Ctrl Pts',(-19.2342398512339,-24.463557428864,124.909018469906)) ;
#74459 = CARTESIAN_POINT('Ctrl Pts',(-19.2692552091276,-24.2835683484452,
124.609578862469)) ;
#74460 = CARTESIAN_POINT('Ctrl Pts',(-19.4965930730574,-24.4735460383939,
124.916794312938)) ;
#74461 = CARTESIAN_POINT('Ctrl Pts',(-19.4791376938432,-24.2935569579751,
124.615797717518)) ;
#74462 = CARTESIAN_POINT('Ctrl Pts',(-19.7547810174252,-24.483474694418,124.879120015972)) ;
#74463 = CARTESIAN_POINT('Ctrl Pts',(-19.685687402309,-24.3034856139992,124.585656541612)) ;
#74464 = CARTESIAN_POINT('Ctrl Pts',(-20.0041249025527,-24.4934624405958,
124.797121058198)) ;
#74465 = CARTESIAN_POINT('Ctrl Pts',(-19.8851618270809,-24.313473360177,124.520055766498)) ;
#74466 = CARTESIAN_POINT('Ctrl Pts',(-20.2363287244197,-24.5034984295315,
124.672094532579)) ;
#74467 = CARTESIAN_POINT('Ctrl Pts',(-20.0709240851037,-24.3235093491128,
124.42003291363)) ;
#74468 = CARTESIAN_POINT('Ctrl Pts',(-20.4398532894537,-24.5133532993451,
124.511915768952)) ;
#74469 = CARTESIAN_POINT('Ctrl Pts',(-20.23374208075,-24.3333642189264,124.291888988596)) ;
#74470 = CARTESIAN_POINT('Ctrl Pts',(-20.6152286146968,-24.5233527405869,
124.316286380205)) ;
#74471 = CARTESIAN_POINT('Ctrl Pts',(-20.3740410150847,-24.3433636601681,
124.135384433191)) ;
#74472 = CARTESIAN_POINT('Ctrl Pts',(-20.7528077612701,-24.533247814767,124.095579716409)) ;
#74473 = CARTESIAN_POINT('Ctrl Pts',(-20.4841026378956,-24.3532587343482,
123.958818739032)) ;
#74474 = CARTESIAN_POINT('Ctrl Pts',(-20.8515452177521,-24.5433084706067,
123.850362627623)) ;
#74475 = CARTESIAN_POINT('Ctrl Pts',(-20.5630911554068,-24.3633193901879,
123.762644277068)) ;
#74476 = CARTESIAN_POINT('Ctrl Pts',(-20.9052114657529,-24.5531573448023,
123.597149046197)) ;
#74477 = CARTESIAN_POINT('Ctrl Pts',(-20.6060224056543,-24.3731682643835,
123.560073894341)) ;
#74478 = CARTESIAN_POINT('Ctrl Pts',(-20.9149218985276,-24.5631860567655,
123.333787858279)) ;
#74479 = CARTESIAN_POINT('Ctrl Pts',(-20.6137892700435,-24.3831969763468,
123.349384859398)) ;
#74480 = CARTESIAN_POINT('Ctrl Pts',(-20.8780431868156,-24.5732154573486,
123.072813707598)) ;
#74481 = CARTESIAN_POINT('Ctrl Pts',(-20.5842846871539,-24.3932263769299,
123.140605706527)) ;
#74482 = CARTESIAN_POINT('Ctrl Pts',(-20.7984988601389,-24.5830556509655,
122.826757371422)) ;
#74483 = CARTESIAN_POINT('Ctrl Pts',(-20.5206480690799,-24.4030665705467,
122.943761971265)) ;
#74484 = CARTESIAN_POINT('Ctrl Pts',(-20.6758759732977,-24.5930590735407,
122.594259198582)) ;
#74485 = CARTESIAN_POINT('Ctrl Pts',(-20.4225485501973,-24.4130699931219,
122.757764169377)) ;
#74486 = CARTESIAN_POINT('Ctrl Pts',(-20.5149236679389,-24.6030446106337,
122.386952011264)) ;
#74487 = CARTESIAN_POINT('Ctrl Pts',(-20.2937856775477,-24.423055530215,122.591919429252)) ;
#74488 = CARTESIAN_POINT('Ctrl Pts',(-20.3192148830305,-24.6130856151206,
122.210004149997)) ;
#74489 = CARTESIAN_POINT('Ctrl Pts',(-20.1372175724213,-24.4330965347018,
122.450362171703)) ;
#74490 = CARTESIAN_POINT('Ctrl Pts',(-20.1002988243439,-24.6229291540618,
122.072161974202)) ;
#74491 = CARTESIAN_POINT('Ctrl Pts',(-19.9620847673465,-24.442940073643,122.340090125974)) ;
#74492 = CARTESIAN_POINT('Ctrl Pts',(-19.8575938758028,-24.6329141850526,
121.972533729816)) ;
#74493 = CARTESIAN_POINT('Ctrl Pts',(-19.7679204996431,-24.4529251046338,
122.260388809874)) ;
#74494 = CARTESIAN_POINT('Ctrl Pts',(-19.6023947114869,-24.6428536475746,
121.916697509482)) ;
#74495 = CARTESIAN_POINT('Ctrl Pts',(-19.5637613212233,-24.4628645671558,
122.215721172914)) ;
#74496 = CARTESIAN_POINT('Ctrl Pts',(-19.3388001962172,-24.6528933797984,
121.905974359245)) ;
#74497 = CARTESIAN_POINT('Ctrl Pts',(-19.3528855389491,-24.4729042993796,
122.207143937649)) ;
#74498 = CARTESIAN_POINT('Ctrl Pts',(-19.0812413724827,-24.6627815601156,
121.940528367515)) ;
#74499 = CARTESIAN_POINT('Ctrl Pts',(-19.1468393800042,-24.4827924796968,
122.23478829755)) ;
#74500 = CARTESIAN_POINT('Ctrl Pts',(-18.8309303395571,-24.6727710758181,
122.019607849818)) ;
#74501 = CARTESIAN_POINT('Ctrl Pts',(-18.9465910651468,-24.4927819953993,
122.298052933552)) ;
#74502 = CARTESIAN_POINT('Ctrl Pts',(-18.5989667873203,-24.6827296264728,
122.140752466217)) ;
#74503 = CARTESIAN_POINT('Ctrl Pts',(-18.7610210868457,-24.502740546054,122.394969531165)) ;
#74504 = CARTESIAN_POINT('Ctrl Pts',(-18.3923783176622,-24.6926290335778,
122.298887165162)) ;
#74505 = CARTESIAN_POINT('Ctrl Pts',(-18.5957515114888,-24.5126399531591,
122.521477699572)) ;
#74506 = CARTESIAN_POINT('Ctrl Pts',(-18.2138481636783,-24.7026776199941,
122.49341457571)) ;
#74507 = CARTESIAN_POINT('Ctrl Pts',(-18.4529280643294,-24.5226885395753,
122.677100488762)) ;
#74508 = CARTESIAN_POINT('Ctrl Pts',(-18.0737497674952,-24.7125704389585,
122.712471449069)) ;
#74509 = CARTESIAN_POINT('Ctrl Pts',(-18.3408506079003,-24.5325813585398,
122.852345913931)) ;
#74510 = CARTESIAN_POINT('Ctrl Pts',(-17.9721440403663,-24.7226415564883,
122.956790585532)) ;
#74511 = CARTESIAN_POINT('Ctrl Pts',(-18.2595668744231,-24.5426524760696,
123.047801904658)) ;
#74512 = CARTESIAN_POINT('Ctrl Pts',(-17.9156039986773,-24.7324572504544,
123.20851484051)) ;
#74513 = CARTESIAN_POINT('Ctrl Pts',(-18.214336048054,-24.5524681700357,123.249180320883)) ;
#74514 = CARTESIAN_POINT('Ctrl Pts',(-17.9029486724809,-24.7425236279517,
123.472689210433)) ;
#74515 = CARTESIAN_POINT('Ctrl Pts',(-18.2042126493569,-24.562534547533,123.460520152789)) ;
#74516 = CARTESIAN_POINT('Ctrl Pts',(-17.9358920954066,-24.7524226140335,
123.730795685737)) ;
#74517 = CARTESIAN_POINT('Ctrl Pts',(-18.2305681821553,-24.5724335336148,
123.667004510187)) ;
#74518 = CARTESIAN_POINT('Ctrl Pts',(-18.0142279453785,-24.7624767940271,
123.983068491414)) ;
#74519 = CARTESIAN_POINT('Ctrl Pts',(-18.2932377609771,-24.5824877136083,
123.868822703197)) ;
#74520 = CARTESIAN_POINT('Ctrl Pts',(-18.1327982652651,-24.7723476069598,
124.213846997065)) ;
#74521 = CARTESIAN_POINT('Ctrl Pts',(-18.3880943171351,-24.592358526541,124.053444317472)) ;
#74522 = CARTESIAN_POINT('Ctrl Pts',(-18.2927953165184,-24.7824215078136,
124.42468023211)) ;
#74523 = CARTESIAN_POINT('Ctrl Pts',(-18.5160928152564,-24.6024324273948,
124.222110690457)) ;
#74524 = CARTESIAN_POINT('Ctrl Pts',(-18.4819523062245,-24.7922416632002,
124.600316090987)) ;
#74525 = CARTESIAN_POINT('Ctrl Pts',(-18.6674179941489,-24.6122525827815,
124.36261799151)) ;
#74526 = CARTESIAN_POINT('Ctrl Pts',(-18.7041959808915,-24.8023203701525,
124.744270009399)) ;
#74527 = CARTESIAN_POINT('Ctrl Pts',(-18.8452136184264,-24.6223312897337,
124.477780764093)) ;
#74528 = CARTESIAN_POINT('Ctrl Pts',(-18.9426453969899,-24.8121719586913,
124.845254460317)) ;
#74529 = CARTESIAN_POINT('Ctrl Pts',(-19.0359724337194,-24.6321828782725,
124.558567311492)) ;
#74530 = CARTESIAN_POINT('Ctrl Pts',(-19.200521069124,-24.8222450752162,124.904809172644)) ;
#74531 = CARTESIAN_POINT('Ctrl Pts',(-19.2422734477073,-24.6422559947975,
124.606210577257)) ;
#74532 = CARTESIAN_POINT('Ctrl Pts',(-19.4588424041195,-24.8320875923121,
124.918328324864)) ;
#74533 = CARTESIAN_POINT('Ctrl Pts',(-19.4489294152064,-24.6520985118933,
124.617025231616)) ;
#74534 = CARTESIAN_POINT('Ctrl Pts',(-19.719255391812,-24.8420680538661,124.887225976223)) ;
#74535 = CARTESIAN_POINT('Ctrl Pts',(-19.6572595128658,-24.6620789734473,
124.592142995155)) ;
#74536 = CARTESIAN_POINT('Ctrl Pts',(-19.9711242826378,-24.8520863038568,
124.810604842159)) ;
#74537 = CARTESIAN_POINT('Ctrl Pts',(-19.8587544824804,-24.6720972234381,
124.530845590783)) ;
#74538 = CARTESIAN_POINT('Ctrl Pts',(-20.2029896411128,-24.8619704640506,
124.693474375269)) ;
#74539 = CARTESIAN_POINT('Ctrl Pts',(-20.0442458164623,-24.6819813836318,
124.437141271385)) ;
#74540 = CARTESIAN_POINT('Ctrl Pts',(-20.4147243951866,-24.8720356110256,
124.535001991893)) ;
#74541 = CARTESIAN_POINT('Ctrl Pts',(-20.2136336325646,-24.6920465306068,
124.310362857701)) ;
#74542 = CARTESIAN_POINT('Ctrl Pts',(-20.5918496187406,-24.8818774346664,
124.346514930606)) ;
#74543 = CARTESIAN_POINT('Ctrl Pts',(-20.3553327465534,-24.7018883542476,
124.159573817455)) ;
#74544 = CARTESIAN_POINT('Ctrl Pts',(-20.7368372685896,-24.8919069071272,
124.126420308685)) ;
#74545 = CARTESIAN_POINT('Ctrl Pts',(-20.4713227600886,-24.7119178267085,
123.983497953276)) ;
#74546 = CARTESIAN_POINT('Ctrl Pts',(-20.8407071585542,-24.9019337623892,
123.884255456022)) ;
#74547 = CARTESIAN_POINT('Ctrl Pts',(-20.5544183607699,-24.7219446819705,
123.789765854984)) ;
#74548 = CARTESIAN_POINT('Ctrl Pts',(-20.9004509563843,-24.9117770124998,
123.632574419161)) ;
#74549 = CARTESIAN_POINT('Ctrl Pts',(-20.6022129291242,-24.731787932081,123.588422099066)) ;
#74550 = CARTESIAN_POINT('Ctrl Pts',(-20.9162606113356,-24.9218254520829,
123.368993380641)) ;
#74551 = CARTESIAN_POINT('Ctrl Pts',(-20.614860543706,-24.7418363716642,123.377557052921)) ;
#74552 = CARTESIAN_POINT('Ctrl Pts',(-20.8859488524608,-24.9317749463308,
123.10929263775)) ;
#74553 = CARTESIAN_POINT('Ctrl Pts',(-20.59061096289,-24.7517858659121,123.169796946132)) ;
#74554 = CARTESIAN_POINT('Ctrl Pts',(-20.8120633746021,-24.9416828020568,
122.859612422506)) ;
#74555 = CARTESIAN_POINT('Ctrl Pts',(-20.531502761985,-24.7616937216381,122.970053477872)) ;
#74556 = CARTESIAN_POINT('Ctrl Pts',(-20.6939388265483,-24.9517422787068,
122.623150935592)) ;
#74557 = CARTESIAN_POINT('Ctrl Pts',(-20.4370029110324,-24.771753198288,122.7808840852)) ;
#74558 = CARTESIAN_POINT('Ctrl Pts',(-20.540217779766,-24.9615830881155,122.415150839265)) ;
#74559 = CARTESIAN_POINT('Ctrl Pts',(-20.3140267650596,-24.7815940076967,
122.614484958291)) ;
#74560 = CARTESIAN_POINT('Ctrl Pts',(-20.3487716521586,-24.9716452384163,
122.232796879452)) ;
#74561 = CARTESIAN_POINT('Ctrl Pts',(-20.1608697005257,-24.7916561579975,
122.46860153275)) ;
#74562 = CARTESIAN_POINT('Ctrl Pts',(-20.1319979379297,-24.9815423995388,
122.089055106635)) ;
#74563 = CARTESIAN_POINT('Ctrl Pts',(-19.9874513995793,-24.8015533191201,
122.353608554069)) ;
#74564 = CARTESIAN_POINT('Ctrl Pts',(-19.8931048762983,-24.9914735739429,
121.98399178358)) ;
#74565 = CARTESIAN_POINT('Ctrl Pts',(-19.7963375692776,-24.8114844935241,
122.269557920393)) ;
#74566 = CARTESIAN_POINT('Ctrl Pts',(-19.6366938542518,-25.0015157776679,
121.921591372293)) ;
#74567 = CARTESIAN_POINT('Ctrl Pts',(-19.5912086257086,-24.8215266972492,
122.219637404033)) ;
#74568 = CARTESIAN_POINT('Ctrl Pts',(-19.3774193320299,-25.0114023600983,
121.904731667658)) ;
#74569 = CARTESIAN_POINT('Ctrl Pts',(-19.3837898885551,-24.8314132796796,
122.206149496955)) ;
#74570 = CARTESIAN_POINT('Ctrl Pts',(-19.1163451180578,-25.0213957958467,
121.933019785977)) ;
#74571 = CARTESIAN_POINT('Ctrl Pts',(-19.1749306450464,-24.8414067154279,
122.228779665525)) ;
#74572 = CARTESIAN_POINT('Ctrl Pts',(-18.8653899853396,-25.0313402642048,
122.005933155613)) ;
#74573 = CARTESIAN_POINT('Ctrl Pts',(-18.9741669200582,-24.8513511837861,
122.287109951159)) ;
#74574 = CARTESIAN_POINT('Ctrl Pts',(-18.630508190403,-25.0412920804504,122.120959221041)) ;
#74575 = CARTESIAN_POINT('Ctrl Pts',(-18.7862616983895,-24.8613030000317,
122.379130236719)) ;
#74576 = CARTESIAN_POINT('Ctrl Pts',(-18.417510698376,-25.0513295165649,122.276526693795)) ;
#74577 = CARTESIAN_POINT('Ctrl Pts',(-18.6158633904333,-24.8713404361461,
122.503584006888)) ;
#74578 = CARTESIAN_POINT('Ctrl Pts',(-18.2373294886362,-25.0612144757412,
122.463677159513)) ;
#74579 = CARTESIAN_POINT('Ctrl Pts',(-18.4717187211798,-24.8812253953225,
122.653303473347)) ;
#74580 = CARTESIAN_POINT('Ctrl Pts',(-18.0904935272417,-25.0712125939532,
122.681519130297)) ;
#74581 = CARTESIAN_POINT('Ctrl Pts',(-18.3542496121446,-24.8912235135344,
122.82757667031)) ;
#74582 = CARTESIAN_POINT('Ctrl Pts',(-17.9843474113047,-25.0811335264651,
122.919675638683)) ;
#74583 = CARTESIAN_POINT('Ctrl Pts',(-18.2693324840715,-24.9011444460464,
123.018101090549)) ;
#74584 = CARTESIAN_POINT('Ctrl Pts',(-17.9203421284169,-25.0911748266872,
123.17565728928)) ;
#74585 = CARTESIAN_POINT('Ctrl Pts',(-18.2181276878849,-24.9111857462685,
123.222886415152)) ;
#74586 = CARTESIAN_POINT('Ctrl Pts',(-17.9020926497319,-25.1010817450772,
123.435363279086)) ;
#74587 = CARTESIAN_POINT('Ctrl Pts',(-18.2035276252548,-24.9210926646584,
123.430650454951)) ;
#74588 = CARTESIAN_POINT('Ctrl Pts',(-17.9285484880393,-25.1110175367862,
123.695123310098)) ;
#74589 = CARTESIAN_POINT('Ctrl Pts',(-18.2246915312731,-24.9310284563675,
123.638458030304)) ;
#74590 = CARTESIAN_POINT('Ctrl Pts',(-18.0007127841667,-25.1210584313641,
123.948921149968)) ;
#74591 = CARTESIAN_POINT('Ctrl Pts',(-18.2824223843685,-24.9410693509454,
123.841496622937)) ;
#74592 = CARTESIAN_POINT('Ctrl Pts',(-18.1139247514604,-25.130945633078,124.182800630708)) ;
#74593 = CARTESIAN_POINT('Ctrl Pts',(-18.3729909704001,-24.9509565526592,
124.028599762318)) ;
#74594 = CARTESIAN_POINT('Ctrl Pts',(-18.2672700656085,-25.1409379008396,
124.395937506913)) ;
#74595 = CARTESIAN_POINT('Ctrl Pts',(-18.4956664766225,-24.9609488204208,
124.199109598826)) ;
#74596 = CARTESIAN_POINT('Ctrl Pts',(-18.4545445264255,-25.1508864218614,
124.578379945121)) ;
#74597 = CARTESIAN_POINT('Ctrl Pts',(-18.6454851891911,-24.9708973414426,
124.345063807)) ;
#74598 = CARTESIAN_POINT('Ctrl Pts',(-18.6701593794366,-25.1608231954391,
124.725644505592)) ;
#74599 = CARTESIAN_POINT('Ctrl Pts',(-18.8179761594363,-24.9808341150203,
124.462875886773)) ;
#74600 = CARTESIAN_POINT('Ctrl Pts',(-18.9090898745942,-25.1708062435801,
124.83405904649)) ;
#74601 = CARTESIAN_POINT('Ctrl Pts',(-19.0091199773882,-24.9908171631614,
124.549608297516)) ;
#74602 = CARTESIAN_POINT('Ctrl Pts',(-19.1648198261258,-25.1808499511902,
124.899256681816)) ;
#74603 = CARTESIAN_POINT('Ctrl Pts',(-19.2137038781447,-25.0008608707714,
124.601767252083)) ;
#74604 = CARTESIAN_POINT('Ctrl Pts',(-19.4223677819922,-25.1906786443434,
124.919232914467)) ;
#74605 = CARTESIAN_POINT('Ctrl Pts',(-19.4197410212802,-25.0106895639247,
124.617749120168)) ;
#74606 = CARTESIAN_POINT('Ctrl Pts',(-19.6858526790718,-25.2007533934729,
124.893750955918)) ;
#74607 = CARTESIAN_POINT('Ctrl Pts',(-19.6305293633067,-25.0207643130542,
124.59736453674)) ;
#74608 = CARTESIAN_POINT('Ctrl Pts',(-19.9356579462485,-25.2106187192684,
124.824304856652)) ;
#74609 = CARTESIAN_POINT('Ctrl Pts',(-19.8303729649698,-25.0306296388497,
124.541808869368)) ;
#74610 = CARTESIAN_POINT('Ctrl Pts',(-20.1735854693504,-25.2206408936254,
124.711387601667)) ;
#74611 = CARTESIAN_POINT('Ctrl Pts',(-20.0207155100975,-25.0406518132067,
124.451476093775)) ;
#74612 = CARTESIAN_POINT('Ctrl Pts',(-20.388022656134,-25.2306669468323,124.558270853455)) ;
#74613 = CARTESIAN_POINT('Ctrl Pts',(-20.1922658914238,-25.0506778664136,
124.328983483751)) ;
#74614 = CARTESIAN_POINT('Ctrl Pts',(-20.5697163879502,-25.2405206436786,
124.373799671738)) ;
#74615 = CARTESIAN_POINT('Ctrl Pts',(-20.3376209782561,-25.0605315632599,
124.181408007588)) ;
#74616 = CARTESIAN_POINT('Ctrl Pts',(-20.7188606914662,-25.2504800484316,
124.158719634567)) ;
#74617 = CARTESIAN_POINT('Ctrl Pts',(-20.4569372775264,-25.0704909680128,
124.009344986073)) ;
#74618 = CARTESIAN_POINT('Ctrl Pts',(-20.8288249196023,-25.2605182941365,
123.918954163192)) ;
#74619 = CARTESIAN_POINT('Ctrl Pts',(-20.5449097751489,-25.0805292137177,
123.817532999354)) ;
#74620 = CARTESIAN_POINT('Ctrl Pts',(-20.8948612314061,-25.2703924782985,
123.667978712692)) ;
#74621 = CARTESIAN_POINT('Ctrl Pts',(-20.5977398529196,-25.0904033978798,
123.616753747338)) ;
#74622 = CARTESIAN_POINT('Ctrl Pts',(-20.9167246662131,-25.2804622614364,
123.404296836379)) ;
#74623 = CARTESIAN_POINT('Ctrl Pts',(-20.6152318948764,-25.1004731810177,
123.405808073507)) ;
#74624 = CARTESIAN_POINT('Ctrl Pts',(-20.8931748951374,-25.2902955164572,
123.146942101515)) ;
#74625 = CARTESIAN_POINT('Ctrl Pts',(-20.5963934691841,-25.1103064360384,
123.199925185877)) ;
#74626 = CARTESIAN_POINT('Ctrl Pts',(-20.8246646035839,-25.3003259425889,
122.892421113389)) ;
#74627 = CARTESIAN_POINT('Ctrl Pts',(-20.5415866267975,-25.1203368621701,
122.996307948949)) ;
#74628 = CARTESIAN_POINT('Ctrl Pts',(-20.7122848539865,-25.3103575547759,
122.653938383756)) ;
#74629 = CARTESIAN_POINT('Ctrl Pts',(-20.4516839742709,-25.1303684743571,
122.805521151809)) ;
#74630 = CARTESIAN_POINT('Ctrl Pts',(-20.5637225648763,-25.3201872516305,
122.442640422415)) ;
#74631 = CARTESIAN_POINT('Ctrl Pts',(-20.3328358819854,-25.1401981712117,
122.636482800151)) ;
#74632 = CARTESIAN_POINT('Ctrl Pts',(-20.3782914259856,-25.330176693533,122.256812973028)) ;
#74633 = CARTESIAN_POINT('Ctrl Pts',(-20.1844921808869,-25.1501876131142,
122.487819833207)) ;
#74634 = CARTESIAN_POINT('Ctrl Pts',(-20.1618642262866,-25.3402205855486,
122.105737144938)) ;
#74635 = CARTESIAN_POINT('Ctrl Pts',(-20.0113511467643,-25.1602315051299,
122.366957925949)) ;
#74636 = CARTESIAN_POINT('Ctrl Pts',(-19.9280150892586,-25.3500421473179,
121.996514020468)) ;
#74637 = CARTESIAN_POINT('Ctrl Pts',(-19.8242733908789,-25.1700530668991,
122.279578452109)) ;
#74638 = CARTESIAN_POINT('Ctrl Pts',(-19.6734892887017,-25.3600777189421,
121.927457195614)) ;
#74639 = CARTESIAN_POINT('Ctrl Pts',(-19.6206531100156,-25.1800886385233,
122.224331363423)) ;
#74640 = CARTESIAN_POINT('Ctrl Pts',(-19.4109364974855,-25.3701069932239,
121.904446478654)) ;
#74641 = CARTESIAN_POINT('Ctrl Pts',(-19.410610970347,-25.1901179128051,122.205921274802)) ;
#74642 = CARTESIAN_POINT('Ctrl Pts',(-19.1534256983001,-25.3799408303425,
121.926236678618)) ;
#74643 = CARTESIAN_POINT('Ctrl Pts',(-19.2046030736676,-25.1999517499238,
122.223351721254)) ;
#74644 = CARTESIAN_POINT('Ctrl Pts',(-18.8979973838584,-25.3899932264307,
121.993564432332)) ;
#74645 = CARTESIAN_POINT('Ctrl Pts',(-19.0002598327071,-25.2100041460119,
122.277212317537)) ;
#74646 = CARTESIAN_POINT('Ctrl Pts',(-18.6610161340468,-25.3999299933812,
122.103265136515)) ;
#74647 = CARTESIAN_POINT('Ctrl Pts',(-18.8106744978957,-25.2199409129625,
122.364971228474)) ;
#74648 = CARTESIAN_POINT('Ctrl Pts',(-18.4463642083807,-25.4098642283605,
122.251846102336)) ;
#74649 = CARTESIAN_POINT('Ctrl Pts',(-18.6389522789307,-25.2298751479417,
122.483834331329)) ;
#74650 = CARTESIAN_POINT('Ctrl Pts',(-18.2592125480837,-25.4198879916873,
122.437210228651)) ;
#74651 = CARTESIAN_POINT('Ctrl Pts',(-18.4892297234926,-25.2398989112685,
122.632124410148)) ;
#74652 = CARTESIAN_POINT('Ctrl Pts',(-18.1090179640619,-25.4297743330719,
122.649196677349)) ;
#74653 = CARTESIAN_POINT('Ctrl Pts',(-18.3690729553001,-25.2497852526532,
122.801712072819)) ;
#74654 = CARTESIAN_POINT('Ctrl Pts',(-17.9962023975987,-25.4397633818389,
122.88622883429)) ;
#74655 = CARTESIAN_POINT('Ctrl Pts',(-18.2788188754758,-25.2597743014202,
122.991336884264)) ;
#74656 = CARTESIAN_POINT('Ctrl Pts',(-17.926423247948,-25.4498046025363,123.140706746053)) ;
#74657 = CARTESIAN_POINT('Ctrl Pts',(-18.2229938254166,-25.2698155221175,
123.194918814878)) ;
#74658 = CARTESIAN_POINT('Ctrl Pts',(-17.9019779829779,-25.4596372427142,
123.397935296117)) ;
#74659 = CARTESIAN_POINT('Ctrl Pts',(-18.2034358520446,-25.2796481622954,
123.400700720434)) ;
#74660 = CARTESIAN_POINT('Ctrl Pts',(-17.9221548129474,-25.4696311720221,
123.659787613419)) ;
#74661 = CARTESIAN_POINT('Ctrl Pts',(-18.2195753605606,-25.2896420916034,
123.610182627543)) ;
#74662 = CARTESIAN_POINT('Ctrl Pts',(-17.9882634626665,-25.4796603797027,
123.914920831984)) ;
#74663 = CARTESIAN_POINT('Ctrl Pts',(-18.2724604733462,-25.2996712992839,
123.814289688043)) ;
#74664 = CARTESIAN_POINT('Ctrl Pts',(-18.0956149027315,-25.4895361914068,
124.151219574851)) ;
#74665 = CARTESIAN_POINT('Ctrl Pts',(-18.3583396441264,-25.309547110988,124.003328991269)) ;
#74666 = CARTESIAN_POINT('Ctrl Pts',(-18.2439323543506,-25.4995354183782,
124.368086107254)) ;
#74667 = CARTESIAN_POINT('Ctrl Pts',(-18.4769919264261,-25.3195463379594,
124.176823257669)) ;
#74668 = CARTESIAN_POINT('Ctrl Pts',(-18.4258762774548,-25.5094448995339,
124.554446462842)) ;
#74669 = CARTESIAN_POINT('Ctrl Pts',(-18.6225453691918,-25.3294558191151,
124.325912669467)) ;
#74670 = CARTESIAN_POINT('Ctrl Pts',(-18.640448928703,-25.5194981298348,124.708521880039)) ;
#74671 = CARTESIAN_POINT('Ctrl Pts',(-18.7942023889779,-25.339509049416,124.449174675351)) ;
#74672 = CARTESIAN_POINT('Ctrl Pts',(-18.8741769469214,-25.5293687463858,
124.821053391343)) ;
#74673 = CARTESIAN_POINT('Ctrl Pts',(-18.981183490012,-25.3493796659671,124.539201487123)) ;
#74674 = CARTESIAN_POINT('Ctrl Pts',(-19.1275355267195,-25.5393904081179,
124.89292358676)) ;
#74675 = CARTESIAN_POINT('Ctrl Pts',(-19.1838697832088,-25.3594013276991,
124.596699645032)) ;
#74676 = CARTESIAN_POINT('Ctrl Pts',(-19.3896325300269,-25.549413221299,124.919115026296)) ;
#74677 = CARTESIAN_POINT('Ctrl Pts',(-19.3935471728134,-25.3694241408802,
124.617654797419)) ;
#74678 = CARTESIAN_POINT('Ctrl Pts',(-19.6482244565254,-25.5592803857589,
124.900141299452)) ;
#74679 = CARTESIAN_POINT('Ctrl Pts',(-19.6004204014471,-25.3792913053402,
124.602477906034)) ;
#74680 = CARTESIAN_POINT('Ctrl Pts',(-19.9029765855987,-25.5692738279788,
124.836321404658)) ;
#74681 = CARTESIAN_POINT('Ctrl Pts',(-19.8042225357259,-25.3892847475601,
124.551424072953)) ;
#74682 = CARTESIAN_POINT('Ctrl Pts',(-20.143477500317,-25.5793055015792,124.728362358355)) ;
#74683 = CARTESIAN_POINT('Ctrl Pts',(-19.9966241166619,-25.3993164211604,
124.465058726285)) ;
#74684 = CARTESIAN_POINT('Ctrl Pts',(-20.3582214202601,-25.5891719366922,
124.583046155719)) ;
#74685 = CARTESIAN_POINT('Ctrl Pts',(-20.1684200947875,-25.4091828562734,
124.348807744366)) ;
#74686 = CARTESIAN_POINT('Ctrl Pts',(-20.5470220993923,-25.5991593872253,
124.400775187898)) ;
#74687 = CARTESIAN_POINT('Ctrl Pts',(-20.3194620631275,-25.4191703068065,
124.202992587349)) ;
#74688 = CARTESIAN_POINT('Ctrl Pts',(-20.7008042110465,-25.6091043170532,
124.189419968469)) ;
#74689 = CARTESIAN_POINT('Ctrl Pts',(-20.4424893892085,-25.4291152366345,
124.033909833955)) ;
#74690 = CARTESIAN_POINT('Ctrl Pts',(-20.8165443609965,-25.6191492121083,
123.95220482888)) ;
#74691 = CARTESIAN_POINT('Ctrl Pts',(-20.535083449004,-25.4391601316896,123.844138651969)) ;
#74692 = CARTESIAN_POINT('Ctrl Pts',(-20.8882445302655,-25.6290112737942,
123.703135751158)) ;
#74693 = CARTESIAN_POINT('Ctrl Pts',(-20.5924455729224,-25.4490221933754,
123.644884316791)) ;
#74694 = CARTESIAN_POINT('Ctrl Pts',(-20.916487089586,-25.639002996581,123.442107956853)) ;
#74695 = CARTESIAN_POINT('Ctrl Pts',(-20.6150418055074,-25.4590139161623,
123.436062394398)) ;
#74696 = CARTESIAN_POINT('Ctrl Pts',(-20.8989852871398,-25.648935210821,123.181683998681)) ;
#74697 = CARTESIAN_POINT('Ctrl Pts',(-20.6010425682798,-25.4689461304023,
123.227723257091)) ;
#74698 = CARTESIAN_POINT('Ctrl Pts',(-20.8370703424322,-25.6588745293867,
122.927926047639)) ;
#74699 = CARTESIAN_POINT('Ctrl Pts',(-20.5515128122733,-25.478885448968,123.024716500619)) ;
#74700 = CARTESIAN_POINT('Ctrl Pts',(-20.7307098427512,-25.6689187041626,
122.686357803577)) ;
#74701 = CARTESIAN_POINT('Ctrl Pts',(-20.4664264490109,-25.4889296237439,
122.831461026835)) ;
#74702 = CARTESIAN_POINT('Ctrl Pts',(-20.5866715410946,-25.6787892582276,
122.470638672561)) ;
#74703 = CARTESIAN_POINT('Ctrl Pts',(-20.351197775471,-25.4988001778088,122.658884659411)) ;
#74704 = CARTESIAN_POINT('Ctrl Pts',(-20.4061979029377,-25.6887542405818,
122.280888722107)) ;
#74705 = CARTESIAN_POINT('Ctrl Pts',(-20.2068205491805,-25.508765160163,122.507083201106)) ;
#74706 = CARTESIAN_POINT('Ctrl Pts',(-20.1938959519835,-25.6987849434716,
122.124661424596)) ;
#74707 = CARTESIAN_POINT('Ctrl Pts',(-20.0369803529524,-25.5187958630528,
122.382099587623)) ;
#74708 = CARTESIAN_POINT('Ctrl Pts',(-19.9610841220757,-25.7086772834968,
122.008927766467)) ;
#74709 = CARTESIAN_POINT('Ctrl Pts',(-19.8507319966017,-25.528688203078,122.289510701505)) ;
#74710 = CARTESIAN_POINT('Ctrl Pts',(-19.7077317559473,-25.7187305166567,
121.934171888527)) ;
#74711 = CARTESIAN_POINT('Ctrl Pts',(-19.6480507770561,-25.538741436238,122.229703850899)) ;
#74712 = CARTESIAN_POINT('Ctrl Pts',(-19.4496748815456,-25.7286117611335,
121.90488225927)) ;
#74713 = CARTESIAN_POINT('Ctrl Pts',(-19.4416056279945,-25.5486226807147,
122.206269922949)) ;
#74714 = CARTESIAN_POINT('Ctrl Pts',(-19.1865495494693,-25.7386448820045,
121.920889891574)) ;
#74715 = CARTESIAN_POINT('Ctrl Pts',(-19.2311052788292,-25.5586558015858,
122.219073772921)) ;
#74716 = CARTESIAN_POINT('Ctrl Pts',(-18.9339340957585,-25.7485260922796,
121.981208014926)) ;
#74717 = CARTESIAN_POINT('Ctrl Pts',(-19.029012442334,-25.5685370118608,122.26732607008)) ;
#74718 = CARTESIAN_POINT('Ctrl Pts',(-18.6913224502275,-25.7585881680489,
122.086259918681)) ;
#74719 = CARTESIAN_POINT('Ctrl Pts',(-18.8349222926242,-25.5785990876302,
122.351365495269)) ;
#74720 = CARTESIAN_POINT('Ctrl Pts',(-18.4750177695865,-25.7684452264307,
122.228841554616)) ;
#74721 = CARTESIAN_POINT('Ctrl Pts',(-18.6618773148377,-25.5884561460119,
122.465428920654)) ;
#74722 = CARTESIAN_POINT('Ctrl Pts',(-18.2838238476574,-25.7784397817196,
122.408857735646)) ;
#74723 = CARTESIAN_POINT('Ctrl Pts',(-18.5089206655225,-25.5984507013009,
122.60944020259)) ;
#74724 = CARTESIAN_POINT('Ctrl Pts',(-18.1277492565297,-25.7883656692552,
122.61789787757)) ;
#74725 = CARTESIAN_POINT('Ctrl Pts',(-18.3840591928632,-25.6083765888364,
122.77667098702)) ;
#74726 = CARTESIAN_POINT('Ctrl Pts',(-18.0091260993102,-25.7983906892504,
122.8531052283)) ;
#74727 = CARTESIAN_POINT('Ctrl Pts',(-18.2891587030672,-25.6184016088317,
122.964835791046)) ;
#74728 = CARTESIAN_POINT('Ctrl Pts',(-17.9340157761672,-25.8082880663541,
123.102124235162)) ;
#74729 = CARTESIAN_POINT('Ctrl Pts',(-18.2290682857916,-25.6282989859354,
123.164050416227)) ;
#74730 = CARTESIAN_POINT('Ctrl Pts',(-17.9024264991697,-25.818278303435,123.362756958183)) ;
#74731 = CARTESIAN_POINT('Ctrl Pts',(-18.2037946795891,-25.6382892230162,
123.372556307197)) ;
#74732 = CARTESIAN_POINT('Ctrl Pts',(-17.9171433201886,-25.8283149162438,
123.626094022944)) ;
#74733 = CARTESIAN_POINT('Ctrl Pts',(-18.2155658929526,-25.648325835825,123.583225962692)) ;
#74734 = CARTESIAN_POINT('Ctrl Pts',(-17.9758333008646,-25.8381647996618,
123.878206838387)) ;
#74735 = CARTESIAN_POINT('Ctrl Pts',(-18.2625157992265,-25.658175719243,123.784916942111)) ;
#74736 = CARTESIAN_POINT('Ctrl Pts',(-18.0784917994839,-25.8481684165642,
124.120189945123)) ;
#74737 = CARTESIAN_POINT('Ctrl Pts',(-18.3446404819217,-25.6681793361455,
123.978504135792)) ;
#74738 = CARTESIAN_POINT('Ctrl Pts',(-18.2215613396914,-25.8581578283294,
124.340338256961)) ;
#74739 = CARTESIAN_POINT('Ctrl Pts',(-18.4590946437798,-25.6781687479106,
124.154624345632)) ;
#74740 = CARTESIAN_POINT('Ctrl Pts',(-18.4012825634563,-25.8681765896742,
124.532704279354)) ;
#74741 = CARTESIAN_POINT('Ctrl Pts',(-18.6028685580281,-25.6881875092555,
124.308517112761)) ;
#74742 = CARTESIAN_POINT('Ctrl Pts',(-18.6786331146078,-25.8813952650552,
124.741942400083)) ;
#74743 = CARTESIAN_POINT('Ctrl Pts',(-18.8247543705837,-25.7014061846365,
124.475917413394)) ;
#74744 = CARTESIAN_POINT('Ctrl Pts',(-19.0063037436374,-25.8947055723,124.87503799074)) ;
#74745 = CARTESIAN_POINT('Ctrl Pts',(-19.0869232033359,-25.7147164918812,
124.582399636663)) ;
#74746 = CARTESIAN_POINT('Ctrl Pts',(-19.3515492792996,-25.907943238526,124.918059062517)) ;
#74747 = CARTESIAN_POINT('Ctrl Pts',(-19.3630728386149,-25.7279541581072,
124.616808324183)) ;
#74748 = CARTESIAN_POINT('Ctrl Pts',(-19.6119358669672,-25.9178629339367,
124.905712873571)) ;
#74749 = CARTESIAN_POINT('Ctrl Pts',(-19.5713918638856,-25.7378738535179,
124.606935541768)) ;
#74750 = CARTESIAN_POINT('Ctrl Pts',(-19.8695568707242,-25.9279158009352,
124.847282646944)) ;
#74751 = CARTESIAN_POINT('Ctrl Pts',(-19.7774862246626,-25.7479267205165,
124.560193132552)) ;
#74752 = CARTESIAN_POINT('Ctrl Pts',(-20.1084811471068,-25.9377712092645,
124.747272818654)) ;
#74753 = CARTESIAN_POINT('Ctrl Pts',(-19.9686281873536,-25.7577821288458,
124.480186034087)) ;
#74754 = CARTESIAN_POINT('Ctrl Pts',(-20.3306652048193,-25.9478098409411,
124.605081165744)) ;
#74755 = CARTESIAN_POINT('Ctrl Pts',(-20.1463738336963,-25.7678207605223,
124.366438470224)) ;
#74756 = CARTESIAN_POINT('Ctrl Pts',(-20.5876341489434,-25.9611120232081,
124.368071353077)) ;
#74757 = CARTESIAN_POINT('Ctrl Pts',(-20.3519625615486,-25.7811229427894,
124.176812457001)) ;
#74758 = CARTESIAN_POINT('Ctrl Pts',(-20.8234715239906,-25.977657036291,123.996893725418)) ;
#74759 = CARTESIAN_POINT('Ctrl Pts',(-20.5406208335467,-25.7976679558722,
123.87990862136)) ;
#74760 = CARTESIAN_POINT('Ctrl Pts',(-20.9191905980385,-25.9943090523672,
123.56485434144)) ;
#74761 = CARTESIAN_POINT('Ctrl Pts',(-20.6172087980807,-25.8143199719484,
123.534214776845)) ;
#74762 = CARTESIAN_POINT('Ctrl Pts',(-20.9040855807163,-26.0075321432724,
123.217655815584)) ;
#74763 = CARTESIAN_POINT('Ctrl Pts',(-20.6051216995438,-25.8275430628537,
123.256506511511)) ;
#74764 = CARTESIAN_POINT('Ctrl Pts',(-20.8481710289806,-26.0174931028318,
122.9619384918)) ;
#74765 = CARTESIAN_POINT('Ctrl Pts',(-20.5603924152172,-25.837504022413,123.051921427646)) ;
#74766 = CARTESIAN_POINT('Ctrl Pts',(-20.7477672744472,-26.0275178995829,
122.718386742836)) ;
#74767 = CARTESIAN_POINT('Ctrl Pts',(-20.4800725252395,-25.8475288191641,
122.857083778402)) ;
#74768 = CARTESIAN_POINT('Ctrl Pts',(-20.5619333818836,-26.0407423469787,
122.42467916469)) ;
#74769 = CARTESIAN_POINT('Ctrl Pts',(-20.3313987756676,-25.8607532665599,
122.622107468328)) ;
#74770 = CARTESIAN_POINT('Ctrl Pts',(-20.2373134507114,-26.0573761316778,
122.124643357332)) ;
#74771 = CARTESIAN_POINT('Ctrl Pts',(-20.0717139940136,-25.877387051259,122.382085646915)) ;
#74772 = CARTESIAN_POINT('Ctrl Pts',(-19.7495611854101,-26.0772787984027,
121.919792632178)) ;
#74773 = CARTESIAN_POINT('Ctrl Pts',(-19.6815098776299,-25.897289717984,122.218198920366)) ;
#74774 = CARTESIAN_POINT('Ctrl Pts',(-19.2213622812283,-26.0971790261846,
121.89299185719)) ;
#74775 = CARTESIAN_POINT('Ctrl Pts',(-19.2589510054893,-25.9171899457658,
122.196756056214)) ;
#74776 = CARTESIAN_POINT('Ctrl Pts',(-18.7151476741329,-26.1170965137161,
122.047840068811)) ;
#74777 = CARTESIAN_POINT('Ctrl Pts',(-18.8539776981445,-25.9371074332973,
122.320631958508)) ;
#74778 = CARTESIAN_POINT('Ctrl Pts',(-18.2916834898389,-26.137026039533,122.366086543257)) ;
#74779 = CARTESIAN_POINT('Ctrl Pts',(-18.5152044325254,-25.9570369591142,
122.575227523537)) ;
#74780 = CARTESIAN_POINT('Ctrl Pts',(-18.0018457090741,-26.1569883074192,
122.810521280974)) ;
#74781 = CARTESIAN_POINT('Ctrl Pts',(-18.283332009678,-25.9769992270005,122.930774214087)) ;
#74782 = CARTESIAN_POINT('Ctrl Pts',(-17.8814876927673,-26.1768785023714,
123.325213587116)) ;
#74783 = CARTESIAN_POINT('Ctrl Pts',(-18.1870431423497,-25.9968894219527,
123.342528513262)) ;
#74784 = CARTESIAN_POINT('Ctrl Pts',(-17.9426863607119,-26.1967687471177,
123.850425839063)) ;
#74785 = CARTESIAN_POINT('Ctrl Pts',(-18.2360005788665,-26.016779666699,123.762699536368)) ;
#74786 = CARTESIAN_POINT('Ctrl Pts',(-18.1825328725628,-26.2168431196802,
124.326942241142)) ;
#74787 = CARTESIAN_POINT('Ctrl Pts',(-18.4278757324527,-26.0368540392614,
124.143912810045)) ;
#74788 = CARTESIAN_POINT('Ctrl Pts',(-18.5649877789948,-26.2366284970405,
124.687956672243)) ;
#74789 = CARTESIAN_POINT('Ctrl Pts',(-18.7338401401723,-26.0566394166217,
124.432727122548)) ;
#74790 = CARTESIAN_POINT('Ctrl Pts',(-19.0512197803055,-26.2565903711076,
124.900124064246)) ;
#74791 = CARTESIAN_POINT('Ctrl Pts',(-19.1228258509435,-26.0766012906889,
124.602461970491)) ;
#74792 = CARTESIAN_POINT('Ctrl Pts',(-19.5812880978493,-26.2765703465981,
124.932395779839)) ;
#74793 = CARTESIAN_POINT('Ctrl Pts',(-19.5468805975335,-26.0965812661794,
124.628280541388)) ;
#74794 = CARTESIAN_POINT('Ctrl Pts',(-20.0865875254808,-26.296382776476,124.784090581371)) ;
#74795 = CARTESIAN_POINT('Ctrl Pts',(-19.9511225306785,-26.1163936960573,
124.50963622777)) ;
#74796 = CARTESIAN_POINT('Ctrl Pts',(-20.5148410357774,-26.3163628845663,
124.470248873514)) ;
#74797 = CARTESIAN_POINT('Ctrl Pts',(-20.2937255891069,-26.1363738041476,
124.258562667596)) ;
#74798 = CARTESIAN_POINT('Ctrl Pts',(-20.8089496481793,-26.3362572681636,
124.030690459084)) ;
#74799 = CARTESIAN_POINT('Ctrl Pts',(-20.5290131148898,-26.1562681877448,
123.906914797705)) ;
#74800 = CARTESIAN_POINT('Ctrl Pts',(-20.9360216456887,-26.3561841961408,
123.516657893159)) ;
#74801 = CARTESIAN_POINT('Ctrl Pts',(-20.6306703947907,-26.1761951157221,
123.495687702575)) ;
#74802 = CARTESIAN_POINT('Ctrl Pts',(-20.8808211229256,-26.376079053442,122.990653192989)) ;
#74803 = CARTESIAN_POINT('Ctrl Pts',(-20.5865088182755,-26.1960899730233,
123.074882896028)) ;
#74804 = CARTESIAN_POINT('Ctrl Pts',(-20.6473502027379,-26.3961182470457,
122.512000068549)) ;
#74805 = CARTESIAN_POINT('Ctrl Pts',(-20.3997313810415,-26.2161291666269,
122.691961220065)) ;
#74806 = CARTESIAN_POINT('Ctrl Pts',(-20.2682064550008,-26.4159582149564,
122.145440895257)) ;
#74807 = CARTESIAN_POINT('Ctrl Pts',(-20.0964143290626,-26.2359691345377,
122.398713470548)) ;
#74808 = CARTESIAN_POINT('Ctrl Pts',(-19.7855675978604,-26.4358730319205,
121.92824336016)) ;
#74809 = CARTESIAN_POINT('Ctrl Pts',(-19.7103017055272,-26.2558839515018,
122.224956789686)) ;
#74810 = CARTESIAN_POINT('Ctrl Pts',(-19.2570238059644,-26.4558152773168,
121.889095738651)) ;
#74811 = CARTESIAN_POINT('Ctrl Pts',(-19.2874659515853,-26.275826196898,122.193640519728)) ;
#74812 = CARTESIAN_POINT('Ctrl Pts',(-18.748249738838,-26.4756873254313,122.031335489846)) ;
#74813 = CARTESIAN_POINT('Ctrl Pts',(-18.8804462675257,-26.2956982450125,
122.307434864793)) ;
#74814 = CARTESIAN_POINT('Ctrl Pts',(-18.3160101802947,-26.4956983903854,
122.340952921537)) ;
#74815 = CARTESIAN_POINT('Ctrl Pts',(-18.5346560494726,-26.3157093099666,
122.555130681776)) ;
#74816 = CARTESIAN_POINT('Ctrl Pts',(-18.0174531568,-26.515509914689,122.774978345827)) ;
#74817 = CARTESIAN_POINT('Ctrl Pts',(-18.2958118673303,-26.3355208342703,
122.902353753564)) ;
#74818 = CARTESIAN_POINT('Ctrl Pts',(-17.8834572829533,-26.5356051266524,
123.291778439983)) ;
#74819 = CARTESIAN_POINT('Ctrl Pts',(-18.188618039186,-26.3556160462336,123.315793821141)) ;
#74820 = CARTESIAN_POINT('Ctrl Pts',(-17.9332038025589,-26.5553858505722,
123.815368387759)) ;
#74821 = CARTESIAN_POINT('Ctrl Pts',(-18.2284182371962,-26.3753967701534,
123.734667085211)) ;
#74822 = CARTESIAN_POINT('Ctrl Pts',(-18.1597535329201,-26.575376926215,124.295760856993)) ;
#74823 = CARTESIAN_POINT('Ctrl Pts',(-18.409661050836,-26.3953878457962,124.118979676145)) ;
#74824 = CARTESIAN_POINT('Ctrl Pts',(-18.5350790244708,-26.595258865258,124.667951356092)) ;
#74825 = CARTESIAN_POINT('Ctrl Pts',(-18.7099242517618,-26.4152697848392,
124.416730225271)) ;
#74826 = CARTESIAN_POINT('Ctrl Pts',(-19.0161267181929,-26.6152114697612,
124.890949085832)) ;
#74827 = CARTESIAN_POINT('Ctrl Pts',(-19.0947641449975,-26.4352223893425,
124.595125248235)) ;
#74828 = CARTESIAN_POINT('Ctrl Pts',(-19.5431138580718,-26.6351103384919,
124.936289536538)) ;
#74829 = CARTESIAN_POINT('Ctrl Pts',(-19.5163546351924,-26.4551212580731,
124.631394176078)) ;
#74830 = CARTESIAN_POINT('Ctrl Pts',(-20.0538241489815,-26.6550037383015,
124.79978424578)) ;
#74831 = CARTESIAN_POINT('Ctrl Pts',(-19.9249224379141,-26.4750146578827,
124.522185551533)) ;
#74832 = CARTESIAN_POINT('Ctrl Pts',(-20.4882718450487,-26.6749128691415,
124.497507103276)) ;
#74833 = CARTESIAN_POINT('Ctrl Pts',(-20.2724781151579,-26.4949237887228,
124.280362392057)) ;
#74834 = CARTESIAN_POINT('Ctrl Pts',(-20.7946862217622,-26.6949449689051,
124.062171882812)) ;
#74835 = CARTESIAN_POINT('Ctrl Pts',(-20.5176077611612,-26.5149558884863,
123.932084425509)) ;
#74836 = CARTESIAN_POINT('Ctrl Pts',(-20.9099487232185,-26.7114770420745,
123.638071483018)) ;
#74837 = CARTESIAN_POINT('Ctrl Pts',(-20.6098098769218,-26.5314879616558,
123.592826514406)) ;
#74838 = CARTESIAN_POINT('Ctrl Pts',(-20.9115489478564,-26.7248123826805,
123.287684923667)) ;
#74839 = CARTESIAN_POINT('Ctrl Pts',(-20.6110911397521,-26.5448233022617,
123.312495827901)) ;
#74840 = CARTESIAN_POINT('Ctrl Pts',(-20.8682561092861,-26.7346549412202,
123.032650001419)) ;
#74841 = CARTESIAN_POINT('Ctrl Pts',(-20.5764556671409,-26.5546658608015,
123.108474233604)) ;
#74842 = CARTESIAN_POINT('Ctrl Pts',(-20.7797708303451,-26.7447068480701,
122.783795004311)) ;
#74843 = CARTESIAN_POINT('Ctrl Pts',(-20.5056588060069,-26.5647177676514,
122.909381558418)) ;
#74844 = CARTESIAN_POINT('Ctrl Pts',(-20.6078481494065,-26.757955362461,122.48098979156)) ;
#74845 = CARTESIAN_POINT('Ctrl Pts',(-20.368152466766,-26.5779662820423,122.667181160605)) ;
#74846 = CARTESIAN_POINT('Ctrl Pts',(-20.2986718810033,-26.7745545374087,
122.166348506582)) ;
#74847 = CARTESIAN_POINT('Ctrl Pts',(-20.120762032831,-26.59456545699,122.415419305003)) ;
#74848 = CARTESIAN_POINT('Ctrl Pts',(-19.9009478345322,-26.7911433232038,
121.976048096969)) ;
#74849 = CARTESIAN_POINT('Ctrl Pts',(-19.8026233502208,-26.6111542427851,
122.263209553901)) ;
#74850 = CARTESIAN_POINT('Ctrl Pts',(-19.5580496300538,-26.8044191395458,
121.911724128116)) ;
#74851 = CARTESIAN_POINT('Ctrl Pts',(-19.5282751818262,-26.624430059127,122.211739560136)) ;
#74852 = CARTESIAN_POINT('Ctrl Pts',(-19.2959531359135,-26.8143929903396,
121.908486612998)) ;
#74853 = CARTESIAN_POINT('Ctrl Pts',(-19.3186038165586,-26.6344039099208,
122.209154538032)) ;
#74854 = CARTESIAN_POINT('Ctrl Pts',(-19.035911538622,-26.824422022432,121.951317775041)) ;
#74855 = CARTESIAN_POINT('Ctrl Pts',(-19.1105694160277,-26.6444329420132,
122.243420903689)) ;
#74856 = CARTESIAN_POINT('Ctrl Pts',(-18.7905877642868,-26.8343121479339,
122.037189061947)) ;
#74857 = CARTESIAN_POINT('Ctrl Pts',(-18.9143114743061,-26.6543230675151,
122.312120264419)) ;
#74858 = CARTESIAN_POINT('Ctrl Pts',(-18.56142280297,-26.8443046262054,122.165337469994)) ;
#74859 = CARTESIAN_POINT('Ctrl Pts',(-18.7309805312086,-26.6643155457866,
122.414640877474)) ;
#74860 = CARTESIAN_POINT('Ctrl Pts',(-18.3586851595701,-26.8542558413028,
122.330580371104)) ;
#74861 = CARTESIAN_POINT('Ctrl Pts',(-18.5687918791563,-26.674266760884,122.546836944886)) ;
#74862 = CARTESIAN_POINT('Ctrl Pts',(-18.1862556412877,-26.8643043430578,
122.53053785774)) ;
#74863 = CARTESIAN_POINT('Ctrl Pts',(-18.4308500085545,-26.6843152626391,
122.706804337278)) ;
#74864 = CARTESIAN_POINT('Ctrl Pts',(-18.0536640723902,-26.8741456926746,
122.752611956665)) ;
#74865 = CARTESIAN_POINT('Ctrl Pts',(-18.3247786705187,-26.6941566122558,
122.884464800855)) ;
#74866 = CARTESIAN_POINT('Ctrl Pts',(-17.9597894558871,-26.8841319836948,
122.997630523687)) ;
#74867 = CARTESIAN_POINT('Ctrl Pts',(-18.2496811140076,-26.7041429032761,
123.080480402911)) ;
#74868 = CARTESIAN_POINT('Ctrl Pts',(-17.9099883260882,-26.8940685954234,
123.254005646123)) ;
#74869 = CARTESIAN_POINT('Ctrl Pts',(-18.2098424357147,-26.7140795150047,
123.285580874397)) ;
#74870 = CARTESIAN_POINT('Ctrl Pts',(-17.9055405281583,-26.904118470791,123.51804154586)) ;
#74871 = CARTESIAN_POINT('Ctrl Pts',(-18.2062864585873,-26.7241293903722,
123.496809585011)) ;
#74872 = CARTESIAN_POINT('Ctrl Pts',(-17.9459982768416,-26.9139689293264,
123.773739288623)) ;
#74873 = CARTESIAN_POINT('Ctrl Pts',(-18.2386548730221,-26.7339798489077,
123.70136733283)) ;
#74874 = CARTESIAN_POINT('Ctrl Pts',(-18.0306120393503,-26.9239408662792,
124.021720774569)) ;
#74875 = CARTESIAN_POINT('Ctrl Pts',(-18.3063479820366,-26.7439517858604,
123.89975170688)) ;
#74876 = CARTESIAN_POINT('Ctrl Pts',(-18.1573679302454,-26.9339363232113,
124.251828560774)) ;
#74877 = CARTESIAN_POINT('Ctrl Pts',(-18.4077546301214,-26.7539472427925,
124.083836797404)) ;
#74878 = CARTESIAN_POINT('Ctrl Pts',(-18.322964634766,-26.9439691302644,124.456964358617)) ;
#74879 = CARTESIAN_POINT('Ctrl Pts',(-18.540233729948,-26.7639800498456,124.24794399399)) ;
#74880 = CARTESIAN_POINT('Ctrl Pts',(-18.518031277806,-26.9538290168543,124.627530239038)) ;
#74881 = CARTESIAN_POINT('Ctrl Pts',(-18.6962883826648,-26.7738399364356,
124.384394886845)) ;
#74882 = CARTESIAN_POINT('Ctrl Pts',(-18.7423698226373,-26.9638180974196,
124.763794005541)) ;
#74883 = CARTESIAN_POINT('Ctrl Pts',(-18.8757603004552,-26.7838290170008,
124.493403950581)) ;
#74884 = CARTESIAN_POINT('Ctrl Pts',(-18.9855793301348,-26.9737495766287,
124.858494603995)) ;
#74885 = CARTESIAN_POINT('Ctrl Pts',(-19.07032857135,-26.79376049621,124.569162300801)) ;
#74886 = CARTESIAN_POINT('Ctrl Pts',(-19.2428644372131,-26.9837354360747,
124.910233267547)) ;
#74887 = CARTESIAN_POINT('Ctrl Pts',(-19.2761570014402,-26.8037463556559,
124.610551055388)) ;
#74888 = CARTESIAN_POINT('Ctrl Pts',(-19.5065740592346,-26.9937735867218,
124.91607984277)) ;
#74889 = CARTESIAN_POINT('Ctrl Pts',(-19.4871247473151,-26.8137845063031,
124.615226085904)) ;
#74890 = CARTESIAN_POINT('Ctrl Pts',(-19.7624778086787,-27.0036216772263,
124.877322071488)) ;
#74891 = CARTESIAN_POINT('Ctrl Pts',(-19.691847097787,-26.8236325968075,124.584217745267)) ;
#74892 = CARTESIAN_POINT('Ctrl Pts',(-20.0130872707403,-27.0136825857442,
124.793163184931)) ;
#74893 = CARTESIAN_POINT('Ctrl Pts',(-19.892334005724,-26.8336935053255,124.51688855541)) ;
#74894 = CARTESIAN_POINT('Ctrl Pts',(-20.2414042797423,-27.0235774329022,
124.668672645379)) ;
#74895 = CARTESIAN_POINT('Ctrl Pts',(-20.0749863296734,-26.8435883524835,
124.417294323175)) ;
#74896 = CARTESIAN_POINT('Ctrl Pts',(-20.4459889975372,-27.0335191049473,
124.506241389313)) ;
#74897 = CARTESIAN_POINT('Ctrl Pts',(-20.238652605061,-26.8535300245285,124.287347771796)) ;
#74898 = CARTESIAN_POINT('Ctrl Pts',(-20.620444844537,-27.0435216320727,124.3095765436)) ;
#74899 = CARTESIAN_POINT('Ctrl Pts',(-20.3782156448559,-26.863532551654,124.130014531869)) ;
#74900 = CARTESIAN_POINT('Ctrl Pts',(-20.7581648056357,-27.0535564232602,
124.084711962455)) ;
#74901 = CARTESIAN_POINT('Ctrl Pts',(-20.4883897705064,-26.8735673428414,
123.950121722146)) ;
#74902 = CARTESIAN_POINT('Ctrl Pts',(-20.8533381772439,-27.0634013031193,
123.844121950427)) ;
#74903 = CARTESIAN_POINT('Ctrl Pts',(-20.5645263213738,-26.8834122227005,
123.757649351723)) ;
#74904 = CARTESIAN_POINT('Ctrl Pts',(-20.906507383153,-27.0733871837378,123.587189440389)) ;
#74905 = CARTESIAN_POINT('Ctrl Pts',(-20.6070596196296,-26.893398103319,123.552103047888)) ;
#74906 = CARTESIAN_POINT('Ctrl Pts',(-20.9144081115239,-27.083321906831,123.326185418477)) ;
#74907 = CARTESIAN_POINT('Ctrl Pts',(-20.6133781382632,-26.9033328264122,
123.343300030194)) ;
#74908 = CARTESIAN_POINT('Ctrl Pts',(-20.8761775035436,-27.0933797471422,
123.064696003681)) ;
#74909 = CARTESIAN_POINT('Ctrl Pts',(-20.5827915712378,-26.9133906667234,
123.134108707124)) ;
#74910 = CARTESIAN_POINT('Ctrl Pts',(-20.7954566741114,-27.1032002345387,
122.819537535235)) ;
#74911 = CARTESIAN_POINT('Ctrl Pts',(-20.5182131694661,-26.9232111541199,
122.937983169382)) ;
#74912 = CARTESIAN_POINT('Ctrl Pts',(-20.6708300596011,-27.1132606358838,
122.586414372797)) ;
#74913 = CARTESIAN_POINT('Ctrl Pts',(-20.418510079688,-26.9332715554651,122.751485490579)) ;
#74914 = CARTESIAN_POINT('Ctrl Pts',(-20.5094030853838,-27.1231916014367,
122.381316698567)) ;
#74915 = CARTESIAN_POINT('Ctrl Pts',(-20.2893670916496,-26.943202521018,122.587408842451)) ;
#74916 = CARTESIAN_POINT('Ctrl Pts',(-20.3150919759959,-27.1331304637732,
122.206830149634)) ;
#74917 = CARTESIAN_POINT('Ctrl Pts',(-20.133917119692,-26.9531413833544,122.44782126066)) ;
#74918 = CARTESIAN_POINT('Ctrl Pts',(-20.0924353594026,-27.1431161946993,
122.067902692441)) ;
#74919 = CARTESIAN_POINT('Ctrl Pts',(-19.9557909146957,-26.9631271142806,
122.336681000983)) ;
#74920 = CARTESIAN_POINT('Ctrl Pts',(-19.8480377025448,-27.1531405801268,
121.96964338509)) ;
#74921 = CARTESIAN_POINT('Ctrl Pts',(-19.7602720483066,-26.9731514997081,
122.258075383028)) ;
#74922 = CARTESIAN_POINT('Ctrl Pts',(-19.5934350819515,-27.1630438644801,
121.915568323327)) ;
#74923 = CARTESIAN_POINT('Ctrl Pts',(-19.5565899913194,-26.9830547840613,
122.214817300124)) ;
#74924 = CARTESIAN_POINT('Ctrl Pts',(-19.3292573389853,-27.1731038690581,
121.906468774186)) ;
#74925 = CARTESIAN_POINT('Ctrl Pts',(-19.3452475890792,-26.9931147886393,
122.207539583563)) ;
#74926 = CARTESIAN_POINT('Ctrl Pts',(-19.0730690560333,-27.1829471381272,
121.942410468998)) ;
#74927 = CARTESIAN_POINT('Ctrl Pts',(-19.1402979129544,-27.0029580577084,
122.236294726187)) ;
#74928 = CARTESIAN_POINT('Ctrl Pts',(-18.8231985706341,-27.1929377037349,
122.022885562064)) ;
#74929 = CARTESIAN_POINT('Ctrl Pts',(-18.9404022136018,-27.0129486233161,
122.300676481672)) ;
#74930 = CARTESIAN_POINT('Ctrl Pts',(-18.5925284415129,-27.2028658355137,
122.144814464939)) ;
#74931 = CARTESIAN_POINT('Ctrl Pts',(-18.7558673038755,-27.022876755095,122.398221026076)) ;
#74932 = CARTESIAN_POINT('Ctrl Pts',(-18.3850125184696,-27.2128537225946,
122.305545417233)) ;
#74933 = CARTESIAN_POINT('Ctrl Pts',(-18.5898557473657,-27.0328646421759,
122.526807075092)) ;
#74934 = CARTESIAN_POINT('Ctrl Pts',(-18.2080550367368,-27.2228896721633,
122.501085855597)) ;
#74935 = CARTESIAN_POINT('Ctrl Pts',(-18.4482910618857,-27.0429005917445,
122.683240696432)) ;
#74936 = CARTESIAN_POINT('Ctrl Pts',(-18.0698877944211,-27.2327445585421,
122.720150718089)) ;
#74937 = CARTESIAN_POINT('Ctrl Pts',(-18.3377591347981,-27.0527554781234,
122.858492893348)) ;
#74938 = CARTESIAN_POINT('Ctrl Pts',(-17.9701127119462,-27.24274397289,122.963197940048)) ;
#74939 = CARTESIAN_POINT('Ctrl Pts',(-18.2579406678591,-27.0627548924712,
123.05293121135)) ;
#74940 = CARTESIAN_POINT('Ctrl Pts',(-17.9143476220501,-27.2526391380805,
123.217227543741)) ;
#74941 = CARTESIAN_POINT('Ctrl Pts',(-18.2133303139703,-27.0726500576617,
123.256154668995)) ;
#74942 = CARTESIAN_POINT('Ctrl Pts',(-17.9033877647494,-27.2626994567724,
123.481339637187)) ;
#74943 = CARTESIAN_POINT('Ctrl Pts',(-18.2045640578609,-27.0827103763537,
123.467444605589)) ;
#74944 = CARTESIAN_POINT('Ctrl Pts',(-17.9375767428716,-27.2725495885485,
123.737946697379)) ;
#74945 = CARTESIAN_POINT('Ctrl Pts',(-18.2319167231407,-27.0925605081298,
123.672729209851)) ;
#74946 = CARTESIAN_POINT('Ctrl Pts',(-18.016630672151,-27.2825801589988,123.989393136754)) ;
#74947 = CARTESIAN_POINT('Ctrl Pts',(-18.2951613035429,-27.10259107858,123.873885960265)) ;
#74948 = CARTESIAN_POINT('Ctrl Pts',(-18.1384764759908,-27.2925943096716,
124.222663794545)) ;
#74949 = CARTESIAN_POINT('Ctrl Pts',(-18.3926393637792,-27.1126052292528,
124.060501732075)) ;
#74950 = CARTESIAN_POINT('Ctrl Pts',(-18.2966929164061,-27.302487243217,124.428958569304)) ;
#74951 = CARTESIAN_POINT('Ctrl Pts',(-18.5192133357134,-27.1224981627982,
124.225536119169)) ;
#74952 = CARTESIAN_POINT('Ctrl Pts',(-18.4899718703588,-27.3124767572072,
124.606563738804)) ;
#74953 = CARTESIAN_POINT('Ctrl Pts',(-18.673837373234,-27.1324876767885,124.367619065612)) ;
#74954 = CARTESIAN_POINT('Ctrl Pts',(-18.7103215045475,-27.3224305278597,
124.747585098893)) ;
#74955 = CARTESIAN_POINT('Ctrl Pts',(-18.8501175596139,-27.1424414474409,
124.480434760865)) ;
#74956 = CARTESIAN_POINT('Ctrl Pts',(-18.9541222140614,-27.3324782965202,
124.848911596921)) ;
#74957 = CARTESIAN_POINT('Ctrl Pts',(-19.0451588376447,-27.1524892161015,
124.561494652999)) ;
#74958 = CARTESIAN_POINT('Ctrl Pts',(-19.2065092981339,-27.3423200229601,
124.905498198079)) ;
#74959 = CARTESIAN_POINT('Ctrl Pts',(-19.2470678872194,-27.1623309425413,
124.606762343776)) ;
#74960 = CARTESIAN_POINT('Ctrl Pts',(-19.4685730602029,-27.3523055397828,
124.918145049044)) ;
#74961 = CARTESIAN_POINT('Ctrl Pts',(-19.456718762585,-27.172316459364,124.616878517439)) ;
#74962 = CARTESIAN_POINT('Ctrl Pts',(-19.7277379052748,-27.3622448714784,
124.88533514878)) ;
#74963 = CARTESIAN_POINT('Ctrl Pts',(-19.6640500453479,-27.1822557910596,
124.590629385903)) ;
#74964 = CARTESIAN_POINT('Ctrl Pts',(-19.9797167083785,-27.3722846411759,
124.807206664795)) ;
#74965 = CARTESIAN_POINT('Ctrl Pts',(-19.8656328181808,-27.1922955607571,
124.528125331113)) ;
#74966 = CARTESIAN_POINT('Ctrl Pts',(-20.2108513393377,-27.3821728024247,
124.68843293536)) ;
#74967 = CARTESIAN_POINT('Ctrl Pts',(-20.0505392887375,-27.2021837220059,
124.433105562087)) ;
#74968 = CARTESIAN_POINT('Ctrl Pts',(-20.4202523049832,-27.392162356927,124.530127299202)) ;
#74969 = CARTESIAN_POINT('Ctrl Pts',(-20.2180592277372,-27.2121732765083,
124.306460234651)) ;
#74970 = CARTESIAN_POINT('Ctrl Pts',(-20.5982841261792,-27.4021207714507,
124.338329003552)) ;
#74971 = CARTESIAN_POINT('Ctrl Pts',(-20.360483568371,-27.222131691032,124.153021035403)) ;
#74972 = CARTESIAN_POINT('Ctrl Pts',(-20.7400208953104,-27.4120206842801,
124.120151747185)) ;
#74973 = CARTESIAN_POINT('Ctrl Pts',(-20.473871715113,-27.2320316038613,123.9784792444)) ;
#74974 = CARTESIAN_POINT('Ctrl Pts',(-20.8431437131481,-27.42206738393,123.877134998713)) ;
#74975 = CARTESIAN_POINT('Ctrl Pts',(-20.5563690459131,-27.2420783035112,
123.784065268537)) ;
#74976 = CARTESIAN_POINT('Ctrl Pts',(-20.9018126856144,-27.4319672442356,
123.623637353361)) ;
#74977 = CARTESIAN_POINT('Ctrl Pts',(-20.6033030544183,-27.2519781638168,
123.581267614642)) ;
#74978 = CARTESIAN_POINT('Ctrl Pts',(-20.9158681862784,-27.442018648441,123.359908517842)) ;
#74979 = CARTESIAN_POINT('Ctrl Pts',(-20.614546450276,-27.2620295680223,123.370284295332)) ;
#74980 = CARTESIAN_POINT('Ctrl Pts',(-20.8845444216374,-27.4518996853622,
123.102102763096)) ;
#74981 = CARTESIAN_POINT('Ctrl Pts',(-20.5894865476393,-27.2719106049434,
123.164040624998)) ;
#74982 = CARTESIAN_POINT('Ctrl Pts',(-20.8083897018566,-27.4618995175397,
122.850639705385)) ;
#74983 = CARTESIAN_POINT('Ctrl Pts',(-20.5285619312095,-27.2819104371209,
122.962870552448)) ;
#74984 = CARTESIAN_POINT('Ctrl Pts',(-20.6908521996754,-27.4718175205245,
122.617961007271)) ;
#74985 = CARTESIAN_POINT('Ctrl Pts',(-20.43453143348,-27.2918284401058,122.776728527516)) ;
#74986 = CARTESIAN_POINT('Ctrl Pts',(-20.5325862277166,-27.4818688263991,
122.406544566077)) ;
#74987 = CARTESIAN_POINT('Ctrl Pts',(-20.3079178321186,-27.3018797459804,
122.607595752983)) ;
#74988 = CARTESIAN_POINT('Ctrl Pts',(-20.3436360268456,-27.4917386497907,
122.228783160623)) ;
#74989 = CARTESIAN_POINT('Ctrl Pts',(-20.1567577854576,-27.3117495693719,
122.465387842878)) ;
#74990 = CARTESIAN_POINT('Ctrl Pts',(-20.1222882553829,-27.501812815841,122.083664260609)) ;
#74991 = CARTESIAN_POINT('Ctrl Pts',(-19.9796788329855,-27.3218237354222,
122.349293214515)) ;
#74992 = CARTESIAN_POINT('Ctrl Pts',(-19.8852542608769,-27.5116328999826,
121.981478175985)) ;
#74993 = CARTESIAN_POINT('Ctrl Pts',(-19.7900524902871,-27.3316438195639,
122.267545514143)) ;
#74994 = CARTESIAN_POINT('Ctrl Pts',(-19.6276445348862,-27.5217116267184,
121.920220233183)) ;
#74995 = CARTESIAN_POINT('Ctrl Pts',(-19.5839641856869,-27.3417225462997,
122.218539730451)) ;
#74996 = CARTESIAN_POINT('Ctrl Pts',(-19.3691479103159,-27.531563207368,121.904877852265)) ;
#74997 = CARTESIAN_POINT('Ctrl Pts',(-19.3771679014181,-27.3515741269492,
122.206266540335)) ;
#74998 = CARTESIAN_POINT('Ctrl Pts',(-19.1062132173392,-27.5416363356664,
121.935078087931)) ;
#74999 = CARTESIAN_POINT('Ctrl Pts',(-19.1668198669398,-27.3616472552476,
122.230427363407)) ;
#75000 = CARTESIAN_POINT('Ctrl Pts',(-18.8582685979717,-27.5514788135578,
122.008806224797)) ;
#75001 = CARTESIAN_POINT('Ctrl Pts',(-18.9684654319779,-27.3714897331391,
122.289410133124)) ;
#75002 = CARTESIAN_POINT('Ctrl Pts',(-18.6232876860995,-27.5614594201559,
122.125286522792)) ;
#75003 = CARTESIAN_POINT('Ctrl Pts',(-18.7804810973601,-27.3814703397371,
122.382594611719)) ;
#75004 = CARTESIAN_POINT('Ctrl Pts',(-18.411600270402,-27.5714771291747,122.281782687908)) ;
#75005 = CARTESIAN_POINT('Ctrl Pts',(-18.6111314675826,-27.3914880487559,
122.507791959957)) ;
#75006 = CARTESIAN_POINT('Ctrl Pts',(-18.2323009870083,-27.5813633082121,
122.469819398484)) ;
#75007 = CARTESIAN_POINT('Ctrl Pts',(-18.4676929146779,-27.4013742277934,
122.65822097498)) ;
#75008 = CARTESIAN_POINT('Ctrl Pts',(-18.085888722091,-27.5914209207844,122.689836404028)) ;
#75009 = CARTESIAN_POINT('Ctrl Pts',(-18.3505632824027,-27.4114318403657,
122.834234999918)) ;
#75010 = CARTESIAN_POINT('Ctrl Pts',(-17.9817726806253,-27.6012973141566,
122.92759672565)) ;
#75011 = CARTESIAN_POINT('Ctrl Pts',(-18.2672711670262,-27.4213082337378,
123.024442556299)) ;
#75012 = CARTESIAN_POINT('Ctrl Pts',(-17.9191542664928,-27.611292342307,123.182674524729)) ;
#75013 = CARTESIAN_POINT('Ctrl Pts',(-18.2171766775005,-27.4313032618883,
123.228504708676)) ;
#75014 = CARTESIAN_POINT('Ctrl Pts',(-17.9021807329036,-27.621313089153,123.445473162293)) ;
#75015 = CARTESIAN_POINT('Ctrl Pts',(-18.2035981738734,-27.4413240087343,
123.4387436757)) ;
#75016 = CARTESIAN_POINT('Ctrl Pts',(-17.9304488696092,-27.6312151578194,
123.704146901857)) ;
#75017 = CARTESIAN_POINT('Ctrl Pts',(-18.2262128505501,-27.4512260774006,
123.645681876394)) ;
#75018 = CARTESIAN_POINT('Ctrl Pts',(-18.0034825911489,-27.6412058976391,
123.956332064163)) ;
#75019 = CARTESIAN_POINT('Ctrl Pts',(-18.2846399233845,-27.4612168172203,
123.847429782292)) ;
#75020 = CARTESIAN_POINT('Ctrl Pts',(-18.1190427861828,-27.6511690938494,
124.191258163487)) ;
#75021 = CARTESIAN_POINT('Ctrl Pts',(-18.3770881012001,-27.4711800134306,
124.035370248739)) ;
#75022 = CARTESIAN_POINT('Ctrl Pts',(-18.2722240570059,-27.6610732781495,
124.401708795439)) ;
#75023 = CARTESIAN_POINT('Ctrl Pts',(-18.4996327056077,-27.4810841977308,
124.203730123677)) ;
#75024 = CARTESIAN_POINT('Ctrl Pts',(-18.4626903999786,-27.6711337385404,
124.585014918557)) ;
#75025 = CARTESIAN_POINT('Ctrl Pts',(-18.6520060497622,-27.4911446581216,
124.350375149966)) ;
#75026 = CARTESIAN_POINT('Ctrl Pts',(-18.6771667745234,-27.6809742844111,
124.729554078356)) ;
#75027 = CARTESIAN_POINT('Ctrl Pts',(-18.8235861793774,-27.5009852039924,
124.466005811902)) ;
#75028 = CARTESIAN_POINT('Ctrl Pts',(-18.9186090603033,-27.6910365051229,
124.837307374899)) ;
#75029 = CARTESIAN_POINT('Ctrl Pts',(-19.016740247443,-27.5110474247042,124.552208638131)) ;
#75030 = CARTESIAN_POINT('Ctrl Pts',(-19.1709926750381,-27.7009336481395,
124.900195583819)) ;
#75031 = CARTESIAN_POINT('Ctrl Pts',(-19.2186463603094,-27.5209445677207,
124.602519015299)) ;
#75032 = CARTESIAN_POINT('Ctrl Pts',(-19.4312729665499,-27.7108648245567,
124.919233320741)) ;
#75033 = CARTESIAN_POINT('Ctrl Pts',(-19.4268700019089,-27.5308757441379,
124.617749388828)) ;
#75034 = CARTESIAN_POINT('Ctrl Pts',(-19.6937795869066,-27.7209070383353,
124.892204557347)) ;
#75035 = CARTESIAN_POINT('Ctrl Pts',(-19.636875479684,-27.5409179579165,124.59612651213)) ;
#75036 = CARTESIAN_POINT('Ctrl Pts',(-19.9437421483917,-27.730793578538,124.821306255777)) ;
#75037 = CARTESIAN_POINT('Ctrl Pts',(-19.836844746594,-27.5508044981193,124.539408302028)) ;
#75038 = CARTESIAN_POINT('Ctrl Pts',(-20.1802824076589,-27.7407871731435,
124.707252644215)) ;
#75039 = CARTESIAN_POINT('Ctrl Pts',(-20.0260769445174,-27.5607980927247,
124.448165758018)) ;
#75040 = CARTESIAN_POINT('Ctrl Pts',(-20.3923713221188,-27.7507310483009,
124.554570637496)) ;
#75041 = CARTESIAN_POINT('Ctrl Pts',(-20.1957478479467,-27.5707419678822,
124.326020684454)) ;
#75042 = CARTESIAN_POINT('Ctrl Pts',(-20.5752568934458,-27.7606915844158,
124.36733113008)) ;
#75043 = CARTESIAN_POINT('Ctrl Pts',(-20.3420563159796,-27.5807025039971,
124.176229618266)) ;
#75044 = CARTESIAN_POINT('Ctrl Pts',(-20.7235437791157,-27.7706881877385,
124.150451479932)) ;
#75045 = CARTESIAN_POINT('Ctrl Pts',(-20.4606861037265,-27.5906991073198,
124.002726235317)) ;
#75046 = CARTESIAN_POINT('Ctrl Pts',(-20.8319614751278,-27.780721270693,123.910121632743)) ;
#75047 = CARTESIAN_POINT('Ctrl Pts',(-20.5474206058342,-27.6007321902743,
123.810462391625)) ;
#75048 = CARTESIAN_POINT('Ctrl Pts',(-20.8961417941219,-27.7905724393946,
123.659328927906)) ;
#75049 = CARTESIAN_POINT('Ctrl Pts',(-20.5987649851893,-27.6105833589758,
123.609829391344)) ;
#75050 = CARTESIAN_POINT('Ctrl Pts',(-20.9167937428993,-27.8005349300935,
123.398350225033)) ;
#75051 = CARTESIAN_POINT('Ctrl Pts',(-20.6152871158748,-27.6205458496747,
123.401046845239)) ;
#75052 = CARTESIAN_POINT('Ctrl Pts',(-20.8913248728569,-27.8105633585112,
123.13603219385)) ;
#75053 = CARTESIAN_POINT('Ctrl Pts',(-20.5949125321571,-27.6305742780925,
123.191192291486)) ;
#75054 = CARTESIAN_POINT('Ctrl Pts',(-20.8216156441421,-27.8204737258758,
122.88511292039)) ;
#75055 = CARTESIAN_POINT('Ctrl Pts',(-20.5391458591745,-27.640484645457,122.990457403175)) ;
#75056 = CARTESIAN_POINT('Ctrl Pts',(-20.7097290522981,-27.8304085934909,
122.649216253088)) ;
#75057 = CARTESIAN_POINT('Ctrl Pts',(-20.4496374549925,-27.6504195130721,
122.801740241644)) ;
#75058 = CARTESIAN_POINT('Ctrl Pts',(-20.5567753118264,-27.8404497354699,
122.434208642575)) ;
#75059 = CARTESIAN_POINT('Ctrl Pts',(-20.3272749058312,-27.6604606550512,
122.629733654314)) ;
#75060 = CARTESIAN_POINT('Ctrl Pts',(-20.3718067249568,-27.8503368716731,
122.251718186842)) ;
#75061 = CARTESIAN_POINT('Ctrl Pts',(-20.1793011160621,-27.6703477912543,
122.483741378946)) ;
#75062 = CARTESIAN_POINT('Ctrl Pts',(-20.1559638842392,-27.8603291540765,
122.102205529712)) ;
#75063 = CARTESIAN_POINT('Ctrl Pts',(-20.006627433317,-27.6803400736577,122.364130687556)) ;
#75064 = CARTESIAN_POINT('Ctrl Pts',(-19.9184230348572,-27.8702776820417,
121.992974547552)) ;
#75065 = CARTESIAN_POINT('Ctrl Pts',(-19.816595474273,-27.6902886016229,122.276745372545)) ;
#75066 = CARTESIAN_POINT('Ctrl Pts',(-19.6659531803029,-27.8802144132038,
121.926377817736)) ;
#75067 = CARTESIAN_POINT('Ctrl Pts',(-19.6146203057764,-27.7002253327851,
122.223467276849)) ;
#75068 = CARTESIAN_POINT('Ctrl Pts',(-19.4045120642445,-27.8901976240638,
121.904196807102)) ;
#75069 = CARTESIAN_POINT('Ctrl Pts',(-19.4054676973117,-27.710208543645,122.205721541653)) ;
#75070 = CARTESIAN_POINT('Ctrl Pts',(-19.1417251311508,-27.9002407232137,
121.928354401178)) ;
#75071 = CARTESIAN_POINT('Ctrl Pts',(-19.1952379245654,-27.7202516427949,
122.225046799241)) ;
#75072 = CARTESIAN_POINT('Ctrl Pts',(-18.8922932247539,-27.9100716874885,
121.99576525242)) ;
#75073 = CARTESIAN_POINT('Ctrl Pts',(-18.9956932551907,-27.7300826070698,
122.278974240053)) ;
#75074 = CARTESIAN_POINT('Ctrl Pts',(-18.6525836804563,-27.9201445398745,
122.107953193287)) ;
#75075 = CARTESIAN_POINT('Ctrl Pts',(-18.8039248906843,-27.7401554594558,
122.368723808351)) ;
#75076 = CARTESIAN_POINT('Ctrl Pts',(-18.4404518361737,-27.9300086675863,
122.256983728399)) ;
#75077 = CARTESIAN_POINT('Ctrl Pts',(-18.6342195866533,-27.7500195871675,
122.487946889381)) ;
#75078 = CARTESIAN_POINT('Ctrl Pts',(-18.2540538809993,-27.9400308697212,
122.44303741663)) ;
#75079 = CARTESIAN_POINT('Ctrl Pts',(-18.4851003818533,-27.7600417893024,
122.636789047312)) ;
#75080 = CARTESIAN_POINT('Ctrl Pts',(-18.1032133229572,-27.9500580626896,
122.659116134861)) ;
#75081 = CARTESIAN_POINT('Ctrl Pts',(-18.3644270759834,-27.7700689822708,
122.809651490149)) ;
#75082 = CARTESIAN_POINT('Ctrl Pts',(-17.9937284542524,-27.9599136566566,
122.893810711262)) ;
#75083 = CARTESIAN_POINT('Ctrl Pts',(-18.2768385935525,-27.7799245762378,
122.997405800576)) ;
#75084 = CARTESIAN_POINT('Ctrl Pts',(-17.9252066476934,-27.9698708285219,
123.146353412753)) ;
#75085 = CARTESIAN_POINT('Ctrl Pts',(-18.2220200039114,-27.7898817481031,
123.199439298674)) ;
#75086 = CARTESIAN_POINT('Ctrl Pts',(-17.901836392515,-27.9799096725203,123.409110487333)) ;
#75087 = CARTESIAN_POINT('Ctrl Pts',(-18.2033226182715,-27.7999205921015,
123.409644963665)) ;
#75088 = CARTESIAN_POINT('Ctrl Pts',(-17.9236207436756,-27.9897836963958,
123.667708642631)) ;
#75089 = CARTESIAN_POINT('Ctrl Pts',(-18.2207487591916,-27.8097946159771,
123.616522787693)) ;
#75090 = CARTESIAN_POINT('Ctrl Pts',(-17.9912807796394,-27.9998535223862,
123.923499029273)) ;
#75091 = CARTESIAN_POINT('Ctrl Pts',(-18.2748756263371,-27.8198644419675,
123.821155692994)) ;
#75092 = CARTESIAN_POINT('Ctrl Pts',(-18.0996170115051,-28.0096867662835,
124.158124720486)) ;
#75093 = CARTESIAN_POINT('Ctrl Pts',(-18.3615429995661,-27.8296976858648,
124.008855863308)) ;
#75094 = CARTESIAN_POINT('Ctrl Pts',(-18.2493713827489,-28.0197171940566,
124.375030745344)) ;
#75095 = CARTESIAN_POINT('Ctrl Pts',(-18.481345335379,-27.8397281136378,124.182381569428)) ;
#75096 = CARTESIAN_POINT('Ctrl Pts',(-18.4350962680319,-28.0297488108017,
124.562139179314)) ;
#75097 = CARTESIAN_POINT('Ctrl Pts',(-18.6299243679393,-27.8497597303829,
124.332069278655)) ;
#75098 = CARTESIAN_POINT('Ctrl Pts',(-18.6458160519493,-28.0395784877824,
124.71151934182)) ;
#75099 = CARTESIAN_POINT('Ctrl Pts',(-18.798498550654,-27.8595894073637,124.451573974288)) ;
#75100 = CARTESIAN_POINT('Ctrl Pts',(-18.8827549500169,-28.0495680046223,
124.824558143957)) ;
#75101 = CARTESIAN_POINT('Ctrl Pts',(-18.9880488657586,-27.8695789242036,
124.542006370576)) ;
#75102 = CARTESIAN_POINT('Ctrl Pts',(-19.1372585886955,-28.0596116167621,
124.894470815624)) ;
#75103 = CARTESIAN_POINT('Ctrl Pts',(-19.1916515109275,-27.8796225363434,
124.597937922925)) ;
#75104 = CARTESIAN_POINT('Ctrl Pts',(-19.3942099817869,-28.0694342230974,
124.919127791783)) ;
#75105 = CARTESIAN_POINT('Ctrl Pts',(-19.3972114824336,-27.8894451426787,
124.617664945199)) ;
#75106 = CARTESIAN_POINT('Ctrl Pts',(-19.6572218646188,-28.0794724529966,
124.898947663113)) ;
#75107 = CARTESIAN_POINT('Ctrl Pts',(-19.6076212137935,-27.8994833725779,
124.601522486604)) ;
#75108 = CARTESIAN_POINT('Ctrl Pts',(-19.9119170104827,-28.0894834877886,
124.832984826459)) ;
#75109 = CARTESIAN_POINT('Ctrl Pts',(-19.8113776795567,-27.9094944073698,
124.548753715423)) ;
#75110 = CARTESIAN_POINT('Ctrl Pts',(-20.1487320477666,-28.0993812187557,
124.725423875362)) ;
#75111 = CARTESIAN_POINT('Ctrl Pts',(-20.000829845105,-27.919392138337,124.462706670356)) ;
#75112 = CARTESIAN_POINT('Ctrl Pts',(-20.3654611749056,-28.1093708466062,
124.577295140872)) ;
#75113 = CARTESIAN_POINT('Ctrl Pts',(-20.1742139780183,-27.9293817661874,
124.344205147162)) ;
#75114 = CARTESIAN_POINT('Ctrl Pts',(-20.5524779416737,-28.1193266370522,
124.394341663495)) ;
#75115 = CARTESIAN_POINT('Ctrl Pts',(-20.3238283305594,-27.9393375566334,
124.197843770989)) ;
#75116 = CARTESIAN_POINT('Ctrl Pts',(-20.7048656205572,-28.1292540356142,
124.182581520331)) ;
#75117 = CARTESIAN_POINT('Ctrl Pts',(-20.4457396528893,-27.9492649551955,
124.028437013102)) ;
#75118 = CARTESIAN_POINT('Ctrl Pts',(-20.8192132352062,-28.1392796307241,
123.945237856625)) ;
#75119 = CARTESIAN_POINT('Ctrl Pts',(-20.5372193152296,-27.9592905503054,
123.838562820331)) ;
#75120 = CARTESIAN_POINT('Ctrl Pts',(-20.8897744388912,-28.1491654813937,
123.695212486586)) ;
#75121 = CARTESIAN_POINT('Ctrl Pts',(-20.5936698151312,-27.9691764009749,
123.638543566476)) ;
#75122 = CARTESIAN_POINT('Ctrl Pts',(-20.916742686365,-28.1591546612379,123.434089007644)) ;
#75123 = CARTESIAN_POINT('Ctrl Pts',(-20.6152462522755,-27.9791655808191,
123.429645100009)) ;
#75124 = CARTESIAN_POINT('Ctrl Pts',(-20.8973138530435,-28.1691958483415,
123.170934263107)) ;
#75125 = CARTESIAN_POINT('Ctrl Pts',(-20.5997049495287,-27.9892067679227,
123.219121101024)) ;
#75126 = CARTESIAN_POINT('Ctrl Pts',(-20.8342467262593,-28.1790284918174,
122.920361624819)) ;
#75127 = CARTESIAN_POINT('Ctrl Pts',(-20.5492532207289,-27.9990394113987,
123.018663281372)) ;
#75128 = CARTESIAN_POINT('Ctrl Pts',(-20.727582872687,-28.1890224415269,122.680368443605)) ;
#75129 = CARTESIAN_POINT('Ctrl Pts',(-20.463923962656,-28.0090333611081,122.826668031653)) ;
#75130 = CARTESIAN_POINT('Ctrl Pts',(-20.5798888067708,-28.1990515643034,
122.462081994055)) ;
#75131 = CARTESIAN_POINT('Ctrl Pts',(-20.3457702502389,-28.0190624838847,
122.652037809533)) ;
#75132 = CARTESIAN_POINT('Ctrl Pts',(-20.3996251641933,-28.2089276952221,
122.275347174476)) ;
#75133 = CARTESIAN_POINT('Ctrl Pts',(-20.2015610992789,-28.0289386148033,
122.502648999522)) ;
#75134 = CARTESIAN_POINT('Ctrl Pts',(-20.1873021799924,-28.2189257302391,
122.120642324666)) ;
#75135 = CARTESIAN_POINT('Ctrl Pts',(-20.0317039475205,-28.0389366498204,
122.37888357736)) ;
#75136 = CARTESIAN_POINT('Ctrl Pts',(-19.9533587455993,-28.2288396599978,
122.005916898507)) ;
#75137 = CARTESIAN_POINT('Ctrl Pts',(-19.8445504140462,-28.0488505795791,
122.287101605949)) ;
#75138 = CARTESIAN_POINT('Ctrl Pts',(-19.6998517914113,-28.2388828477356,
121.932573093213)) ;
#75139 = CARTESIAN_POINT('Ctrl Pts',(-19.6417453532736,-28.0588937673169,
122.228424618319)) ;
#75140 = CARTESIAN_POINT('Ctrl Pts',(-19.4411734358219,-28.248782689876,121.904743447145)) ;
#75141 = CARTESIAN_POINT('Ctrl Pts',(-19.4348032777468,-28.0687936094572,
122.206158949824)) ;
#75142 = CARTESIAN_POINT('Ctrl Pts',(-19.1791693222419,-28.258773956684,121.921854203965)) ;
#75143 = CARTESIAN_POINT('Ctrl Pts',(-19.2251999469823,-28.0787848762652,
122.219845480099)) ;
#75144 = CARTESIAN_POINT('Ctrl Pts',(-18.9231809982918,-28.2688060588159,
121.984895781364)) ;
#75145 = CARTESIAN_POINT('Ctrl Pts',(-19.0204087941554,-28.0888169783972,
122.270276784581)) ;
#75146 = CARTESIAN_POINT('Ctrl Pts',(-18.6858684267208,-28.2786729397707,
122.089356190558)) ;
#75147 = CARTESIAN_POINT('Ctrl Pts',(-18.830558338332,-28.098683859352,122.353843037551)) ;
#75148 = CARTESIAN_POINT('Ctrl Pts',(-18.4672132264003,-28.2886647310588,
122.234743944301)) ;
#75149 = CARTESIAN_POINT('Ctrl Pts',(-18.6556330730798,-28.1086756506401,
122.470151422643)) ;
#75150 = CARTESIAN_POINT('Ctrl Pts',(-18.2767129740866,-28.2986968469704,
122.416985014521)) ;
#75151 = CARTESIAN_POINT('Ctrl Pts',(-18.5032314387329,-28.1187077665516,
122.615942781619)) ;
#75152 = CARTESIAN_POINT('Ctrl Pts',(-18.123001634018,-28.3085631637704,122.62579831498)) ;
#75153 = CARTESIAN_POINT('Ctrl Pts',(-18.380260910136,-28.1285740833517,122.782991837959)) ;
#75154 = CARTESIAN_POINT('Ctrl Pts',(-18.0061033568206,-28.318550645244,122.860752752816)) ;
#75155 = CARTESIAN_POINT('Ctrl Pts',(-18.2867404042396,-28.1385615648253,
122.970954341277)) ;
#75156 = CARTESIAN_POINT('Ctrl Pts',(-17.9319400038303,-28.3284955696229,
123.111391293692)) ;
#75157 = CARTESIAN_POINT('Ctrl Pts',(-18.2274077034628,-28.1485064892042,
123.171464381746)) ;
#75158 = CARTESIAN_POINT('Ctrl Pts',(-17.9022796487735,-28.3385404555336,
123.373664123608)) ;
#75159 = CARTESIAN_POINT('Ctrl Pts',(-18.2036772802856,-28.1585513751149,
123.381282418945)) ;
#75160 = CARTESIAN_POINT('Ctrl Pts',(-17.9180879855161,-28.3484025592462,
123.632366059923)) ;
#75161 = CARTESIAN_POINT('Ctrl Pts',(-18.2163217656105,-28.1684134788274,
123.588243760099)) ;
#75162 = CARTESIAN_POINT('Ctrl Pts',(-17.9788452222252,-28.3583941230706,
123.887787950751)) ;
#75163 = CARTESIAN_POINT('Ctrl Pts',(-18.2649253910361,-28.1784050426519,
123.792581709161)) ;
#75164 = CARTESIAN_POINT('Ctrl Pts',(-18.0825235359367,-28.3683269311335,
124.127337211382)) ;
#75165 = CARTESIAN_POINT('Ctrl Pts',(-18.3478659549648,-28.1883378507148,
123.984221828264)) ;
#75166 = CARTESIAN_POINT('Ctrl Pts',(-18.2257556810704,-28.3782640333699,
124.345706898294)) ;
#75167 = CARTESIAN_POINT('Ctrl Pts',(-18.4624497295589,-28.1982749529511,
124.158918686381)) ;
#75168 = CARTESIAN_POINT('Ctrl Pts',(-18.4070352869931,-28.3883164796403,
124.537830699368)) ;
#75169 = CARTESIAN_POINT('Ctrl Pts',(-18.6074717934068,-28.2083273992215,
124.312619238854)) ;
#75170 = CARTESIAN_POINT('Ctrl Pts',(-18.61438364314,-28.3981625952219,124.692645379535)) ;
#75171 = CARTESIAN_POINT('Ctrl Pts',(-18.7733489636727,-28.2181735148031,
124.436472636285)) ;
#75172 = CARTESIAN_POINT('Ctrl Pts',(-18.8499799673365,-28.4082106149368,
124.811841582579)) ;
#75173 = CARTESIAN_POINT('Ctrl Pts',(-18.9618249984737,-28.228221534518,124.531831597543)) ;
#75174 = CARTESIAN_POINT('Ctrl Pts',(-19.100163676913,-28.4181525665657,124.887173703437)) ;
#75175 = CARTESIAN_POINT('Ctrl Pts',(-19.1619712108279,-28.238163486147,124.592099400923)) ;
#75176 = CARTESIAN_POINT('Ctrl Pts',(-19.3594558684225,-28.4280913475648,
124.918552242623)) ;
#75177 = CARTESIAN_POINT('Ctrl Pts',(-19.3694046064628,-28.248102267146,124.61720445296)) ;
#75178 = CARTESIAN_POINT('Ctrl Pts',(-19.6225169288558,-28.4381173962909,
124.904110048456)) ;
#75179 = CARTESIAN_POINT('Ctrl Pts',(-19.5798535127197,-28.2581283158721,
124.60565295931)) ;
#75180 = CARTESIAN_POINT('Ctrl Pts',(-19.8756354818574,-28.4480042566991,
124.845353062443)) ;
#75181 = CARTESIAN_POINT('Ctrl Pts',(-19.7823488152932,-28.2680151762803,
124.55864953328)) ;
#75182 = CARTESIAN_POINT('Ctrl Pts',(-20.1181752200721,-28.4580355318309,
124.742190925172)) ;
#75183 = CARTESIAN_POINT('Ctrl Pts',(-19.9763812831176,-28.2780464514121,
124.476122110811)) ;
#75184 = CARTESIAN_POINT('Ctrl Pts',(-20.3360779497552,-28.4679185091313,
124.600777052359)) ;
#75185 = CARTESIAN_POINT('Ctrl Pts',(-20.1507052303913,-28.2879294287125,
124.362992221081)) ;
#75186 = CARTESIAN_POINT('Ctrl Pts',(-20.5293776949433,-28.4779753625384,
124.42064431498)) ;
#75187 = CARTESIAN_POINT('Ctrl Pts',(-20.3053443489214,-28.2979862821197,
124.218890369488)) ;
#75188 = CARTESIAN_POINT('Ctrl Pts',(-20.7382563361308,-28.4911436036144,
124.144618304014)) ;
#75189 = CARTESIAN_POINT('Ctrl Pts',(-20.4724604249661,-28.3111545231956,
123.998058237581)) ;
#75190 = CARTESIAN_POINT('Ctrl Pts',(-20.8725696184316,-28.5045446328409,
123.814898573021)) ;
#75191 = CARTESIAN_POINT('Ctrl Pts',(-20.5799131718557,-28.3245555524222,
123.734258095252)) ;
#75192 = CARTESIAN_POINT('Ctrl Pts',(-20.9154664865249,-28.5177575495718,
123.47022980443)) ;
#75193 = CARTESIAN_POINT('Ctrl Pts',(-20.6142236339119,-28.337768469153,123.458566993245)) ;
#75194 = CARTESIAN_POINT('Ctrl Pts',(-20.903122860515,-28.527685944025,123.209668872565)) ;
#75195 = CARTESIAN_POINT('Ctrl Pts',(-20.6043529645336,-28.3476968636062,
123.250109340891)) ;
#75196 = CARTESIAN_POINT('Ctrl Pts',(-20.8455899284453,-28.5376674441531,
122.953713451774)) ;
#75197 = CARTESIAN_POINT('Ctrl Pts',(-20.5583282472634,-28.3576783637344,
123.045346890605)) ;
#75198 = CARTESIAN_POINT('Ctrl Pts',(-20.7435726950686,-28.5477079874232,
122.710393832295)) ;
#75199 = CARTESIAN_POINT('Ctrl Pts',(-20.4767166760668,-28.3677189070045,
122.850689784726)) ;
#75200 = CARTESIAN_POINT('Ctrl Pts',(-20.6038530330723,-28.5575573192063,
122.492510433915)) ;
#75201 = CARTESIAN_POINT('Ctrl Pts',(-20.3649427782715,-28.3775682387876,
122.676381961247)) ;
#75202 = CARTESIAN_POINT('Ctrl Pts',(-20.4263234254908,-28.567552723678,122.298921849218)) ;
#75203 = CARTESIAN_POINT('Ctrl Pts',(-20.2229202780013,-28.3875636432592,
122.521509270193)) ;
#75204 = CARTESIAN_POINT('Ctrl Pts',(-20.217150439779,-28.5775690511266,122.139134607497)) ;
#75205 = CARTESIAN_POINT('Ctrl Pts',(-20.0555849188895,-28.3975799707078,
122.393679028551)) ;
#75206 = CARTESIAN_POINT('Ctrl Pts',(-19.9087920778234,-28.5907927082931,
121.978832990182)) ;
#75207 = CARTESIAN_POINT('Ctrl Pts',(-19.8088913174118,-28.4108036278744,
122.265428956437)) ;
#75208 = CARTESIAN_POINT('Ctrl Pts',(-19.5639959876128,-28.6040869996825,
121.902007063476)) ;
#75209 = CARTESIAN_POINT('Ctrl Pts',(-19.5330215630254,-28.4240979192637,
122.203967911005)) ;
#75210 = CARTESIAN_POINT('Ctrl Pts',(-19.2151418343575,-28.617371350614,121.916882629561)) ;
#75211 = CARTESIAN_POINT('Ctrl Pts',(-19.2539858779433,-28.4373822701952,
122.215868656955)) ;
#75212 = CARTESIAN_POINT('Ctrl Pts',(-18.9592277477031,-28.6273437316758,
121.973142750663)) ;
#75213 = CARTESIAN_POINT('Ctrl Pts',(-19.0492444708714,-28.447354651257,122.260874150028)) ;
#75214 = CARTESIAN_POINT('Ctrl Pts',(-18.7182849243159,-28.6372521113014,
122.07194877023)) ;
#75215 = CARTESIAN_POINT('Ctrl Pts',(-18.8564918768448,-28.4572630308826,
122.33991702492)) ;
#75216 = CARTESIAN_POINT('Ctrl Pts',(-18.4950390577164,-28.6473061100494,
122.213201779961)) ;
#75217 = CARTESIAN_POINT('Ctrl Pts',(-18.6778931410017,-28.4673170296307,
122.452918687146)) ;
#75218 = CARTESIAN_POINT('Ctrl Pts',(-18.3032620687832,-28.6571683071657,
122.387567726326)) ;
#75219 = CARTESIAN_POINT('Ctrl Pts',(-18.5244716495436,-28.477179226747,122.592405885585)) ;
#75220 = CARTESIAN_POINT('Ctrl Pts',(-18.0882237966401,-28.6705154335399,
122.6646378721)) ;
#75221 = CARTESIAN_POINT('Ctrl Pts',(-18.352430803744,-28.4905263531211,122.814082073788)) ;
#75222 = CARTESIAN_POINT('Ctrl Pts',(-17.9176634711222,-28.6870523991813,
123.069772556852)) ;
#75223 = CARTESIAN_POINT('Ctrl Pts',(-18.2159875992731,-28.5070633187626,
123.138150149593)) ;
#75224 = CARTESIAN_POINT('Ctrl Pts',(-17.8947632868144,-28.7036870033552,
123.511208297087)) ;
#75225 = CARTESIAN_POINT('Ctrl Pts',(-18.1976653221791,-28.5236979229365,
123.491362432851)) ;
#75226 = CARTESIAN_POINT('Ctrl Pts',(-17.9677541225909,-28.7169767965979,
123.852806493796)) ;
#75227 = CARTESIAN_POINT('Ctrl Pts',(-18.256052534024,-28.5369877161791,123.764590263567)) ;
#75228 = CARTESIAN_POINT('Ctrl Pts',(-18.0656567608819,-28.7269294278573,
124.095304375475)) ;
#75229 = CARTESIAN_POINT('Ctrl Pts',(-18.3343741827955,-28.5469403474385,
123.9586001496)) ;
#75230 = CARTESIAN_POINT('Ctrl Pts',(-18.2039394802369,-28.736881395162,124.317317362314)) ;
#75231 = CARTESIAN_POINT('Ctrl Pts',(-18.444996651739,-28.5568923147432,124.136207458359)) ;
#75232 = CARTESIAN_POINT('Ctrl Pts',(-18.438736320031,-28.7502486536258,124.578542730228)) ;
#75233 = CARTESIAN_POINT('Ctrl Pts',(-18.6328430825618,-28.570259573207,124.345197322045)) ;
#75234 = CARTESIAN_POINT('Ctrl Pts',(-18.8064292375722,-28.7667654655749,
124.818587725971)) ;
#75235 = CARTESIAN_POINT('Ctrl Pts',(-18.9269842710425,-28.5867763851562,
124.537227610055)) ;
#75236 = CARTESIAN_POINT('Ctrl Pts',(-19.3245222155881,-28.7867913605813,
124.93992203315)) ;
#75237 = CARTESIAN_POINT('Ctrl Pts',(-19.3414616488824,-28.6068022801626,
124.634301067543)) ;
#75238 = CARTESIAN_POINT('Ctrl Pts',(-19.8475073460712,-28.8066020907114,
124.877979440218)) ;
#75239 = CARTESIAN_POINT('Ctrl Pts',(-19.7598502986681,-28.6266130102927,
124.58474931514)) ;
#75240 = CARTESIAN_POINT('Ctrl Pts',(-20.3222930273454,-28.8265793068413,
124.640387404722)) ;
#75241 = CARTESIAN_POINT('Ctrl Pts',(-20.1396805393653,-28.6465902264226,
124.39467832848)) ;
#75242 = CARTESIAN_POINT('Ctrl Pts',(-20.6858890814161,-28.8465061822366,
124.255335344377)) ;
#75243 = CARTESIAN_POINT('Ctrl Pts',(-20.4305598381238,-28.6665171018178,
124.086638285115)) ;
#75244 = CARTESIAN_POINT('Ctrl Pts',(-20.8967489377304,-28.8663276437128,
123.772474684053)) ;
#75245 = CARTESIAN_POINT('Ctrl Pts',(-20.5992504644692,-28.6863385632941,
123.700349310091)) ;
#75246 = CARTESIAN_POINT('Ctrl Pts',(-20.9302406514315,-28.8864019615222,
123.240064582402)) ;
#75247 = CARTESIAN_POINT('Ctrl Pts',(-20.6260460784137,-28.7064128811034,
123.27442205142)) ;
#75248 = CARTESIAN_POINT('Ctrl Pts',(-20.781174527664,-28.9062499305301,122.733886817076)) ;
#75249 = CARTESIAN_POINT('Ctrl Pts',(-20.5067950359757,-28.7262608501113,
122.869477923346)) ;
#75250 = CARTESIAN_POINT('Ctrl Pts',(-20.4677973260754,-28.9261969645933,
122.306404432503)) ;
#75251 = CARTESIAN_POINT('Ctrl Pts',(-20.2560944036663,-28.7462078841745,
122.527490503496)) ;
#75252 = CARTESIAN_POINT('Ctrl Pts',(-20.0282780333266,-28.9460929155654,
122.012300463445)) ;
#75253 = CARTESIAN_POINT('Ctrl Pts',(-19.9044790239162,-28.7661038351467,
122.292205334614)) ;
#75254 = CARTESIAN_POINT('Ctrl Pts',(-19.5150711784619,-28.9659883951837,
121.885006525094)) ;
#75255 = CARTESIAN_POINT('Ctrl Pts',(-19.4939126765269,-28.7859993147649,
122.190368780619)) ;
#75256 = CARTESIAN_POINT('Ctrl Pts',(-18.9875437561368,-28.9859445061485,
121.940541079265)) ;
#75257 = CARTESIAN_POINT('Ctrl Pts',(-19.0718901729245,-28.8059554257297,
122.234795557163)) ;
#75258 = CARTESIAN_POINT('Ctrl Pts',(-18.5120357100292,-29.0058490541885,
122.172247469398)) ;
#75259 = CARTESIAN_POINT('Ctrl Pts',(-18.6914823057681,-28.8258599737697,
122.420160465214)) ;
#75260 = CARTESIAN_POINT('Ctrl Pts',(-18.1436273509205,-29.0257231785076,
122.55092549477)) ;
#75261 = CARTESIAN_POINT('Ctrl Pts',(-18.3967545360288,-28.8457340980888,
122.723104052043)) ;
#75262 = CARTESIAN_POINT('Ctrl Pts',(-17.9253569900103,-29.0457777085066,
123.037111210468)) ;
#75263 = CARTESIAN_POINT('Ctrl Pts',(-18.2221384159378,-28.8657886280878,
123.112051915873)) ;
#75264 = CARTESIAN_POINT('Ctrl Pts',(-17.8864107135398,-29.0655852222666,
123.562230606213)) ;
#75265 = CARTESIAN_POINT('Ctrl Pts',(-18.1909813694771,-28.8855961418478,
123.532149866875)) ;
#75266 = CARTESIAN_POINT('Ctrl Pts',(-18.0291344864782,-29.0855685780343,
124.073742812793)) ;
#75267 = CARTESIAN_POINT('Ctrl Pts',(-18.3051612924804,-28.9055794976156,
123.941359571674)) ;
#75268 = CARTESIAN_POINT('Ctrl Pts',(-18.3375275326525,-29.1054868806182,
124.504029337566)) ;
#75269 = CARTESIAN_POINT('Ctrl Pts',(-18.5518768788528,-28.9254978001995,
124.285589192693)) ;
#75270 = CARTESIAN_POINT('Ctrl Pts',(-18.77243317676,-29.125355096064,124.803732067738)) ;
#75271 = CARTESIAN_POINT('Ctrl Pts',(-18.8998033875348,-28.9453660156452,
124.525350924034)) ;
#75272 = CARTESIAN_POINT('Ctrl Pts',(-19.288147951908,-29.1454054128603,124.937374691258)) ;
#75273 = CARTESIAN_POINT('Ctrl Pts',(-19.3123750642973,-28.9654163324415,
124.632263609282)) ;
#75274 = CARTESIAN_POINT('Ctrl Pts',(-19.8116842876808,-29.1651814747427,
124.888368150147)) ;
#75275 = CARTESIAN_POINT('Ctrl Pts',(-19.7312061711631,-28.985192394324,124.59305641669)) ;
#75276 = CARTESIAN_POINT('Ctrl Pts',(-20.2935470559917,-29.1852360804352,
124.661024000747)) ;
#75277 = CARTESIAN_POINT('Ctrl Pts',(-20.1166950466578,-29.0052470000165,
124.411179407397)) ;
#75278 = CARTESIAN_POINT('Ctrl Pts',(-20.6641709204991,-29.2050297695911,
124.28743570735)) ;
#75279 = CARTESIAN_POINT('Ctrl Pts',(-20.413193887911,-29.0250406891723,124.112305976162)) ;
#75280 = CARTESIAN_POINT('Ctrl Pts',(-20.8881946383036,-29.2249964611855,
123.806481690349)) ;
#75281 = CARTESIAN_POINT('Ctrl Pts',(-20.592410427374,-29.0450073807667,123.727541366071)) ;
#75282 = CARTESIAN_POINT('Ctrl Pts',(-20.9338249694019,-29.2449565069365,
123.277844260734)) ;
#75283 = CARTESIAN_POINT('Ctrl Pts',(-20.62891209658,-29.0649674265177,123.304630928054)) ;
#75284 = CARTESIAN_POINT('Ctrl Pts',(-20.7971171357436,-29.2648547670867,
122.766988876767)) ;
#75285 = CARTESIAN_POINT('Ctrl Pts',(-20.5195428530867,-29.084865686668,122.895946613903)) ;
#75286 = CARTESIAN_POINT('Ctrl Pts',(-20.4948597930559,-29.2847496826359,
122.333148374943)) ;
#75287 = CARTESIAN_POINT('Ctrl Pts',(-20.2777339778196,-29.1047606022171,
122.548875457773)) ;
#75288 = CARTESIAN_POINT('Ctrl Pts',(-20.0626359965353,-29.3046598630495,
122.027845909636)) ;
#75289 = CARTESIAN_POINT('Ctrl Pts',(-19.9319525576066,-29.1246707826307,
122.304635941344)) ;
#75290 = CARTESIAN_POINT('Ctrl Pts',(-19.551559332726,-29.3245956621637,121.887948224287)) ;
#75291 = CARTESIAN_POINT('Ctrl Pts',(-19.5230899669336,-29.144606581745,122.19272116096)) ;
#75292 = CARTESIAN_POINT('Ctrl Pts',(-19.0233846938504,-29.3445335238179,
121.930820616994)) ;
#75293 = CARTESIAN_POINT('Ctrl Pts',(-19.1005502612154,-29.1645444433991,
122.227022574999)) ;
#75294 = CARTESIAN_POINT('Ctrl Pts',(-18.5418309889257,-29.3644525704555,
122.150865733226)) ;
#75295 = CARTESIAN_POINT('Ctrl Pts',(-18.7153085362879,-29.1844634900368,
122.403062807844)) ;
#75296 = CARTESIAN_POINT('Ctrl Pts',(-18.1636813293389,-29.3844014685097,
122.522511403311)) ;
#75297 = CARTESIAN_POINT('Ctrl Pts',(-18.4127914568634,-29.2044123880909,
122.700380148177)) ;
#75298 = CARTESIAN_POINT('Ctrl Pts',(-17.9354075383592,-29.4043072959527,
122.999821271238)) ;
#75299 = CARTESIAN_POINT('Ctrl Pts',(-18.2301756194061,-29.224318215534,123.082237846385)) ;
#75300 = CARTESIAN_POINT('Ctrl Pts',(-17.8918934978953,-29.420889991318,123.438338526593)) ;
#75301 = CARTESIAN_POINT('Ctrl Pts',(-18.195368494416,-29.2409009108993,123.4330280738)) ;
#75302 = CARTESIAN_POINT('Ctrl Pts',(-17.9480247351245,-29.4341642050417,
123.782679410184)) ;
#75303 = CARTESIAN_POINT('Ctrl Pts',(-18.2402760241612,-29.2541751246229,
123.708522277928)) ;
#75304 = CARTESIAN_POINT('Ctrl Pts',(-18.035229582076,-29.444210924241,124.031850013666)) ;
#75305 = CARTESIAN_POINT('Ctrl Pts',(-18.3100397891959,-29.2642218438223,
123.907851739695)) ;
#75306 = CARTESIAN_POINT('Ctrl Pts',(-18.1615379686828,-29.4540549588867,
124.257627504395)) ;
#75307 = CARTESIAN_POINT('Ctrl Pts',(-18.4110966944545,-29.2740658784679,
124.088481420666)) ;
#75308 = CARTESIAN_POINT('Ctrl Pts',(-18.3825117400289,-29.4673893437912,
124.529570908601)) ;
#75309 = CARTESIAN_POINT('Ctrl Pts',(-18.587837079466,-29.2874002633725,124.305998087073)) ;
#75310 = CARTESIAN_POINT('Ctrl Pts',(-18.7397290348901,-29.483976561091,124.788022651573)) ;
#75311 = CARTESIAN_POINT('Ctrl Pts',(-18.8736672821377,-29.3039874806722,
124.512799388885)) ;
#75312 = CARTESIAN_POINT('Ctrl Pts',(-19.1646822605665,-29.5006097731289,
124.909710774663)) ;
#75313 = CARTESIAN_POINT('Ctrl Pts',(-19.2135860980992,-29.3206206927101,
124.610126710635)) ;
#75314 = CARTESIAN_POINT('Ctrl Pts',(-19.513720388534,-29.5138922154011,124.915596996218)) ;
#75315 = CARTESIAN_POINT('Ctrl Pts',(-19.4928464224192,-29.3339031349823,
124.614841247233)) ;
#75316 = CARTESIAN_POINT('Ctrl Pts',(-19.770872928767,-29.5237981033153,124.875254844447)) ;
#75317 = CARTESIAN_POINT('Ctrl Pts',(-19.6985621395063,-29.3438090228965,
124.582563747932)) ;
#75318 = CARTESIAN_POINT('Ctrl Pts',(-20.0193014854931,-29.5337865214204,
124.790472867308)) ;
#75319 = CARTESIAN_POINT('Ctrl Pts',(-19.8973061999821,-29.3537974410017,
124.51473599808)) ;
#75320 = CARTESIAN_POINT('Ctrl Pts',(-20.2499022752386,-29.5438099486591,
124.66315381133)) ;
#75321 = CARTESIAN_POINT('Ctrl Pts',(-20.0817838661683,-29.3638208682404,
124.412880687566)) ;
#75322 = CARTESIAN_POINT('Ctrl Pts',(-20.4525327560712,-29.5537143797761,
124.499823981661)) ;
#75323 = CARTESIAN_POINT('Ctrl Pts',(-20.2438922431529,-29.3737252993574,
124.282207749836)) ;
#75324 = CARTESIAN_POINT('Ctrl Pts',(-20.6825120255317,-29.5669775323866,
124.237867726883)) ;
#75325 = CARTESIAN_POINT('Ctrl Pts',(-20.4278473773578,-29.3869884519678,
124.072677218546)) ;
#75326 = CARTESIAN_POINT('Ctrl Pts',(-20.8392151517618,-29.5803024302904,
123.920338199531)) ;
#75327 = CARTESIAN_POINT('Ctrl Pts',(-20.553226732279,-29.4003133498717,123.818635845126)) ;
#75328 = CARTESIAN_POINT('Ctrl Pts',(-20.9074394905509,-29.5935581739061,
123.578684401658)) ;
#75329 = CARTESIAN_POINT('Ctrl Pts',(-20.6078059447763,-29.4135690934873,
123.545295374543)) ;
#75330 = CARTESIAN_POINT('Ctrl Pts',(-20.9137330389312,-29.6035175473534,
123.317072430937)) ;
#75331 = CARTESIAN_POINT('Ctrl Pts',(-20.6128379811963,-29.4235284669346,
123.336009184031)) ;
#75332 = CARTESIAN_POINT('Ctrl Pts',(-20.8748846542683,-29.6134613712803,
123.058630457431)) ;
#75333 = CARTESIAN_POINT('Ctrl Pts',(-20.5817571955094,-29.4334722908616,
123.129255093572)) ;
#75334 = CARTESIAN_POINT('Ctrl Pts',(-20.7906838438888,-29.6235093154276,
122.808386846947)) ;
#75335 = CARTESIAN_POINT('Ctrl Pts',(-20.5143943808657,-29.4435202350089,
122.929061213128)) ;
#75336 = CARTESIAN_POINT('Ctrl Pts',(-20.6669727396091,-29.6333602866458,
122.580969032594)) ;
#75337 = CARTESIAN_POINT('Ctrl Pts',(-20.4154235694875,-29.4533712062271,
122.747128058925)) ;
#75338 = CARTESIAN_POINT('Ctrl Pts',(-20.5042317391109,-29.6433321040879,
122.375617475146)) ;
#75339 = CARTESIAN_POINT('Ctrl Pts',(-20.285229061277,-29.4633430236691,122.582848300707)) ;
#75340 = CARTESIAN_POINT('Ctrl Pts',(-20.3077646578512,-29.65332752638,122.201218734674)) ;
#75341 = CARTESIAN_POINT('Ctrl Pts',(-20.1280539536979,-29.4733384459612,
122.443331024174)) ;
#75342 = CARTESIAN_POINT('Ctrl Pts',(-20.0830517817322,-29.6633605915037,
122.063322483004)) ;
#75343 = CARTESIAN_POINT('Ctrl Pts',(-19.9482825016034,-29.4833715110849,
122.333015964112)) ;
#75344 = CARTESIAN_POINT('Ctrl Pts',(-19.8419990548068,-29.6732259241689,
121.967921099616)) ;
#75345 = CARTESIAN_POINT('Ctrl Pts',(-19.7554396557229,-29.4932368437501,
122.256697012164)) ;
#75346 = CARTESIAN_POINT('Ctrl Pts',(-19.5857362753645,-29.6831864667665,
121.914563791479)) ;
#75347 = CARTESIAN_POINT('Ctrl Pts',(-19.5504291017455,-29.5031973863477,
122.214013362556)) ;
#75348 = CARTESIAN_POINT('Ctrl Pts',(-19.3221856204201,-29.6932201522682,
121.906899471653)) ;
#75349 = CARTESIAN_POINT('Ctrl Pts',(-19.3395885271886,-29.5132310718494,
122.207884142788)) ;
#75350 = CARTESIAN_POINT('Ctrl Pts',(-19.0650645565707,-29.7031049842585,
121.944106565248)) ;
#75351 = CARTESIAN_POINT('Ctrl Pts',(-19.1338922165619,-29.5231159038397,
122.237651976139)) ;
#75352 = CARTESIAN_POINT('Ctrl Pts',(-18.8138468784556,-29.7131724110183,
122.026926609353)) ;
#75353 = CARTESIAN_POINT('Ctrl Pts',(-18.9329187385003,-29.5331833305995,
122.303910131109)) ;
#75354 = CARTESIAN_POINT('Ctrl Pts',(-18.5859272207693,-29.7230109001771,
122.149077864709)) ;
#75355 = CARTESIAN_POINT('Ctrl Pts',(-18.7505843444716,-29.5430218197584,
122.401632918194)) ;
#75356 = CARTESIAN_POINT('Ctrl Pts',(-18.3778786570195,-29.7330743813672,
122.312276880573)) ;
#75357 = CARTESIAN_POINT('Ctrl Pts',(-18.5841468108762,-29.5530853009485,
122.532193870255)) ;
#75358 = CARTESIAN_POINT('Ctrl Pts',(-18.2044212592288,-29.7429685391823,
122.506008820016)) ;
#75359 = CARTESIAN_POINT('Ctrl Pts',(-18.4453827052769,-29.5629794587636,
122.687180688913)) ;
#75360 = CARTESIAN_POINT('Ctrl Pts',(-18.066004470774,-29.7529103959266,122.727551566426)) ;
#75361 = CARTESIAN_POINT('Ctrl Pts',(-18.334651204385,-29.5729213155079,122.864415841661)) ;
#75362 = CARTESIAN_POINT('Ctrl Pts',(-17.9674436495198,-29.7629128735981,
122.971267274074)) ;
#75363 = CARTESIAN_POINT('Ctrl Pts',(-18.255804547113,-29.5829237931793,123.059389144256)) ;
#75364 = CARTESIAN_POINT('Ctrl Pts',(-17.9129372901095,-29.7729476779024,
123.229259453653)) ;
#75365 = CARTESIAN_POINT('Ctrl Pts',(-18.2122015796833,-29.5929585974836,
123.265783349704)) ;
#75366 = CARTESIAN_POINT('Ctrl Pts',(-17.903787325648,-29.782792554748,123.487828320681)) ;
#75367 = CARTESIAN_POINT('Ctrl Pts',(-18.2048837514533,-29.6028034743293,
123.472638064826)) ;
#75368 = CARTESIAN_POINT('Ctrl Pts',(-17.9396889313481,-29.7927784343036,
123.747736250543)) ;
#75369 = CARTESIAN_POINT('Ctrl Pts',(-18.2336070824238,-29.6127893538848,
123.680563995791)) ;
#75370 = CARTESIAN_POINT('Ctrl Pts',(-18.0196096203183,-29.8027131646621,
123.99633015852)) ;
#75371 = CARTESIAN_POINT('Ctrl Pts',(-18.2975455112086,-29.6227240842433,
123.879438242773)) ;
#75372 = CARTESIAN_POINT('Ctrl Pts',(-18.1431663386496,-29.8127709769749,
124.229931834486)) ;
#75373 = CARTESIAN_POINT('Ctrl Pts',(-18.3963927784555,-29.6327818965562,
124.066318691056)) ;
#75374 = CARTESIAN_POINT('Ctrl Pts',(-18.3012830487224,-29.8225915690993,
124.433951656965)) ;
#75375 = CARTESIAN_POINT('Ctrl Pts',(-18.5228873635076,-29.6426024886806,
124.229532798967)) ;
#75376 = CARTESIAN_POINT('Ctrl Pts',(-18.4969190823567,-29.8326581547091,
124.611938648254)) ;
#75377 = CARTESIAN_POINT('Ctrl Pts',(-18.679397626606,-29.6526690742904,124.37192099675)) ;
#75378 = CARTESIAN_POINT('Ctrl Pts',(-18.7169004533169,-29.842557735291,124.750929340438)) ;
#75379 = CARTESIAN_POINT('Ctrl Pts',(-18.8553834510956,-29.6625686548722,
124.483111642557)) ;
#75380 = CARTESIAN_POINT('Ctrl Pts',(-18.9612300161898,-29.8526093349692,
124.851178041626)) ;
#75381 = CARTESIAN_POINT('Ctrl Pts',(-19.050847943237,-29.6726202545505,124.563308795822)) ;
#75382 = CARTESIAN_POINT('Ctrl Pts',(-19.2147547487761,-29.8624835213862,
124.906699600803)) ;
#75383 = CARTESIAN_POINT('Ctrl Pts',(-19.2536676428027,-29.6824944409674,
124.607724013081)) ;
#75384 = CARTESIAN_POINT('Ctrl Pts',(-19.4787496446866,-29.8725399972671,
124.917720031987)) ;
#75385 = CARTESIAN_POINT('Ctrl Pts',(-19.4648637461611,-29.6925509168483,
124.616538418507)) ;
#75386 = CARTESIAN_POINT('Ctrl Pts',(-19.7365039466666,-29.8824329285696,
124.883386677923)) ;
#75387 = CARTESIAN_POINT('Ctrl Pts',(-19.6710664653841,-29.7024438481509,
124.589069887457)) ;
#75388 = CARTESIAN_POINT('Ctrl Pts',(-19.9885582401288,-29.8924957072823,
124.803550123719)) ;
#75389 = CARTESIAN_POINT('Ctrl Pts',(-19.8727094596313,-29.7125066268636,
124.52519876481)) ;
#75390 = CARTESIAN_POINT('Ctrl Pts',(-20.2179182729885,-29.9023382328635,
124.68392271181)) ;
#75391 = CARTESIAN_POINT('Ctrl Pts',(-20.0561959904771,-29.7223491524447,
124.429495469086)) ;
#75392 = CARTESIAN_POINT('Ctrl Pts',(-20.4264420362818,-29.9123289982884,
124.52445158431)) ;
#75393 = CARTESIAN_POINT('Ctrl Pts',(-20.2230137897094,-29.7323399178696,
124.301917213795)) ;
#75394 = CARTESIAN_POINT('Ctrl Pts',(-20.602990790598,-29.9222570742864,124.332343420882)) ;
#75395 = CARTESIAN_POINT('Ctrl Pts',(-20.3642511922906,-29.7422679938676,
124.148229742484)) ;
#75396 = CARTESIAN_POINT('Ctrl Pts',(-20.7447343009426,-29.9322449846734,
124.111422181903)) ;
#75397 = CARTESIAN_POINT('Ctrl Pts',(-20.4776444559696,-29.7522559042547,
123.971491933959)) ;
#75398 = CARTESIAN_POINT('Ctrl Pts',(-20.8460304546489,-29.9422808967983,
123.867929241407)) ;
#75399 = CARTESIAN_POINT('Ctrl Pts',(-20.5586797287902,-29.7622918163796,
123.776696819529)) ;
#75400 = CARTESIAN_POINT('Ctrl Pts',(-20.9028976476815,-29.952135909646,123.615249639793)) ;
#75401 = CARTESIAN_POINT('Ctrl Pts',(-20.6041716209895,-29.7721468292273,
123.574553473142)) ;
#75402 = CARTESIAN_POINT('Ctrl Pts',(-20.9155677102884,-29.9621348555623,
123.352835793813)) ;
#75403 = CARTESIAN_POINT('Ctrl Pts',(-20.6143059849255,-29.7821457751435,
123.364622425134)) ;
#75404 = CARTESIAN_POINT('Ctrl Pts',(-20.8830605295313,-29.9720317680103,
123.094753953396)) ;
#75405 = CARTESIAN_POINT('Ctrl Pts',(-20.5882986910333,-29.7920426875915,
123.158157729796)) ;
#75406 = CARTESIAN_POINT('Ctrl Pts',(-20.8050694040147,-29.9820855661038,
122.842358190295)) ;
#75407 = CARTESIAN_POINT('Ctrl Pts',(-20.5259041888426,-29.802096485685,122.956241456897)) ;
#75408 = CARTESIAN_POINT('Ctrl Pts',(-20.6865523392665,-29.9919664869304,
122.611290225782)) ;
#75409 = CARTESIAN_POINT('Ctrl Pts',(-20.4310894079275,-29.8119774065117,
122.771388421395)) ;
#75410 = CARTESIAN_POINT('Ctrl Pts',(-20.5281670016261,-30.0019710129282,
122.401483413307)) ;
#75411 = CARTESIAN_POINT('Ctrl Pts',(-20.3043799645414,-29.8219819325095,
122.603543955252)) ;
#75412 = CARTESIAN_POINT('Ctrl Pts',(-20.3360451640972,-30.0119549765457,
122.222739387127)) ;
#75413 = CARTESIAN_POINT('Ctrl Pts',(-20.1506815650826,-29.8319658961269,
122.460549974152)) ;
#75414 = CARTESIAN_POINT('Ctrl Pts',(-20.1144958156019,-30.021994617097,122.079517699104)) ;
#75415 = CARTESIAN_POINT('Ctrl Pts',(-19.9734411337302,-29.8420055366782,
122.345973905275)) ;
#75416 = CARTESIAN_POINT('Ctrl Pts',(-19.8762838854864,-30.0318386427117,
121.978637774612)) ;
#75417 = CARTESIAN_POINT('Ctrl Pts',(-19.7828718281963,-29.8518495622929,
122.265271730029)) ;
#75418 = CARTESIAN_POINT('Ctrl Pts',(-19.620581079662,-30.041829648529,121.919049659256)) ;
#75419 = CARTESIAN_POINT('Ctrl Pts',(-19.5783094204032,-29.8618405681103,
122.217602616233)) ;
#75420 = CARTESIAN_POINT('Ctrl Pts',(-19.3571576412115,-30.0518674400612,
121.905299416059)) ;
#75421 = CARTESIAN_POINT('Ctrl Pts',(-19.3675704851451,-29.8718783596425,
122.206603915684)) ;
#75422 = CARTESIAN_POINT('Ctrl Pts',(-19.1003268168812,-30.0617118398496,
121.936426083641)) ;
#75423 = CARTESIAN_POINT('Ctrl Pts',(-19.1621069272286,-29.8817227594309,
122.231506534638)) ;
#75424 = CARTESIAN_POINT('Ctrl Pts',(-18.8491638610949,-30.0716966404063,
122.012238721602)) ;
#75425 = CARTESIAN_POINT('Ctrl Pts',(-18.9611771300981,-29.8917075599876,
122.292157833579)) ;
#75426 = CARTESIAN_POINT('Ctrl Pts',(-18.6159274222677,-30.0816361638175,
122.129904287685)) ;
#75427 = CARTESIAN_POINT('Ctrl Pts',(-18.774588942654,-29.9016470833988,122.386291228805)) ;
#75428 = CARTESIAN_POINT('Ctrl Pts',(-18.404637738631,-30.0916758829185,122.287871780177)) ;
#75429 = CARTESIAN_POINT('Ctrl Pts',(-18.6055578744043,-29.9116868024998,
122.512666327168)) ;
#75430 = CARTESIAN_POINT('Ctrl Pts',(-18.2265933389439,-30.1015640548378,
122.477161788277)) ;
#75431 = CARTESIAN_POINT('Ctrl Pts',(-18.4631237804811,-29.921574974419,122.664098660573)) ;
#75432 = CARTESIAN_POINT('Ctrl Pts',(-18.0822626445638,-30.1115536172548,
122.696428624397)) ;
#75433 = CARTESIAN_POINT('Ctrl Pts',(-18.3476602845798,-29.931564536836,122.839512622054)) ;
#75434 = CARTESIAN_POINT('Ctrl Pts',(-17.9786995241007,-30.1215119894495,
122.936755300678)) ;
#75435 = CARTESIAN_POINT('Ctrl Pts',(-18.2648110278588,-29.9415229090307,
123.031774118599)) ;
#75436 = CARTESIAN_POINT('Ctrl Pts',(-17.9181786121027,-30.1314120636802,
123.189791746342)) ;
#75437 = CARTESIAN_POINT('Ctrl Pts',(-18.2163954912986,-29.9514229832614,
123.234202841237)) ;
#75438 = CARTESIAN_POINT('Ctrl Pts',(-17.902317704542,-30.1414581600538,123.453303427387)) ;
#75439 = CARTESIAN_POINT('Ctrl Pts',(-18.2037078197734,-29.961469079635,123.445012405779)) ;
#75440 = CARTESIAN_POINT('Ctrl Pts',(-17.932026969616,-30.1513667440509,123.712002752088)) ;
#75441 = CARTESIAN_POINT('Ctrl Pts',(-18.2274762127078,-29.9713776636321,
123.651971093748)) ;
#75442 = CARTESIAN_POINT('Ctrl Pts',(-18.0064982864425,-30.1613773226418,
123.964313150641)) ;
#75443 = CARTESIAN_POINT('Ctrl Pts',(-18.2870541704328,-29.981388242223,123.853819106392)) ;
#75444 = CARTESIAN_POINT('Ctrl Pts',(-18.1243449647309,-30.1714064807546,
124.200064581394)) ;
#75445 = CARTESIAN_POINT('Ctrl Pts',(-18.3813325117191,-29.9914174003359,
124.042419843847)) ;
#75446 = CARTESIAN_POINT('Ctrl Pts',(-18.2782623863154,-30.1812593625927,
124.40825332171)) ;
#75447 = CARTESIAN_POINT('Ctrl Pts',(-18.5044666446186,-30.0012702821739,
124.208969431975)) ;
#75448 = CARTESIAN_POINT('Ctrl Pts',(-18.4674836004479,-30.1912189237437,
124.589086196472)) ;
#75449 = CARTESIAN_POINT('Ctrl Pts',(-18.6558438971189,-30.0112298433249,
124.35363489223)) ;
#75450 = CARTESIAN_POINT('Ctrl Pts',(-18.6871993887811,-30.2012573583328,
124.735052040816)) ;
#75451 = CARTESIAN_POINT('Ctrl Pts',(-18.8316171435154,-30.021268277914,124.470406880302)) ;
#75452 = CARTESIAN_POINT('Ctrl Pts',(-18.9248025260777,-30.2111306305599,
124.839385850432)) ;
#75453 = CARTESIAN_POINT('Ctrl Pts',(-19.0216991485207,-30.0311415501411,
124.553872836708)) ;
#75454 = CARTESIAN_POINT('Ctrl Pts',(-19.181943910287,-30.2212038725534,124.902021223961)) ;
#75455 = CARTESIAN_POINT('Ctrl Pts',(-19.2274127817706,-30.0412147921347,
124.603980422162)) ;
#75456 = CARTESIAN_POINT('Ctrl Pts',(-19.4395127810936,-30.2310242040865,
124.918975069685)) ;
#75457 = CARTESIAN_POINT('Ctrl Pts',(-19.433466684621,-30.0510351236678,124.617542685309)) ;
#75458 = CARTESIAN_POINT('Ctrl Pts',(-19.7027659038586,-30.2411028653133,
124.89046761584)) ;
#75459 = CARTESIAN_POINT('Ctrl Pts',(-19.6440694852678,-30.0611137848945,
124.594736008976)) ;
#75460 = CARTESIAN_POINT('Ctrl Pts',(-19.9514865660773,-30.2509544606075,
124.818398357358)) ;
#75461 = CARTESIAN_POINT('Ctrl Pts',(-19.8430448190709,-30.0709653801888,
124.537080268754)) ;
#75462 = CARTESIAN_POINT('Ctrl Pts',(-20.1891444820708,-30.2610275958363,
124.701927251156)) ;
#75463 = CARTESIAN_POINT('Ctrl Pts',(-20.0331712033916,-30.0810385154176,
124.44390269208)) ;
#75464 = CARTESIAN_POINT('Ctrl Pts',(-20.3981066042544,-30.2708700313613,
124.549458419437)) ;
#75465 = CARTESIAN_POINT('Ctrl Pts',(-20.2003396262217,-30.0908809509426,
124.321927803439)) ;
#75466 = CARTESIAN_POINT('Ctrl Pts',(-20.5805436588615,-30.2808508004947,
124.361037704467)) ;
#75467 = CARTESIAN_POINT('Ctrl Pts',(-20.3462888173977,-30.100861720076,124.171191137294)) ;
#75468 = CARTESIAN_POINT('Ctrl Pts',(-20.7276313527924,-30.2908679017386,
124.142726286171)) ;
#75469 = CARTESIAN_POINT('Ctrl Pts',(-20.4639585479526,-30.1108788213199,
123.99654171188)) ;
#75470 = CARTESIAN_POINT('Ctrl Pts',(-20.8336603364787,-30.3007563493404,
123.905461600846)) ;
#75471 = CARTESIAN_POINT('Ctrl Pts',(-20.5487810297276,-30.1207672689217,
123.806730589124)) ;
#75472 = CARTESIAN_POINT('Ctrl Pts',(-20.8979668750265,-30.3108120635213,
123.649176787993)) ;
#75473 = CARTESIAN_POINT('Ctrl Pts',(-20.6002259506018,-30.1308229831026,
123.601702402648)) ;
#75474 = CARTESIAN_POINT('Ctrl Pts',(-20.9165011055826,-30.3206872699351,
123.390311340075)) ;
#75475 = CARTESIAN_POINT('Ctrl Pts',(-20.6150528932545,-30.1406981895164,
123.39461094526)) ;
#75476 = CARTESIAN_POINT('Ctrl Pts',(-20.8901135578881,-30.3306823224079,
123.128988240044)) ;
#75477 = CARTESIAN_POINT('Ctrl Pts',(-20.5939426563615,-30.1506932419891,
123.185552627896)) ;
#75478 = CARTESIAN_POINT('Ctrl Pts',(-20.8181453544981,-30.34070420637,122.875637484416)) ;
#75479 = CARTESIAN_POINT('Ctrl Pts',(-20.5363677699957,-30.1607151259512,
122.982872078019)) ;
#75480 = CARTESIAN_POINT('Ctrl Pts',(-20.7048988528547,-30.3506081788993,
122.641302484531)) ;
#75481 = CARTESIAN_POINT('Ctrl Pts',(-20.4457706757612,-30.1706190984805,
122.795404879528)) ;
#75482 = CARTESIAN_POINT('Ctrl Pts',(-20.5516896930271,-30.3605966755602,
122.428164932621)) ;
#75483 = CARTESIAN_POINT('Ctrl Pts',(-20.3232033327596,-30.1806075951414,
122.624895080866)) ;
#75484 = CARTESIAN_POINT('Ctrl Pts',(-20.3641515811643,-30.3705604728081,
122.245458339218)) ;
#75485 = CARTESIAN_POINT('Ctrl Pts',(-20.17317296099,-30.1905713923894,122.478730202668)) ;
#75486 = CARTESIAN_POINT('Ctrl Pts',(-20.1493641424426,-30.3804644961162,
122.098426355277)) ;
#75487 = CARTESIAN_POINT('Ctrl Pts',(-20.0013436095708,-30.2004754156974,
122.361105071754)) ;
#75488 = CARTESIAN_POINT('Ctrl Pts',(-19.9085262576958,-30.3905249994378,
121.98944865862)) ;
#75489 = CARTESIAN_POINT('Ctrl Pts',(-19.8086730047828,-30.2105359190191,
122.273922884312)) ;
#75490 = CARTESIAN_POINT('Ctrl Pts',(-19.6580405513077,-30.4003655345777,
121.925039834699)) ;
#75491 = CARTESIAN_POINT('Ctrl Pts',(-19.6082855766348,-30.2203764541589,
122.222396127967)) ;
#75492 = CARTESIAN_POINT('Ctrl Pts',(-19.3944577950564,-30.4104277552823,
121.904320740001)) ;
#75493 = CARTESIAN_POINT('Ctrl Pts',(-19.3974190827422,-30.2304386748635,
122.205820754266)) ;
#75494 = CARTESIAN_POINT('Ctrl Pts',(-19.1355824753034,-30.4203249090585,
121.929541442094)) ;
#75495 = CARTESIAN_POINT('Ctrl Pts',(-19.1903196245163,-30.2403358286398,
122.225997234219)) ;
#75496 = CARTESIAN_POINT('Ctrl Pts',(-18.8839449757673,-30.430256042444,121.998725089926)) ;
#75497 = CARTESIAN_POINT('Ctrl Pts',(-18.9890101207813,-30.2502669620252,
122.281343781079)) ;
#75498 = CARTESIAN_POINT('Ctrl Pts',(-18.6456264179533,-30.4402984175897,
122.1120674788)) ;
#75499 = CARTESIAN_POINT('Ctrl Pts',(-18.7983550586508,-30.260309337171,122.372017626633)) ;
#75500 = CARTESIAN_POINT('Ctrl Pts',(-18.4338243468948,-30.4501843553558,
122.262533293048)) ;
#75501 = CARTESIAN_POINT('Ctrl Pts',(-18.6289139946321,-30.2701952749371,
122.492389609933)) ;
#75502 = CARTESIAN_POINT('Ctrl Pts',(-18.2490727523449,-30.4601801983407,
122.449233759721)) ;
#75503 = CARTESIAN_POINT('Ctrl Pts',(-18.4811126123803,-30.2801911179219,
122.641749654634)) ;
#75504 = CARTESIAN_POINT('Ctrl Pts',(-18.1003554685412,-30.4701221762193,
122.664059702214)) ;
#75505 = CARTESIAN_POINT('Ctrl Pts',(-18.3621388222961,-30.2901330958005,
122.813609831262)) ;
#75506 = CARTESIAN_POINT('Ctrl Pts',(-17.9906956059889,-30.4800815507003,
122.901684237762)) ;
#75507 = CARTESIAN_POINT('Ctrl Pts',(-18.2744107413088,-30.3000924702815,
123.003708954726)) ;
#75508 = CARTESIAN_POINT('Ctrl Pts',(-17.9235701572944,-30.490078166534,123.155692351254)) ;
#75509 = CARTESIAN_POINT('Ctrl Pts',(-18.2207100063737,-30.3100890861153,
123.206915221358)) ;
#75510 = CARTESIAN_POINT('Ctrl Pts',(-17.9018377986433,-30.5001123851076,
123.418476175523)) ;
#75511 = CARTESIAN_POINT('Ctrl Pts',(-18.203323782619,-30.3201233046888,123.417142364106)) ;
#75512 = CARTESIAN_POINT('Ctrl Pts',(-17.9253133851057,-30.5099654523182,
123.676335153518)) ;
#75513 = CARTESIAN_POINT('Ctrl Pts',(-18.2221037452179,-30.3299763718994,
123.623428491503)) ;
#75514 = CARTESIAN_POINT('Ctrl Pts',(-17.9932051453704,-30.5199257101958,
123.929113114996)) ;
#75515 = CARTESIAN_POINT('Ctrl Pts',(-18.2764164755412,-30.339936629777,123.825650660064)) ;
#75516 = CARTESIAN_POINT('Ctrl Pts',(-18.1050124820185,-30.5299547369014,
124.167789386628)) ;
#75517 = CARTESIAN_POINT('Ctrl Pts',(-18.3658619051834,-30.3499656564826,
124.016591970179)) ;
#75518 = CARTESIAN_POINT('Ctrl Pts',(-18.2546907014381,-30.5398649439358,
124.380895877624)) ;
#75519 = CARTESIAN_POINT('Ctrl Pts',(-18.4856036341333,-30.3598758635171,
124.18707690079)) ;
#75520 = CARTESIAN_POINT('Ctrl Pts',(-18.439085172546,-30.5497998545834,124.565733592048)) ;
#75521 = CARTESIAN_POINT('Ctrl Pts',(-18.633118334194,-30.3698107741647,124.334947200933)) ;
#75522 = CARTESIAN_POINT('Ctrl Pts',(-18.6551854058233,-30.5598409847626,
124.717139371071)) ;
#75523 = CARTESIAN_POINT('Ctrl Pts',(-18.805998270169,-30.3798519043439,124.456072442656)) ;
#75524 = CARTESIAN_POINT('Ctrl Pts',(-18.8905691521893,-30.5697281251326,
124.827187732262)) ;
#75525 = CARTESIAN_POINT('Ctrl Pts',(-18.994304219969,-30.3897390447139,124.544111408934)) ;
#75526 = CARTESIAN_POINT('Ctrl Pts',(-19.1440074490073,-30.5797204026685,
124.895826199271)) ;
#75527 = CARTESIAN_POINT('Ctrl Pts',(-19.1970544909255,-30.3997313222498,
124.599022913111)) ;
#75528 = CARTESIAN_POINT('Ctrl Pts',(-19.4044083048239,-30.5896689459369,
124.919242869025)) ;
#75529 = CARTESIAN_POINT('Ctrl Pts',(-19.405374674023,-30.4096798655181,124.61775698852)) ;
#75530 = CARTESIAN_POINT('Ctrl Pts',(-19.6646066985236,-30.5996056207541,
124.897490651065)) ;
#75531 = CARTESIAN_POINT('Ctrl Pts',(-19.6135329527055,-30.4196165403353,
124.600356125457)) ;
#75532 = CARTESIAN_POINT('Ctrl Pts',(-19.918388569691,-30.6095890416904,124.830870140945)) ;
#75533 = CARTESIAN_POINT('Ctrl Pts',(-19.816558494324,-30.4295999612717,124.547060681517)) ;
#75534 = CARTESIAN_POINT('Ctrl Pts',(-20.1579384638651,-30.6196313568797,
124.720177686915)) ;
#75535 = CARTESIAN_POINT('Ctrl Pts',(-20.0081988873676,-30.4396422764609,
124.458507428981)) ;
#75536 = CARTESIAN_POINT('Ctrl Pts',(-20.3705238610146,-30.6294716743189,
124.572936951998)) ;
#75537 = CARTESIAN_POINT('Ctrl Pts',(-20.1782668479969,-30.4494825939001,
124.340716237617)) ;
#75538 = CARTESIAN_POINT('Ctrl Pts',(-20.5582851076625,-30.6395013783764,
124.387959911848)) ;
#75539 = CARTESIAN_POINT('Ctrl Pts',(-20.3284766672307,-30.4595122979576,
124.192735318187)) ;
#75540 = CARTESIAN_POINT('Ctrl Pts',(-20.7103623023871,-30.6495223350989,
124.1729709106)) ;
#75541 = CARTESIAN_POINT('Ctrl Pts',(-20.450139188978,-30.4695332546801,124.020744631255)) ;
#75542 = CARTESIAN_POINT('Ctrl Pts',(-20.8216762307173,-30.6593888774025,
123.938777584524)) ;
#75543 = CARTESIAN_POINT('Ctrl Pts',(-20.5391909126625,-30.4793997969837,
123.833391248542)) ;
#75544 = CARTESIAN_POINT('Ctrl Pts',(-20.8920560098693,-30.6694599773476,
123.683674797195)) ;
#75545 = CARTESIAN_POINT('Ctrl Pts',(-20.5954958516475,-30.4894708969289,
123.629309014543)) ;
#75546 = CARTESIAN_POINT('Ctrl Pts',(-20.9165006065957,-30.6793020515252,
123.426182698947)) ;
#75547 = CARTESIAN_POINT('Ctrl Pts',(-20.6150525003073,-30.4993129711065,
123.423316470327)) ;
#75548 = CARTESIAN_POINT('Ctrl Pts',(-20.8965796707046,-30.6892628461122,
123.165188338051)) ;
#75549 = CARTESIAN_POINT('Ctrl Pts',(-20.5991170611532,-30.5092737656935,
123.214521207781)) ;
#75550 = CARTESIAN_POINT('Ctrl Pts',(-20.8306367979859,-30.6993007190131,
122.909788435408)) ;
#75551 = CARTESIAN_POINT('Ctrl Pts',(-20.5463638720667,-30.5193116385943,
123.010200889343)) ;
#75552 = CARTESIAN_POINT('Ctrl Pts',(-20.7235512012053,-30.7091750045571,
122.673393853089)) ;
#75553 = CARTESIAN_POINT('Ctrl Pts',(-20.4606968923866,-30.5291859241384,
122.821085433644)) ;
#75554 = CARTESIAN_POINT('Ctrl Pts',(-20.5741723490005,-30.7192447549711,
122.455008665901)) ;
#75555 = CARTESIAN_POINT('Ctrl Pts',(-20.3411947055965,-30.5392556745523,
122.646376333744)) ;
#75556 = CARTESIAN_POINT('Ctrl Pts',(-20.3935486501348,-30.7290780395057,
122.270181067648)) ;
#75557 = CARTESIAN_POINT('Ctrl Pts',(-20.1966973937778,-30.549088959087,122.498514076006)) ;
#75558 = CARTESIAN_POINT('Ctrl Pts',(-20.1798297267622,-30.7391083803058,
122.115914599619)) ;
#75559 = CARTESIAN_POINT('Ctrl Pts',(-20.0257230530562,-30.559119299887,122.375099677665)) ;
#75560 = CARTESIAN_POINT('Ctrl Pts',(-19.9421798972876,-30.7491403043054,
122.001770363391)) ;
#75561 = CARTESIAN_POINT('Ctrl Pts',(-19.8356036909516,-30.5691512238866,
122.28378308955)) ;
#75562 = CARTESIAN_POINT('Ctrl Pts',(-19.6936420289433,-30.7589688392413,
121.931532551755)) ;
#75563 = CARTESIAN_POINT('Ctrl Pts',(-19.6367747626622,-30.5789797588226,
122.227591754788)) ;
#75564 = CARTESIAN_POINT('Ctrl Pts',(-19.4324272173861,-30.768962617006,121.90436106235)) ;
#75565 = CARTESIAN_POINT('Ctrl Pts',(-19.4278031940052,-30.5889735365872,
122.205853025448)) ;
#75566 = CARTESIAN_POINT('Ctrl Pts',(-19.1696001927658,-30.7789903274915,
121.923539411907)) ;
#75567 = CARTESIAN_POINT('Ctrl Pts',(-19.2175414369296,-30.5990012470728,
122.221194254643)) ;
#75568 = CARTESIAN_POINT('Ctrl Pts',(-18.9175710994539,-30.7888787383255,
121.98685039034)) ;
#75569 = CARTESIAN_POINT('Ctrl Pts',(-19.0159184367103,-30.6088896579067,
122.271841400405)) ;
#75570 = CARTESIAN_POINT('Ctrl Pts',(-18.6780751167971,-30.798855588861,122.093481958298)) ;
#75571 = CARTESIAN_POINT('Ctrl Pts',(-18.8243211846636,-30.6188665084423,
122.357145104466)) ;
#75572 = CARTESIAN_POINT('Ctrl Pts',(-18.4603462227965,-30.8088473854115,
122.240311680706)) ;
#75573 = CARTESIAN_POINT('Ctrl Pts',(-18.6501372714632,-30.6288583049927,
122.474607479311)) ;
#75574 = CARTESIAN_POINT('Ctrl Pts',(-18.2708493729533,-30.8188833915051,
122.423713476648)) ;
#75575 = CARTESIAN_POINT('Ctrl Pts',(-18.4985386630892,-30.6388943110864,
122.621327853477)) ;
#75576 = CARTESIAN_POINT('Ctrl Pts',(-18.1185854662254,-30.828734125768,122.633088418397)) ;
#75577 = CARTESIAN_POINT('Ctrl Pts',(-18.376726707459,-30.6487450453492,122.788826190101)) ;
#75578 = CARTESIAN_POINT('Ctrl Pts',(-18.0029869057309,-30.8387253842962,
122.86878945056)) ;
#75579 = CARTESIAN_POINT('Ctrl Pts',(-18.2842463850415,-30.6587363038774,
122.97738614376)) ;
#75580 = CARTESIAN_POINT('Ctrl Pts',(-17.9304364000927,-30.8486432791994,
123.119155041254)) ;
#75581 = CARTESIAN_POINT('Ctrl Pts',(-18.2262044469805,-30.6686541987806,
123.177677695621)) ;
#75582 = CARTESIAN_POINT('Ctrl Pts',(-17.9020877613563,-30.8586714208624,
123.381133283298)) ;
#75583 = CARTESIAN_POINT('Ctrl Pts',(-18.2035238003672,-30.6786823404437,
123.387260129306)) ;
#75584 = CARTESIAN_POINT('Ctrl Pts',(-17.9193001863973,-30.8685565889783,
123.640341140636)) ;
#75585 = CARTESIAN_POINT('Ctrl Pts',(-18.2172919455385,-30.6885675085595,
123.594625944928)) ;
#75586 = CARTESIAN_POINT('Ctrl Pts',(-17.9812908654965,-30.8785459524843,
123.895432047581)) ;
#75587 = CARTESIAN_POINT('Ctrl Pts',(-18.2668826491316,-30.6985568720655,
123.798698988406)) ;
#75588 = CARTESIAN_POINT('Ctrl Pts',(-18.0876859530598,-30.8885870874943,
124.136901868382)) ;
#75589 = CARTESIAN_POINT('Ctrl Pts',(-18.3519971252596,-30.7085980070756,
123.991875626918)) ;
#75590 = CARTESIAN_POINT('Ctrl Pts',(-18.2309896742037,-30.8984197556824,
124.351909547768)) ;
#75591 = CARTESIAN_POINT('Ctrl Pts',(-18.4666381458969,-30.7184306752636,
124.163882156588)) ;
#75592 = CARTESIAN_POINT('Ctrl Pts',(-18.4118327451986,-30.9084136586368,
124.542354351719)) ;
#75593 = CARTESIAN_POINT('Ctrl Pts',(-18.6113111190892,-30.7284245782181,
124.316239274634)) ;
#75594 = CARTESIAN_POINT('Ctrl Pts',(-18.6240784847576,-30.9184429437214,
124.698611210616)) ;
#75595 = CARTESIAN_POINT('Ctrl Pts',(-18.78110661491,-30.7384538633026,124.441246278568)) ;
#75596 = CARTESIAN_POINT('Ctrl Pts',(-18.8564336547717,-30.9283184721633,
124.814232094013)) ;
#75597 = CARTESIAN_POINT('Ctrl Pts',(-18.96698940901,-30.7483293917445,124.533744474627)) ;
#75598 = CARTESIAN_POINT('Ctrl Pts',(-19.1083519713404,-30.9383187547793,
124.888948210895)) ;
#75599 = CARTESIAN_POINT('Ctrl Pts',(-19.168523414082,-30.7583296743606,124.593519235513)) ;
#75600 = CARTESIAN_POINT('Ctrl Pts',(-19.3671515658178,-30.9482307708364,
124.918740815802)) ;
#75601 = CARTESIAN_POINT('Ctrl Pts',(-19.3755624914892,-30.7682416904176,
124.617355261869)) ;
#75602 = CARTESIAN_POINT('Ctrl Pts',(-19.6305583756984,-30.9582728461754,
124.903010863117)) ;
#75603 = CARTESIAN_POINT('Ctrl Pts',(-19.5862881163539,-30.7782837657566,
124.604773299001)) ;
#75604 = CARTESIAN_POINT('Ctrl Pts',(-19.883627140372,-30.9681726788315,124.842636497085)) ;
#75605 = CARTESIAN_POINT('Ctrl Pts',(-19.7887432076105,-30.7881835984127,
124.55647584906)) ;
#75606 = CARTESIAN_POINT('Ctrl Pts',(-20.1248202353474,-30.9781650794095,
124.738811837768)) ;
#75607 = CARTESIAN_POINT('Ctrl Pts',(-19.9816984157365,-30.7981759989908,
124.473418063959)) ;
#75608 = CARTESIAN_POINT('Ctrl Pts',(-20.3449819506754,-30.9881991011689,
124.593690835945)) ;
#75609 = CARTESIAN_POINT('Ctrl Pts',(-20.157828908641,-30.8082100207501,124.357322942106)) ;
#75610 = CARTESIAN_POINT('Ctrl Pts',(-20.5335886315247,-30.9980637120101,
124.415853378469)) ;
#75611 = CARTESIAN_POINT('Ctrl Pts',(-20.3087153229984,-30.8180746315913,
124.215054797051)) ;
#75612 = CARTESIAN_POINT('Ctrl Pts',(-20.6909778266609,-31.0080561114712,
124.205652827194)) ;
#75613 = CARTESIAN_POINT('Ctrl Pts',(-20.4346283289395,-30.8280670310525,
124.046895699291)) ;
#75614 = CARTESIAN_POINT('Ctrl Pts',(-20.8094832863514,-31.0180880648041,
123.970160489442)) ;
#75615 = CARTESIAN_POINT('Ctrl Pts',(-20.5294345476933,-30.8380989843854,
123.85850276039)) ;
#75616 = CARTESIAN_POINT('Ctrl Pts',(-20.8844320813034,-31.0279544237458,
123.721940205745)) ;
#75617 = CARTESIAN_POINT('Ctrl Pts',(-20.5893954864046,-30.8479653433271,
123.659927538539)) ;
#75618 = CARTESIAN_POINT('Ctrl Pts',(-20.9159397609847,-31.0379418992316,
123.461410041661)) ;
#75619 = CARTESIAN_POINT('Ctrl Pts',(-20.6146037560401,-30.8579528188129,
123.451503763144)) ;
#75620 = CARTESIAN_POINT('Ctrl Pts',(-20.901928788736,-31.0478868054201,123.200405236566)) ;
#75621 = CARTESIAN_POINT('Ctrl Pts',(-20.6033971453962,-30.8678977250013,
123.242699989987)) ;
#75622 = CARTESIAN_POINT('Ctrl Pts',(-20.8420850391347,-31.0579317700803,
122.943333258404)) ;
#75623 = CARTESIAN_POINT('Ctrl Pts',(-20.5555242372743,-30.8779426896616,
123.037041905058)) ;
#75624 = CARTESIAN_POINT('Ctrl Pts',(-20.740600364807,-31.0677935769852,122.704848430395)) ;
#75625 = CARTESIAN_POINT('Ctrl Pts',(-20.4743386257341,-30.8878044965664,
122.846253507543)) ;
#75626 = CARTESIAN_POINT('Ctrl Pts',(-20.5978221441658,-31.0777862492909,
122.484491140216)) ;
#75627 = CARTESIAN_POINT('Ctrl Pts',(-20.3601179413071,-30.8977971688722,
122.669966539594)) ;
#75628 = CARTESIAN_POINT('Ctrl Pts',(-20.4200444703825,-31.0877149202363,
122.293491950939)) ;
#75629 = CARTESIAN_POINT('Ctrl Pts',(-20.2178975346058,-30.9077258398175,
122.517165820862)) ;
#75630 = CARTESIAN_POINT('Ctrl Pts',(-20.2115893828335,-31.0976674624616,
122.135563380037)) ;
#75631 = CARTESIAN_POINT('Ctrl Pts',(-20.0511349097933,-30.9176783820428,
122.390821266279)) ;
#75632 = CARTESIAN_POINT('Ctrl Pts',(-19.9777608298646,-31.1076688184575,
122.015498299293)) ;
#75633 = CARTESIAN_POINT('Ctrl Pts',(-19.864073138811,-30.9276797380387,122.29476724589)) ;
#75634 = CARTESIAN_POINT('Ctrl Pts',(-19.72588370907,-31.1176974307322,121.938001760839)) ;
#75635 = CARTESIAN_POINT('Ctrl Pts',(-19.6625721285863,-30.9377083503134,
122.2327679101)) ;
#75636 = CARTESIAN_POINT('Ctrl Pts',(-19.4686784023186,-31.1275617652817,
121.905569609701)) ;
#75637 = CARTESIAN_POINT('Ctrl Pts',(-19.4568083670694,-30.9475726848629,
122.206820002847)) ;
#75638 = CARTESIAN_POINT('Ctrl Pts',(-19.2064222623086,-31.1375540893583,
121.918044378352)) ;
#75639 = CARTESIAN_POINT('Ctrl Pts',(-19.2470034110608,-30.9575650089395,
122.21679756988)) ;
#75640 = CARTESIAN_POINT('Ctrl Pts',(-18.9518724579804,-31.1474815817241,
121.975353810709)) ;
#75641 = CARTESIAN_POINT('Ctrl Pts',(-19.043363176175,-30.9674925013054,122.262642901527)) ;
#75642 = CARTESIAN_POINT('Ctrl Pts',(-18.7087875924744,-31.157508940275,122.076985697082)) ;
#75643 = CARTESIAN_POINT('Ctrl Pts',(-18.8488944626726,-30.9775198598562,
122.343946315082)) ;
#75644 = CARTESIAN_POINT('Ctrl Pts',(-18.489949403091,-31.1673953583261,122.217086575925)) ;
#75645 = CARTESIAN_POINT('Ctrl Pts',(-18.6738227767691,-30.9874062779074,
122.456025072437)) ;
#75646 = CARTESIAN_POINT('Ctrl Pts',(-18.2959218217768,-31.1774270930615,
122.395489361703)) ;
#75647 = CARTESIAN_POINT('Ctrl Pts',(-18.5185992246313,-30.9974380126427,
122.59874560302)) ;
#75648 = CARTESIAN_POINT('Ctrl Pts',(-18.1379570317047,-31.1873086743047,
122.601654224037)) ;
#75649 = CARTESIAN_POINT('Ctrl Pts',(-18.3922256360828,-31.007319593886,122.763676083483)) ;
#75650 = CARTESIAN_POINT('Ctrl Pts',(-18.0159864387132,-31.1973706523371,
122.836214609543)) ;
#75651 = CARTESIAN_POINT('Ctrl Pts',(-18.2946471919646,-31.0173815719183,
122.951323289987)) ;
#75652 = CARTESIAN_POINT('Ctrl Pts',(-17.9380997061781,-31.2072277306988,
123.083299705071)) ;
#75653 = CARTESIAN_POINT('Ctrl Pts',(-18.2323356602816,-31.02723865028,123.148990682481)) ;
#75654 = CARTESIAN_POINT('Ctrl Pts',(-17.9033134791433,-31.2172223038048,
123.343589981841)) ;
#75655 = CARTESIAN_POINT('Ctrl Pts',(-18.204504458958,-31.037233223386,123.357222569661)) ;
#75656 = CARTESIAN_POINT('Ctrl Pts',(-17.9140838362629,-31.2271481000924,
123.604243273491)) ;
#75657 = CARTESIAN_POINT('Ctrl Pts',(-18.2131185010766,-31.0471590196736,
123.565745298409)) ;
#75658 = CARTESIAN_POINT('Ctrl Pts',(-17.9704288396059,-31.2371734672621,
123.861581949271)) ;
#75659 = CARTESIAN_POINT('Ctrl Pts',(-18.2581923330531,-31.0571843868434,
123.77161667508)) ;
#75660 = CARTESIAN_POINT('Ctrl Pts',(-18.0692181289341,-31.247069546916,124.102157307111)) ;
#75661 = CARTESIAN_POINT('Ctrl Pts',(-18.3372216027186,-31.0670804664972,
123.964077752132)) ;
#75662 = CARTESIAN_POINT('Ctrl Pts',(-18.2092168772367,-31.2570646266215,
124.324401075044)) ;
#75663 = CARTESIAN_POINT('Ctrl Pts',(-18.4492191754673,-31.0770755462028,
124.141874372406)) ;
#75664 = CARTESIAN_POINT('Ctrl Pts',(-18.3865390045604,-31.2670897144374,
124.519239586953)) ;
#75665 = CARTESIAN_POINT('Ctrl Pts',(-18.5910734554309,-31.0871006340186,
124.297744917431)) ;
#75666 = CARTESIAN_POINT('Ctrl Pts',(-18.6602990640398,-31.2802735368046,
124.731576473169)) ;
#75667 = CARTESIAN_POINT('Ctrl Pts',(-18.8100883440291,-31.1002844563859,
124.46762529973)) ;
#75668 = CARTESIAN_POINT('Ctrl Pts',(-18.9862948594046,-31.2935956549506,
124.869711357403)) ;
#75669 = CARTESIAN_POINT('Ctrl Pts',(-19.0709153826081,-31.1136065745318,
124.578138411476)) ;
#75670 = CARTESIAN_POINT('Ctrl Pts',(-19.3347015527529,-31.3069748645782,
124.917347223271)) ;
#75671 = CARTESIAN_POINT('Ctrl Pts',(-19.3495941692662,-31.1269857841594,
124.616238563571)) ;
#75672 = CARTESIAN_POINT('Ctrl Pts',(-19.5930836021326,-31.3168131018224,
124.908057132402)) ;
#75673 = CARTESIAN_POINT('Ctrl Pts',(-19.5563095018621,-31.1368240214036,
124.608810852484)) ;
#75674 = CARTESIAN_POINT('Ctrl Pts',(-19.8519437779512,-31.3268860250811,
124.852876717785)) ;
#75675 = CARTESIAN_POINT('Ctrl Pts',(-19.7633952063794,-31.1468969446624,
124.564668365869)) ;
#75676 = CARTESIAN_POINT('Ctrl Pts',(-20.0920602273385,-31.3367426665362,
124.755670606762)) ;
#75677 = CARTESIAN_POINT('Ctrl Pts',(-19.9554908730702,-31.1567535861175,
124.486904328256)) ;
#75678 = CARTESIAN_POINT('Ctrl Pts',(-20.3148623984848,-31.3467280420423,
124.617067390119)) ;
#75679 = CARTESIAN_POINT('Ctrl Pts',(-20.1337308377886,-31.1667389616235,
124.376027861451)) ;
#75680 = CARTESIAN_POINT('Ctrl Pts',(-20.5745088880156,-31.3600120735027,
124.383813943034)) ;
#75681 = CARTESIAN_POINT('Ctrl Pts',(-20.3414635227013,-31.180022993084,124.18940523939)) ;
#75682 = CARTESIAN_POINT('Ctrl Pts',(-20.8154916493389,-31.376530865373,124.016626072698)) ;
#75683 = CARTESIAN_POINT('Ctrl Pts',(-20.5342357532926,-31.1965417849543,
123.895695702942)) ;
#75684 = CARTESIAN_POINT('Ctrl Pts',(-20.917307049365,-31.3933165823797,123.582394229594)) ;
#75685 = CARTESIAN_POINT('Ctrl Pts',(-20.6157025962168,-31.2133275019609,
123.548246263072)) ;
#75686 = CARTESIAN_POINT('Ctrl Pts',(-20.90651529499,-31.4064297308887,123.237879258047)) ;
#75687 = CARTESIAN_POINT('Ctrl Pts',(-20.6070652302265,-31.2264406504699,
123.272686121829)) ;
#75688 = CARTESIAN_POINT('Ctrl Pts',(-20.8536524124441,-31.4164652799689,
122.979546305383)) ;
#75689 = CARTESIAN_POINT('Ctrl Pts',(-20.56477758318,-31.2364761995501,123.066008431127)) ;
#75690 = CARTESIAN_POINT('Ctrl Pts',(-20.7561932614657,-31.4264813361483,
122.735008678748)) ;
#75691 = CARTESIAN_POINT('Ctrl Pts',(-20.4868138633641,-31.2464922557295,
122.870382595949)) ;
#75692 = CARTESIAN_POINT('Ctrl Pts',(-20.574735633146,-31.4396593720143,122.440107128118)) ;
#75693 = CARTESIAN_POINT('Ctrl Pts',(-20.3416392942912,-31.2596702915955,
122.634448243853)) ;
#75694 = CARTESIAN_POINT('Ctrl Pts',(-20.2550642401777,-31.4562612492014,
122.135837120559)) ;
#75695 = CARTESIAN_POINT('Ctrl Pts',(-20.0859155602014,-31.2762721687826,
122.391041933051)) ;
#75696 = CARTESIAN_POINT('Ctrl Pts',(-19.7659328720119,-31.4763243938173,
121.923514400655)) ;
#75697 = CARTESIAN_POINT('Ctrl Pts',(-19.6946085896363,-31.2963353133985,
122.221176679855)) ;
#75698 = CARTESIAN_POINT('Ctrl Pts',(-19.2406043647769,-31.496125283901,121.890949553515)) ;
#75699 = CARTESIAN_POINT('Ctrl Pts',(-19.2743458623151,-31.3161362034822,
122.195122232715)) ;
#75700 = CARTESIAN_POINT('Ctrl Pts',(-18.7318418664049,-31.5160684091797,
122.039356586139)) ;
#75701 = CARTESIAN_POINT('Ctrl Pts',(-18.8673343450499,-31.3360793287609,
122.313844690629)) ;
#75702 = CARTESIAN_POINT('Ctrl Pts',(-18.3053752398977,-31.5359664542993,
122.35209220287)) ;
#75703 = CARTESIAN_POINT('Ctrl Pts',(-18.5261587181132,-31.3559773738805,
122.564031167843)) ;
#75704 = CARTESIAN_POINT('Ctrl Pts',(-18.010266411361,-31.555852213926,122.79064987689)) ;
#75705 = CARTESIAN_POINT('Ctrl Pts',(-18.2900689875788,-31.3758631335073,
122.914876579139)) ;
#75706 = CARTESIAN_POINT('Ctrl Pts',(-17.8822137796121,-31.5759173891059,
123.308303291764)) ;
#75707 = CARTESIAN_POINT('Ctrl Pts',(-18.1876243873306,-31.3959283086872,
123.328998110787)) ;
#75708 = CARTESIAN_POINT('Ctrl Pts',(-17.9380242802495,-31.5957440322087,
123.832388879127)) ;
#75709 = CARTESIAN_POINT('Ctrl Pts',(-18.2322702877505,-31.41575495179,123.748268249303)) ;
#75710 = CARTESIAN_POINT('Ctrl Pts',(-18.1688732799424,-31.6156527416571,
124.308361931738)) ;
#75711 = CARTESIAN_POINT('Ctrl Pts',(-18.4169480416883,-31.4356636612383,
124.129048386258)) ;
#75712 = CARTESIAN_POINT('Ctrl Pts',(-18.5492284834429,-31.6356045786889,
124.678079899734)) ;
#75713 = CARTESIAN_POINT('Ctrl Pts',(-18.7212312265001,-31.4556154982701,
124.424824341634)) ;
#75714 = CARTESIAN_POINT('Ctrl Pts',(-19.0344540489787,-31.655613053392,124.895564294093)) ;
#75715 = CARTESIAN_POINT('Ctrl Pts',(-19.1094107625724,-31.4756239729733,
124.598813645085)) ;
#75716 = CARTESIAN_POINT('Ctrl Pts',(-19.5593044714974,-31.6754145121535,
124.9346386812)) ;
#75717 = CARTESIAN_POINT('Ctrl Pts',(-19.529293065133,-31.4954254317348,124.630074897987)) ;
#75718 = CARTESIAN_POINT('Ctrl Pts',(-20.0703188207623,-31.6953714003894,
124.792477849168)) ;
#75719 = CARTESIAN_POINT('Ctrl Pts',(-19.9381052599703,-31.5153823199707,
124.516346913691)) ;
#75720 = CARTESIAN_POINT('Ctrl Pts',(-20.5020147231409,-31.7153552378035,
124.483083841994)) ;
#75721 = CARTESIAN_POINT('Ctrl Pts',(-20.2834628020649,-31.5353661573848,
124.268832576871)) ;
#75722 = CARTESIAN_POINT('Ctrl Pts',(-20.8005129694073,-31.7351636770245,
124.049324638375)) ;
#75723 = CARTESIAN_POINT('Ctrl Pts',(-20.5222631468944,-31.5551745966057,
123.921823569577)) ;
#75724 = CARTESIAN_POINT('Ctrl Pts',(-20.9347328466543,-31.7551493864047,
123.535538119664)) ;
#75725 = CARTESIAN_POINT('Ctrl Pts',(-20.629639166781,-31.5751603059859,123.510794112745)) ;
#75726 = CARTESIAN_POINT('Ctrl Pts',(-20.8859933952237,-31.77501890942,123.009476827428)) ;
#75727 = CARTESIAN_POINT('Ctrl Pts',(-20.5906472054233,-31.5950298290012,
123.089943545706)) ;
#75728 = CARTESIAN_POINT('Ctrl Pts',(-20.6589290213738,-31.7950396485372,
122.528458277119)) ;
#75729 = CARTESIAN_POINT('Ctrl Pts',(-20.4089954572022,-31.6150505681184,
122.705129026127)) ;
#75730 = CARTESIAN_POINT('Ctrl Pts',(-20.2856318117537,-31.8148437135141,
122.157092624958)) ;
#75731 = CARTESIAN_POINT('Ctrl Pts',(-20.1103554752544,-31.6348546330954,
122.408035494353)) ;
#75732 = CARTESIAN_POINT('Ctrl Pts',(-19.8021889397238,-31.8349056772449,
121.932500294407)) ;
#75733 = CARTESIAN_POINT('Ctrl Pts',(-19.7236013288936,-31.6549165968261,
122.228362959859)) ;
#75734 = CARTESIAN_POINT('Ctrl Pts',(-19.2768672597624,-31.8547388575334,
121.887382590685)) ;
#75735 = CARTESIAN_POINT('Ctrl Pts',(-19.3033420853306,-31.6747497771146,
122.192269707988)) ;
#75736 = CARTESIAN_POINT('Ctrl Pts',(-18.7652950498468,-31.8746580548595,
122.023339535084)) ;
#75737 = CARTESIAN_POINT('Ctrl Pts',(-18.894083985732,-31.6946689744407,122.301037293139)) ;
#75738 = CARTESIAN_POINT('Ctrl Pts',(-18.3305352276094,-31.8945960799728,
122.326324931623)) ;
#75739 = CARTESIAN_POINT('Ctrl Pts',(-18.5462767220526,-31.714606999554,122.543427492195)) ;
#75740 = CARTESIAN_POINT('Ctrl Pts',(-18.0255423059976,-31.9144741260288,
122.757789608144)) ;
#75741 = CARTESIAN_POINT('Ctrl Pts',(-18.3022836422757,-31.7344850456101,
122.888601425754)) ;
#75742 = CARTESIAN_POINT('Ctrl Pts',(-17.8853325730449,-31.9344588603169,
123.270040998402)) ;
#75743 = CARTESIAN_POINT('Ctrl Pts',(-18.190118198044,-31.7544697798982,123.298403291928)) ;
#75744 = CARTESIAN_POINT('Ctrl Pts',(-17.928106557401,-31.9543696769954,123.797659471947)) ;
#75745 = CARTESIAN_POINT('Ctrl Pts',(-18.2243400264694,-31.7743805965766,
123.720498525304)) ;
#75746 = CARTESIAN_POINT('Ctrl Pts',(-18.1495333781648,-31.9743686525141,
124.280744001263)) ;
#75747 = CARTESIAN_POINT('Ctrl Pts',(-18.4014839037645,-31.7943795720954,
124.106965091444)) ;
#75748 = CARTESIAN_POINT('Ctrl Pts',(-18.5185878610474,-31.9941735731593,
124.656228575468)) ;
#75749 = CARTESIAN_POINT('Ctrl Pts',(-18.6967305737938,-31.8141844927406,
124.407351675959)) ;
#75750 = CARTESIAN_POINT('Ctrl Pts',(-18.9973682959975,-32.0141575334505,
124.885894562738)) ;
#75751 = CARTESIAN_POINT('Ctrl Pts',(-19.0797564164797,-31.8341684530318,
124.59108154804)) ;
#75752 = CARTESIAN_POINT('Ctrl Pts',(-19.5234477413655,-32.0340437371745,
124.937928873711)) ;
#75753 = CARTESIAN_POINT('Ctrl Pts',(-19.5006209678039,-31.8540546567557,
124.632705726637)) ;
#75754 = CARTESIAN_POINT('Ctrl Pts',(-20.0373301586024,-32.0539929154977,
124.807521706243)) ;
#75755 = CARTESIAN_POINT('Ctrl Pts',(-19.9117263038171,-31.8740038350789,
124.528376628622)) ;
#75756 = CARTESIAN_POINT('Ctrl Pts',(-20.4747803851677,-32.0738947147372,
124.510171457497)) ;
#75757 = CARTESIAN_POINT('Ctrl Pts',(-20.261684750146,-31.8939056343185,124.290492599356)) ;
#75758 = CARTESIAN_POINT('Ctrl Pts',(-20.7850691733475,-32.0937733197896,
124.082510674335)) ;
#75759 = CARTESIAN_POINT('Ctrl Pts',(-20.5099133229686,-31.9137842393708,
123.948363354658)) ;
#75760 = CARTESIAN_POINT('Ctrl Pts',(-20.9316880819993,-32.1138056795153,
123.570639458994)) ;
#75761 = CARTESIAN_POINT('Ctrl Pts',(-20.6272030682315,-31.9338165990965,
123.538857703905)) ;
#75762 = CARTESIAN_POINT('Ctrl Pts',(-20.9004840929352,-32.1303874054713,
123.131013871463)) ;
#75763 = CARTESIAN_POINT('Ctrl Pts',(-20.6022414356194,-31.9503983250526,
123.18718139994)) ;
#75764 = CARTESIAN_POINT('Ctrl Pts',(-20.7882628388064,-32.1435815757693,
122.802971043157)) ;
#75765 = CARTESIAN_POINT('Ctrl Pts',(-20.5124528334552,-31.9635924953505,
122.924720353763)) ;
#75766 = CARTESIAN_POINT('Ctrl Pts',(-20.6197762199755,-32.1568937538625,
122.49638698779)) ;
#75767 = CARTESIAN_POINT('Ctrl Pts',(-20.3776944292789,-31.9769046734437,
122.679499995801)) ;
#75768 = CARTESIAN_POINT('Ctrl Pts',(-20.315208446771,-32.1734599334558,122.178383590864)) ;
#75769 = CARTESIAN_POINT('Ctrl Pts',(-20.1339927311637,-31.9934708530371,
122.425047213569)) ;
#75770 = CARTESIAN_POINT('Ctrl Pts',(-19.919195114621,-32.190088128316,121.982318683978)) ;
#75771 = CARTESIAN_POINT('Ctrl Pts',(-19.8172191413778,-32.0100990478972,
122.268225564694)) ;
#75772 = CARTESIAN_POINT('Ctrl Pts',(-19.5767420543865,-32.2033767100257,
121.913670003238)) ;
#75773 = CARTESIAN_POINT('Ctrl Pts',(-19.5432298830773,-32.023387629607,122.21329620248)) ;
#75774 = CARTESIAN_POINT('Ctrl Pts',(-19.3148866166787,-32.2133449581293,
121.907334290393)) ;
#75775 = CARTESIAN_POINT('Ctrl Pts',(-19.3337508380696,-32.0333558777106,
122.208232314246)) ;
#75776 = CARTESIAN_POINT('Ctrl Pts',(-19.0572238635759,-32.2232597143854,
121.946033185514)) ;
#75777 = CARTESIAN_POINT('Ctrl Pts',(-19.1276189170704,-32.0432706339667,
122.239193494291)) ;
#75778 = CARTESIAN_POINT('Ctrl Pts',(-18.8076409322164,-32.2332728650367,
122.029433371306)) ;
#75779 = CARTESIAN_POINT('Ctrl Pts',(-18.9279556714256,-32.0532837846179,
122.305913714308)) ;
#75780 = CARTESIAN_POINT('Ctrl Pts',(-18.5765593856739,-32.2432855722387,
122.155251712084)) ;
#75781 = CARTESIAN_POINT('Ctrl Pts',(-18.7430841787746,-32.0632964918199,
122.406578419691)) ;
#75782 = CARTESIAN_POINT('Ctrl Pts',(-18.3044914721086,-32.25650486093,122.37133980811)) ;
#75783 = CARTESIAN_POINT('Ctrl Pts',(-18.5254677230784,-32.0765157805112,
122.579410561966)) ;
#75784 = CARTESIAN_POINT('Ctrl Pts',(-18.0412520384418,-32.273123541928,122.725865755981)) ;
#75785 = CARTESIAN_POINT('Ctrl Pts',(-18.3148360322381,-32.0931344615093,
122.863088795251)) ;
#75786 = CARTESIAN_POINT('Ctrl Pts',(-17.9146049569576,-32.2896884497015,
123.147620680719)) ;
#75787 = CARTESIAN_POINT('Ctrl Pts',(-18.2135427847506,-32.1096993692827,
123.200444214174)) ;
#75788 = CARTESIAN_POINT('Ctrl Pts',(-17.9043631044386,-32.3030869213123,
123.499558748907)) ;
#75789 = CARTESIAN_POINT('Ctrl Pts',(-18.2053428096442,-32.1230978408936,
123.482028671522)) ;
#75790 = CARTESIAN_POINT('Ctrl Pts',(-17.9415874188151,-32.3129281767992,
123.755505137572)) ;
#75791 = CARTESIAN_POINT('Ctrl Pts',(-18.2351264004454,-32.1329390963805,
123.686778655729)) ;
#75792 = CARTESIAN_POINT('Ctrl Pts',(-18.0233154439274,-32.3229144923875,
124.004839610879)) ;
#75793 = CARTESIAN_POINT('Ctrl Pts',(-18.3005104402209,-32.1429254119687,
123.886247298971)) ;
#75794 = CARTESIAN_POINT('Ctrl Pts',(-18.1464078762441,-32.3328510999739,
124.235179732751)) ;
#75795 = CARTESIAN_POINT('Ctrl Pts',(-18.3989864852805,-32.1528620195551,
124.070517791497)) ;
#75796 = CARTESIAN_POINT('Ctrl Pts',(-18.3095220074797,-32.3429009673422,
124.442853309924)) ;
#75797 = CARTESIAN_POINT('Ctrl Pts',(-18.5294795023595,-32.1629118869234,
124.23665535116)) ;
#75798 = CARTESIAN_POINT('Ctrl Pts',(-18.5022200305322,-32.352751462017,124.615730119518)) ;
#75799 = CARTESIAN_POINT('Ctrl Pts',(-18.6836393679515,-32.1727623815982,
124.374955019593)) ;
#75800 = CARTESIAN_POINT('Ctrl Pts',(-18.7243070866901,-32.3627232624115,
124.754758703719)) ;
#75801 = CARTESIAN_POINT('Ctrl Pts',(-18.8613101252405,-32.1827341819927,
124.486175940165)) ;
#75802 = CARTESIAN_POINT('Ctrl Pts',(-18.9678327868279,-32.3727192294373,
124.853354582508)) ;
#75803 = CARTESIAN_POINT('Ctrl Pts',(-19.0561314683988,-32.1927301490186,
124.565050536217)) ;
#75804 = CARTESIAN_POINT('Ctrl Pts',(-19.2258519489846,-32.3827566888185,
124.908029994952)) ;
#75805 = CARTESIAN_POINT('Ctrl Pts',(-19.2625472401696,-32.2027676083997,
124.608788652274)) ;
#75806 = CARTESIAN_POINT('Ctrl Pts',(-19.4843048557943,-32.3925973897192,
124.917387851488)) ;
#75807 = CARTESIAN_POINT('Ctrl Pts',(-19.4693094439586,-32.2126083093005,
124.616272690437)) ;
#75808 = CARTESIAN_POINT('Ctrl Pts',(-19.7458762677013,-32.4026454109866,
124.881367125356)) ;
#75809 = CARTESIAN_POINT('Ctrl Pts',(-19.6785662481788,-32.2226563305678,
124.587453906341)) ;
#75810 = CARTESIAN_POINT('Ctrl Pts',(-19.9945882738424,-32.4125928040693,
124.800883482225)) ;
#75811 = CARTESIAN_POINT('Ctrl Pts',(-19.8775350535338,-32.2326037236505,
124.523064890071)) ;
#75812 = CARTESIAN_POINT('Ctrl Pts',(-20.2250646864161,-32.4225029501157,
124.679595400732)) ;
#75813 = CARTESIAN_POINT('Ctrl Pts',(-20.0619149780218,-32.2425138696969,
124.426032565424)) ;
#75814 = CARTESIAN_POINT('Ctrl Pts',(-20.4338556735441,-32.4325618639653,
124.517526669019)) ;
#75815 = CARTESIAN_POINT('Ctrl Pts',(-20.2289464252875,-32.2525727835465,
124.296375807091)) ;
#75816 = CARTESIAN_POINT('Ctrl Pts',(-20.6077963924508,-32.4424026342546,
124.326112710834)) ;
#75817 = CARTESIAN_POINT('Ctrl Pts',(-20.3680971502017,-32.2624135538358,
124.143243405943)) ;
#75818 = CARTESIAN_POINT('Ctrl Pts',(-20.7492002051282,-32.4524655038332,
124.102692225391)) ;
#75819 = CARTESIAN_POINT('Ctrl Pts',(-20.4812183762259,-32.2724764234145,
123.964505819681)) ;
#75820 = CARTESIAN_POINT('Ctrl Pts',(-20.8478072363994,-32.4623598269637,
123.862073047609)) ;
#75821 = CARTESIAN_POINT('Ctrl Pts',(-20.5601018691605,-32.2823707465449,
123.772009890152)) ;
#75822 = CARTESIAN_POINT('Ctrl Pts',(-20.9040808602979,-32.4723016340582,
123.606978235606)) ;
#75823 = CARTESIAN_POINT('Ctrl Pts',(-20.6051186298419,-32.2923125536394,
123.567933786065)) ;
#75824 = CARTESIAN_POINT('Ctrl Pts',(-20.9153764258994,-32.4823041450135,
123.344329862465)) ;
#75825 = CARTESIAN_POINT('Ctrl Pts',(-20.6141529513669,-32.3023150645948,
123.357815062894)) ;
#75826 = CARTESIAN_POINT('Ctrl Pts',(-20.8803820948973,-32.4923388658319,
123.082976330984)) ;
#75827 = CARTESIAN_POINT('Ctrl Pts',(-20.5861553344511,-32.3123497854131,
123.148732512367)) ;
#75828 = CARTESIAN_POINT('Ctrl Pts',(-20.8024460213964,-32.5021840433376,
122.83625706858)) ;
#75829 = CARTESIAN_POINT('Ctrl Pts',(-20.5238045816804,-32.3221949629189,
122.951358176035)) ;
#75830 = CARTESIAN_POINT('Ctrl Pts',(-20.6816420858967,-32.5121688037387,
122.603373026564)) ;
#75831 = CARTESIAN_POINT('Ctrl Pts',(-20.427159646758,-32.3321797233199,122.765052018463)) ;
#75832 = CARTESIAN_POINT('Ctrl Pts',(-20.5230220508971,-32.5221077100551,
122.395822102381)) ;
#75833 = CARTESIAN_POINT('Ctrl Pts',(-20.3002621303212,-32.3421186296363,
122.59901272905)) ;
#75834 = CARTESIAN_POINT('Ctrl Pts',(-20.328762472991,-32.5321499376908,122.217239391527)) ;
#75835 = CARTESIAN_POINT('Ctrl Pts',(-20.1448530337361,-32.3521608572721,
122.456148061873)) ;
#75836 = CARTESIAN_POINT('Ctrl Pts',(-20.1099755421351,-32.5420351492752,
122.077133850334)) ;
#75837 = CARTESIAN_POINT('Ctrl Pts',(-19.9698227394801,-32.3620460688564,
122.344065585937)) ;
#75838 = CARTESIAN_POINT('Ctrl Pts',(-19.8676198087707,-32.5520340794771,
121.975708802739)) ;
#75839 = CARTESIAN_POINT('Ctrl Pts',(-19.7759374551782,-32.3720449990584,
122.262927442215)) ;
#75840 = CARTESIAN_POINT('Ctrl Pts',(-19.6133877400245,-32.5619515023875,
121.918164610149)) ;
#75841 = CARTESIAN_POINT('Ctrl Pts',(-19.5725517025332,-32.3819624219688,
122.216894103057)) ;
#75842 = CARTESIAN_POINT('Ctrl Pts',(-19.3496802081927,-32.5719994344663,
121.90552817767)) ;
#75843 = CARTESIAN_POINT('Ctrl Pts',(-19.3615855024817,-32.3920103540475,
122.206786949623)) ;
#75844 = CARTESIAN_POINT('Ctrl Pts',(-19.0921154350344,-32.5818768102757,
121.938063647329)) ;
#75845 = CARTESIAN_POINT('Ctrl Pts',(-19.1555344414447,-32.4018877298569,
122.232817207828)) ;
#75846 = CARTESIAN_POINT('Ctrl Pts',(-18.8397271603411,-32.5919307034436,
122.016043063016)) ;
#75847 = CARTESIAN_POINT('Ctrl Pts',(-18.9536242958656,-32.4119416230248,
122.295202630568)) ;
#75848 = CARTESIAN_POINT('Ctrl Pts',(-18.6083164557065,-32.6018243266969,
122.13467532395)) ;
#75849 = CARTESIAN_POINT('Ctrl Pts',(-18.7684970311458,-32.4218352462781,
122.390109938702)) ;
#75850 = CARTESIAN_POINT('Ctrl Pts',(-18.3975309341111,-32.6118869203199,
122.294276744081)) ;
#75851 = CARTESIAN_POINT('Ctrl Pts',(-18.5998696580958,-32.4318978399011,
122.517792698231)) ;
#75852 = CARTESIAN_POINT('Ctrl Pts',(-18.2214436963193,-32.6217294943089,
122.48377741207)) ;
#75853 = CARTESIAN_POINT('Ctrl Pts',(-18.4590017343272,-32.4417404138902,
122.669394019431)) ;
#75854 = CARTESIAN_POINT('Ctrl Pts',(-18.0783294581763,-32.6317202511919,
122.703848805857)) ;
#75855 = CARTESIAN_POINT('Ctrl Pts',(-18.3445119383423,-32.4517311707731,
122.845452004202)) ;
#75856 = CARTESIAN_POINT('Ctrl Pts',(-17.9762694761468,-32.6416483129498,
122.943971098635)) ;
#75857 = CARTESIAN_POINT('Ctrl Pts',(-18.2628657760219,-32.4616592325311,
123.037550188827)) ;
#75858 = CARTESIAN_POINT('Ctrl Pts',(-17.9166533726252,-32.651636288839,123.199595350727)) ;
#75859 = CARTESIAN_POINT('Ctrl Pts',(-18.2151746225017,-32.4716472084202,
123.242049843833)) ;
#75860 = CARTESIAN_POINT('Ctrl Pts',(-17.9027006001273,-32.6616719531954,
123.462944824452)) ;
#75861 = CARTESIAN_POINT('Ctrl Pts',(-18.2040142137418,-32.4816828727767,
123.452729587914)) ;
#75862 = CARTESIAN_POINT('Ctrl Pts',(-17.9337120200505,-32.6715278916151,
123.720099296873)) ;
#75863 = CARTESIAN_POINT('Ctrl Pts',(-18.2288249953322,-32.4915388111963,
123.658452229222)) ;
#75864 = CARTESIAN_POINT('Ctrl Pts',(-18.009543101107,-32.681523383012,123.971557376354)) ;
#75865 = CARTESIAN_POINT('Ctrl Pts',(-18.2894914284038,-32.5015343025932,
123.859618092693)) ;
#75866 = CARTESIAN_POINT('Ctrl Pts',(-18.1268171254845,-32.6914331879654,
124.204090672369)) ;
#75867 = CARTESIAN_POINT('Ctrl Pts',(-18.3833118888715,-32.5114441075467,
124.045643510793)) ;
#75868 = CARTESIAN_POINT('Ctrl Pts',(-18.283949331049,-32.7014454102322,124.415135395342)) ;
#75869 = CARTESIAN_POINT('Ctrl Pts',(-18.509018896985,-32.5214563298134,124.214478314619)) ;
#75870 = CARTESIAN_POINT('Ctrl Pts',(-18.4759885041696,-32.711473290925,124.595595889939)) ;
#75871 = CARTESIAN_POINT('Ctrl Pts',(-18.6626514215253,-32.5314842105063,
124.358845523371)) ;
#75872 = CARTESIAN_POINT('Ctrl Pts',(-18.6924294796263,-32.7213296869076,
124.737869480945)) ;
#75873 = CARTESIAN_POINT('Ctrl Pts',(-18.8358044087005,-32.5413406064889,
124.472662626393)) ;
#75874 = CARTESIAN_POINT('Ctrl Pts',(-18.9341360919436,-32.7313544840876,
124.842659911691)) ;
#75875 = CARTESIAN_POINT('Ctrl Pts',(-19.0291703120113,-32.5513654036688,
124.556493611938)) ;
#75876 = CARTESIAN_POINT('Ctrl Pts',(-19.1906775296602,-32.7413854140714,
124.903298738931)) ;
#75877 = CARTESIAN_POINT('Ctrl Pts',(-19.2344038900453,-32.5613963336526,
124.605003114696)) ;
#75878 = CARTESIAN_POINT('Ctrl Pts',(-19.4489157332654,-32.7512300165801,
124.918654695637)) ;
#75879 = CARTESIAN_POINT('Ctrl Pts',(-19.4409936483921,-32.5712409361613,
124.617286306339)) ;
#75880 = CARTESIAN_POINT('Ctrl Pts',(-19.7098139114715,-32.7612208678041,
124.889204775751)) ;
#75881 = CARTESIAN_POINT('Ctrl Pts',(-19.6497118803502,-32.5812317873854,
124.593725014445)) ;
#75882 = CARTESIAN_POINT('Ctrl Pts',(-19.9626440102893,-32.7712587008154,
124.81398793579)) ;
#75883 = CARTESIAN_POINT('Ctrl Pts',(-19.8519756339455,-32.5912696203966,
124.533550073541)) ;
#75884 = CARTESIAN_POINT('Ctrl Pts',(-20.1942400544796,-32.7811030892808,
124.698686780545)) ;
#75885 = CARTESIAN_POINT('Ctrl Pts',(-20.037251000993,-32.6011140088621,124.441308307128)) ;
#75886 = CARTESIAN_POINT('Ctrl Pts',(-20.4055373690986,-32.7910878936504,
124.543175419244)) ;
#75887 = CARTESIAN_POINT('Ctrl Pts',(-20.2062879201296,-32.6110988132316,
124.316898288086)) ;
#75888 = CARTESIAN_POINT('Ctrl Pts',(-20.5859328055609,-32.8010274131332,
124.354225946047)) ;
#75889 = CARTESIAN_POINT('Ctrl Pts',(-20.3506030458168,-32.6210383327145,
124.16573814407)) ;
#75890 = CARTESIAN_POINT('Ctrl Pts',(-20.7321570745328,-32.8110671441346,
124.134645385884)) ;
#75891 = CARTESIAN_POINT('Ctrl Pts',(-20.4675814518196,-32.6310780637158,
123.990072882451)) ;
#75892 = CARTESIAN_POINT('Ctrl Pts',(-20.8365696228961,-32.8209552723808,
123.896678841606)) ;
#75893 = CARTESIAN_POINT('Ctrl Pts',(-20.551110037506,-32.6409661919621,123.79969981623)) ;
#75894 = CARTESIAN_POINT('Ctrl Pts',(-20.8991776004823,-32.8309449975894,
123.641744550602)) ;
#75895 = CARTESIAN_POINT('Ctrl Pts',(-20.6011952561969,-32.6509559171706,
123.595752273945)) ;
#75896 = CARTESIAN_POINT('Ctrl Pts',(-20.9163259244539,-32.8409027622909,
123.380631029216)) ;
#75897 = CARTESIAN_POINT('Ctrl Pts',(-20.6149126952404,-32.6609136818721,
123.386861725222)) ;
#75898 = CARTESIAN_POINT('Ctrl Pts',(-20.8886398162672,-32.8508051037029,
123.121875613557)) ;
#75899 = CARTESIAN_POINT('Ctrl Pts',(-20.5927628294816,-32.6708160232841,
123.179858200967)) ;
#75900 = CARTESIAN_POINT('Ctrl Pts',(-20.8153934382436,-32.8608492994093,
122.868304834819)) ;
#75901 = CARTESIAN_POINT('Ctrl Pts',(-20.5341646599949,-32.6808602189905,
122.977001723796)) ;
#75902 = CARTESIAN_POINT('Ctrl Pts',(-20.7008271859404,-32.8707567001685,
122.634494488464)) ;
#75903 = CARTESIAN_POINT('Ctrl Pts',(-20.4425109923345,-32.6907676197498,
122.789954502378)) ;
#75904 = CARTESIAN_POINT('Ctrl Pts',(-20.546186232059,-32.8807673000429,122.421673048504)) ;
#75905 = CARTESIAN_POINT('Ctrl Pts',(-20.3187974795829,-32.7007782196241,
122.619697941561)) ;
#75906 = CARTESIAN_POINT('Ctrl Pts',(-20.3562127677178,-32.8907975959551,
122.238939688414)) ;
#75907 = CARTESIAN_POINT('Ctrl Pts',(-20.1668179033373,-32.7108085155363,
122.473511971535)) ;
#75908 = CARTESIAN_POINT('Ctrl Pts',(-20.1414444851977,-32.9006523756048,
122.094253937505)) ;
#75909 = CARTESIAN_POINT('Ctrl Pts',(-19.9950035629509,-32.720663295186,122.35776475964)) ;
#75910 = CARTESIAN_POINT('Ctrl Pts',(-19.9026572208849,-32.9106097038223,
121.98722381841)) ;
#75911 = CARTESIAN_POINT('Ctrl Pts',(-19.8039737675108,-32.7306206234035,
122.272141549309)) ;
#75912 = CARTESIAN_POINT('Ctrl Pts',(-19.6467435512294,-32.9206487367292,
121.923215339436)) ;
#75913 = CARTESIAN_POINT('Ctrl Pts',(-19.5992424816828,-32.7406596563104,
122.220935620064)) ;
#75914 = CARTESIAN_POINT('Ctrl Pts',(-19.3879265897754,-32.9305218486184,
121.904435880126)) ;
#75915 = CARTESIAN_POINT('Ctrl Pts',(-19.3921897535148,-32.7505327681997,
122.205912911945)) ;
#75916 = CARTESIAN_POINT('Ctrl Pts',(-19.1246518187911,-32.9405951336456,
121.931486510168)) ;
#75917 = CARTESIAN_POINT('Ctrl Pts',(-19.18156967997,-32.7606060532268,122.227554264233)) ;
#75918 = CARTESIAN_POINT('Ctrl Pts',(-18.8762664626963,-32.9504154533823,
122.001727342431)) ;
#75919 = CARTESIAN_POINT('Ctrl Pts',(-18.9828627923026,-32.7704263729636,
122.283747296942)) ;
#75920 = CARTESIAN_POINT('Ctrl Pts',(-18.6377418414705,-32.9604941187608,
122.116709479885)) ;
#75921 = CARTESIAN_POINT('Ctrl Pts',(-18.7920430490926,-32.780505038342,122.375733780278)) ;
#75922 = CARTESIAN_POINT('Ctrl Pts',(-18.4274927506515,-32.9703457092446,
122.267875972301)) ;
#75923 = CARTESIAN_POINT('Ctrl Pts',(-18.623845014994,-32.7903566288258,122.496666887985)) ;
#75924 = CARTESIAN_POINT('Ctrl Pts',(-18.2425317133348,-32.9804188595635,
122.457180219364)) ;
#75925 = CARTESIAN_POINT('Ctrl Pts',(-18.4758763682574,-32.8004297791447,
122.648110955056)) ;
#75926 = CARTESIAN_POINT('Ctrl Pts',(-18.0966577529287,-32.9902612395385,
122.670798846619)) ;
#75927 = CARTESIAN_POINT('Ctrl Pts',(-18.3591783416525,-32.8102721591198,
122.819005262211)) ;
#75928 = CARTESIAN_POINT('Ctrl Pts',(-17.9878239542767,-33.0002422157816,
122.909421734019)) ;
#75929 = CARTESIAN_POINT('Ctrl Pts',(-18.272111762497,-32.8202531353628,123.009903514452)) ;
#75930 = CARTESIAN_POINT('Ctrl Pts',(-17.9222646671379,-33.0102585441368,
123.164359426902)) ;
#75931 = CARTESIAN_POINT('Ctrl Pts',(-18.2196648233517,-32.8302694637181,
123.213853781775)) ;
#75932 = CARTESIAN_POINT('Ctrl Pts',(-17.9018796512239,-33.020156341128,123.423653833823)) ;
#75933 = CARTESIAN_POINT('Ctrl Pts',(-18.2033572916693,-32.8401672607093,
123.421288551752)) ;
#75934 = CARTESIAN_POINT('Ctrl Pts',(-17.9266701885692,-33.0301688978601,
123.685622214855)) ;
#75935 = CARTESIAN_POINT('Ctrl Pts',(-18.2231900289858,-32.8501798174413,
123.630863208958)) ;
#75936 = CARTESIAN_POINT('Ctrl Pts',(-17.9972994488125,-33.0402009327065,
123.939603199714)) ;
#75937 = CARTESIAN_POINT('Ctrl Pts',(-18.2796939144183,-32.8602118522878,
123.834047973384)) ;
#75938 = CARTESIAN_POINT('Ctrl Pts',(-18.1082062115513,-33.050040333522,124.173202825611)) ;
#75939 = CARTESIAN_POINT('Ctrl Pts',(-18.3684190950603,-32.8700512531033,
124.020926481006)) ;
#75940 = CARTESIAN_POINT('Ctrl Pts',(-18.2612411136302,-33.0601061191736,
124.388920029525)) ;
#75941 = CARTESIAN_POINT('Ctrl Pts',(-18.4908474005065,-32.8801170387548,
124.193500344908)) ;
#75942 = CARTESIAN_POINT('Ctrl Pts',(-18.4462566310749,-33.0699965742882,
124.571505176975)) ;
#75943 = CARTESIAN_POINT('Ctrl Pts',(-18.6388594192354,-32.8900074938694,
124.339567673731)) ;
#75944 = CARTESIAN_POINT('Ctrl Pts',(-18.6620084680825,-33.0799886929239,
124.721150558797)) ;
#75945 = CARTESIAN_POINT('Ctrl Pts',(-18.8114608287963,-32.8999996125052,
124.459283763965)) ;
#75946 = CARTESIAN_POINT('Ctrl Pts',(-18.8998759883015,-33.089951519687,124.830519144771)) ;
#75947 = CARTESIAN_POINT('Ctrl Pts',(-19.0017545994413,-32.9099624392683,
124.546778293489)) ;
#75948 = CARTESIAN_POINT('Ctrl Pts',(-19.1514920072982,-33.0998558029599,
124.897179406817)) ;
#75949 = CARTESIAN_POINT('Ctrl Pts',(-19.2030466974503,-32.9198667225411,
124.600106275238)) ;
#75950 = CARTESIAN_POINT('Ctrl Pts',(-19.4149143853566,-33.109916236907,124.919252762211)) ;
#75951 = CARTESIAN_POINT('Ctrl Pts',(-19.4137848897019,-32.9299271564882,
124.617764888164)) ;
#75952 = CARTESIAN_POINT('Ctrl Pts',(-19.6725102686818,-33.1197567895802,
124.896100987833)) ;
#75953 = CARTESIAN_POINT('Ctrl Pts',(-19.6198604236689,-32.9397677091614,
124.599243563997)) ;
#75954 = CARTESIAN_POINT('Ctrl Pts',(-19.9278232585539,-33.1298190095259,
124.827395120456)) ;
#75955 = CARTESIAN_POINT('Ctrl Pts',(-19.824111120568,-32.9498299291071,124.544278865711)) ;
#75956 = CARTESIAN_POINT('Ctrl Pts',(-20.1633223010503,-33.1397161488044,
124.716975844199)) ;
#75957 = CARTESIAN_POINT('Ctrl Pts',(-20.0125096303553,-32.9597270683857,
124.455943788509)) ;
#75958 = CARTESIAN_POINT('Ctrl Pts',(-20.3772875393631,-33.1496473409395,
124.567550900656)) ;
#75959 = CARTESIAN_POINT('Ctrl Pts',(-20.1836814780393,-32.9696582605208,
124.336404350332)) ;
#75960 = CARTESIAN_POINT('Ctrl Pts',(-20.563912219423,-33.1596894955846,124.380978396935)) ;
#75961 = CARTESIAN_POINT('Ctrl Pts',(-20.3329814474512,-32.9797004151658,
124.187146334296)) ;
#75962 = CARTESIAN_POINT('Ctrl Pts',(-20.7131557898249,-33.1695762566039,
124.168279265525)) ;
#75963 = CARTESIAN_POINT('Ctrl Pts',(-20.4523759687857,-32.9895871761851,
124.016987866727)) ;
#75964 = CARTESIAN_POINT('Ctrl Pts',(-20.8247334246548,-33.1795755583211,
123.930412036543)) ;
#75965 = CARTESIAN_POINT('Ctrl Pts',(-20.5416382872207,-32.9995864779024,
123.826694322003)) ;
#75966 = CARTESIAN_POINT('Ctrl Pts',(-20.8929652907576,-33.1894963564879,
123.67875334174)) ;
#75967 = CARTESIAN_POINT('Ctrl Pts',(-20.5962239379931,-33.0095072760691,
123.625368054938)) ;
#75968 = CARTESIAN_POINT('Ctrl Pts',(-20.9167545831049,-33.1995304100846,
123.416173818305)) ;
#75969 = CARTESIAN_POINT('Ctrl Pts',(-20.6152557226043,-33.0195413296658,
123.415304354511)) ;
#75970 = CARTESIAN_POINT('Ctrl Pts',(-20.8949864127053,-33.209453527651,123.156274431555)) ;
#75971 = CARTESIAN_POINT('Ctrl Pts',(-20.5978416138883,-33.0294644472322,
123.207385423938)) ;
#75972 = CARTESIAN_POINT('Ctrl Pts',(-20.8274911535787,-33.2195096511501,
122.900802570395)) ;
#75973 = CARTESIAN_POINT('Ctrl Pts',(-20.5438456966334,-33.0395205707314,
123.003007611585)) ;
#75974 = CARTESIAN_POINT('Ctrl Pts',(-20.7190711619547,-33.2293550928049,
122.66587466645)) ;
#75975 = CARTESIAN_POINT('Ctrl Pts',(-20.4571105336298,-33.0493660123862,
122.815066148446)) ;
#75976 = CARTESIAN_POINT('Ctrl Pts',(-20.5704789954132,-33.2393173939291,
122.450351068631)) ;
#75977 = CARTESIAN_POINT('Ctrl Pts',(-20.3382375063864,-33.0593283135103,
122.64264722283)) ;
#75978 = CARTESIAN_POINT('Ctrl Pts',(-20.3852299652327,-33.2493458732042,
122.262882911271)) ;
#75979 = CARTESIAN_POINT('Ctrl Pts',(-20.1900385985285,-33.0693567927855,
122.492672276396)) ;
#75980 = CARTESIAN_POINT('Ctrl Pts',(-20.1728523554224,-33.2592562267139,
122.112168057939)) ;
#75981 = CARTESIAN_POINT('Ctrl Pts',(-20.020137396195,-33.0792671462951,122.37210035673)) ;
#75982 = CARTESIAN_POINT('Ctrl Pts',(-19.9372239609751,-33.2691910988911,
121.99971673784)) ;
#75983 = CARTESIAN_POINT('Ctrl Pts',(-19.8316354638329,-33.0892020184723,
122.282138886147)) ;
#75984 = CARTESIAN_POINT('Ctrl Pts',(-19.6829095120149,-33.2792322364768,
121.929380340477)) ;
#75985 = CARTESIAN_POINT('Ctrl Pts',(-19.6281839338197,-33.099243156058,122.225869101484)) ;
#75986 = CARTESIAN_POINT('Ctrl Pts',(-19.4242673412643,-33.2891193856913,
121.90447101779)) ;
#75987 = CARTESIAN_POINT('Ctrl Pts',(-19.4212710912674,-33.1091303052726,
122.205941031457)) ;
#75988 = CARTESIAN_POINT('Ctrl Pts',(-19.1624743734759,-33.2991116204424,
121.924625119978)) ;
#75989 = CARTESIAN_POINT('Ctrl Pts',(-19.2118368178498,-33.1191225400237,
122.222063502103)) ;
#75990 = CARTESIAN_POINT('Ctrl Pts',(-18.9092537721771,-33.3090603260054,
121.989726729826)) ;
#75991 = CARTESIAN_POINT('Ctrl Pts',(-19.009260561855,-33.1290712455866,122.274143925144)) ;
#75992 = CARTESIAN_POINT('Ctrl Pts',(-18.6713579683,-33.3189963944291,122.097309682387)) ;
#75993 = CARTESIAN_POINT('Ctrl Pts',(-18.8189440248541,-33.1390073140103,
122.360209282463)) ;
#75994 = CARTESIAN_POINT('Ctrl Pts',(-18.4544730862857,-33.3289820786449,
122.245077547406)) ;
#75995 = CARTESIAN_POINT('Ctrl Pts',(-18.6454357542757,-33.1489929982261,
122.478422680742)) ;
#75996 = CARTESIAN_POINT('Ctrl Pts',(-18.2658309061673,-33.3390225052135,
122.429534786663)) ;
#75997 = CARTESIAN_POINT('Ctrl Pts',(-18.494521322166,-33.1590334247948,122.625987962609)) ;
#75998 = CARTESIAN_POINT('Ctrl Pts',(-18.1148023370234,-33.3488616186773,
122.639409270559)) ;
#75999 = CARTESIAN_POINT('Ctrl Pts',(-18.3736983361703,-33.1688725382585,
122.793886113984)) ;
#76000 = CARTESIAN_POINT('Ctrl Pts',(-17.9997997484808,-33.3588913528531,
122.876570796165)) ;
#76001 = CARTESIAN_POINT('Ctrl Pts',(-18.2816952521632,-33.1789022724343,
122.983614938204)) ;
#76002 = CARTESIAN_POINT('Ctrl Pts',(-17.9284390776432,-33.368913452359,123.130086625295)) ;
#76003 = CARTESIAN_POINT('Ctrl Pts',(-18.2246058215283,-33.1889243719402,
123.186427373328)) ;
#76004 = CARTESIAN_POINT('Ctrl Pts',(-17.9019339657946,-33.3787818922524,
123.388080969437)) ;
#76005 = CARTESIAN_POINT('Ctrl Pts',(-18.2034007565293,-33.1987928118337,
123.3928218386)) ;
#76006 = CARTESIAN_POINT('Ctrl Pts',(-17.9210110194768,-33.388850756938,123.651967424928)) ;
#76007 = CARTESIAN_POINT('Ctrl Pts',(-18.2186613497739,-33.2088616765193,
123.603931380545)) ;
#76008 = CARTESIAN_POINT('Ctrl Pts',(-17.9841657909926,-33.3986934300366,
123.902803793682)) ;
#76009 = CARTESIAN_POINT('Ctrl Pts',(-18.2691838719648,-33.2187043496179,
123.804599731666)) ;
#76010 = CARTESIAN_POINT('Ctrl Pts',(-18.0903011026987,-33.4086540641991,
124.142069897839)) ;
#76011 = CARTESIAN_POINT('Ctrl Pts',(-18.3540908116242,-33.2286649837803,
123.996012840234)) ;
#76012 = CARTESIAN_POINT('Ctrl Pts',(-18.2379303217283,-33.4186919798772,
124.360664605531)) ;
#76013 = CARTESIAN_POINT('Ctrl Pts',(-18.4721932743968,-33.2387028994585,
124.170889351092)) ;
#76014 = CARTESIAN_POINT('Ctrl Pts',(-18.4179673638291,-33.4285662547366,
124.547577121992)) ;
#76015 = CARTESIAN_POINT('Ctrl Pts',(-18.6162214263879,-33.2485771743179,
124.320419667571)) ;
#76016 = CARTESIAN_POINT('Ctrl Pts',(-18.631829456025,-33.4386360051118,124.703362669237)) ;
#76017 = CARTESIAN_POINT('Ctrl Pts',(-18.7873105748439,-33.258646924693,124.445049300282)) ;
#76018 = CARTESIAN_POINT('Ctrl Pts',(-18.8639015606076,-33.4484693004863,
124.8170675459)) ;
#76019 = CARTESIAN_POINT('Ctrl Pts',(-18.9729667662246,-33.2684802200675,
124.536013921811)) ;
#76020 = CARTESIAN_POINT('Ctrl Pts',(-19.1169286180859,-33.4584995979659,
124.890896842936)) ;
#76021 = CARTESIAN_POINT('Ctrl Pts',(-19.1753880699453,-33.2785105175472,
124.595078779856)) ;
#76022 = CARTESIAN_POINT('Ctrl Pts',(-19.3790808832742,-33.4685316844073,
124.918905806872)) ;
#76023 = CARTESIAN_POINT('Ctrl Pts',(-19.3851098109455,-33.2885426039886,
124.617487248845)) ;
#76024 = CARTESIAN_POINT('Ctrl Pts',(-19.63677762178,-33.4783596128963,124.901904690661)) ;
#76025 = CARTESIAN_POINT('Ctrl Pts',(-19.5912662774906,-33.2983705324775,
124.603887836004)) ;
#76026 = CARTESIAN_POINT('Ctrl Pts',(-19.8920737335498,-33.4883556540071,
124.840047977174)) ;
#76027 = CARTESIAN_POINT('Ctrl Pts',(-19.7955034173776,-33.3083665735883,
124.554404008552)) ;
#76028 = CARTESIAN_POINT('Ctrl Pts',(-20.133272867341,-33.4983814661083,124.734019156256)) ;
#76029 = CARTESIAN_POINT('Ctrl Pts',(-19.9884633393389,-33.3183923856895,
124.469582272309)) ;
#76030 = CARTESIAN_POINT('Ctrl Pts',(-20.3495536622169,-33.5082687010031,
124.590024685986)) ;
#76031 = CARTESIAN_POINT('Ctrl Pts',(-20.1614882643308,-33.3282796205843,
124.35438833044)) ;
#76032 = CARTESIAN_POINT('Ctrl Pts',(-20.5395336849035,-33.5182455672141,
124.409369154999)) ;
#76033 = CARTESIAN_POINT('Ctrl Pts',(-20.3134732405899,-33.3382564867954,
124.209865210489)) ;
#76034 = CARTESIAN_POINT('Ctrl Pts',(-20.6955808167285,-33.5282385110859,
124.198113299895)) ;
#76035 = CARTESIAN_POINT('Ctrl Pts',(-20.4383121677193,-33.3482494306672,
124.040861581618)) ;
#76036 = CARTESIAN_POINT('Ctrl Pts',(-20.812778041228,-33.5382764337573,123.961814580472)) ;
#76037 = CARTESIAN_POINT('Ctrl Pts',(-20.5320713666861,-33.3582873533385,
123.851823229752)) ;
#76038 = CARTESIAN_POINT('Ctrl Pts',(-20.8861474399922,-33.548124898019,123.713603887061)) ;
#76039 = CARTESIAN_POINT('Ctrl Pts',(-20.5907682089124,-33.3681358176002,
123.653255920477)) ;
#76040 = CARTESIAN_POINT('Ctrl Pts',(-20.9161879632352,-33.558116764763,123.45279073019)) ;
#76041 = CARTESIAN_POINT('Ctrl Pts',(-20.6148023084948,-33.3781276843442,
123.444605723383)) ;
#76042 = CARTESIAN_POINT('Ctrl Pts',(-20.9007460376538,-33.5680344968042,
123.192586764774)) ;
#76043 = CARTESIAN_POINT('Ctrl Pts',(-20.6024505212769,-33.3880454163854,
123.236442905293)) ;
#76044 = CARTESIAN_POINT('Ctrl Pts',(-20.839767398119,-33.5780626816995,122.936230922759)) ;
#76045 = CARTESIAN_POINT('Ctrl Pts',(-20.5536692986984,-33.3980736012807,
123.031357801439)) ;
#76046 = CARTESIAN_POINT('Ctrl Pts',(-20.7367825953331,-33.5879478397483,
122.697737712754)) ;
#76047 = CARTESIAN_POINT('Ctrl Pts',(-20.4712833051947,-33.4079587593295,
122.840563075759)) ;
#76048 = CARTESIAN_POINT('Ctrl Pts',(-20.5929810835081,-33.59793720029,122.478112272393)) ;
#76049 = CARTESIAN_POINT('Ctrl Pts',(-20.3562437228865,-33.4179481198712,
122.664861808084)) ;
#76050 = CARTESIAN_POINT('Ctrl Pts',(-20.4118953447664,-33.6079783572243,
122.28618599591)) ;
#76051 = CARTESIAN_POINT('Ctrl Pts',(-20.211376372118,-33.4279892768056,122.511319516605)) ;
#76052 = CARTESIAN_POINT('Ctrl Pts',(-20.2048905332115,-33.6178109406795,
122.131549195087)) ;
#76053 = CARTESIAN_POINT('Ctrl Pts',(-20.0457742371618,-33.4378218602607,
122.387609057188)) ;
#76054 = CARTESIAN_POINT('Ctrl Pts',(-19.9707238078084,-33.6278051606415,
122.012626278737)) ;
#76055 = CARTESIAN_POINT('Ctrl Pts',(-19.8584418276612,-33.4478160802227,
122.292469026325)) ;
#76056 = CARTESIAN_POINT('Ctrl Pts',(-19.7184472437262,-33.6378332624288,
121.936421881555)) ;
#76057 = CARTESIAN_POINT('Ctrl Pts',(-19.6566211029712,-33.45784418201,122.231503711827)) ;
#76058 = CARTESIAN_POINT('Ctrl Pts',(-19.4606834132715,-33.6477132070518,
121.905273090472)) ;
#76059 = CARTESIAN_POINT('Ctrl Pts',(-19.450410798269,-33.4677241266331,122.206582828695)) ;
#76060 = CARTESIAN_POINT('Ctrl Pts',(-19.1985284829014,-33.6577035336089,
121.919105510817)) ;
#76061 = CARTESIAN_POINT('Ctrl Pts',(-19.2406868632452,-33.4777144531901,
122.217646778312)) ;
#76062 = CARTESIAN_POINT('Ctrl Pts',(-18.9440006247373,-33.6676444652632,
121.977957452848)) ;
#76063 = CARTESIAN_POINT('Ctrl Pts',(-19.037064402286,-33.4876553848444,122.264726340451)) ;
#76064 = CARTESIAN_POINT('Ctrl Pts',(-18.7022824096252,-33.6776315837661,
122.080244334411)) ;
#76065 = CARTESIAN_POINT('Ctrl Pts',(-18.8436891442797,-33.4976425033473,
122.346553933699)) ;
#76066 = CARTESIAN_POINT('Ctrl Pts',(-18.4812344248133,-33.6876649166633,
122.223936502214)) ;
#76067 = CARTESIAN_POINT('Ctrl Pts',(-18.6668496639801,-33.5076758362445,
122.461506021483)) ;
#76068 = CARTESIAN_POINT('Ctrl Pts',(-18.2913247034352,-33.697531021108,122.40049026279)) ;
#76069 = CARTESIAN_POINT('Ctrl Pts',(-18.514920867317,-33.5175419406893,122.602747196414)) ;
#76070 = CARTESIAN_POINT('Ctrl Pts',(-18.1317726323922,-33.7075971349883,
122.611443968971)) ;
#76071 = CARTESIAN_POINT('Ctrl Pts',(-18.3872775066212,-33.5276080545696,
122.771509020567)) ;
#76072 = CARTESIAN_POINT('Ctrl Pts',(-18.0137527034609,-33.7174531467568,
122.842018843075)) ;
#76073 = CARTESIAN_POINT('Ctrl Pts',(-18.2928599689319,-33.537464066338,122.955967544122)) ;
#76074 = CARTESIAN_POINT('Ctrl Pts',(-17.9357556599611,-33.7274478503881,
123.09281337308)) ;
#76075 = CARTESIAN_POINT('Ctrl Pts',(-18.2304603236921,-33.5474587699693,
123.156602459403)) ;
#76076 = CARTESIAN_POINT('Ctrl Pts',(-17.902925994022,-33.7374791861129,123.354378720206)) ;
#76077 = CARTESIAN_POINT('Ctrl Pts',(-18.2041945366287,-33.5574901056942,
123.365854477829)) ;
#76078 = CARTESIAN_POINT('Ctrl Pts',(-17.9153845548777,-33.7473457113166,
123.613370405314)) ;
#76079 = CARTESIAN_POINT('Ctrl Pts',(-18.2141592554439,-33.5673566308979,
123.573047516046)) ;
#76080 = CARTESIAN_POINT('Ctrl Pts',(-17.9729030335176,-33.7573331393624,
123.869417371831)) ;
#76081 = CARTESIAN_POINT('Ctrl Pts',(-18.2601719160976,-33.5773440589437,
123.777885465428)) ;
#76082 = CARTESIAN_POINT('Ctrl Pts',(-18.0734724275079,-33.7672780690488,
124.110676065915)) ;
#76083 = CARTESIAN_POINT('Ctrl Pts',(-18.3406253653803,-33.5872889886301,
123.970893079309)) ;
#76084 = CARTESIAN_POINT('Ctrl Pts',(-18.2159131529167,-33.7773229871573,
124.332886434343)) ;
#76085 = CARTESIAN_POINT('Ctrl Pts',(-18.4545761429792,-33.5973339067386,
124.14866254757)) ;
#76086 = CARTESIAN_POINT('Ctrl Pts',(-18.391376037984,-33.7871849567712,124.523645046394)) ;
#76087 = CARTESIAN_POINT('Ctrl Pts',(-18.5949446249841,-33.6071958763525,
124.301270653746)) ;
#76088 = CARTESIAN_POINT('Ctrl Pts',(-18.5996633148783,-33.7971770247925,
124.683493416161)) ;
#76089 = CARTESIAN_POINT('Ctrl Pts',(-18.7615730437336,-33.6171879443737,
124.429151053145)) ;
#76090 = CARTESIAN_POINT('Ctrl Pts',(-18.8311757134358,-33.807107950167,124.803984732188)) ;
#76091 = CARTESIAN_POINT('Ctrl Pts',(-18.9467817879391,-33.6271188697483,
124.525545974419)) ;
#76092 = CARTESIAN_POINT('Ctrl Pts',(-19.0804210324895,-33.8170585783905,
124.883010582598)) ;
#76093 = CARTESIAN_POINT('Ctrl Pts',(-19.1461772488705,-33.6370694979717,
124.588768739218)) ;
#76094 = CARTESIAN_POINT('Ctrl Pts',(-19.3409209971881,-33.8270588174496,
124.917887618055)) ;
#76095 = CARTESIAN_POINT('Ctrl Pts',(-19.3545768691479,-33.6470697370308,
124.616672564472)) ;
#76096 = CARTESIAN_POINT('Ctrl Pts',(-19.6042058083213,-33.8370872728188,
124.906594290963)) ;
#76097 = CARTESIAN_POINT('Ctrl Pts',(-19.5652047628629,-33.6570981924,124.607640132786)) ;
#76098 = CARTESIAN_POINT('Ctrl Pts',(-19.8574687091676,-33.8469533074021,
124.851055548334)) ;
#76099 = CARTESIAN_POINT('Ctrl Pts',(-19.767815408138,-33.6669642269833,124.563211299104)) ;
#76100 = CARTESIAN_POINT('Ctrl Pts',(-20.1004399415892,-33.8569456291495,
124.751536397017)) ;
#76101 = CARTESIAN_POINT('Ctrl Pts',(-19.9621930061691,-33.6769565487307,
124.483598313414)) ;
#76102 = CARTESIAN_POINT('Ctrl Pts',(-20.3211678424229,-33.8668779188265,
124.612195664148)) ;
#76103 = CARTESIAN_POINT('Ctrl Pts',(-20.1387771157398,-33.6868888384077,
124.372126818241)) ;
#76104 = CARTESIAN_POINT('Ctrl Pts',(-20.5158504185052,-33.8768795637972,
124.435627299948)) ;
#76105 = CARTESIAN_POINT('Ctrl Pts',(-20.2945221175348,-33.6968904833785,
124.230877050889)) ;
#76106 = CARTESIAN_POINT('Ctrl Pts',(-20.730134344233,-33.8901921972132,124.159073181057)) ;
#76107 = CARTESIAN_POINT('Ctrl Pts',(-20.4659641625927,-33.7102031167945,
124.009619650892)) ;
#76108 = CARTESIAN_POINT('Ctrl Pts',(-20.8667466131401,-33.9034239465948,
123.835025634175)) ;
#76109 = CARTESIAN_POINT('Ctrl Pts',(-20.5752544036822,-33.7234348661761,
123.750361646045)) ;
#76110 = CARTESIAN_POINT('Ctrl Pts',(-20.9147529609459,-33.9167472114119,
123.488209575829)) ;
#76111 = CARTESIAN_POINT('Ctrl Pts',(-20.613652637114,-33.7367581309931,123.47295053957)) ;
#76112 = CARTESIAN_POINT('Ctrl Pts',(-20.9055507234748,-33.9266229176296,
123.228839180921)) ;
#76113 = CARTESIAN_POINT('Ctrl Pts',(-20.6062950688991,-33.7466338372108,
123.265445862905)) ;
#76114 = CARTESIAN_POINT('Ctrl Pts',(-20.8511725358369,-33.9366125087296,
122.972045792738)) ;
#76115 = CARTESIAN_POINT('Ctrl Pts',(-20.5627941970681,-33.7566234283109,
123.060012946144)) ;
#76116 = CARTESIAN_POINT('Ctrl Pts',(-20.7537843024059,-33.946539605185,122.729998734827)) ;
#76117 = CARTESIAN_POINT('Ctrl Pts',(-20.4848858225803,-33.7665505247663,
122.866373858558)) ;
#76118 = CARTESIAN_POINT('Ctrl Pts',(-20.6145413557594,-33.9565647536896,
122.506380398541)) ;
#76119 = CARTESIAN_POINT('Ctrl Pts',(-20.3734933698443,-33.7765756732709,
122.687478231554)) ;
#76120 = CARTESIAN_POINT('Ctrl Pts',(-20.4409482370031,-33.9664604078363,
122.312726536697)) ;
#76121 = CARTESIAN_POINT('Ctrl Pts',(-20.2346204969347,-33.7864713274175,
122.532553555553)) ;
#76122 = CARTESIAN_POINT('Ctrl Pts',(-20.2344050443402,-33.9764639422145,
122.15014179103)) ;
#76123 = CARTESIAN_POINT('Ctrl Pts',(-20.0693873459231,-33.7964748617957,
122.402484058768)) ;
#76124 = CARTESIAN_POINT('Ctrl Pts',(-20.0031251937128,-33.9864490806545,
122.026110363631)) ;
#76125 = CARTESIAN_POINT('Ctrl Pts',(-19.8843645383385,-33.8064600002358,
122.303256977614)) ;
#76126 = CARTESIAN_POINT('Ctrl Pts',(-19.7525232072427,-33.9964850052499,
121.943972168171)) ;
#76127 = CARTESIAN_POINT('Ctrl Pts',(-19.6838837485256,-33.8164959248312,
122.237544337022)) ;
#76128 = CARTESIAN_POINT('Ctrl Pts',(-19.4963012262172,-34.0063362806776,
121.906976170248)) ;
#76129 = CARTESIAN_POINT('Ctrl Pts',(-19.4789062849549,-33.8263472002588,
122.207945321101)) ;
#76130 = CARTESIAN_POINT('Ctrl Pts',(-19.2338112579633,-34.0163285418389,
121.914396519878)) ;
#76131 = CARTESIAN_POINT('Ctrl Pts',(-19.2689142641197,-33.8363394614202,
122.213879435451)) ;
#76132 = CARTESIAN_POINT('Ctrl Pts',(-18.9755284714403,-34.0263684258565,
121.968182550253)) ;
#76133 = CARTESIAN_POINT('Ctrl Pts',(-19.0622876995497,-33.8463793454378,
122.256906084154)) ;
#76134 = CARTESIAN_POINT('Ctrl Pts',(-18.7352293588576,-34.036203200359,122.063406918067)) ;
#76135 = CARTESIAN_POINT('Ctrl Pts',(-18.8700473962123,-33.8562141199402,
122.333083630202)) ;
#76136 = CARTESIAN_POINT('Ctrl Pts',(-18.5097194263929,-34.0462795813793,
122.202115742351)) ;
#76137 = CARTESIAN_POINT('Ctrl Pts',(-18.6896381792612,-33.8662905009605,
122.444048990142)) ;
#76138 = CARTESIAN_POINT('Ctrl Pts',(-18.3161370097304,-34.0561258545299,
122.373856170595)) ;
#76139 = CARTESIAN_POINT('Ctrl Pts',(-18.534771813737,-33.8761367741112,122.581439034222)) ;
#76140 = CARTESIAN_POINT('Ctrl Pts',(-18.0973641720039,-34.0694903758151,
122.648596301524)) ;
#76141 = CARTESIAN_POINT('Ctrl Pts',(-18.3597451619224,-33.8895012953964,
122.801233992996)) ;
#76142 = CARTESIAN_POINT('Ctrl Pts',(-17.9574233666502,-34.0826966202496,
122.970485787033)) ;
#76143 = CARTESIAN_POINT('Ctrl Pts',(-18.2477846414627,-33.9027075398308,
123.058779978968)) ;
#76144 = CARTESIAN_POINT('Ctrl Pts',(-17.9048166903055,-34.0959615749268,
123.315069758418)) ;
#76145 = CARTESIAN_POINT('Ctrl Pts',(-18.2057090036201,-33.9159724945081,
123.334400438449)) ;
#76146 = CARTESIAN_POINT('Ctrl Pts',(-17.9110068531444,-34.1059938554785,
123.57864144409)) ;
#76147 = CARTESIAN_POINT('Ctrl Pts',(-18.2106566732483,-33.9260047750597,
123.545267055076)) ;
#76148 = CARTESIAN_POINT('Ctrl Pts',(-17.9622064694979,-34.1159025889964,
123.83394390301)) ;
#76149 = CARTESIAN_POINT('Ctrl Pts',(-18.2516149524503,-33.9359135085776,
123.749507096678)) ;
#76150 = CARTESIAN_POINT('Ctrl Pts',(-18.0566040744256,-34.1258401398639,
124.077443630535)) ;
#76151 = CARTESIAN_POINT('Ctrl Pts',(-18.3271318142154,-33.9458510594451,
123.944309004323)) ;
#76152 = CARTESIAN_POINT('Ctrl Pts',(-18.1932746080378,-34.1358699874578,
124.302786499477)) ;
#76153 = CARTESIAN_POINT('Ctrl Pts',(-18.4364641738599,-33.9558809070391,
124.124582034141)) ;
#76154 = CARTESIAN_POINT('Ctrl Pts',(-18.4222258928421,-34.1491051273782,
124.564718290343)) ;
#76155 = CARTESIAN_POINT('Ctrl Pts',(-18.6196353445962,-33.9691160469595,
124.334139139703)) ;
#76156 = CARTESIAN_POINT('Ctrl Pts',(-18.79005327306,-34.1657735917494,124.811391878925)) ;
#76157 = CARTESIAN_POINT('Ctrl Pts',(-18.9138856664441,-33.9857845113307,
124.531468849858)) ;
#76158 = CARTESIAN_POINT('Ctrl Pts',(-19.302810003159,-34.1856446036233,124.93867473504)) ;
#76159 = CARTESIAN_POINT('Ctrl Pts',(-19.3240782602018,-34.0056555232046,
124.633306456755)) ;
#76160 = CARTESIAN_POINT('Ctrl Pts',(-19.7442781237736,-34.2023516880063,
124.892055705492)) ;
#76161 = CARTESIAN_POINT('Ctrl Pts',(-19.6773043553831,-34.0223626075875,
124.596000463399)) ;
#76162 = CARTESIAN_POINT('Ctrl Pts',(-20.0675644893063,-34.2155289693169,
124.767792583649)) ;
#76163 = CARTESIAN_POINT('Ctrl Pts',(-19.935888328374,-34.0355398888981,124.496604100906)) ;
#76164 = CARTESIAN_POINT('Ctrl Pts',(-20.3669683528388,-34.228796429831,124.589169379332)) ;
#76165 = CARTESIAN_POINT('Ctrl Pts',(-20.1754272032707,-34.0488073494122,
124.353698951168)) ;
#76166 = CARTESIAN_POINT('Ctrl Pts',(-20.6747925424677,-34.2454103205182,
124.272577564585)) ;
#76167 = CARTESIAN_POINT('Ctrl Pts',(-20.4216796479605,-34.0654212400994,
124.100434565729)) ;
#76168 = CARTESIAN_POINT('Ctrl Pts',(-20.8925501700645,-34.2653591199456,
123.789095141631)) ;
#76169 = CARTESIAN_POINT('Ctrl Pts',(-20.5958914715679,-34.0853700395268,
123.713647108598)) ;
#76170 = CARTESIAN_POINT('Ctrl Pts',(-20.9320934628984,-34.2852802314764,
123.261176948921)) ;
#76171 = CARTESIAN_POINT('Ctrl Pts',(-20.627528243359,-34.1052911510577,123.29131282389)) ;
#76172 = CARTESIAN_POINT('Ctrl Pts',(-20.7905220574422,-34.3051466796493,
122.752407298915)) ;
#76173 = CARTESIAN_POINT('Ctrl Pts',(-20.5142733449368,-34.1251575992306,
122.884295234101)) ;
#76174 = CARTESIAN_POINT('Ctrl Pts',(-20.4811847889184,-34.3251730262664,
122.319328242718)) ;
#76175 = CARTESIAN_POINT('Ctrl Pts',(-20.2668055516656,-34.1451839458477,
122.537830873447)) ;
#76176 = CARTESIAN_POINT('Ctrl Pts',(-20.046046929039,-34.345035070656,122.02027991162)) ;
#76177 = CARTESIAN_POINT('Ctrl Pts',(-19.9186955596424,-34.1650459902372,
122.298589641338)) ;
#76178 = CARTESIAN_POINT('Ctrl Pts',(-19.5332082975731,-34.3649803733371,
121.886348768539)) ;
#76179 = CARTESIAN_POINT('Ctrl Pts',(-19.5084245595147,-34.1849912929184,
122.191442818576)) ;
#76180 = CARTESIAN_POINT('Ctrl Pts',(-19.0066946738913,-34.384875680396,121.935430157998)) ;
#76181 = CARTESIAN_POINT('Ctrl Pts',(-19.0872124491375,-34.2048865999772,
122.230706348824)) ;
#76182 = CARTESIAN_POINT('Ctrl Pts',(-18.5281796662803,-34.4047689505636,
122.160351280657)) ;
#76183 = CARTESIAN_POINT('Ctrl Pts',(-18.7043988887934,-34.2247798701449,
122.410642726589)) ;
#76184 = CARTESIAN_POINT('Ctrl Pts',(-18.1538942484392,-34.424734543244,122.536474463876)) ;
#76185 = CARTESIAN_POINT('Ctrl Pts',(-18.404969560696,-34.2447454628253,122.711540862601)) ;
#76186 = CARTESIAN_POINT('Ctrl Pts',(-17.9310744456909,-34.4446098669289,
123.015467619832)) ;
#76187 = CARTESIAN_POINT('Ctrl Pts',(-18.2267125107953,-34.2646207865101,
123.094736487549)) ;
#76188 = CARTESIAN_POINT('Ctrl Pts',(-17.8843177629388,-34.4645849295038,
123.544333074605)) ;
#76189 = CARTESIAN_POINT('Ctrl Pts',(-18.1893069457108,-34.2845958490851,
123.517829108664)) ;
#76190 = CARTESIAN_POINT('Ctrl Pts',(-18.0214586110125,-34.484537339135,124.056594429995)) ;
#76191 = CARTESIAN_POINT('Ctrl Pts',(-18.2990194229785,-34.3045482587162,
123.927638867659)) ;
#76192 = CARTESIAN_POINT('Ctrl Pts',(-18.3225640751272,-34.504373393371,124.489356119878)) ;
#76193 = CARTESIAN_POINT('Ctrl Pts',(-18.5399052793811,-34.3243843129523,
124.27384976748)) ;
#76194 = CARTESIAN_POINT('Ctrl Pts',(-18.7560161142361,-34.5243513047886,
124.796045846315)) ;
#76195 = CARTESIAN_POINT('Ctrl Pts',(-18.8866675828867,-34.3443622243698,
124.519201026929)) ;
#76196 = CARTESIAN_POINT('Ctrl Pts',(-19.266703075915,-34.5442693542921,124.935377333692)) ;
#76197 = CARTESIAN_POINT('Ctrl Pts',(-19.2952182947917,-34.3642802738733,
124.630665776378)) ;
#76198 = CARTESIAN_POINT('Ctrl Pts',(-19.7932159078687,-34.5641374980602,
124.893556756137)) ;
#76199 = CARTESIAN_POINT('Ctrl Pts',(-19.7164298223103,-34.3841484176414,
124.597207716313)) ;
#76200 = CARTESIAN_POINT('Ctrl Pts',(-20.2777146691111,-34.5841883546475,
124.671918199615)) ;
#76201 = CARTESIAN_POINT('Ctrl Pts',(-20.1040278270987,-34.4041992742287,
124.419895848041)) ;
#76202 = CARTESIAN_POINT('Ctrl Pts',(-20.6529658815837,-34.6039687911034,
124.3034966869)) ;
#76203 = CARTESIAN_POINT('Ctrl Pts',(-20.4042291464414,-34.4239797106846,
124.125155886527)) ;
#76204 = CARTESIAN_POINT('Ctrl Pts',(-20.8834863291553,-34.6239988467812,
123.823760909357)) ;
#76205 = CARTESIAN_POINT('Ctrl Pts',(-20.5886433844177,-34.4440097663624,
123.74136659525)) ;
#76206 = CARTESIAN_POINT('Ctrl Pts',(-20.9351889706726,-34.643879951956,123.297798988624)) ;
#76207 = CARTESIAN_POINT('Ctrl Pts',(-20.6300035954088,-34.4638908715372,
123.32059580445)) ;
#76208 = CARTESIAN_POINT('Ctrl Pts',(-20.8057903344438,-34.6637604143238,
122.785553366856)) ;
#76209 = CARTESIAN_POINT('Ctrl Pts',(-20.5264818601808,-34.483771333905,122.910799001557)) ;
#76210 = CARTESIAN_POINT('Ctrl Pts',(-20.5076352220896,-34.6837455614681,
122.345932909979)) ;
#76211 = CARTESIAN_POINT('Ctrl Pts',(-20.2879554585398,-34.5037564810494,
122.559104093687)) ;
#76212 = CARTESIAN_POINT('Ctrl Pts',(-20.0793236955873,-34.7036361400045,
122.036027427031)) ;
#76213 = CARTESIAN_POINT('Ctrl Pts',(-19.9453039222835,-34.5236470595857,
122.311181522728)) ;
#76214 = CARTESIAN_POINT('Ctrl Pts',(-19.5711560383536,-34.7235301598789,
121.889965636208)) ;
#76215 = CARTESIAN_POINT('Ctrl Pts',(-19.5387682446119,-34.5435410794601,
122.1943349732)) ;
#76216 = CARTESIAN_POINT('Ctrl Pts',(-19.0429893283556,-34.7434516046053,
121.925987779799)) ;
#76217 = CARTESIAN_POINT('Ctrl Pts',(-19.1162346135711,-34.5634625241865,
122.223156059284)) ;
#76218 = CARTESIAN_POINT('Ctrl Pts',(-18.5587933442751,-34.7633497426607,
122.139065599322)) ;
#76219 = CARTESIAN_POINT('Ctrl Pts',(-18.7288788359676,-34.583360662242,122.393621850554)) ;
#76220 = CARTESIAN_POINT('Ctrl Pts',(-18.1739396123522,-34.7834204978768,
122.508326536846)) ;
#76221 = CARTESIAN_POINT('Ctrl Pts',(-18.4209985757421,-34.603431417458,122.689032837873)) ;
#76222 = CARTESIAN_POINT('Ctrl Pts',(-17.9412291316827,-34.803206047928,122.980030562357)) ;
#76223 = CARTESIAN_POINT('Ctrl Pts',(-18.234833032526,-34.6232169675093,123.066398644646)) ;
#76224 = CARTESIAN_POINT('Ctrl Pts',(-17.8816194221956,-34.8231891228054,
123.507694573196)) ;
#76225 = CARTESIAN_POINT('Ctrl Pts',(-18.1871490553495,-34.6432000423866,
123.488530272471)) ;
#76226 = CARTESIAN_POINT('Ctrl Pts',(-18.0060182322605,-34.8430982054513,
124.022021160896)) ;
#76227 = CARTESIAN_POINT('Ctrl Pts',(-18.2866725880628,-34.6631091250326,
123.899991117196)) ;
#76228 = CARTESIAN_POINT('Ctrl Pts',(-18.296486524571,-34.8629567645741,124.462795927033)) ;
#76229 = CARTESIAN_POINT('Ctrl Pts',(-18.5190486895846,-34.6829676841553,
124.252608470384)) ;
#76230 = CARTESIAN_POINT('Ctrl Pts',(-18.7241036773719,-34.8830002084128,
124.780319588306)) ;
#76231 = CARTESIAN_POINT('Ctrl Pts',(-18.8611532239642,-34.703011127994,124.506625843281)) ;
#76232 = CARTESIAN_POINT('Ctrl Pts',(-19.1443314362072,-34.899500273142,124.906184977556)) ;
#76233 = CARTESIAN_POINT('Ctrl Pts',(-19.1973104768277,-34.7195111927232,
124.607308957452)) ;
#76234 = CARTESIAN_POINT('Ctrl Pts',(-19.4959856145743,-34.9128900129909,
124.916808895256)) ;
#76235 = CARTESIAN_POINT('Ctrl Pts',(-19.4786571226114,-34.7329009325721,
124.615810467763)) ;
#76236 = CARTESIAN_POINT('Ctrl Pts',(-19.7523697501697,-34.9227469141993,
124.879642738645)) ;
#76237 = CARTESIAN_POINT('Ctrl Pts',(-19.6837596469558,-34.7427578337805,
124.586074466439)) ;
#76238 = CARTESIAN_POINT('Ctrl Pts',(-20.0018598352165,-34.9327384400458,
124.797951435876)) ;
#76239 = CARTESIAN_POINT('Ctrl Pts',(-19.8833526563097,-34.752749359627,124.520719090591)) ;
#76240 = CARTESIAN_POINT('Ctrl Pts',(-20.2319445661498,-34.9426631204967,
124.675054574877)) ;
#76241 = CARTESIAN_POINT('Ctrl Pts',(-20.0674176841992,-34.762674040078,124.4224015819)) ;
#76242 = CARTESIAN_POINT('Ctrl Pts',(-20.4389718038519,-34.9526737105411,
124.512809926681)) ;
#76243 = CARTESIAN_POINT('Ctrl Pts',(-20.2330436587693,-34.7726846301224,
124.292596602303)) ;
#76244 = CARTESIAN_POINT('Ctrl Pts',(-20.6720998991918,-34.9659329712448,
124.253723717927)) ;
#76245 = CARTESIAN_POINT('Ctrl Pts',(-20.4195165683706,-34.7859438908261,
124.085363349355)) ;
#76246 = CARTESIAN_POINT('Ctrl Pts',(-20.8329350806872,-34.9792840463951,
123.937545082289)) ;
#76247 = CARTESIAN_POINT('Ctrl Pts',(-20.5482036204118,-34.7992949659763,
123.832398938157)) ;
#76248 = CARTESIAN_POINT('Ctrl Pts',(-20.9051329386564,-34.9924903556299,
123.598017654261)) ;
#76249 = CARTESIAN_POINT('Ctrl Pts',(-20.605960739995,-34.8125012752111,123.56076258238)) ;
#76250 = CARTESIAN_POINT('Ctrl Pts',(-20.9148428908615,-35.0024771892202,
123.335798885089)) ;
#76251 = CARTESIAN_POINT('Ctrl Pts',(-20.6137261079857,-34.8224881088014,
123.350990280824)) ;
#76252 = CARTESIAN_POINT('Ctrl Pts',(-20.8791149641005,-35.0124299167163,
123.076657694383)) ;
#76253 = CARTESIAN_POINT('Ctrl Pts',(-20.5851416344258,-34.8324408362975,
123.143676914264)) ;
#76254 = CARTESIAN_POINT('Ctrl Pts',(-20.7979778137027,-35.0224780135579,
122.825409407671)) ;
#76255 = CARTESIAN_POINT('Ctrl Pts',(-20.5202297765397,-34.8424889331391,
122.942679247368)) ;
#76256 = CARTESIAN_POINT('Ctrl Pts',(-20.6772333062883,-35.0323194704297,
122.596674503365)) ;
#76257 = CARTESIAN_POINT('Ctrl Pts',(-20.4236321706692,-34.8523303900109,
122.759692291335)) ;
#76258 = CARTESIAN_POINT('Ctrl Pts',(-20.5167579761927,-35.0423057373431,
122.389083764438)) ;
#76259 = CARTESIAN_POINT('Ctrl Pts',(-20.2952501539374,-34.8623166569244,
122.593621150654)) ;
#76260 = CARTESIAN_POINT('Ctrl Pts',(-20.3236651758144,-35.0522423382436,
122.213233449204)) ;
#76261 = CARTESIAN_POINT('Ctrl Pts',(-20.1407744379203,-34.8722532578248,
122.452942601343)) ;
#76262 = CARTESIAN_POINT('Ctrl Pts',(-20.1004431976112,-35.0622922810306,
122.072138574623)) ;
#76263 = CARTESIAN_POINT('Ctrl Pts',(-19.9621956872849,-34.8823032006119,
122.340068638975)) ;
#76264 = CARTESIAN_POINT('Ctrl Pts',(-19.8610023890791,-35.0721424807164,
121.973740369794)) ;
#76265 = CARTESIAN_POINT('Ctrl Pts',(-19.7706422695711,-34.8921534002976,
122.261352199334)) ;
#76266 = CARTESIAN_POINT('Ctrl Pts',(-19.6051578614326,-35.0821153856485,
121.917057183001)) ;
#76267 = CARTESIAN_POINT('Ctrl Pts',(-19.5659662526582,-34.9021263052297,
122.216007866642)) ;
#76268 = CARTESIAN_POINT('Ctrl Pts',(-19.3426236375275,-35.0921137601281,
121.905710783853)) ;
#76269 = CARTESIAN_POINT('Ctrl Pts',(-19.3559388367088,-34.9121246797094,
122.206932993469)) ;
#76270 = CARTESIAN_POINT('Ctrl Pts',(-19.0816040718375,-35.1021339339981,
121.940379135777)) ;
#76271 = CARTESIAN_POINT('Ctrl Pts',(-19.1471235237251,-34.9221448535794,
122.234669903381)) ;
#76272 = CARTESIAN_POINT('Ctrl Pts',(-18.8334713867964,-35.1120349779401,
122.018687487748)) ;
#76273 = CARTESIAN_POINT('Ctrl Pts',(-18.9486181859309,-34.9320458975213,
122.297318684873)) ;
#76274 = CARTESIAN_POINT('Ctrl Pts',(-18.6004760333388,-35.1220237816644,
122.139585076193)) ;
#76275 = CARTESIAN_POINT('Ctrl Pts',(-18.7622230038763,-34.9420347012456,
122.394038699726)) ;
#76276 = CARTESIAN_POINT('Ctrl Pts',(-18.3926205882541,-35.1319892484962,
122.298870810945)) ;
#76277 = CARTESIAN_POINT('Ctrl Pts',(-18.5959400898762,-34.9520001680775,
122.521469007001)) ;
#76278 = CARTESIAN_POINT('Ctrl Pts',(-18.2161904040798,-35.1418928107692,
122.490230413677)) ;
#76279 = CARTESIAN_POINT('Ctrl Pts',(-18.4547977047164,-34.9619037303504,
122.674558035766)) ;
#76280 = CARTESIAN_POINT('Ctrl Pts',(-18.0736527311834,-35.1519534886472,
122.712860272245)) ;
#76281 = CARTESIAN_POINT('Ctrl Pts',(-18.3407694238614,-34.9719644082284,
122.852663144503)) ;
#76282 = CARTESIAN_POINT('Ctrl Pts',(-17.9738293171921,-35.1617937865966,
122.951450001388)) ;
#76283 = CARTESIAN_POINT('Ctrl Pts',(-18.2609128496764,-34.9818047061779,
123.043535471726)) ;
#76284 = CARTESIAN_POINT('Ctrl Pts',(-17.9153656042715,-35.1718567815061,
123.209316008971)) ;
#76285 = CARTESIAN_POINT('Ctrl Pts',(-18.2141439991331,-34.9918677010873,
123.249828796046)) ;
#76286 = CARTESIAN_POINT('Ctrl Pts',(-17.9029906880306,-35.1817510756532,
123.469061216251)) ;
#76287 = CARTESIAN_POINT('Ctrl Pts',(-18.2042462718512,-35.0017619952345,
123.457624801608)) ;
#76288 = CARTESIAN_POINT('Ctrl Pts',(-17.9353509723989,-35.1916928733501,
123.728277083036)) ;
#76289 = CARTESIAN_POINT('Ctrl Pts',(-18.230136599556,-35.0117037929313,123.664997019035)) ;
#76290 = CARTESIAN_POINT('Ctrl Pts',(-18.0126256103988,-35.2016954508792,
123.979555436244)) ;
#76291 = CARTESIAN_POINT('Ctrl Pts',(-18.2919583264141,-35.0217063704604,
123.866019011557)) ;
#76292 = CARTESIAN_POINT('Ctrl Pts',(-18.1330779755953,-35.2117299148002,
124.214117512303)) ;
#76293 = CARTESIAN_POINT('Ctrl Pts',(-18.3883221539504,-35.0317408343815,
124.053667693136)) ;
#76294 = CARTESIAN_POINT('Ctrl Pts',(-18.2891276129428,-35.2215760533213,
124.420521008454)) ;
#76295 = CARTESIAN_POINT('Ctrl Pts',(-18.5131632916011,-35.0415869729026,
124.218788844697)) ;
#76296 = CARTESIAN_POINT('Ctrl Pts',(-18.4808245708617,-35.2315572265583,
124.599517750244)) ;
#76297 = CARTESIAN_POINT('Ctrl Pts',(-18.6665221721677,-35.0515681461396,
124.361984625144)) ;
#76298 = CARTESIAN_POINT('Ctrl Pts',(-18.7001113066262,-35.2415095205156,
124.742060651138)) ;
#76299 = CARTESIAN_POINT('Ctrl Pts',(-18.8419525117809,-35.0615204400968,
124.476017085114)) ;
#76300 = CARTESIAN_POINT('Ctrl Pts',(-18.9418196622189,-35.2515083156502,
124.845159871801)) ;
#76301 = CARTESIAN_POINT('Ctrl Pts',(-19.0353199196314,-35.0715192352314,
124.558494551332)) ;
#76302 = CARTESIAN_POINT('Ctrl Pts',(-19.1988694220075,-35.261547423911,124.904462676916)) ;
#76303 = CARTESIAN_POINT('Ctrl Pts',(-19.2409602470283,-35.0815583434922,
124.605934759269)) ;
#76304 = CARTESIAN_POINT('Ctrl Pts',(-19.4566932433143,-35.2713723653501,
124.918494235249)) ;
#76305 = CARTESIAN_POINT('Ctrl Pts',(-19.4472187973089,-35.0913832849314,
124.617157941595)) ;
#76306 = CARTESIAN_POINT('Ctrl Pts',(-19.7190507496246,-35.2814270524245,
124.887257605377)) ;
#76307 = CARTESIAN_POINT('Ctrl Pts',(-19.6571046535086,-35.1014379720058,
124.592166657345)) ;
#76308 = CARTESIAN_POINT('Ctrl Pts',(-19.9690783925478,-35.2913698573647,
124.811356103784)) ;
#76309 = CARTESIAN_POINT('Ctrl Pts',(-19.8571259192075,-35.1113807769459,
124.531443580824)) ;
#76310 = CARTESIAN_POINT('Ctrl Pts',(-20.201572991337,-35.3012736433612,124.694371844352)) ;
#76311 = CARTESIAN_POINT('Ctrl Pts',(-20.0431203471688,-35.1212845629424,
124.437854636998)) ;
#76312 = CARTESIAN_POINT('Ctrl Pts',(-20.4131178490752,-35.311320459926,124.536438012356)) ;
#76313 = CARTESIAN_POINT('Ctrl Pts',(-20.2123551289518,-35.1313313795072,
124.311505953245)) ;
#76314 = CARTESIAN_POINT('Ctrl Pts',(-20.5915179796909,-35.3212159794047,
124.347180770811)) ;
#76315 = CARTESIAN_POINT('Ctrl Pts',(-20.3550735141645,-35.1412268989859,
124.160099180785)) ;
#76316 = CARTESIAN_POINT('Ctrl Pts',(-20.7367072779977,-35.3312780647291,
124.126231712298)) ;
#76317 = CARTESIAN_POINT('Ctrl Pts',(-20.4712234236235,-35.1512889843104,
123.983338754042)) ;
#76318 = CARTESIAN_POINT('Ctrl Pts',(-20.8392082178342,-35.341120775687,123.888720097005)) ;
#76319 = CARTESIAN_POINT('Ctrl Pts',(-20.5532221538063,-35.1611316952683,
123.793329345071)) ;
#76320 = CARTESIAN_POINT('Ctrl Pts',(-20.9004009017914,-35.3511114929931,
123.633439183863)) ;
#76321 = CARTESIAN_POINT('Ctrl Pts',(-20.6021745071673,-35.1711224125743,
123.589104328749)) ;
#76322 = CARTESIAN_POINT('Ctrl Pts',(-20.9161968439774,-35.3610395760897,
123.373005745108)) ;
#76323 = CARTESIAN_POINT('Ctrl Pts',(-20.6148094255355,-35.1810504956709,
123.38075785787)) ;
#76324 = CARTESIAN_POINT('Ctrl Pts',(-20.8868090726175,-35.3710275062014,
123.112172972234)) ;
#76325 = CARTESIAN_POINT('Ctrl Pts',(-20.5912974941036,-35.1910384257827,
123.172091979698)) ;
#76326 = CARTESIAN_POINT('Ctrl Pts',(-20.8118024545618,-35.3810633323287,
122.859341843784)) ;
#76327 = CARTESIAN_POINT('Ctrl Pts',(-20.5312904395145,-35.20107425191,122.969827526995)) ;
#76328 = CARTESIAN_POINT('Ctrl Pts',(-20.6965136130344,-35.3909186694423,
122.627413231275)) ;
#76329 = CARTESIAN_POINT('Ctrl Pts',(-20.4390581291398,-35.2109295890236,
122.784286070346)) ;
#76330 = CARTESIAN_POINT('Ctrl Pts',(-20.5408432692732,-35.4009164042925,
122.415802978971)) ;
#76331 = CARTESIAN_POINT('Ctrl Pts',(-20.3145205770678,-35.2209273238737,
122.614998959278)) ;
#76332 = CARTESIAN_POINT('Ctrl Pts',(-20.3525343320778,-35.4108243082769,
122.235974665566)) ;
#76333 = CARTESIAN_POINT('Ctrl Pts',(-20.1638726660472,-35.2308352278582,
122.471137872087)) ;
#76334 = CARTESIAN_POINT('Ctrl Pts',(-20.1338538120055,-35.4208353828254,
122.089706748556)) ;
#76335 = CARTESIAN_POINT('Ctrl Pts',(-19.9889274042967,-35.2408463024066,
122.354124872877)) ;
#76336 = CARTESIAN_POINT('Ctrl Pts',(-19.8924829761776,-35.430863238361,121.983948431129)) ;
#76337 = CARTESIAN_POINT('Ctrl Pts',(-19.7958300154897,-35.2508741579423,
122.26951973446)) ;
#76338 = CARTESIAN_POINT('Ctrl Pts',(-19.6408783355225,-35.4407208322662,
121.922312589323)) ;
#76339 = CARTESIAN_POINT('Ctrl Pts',(-19.5945467001667,-35.2607317518475,
122.220212798044)) ;
#76340 = CARTESIAN_POINT('Ctrl Pts',(-19.3779878358357,-35.4507475191043,
121.904471410779)) ;
#76341 = CARTESIAN_POINT('Ctrl Pts',(-19.3842341773709,-35.2707584386856,
122.205941341526)) ;
#76342 = CARTESIAN_POINT('Ctrl Pts',(-19.1160071597598,-35.4607761882581,
121.933207053229)) ;
#76343 = CARTESIAN_POINT('Ctrl Pts',(-19.1746497551832,-35.2807871078393,
122.228931467457)) ;
#76344 = CARTESIAN_POINT('Ctrl Pts',(-18.8675097602548,-35.4706213965395,
122.005176454191)) ;
#76345 = CARTESIAN_POINT('Ctrl Pts',(-18.975853120482,-35.2906323161207,122.286508201954)) ;
#76346 = CARTESIAN_POINT('Ctrl Pts',(-18.6315240045913,-35.4806120855026,
122.120258716162)) ;
#76347 = CARTESIAN_POINT('Ctrl Pts',(-18.787065262531,-35.3006230050839,122.3785751853)) ;
#76348 = CARTESIAN_POINT('Ctrl Pts',(-18.4184551336029,-35.4906499617849,
122.275766762473)) ;
#76349 = CARTESIAN_POINT('Ctrl Pts',(-18.6166109641243,-35.3106608813661,
122.502982897611)) ;
#76350 = CARTESIAN_POINT('Ctrl Pts',(-18.2388143580411,-35.5004943394271,
122.461939201229)) ;
#76351 = CARTESIAN_POINT('Ctrl Pts',(-18.472900009195,-35.3205052590084,122.651921150758)) ;
#76352 = CARTESIAN_POINT('Ctrl Pts',(-18.0917605509489,-35.5104791438185,
122.679207506893)) ;
#76353 = CARTESIAN_POINT('Ctrl Pts',(-18.3552581535845,-35.3304900633998,
122.825736359485)) ;
#76354 = CARTESIAN_POINT('Ctrl Pts',(-17.9850190705562,-35.5204186740371,
122.917641507262)) ;
#76355 = CARTESIAN_POINT('Ctrl Pts',(-18.2698663114521,-35.3404295936183,
123.016483683079)) ;
#76356 = CARTESIAN_POINT('Ctrl Pts',(-17.9207300902024,-35.530458362074,123.173500108598)) ;
#76357 = CARTESIAN_POINT('Ctrl Pts',(-18.2184363504254,-35.3504692816552,
123.221170992911)) ;
#76358 = CARTESIAN_POINT('Ctrl Pts',(-17.9019975599719,-35.5403466514423,
123.432693219791)) ;
#76359 = CARTESIAN_POINT('Ctrl Pts',(-18.2034516388014,-35.3603575710235,
123.428524836043)) ;
#76360 = CARTESIAN_POINT('Ctrl Pts',(-17.9283290133231,-35.5503357751271,
123.693863790496)) ;
#76361 = CARTESIAN_POINT('Ctrl Pts',(-18.2245179343512,-35.3703466947083,
123.637461006412)) ;
#76362 = CARTESIAN_POINT('Ctrl Pts',(-17.9995984432438,-35.5602957848017,
123.945708092108)) ;
#76363 = CARTESIAN_POINT('Ctrl Pts',(-18.2815345383664,-35.3803067043829,
123.83893578616)) ;
#76364 = CARTESIAN_POINT('Ctrl Pts',(-18.1122794988798,-35.5701962145059,
124.180223126133)) ;
#76365 = CARTESIAN_POINT('Ctrl Pts',(-18.3716800348444,-35.3902071340872,
124.026546724073)) ;
#76366 = CARTESIAN_POINT('Ctrl Pts',(-18.2661525939109,-35.5802392959127,
124.394633262536)) ;
#76367 = CARTESIAN_POINT('Ctrl Pts',(-18.4947794676731,-35.4002502154939,
124.198074338897)) ;
#76368 = CARTESIAN_POINT('Ctrl Pts',(-18.4523813316654,-35.5901466898203,
124.576598857735)) ;
#76369 = CARTESIAN_POINT('Ctrl Pts',(-18.6437627318548,-35.4101576094016,
124.343645597368)) ;
#76370 = CARTESIAN_POINT('Ctrl Pts',(-18.6693558213906,-35.6001584208095,
124.725406064424)) ;
#76371 = CARTESIAN_POINT('Ctrl Pts',(-18.817342832175,-35.4201693403907,124.462690554545)) ;
#76372 = CARTESIAN_POINT('Ctrl Pts',(-18.9095840015466,-35.6101906385243,
124.834028669313)) ;
#76373 = CARTESIAN_POINT('Ctrl Pts',(-19.0095258944054,-35.4302015581055,
124.549587692303)) ;
#76374 = CARTESIAN_POINT('Ctrl Pts',(-19.1603393482512,-35.6200431477704,
124.898453661769)) ;
#76375 = CARTESIAN_POINT('Ctrl Pts',(-19.2101294376099,-35.4400540673517,
124.601126473367)) ;
#76376 = CARTESIAN_POINT('Ctrl Pts',(-19.4211928177093,-35.6300010843134,
124.919386454417)) ;
#76377 = CARTESIAN_POINT('Ctrl Pts',(-19.4188119019026,-35.4500120038947,
124.617871878894)) ;
#76378 = CARTESIAN_POINT('Ctrl Pts',(-19.6837654584698,-35.6400399543217,
124.894038281301)) ;
#76379 = CARTESIAN_POINT('Ctrl Pts',(-19.6288700585704,-35.460050873903,124.59759241855)) ;
#76380 = CARTESIAN_POINT('Ctrl Pts',(-19.933939291399,-35.64991310948,124.825100619507)) ;
#76381 = CARTESIAN_POINT('Ctrl Pts',(-19.8290080447909,-35.4699240290612,
124.542441760864)) ;
#76382 = CARTESIAN_POINT('Ctrl Pts',(-20.1729716448269,-35.6599863843297,
124.711483830353)) ;
#76383 = CARTESIAN_POINT('Ctrl Pts',(-20.0202338855392,-35.4799973039109,
124.451547444271)) ;
#76384 = CARTESIAN_POINT('Ctrl Pts',(-20.3835167615807,-35.6698067015071,
124.562152640073)) ;
#76385 = CARTESIAN_POINT('Ctrl Pts',(-20.1886685395271,-35.4898176210883,
124.332082614018)) ;
#76386 = CARTESIAN_POINT('Ctrl Pts',(-20.5697933970756,-35.6798853873006,
124.373961088666)) ;
#76387 = CARTESIAN_POINT('Ctrl Pts',(-20.337689632591,-35.4998963068818,124.1815286286)) ;
#76388 = CARTESIAN_POINT('Ctrl Pts',(-20.7173141231038,-35.6897368986837,
124.161139832824)) ;
#76389 = CARTESIAN_POINT('Ctrl Pts',(-20.4557050752507,-35.5097478182649,
124.011272119984)) ;
#76390 = CARTESIAN_POINT('Ctrl Pts',(-20.8282376598515,-35.6998103449903,
123.920835993588)) ;
#76391 = CARTESIAN_POINT('Ctrl Pts',(-20.5444435077093,-35.5198212645716,
123.81902847826)) ;
#76392 = CARTESIAN_POINT('Ctrl Pts',(-20.8941975463074,-35.709651620115,123.670739828065)) ;
#76393 = CARTESIAN_POINT('Ctrl Pts',(-20.5972105412205,-35.5296625396963,
123.618952491442)) ;
#76394 = CARTESIAN_POINT('Ctrl Pts',(-20.9168565667125,-35.7196367197718,
123.409346913405)) ;
#76395 = CARTESIAN_POINT('Ctrl Pts',(-20.6153373392901,-35.539647639353,123.409838356451)) ;
#76396 = CARTESIAN_POINT('Ctrl Pts',(-20.8933643886205,-35.7296441959061,
123.147392528949)) ;
#76397 = CARTESIAN_POINT('Ctrl Pts',(-20.5965431125166,-35.5496551154873,
123.200274949627)) ;
#76398 = CARTESIAN_POINT('Ctrl Pts',(-20.8255661488253,-35.739566783615,122.895618637238)) ;
#76399 = CARTESIAN_POINT('Ctrl Pts',(-20.5423042616246,-35.5595777031963,
122.998856548276)) ;
#76400 = CARTESIAN_POINT('Ctrl Pts',(-20.7147391059378,-35.7495533878884,
122.657703592523)) ;
#76401 = CARTESIAN_POINT('Ctrl Pts',(-20.4536424122356,-35.5695643074696,
122.80852482131)) ;
#76402 = CARTESIAN_POINT('Ctrl Pts',(-20.5631005958561,-35.7595935162225,
122.44181432367)) ;
#76403 = CARTESIAN_POINT('Ctrl Pts',(-20.3323311466458,-35.5796044358037,
122.635813545013)) ;
#76404 = CARTESIAN_POINT('Ctrl Pts',(-20.3803788347583,-35.7694329507559,
122.258824742505)) ;
#76405 = CARTESIAN_POINT('Ctrl Pts',(-20.1861543576817,-35.5894438703371,
122.489422939203)) ;
#76406 = CARTESIAN_POINT('Ctrl Pts',(-20.1640017994707,-35.7794970052469,
122.106806406676)) ;
#76407 = CARTESIAN_POINT('Ctrl Pts',(-20.0130523328328,-35.5995079248281,
122.36780830073)) ;
#76408 = CARTESIAN_POINT('Ctrl Pts',(-19.9285321533721,-35.789387924484,121.996676734364)) ;
#76409 = CARTESIAN_POINT('Ctrl Pts',(-19.8246772528639,-35.6093988440653,
122.279705175091)) ;
#76410 = CARTESIAN_POINT('Ctrl Pts',(-19.6751379025665,-35.7993799177901,
121.927884966062)) ;
#76411 = CARTESIAN_POINT('Ctrl Pts',(-19.6219619807546,-35.6193908373713,
122.224671942912)) ;
#76412 = CARTESIAN_POINT('Ctrl Pts',(-19.414382263436,-35.8093427817494,121.904446853301)) ;
#76413 = CARTESIAN_POINT('Ctrl Pts',(-19.4133578143958,-35.6293537013306,
122.205921690293)) ;
#76414 = CARTESIAN_POINT('Ctrl Pts',(-19.1549680514834,-35.8192470415671,
121.925855666105)) ;
#76415 = CARTESIAN_POINT('Ctrl Pts',(-19.2058271969419,-35.6392579611484,
122.223048715094)) ;
#76416 = CARTESIAN_POINT('Ctrl Pts',(-18.899352673591,-35.8293075321386,121.993232864623)) ;
#76417 = CARTESIAN_POINT('Ctrl Pts',(-19.001334645375,-35.6493184517198,122.276950638567)) ;
#76418 = CARTESIAN_POINT('Ctrl Pts',(-18.6643671184451,-35.8391478817696,
122.101269435789)) ;
#76419 = CARTESIAN_POINT('Ctrl Pts',(-18.8133472746285,-35.6591588013508,
122.363379411723)) ;
#76420 = CARTESIAN_POINT('Ctrl Pts',(-18.4467771153148,-35.8492108572596,
122.251492745657)) ;
#76421 = CARTESIAN_POINT('Ctrl Pts',(-18.6392749852965,-35.6692217768408,
122.483558171074)) ;
#76422 = CARTESIAN_POINT('Ctrl Pts',(-18.2618359406519,-35.859105177403,122.43429871186)) ;
#76423 = CARTESIAN_POINT('Ctrl Pts',(-18.491322616233,-35.6791160969842,122.629802358124)) ;
#76424 = CARTESIAN_POINT('Ctrl Pts',(-18.1101865600528,-35.8690468905346,
122.646995886954)) ;
#76425 = CARTESIAN_POINT('Ctrl Pts',(-18.3700032496171,-35.6890578101158,
122.799959569415)) ;
#76426 = CARTESIAN_POINT('Ctrl Pts',(-17.9969449046416,-35.8790497803287,
122.884263259483)) ;
#76427 = CARTESIAN_POINT('Ctrl Pts',(-18.2794097634867,-35.69906069991,122.989773283224)) ;
#76428 = CARTESIAN_POINT('Ctrl Pts',(-17.9268443213951,-35.8890896374892,
123.138590645387)) ;
#76429 = CARTESIAN_POINT('Ctrl Pts',(-18.2233291597186,-35.7091005570704,
123.193235305604)) ;
#76430 = CARTESIAN_POINT('Ctrl Pts',(-17.9019122828192,-35.8989138183268,
123.395574782341)) ;
#76431 = CARTESIAN_POINT('Ctrl Pts',(-18.2033834027197,-35.7189247379081,
123.398821321961)) ;
#76432 = CARTESIAN_POINT('Ctrl Pts',(-17.9220883777704,-35.90897079183,123.659068393634)) ;
#76433 = CARTESIAN_POINT('Ctrl Pts',(-18.2195239554329,-35.7289817114113,
123.609616505664)) ;
#76434 = CARTESIAN_POINT('Ctrl Pts',(-17.987198604821,-35.9188989160171,123.91172955812)) ;
#76435 = CARTESIAN_POINT('Ctrl Pts',(-18.271611742449,-35.7389098355983,123.811744931268)) ;
#76436 = CARTESIAN_POINT('Ctrl Pts',(-18.0948259750303,-35.9288526110905,
124.150136156843)) ;
#76437 = CARTESIAN_POINT('Ctrl Pts',(-18.3577130663129,-35.7488635306717,
124.002469995443)) ;
#76438 = CARTESIAN_POINT('Ctrl Pts',(-18.2438917114854,-35.9388988046658,
124.368025600054)) ;
#76439 = CARTESIAN_POINT('Ctrl Pts',(-18.4769654839936,-35.758909724247,124.176781901697)) ;
#76440 = CARTESIAN_POINT('Ctrl Pts',(-18.4247087144737,-35.9487469070257,
124.553177298438)) ;
#76441 = CARTESIAN_POINT('Ctrl Pts',(-18.6216180178333,-35.7687578266069,
124.324902741368)) ;
#76442 = CARTESIAN_POINT('Ctrl Pts',(-18.6368680942893,-35.9587084952533,
124.706511430736)) ;
#76443 = CARTESIAN_POINT('Ctrl Pts',(-18.7913448718134,-35.7787194148345,
124.44757032455)) ;
#76444 = CARTESIAN_POINT('Ctrl Pts',(-18.8741832744465,-35.9687371654095,
124.821161297366)) ;
#76445 = CARTESIAN_POINT('Ctrl Pts',(-18.9811968587923,-35.7887480849908,
124.539290720976)) ;
#76446 = CARTESIAN_POINT('Ctrl Pts',(-19.1247583601931,-35.9786474682913,
124.892091064611)) ;
#76447 = CARTESIAN_POINT('Ctrl Pts',(-19.1816561053087,-35.7986583878725,
124.59603486579)) ;
#76448 = CARTESIAN_POINT('Ctrl Pts',(-19.3844352240808,-35.9885823520992,
124.919183512101)) ;
#76449 = CARTESIAN_POINT('Ctrl Pts',(-19.3893969971606,-35.8085932716804,
124.617709476599)) ;
#76450 = CARTESIAN_POINT('Ctrl Pts',(-19.6476231191656,-35.9986234937898,
124.900335055158)) ;
#76451 = CARTESIAN_POINT('Ctrl Pts',(-19.5999475089394,-35.8186344133711,
124.602631349119)) ;
#76452 = CARTESIAN_POINT('Ctrl Pts',(-19.8996824513268,-36.0085106149538,
124.83723224939)) ;
#76453 = CARTESIAN_POINT('Ctrl Pts',(-19.8015943370243,-35.828521534535,124.552149980266)) ;
#76454 = CARTESIAN_POINT('Ctrl Pts',(-20.1396295183262,-36.0185029578023,
124.730608252224)) ;
#76455 = CARTESIAN_POINT('Ctrl Pts',(-19.9935521670757,-35.8385138773836,
124.466851580924)) ;
#76456 = CARTESIAN_POINT('Ctrl Pts',(-20.3564426703824,-36.0284512590263,
124.584508836184)) ;
#76457 = CARTESIAN_POINT('Ctrl Pts',(-20.1670027663451,-35.8484621786075,
124.34997293713)) ;
#76458 = CARTESIAN_POINT('Ctrl Pts',(-20.544635127036,-36.0383888367084,124.403471920476)) ;
#76459 = CARTESIAN_POINT('Ctrl Pts',(-20.3175569672634,-35.8583997562896,
124.205144391475)) ;
#76460 = CARTESIAN_POINT('Ctrl Pts',(-20.6995297068178,-36.0483754111589,
124.191598913506)) ;
#76461 = CARTESIAN_POINT('Ctrl Pts',(-20.4414732773456,-35.8683863307402,
124.035646689111)) ;
#76462 = CARTESIAN_POINT('Ctrl Pts',(-20.8154914357091,-36.0584042210674,
123.95493766918)) ;
#76463 = CARTESIAN_POINT('Ctrl Pts',(-20.5342434668736,-35.8784151406487,
123.846318005785)) ;
#76464 = CARTESIAN_POINT('Ctrl Pts',(-20.8877452575708,-36.0682825423742,
123.705606150778)) ;
#76465 = CARTESIAN_POINT('Ctrl Pts',(-20.5920471744882,-35.8882934619554,
123.646853866704)) ;
#76466 = CARTESIAN_POINT('Ctrl Pts',(-20.9165435265095,-36.0782741897216,
123.444611225451)) ;
#76467 = CARTESIAN_POINT('Ctrl Pts',(-20.6150868306485,-35.8982851093029,
123.438058194467)) ;
#76468 = CARTESIAN_POINT('Ctrl Pts',(-20.8989774526659,-36.0883087131594,
123.181512331522)) ;
#76469 = CARTESIAN_POINT('Ctrl Pts',(-20.6010349029805,-35.9083196327406,
123.227578932499)) ;
#76470 = CARTESIAN_POINT('Ctrl Pts',(-20.8375844348363,-36.098172070038,122.929660650896)) ;
#76471 = CARTESIAN_POINT('Ctrl Pts',(-20.55192174251,-35.9181829896192,123.026098230027)) ;
#76472 = CARTESIAN_POINT('Ctrl Pts',(-20.7312794062395,-36.1082422967183,
122.687347241502)) ;
#76473 = CARTESIAN_POINT('Ctrl Pts',(-20.4668785833512,-35.9282532162995,
122.832246790872)) ;
#76474 = CARTESIAN_POINT('Ctrl Pts',(-20.5878041611875,-36.118084604853,122.472130151243)) ;
#76475 = CARTESIAN_POINT('Ctrl Pts',(-20.3520998563727,-35.9380955244342,
122.660073387355)) ;
#76476 = CARTESIAN_POINT('Ctrl Pts',(-20.4077016433411,-36.1280453368764,
122.282190824052)) ;
#76477 = CARTESIAN_POINT('Ctrl Pts',(-20.2080190009201,-35.9480562564576,
122.50812127463)) ;
#76478 = CARTESIAN_POINT('Ctrl Pts',(-20.1954179813538,-36.1380832260745,
122.125622966296)) ;
#76479 = CARTESIAN_POINT('Ctrl Pts',(-20.0381926818535,-35.9580941456557,
122.382865981336)) ;
#76480 = CARTESIAN_POINT('Ctrl Pts',(-19.9632011128063,-36.1479575089933,
122.009756791279)) ;
#76481 = CARTESIAN_POINT('Ctrl Pts',(-19.852420481698,-35.9679684285746,122.290172259536)) ;
#76482 = CARTESIAN_POINT('Ctrl Pts',(-19.7095295605518,-36.1580272536108,
121.934544304188)) ;
#76483 = CARTESIAN_POINT('Ctrl Pts',(-19.6494833349554,-35.978038173192,122.230000967982)) ;
#76484 = CARTESIAN_POINT('Ctrl Pts',(-19.4527844207,-36.1678605639564,121.905081249656)) ;
#76485 = CARTESIAN_POINT('Ctrl Pts',(-19.4440883880503,-35.9878714835377,
122.206429346442)) ;
#76486 = CARTESIAN_POINT('Ctrl Pts',(-19.1896400044827,-36.1778908073091,
121.920204651344)) ;
#76487 = CARTESIAN_POINT('Ctrl Pts',(-19.2335727027001,-35.9979017268903,
122.218526613797)) ;
#76488 = CARTESIAN_POINT('Ctrl Pts',(-18.9332371753913,-36.1879230952875,
121.981571396633)) ;
#76489 = CARTESIAN_POINT('Ctrl Pts',(-19.0284500699383,-36.0079340148687,
122.267618766793)) ;
#76490 = CARTESIAN_POINT('Ctrl Pts',(-18.6960884546882,-36.1977502717556,
122.083816541802)) ;
#76491 = CARTESIAN_POINT('Ctrl Pts',(-18.838731476733,-36.0177611913368,122.349413165543)) ;
#76492 = CARTESIAN_POINT('Ctrl Pts',(-18.4761127316543,-36.2077556546224,
122.227783640436)) ;
#76493 = CARTESIAN_POINT('Ctrl Pts',(-18.6627501158308,-36.0277665742037,
122.464585522614)) ;
#76494 = CARTESIAN_POINT('Ctrl Pts',(-18.2849106465247,-36.2177382936152,
122.407469429995)) ;
#76495 = CARTESIAN_POINT('Ctrl Pts',(-18.5097875384203,-36.0377492131964,
122.60833293523)) ;
#76496 = CARTESIAN_POINT('Ctrl Pts',(-18.1271511615544,-36.2277823607518,
122.61904959903)) ;
#76497 = CARTESIAN_POINT('Ctrl Pts',(-18.3835787128746,-36.047793280333,122.777596301397)) ;
#76498 = CARTESIAN_POINT('Ctrl Pts',(-18.0107408056711,-36.2376035795558,
122.84940714592)) ;
#76499 = CARTESIAN_POINT('Ctrl Pts',(-18.2904495064269,-36.057614499137,122.961880755855)) ;
#76500 = CARTESIAN_POINT('Ctrl Pts',(-17.9338160940377,-36.2476404184938,
123.101693464126)) ;
#76501 = CARTESIAN_POINT('Ctrl Pts',(-18.2289081204975,-36.0676513380751,
123.163709405385)) ;
#76502 = CARTESIAN_POINT('Ctrl Pts',(-17.9026486631105,-36.2576648305916,
123.36328314838)) ;
#76503 = CARTESIAN_POINT('Ctrl Pts',(-18.2039726598348,-36.0776757501728,
123.372980991972)) ;
#76504 = CARTESIAN_POINT('Ctrl Pts',(-17.9165495302579,-36.2675169149969,
123.621816862734)) ;
#76505 = CARTESIAN_POINT('Ctrl Pts',(-18.2150916816491,-36.0875278345781,
123.579807245692)) ;
#76506 = CARTESIAN_POINT('Ctrl Pts',(-17.9755567900493,-36.27750781174,123.877618050262)) ;
#76507 = CARTESIAN_POINT('Ctrl Pts',(-18.2622957977157,-36.0975187313213,
123.784448445474)) ;
#76508 = CARTESIAN_POINT('Ctrl Pts',(-18.077203160799,-36.287425803641,124.117648747787)) ;
#76509 = CARTESIAN_POINT('Ctrl Pts',(-18.3436111230473,-36.1074367232222,
123.976473257481)) ;
#76510 = CARTESIAN_POINT('Ctrl Pts',(-18.2204755142944,-36.297453919098,124.338803226276)) ;
#76511 = CARTESIAN_POINT('Ctrl Pts',(-18.4582275584006,-36.1174648386792,
124.153397810827)) ;
#76512 = CARTESIAN_POINT('Ctrl Pts',(-18.3973504808936,-36.3073390950401,
124.529066690631)) ;
#76513 = CARTESIAN_POINT('Ctrl Pts',(-18.5997258423448,-36.1273500146213,
124.30560934978)) ;
#76514 = CARTESIAN_POINT('Ctrl Pts',(-18.606372387198,-36.317328453447,124.687887703302)) ;
#76515 = CARTESIAN_POINT('Ctrl Pts',(-18.7669421404985,-36.1373393730282,
124.43266756716)) ;
#76516 = CARTESIAN_POINT('Ctrl Pts',(-18.8412552934067,-36.3273696010273,
124.808127004858)) ;
#76517 = CARTESIAN_POINT('Ctrl Pts',(-18.9548477220754,-36.1473805206085,
124.528860620491)) ;
#76518 = CARTESIAN_POINT('Ctrl Pts',(-19.0880822046811,-36.3372022240337,
124.884553235506)) ;
#76519 = CARTESIAN_POINT('Ctrl Pts',(-19.1523079763883,-36.157213143615,124.590003139103)) ;
#76520 = CARTESIAN_POINT('Ctrl Pts',(-19.3485418518616,-36.3471962951445,
124.918229067324)) ;
#76521 = CARTESIAN_POINT('Ctrl Pts',(-19.3606753488184,-36.1672072147257,
124.616945728324)) ;
#76522 = CARTESIAN_POINT('Ctrl Pts',(-19.6117962054369,-36.3572249527853,
124.905606556928)) ;
#76523 = CARTESIAN_POINT('Ctrl Pts',(-19.571278932422,-36.1772358723666,124.606849593265)) ;
#76524 = CARTESIAN_POINT('Ctrl Pts',(-19.8651977310147,-36.3671092789782,
124.848586979644)) ;
#76525 = CARTESIAN_POINT('Ctrl Pts',(-19.7740000730835,-36.1871201985594,
124.561235916018)) ;
#76526 = CARTESIAN_POINT('Ctrl Pts',(-20.1070919689102,-36.3770750224688,
124.748197482078)) ;
#76527 = CARTESIAN_POINT('Ctrl Pts',(-19.9675160571563,-36.19708594205,124.480926240918)) ;
#76528 = CARTESIAN_POINT('Ctrl Pts',(-20.3290461476905,-36.3871034016,124.606136879373)) ;
#76529 = CARTESIAN_POINT('Ctrl Pts',(-20.1450804639494,-36.2071143211812,
124.367279397955)) ;
#76530 = CARTESIAN_POINT('Ctrl Pts',(-20.5207969132136,-36.3970042478069,
124.430224963432)) ;
#76531 = CARTESIAN_POINT('Ctrl Pts',(-20.2984821301222,-36.2170151673881,
124.226551616459)) ;
#76532 = CARTESIAN_POINT('Ctrl Pts',(-20.6815114755106,-36.407062905224,124.220415524645)) ;
#76533 = CARTESIAN_POINT('Ctrl Pts',(-20.4270554231223,-36.2270738248052,
124.058705203557)) ;
#76534 = CARTESIAN_POINT('Ctrl Pts',(-20.8012013744469,-36.4169204680059,
123.990625446844)) ;
#76535 = CARTESIAN_POINT('Ctrl Pts',(-20.5228088997045,-36.2369313875871,
123.874874540363)) ;
#76536 = CARTESIAN_POINT('Ctrl Pts',(-20.8809810995095,-36.4269888705591,
123.738394192403)) ;
#76537 = CARTESIAN_POINT('Ctrl Pts',(-20.5866346717548,-36.2469997901403,
123.673090038089)) ;
#76538 = CARTESIAN_POINT('Ctrl Pts',(-20.9150001538279,-36.4368442692987,
123.481625971232)) ;
#76539 = CARTESIAN_POINT('Ctrl Pts',(-20.6138518770455,-36.2568551888799,
123.467676224677)) ;
#76540 = CARTESIAN_POINT('Ctrl Pts',(-20.9045521215067,-36.4468391363726,
123.219187981019)) ;
#76541 = CARTESIAN_POINT('Ctrl Pts',(-20.6054955832144,-36.2668500559538,
123.257725827146)) ;
#76542 = CARTESIAN_POINT('Ctrl Pts',(-20.8479327597184,-36.456870431356,122.961723074858)) ;
#76543 = CARTESIAN_POINT('Ctrl Pts',(-20.5602021162859,-36.2768813509373,
123.051753458956)) ;
#76544 = CARTESIAN_POINT('Ctrl Pts',(-20.7495006731803,-36.4667369560826,
122.721841789023)) ;
#76545 = CARTESIAN_POINT('Ctrl Pts',(-20.4814585578185,-36.2867478756638,
122.859848009329)) ;
#76546 = CARTESIAN_POINT('Ctrl Pts',(-20.6095919097615,-36.4767244267783,
122.499818683209)) ;
#76547 = CARTESIAN_POINT('Ctrl Pts',(-20.36953342095,-36.2967353463596,122.68222845983)) ;
#76548 = CARTESIAN_POINT('Ctrl Pts',(-20.4340715147178,-36.4866691863422,
122.306140896077)) ;
#76549 = CARTESIAN_POINT('Ctrl Pts',(-20.2291188313566,-36.3066801059234,
122.527284917964)) ;
#76550 = CARTESIAN_POINT('Ctrl Pts',(-20.2254502142626,-36.496714742291,122.144429454207)) ;
#76551 = CARTESIAN_POINT('Ctrl Pts',(-20.0622230962988,-36.3167256618723,
122.397914055264)) ;
#76552 = CARTESIAN_POINT('Ctrl Pts',(-19.9963181527687,-36.5065743306661,
122.023404638943)) ;
#76553 = CARTESIAN_POINT('Ctrl Pts',(-19.8789187628921,-36.3265852502474,
122.301092445277)) ;
#76554 = CARTESIAN_POINT('Ctrl Pts',(-19.7463087037806,-36.5165752858022,
121.942510562541)) ;
#76555 = CARTESIAN_POINT('Ctrl Pts',(-19.6789119467519,-36.3365862053834,
122.236375109967)) ;
#76556 = CARTESIAN_POINT('Ctrl Pts',(-19.488513689031,-36.5264795130797,121.906393185081)) ;
#76557 = CARTESIAN_POINT('Ctrl Pts',(-19.472676448649,-36.346490432661,122.207479050223)) ;
#76558 = CARTESIAN_POINT('Ctrl Pts',(-19.22481600771,-36.5365215899749,121.91563802328)) ;
#76559 = CARTESIAN_POINT('Ctrl Pts',(-19.2617182336787,-36.3565325095561,
122.214872707114)) ;
#76560 = CARTESIAN_POINT('Ctrl Pts',(-18.9700774883561,-36.546429202661,121.969685726369)) ;
#76561 = CARTESIAN_POINT('Ctrl Pts',(-19.0579271360362,-36.3664401222423,
122.258108661664)) ;
#76562 = CARTESIAN_POINT('Ctrl Pts',(-18.7250847627376,-36.5564837332768,
122.068538595385)) ;
#76563 = CARTESIAN_POINT('Ctrl Pts',(-18.8619321279312,-36.376494652858,122.337188894249)) ;
#76564 = CARTESIAN_POINT('Ctrl Pts',(-18.5051552712521,-36.5663445198256,
122.20564207096)) ;
#76565 = CARTESIAN_POINT('Ctrl Pts',(-18.6859875392954,-36.3863554394069,
122.446869671373)) ;
#76566 = CARTESIAN_POINT('Ctrl Pts',(-18.3095046249298,-36.5763382748967,
122.380772756674)) ;
#76567 = CARTESIAN_POINT('Ctrl Pts',(-18.5294655677005,-36.396349194478,122.586972503952)) ;
#76568 = CARTESIAN_POINT('Ctrl Pts',(-18.1481936176702,-36.5862636351367,
122.585788118873)) ;
#76569 = CARTESIAN_POINT('Ctrl Pts',(-18.4004150621657,-36.406274554718,122.750983322731)) ;
#76570 = CARTESIAN_POINT('Ctrl Pts',(-18.0236841921793,-36.596291564532,122.818002834844)) ;
#76571 = CARTESIAN_POINT('Ctrl Pts',(-18.300805562702,-36.4163024841132,122.936753987693)) ;
#76572 = CARTESIAN_POINT('Ctrl Pts',(-17.9422706635279,-36.6061778313313,
123.064758942324)) ;
#76573 = CARTESIAN_POINT('Ctrl Pts',(-18.2356726313687,-36.4261887509125,
123.134158078855)) ;
#76574 = CARTESIAN_POINT('Ctrl Pts',(-17.9042663341552,-36.6162096002296,
123.325585129756)) ;
#76575 = CARTESIAN_POINT('Ctrl Pts',(-18.2052669459445,-36.4362205198108,
123.342818652238)) ;
#76576 = CARTESIAN_POINT('Ctrl Pts',(-17.9117588181507,-36.6260911960731,
123.585201643662)) ;
#76577 = CARTESIAN_POINT('Ctrl Pts',(-18.2112586694567,-36.4461021156544,
123.55051186725)) ;
#76578 = CARTESIAN_POINT('Ctrl Pts',(-17.9650896019866,-36.6361530815411,
123.844142860271)) ;
#76579 = CARTESIAN_POINT('Ctrl Pts',(-18.2539211167218,-36.4561640011224,
123.757665267779)) ;
#76580 = CARTESIAN_POINT('Ctrl Pts',(-18.0605371632968,-36.6460105155599,
124.084996144614)) ;
#76581 = CARTESIAN_POINT('Ctrl Pts',(-18.3302769065666,-36.4660214351412,
123.950348570272)) ;
#76582 = CARTESIAN_POINT('Ctrl Pts',(-18.1977180728427,-36.6560037586019,
124.308890236656)) ;
#76583 = CARTESIAN_POINT('Ctrl Pts',(-18.4400203090856,-36.4760146781832,
124.129465536782)) ;
#76584 = CARTESIAN_POINT('Ctrl Pts',(-18.3706217887722,-36.6659345194883,
124.50438473476)) ;
#76585 = CARTESIAN_POINT('Ctrl Pts',(-18.5783393320726,-36.4859454390695,
124.285860564829)) ;
#76586 = CARTESIAN_POINT('Ctrl Pts',(-18.6449288885394,-36.6792835116855,
124.723100111682)) ;
#76587 = CARTESIAN_POINT('Ctrl Pts',(-18.797794429001,-36.4992944312667,124.46084539929)) ;
#76588 = CARTESIAN_POINT('Ctrl Pts',(-18.9682246085293,-36.6925518845019,
124.863897618104)) ;
#76589 = CARTESIAN_POINT('Ctrl Pts',(-19.0564576791259,-36.5125628040832,
124.573487208325)) ;
#76590 = CARTESIAN_POINT('Ctrl Pts',(-19.3133563776457,-36.7058348258862,
124.916340475297)) ;
#76591 = CARTESIAN_POINT('Ctrl Pts',(-19.3325181777442,-36.5258457454675,
124.615432945298)) ;
#76592 = CARTESIAN_POINT('Ctrl Pts',(-19.5771730601713,-36.7158776117285,
124.909887095893)) ;
#76593 = CARTESIAN_POINT('Ctrl Pts',(-19.5435804546175,-36.5358885313097,
124.610274688818)) ;
#76594 = CARTESIAN_POINT('Ctrl Pts',(-19.8309776236179,-36.7257275542806,
124.858999538659)) ;
#76595 = CARTESIAN_POINT('Ctrl Pts',(-19.7466221103153,-36.5457384738618,
124.569566509396)) ;
#76596 = CARTESIAN_POINT('Ctrl Pts',(-20.0759163398703,-36.7357247871995,
124.764028514436)) ;
#76597 = CARTESIAN_POINT('Ctrl Pts',(-19.9425753637021,-36.5557357067808,
124.493590557892)) ;
#76598 = CARTESIAN_POINT('Ctrl Pts',(-20.300851683239,-36.7457396825341,124.627366616285)) ;
#76599 = CARTESIAN_POINT('Ctrl Pts',(-20.1225212573089,-36.5657506021153,
124.384267868071)) ;
#76600 = CARTESIAN_POINT('Ctrl Pts',(-20.5625371626539,-36.7589793591723,
124.39808728951)) ;
#76601 = CARTESIAN_POINT('Ctrl Pts',(-20.3318880358835,-36.5789902787535,
124.200821860388)) ;
#76602 = CARTESIAN_POINT('Ctrl Pts',(-20.8079029754559,-36.7755265835776,
124.033128787395)) ;
#76603 = CARTESIAN_POINT('Ctrl Pts',(-20.5281632731602,-36.5955375031589,
123.908899479938)) ;
#76604 = CARTESIAN_POINT('Ctrl Pts',(-20.914868930944,-36.7921740207087,123.603796766482)) ;
#76605 = CARTESIAN_POINT('Ctrl Pts',(-20.6137528357625,-36.6121849402899,
123.56536784602)) ;
#76606 = CARTESIAN_POINT('Ctrl Pts',(-20.9083945688034,-36.8054635181869,
123.254597757713)) ;
#76607 = CARTESIAN_POINT('Ctrl Pts',(-20.6085683029633,-36.6254744377682,
123.286061935331)) ;
#76608 = CARTESIAN_POINT('Ctrl Pts',(-20.8593749514375,-36.8153369260093,
122.999807024194)) ;
#76609 = CARTESIAN_POINT('Ctrl Pts',(-20.56935600526,-36.6353478455905,123.082217773299)) ;
#76610 = CARTESIAN_POINT('Ctrl Pts',(-20.7652312033455,-36.825389303602,122.752998369498)) ;
#76611 = CARTESIAN_POINT('Ctrl Pts',(-20.4940428185494,-36.6454002231832,
122.884773343294)) ;
#76612 = CARTESIAN_POINT('Ctrl Pts',(-20.6315577728681,-36.8352929571429,
122.529670136129)) ;
#76613 = CARTESIAN_POINT('Ctrl Pts',(-20.3871046825718,-36.6553038767241,
122.706108244707)) ;
#76614 = CARTESIAN_POINT('Ctrl Pts',(-20.4609498468132,-36.8452372261382,
122.331765024451)) ;
#76615 = CARTESIAN_POINT('Ctrl Pts',(-20.250623548332,-36.6652481457194,122.547784435435)) ;
#76616 = CARTESIAN_POINT('Ctrl Pts',(-20.1896663856008,-36.8585682344709,
122.109990345242)) ;
#76617 = CARTESIAN_POINT('Ctrl Pts',(-20.0335788518521,-36.6785791540521,
122.3703552458)) ;
#76618 = CARTESIAN_POINT('Ctrl Pts',(-19.7868089892169,-36.8751898149952,
121.928852787631)) ;
#76619 = CARTESIAN_POINT('Ctrl Pts',(-19.7113302438444,-36.6952007345764,
122.22544992753)) ;
#76620 = CARTESIAN_POINT('Ctrl Pts',(-19.3483970122158,-36.8917324856935,
121.895325330599)) ;
#76621 = CARTESIAN_POINT('Ctrl Pts',(-19.3605382150688,-36.7117434052748,
122.198625176032)) ;
#76622 = CARTESIAN_POINT('Ctrl Pts',(-19.0036058958817,-36.9050816452565,
121.959959179147)) ;
#76623 = CARTESIAN_POINT('Ctrl Pts',(-19.084756195026,-36.7250925648377,122.250326885057)) ;
#76624 = CARTESIAN_POINT('Ctrl Pts',(-18.6780618920126,-36.918309795416,122.081981866983)) ;
#76625 = CARTESIAN_POINT('Ctrl Pts',(-18.8243006830399,-36.7383207149972,
122.347949900398)) ;
#76626 = CARTESIAN_POINT('Ctrl Pts',(-18.3181836590694,-36.9349404725535,
122.338513488484)) ;
#76627 = CARTESIAN_POINT('Ctrl Pts',(-18.536409956563,-36.7549513921347,122.553165511551)) ;
#76628 = CARTESIAN_POINT('Ctrl Pts',(-18.0180562107128,-36.9548434118416,
122.774198058424)) ;
#76629 = CARTESIAN_POINT('Ctrl Pts',(-18.2963005856459,-36.7748543314228,
122.901714217013)) ;
#76630 = CARTESIAN_POINT('Ctrl Pts',(-17.8841306987683,-36.9747462784449,
123.285845641886)) ;
#76631 = CARTESIAN_POINT('Ctrl Pts',(-18.1891582490799,-36.7947571980261,
123.311031567695)) ;
#76632 = CARTESIAN_POINT('Ctrl Pts',(-17.9320811340281,-36.9946594435497,
123.813046654352)) ;
#76633 = CARTESIAN_POINT('Ctrl Pts',(-18.2275157048257,-36.8146703631309,
123.732793421951)) ;
#76634 = CARTESIAN_POINT('Ctrl Pts',(-18.1591155085534,-37.014695272691,124.294661831173)) ;
#76635 = CARTESIAN_POINT('Ctrl Pts',(-18.4091406225134,-36.8347061922723,
124.118086406354)) ;
#76636 = CARTESIAN_POINT('Ctrl Pts',(-18.5326928560292,-37.0345138475691,
124.666191700526)) ;
#76637 = CARTESIAN_POINT('Ctrl Pts',(-18.7080017265223,-36.8545247671503,
124.415313158299)) ;
#76638 = CARTESIAN_POINT('Ctrl Pts',(-19.0136563927,-37.0544841486111,124.890270639993)) ;
#76639 = CARTESIAN_POINT('Ctrl Pts',(-19.0927719398134,-36.8744950681923,
124.594578398497)) ;
#76640 = CARTESIAN_POINT('Ctrl Pts',(-19.5404829664597,-37.0743756809756,
124.936789595274)) ;
#76641 = CARTESIAN_POINT('Ctrl Pts',(-19.5142340085164,-36.8943866005569,
124.63179555628)) ;
#76642 = CARTESIAN_POINT('Ctrl Pts',(-20.0545360586527,-37.0943987787921,
124.799534983154)) ;
#76643 = CARTESIAN_POINT('Ctrl Pts',(-19.9254767467742,-36.9144096983734,
124.52199379209)) ;
#76644 = CARTESIAN_POINT('Ctrl Pts',(-20.4863256455072,-37.1141955317121,
124.498745537884)) ;
#76645 = CARTESIAN_POINT('Ctrl Pts',(-20.2709110786742,-36.9342064512933,
124.281362358102)) ;
#76646 = CARTESIAN_POINT('Ctrl Pts',(-20.7931678600069,-37.1341566202009,
124.066005974666)) ;
#76647 = CARTESIAN_POINT('Ctrl Pts',(-20.5163858339727,-36.9541675397821,
123.93517078883)) ;
#76648 = CARTESIAN_POINT('Ctrl Pts',(-20.9329957735426,-37.154134889133,123.553712501951)) ;
#76649 = CARTESIAN_POINT('Ctrl Pts',(-20.6282493161937,-36.9741458087143,
123.525336142619)) ;
#76650 = CARTESIAN_POINT('Ctrl Pts',(-20.8907271346695,-37.173954903924,123.028678283214)) ;
#76651 = CARTESIAN_POINT('Ctrl Pts',(-20.5944348575025,-36.9939658235053,
123.105306484844)) ;
#76652 = CARTESIAN_POINT('Ctrl Pts',(-20.6717362479784,-37.1938933131759,
122.546084069882)) ;
#76653 = CARTESIAN_POINT('Ctrl Pts',(-20.4192415860018,-37.0139042327571,
122.719230493431)) ;
#76654 = CARTESIAN_POINT('Ctrl Pts',(-20.2983002158022,-37.2139404305683,
122.165933042797)) ;
#76655 = CARTESIAN_POINT('Ctrl Pts',(-20.1204933529623,-37.0339513501496,
122.415110073134)) ;
#76656 = CARTESIAN_POINT('Ctrl Pts',(-19.8223796113184,-37.2337866764021,
121.938614397135)) ;
#76657 = CARTESIAN_POINT('Ctrl Pts',(-19.7397550078523,-37.0537975959834,
122.233254223609)) ;
#76658 = CARTESIAN_POINT('Ctrl Pts',(-19.2975051439778,-37.2536356449142,
121.885263707543)) ;
#76659 = CARTESIAN_POINT('Ctrl Pts',(-19.3198535804931,-37.0736465644954,
122.190574646049)) ;
#76660 = CARTESIAN_POINT('Ctrl Pts',(-18.7809853426803,-37.2736859472255,
122.016176078783)) ;
#76661 = CARTESIAN_POINT('Ctrl Pts',(-18.9066385592989,-37.0936968668067,
122.295305374503)) ;
#76662 = CARTESIAN_POINT('Ctrl Pts',(-18.3447935795222,-37.2935208696567,
122.312469305254)) ;
#76663 = CARTESIAN_POINT('Ctrl Pts',(-18.5576842939248,-37.113531789238,122.532341920129)) ;
#76664 = CARTESIAN_POINT('Ctrl Pts',(-18.0337656488262,-37.3134512708826,
122.7410074397)) ;
#76665 = CARTESIAN_POINT('Ctrl Pts',(-18.3088629320483,-37.1334621904638,
122.875174080636)) ;
#76666 = CARTESIAN_POINT('Ctrl Pts',(-17.8872187177166,-37.3333362162414,
123.249003693798)) ;
#76667 = CARTESIAN_POINT('Ctrl Pts',(-18.1916271520052,-37.1533471358227,
123.28157263407)) ;
#76668 = CARTESIAN_POINT('Ctrl Pts',(-17.9240043990121,-37.3534088243928,
123.781130410534)) ;
#76669 = CARTESIAN_POINT('Ctrl Pts',(-18.2210576286058,-37.1734197439741,
123.707273187308)) ;
#76670 = CARTESIAN_POINT('Ctrl Pts',(-18.1371306277128,-37.373200140721,124.262126611291)) ;
#76671 = CARTESIAN_POINT('Ctrl Pts',(-18.3915613312149,-37.1932110603022,
124.092070982679)) ;
#76672 = CARTESIAN_POINT('Ctrl Pts',(-18.5035285318235,-37.3931649304882,
124.64589122131)) ;
#76673 = CARTESIAN_POINT('Ctrl Pts',(-18.6846818764584,-37.2131758500695,
124.399080894642)) ;
#76674 = CARTESIAN_POINT('Ctrl Pts',(-18.9799605391563,-37.4131478862385,
124.880632850291)) ;
#76675 = CARTESIAN_POINT('Ctrl Pts',(-19.0658287233952,-37.2331588058198,
124.586871974143)) ;
#76676 = CARTESIAN_POINT('Ctrl Pts',(-19.5032077670225,-37.4329564082147,
124.939278140905)) ;
#76677 = CARTESIAN_POINT('Ctrl Pts',(-19.4844282141108,-37.2529673277959,
124.633785395356)) ;
#76678 = CARTESIAN_POINT('Ctrl Pts',(-20.0196196743258,-37.4529419829505,
124.815366561312)) ;
#76679 = CARTESIAN_POINT('Ctrl Pts',(-19.8975570540621,-37.2729529025317,
124.534652928844)) ;
#76680 = CARTESIAN_POINT('Ctrl Pts',(-20.4606042547495,-37.4728246230189,
124.523953283935)) ;
#76681 = CARTESIAN_POINT('Ctrl Pts',(-20.2503434533714,-37.2928355426001,
124.301519156789)) ;
#76682 = CARTESIAN_POINT('Ctrl Pts',(-20.7770251298041,-37.4927799351508,
124.098432867977)) ;
#76683 = CARTESIAN_POINT('Ctrl Pts',(-20.5034774694716,-37.312790854732,123.961100528127)) ;
#76684 = CARTESIAN_POINT('Ctrl Pts',(-20.9290068708971,-37.5126542917586,
123.592447664155)) ;
#76685 = CARTESIAN_POINT('Ctrl Pts',(-20.6250594668182,-37.3326652113398,
123.556310724529)) ;
#76686 = CARTESIAN_POINT('Ctrl Pts',(-20.899389956278,-37.5326364986196,123.062239130192)) ;
#76687 = CARTESIAN_POINT('Ctrl Pts',(-20.6013622688047,-37.3526474182009,
123.132144083971)) ;
#76688 = CARTESIAN_POINT('Ctrl Pts',(-20.6908254811286,-37.5525675765696,
122.575167631193)) ;
#76689 = CARTESIAN_POINT('Ctrl Pts',(-20.4345064463008,-37.3725784961509,
122.742488126059)) ;
#76690 = CARTESIAN_POINT('Ctrl Pts',(-20.3288457045905,-37.5724945514246,
122.18869479083)) ;
#76691 = CARTESIAN_POINT('Ctrl Pts',(-20.1449218052122,-37.3925054710058,
122.433312456316)) ;
#76692 = CARTESIAN_POINT('Ctrl Pts',(-19.8592684233699,-37.5923270103735,
121.949075641599)) ;
#76693 = CARTESIAN_POINT('Ctrl Pts',(-19.7692491705873,-37.4123379299547,
122.241620182198)) ;
#76694 = CARTESIAN_POINT('Ctrl Pts',(-19.420065800467,-37.6089846945487,121.894159881115)) ;
#76695 = CARTESIAN_POINT('Ctrl Pts',(-19.4179129229134,-37.4289956141299,
122.197692407191)) ;
#76696 = CARTESIAN_POINT('Ctrl Pts',(-19.0750788995426,-37.6222339184558,
121.941806794285)) ;
#76697 = CARTESIAN_POINT('Ctrl Pts',(-19.1418999521506,-37.442244838037,122.235812007745)) ;
#76698 = CARTESIAN_POINT('Ctrl Pts',(-18.8237258576815,-37.632282939907,122.022687580648)) ;
#76699 = CARTESIAN_POINT('Ctrl Pts',(-18.9408249160599,-37.4522938594882,
122.300516750014)) ;
#76700 = CARTESIAN_POINT('Ctrl Pts',(-18.5945663208292,-37.6421429481375,
122.14362057706)) ;
#76701 = CARTESIAN_POINT('Ctrl Pts',(-18.7574893710446,-37.4621538677187,
122.397273180662)) ;
#76702 = CARTESIAN_POINT('Ctrl Pts',(-18.3180876793282,-37.6554264613621,
122.356789242103)) ;
#76703 = CARTESIAN_POINT('Ctrl Pts',(-18.5363454539202,-37.4754373809433,
122.567770274827)) ;
#76704 = CARTESIAN_POINT('Ctrl Pts',(-18.0500066418884,-37.6720723803629,
122.708670183385)) ;
#76705 = CARTESIAN_POINT('Ctrl Pts',(-18.3218393587194,-37.4920832999442,
122.849331203031)) ;
#76706 = CARTESIAN_POINT('Ctrl Pts',(-17.9182173115326,-37.688626358179,123.128486091683)) ;
#76707 = CARTESIAN_POINT('Ctrl Pts',(-18.2164325852077,-37.5086372777602,
123.185138398988)) ;
#76708 = CARTESIAN_POINT('Ctrl Pts',(-17.9032980830167,-37.7019860871506,
123.479244069039)) ;
#76709 = CARTESIAN_POINT('Ctrl Pts',(-18.2044905709866,-37.5219970067318,
123.465776425923)) ;
#76710 = CARTESIAN_POINT('Ctrl Pts',(-17.9373186786892,-37.7118791389473,
123.737005381488)) ;
#76711 = CARTESIAN_POINT('Ctrl Pts',(-18.2317111977967,-37.5318900585285,
123.671978909914)) ;
#76712 = CARTESIAN_POINT('Ctrl Pts',(-18.015993501647,-37.7218691042283,123.98743356221)) ;
#76713 = CARTESIAN_POINT('Ctrl Pts',(-18.2946526703774,-37.5418800238096,
123.872322439341)) ;
#76714 = CARTESIAN_POINT('Ctrl Pts',(-18.1363891804097,-37.7318209850891,
124.219643590522)) ;
#76715 = CARTESIAN_POINT('Ctrl Pts',(-18.3909713400926,-37.5518319046704,
124.058088956669)) ;
#76716 = CARTESIAN_POINT('Ctrl Pts',(-18.2969510924276,-37.741869336781,124.429245026143)) ;
#76717 = CARTESIAN_POINT('Ctrl Pts',(-18.5194225674474,-37.5618802563622,
124.225768799345)) ;
#76718 = CARTESIAN_POINT('Ctrl Pts',(-18.4872912315673,-37.7517106208872,
124.604366917824)) ;
#76719 = CARTESIAN_POINT('Ctrl Pts',(-18.6716962379228,-37.5717215404684,
124.365864646808)) ;
#76720 = CARTESIAN_POINT('Ctrl Pts',(-18.7080075971964,-37.7616973240128,
124.74626444655)) ;
#76721 = CARTESIAN_POINT('Ctrl Pts',(-18.848270497138,-37.5817082435941,124.479380739021)) ;
#76722 = CARTESIAN_POINT('Ctrl Pts',(-18.948783824352,-37.7716323528303,124.847344520093)) ;
#76723 = CARTESIAN_POINT('Ctrl Pts',(-19.0408922983168,-37.5916432724115,
124.560242693313)) ;
#76724 = CARTESIAN_POINT('Ctrl Pts',(-19.2065084133327,-37.7816881477372,
124.905549326616)) ;
#76725 = CARTESIAN_POINT('Ctrl Pts',(-19.2470724255386,-37.6016990673184,
124.606804323034)) ;
#76726 = CARTESIAN_POINT('Ctrl Pts',(-19.4645118314046,-37.7915165110265,
124.918239663675)) ;
#76727 = CARTESIAN_POINT('Ctrl Pts',(-19.4534751612069,-37.6115274306077,
124.61695433475)) ;
#76728 = CARTESIAN_POINT('Ctrl Pts',(-19.7268395348962,-37.8015774809244,
124.885556198789)) ;
#76729 = CARTESIAN_POINT('Ctrl Pts',(-19.6633370066296,-37.6215884005056,
124.590805332165)) ;
#76730 = CARTESIAN_POINT('Ctrl Pts',(-19.9758209773242,-37.8114917598142,
124.808729302342)) ;
#76731 = CARTESIAN_POINT('Ctrl Pts',(-19.8625213953459,-37.6315026793954,
124.529341692583)) ;
#76732 = CARTESIAN_POINT('Ctrl Pts',(-20.2101091149036,-37.8215007542824,
124.689174409391)) ;
#76733 = CARTESIAN_POINT('Ctrl Pts',(-20.0499508319165,-37.6415116738637,
124.433695808887)) ;
#76734 = CARTESIAN_POINT('Ctrl Pts',(-20.4201860705366,-37.8315305888462,
124.529999912154)) ;
#76735 = CARTESIAN_POINT('Ctrl Pts',(-20.2180110082682,-37.6515415084274,
124.306354429914)) ;
#76736 = CARTESIAN_POINT('Ctrl Pts',(-20.5967424361067,-37.8413888189184,
124.340392518971)) ;
#76737 = CARTESIAN_POINT('Ctrl Pts',(-20.3592543312716,-37.6613997384997,
124.154667125539)) ;
#76738 = CARTESIAN_POINT('Ctrl Pts',(-20.7399359738855,-37.8513875246608,
124.120135025767)) ;
#76739 = CARTESIAN_POINT('Ctrl Pts',(-20.4738072491821,-37.6713984442421,
123.978459973914)) ;
#76740 = CARTESIAN_POINT('Ctrl Pts',(-20.8419611024385,-37.8612821805796,
123.880914135992)) ;
#76741 = CARTESIAN_POINT('Ctrl Pts',(-20.5554252348265,-37.6812931001609,
123.787082588274)) ;
#76742 = CARTESIAN_POINT('Ctrl Pts',(-20.9018013799904,-37.8713452449635,
123.623373162073)) ;
#76743 = CARTESIAN_POINT('Ctrl Pts',(-20.603295299142,-37.6913561645448,123.581049278094)) ;
#76744 = CARTESIAN_POINT('Ctrl Pts',(-20.9159903078622,-37.8811849032434,
123.365144028712)) ;
#76745 = CARTESIAN_POINT('Ctrl Pts',(-20.6146442263728,-37.7011958228247,
123.374466181267)) ;
#76746 = CARTESIAN_POINT('Ctrl Pts',(-20.8847687943629,-37.8912480703253,
123.102580743035)) ;
#76747 = CARTESIAN_POINT('Ctrl Pts',(-20.589664844702,-37.7112589899066,123.16441577383)) ;
#76748 = CARTESIAN_POINT('Ctrl Pts',(-20.809484036213,-37.9011423154524,122.853677895853)) ;
#76749 = CARTESIAN_POINT('Ctrl Pts',(-20.5294350133251,-37.7211532350337,
122.965294385449)) ;
#76750 = CARTESIAN_POINT('Ctrl Pts',(-20.6922226402959,-37.911084137057,122.620247034539)) ;
#76751 = CARTESIAN_POINT('Ctrl Pts',(-20.4356240768759,-37.7310950566383,
122.778550847944)) ;
#76752 = CARTESIAN_POINT('Ctrl Pts',(-20.5352958891587,-37.9210866679751,
122.409330679818)) ;
#76753 = CARTESIAN_POINT('Ctrl Pts',(-20.3100810068094,-37.7410975875563,
122.60981908937)) ;
#76754 = CARTESIAN_POINT('Ctrl Pts',(-20.3432724836096,-37.9311212944326,
122.228617908645)) ;
#76755 = CARTESIAN_POINT('Ctrl Pts',(-20.1564607864245,-37.7511322140138,
122.465250443075)) ;
#76756 = CARTESIAN_POINT('Ctrl Pts',(-20.1271504516015,-37.940966829419,122.086359667604)) ;
#76757 = CARTESIAN_POINT('Ctrl Pts',(-19.9835623661803,-37.7609777490003,
122.351445878483)) ;
#76758 = CARTESIAN_POINT('Ctrl Pts',(-19.8865382084238,-37.950950254258,121.981841696319)) ;
#76759 = CARTESIAN_POINT('Ctrl Pts',(-19.7910718730727,-37.7709611738393,
122.267833461775)) ;
#76760 = CARTESIAN_POINT('Ctrl Pts',(-19.632237024873,-37.9609006446231,121.920936388856)) ;
#76761 = CARTESIAN_POINT('Ctrl Pts',(-19.5876306530056,-37.7809115642044,
122.219111287148)) ;
#76762 = CARTESIAN_POINT('Ctrl Pts',(-19.3699906918053,-37.9708982849202,
121.904681189233)) ;
#76763 = CARTESIAN_POINT('Ctrl Pts',(-19.3778335442572,-37.7909092045014,
122.206109169459)) ;
#76764 = CARTESIAN_POINT('Ctrl Pts',(-19.1079206636086,-37.9809373654834,
121.934852971081)) ;
#76765 = CARTESIAN_POINT('Ctrl Pts',(-19.1681777138388,-37.8009482850646,
122.230248687512)) ;
#76766 = CARTESIAN_POINT('Ctrl Pts',(-18.860240682619,-37.9907635162525,122.007929238494)) ;
#76767 = CARTESIAN_POINT('Ctrl Pts',(-18.9700348973941,-37.8107744358337,
122.288711477367)) ;
#76768 = CARTESIAN_POINT('Ctrl Pts',(-18.6234287246879,-38.0008200911816,
122.125206427467)) ;
#76769 = CARTESIAN_POINT('Ctrl Pts',(-18.7805861344579,-37.8208310107629,
122.382535045153)) ;
#76770 = CARTESIAN_POINT('Ctrl Pts',(-18.4132844278419,-38.0107606305619,
122.280394942206)) ;
#76771 = CARTESIAN_POINT('Ctrl Pts',(-18.6124721241605,-37.8307715501431,
122.506687339545)) ;
#76772 = CARTESIAN_POINT('Ctrl Pts',(-18.2333456790557,-38.0206650235383,
122.46846128284)) ;
#76773 = CARTESIAN_POINT('Ctrl Pts',(-18.4685228183294,-37.8406759431195,
122.657141441045)) ;
#76774 = CARTESIAN_POINT('Ctrl Pts',(-18.0868734495751,-38.0307116777432,
122.688093340425)) ;
#76775 = CARTESIAN_POINT('Ctrl Pts',(-18.3513466170776,-37.8507225973244,
122.832848242214)) ;
#76776 = CARTESIAN_POINT('Ctrl Pts',(-17.9821139834346,-38.0406072396816,
122.926149688443)) ;
#76777 = CARTESIAN_POINT('Ctrl Pts',(-18.2675409920432,-37.8606181592628,
123.023293667874)) ;
#76778 = CARTESIAN_POINT('Ctrl Pts',(-17.9192592235036,-38.0506693175272,
123.182952338483)) ;
#76779 = CARTESIAN_POINT('Ctrl Pts',(-18.2172590200462,-37.8706802371084,
123.228736387907)) ;
#76780 = CARTESIAN_POINT('Ctrl Pts',(-17.9021734627855,-38.0605120159409,
123.441072933948)) ;
#76781 = CARTESIAN_POINT('Ctrl Pts',(-18.2035923555535,-37.8805229355222,
123.43523229754)) ;
#76782 = CARTESIAN_POINT('Ctrl Pts',(-17.929962860664,-38.0705027909024,123.702111270604)) ;
#76783 = CARTESIAN_POINT('Ctrl Pts',(-18.2258256600623,-37.8905137104836,
123.644062635813)) ;
#76784 = CARTESIAN_POINT('Ctrl Pts',(-18.002248222922,-38.0804306559215,123.952806457273)) ;
#76785 = CARTESIAN_POINT('Ctrl Pts',(-18.2836555848188,-37.9004415755027,
123.844617906558)) ;
#76786 = CARTESIAN_POINT('Ctrl Pts',(-18.1172694269182,-38.0904194006877,
124.188763665536)) ;
#76787 = CARTESIAN_POINT('Ctrl Pts',(-18.3756740525521,-37.9104303202689,
124.033382779807)) ;
#76788 = CARTESIAN_POINT('Ctrl Pts',(-18.2725063779135,-38.1004521862746,
124.401872836947)) ;
#76789 = CARTESIAN_POINT('Ctrl Pts',(-18.4998651103405,-37.9204631058559,
124.203869099965)) ;
#76790 = CARTESIAN_POINT('Ctrl Pts',(-18.4590525160072,-38.1103188708953,
124.581942987187)) ;
#76791 = CARTESIAN_POINT('Ctrl Pts',(-18.6491027477406,-37.9303297904765,
124.347923469176)) ;
#76792 = CARTESIAN_POINT('Ctrl Pts',(-18.6756943059333,-38.1202807630584,
124.728918023336)) ;
#76793 = CARTESIAN_POINT('Ctrl Pts',(-18.8224168656527,-37.9402916826396,
124.46550199026)) ;
#76794 = CARTESIAN_POINT('Ctrl Pts',(-18.9164378070636,-38.130314239971,124.836426983347)) ;
#76795 = CARTESIAN_POINT('Ctrl Pts',(-19.0150124287312,-37.9503251595522,
124.551507627464)) ;
#76796 = CARTESIAN_POINT('Ctrl Pts',(-19.1683321359597,-38.1401985812193,
124.899959302474)) ;
#76797 = CARTESIAN_POINT('Ctrl Pts',(-19.2165276738214,-37.9602095008005,
124.602331745054)) ;
#76798 = CARTESIAN_POINT('Ctrl Pts',(-19.4320465863461,-38.1502615233404,
124.919128358808)) ;
#76799 = CARTESIAN_POINT('Ctrl Pts',(-19.4274995576439,-37.9702724429217,
124.617665373635)) ;
#76800 = CARTESIAN_POINT('Ctrl Pts',(-19.6895940464607,-38.16011192496,124.89290473406)) ;
#76801 = CARTESIAN_POINT('Ctrl Pts',(-19.6335365291386,-37.9801228445412,
124.596684955515)) ;
#76802 = CARTESIAN_POINT('Ctrl Pts',(-19.9432929414495,-38.1701388137496,
124.821745925564)) ;
#76803 = CARTESIAN_POINT('Ctrl Pts',(-19.8364952746785,-37.9901497333309,
124.539756471089)) ;
#76804 = CARTESIAN_POINT('Ctrl Pts',(-20.1805416770185,-38.1801674287058,
124.706967424715)) ;
#76805 = CARTESIAN_POINT('Ctrl Pts',(-20.0262936087495,-38.0001783482871,
124.447932190044)) ;
#76806 = CARTESIAN_POINT('Ctrl Pts',(-20.3906137721402,-38.1900126518259,
124.555971632275)) ;
#76807 = CARTESIAN_POINT('Ctrl Pts',(-20.1943496685895,-38.0100235714072,
124.327134842774)) ;
#76808 = CARTESIAN_POINT('Ctrl Pts',(-20.5744646117543,-38.2000033356319,
124.368535624732)) ;
#76809 = CARTESIAN_POINT('Ctrl Pts',(-20.3414292436618,-38.0200142552131,
124.177185180511)) ;
#76810 = CARTESIAN_POINT('Ctrl Pts',(-20.7231886884151,-38.2100412177043,
124.150677424846)) ;
#76811 = CARTESIAN_POINT('Ctrl Pts',(-20.4604073258307,-38.0300521372856,
124.002897686156)) ;
#76812 = CARTESIAN_POINT('Ctrl Pts',(-20.8301490997781,-38.2198855773431,
123.915113415495)) ;
#76813 = CARTESIAN_POINT('Ctrl Pts',(-20.5459739843948,-38.0398964969244,
123.814446751513)) ;
#76814 = CARTESIAN_POINT('Ctrl Pts',(-20.8959919669497,-38.2298704479579,
123.661153850829)) ;
#76815 = CARTESIAN_POINT('Ctrl Pts',(-20.5986469676164,-38.0498813675391,
123.611278966283)) ;
#76816 = CARTESIAN_POINT('Ctrl Pts',(-20.9167692457474,-38.2398097312865,
123.400748772404)) ;
#76817 = CARTESIAN_POINT('Ctrl Pts',(-20.6152674855689,-38.0598206508678,
123.402955237377)) ;
#76818 = CARTESIAN_POINT('Ctrl Pts',(-20.8916876626832,-38.2498503406597,
123.138114322837)) ;
#76819 = CARTESIAN_POINT('Ctrl Pts',(-20.5952009193857,-38.0698612602409,
123.192847680362)) ;
#76820 = CARTESIAN_POINT('Ctrl Pts',(-20.8226462972461,-38.2597351915729,
122.887662089214)) ;
#76821 = CARTESIAN_POINT('Ctrl Pts',(-20.5399668195097,-38.0797461111542,
122.992486951818)) ;
#76822 = CARTESIAN_POINT('Ctrl Pts',(-20.7101619938538,-38.2697371477417,
122.650150261897)) ;
#76823 = CARTESIAN_POINT('Ctrl Pts',(-20.44997835604,-38.089748067323,122.802478099931)) ;
#76824 = CARTESIAN_POINT('Ctrl Pts',(-20.5595370995574,-38.2796557444622,
122.437376954918)) ;
#76825 = CARTESIAN_POINT('Ctrl Pts',(-20.3294778457341,-38.0996666640434,
122.632260578575)) ;
#76826 = CARTESIAN_POINT('Ctrl Pts',(-20.3718806510346,-38.289702566538,122.251710845109)) ;
#76827 = CARTESIAN_POINT('Ctrl Pts',(-20.1793517557982,-38.1097134861192,
122.483728389381)) ;
#76828 = CARTESIAN_POINT('Ctrl Pts',(-20.1586361997341,-38.2995768476507,
122.103781930012)) ;
#76829 = CARTESIAN_POINT('Ctrl Pts',(-20.0087562603686,-38.1195877672319,
122.365386632677)) ;
#76830 = CARTESIAN_POINT('Ctrl Pts',(-19.9188009996672,-38.3096310476953,
121.993039914005)) ;
#76831 = CARTESIAN_POINT('Ctrl Pts',(-19.8168874663292,-38.1296419672765,
122.276793896463)) ;
#76832 = CARTESIAN_POINT('Ctrl Pts',(-19.6673495935164,-38.3195264773305,
121.926560228982)) ;
#76833 = CARTESIAN_POINT('Ctrl Pts',(-19.615726790868,-38.1395373969118,122.223611339034)) ;
#76834 = CARTESIAN_POINT('Ctrl Pts',(-19.4039095755327,-38.3295881056479,
121.904328761381)) ;
#76835 = CARTESIAN_POINT('Ctrl Pts',(-19.4049744286583,-38.1495990252291,
122.20582716044)) ;
#76836 = CARTESIAN_POINT('Ctrl Pts',(-19.1462446839962,-38.3394327344778,
121.92763291997)) ;
#76837 = CARTESIAN_POINT('Ctrl Pts',(-19.1988436604768,-38.159443654059,122.224471403124)) ;
#76838 = CARTESIAN_POINT('Ctrl Pts',(-18.8933810810539,-38.3493927820834,
121.995203018732)) ;
#76839 = CARTESIAN_POINT('Ctrl Pts',(-18.9965533361364,-38.1694037016646,
122.278528153739)) ;
#76840 = CARTESIAN_POINT('Ctrl Pts',(-18.6544538829117,-38.3594310882575,
122.106985936692)) ;
#76841 = CARTESIAN_POINT('Ctrl Pts',(-18.8054118480748,-38.1794420078387,
122.367955372878)) ;
#76842 = CARTESIAN_POINT('Ctrl Pts',(-18.4417836192416,-38.3693043876901,
122.255686315655)) ;
#76843 = CARTESIAN_POINT('Ctrl Pts',(-18.6352768308471,-38.1893153072714,
122.486915811868)) ;
#76844 = CARTESIAN_POINT('Ctrl Pts',(-18.2545726342933,-38.3793776492764,
122.442761738828)) ;
#76845 = CARTESIAN_POINT('Ctrl Pts',(-18.4855083791044,-38.1993885688576,
122.636576970832)) ;
#76846 = CARTESIAN_POINT('Ctrl Pts',(-18.1061577775642,-38.3891978752331,
122.653952115977)) ;
#76847 = CARTESIAN_POINT('Ctrl Pts',(-18.3667778089366,-38.2092087948143,
122.805528675082)) ;
#76848 = CARTESIAN_POINT('Ctrl Pts',(-17.9936243509506,-38.3992769391726,
122.89364946878)) ;
#76849 = CARTESIAN_POINT('Ctrl Pts',(-18.2767515207265,-38.2192878587538,
122.997287189187)) ;
#76850 = CARTESIAN_POINT('Ctrl Pts',(-17.9258375543996,-38.4091270291924,
123.143539427575)) ;
#76851 = CARTESIAN_POINT('Ctrl Pts',(-18.2225229861537,-38.2291379487737,
123.197198298179)) ;
#76852 = CARTESIAN_POINT('Ctrl Pts',(-17.901802683763,-38.4192057828062,123.40723841002)) ;
#76853 = CARTESIAN_POINT('Ctrl Pts',(-18.2032956687307,-38.2392167023874,
123.408157924605)) ;
#76854 = CARTESIAN_POINT('Ctrl Pts',(-17.9231669694518,-38.4290272500656,
123.664509279097)) ;
#76855 = CARTESIAN_POINT('Ctrl Pts',(-18.2203875531494,-38.2490381696469,
123.613973301711)) ;
#76856 = CARTESIAN_POINT('Ctrl Pts',(-17.9900867206305,-38.4390928484233,
123.920355248503)) ;
#76857 = CARTESIAN_POINT('Ctrl Pts',(-18.2739238795727,-38.2591037680045,
123.818650252036)) ;
#76858 = CARTESIAN_POINT('Ctrl Pts',(-18.0987428643618,-38.448995504198,124.156888509118)) ;
#76859 = CARTESIAN_POINT('Ctrl Pts',(-18.3608489306835,-38.2690064237792,
124.007875995514)) ;
#76860 = CARTESIAN_POINT('Ctrl Pts',(-18.2488988280731,-38.4590463300276,
124.374113939664)) ;
#76861 = CARTESIAN_POINT('Ctrl Pts',(-18.4809742059933,-38.2790572496089,
124.181656254911)) ;
#76862 = CARTESIAN_POINT('Ctrl Pts',(-18.4311282812426,-38.4689205343665,
124.558922029274)) ;
#76863 = CARTESIAN_POINT('Ctrl Pts',(-18.6267574017553,-38.2889314539477,
124.329501781547)) ;
#76864 = CARTESIAN_POINT('Ctrl Pts',(-18.6468226000267,-38.4789929844056,
124.712247945109)) ;
#76865 = CARTESIAN_POINT('Ctrl Pts',(-18.7993133663225,-38.2990039039868,
124.452162386081)) ;
#76866 = CARTESIAN_POINT('Ctrl Pts',(-18.8800743167449,-38.4888220011791,
124.823318123701)) ;
#76867 = CARTESIAN_POINT('Ctrl Pts',(-18.985913767497,-38.3088329207603,124.54101769674)) ;
#76868 = CARTESIAN_POINT('Ctrl Pts',(-19.1349034186405,-38.4988888470939,
124.894192497896)) ;
#76869 = CARTESIAN_POINT('Ctrl Pts',(-19.18977742163,-38.3188997666751,124.597717046058)) ;
#76870 = CARTESIAN_POINT('Ctrl Pts',(-19.3936404772046,-38.5087790183957,
124.919135574691)) ;
#76871 = CARTESIAN_POINT('Ctrl Pts',(-19.3967662609791,-38.3287899379769,
124.6176711408)) ;
#76872 = CARTESIAN_POINT('Ctrl Pts',(-19.6554475745785,-38.5187712120195,
124.899143715497)) ;
#76873 = CARTESIAN_POINT('Ctrl Pts',(-19.6062117573264,-38.3387821316008,
124.601677525334)) ;
#76874 = CARTESIAN_POINT('Ctrl Pts',(-19.9090056650596,-38.5287340226429,
124.833945501383)) ;
#76875 = CARTESIAN_POINT('Ctrl Pts',(-19.8090578249638,-38.3487449422242,
124.549518845411)) ;
#76876 = CARTESIAN_POINT('Ctrl Pts',(-20.1462891749029,-38.5386382954864,
124.726937805289)) ;
#76877 = CARTESIAN_POINT('Ctrl Pts',(-19.9988839326754,-38.3586492150676,
124.463912964312)) ;
#76878 = CARTESIAN_POINT('Ctrl Pts',(-20.364605703527,-38.548698787291,124.577884540277)) ;
#76879 = CARTESIAN_POINT('Ctrl Pts',(-20.173537335335,-38.3687097068723,124.344670113735)) ;
#76880 = CARTESIAN_POINT('Ctrl Pts',(-20.5498721513318,-38.5585391189633,
124.397423633109)) ;
#76881 = CARTESIAN_POINT('Ctrl Pts',(-20.3217496440126,-38.3785500385446,
124.200302203012)) ;
#76882 = CARTESIAN_POINT('Ctrl Pts',(-20.7046268369188,-38.5686021650551,
124.183029887314)) ;
#76883 = CARTESIAN_POINT('Ctrl Pts',(-20.4455536256558,-38.3886130846363,
124.028787005913)) ;
#76884 = CARTESIAN_POINT('Ctrl Pts',(-20.8177037944646,-38.5784962207502,
123.948871113665)) ;
#76885 = CARTESIAN_POINT('Ctrl Pts',(-20.5360148493182,-38.3985071403314,
123.841460727974)) ;
#76886 = CARTESIAN_POINT('Ctrl Pts',(-20.889425745964,-38.5884389210731,123.697654055554)) ;
#76887 = CARTESIAN_POINT('Ctrl Pts',(-20.5933924604119,-38.4084498406544,
123.640487633951)) ;
#76888 = CARTESIAN_POINT('Ctrl Pts',(-20.916667441635,-38.5984446620007,123.436101061358)) ;
#76889 = CARTESIAN_POINT('Ctrl Pts',(-20.6151860207473,-38.418455581582,123.431245328084)) ;
#76890 = CARTESIAN_POINT('Ctrl Pts',(-20.8977588228678,-38.6084655725163,
123.173448091047)) ;
#76891 = CARTESIAN_POINT('Ctrl Pts',(-20.6000592553857,-38.4284764920975,
123.221122910589)) ;
#76892 = CARTESIAN_POINT('Ctrl Pts',(-20.8346540511211,-38.6183563079662,
122.921298084091)) ;
#76893 = CARTESIAN_POINT('Ctrl Pts',(-20.5495758458622,-38.4383672275475,
123.019403663293)) ;
#76894 = CARTESIAN_POINT('Ctrl Pts',(-20.7280091757343,-38.6283478486951,
122.681375284334)) ;
#76895 = CARTESIAN_POINT('Ctrl Pts',(-20.4642602954684,-38.4483587682763,
122.827465455942)) ;
#76896 = CARTESIAN_POINT('Ctrl Pts',(-20.5819003599623,-38.6382957091167,
122.464600481012)) ;
#76897 = CARTESIAN_POINT('Ctrl Pts',(-20.3473737456245,-38.458306628698,122.654045845982)) ;
#76898 = CARTESIAN_POINT('Ctrl Pts',(-20.4007533562196,-38.6482423783031,
122.276140396781)) ;
#76899 = CARTESIAN_POINT('Ctrl Pts',(-20.2024567640308,-38.4682532978843,
122.503277819394)) ;
#76900 = CARTESIAN_POINT('Ctrl Pts',(-20.1873323482712,-38.6582904544387,
122.12067245953)) ;
#76901 = CARTESIAN_POINT('Ctrl Pts',(-20.0317199988072,-38.4783013740199,
122.378903072768)) ;
#76902 = CARTESIAN_POINT('Ctrl Pts',(-19.954975200177,-38.6681380524443,122.006738756119)) ;
#76903 = CARTESIAN_POINT('Ctrl Pts',(-19.8458354617128,-38.4881489720256,
122.287756243606)) ;
#76904 = CARTESIAN_POINT('Ctrl Pts',(-19.7037273294392,-38.6780997755288,
121.933263220615)) ;
#76905 = CARTESIAN_POINT('Ctrl Pts',(-19.6448376844739,-38.49811069511,122.228975335749)) ;
#76906 = CARTESIAN_POINT('Ctrl Pts',(-19.4417254602115,-38.6881284106118,
121.904664952623)) ;
#76907 = CARTESIAN_POINT('Ctrl Pts',(-19.435236168815,-38.508139330193,122.206096194811)) ;
#76908 = CARTESIAN_POINT('Ctrl Pts',(-19.1818626712989,-38.6980387189298,
121.921702009189)) ;
#76909 = CARTESIAN_POINT('Ctrl Pts',(-19.2273466015253,-38.5180496385111,
122.219725252916)) ;
#76910 = CARTESIAN_POINT('Ctrl Pts',(-18.9280968781733,-38.7079736160657,
121.983094997381)) ;
#76911 = CARTESIAN_POINT('Ctrl Pts',(-19.0243343132026,-38.5279845356469,
122.268838827757)) ;
#76912 = CARTESIAN_POINT('Ctrl Pts',(-18.6864010148736,-38.7180146990083,
122.088952068189)) ;
#76913 = CARTESIAN_POINT('Ctrl Pts',(-18.830977224545,-38.5380256185895,122.353523948551)) ;
#76914 = CARTESIAN_POINT('Ctrl Pts',(-18.470002959374,-38.7279020418365,122.232792348732)) ;
#76915 = CARTESIAN_POINT('Ctrl Pts',(-18.6578590879055,-38.5479129614178,
122.468595134658)) ;
#76916 = CARTESIAN_POINT('Ctrl Pts',(-18.2795943517483,-38.7378935567758,
122.413563464175)) ;
#76917 = CARTESIAN_POINT('Ctrl Pts',(-18.5055317681181,-38.5579044763571,
122.613211332423)) ;
#76918 = CARTESIAN_POINT('Ctrl Pts',(-18.1241690741951,-38.7478449479723,
122.623883939049)) ;
#76919 = CARTESIAN_POINT('Ctrl Pts',(-18.3811911759621,-38.5678558675536,
122.781466905472)) ;
#76920 = CARTESIAN_POINT('Ctrl Pts',(-18.0074429396935,-38.7577774813049,
122.857344924789)) ;
#76921 = CARTESIAN_POINT('Ctrl Pts',(-18.2878097133205,-38.5777884008862,
122.968234824021)) ;
#76922 = CARTESIAN_POINT('Ctrl Pts',(-17.9324451630924,-38.7677746392044,
123.109116894499)) ;
#76923 = CARTESIAN_POINT('Ctrl Pts',(-18.2278106582551,-38.5877855587856,
123.1696520247)) ;
#76924 = CARTESIAN_POINT('Ctrl Pts',(-17.9022350150064,-38.7777596493679,
123.369808873097)) ;
#76925 = CARTESIAN_POINT('Ctrl Pts',(-18.2036416362819,-38.5977705689491,
123.378205317584)) ;
#76926 = CARTESIAN_POINT('Ctrl Pts',(-17.9182204761014,-38.7878024759377,
123.633203162135)) ;
#76927 = CARTESIAN_POINT('Ctrl Pts',(-18.2164291783058,-38.6078133955189,
123.588920944231)) ;
#76928 = CARTESIAN_POINT('Ctrl Pts',(-17.9778363799748,-38.7976327102426,
123.884601181643)) ;
#76929 = CARTESIAN_POINT('Ctrl Pts',(-18.2641206846296,-38.6176436298239,
123.790038464492)) ;
#76930 = CARTESIAN_POINT('Ctrl Pts',(-18.0826097272587,-38.8077087354773,
124.12771836108)) ;
#76931 = CARTESIAN_POINT('Ctrl Pts',(-18.3479385732616,-38.6277196550586,
123.984532923754)) ;
#76932 = CARTESIAN_POINT('Ctrl Pts',(-18.2247229698765,-38.8175609719682,
124.344203206697)) ;
#76933 = CARTESIAN_POINT('Ctrl Pts',(-18.4616277604428,-38.6375718915494,
124.157720543777)) ;
#76934 = CARTESIAN_POINT('Ctrl Pts',(-18.4060166291927,-38.8276341784023,
124.537031920966)) ;
#76935 = CARTESIAN_POINT('Ctrl Pts',(-18.6066621150346,-38.6476450979836,
124.311984493962)) ;
#76936 = CARTESIAN_POINT('Ctrl Pts',(-18.6132523457623,-38.8374756879095,
124.691787453211)) ;
#76937 = CARTESIAN_POINT('Ctrl Pts',(-18.7724492132766,-38.6574866074907,
124.435789153201)) ;
#76938 = CARTESIAN_POINT('Ctrl Pts',(-18.8465449134699,-38.8474366346893,
124.810489310381)) ;
#76939 = CARTESIAN_POINT('Ctrl Pts',(-18.9590823935704,-38.6674475542705,
124.530751641621)) ;
#76940 = CARTESIAN_POINT('Ctrl Pts',(-19.098990635747,-38.8574744634893,124.886965770344)) ;
#76941 = CARTESIAN_POINT('Ctrl Pts',(-19.1610387331382,-38.6774853830706,
124.591933962578)) ;
#76942 = CARTESIAN_POINT('Ctrl Pts',(-19.3565960865139,-38.8673487732438,
124.918417832389)) ;
#76943 = CARTESIAN_POINT('Ctrl Pts',(-19.3671221354591,-38.687359692825,124.617096782375)) ;
#76944 = CARTESIAN_POINT('Ctrl Pts',(-19.6208093648921,-38.8774184709169,
124.904380279323)) ;
#76945 = CARTESIAN_POINT('Ctrl Pts',(-19.5784931043603,-38.6974293904982,
124.605867998489)) ;
#76946 = CARTESIAN_POINT('Ctrl Pts',(-19.8726090819025,-38.8872519422043,
124.84620010404)) ;
#76947 = CARTESIAN_POINT('Ctrl Pts',(-19.779932174487,-38.7072628617856,124.559325358216)) ;
#76948 = CARTESIAN_POINT('Ctrl Pts',(-20.1154997479341,-38.8972815887343,
124.743876964868)) ;
#76949 = CARTESIAN_POINT('Ctrl Pts',(-19.9742453375795,-38.7172925083155,
124.477468165888)) ;
#76950 = CARTESIAN_POINT('Ctrl Pts',(-20.3366133293016,-38.9073161030616,
124.60018424076)) ;
#76951 = CARTESIAN_POINT('Ctrl Pts',(-20.1511369670628,-38.7273270226429,
124.362515034824)) ;
#76952 = CARTESIAN_POINT('Ctrl Pts',(-20.5258195611414,-38.9171413885325,
124.424489905026)) ;
#76953 = CARTESIAN_POINT('Ctrl Pts',(-20.3025021660536,-38.7371523081138,
124.221961312577)) ;
#76954 = CARTESIAN_POINT('Ctrl Pts',(-20.6849082649732,-38.9271456300811,
124.215225042755)) ;
#76955 = CARTESIAN_POINT('Ctrl Pts',(-20.4297743088031,-38.7471565496623,
124.054550406334)) ;
#76956 = CARTESIAN_POINT('Ctrl Pts',(-20.8049240327782,-38.9371282751602,
123.98189798351)) ;
#76957 = CARTESIAN_POINT('Ctrl Pts',(-20.5257881879668,-38.7571391947414,
123.867889603181)) ;
#76958 = CARTESIAN_POINT('Ctrl Pts',(-20.8827806720489,-38.9471734722517,
123.729693087447)) ;
#76959 = CARTESIAN_POINT('Ctrl Pts',(-20.5880749231069,-38.7671843918329,
123.666125997018)) ;
#76960 = CARTESIAN_POINT('Ctrl Pts',(-20.9153734465156,-38.9569965880118,
123.473607472968)) ;
#76961 = CARTESIAN_POINT('Ctrl Pts',(-20.6141505414293,-38.7770075075931,
123.461258688752)) ;
#76962 = CARTESIAN_POINT('Ctrl Pts',(-20.9034051257654,-38.9670311998121,
123.210183840089)) ;
#76963 = CARTESIAN_POINT('Ctrl Pts',(-20.6045775434522,-38.7870421193933,
123.250519622744)) ;
#76964 = CARTESIAN_POINT('Ctrl Pts',(-20.845214157011,-38.9770562085853,122.953236014163)) ;
#76965 = CARTESIAN_POINT('Ctrl Pts',(-20.5580262508377,-38.7970671281665,
123.044961006179)) ;
#76966 = CARTESIAN_POINT('Ctrl Pts',(-20.7455751867444,-38.9869081334268,
122.714273478696)) ;
#76967 = CARTESIAN_POINT('Ctrl Pts',(-20.4783168903162,-38.8069190530081,
122.853791094508)) ;
#76968 = CARTESIAN_POINT('Ctrl Pts',(-20.6043472153065,-38.9968990717495,
122.492979055676)) ;
#76969 = CARTESIAN_POINT('Ctrl Pts',(-20.3653360237467,-38.8169099913308,
122.676754754454)) ;
#76970 = CARTESIAN_POINT('Ctrl Pts',(-20.4282184151708,-39.006817056896,122.300819554169)) ;
#76971 = CARTESIAN_POINT('Ctrl Pts',(-20.2244345676972,-38.8268279764772,
122.523026321021)) ;
#76972 = CARTESIAN_POINT('Ctrl Pts',(-20.2191839000124,-39.0168451577915,
122.140380206256)) ;
#76973 = CARTESIAN_POINT('Ctrl Pts',(-20.0572079946836,-38.8368560773727,
122.394673443587)) ;
#76974 = CARTESIAN_POINT('Ctrl Pts',(-19.988823563401,-39.026730398734,122.020299045281)) ;
#76975 = CARTESIAN_POINT('Ctrl Pts',(-19.8729210602191,-38.8467413183153,
122.298607226252)) ;
#76976 = CARTESIAN_POINT('Ctrl Pts',(-19.7387023265597,-39.0367195117007,
121.940602617632)) ;
#76977 = CARTESIAN_POINT('Ctrl Pts',(-19.6728247564175,-38.8567304312819,
122.234848346961)) ;
#76978 = CARTESIAN_POINT('Ctrl Pts',(-19.4771010747282,-39.0467615760415,
121.905935512444)) ;
#76979 = CARTESIAN_POINT('Ctrl Pts',(-19.4635439135823,-38.8667724956227,
122.207112896485)) ;
#76980 = CARTESIAN_POINT('Ctrl Pts',(-19.2190051557657,-39.056590777446,121.916489575478)) ;
#76981 = CARTESIAN_POINT('Ctrl Pts',(-19.2570678745084,-38.8766016970272,
122.215554268652)) ;
#76982 = CARTESIAN_POINT('Ctrl Pts',(-18.9620194272322,-39.0665976182042,
121.97212452845)) ;
#76983 = CARTESIAN_POINT('Ctrl Pts',(-19.0514789416566,-38.8866085377854,
122.260060324957)) ;
#76984 = CARTESIAN_POINT('Ctrl Pts',(-18.7190580246496,-39.0765851423961,
122.071516726023)) ;
#76985 = CARTESIAN_POINT('Ctrl Pts',(-18.8571092146858,-38.8965960619773,
122.339572267112)) ;
#76986 = CARTESIAN_POINT('Ctrl Pts',(-18.496263286166,-39.0866147882047,122.212294698835)) ;
#76987 = CARTESIAN_POINT('Ctrl Pts',(-18.6788723982506,-38.9066257077859,
122.452193065279)) ;
#76988 = CARTESIAN_POINT('Ctrl Pts',(-18.304074260206,-39.0964888189434,122.386670421032)) ;
#76989 = CARTESIAN_POINT('Ctrl Pts',(-18.5251202815215,-38.9164997385247,
122.591691852851)) ;
#76990 = CARTESIAN_POINT('Ctrl Pts',(-18.1428504126763,-39.1064881418075,
122.594116058551)) ;
#76991 = CARTESIAN_POINT('Ctrl Pts',(-18.3961396994837,-38.9264990613888,
122.757647081838)) ;
#76992 = CARTESIAN_POINT('Ctrl Pts',(-18.0209136490319,-39.1163989773831,
122.824305926525)) ;
#76993 = CARTESIAN_POINT('Ctrl Pts',(-18.2985886964444,-38.9364098969644,
122.941797703191)) ;
#76994 = CARTESIAN_POINT('Ctrl Pts',(-17.9397564184948,-39.1264532253572,
123.075703741541)) ;
#76995 = CARTESIAN_POINT('Ctrl Pts',(-18.2336609864209,-38.9464641449384,
123.142915426417)) ;
#76996 = CARTESIAN_POINT('Ctrl Pts',(-17.9038739772955,-39.1363119696199,
123.332330097257)) ;
#76997 = CARTESIAN_POINT('Ctrl Pts',(-18.2049530965617,-38.9563228892011,
123.348215715669)) ;
#76998 = CARTESIAN_POINT('Ctrl Pts',(-17.9131303555369,-39.1463800556929,
123.596708290319)) ;
#76999 = CARTESIAN_POINT('Ctrl Pts',(-18.2123561545412,-38.9663909752741,
123.559718464088)) ;
#77000 = CARTESIAN_POINT('Ctrl Pts',(-17.967021152229,-39.1562355388724,123.850053708691)) ;
#77001 = CARTESIAN_POINT('Ctrl Pts',(-18.2554666875822,-38.9762464584537,
123.762394736116)) ;
#77002 = CARTESIAN_POINT('Ctrl Pts',(-18.064713155992,-39.1662303846666,124.09385471535)) ;
#77003 = CARTESIAN_POINT('Ctrl Pts',(-18.3336182833703,-38.9862413042478,
123.957436260119)) ;
#77004 = CARTESIAN_POINT('Ctrl Pts',(-18.2042478280738,-39.1762616803291,
124.317515212266)) ;
#77005 = CARTESIAN_POINT('Ctrl Pts',(-18.4452442635705,-38.9962725999104,
124.136365752348)) ;
#77006 = CARTESIAN_POINT('Ctrl Pts',(-18.3772981541373,-39.186128223619,124.510610102703)) ;
#77007 = CARTESIAN_POINT('Ctrl Pts',(-18.5836826763418,-39.0061391432003,
124.290842767909)) ;
#77008 = CARTESIAN_POINT('Ctrl Pts',(-18.5834523133423,-39.1961156193824,
124.672993813523)) ;
#77009 = CARTESIAN_POINT('Ctrl Pts',(-18.7486045943314,-39.0161265389636,
124.420751367233)) ;
#77010 = CARTESIAN_POINT('Ctrl Pts',(-18.8136849280849,-39.2060606601123,
124.79674572474)) ;
#77011 = CARTESIAN_POINT('Ctrl Pts',(-18.9327894986595,-39.0260715796936,
124.519754710555)) ;
#77012 = CARTESIAN_POINT('Ctrl Pts',(-19.0643744384827,-39.2161051663291,
124.879300115925)) ;
#77013 = CARTESIAN_POINT('Ctrl Pts',(-19.1333404484933,-39.0361160859103,
124.585800271082)) ;
#77014 = CARTESIAN_POINT('Ctrl Pts',(-19.3209006976884,-39.2259686724664,
124.916631731258)) ;
#77015 = CARTESIAN_POINT('Ctrl Pts',(-19.3385608066028,-39.0459795920477,
124.61566765999)) ;
#77016 = CARTESIAN_POINT('Ctrl Pts',(-19.5833595972612,-39.2359615333025,
124.909220187244)) ;
#77017 = CARTESIAN_POINT('Ctrl Pts',(-19.5485279119773,-39.0559724528837,
124.609740630112)) ;
#77018 = CARTESIAN_POINT('Ctrl Pts',(-19.8389276222297,-39.2458877270214,
124.856807197051)) ;
#77019 = CARTESIAN_POINT('Ctrl Pts',(-19.7529826014343,-39.0658986466027,
124.567812433635)) ;
#77020 = CARTESIAN_POINT('Ctrl Pts',(-20.0837340012859,-39.255906653054,124.759990302434)) ;
#77021 = CARTESIAN_POINT('Ctrl Pts',(-19.9488284801805,-39.0759175726352,
124.490360989848)) ;
#77022 = CARTESIAN_POINT('Ctrl Pts',(-20.3058732170056,-39.2658216524216,
124.623740322537)) ;
#77023 = CARTESIAN_POINT('Ctrl Pts',(-20.1265408661882,-39.0858325720028,
124.381362989768)) ;
#77024 = CARTESIAN_POINT('Ctrl Pts',(-20.5036398439104,-39.2758764239789,
124.448561262055)) ;
#77025 = CARTESIAN_POINT('Ctrl Pts',(-20.2847556360216,-39.0958873435601,
124.241221409002)) ;
#77026 = CARTESIAN_POINT('Ctrl Pts',(-20.6649559414728,-39.2857353862764,
124.245785908709)) ;
#77027 = CARTESIAN_POINT('Ctrl Pts',(-20.4138101229452,-39.1057463058577,
124.079002680325)) ;
#77028 = CARTESIAN_POINT('Ctrl Pts',(-20.7907073338541,-39.2957296301143,
124.015257630053)) ;
#77029 = CARTESIAN_POINT('Ctrl Pts',(-20.5144131818237,-39.1157405496955,
123.894581187682)) ;
#77030 = CARTESIAN_POINT('Ctrl Pts',(-20.8740852787271,-39.3056548595385,
123.768075589562)) ;
#77031 = CARTESIAN_POINT('Ctrl Pts',(-20.5811176317263,-39.1256657791198,
123.696836372389)) ;
#77032 = CARTESIAN_POINT('Ctrl Pts',(-20.9136831802489,-39.31568282343,123.507578576394)) ;
#77033 = CARTESIAN_POINT('Ctrl Pts',(-20.6127981700986,-39.1356937430112,
123.488439150127)) ;
#77034 = CARTESIAN_POINT('Ctrl Pts',(-20.9078028794993,-39.3255690830604,
123.247805457991)) ;
#77035 = CARTESIAN_POINT('Ctrl Pts',(-20.6080961812906,-39.1455800026416,
123.280620698185)) ;
#77036 = CARTESIAN_POINT('Ctrl Pts',(-20.8563083056204,-39.3356008461382,
122.989304179188)) ;
#77037 = CARTESIAN_POINT('Ctrl Pts',(-20.5669027458931,-39.1556117657195,
123.07381928786)) ;
#77038 = CARTESIAN_POINT('Ctrl Pts',(-20.7623452755489,-39.3454824724324,
122.747171858477)) ;
#77039 = CARTESIAN_POINT('Ctrl Pts',(-20.4917344390515,-39.1654933920136,
122.880112663831)) ;
#77040 = CARTESIAN_POINT('Ctrl Pts',(-20.6254181999182,-39.3555442419185,
122.52102025999)) ;
#77041 = CARTESIAN_POINT('Ctrl Pts',(-20.3821947440194,-39.1755551614998,
122.699190275451)) ;
#77042 = CARTESIAN_POINT('Ctrl Pts',(-20.4548438165895,-39.365402109414,122.326007790047)) ;
#77043 = CARTESIAN_POINT('Ctrl Pts',(-20.2457369371644,-39.1854130289952,
122.543178822639)) ;
#77044 = CARTESIAN_POINT('Ctrl Pts',(-20.2506752049278,-39.3753937345313,
122.160957633264)) ;
#77045 = CARTESIAN_POINT('Ctrl Pts',(-20.0824034879034,-39.1954046541126,
122.41113697398)) ;
#77046 = CARTESIAN_POINT('Ctrl Pts',(-20.0221459359516,-39.3853305336396,
122.034581725448)) ;
#77047 = CARTESIAN_POINT('Ctrl Pts',(-19.8995811564876,-39.2053414532208,
122.310034285515)) ;
#77048 = CARTESIAN_POINT('Ctrl Pts',(-19.7739378812756,-39.3953213631969,
121.948989845714)) ;
#77049 = CARTESIAN_POINT('Ctrl Pts',(-19.7010154745598,-39.2153322827782,
122.241558685224)) ;
#77050 = CARTESIAN_POINT('Ctrl Pts',(-19.5137457792874,-39.4053445989101,
121.907963203236)) ;
#77051 = CARTESIAN_POINT('Ctrl Pts',(-19.4928622206853,-39.2253555184914,
122.208735172086)) ;
#77052 = CARTESIAN_POINT('Ctrl Pts',(-19.2537240353443,-39.4152409469393,
121.912457737663)) ;
#77053 = CARTESIAN_POINT('Ctrl Pts',(-19.284844725392,-39.2352518665205,122.212328561207)) ;
#77054 = CARTESIAN_POINT('Ctrl Pts',(-18.9959028450321,-39.4252305094418,
121.961952758508)) ;
#77055 = CARTESIAN_POINT('Ctrl Pts',(-19.0785873514741,-39.245241429023,122.251922433717)) ;
#77056 = CARTESIAN_POINT('Ctrl Pts',(-18.7495601440392,-39.4352708171263,
122.056425100512)) ;
#77057 = CARTESIAN_POINT('Ctrl Pts',(-18.8815126089877,-39.2552817367076,
122.327498082193)) ;
#77058 = CARTESIAN_POINT('Ctrl Pts',(-18.5275396488287,-39.4451131204735,
122.189149904803)) ;
#77059 = CARTESIAN_POINT('Ctrl Pts',(-18.7038944864329,-39.2651240400548,
122.433676503167)) ;
#77060 = CARTESIAN_POINT('Ctrl Pts',(-18.3281491908291,-39.4551368287526,
122.361220908114)) ;
#77061 = CARTESIAN_POINT('Ctrl Pts',(-18.544382291125,-39.2751477483338,122.571330259957)) ;
#77062 = CARTESIAN_POINT('Ctrl Pts',(-18.1083641387951,-39.4683590062203,
122.63041569829)) ;
#77063 = CARTESIAN_POINT('Ctrl Pts',(-18.3685442466138,-39.2883699258015,
122.786691064912)) ;
#77064 = CARTESIAN_POINT('Ctrl Pts',(-17.962805114068,-39.4816515912796,122.952220149213)) ;
#77065 = CARTESIAN_POINT('Ctrl Pts',(-18.2520900201739,-39.3016625108608,
123.0441667538)) ;
#77066 = CARTESIAN_POINT('Ctrl Pts',(-17.9061735339547,-39.4949364472012,
123.296785705765)) ;
#77067 = CARTESIAN_POINT('Ctrl Pts',(-18.2067947639732,-39.3149473667824,
123.319772623799)) ;
#77068 = CARTESIAN_POINT('Ctrl Pts',(-17.9090249686714,-39.504908674374,123.558791097665)) ;
#77069 = CARTESIAN_POINT('Ctrl Pts',(-18.2090712941876,-39.3249195939552,
123.529386330433)) ;
#77070 = CARTESIAN_POINT('Ctrl Pts',(-17.9565864888428,-39.514817290813,123.814831513886)) ;
#77071 = CARTESIAN_POINT('Ctrl Pts',(-18.2471189493616,-39.3348282103942,
123.734216637461)) ;
#77072 = CARTESIAN_POINT('Ctrl Pts',(-18.0492936761103,-39.5248704961967,
124.062190998766)) ;
#77073 = CARTESIAN_POINT('Ctrl Pts',(-18.321283555231,-39.3448814157779,123.93210607372)) ;
#77074 = CARTESIAN_POINT('Ctrl Pts',(-18.1809125137279,-39.5347356299569,
124.285566479039)) ;
#77075 = CARTESIAN_POINT('Ctrl Pts',(-18.4265731937417,-39.3547465495382,
124.110805222555)) ;
#77076 = CARTESIAN_POINT('Ctrl Pts',(-18.4080910891847,-39.5480746875833,
124.552496993398)) ;
#77077 = CARTESIAN_POINT('Ctrl Pts',(-18.6083336756882,-39.3680856071645,
124.324363766932)) ;
#77078 = CARTESIAN_POINT('Ctrl Pts',(-18.7706176278764,-39.5646438749164,
124.802631869013)) ;
#77079 = CARTESIAN_POINT('Ctrl Pts',(-18.8983168389849,-39.3846547944977,
124.524458515266)) ;
#77080 = CARTESIAN_POINT('Ctrl Pts',(-19.1984775012454,-39.5812890147675,
124.914837427725)) ;
#77081 = CARTESIAN_POINT('Ctrl Pts',(-19.2406669700555,-39.4012999343487,
124.614238150144)) ;
#77082 = CARTESIAN_POINT('Ctrl Pts',(-19.5473160626192,-39.5945613172409,
124.91294505077)) ;
#77083 = CARTESIAN_POINT('Ctrl Pts',(-19.5196867817272,-39.4145722368221,
124.6127192198)) ;
#77084 = CARTESIAN_POINT('Ctrl Pts',(-19.8054003622154,-39.6045422806885,
124.866324423739)) ;
#77085 = CARTESIAN_POINT('Ctrl Pts',(-19.7261653890183,-39.4245532002698,
124.575425593905)) ;
#77086 = CARTESIAN_POINT('Ctrl Pts',(-20.0506098850286,-39.6144841127578,
124.776085831138)) ;
#77087 = CARTESIAN_POINT('Ctrl Pts',(-19.9223292887017,-39.4344950323391,
124.503237755022)) ;
#77088 = CARTESIAN_POINT('Ctrl Pts',(-20.3531494019728,-39.6278036819732,
124.600140542003)) ;
#77089 = CARTESIAN_POINT('Ctrl Pts',(-20.1643723390079,-39.4478146015545,
124.362474577121)) ;
#77090 = CARTESIAN_POINT('Ctrl Pts',(-20.6634916789112,-39.644333836906,124.28900205581)) ;
#77091 = CARTESIAN_POINT('Ctrl Pts',(-20.4126378083465,-39.4643447564872,
124.11357553459)) ;
#77092 = CARTESIAN_POINT('Ctrl Pts',(-20.8878880489204,-39.6643555623981,
123.806632140315)) ;
#77093 = CARTESIAN_POINT('Ctrl Pts',(-20.5921614310952,-39.4843664819793,
123.727677884978)) ;
#77094 = CARTESIAN_POINT('Ctrl Pts',(-20.9340458411947,-39.6841669590049,
123.281975948013)) ;
#77095 = CARTESIAN_POINT('Ctrl Pts',(-20.6290900257531,-39.5041778785861,
123.307952866676)) ;
#77096 = CARTESIAN_POINT('Ctrl Pts',(-20.7981256341411,-39.7041522077137,
122.768612564894)) ;
#77097 = CARTESIAN_POINT('Ctrl Pts',(-20.5203568572082,-39.524163127295,122.897261068082)) ;
#77098 = CARTESIAN_POINT('Ctrl Pts',(-20.4961474223464,-39.7240462703497,
122.334473379735)) ;
#77099 = CARTESIAN_POINT('Ctrl Pts',(-20.2787761236903,-39.5440571899309,
122.549947532651)) ;
#77100 = CARTESIAN_POINT('Ctrl Pts',(-20.0638627447035,-39.7439779495233,
122.028277249688)) ;
#77101 = CARTESIAN_POINT('Ctrl Pts',(-19.9329493834132,-39.5639888691045,
122.304988270493)) ;
#77102 = CARTESIAN_POINT('Ctrl Pts',(-19.5521053130839,-39.7639420039953,
121.888081012809)) ;
#77103 = CARTESIAN_POINT('Ctrl Pts',(-19.523543821286,-39.5839529235765,122.192828836387)) ;
#77104 = CARTESIAN_POINT('Ctrl Pts',(-19.0253744539785,-39.7838229057582,
121.930361827019)) ;
#77105 = CARTESIAN_POINT('Ctrl Pts',(-19.1021578729861,-39.6038338253394,
122.226651390255)) ;
#77106 = CARTESIAN_POINT('Ctrl Pts',(-18.5431348409181,-39.8037615673665,
122.150015941266)) ;
#77107 = CARTESIAN_POINT('Ctrl Pts',(-18.7163648705892,-39.6237724869478,
122.402373239355)) ;
#77108 = CARTESIAN_POINT('Ctrl Pts',(-18.1655278032644,-39.8236580926219,
122.520218221283)) ;
#77109 = CARTESIAN_POINT('Ctrl Pts',(-18.4142773121928,-39.6436690122031,
122.698534606389)) ;
#77110 = CARTESIAN_POINT('Ctrl Pts',(-17.9361396476805,-39.8435531310762,
122.996669054424)) ;
#77111 = CARTESIAN_POINT('Ctrl Pts',(-18.2307652509137,-39.6635640506575,
123.079695848156)) ;
#77112 = CARTESIAN_POINT('Ctrl Pts',(-17.8830061324122,-39.8635169543823,
123.524568225154)) ;
#77113 = CARTESIAN_POINT('Ctrl Pts',(-18.1882574093228,-39.6835278739635,
123.502015493419)) ;
#77114 = CARTESIAN_POINT('Ctrl Pts',(-18.012259531642,-39.8833910785114,124.036771136657)) ;
#77115 = CARTESIAN_POINT('Ctrl Pts',(-18.2916598855057,-39.7034019980926,
123.911779438151)) ;
#77116 = CARTESIAN_POINT('Ctrl Pts',(-18.309630845073,-39.9033661542386,124.476606505104)) ;
#77117 = CARTESIAN_POINT('Ctrl Pts',(-18.5295569287949,-39.7233770738199,
124.263648070586)) ;
#77118 = CARTESIAN_POINT('Ctrl Pts',(-18.7392016865205,-39.9233197235952,
124.787593898563)) ;
#77119 = CARTESIAN_POINT('Ctrl Pts',(-18.8732138714757,-39.7433306431764,
124.512438635764)) ;
#77120 = CARTESIAN_POINT('Ctrl Pts',(-19.2458886960608,-39.943157633783,124.933442272074)) ;
#77121 = CARTESIAN_POINT('Ctrl Pts',(-19.278565608068,-39.7631685533643,124.629117598788)) ;
#77122 = CARTESIAN_POINT('Ctrl Pts',(-19.7756254405779,-39.963133462354,124.897944226736)) ;
#77123 = CARTESIAN_POINT('Ctrl Pts',(-19.702355195912,-39.7831443819352,124.600718333619)) ;
#77124 = CARTESIAN_POINT('Ctrl Pts',(-20.2597769713168,-39.9830515070642,
124.683907752949)) ;
#77125 = CARTESIAN_POINT('Ctrl Pts',(-20.0896770292724,-39.8030624266455,
124.429488092088)) ;
#77126 = CARTESIAN_POINT('Ctrl Pts',(-20.6419438141652,-40.0029217528519,
124.319255201544)) ;
#77127 = CARTESIAN_POINT('Ctrl Pts',(-20.3954104744399,-39.8229326724332,
124.137764014872)) ;
#77128 = CARTESIAN_POINT('Ctrl Pts',(-20.8780281937701,-40.0229707559515,
123.841688417879)) ;
#77129 = CARTESIAN_POINT('Ctrl Pts',(-20.584276553681,-39.8429816755327,123.755710427859)) ;
#77130 = CARTESIAN_POINT('Ctrl Pts',(-20.9367938162393,-40.0427499971923,
123.31912856274)) ;
#77131 = CARTESIAN_POINT('Ctrl Pts',(-20.6312875872331,-39.8627609167736,
123.337660188172)) ;
#77132 = CARTESIAN_POINT('Ctrl Pts',(-20.8129964069857,-40.0627800609012,
122.801479468791)) ;
#77133 = CARTESIAN_POINT('Ctrl Pts',(-20.5322475926192,-39.8827909804824,
122.92354173138)) ;
#77134 = CARTESIAN_POINT('Ctrl Pts',(-20.5213204072104,-40.0826623458031,
122.360731282059)) ;
#77135 = CARTESIAN_POINT('Ctrl Pts',(-20.2989045254631,-39.9026732653844,
122.570943408871)) ;
#77136 = CARTESIAN_POINT('Ctrl Pts',(-20.0977276287901,-40.1025446466961,
122.04487225265)) ;
#77137 = CARTESIAN_POINT('Ctrl Pts',(-19.9600279171563,-39.9225555662774,
122.31825773152)) ;
#77138 = CARTESIAN_POINT('Ctrl Pts',(-19.5891047472115,-40.1225277563145,
121.891899364557)) ;
#77139 = CARTESIAN_POINT('Ctrl Pts',(-19.5531287369363,-39.9425386758957,
122.195882009548)) ;
#77140 = CARTESIAN_POINT('Ctrl Pts',(-19.0612514000122,-40.1424181516924,
121.921603035581)) ;
#77141 = CARTESIAN_POINT('Ctrl Pts',(-19.1308454119986,-39.9624290712736,
122.219647817995)) ;
#77142 = CARTESIAN_POINT('Ctrl Pts',(-18.5748477162895,-40.1623149417266,
122.128947492309)) ;
#77143 = CARTESIAN_POINT('Ctrl Pts',(-18.7417230650517,-39.9823258613079,
122.385526589855)) ;
#77144 = CARTESIAN_POINT('Ctrl Pts',(-18.1875342171797,-40.1822319956683,
122.489841093168)) ;
#77145 = CARTESIAN_POINT('Ctrl Pts',(-18.4318742437841,-40.0022429152495,
122.674244288826)) ;
#77146 = CARTESIAN_POINT('Ctrl Pts',(-17.945715845596,-40.2022355438718,122.963405930305)) ;
#77147 = CARTESIAN_POINT('Ctrl Pts',(-18.2384227101736,-40.022246463453,123.05309765344)) ;
#77148 = CARTESIAN_POINT('Ctrl Pts',(-17.8810209348164,-40.2221738375244,
123.489343815256)) ;
#77149 = CARTESIAN_POINT('Ctrl Pts',(-18.1866699625709,-40.0421847571056,
123.473848687239)) ;
#77150 = CARTESIAN_POINT('Ctrl Pts',(-17.9977400536668,-40.2419953249573,
124.003081008366)) ;
#77151 = CARTESIAN_POINT('Ctrl Pts',(-18.2800496556778,-40.0620062445386,
123.884838604969)) ;
#77152 = CARTESIAN_POINT('Ctrl Pts',(-18.2845312147726,-40.2619737179482,
124.449892679413)) ;
#77153 = CARTESIAN_POINT('Ctrl Pts',(-18.5094838885054,-40.0819846375294,
124.242285370891)) ;
#77154 = CARTESIAN_POINT('Ctrl Pts',(-18.7051945464621,-40.2818720995619,
124.77055920549)) ;
#77155 = CARTESIAN_POINT('Ctrl Pts',(-18.8460248106455,-40.1018830191431,
124.498817503231)) ;
#77156 = CARTESIAN_POINT('Ctrl Pts',(-19.1255703487642,-40.2984550302918,
124.902674539554)) ;
#77157 = CARTESIAN_POINT('Ctrl Pts',(-19.1823032071528,-40.118465949873,124.604500927526)) ;
#77158 = CARTESIAN_POINT('Ctrl Pts',(-19.4741295857804,-40.3117292658806,
124.917986772778)) ;
#77159 = CARTESIAN_POINT('Ctrl Pts',(-19.461172160329,-40.1317401854619,124.616752617202)) ;
#77160 = CARTESIAN_POINT('Ctrl Pts',(-19.7358425463497,-40.3217756833368,
124.883469686285)) ;
#77161 = CARTESIAN_POINT('Ctrl Pts',(-19.6705356336101,-40.1417866029181,
124.589137624141)) ;
#77162 = CARTESIAN_POINT('Ctrl Pts',(-19.9826774778491,-40.3316209085561,
124.80588177867)) ;
#77163 = CARTESIAN_POINT('Ctrl Pts',(-19.8680131815929,-40.1516318281373,
124.527058888594)) ;
#77164 = CARTESIAN_POINT('Ctrl Pts',(-20.293982933637,-40.3449558795955,124.645032731984)) ;
#77165 = CARTESIAN_POINT('Ctrl Pts',(-20.117012406976,-40.1649667991767,124.398409704518)) ;
#77166 = CARTESIAN_POINT('Ctrl Pts',(-20.6198884115135,-40.3615387363881,
124.348182656284)) ;
#77167 = CARTESIAN_POINT('Ctrl Pts',(-20.3777873723934,-40.1815496559694,
124.160882593775)) ;
#77168 = CARTESIAN_POINT('Ctrl Pts',(-20.8256972516867,-40.3781817387375,
123.956743051185)) ;
#77169 = CARTESIAN_POINT('Ctrl Pts',(-20.5424028051594,-40.1981926583188,
123.84776904717)) ;
#77170 = CARTESIAN_POINT('Ctrl Pts',(-20.9027340823675,-40.3914254697692,
123.617264907888)) ;
#77171 = CARTESIAN_POINT('Ctrl Pts',(-20.6040438274232,-40.2114363893504,
123.576158441857)) ;
#77172 = CARTESIAN_POINT('Ctrl Pts',(-20.9155780418675,-40.4014798644438,
123.353409333887)) ;
#77173 = CARTESIAN_POINT('Ctrl Pts',(-20.6143139039399,-40.221490784025,123.365079497654)) ;
#77174 = CARTESIAN_POINT('Ctrl Pts',(-20.883436236748,-40.4113209258323,123.096754250343)) ;
#77175 = CARTESIAN_POINT('Ctrl Pts',(-20.5885990123171,-40.2313318454136,
123.159754036855)) ;
#77176 = CARTESIAN_POINT('Ctrl Pts',(-20.8057493250627,-40.4213871501888,
122.843935791891)) ;
#77177 = CARTESIAN_POINT('Ctrl Pts',(-20.5264471820404,-40.2413980697701,
122.957500455723)) ;
#77178 = CARTESIAN_POINT('Ctrl Pts',(-20.6874567828828,-40.4312677631085,
122.61274782881)) ;
#77179 = CARTESIAN_POINT('Ctrl Pts',(-20.431811178883,-40.2512786826897,122.77255090532)) ;
#77180 = CARTESIAN_POINT('Ctrl Pts',(-20.5294818312778,-40.4412610562681,
122.403016184091)) ;
#77181 = CARTESIAN_POINT('Ctrl Pts',(-20.3054294355456,-40.2612719758493,
122.604767012198)) ;
#77182 = CARTESIAN_POINT('Ctrl Pts',(-20.3383061145161,-40.4512120644917,
122.224524733041)) ;
#77183 = CARTESIAN_POINT('Ctrl Pts',(-20.1524873435744,-40.271222984073,122.461975496637)) ;
#77184 = CARTESIAN_POINT('Ctrl Pts',(-20.1168471521159,-40.4612605788537,
122.08075282336)) ;
#77185 = CARTESIAN_POINT('Ctrl Pts',(-19.9753190159199,-40.281271498435,122.34695989764)) ;
#77186 = CARTESIAN_POINT('Ctrl Pts',(-19.8788615309388,-40.4711020849164,
121.979450513816)) ;
#77187 = CARTESIAN_POINT('Ctrl Pts',(-19.7849296059222,-40.2911130044976,
122.265920106906)) ;
#77188 = CARTESIAN_POINT('Ctrl Pts',(-19.6234056665273,-40.4810877375461,
121.919608246961)) ;
#77189 = CARTESIAN_POINT('Ctrl Pts',(-19.5805644621411,-40.3010986571273,
122.218048512511)) ;
#77190 = CARTESIAN_POINT('Ctrl Pts',(-19.3625879444261,-40.491026746391,121.904994592933)) ;
#77191 = CARTESIAN_POINT('Ctrl Pts',(-19.3719102147239,-40.3110376659722,
122.206359844841)) ;
#77192 = CARTESIAN_POINT('Ctrl Pts',(-19.1006071741676,-40.501067671684,121.9362672369)) ;
#77193 = CARTESIAN_POINT('Ctrl Pts',(-19.1623259175616,-40.3210785912652,
122.231380198729)) ;
#77194 = CARTESIAN_POINT('Ctrl Pts',(-18.8517347176432,-40.5109579934389,
122.011275192516)) ;
#77195 = CARTESIAN_POINT('Ctrl Pts',(-18.9632286807816,-40.3309689130201,
122.291388701103)) ;
#77196 = CARTESIAN_POINT('Ctrl Pts',(-18.6170528303979,-40.5209539667723,
122.129240595586)) ;
#77197 = CARTESIAN_POINT('Ctrl Pts',(-18.775484242593,-40.3409648863536,122.385763008815)) ;
#77198 = CARTESIAN_POINT('Ctrl Pts',(-18.4077408550666,-40.5308853663543,
122.285152304455)) ;
#77199 = CARTESIAN_POINT('Ctrl Pts',(-18.6080360869343,-40.3508962859356,
122.510494122467)) ;
#77200 = CARTESIAN_POINT('Ctrl Pts',(-18.2270702113385,-40.5408909068314,
122.476201697445)) ;
#77201 = CARTESIAN_POINT('Ctrl Pts',(-18.463501244713,-40.3609018264127,122.663335132753)) ;
#77202 = CARTESIAN_POINT('Ctrl Pts',(-18.0823350470019,-40.5509238907627,
122.696568451473)) ;
#77203 = CARTESIAN_POINT('Ctrl Pts',(-18.3477150174073,-40.370934810344,122.839629750178)) ;
#77204 = CARTESIAN_POINT('Ctrl Pts',(-17.9794720036772,-40.5607795215895,
122.934283776529)) ;
#77205 = CARTESIAN_POINT('Ctrl Pts',(-18.2654267150485,-40.3807904411708,
123.029802727258)) ;
#77206 = CARTESIAN_POINT('Ctrl Pts',(-17.9182550888982,-40.5707789237827,
123.189781090314)) ;
#77207 = CARTESIAN_POINT('Ctrl Pts',(-18.2164553726085,-40.390789843364,123.234201028577)) ;
#77208 = CARTESIAN_POINT('Ctrl Pts',(-17.9021932201745,-40.5806733931438,
123.449349378983)) ;
#77209 = CARTESIAN_POINT('Ctrl Pts',(-18.2036080982215,-40.400684312725,123.441855585745)) ;
#77210 = CARTESIAN_POINT('Ctrl Pts',(-17.9320113008533,-40.590736507308,123.712065167668)) ;
#77211 = CARTESIAN_POINT('Ctrl Pts',(-18.2274647737821,-40.4107474268893,
123.65202799485)) ;
#77212 = CARTESIAN_POINT('Ctrl Pts',(-18.0050786319795,-40.6005761530244,
123.960147159089)) ;
#77213 = CARTESIAN_POINT('Ctrl Pts',(-18.2859206557208,-40.4205870726056,
123.850492648776)) ;
#77214 = CARTESIAN_POINT('Ctrl Pts',(-18.1223872400541,-40.6106393205801,
124.197113300206)) ;
#77215 = CARTESIAN_POINT('Ctrl Pts',(-18.3797695138113,-40.4306502401614,
124.04006462666)) ;
#77216 = CARTESIAN_POINT('Ctrl Pts',(-18.276645110429,-40.620533576375,124.406457589645)) ;
#77217 = CARTESIAN_POINT('Ctrl Pts',(-18.5031774204624,-40.4405444959563,
124.207538542366)) ;
#77218 = CARTESIAN_POINT('Ctrl Pts',(-18.4652776966271,-40.6304753548347,
124.587171422817)) ;
#77219 = CARTESIAN_POINT('Ctrl Pts',(-18.6540848187046,-40.4504862744159,
124.352107914679)) ;
#77220 = CARTESIAN_POINT('Ctrl Pts',(-18.6837565652189,-40.6404780476649,
124.733392656267)) ;
#77221 = CARTESIAN_POINT('Ctrl Pts',(-18.8288690428585,-40.4604889672461,
124.469083093928)) ;
#77222 = CARTESIAN_POINT('Ctrl Pts',(-18.9251772147338,-40.6505120696187,
124.839403238368)) ;
#77223 = CARTESIAN_POINT('Ctrl Pts',(-19.0220064463768,-40.4705229891999,
124.553889578956)) ;
#77224 = CARTESIAN_POINT('Ctrl Pts',(-19.1765096236115,-40.6603598607077,
124.901116406768)) ;
#77225 = CARTESIAN_POINT('Ctrl Pts',(-19.2230724433567,-40.480370780289,124.603257935975)) ;
#77226 = CARTESIAN_POINT('Ctrl Pts',(-19.4381766703667,-40.6703413852567,
124.9190603837)) ;
#77227 = CARTESIAN_POINT('Ctrl Pts',(-19.4324060828598,-40.490352304838,124.617611036855)) ;
#77228 = CARTESIAN_POINT('Ctrl Pts',(-19.6981676204885,-40.6802906087477,
124.891345054744)) ;
#77229 = CARTESIAN_POINT('Ctrl Pts',(-19.6403984071711,-40.5003015283289,
124.595436730586)) ;
#77230 = CARTESIAN_POINT('Ctrl Pts',(-19.9507242764869,-40.6902882649642,
124.818869487546)) ;
#77231 = CARTESIAN_POINT('Ctrl Pts',(-19.8424430882566,-40.5102991845455,
124.537454338467)) ;
#77232 = CARTESIAN_POINT('Ctrl Pts',(-20.1876076662256,-40.7003284780193,
124.702714148728)) ;
#77233 = CARTESIAN_POINT('Ctrl Pts',(-20.0319489184708,-40.5203393976006,
124.444528159668)) ;
#77234 = CARTESIAN_POINT('Ctrl Pts',(-20.3965794743813,-40.7101565252955,
124.550916691097)) ;
#77235 = CARTESIAN_POINT('Ctrl Pts',(-20.1991246693014,-40.5301674448768,
124.323088910881)) ;
#77236 = CARTESIAN_POINT('Ctrl Pts',(-20.5804267072891,-40.7202108723279,
124.361171005095)) ;
#77237 = CARTESIAN_POINT('Ctrl Pts',(-20.346201090862,-40.5402217919092,124.171290919494)) ;
#77238 = CARTESIAN_POINT('Ctrl Pts',(-20.7265146725053,-40.7301520086565,
124.144583500083)) ;
#77239 = CARTESIAN_POINT('Ctrl Pts',(-20.4630696218111,-40.5501629282377,
123.998019996052)) ;
#77240 = CARTESIAN_POINT('Ctrl Pts',(-20.8331181684414,-40.7400562417362,
123.907137322054)) ;
#77241 = CARTESIAN_POINT('Ctrl Pts',(-20.5483504786271,-40.5600671613174,
123.808062650785)) ;
#77242 = CARTESIAN_POINT('Ctrl Pts',(-20.8976239887769,-40.7501029385798,
123.651145500457)) ;
#77243 = CARTESIAN_POINT('Ctrl Pts',(-20.5999532571857,-40.5701138581611,
123.603268634691)) ;
#77244 = CARTESIAN_POINT('Ctrl Pts',(-20.9166549330674,-40.7599984898601,
123.391755647877)) ;
#77245 = CARTESIAN_POINT('Ctrl Pts',(-20.6151760608745,-40.5800094094413,
123.395757077431)) ;
#77246 = CARTESIAN_POINT('Ctrl Pts',(-20.8899239296394,-40.7700605676996,
123.128727559475)) ;
#77247 = CARTESIAN_POINT('Ctrl Pts',(-20.5937893272539,-40.5900714872808,
123.18533465587)) ;
#77248 = CARTESIAN_POINT('Ctrl Pts',(-20.8196225926542,-40.7799032767956,
122.879777795685)) ;
#77249 = CARTESIAN_POINT('Ctrl Pts',(-20.5375466154367,-40.5999141963769,
122.98617602963)) ;
#77250 = CARTESIAN_POINT('Ctrl Pts',(-20.7060594583862,-40.7898940090341,
122.643100332468)) ;
#77251 = CARTESIAN_POINT('Ctrl Pts',(-20.4466945356706,-40.6099049286153,
122.796834968904)) ;
#77252 = CARTESIAN_POINT('Ctrl Pts',(-20.5540244826181,-40.7998220342628,
122.431061345429)) ;
#77253 = CARTESIAN_POINT('Ctrl Pts',(-20.3250653085112,-40.6198329538441,
122.627205154481)) ;
#77254 = CARTESIAN_POINT('Ctrl Pts',(-20.3666704075029,-40.8098101809134,
122.247223536426)) ;
#77255 = CARTESIAN_POINT('Ctrl Pts',(-20.1751809297172,-40.6298211004947,
122.480136252607)) ;
#77256 = CARTESIAN_POINT('Ctrl Pts',(-20.1490005901118,-40.8198451987533,
122.098346117537)) ;
#77257 = CARTESIAN_POINT('Ctrl Pts',(-20.0010440055564,-40.6398561183346,
122.361035777316)) ;
#77258 = CARTESIAN_POINT('Ctrl Pts',(-19.9129860528095,-40.8297099958586,
121.991128079593)) ;
#77259 = CARTESIAN_POINT('Ctrl Pts',(-19.8122322768596,-40.6497209154398,
122.275263239916)) ;
#77260 = CARTESIAN_POINT('Ctrl Pts',(-19.6596753422192,-40.8396707282147,
121.92514335029)) ;
#77261 = CARTESIAN_POINT('Ctrl Pts',(-19.6095835667024,-40.6596816477959,
122.222477106731)) ;
#77262 = CARTESIAN_POINT('Ctrl Pts',(-19.3968323127535,-40.8497041906117,
121.90443177847)) ;
#77263 = CARTESIAN_POINT('Ctrl Pts',(-19.3993089374676,-40.6697151101929,
122.205909546887)) ;
#77264 = CARTESIAN_POINT('Ctrl Pts',(-19.1381719931568,-40.8595897248231,
121.928871855585)) ;
#77265 = CARTESIAN_POINT('Ctrl Pts',(-19.1923814686727,-40.6796006444043,
122.225463173289)) ;
#77266 = CARTESIAN_POINT('Ctrl Pts',(-18.8832051234587,-40.8696545655031,
121.999096372932)) ;
#77267 = CARTESIAN_POINT('Ctrl Pts',(-18.9884082093164,-40.6896654850843,
122.281644418991)) ;
#77268 = CARTESIAN_POINT('Ctrl Pts',(-18.6493502438583,-40.8795026972319,
122.110000505727)) ;
#77269 = CARTESIAN_POINT('Ctrl Pts',(-18.8013257528878,-40.6995136168132,
122.370368822003)) ;
#77270 = CARTESIAN_POINT('Ctrl Pts',(-18.4340900375978,-40.8895301942221,
122.261979815456)) ;
#77271 = CARTESIAN_POINT('Ctrl Pts',(-18.6291184182037,-40.7095411138033,
122.49195350058)) ;
#77272 = CARTESIAN_POINT('Ctrl Pts',(-18.2489515311722,-40.8995586462672,
122.449550692962)) ;
#77273 = CARTESIAN_POINT('Ctrl Pts',(-18.4810087252179,-40.7195695658484,
122.642011378484)) ;
#77274 = CARTESIAN_POINT('Ctrl Pts',(-18.1015397640265,-40.9094039128313,
122.66215418172)) ;
#77275 = CARTESIAN_POINT('Ctrl Pts',(-18.3630810732943,-40.7294148324125,
122.812094300653)) ;
#77276 = CARTESIAN_POINT('Ctrl Pts',(-17.9910357649292,-40.9193945857722,
122.9003183125)) ;
#77277 = CARTESIAN_POINT('Ctrl Pts',(-18.2746791939818,-40.7394055053534,
123.002626045039)) ;
#77278 = CARTESIAN_POINT('Ctrl Pts',(-17.923815012575,-40.9294324678607,123.155391667996)) ;
#77279 = CARTESIAN_POINT('Ctrl Pts',(-18.2209040160254,-40.7494433874419,
123.206685215275)) ;
#77280 = CARTESIAN_POINT('Ctrl Pts',(-17.9018757959,-40.9392768383003,123.413170064838)) ;
#77281 = CARTESIAN_POINT('Ctrl Pts',(-18.2033541255179,-40.7592877578816,
123.41290711647)) ;
#77282 = CARTESIAN_POINT('Ctrl Pts',(-17.9248387221279,-40.9492616656957,
123.674518463685)) ;
#77283 = CARTESIAN_POINT('Ctrl Pts',(-18.2217257460994,-40.7692725852769,
123.621985522676)) ;
#77284 = CARTESIAN_POINT('Ctrl Pts',(-17.9924288979243,-40.959201111101,123.926859520028)) ;
#77285 = CARTESIAN_POINT('Ctrl Pts',(-18.2757990048026,-40.7792120306822,
123.823857616306)) ;
#77286 = CARTESIAN_POINT('Ctrl Pts',(-18.1039644976458,-40.9692411153869,
124.165936540815)) ;
#77287 = CARTESIAN_POINT('Ctrl Pts',(-18.3650287084099,-40.7892520349681,
124.015118795446)) ;
#77288 = CARTESIAN_POINT('Ctrl Pts',(-18.2528993474394,-40.9791282245725,
124.378873025774)) ;
#77289 = CARTESIAN_POINT('Ctrl Pts',(-18.4841771835395,-40.7991391441538,
124.185466648641)) ;
#77290 = CARTESIAN_POINT('Ctrl Pts',(-18.4383623409316,-40.989128284475,124.564995129776)) ;
#77291 = CARTESIAN_POINT('Ctrl Pts',(-18.6325483359507,-40.8091392040562,
124.334363415602)) ;
#77292 = CARTESIAN_POINT('Ctrl Pts',(-18.6514890496994,-40.9990457003897,
124.715068772914)) ;
#77293 = CARTESIAN_POINT('Ctrl Pts',(-18.8030498870585,-40.8190566199709,
124.454421071669)) ;
#77294 = CARTESIAN_POINT('Ctrl Pts',(-18.8904730960072,-41.0090925151305,
124.827199842397)) ;
#77295 = CARTESIAN_POINT('Ctrl Pts',(-18.9942377675479,-40.8291034347117,
124.54412495723)) ;
#77296 = CARTESIAN_POINT('Ctrl Pts',(-19.1409580664959,-41.0189679923272,
124.89523536818)) ;
#77297 = CARTESIAN_POINT('Ctrl Pts',(-19.1946252220464,-40.8389789119084,
124.59855210373)) ;
#77298 = CARTESIAN_POINT('Ctrl Pts',(-19.4040773768786,-41.0290240880484,
124.919312459414)) ;
#77299 = CARTESIAN_POINT('Ctrl Pts',(-19.4051209742534,-40.8490350076296,
124.617812738242)) ;
#77300 = CARTESIAN_POINT('Ctrl Pts',(-19.663216707279,-41.0389172500634,124.897783110562)) ;
#77301 = CARTESIAN_POINT('Ctrl Pts',(-19.612431616485,-40.8589281696447,124.600588287946)) ;
#77302 = CARTESIAN_POINT('Ctrl Pts',(-19.9189173138886,-41.0489794860861,
124.830551760959)) ;
#77303 = CARTESIAN_POINT('Ctrl Pts',(-19.816992096317,-40.8689904056673,124.546802153709)) ;
#77304 = CARTESIAN_POINT('Ctrl Pts',(-20.1539134835789,-41.058823951715,124.7223429247)) ;
#77305 = CARTESIAN_POINT('Ctrl Pts',(-20.0049876465229,-40.8788348712962,
124.460234605023)) ;
#77306 = CARTESIAN_POINT('Ctrl Pts',(-20.3695735131552,-41.0687840444191,
124.574029278999)) ;
#77307 = CARTESIAN_POINT('Ctrl Pts',(-20.1775149195478,-40.8887949640004,
124.34158324237)) ;
#77308 = CARTESIAN_POINT('Ctrl Pts',(-20.5573002807769,-41.0788223334002,
124.388718288862)) ;
#77309 = CARTESIAN_POINT('Ctrl Pts',(-20.3276957826536,-40.8988332529814,
124.193333707095)) ;
#77310 = CARTESIAN_POINT('Ctrl Pts',(-20.7079273847676,-41.0886956565064,
124.177407956279)) ;
#77311 = CARTESIAN_POINT('Ctrl Pts',(-20.4481962954603,-40.9087065760876,
124.024285712482)) ;
#77312 = CARTESIAN_POINT('Ctrl Pts',(-20.821719687652,-41.0987688405915,123.938460528955)) ;
#77313 = CARTESIAN_POINT('Ctrl Pts',(-20.5392295466057,-40.9187797601727,
123.833127110571)) ;
#77314 = CARTESIAN_POINT('Ctrl Pts',(-20.8908771121847,-41.1085893528794,
123.689767340511)) ;
#77315 = CARTESIAN_POINT('Ctrl Pts',(-20.5945544458289,-40.9286002724607,
123.634173561183)) ;
#77316 = CARTESIAN_POINT('Ctrl Pts',(-20.9166985131135,-41.1186673489952,
123.426252975595)) ;
#77317 = CARTESIAN_POINT('Ctrl Pts',(-20.615210932042,-40.9386782685765,123.423361632516)) ;
#77318 = CARTESIAN_POINT('Ctrl Pts',(-20.8968766071767,-41.1285214239785,
123.16799763283)) ;
#77319 = CARTESIAN_POINT('Ctrl Pts',(-20.5993528292853,-40.9485323435597,
123.21675844281)) ;
#77320 = CARTESIAN_POINT('Ctrl Pts',(-20.8314512990884,-41.1385853055622,
122.911802236395)) ;
#77321 = CARTESIAN_POINT('Ctrl Pts',(-20.5470119442779,-40.9585962251434,
123.011802002189)) ;
#77322 = CARTESIAN_POINT('Ctrl Pts',(-20.7244059190005,-41.1484687315359,
122.675111707048)) ;
#77323 = CARTESIAN_POINT('Ctrl Pts',(-20.461375448032,-40.9684796511172,122.822450609287)) ;
#77324 = CARTESIAN_POINT('Ctrl Pts',(-20.5765499861108,-41.158469335457,122.457899543899)) ;
#77325 = CARTESIAN_POINT('Ctrl Pts',(-20.3430903518895,-40.9784802550382,
122.648681253808)) ;
#77326 = CARTESIAN_POINT('Ctrl Pts',(-20.3947593960527,-41.1683891197948,
122.270998373861)) ;
#77327 = CARTESIAN_POINT('Ctrl Pts',(-20.1976579864223,-40.9884000393761,
122.499161080854)) ;
#77328 = CARTESIAN_POINT('Ctrl Pts',(-20.1805968422417,-41.1784364701517,
122.116644489957)) ;
#77329 = CARTESIAN_POINT('Ctrl Pts',(-20.0263275114058,-40.998447389733,122.37567824904)) ;
#77330 = CARTESIAN_POINT('Ctrl Pts',(-19.9469565781319,-41.188313812386,122.003445575684)) ;
#77331 = CARTESIAN_POINT('Ctrl Pts',(-19.8394159581554,-41.0083247319672,
122.285119878453)) ;
#77332 = CARTESIAN_POINT('Ctrl Pts',(-19.6924393110827,-41.1983836934606,
121.931197405245)) ;
#77333 = CARTESIAN_POINT('Ctrl Pts',(-19.6358017081943,-41.0183946130419,
122.227321635127)) ;
#77334 = CARTESIAN_POINT('Ctrl Pts',(-19.4354489668102,-41.2082133986623,
121.904602386761)) ;
#77335 = CARTESIAN_POINT('Ctrl Pts',(-19.430210627212,-41.0282243182436,122.206046078659)) ;
#77336 = CARTESIAN_POINT('Ctrl Pts',(-19.1716002965665,-41.2182800598287,
121.92311830147)) ;
#77337 = CARTESIAN_POINT('Ctrl Pts',(-19.2191313901848,-41.03829097941,122.220859076658)) ;
#77338 = CARTESIAN_POINT('Ctrl Pts',(-18.9194385507668,-41.228170281696,121.986221032393)) ;
#77339 = CARTESIAN_POINT('Ctrl Pts',(-19.0174028771925,-41.0481812012773,
122.271341336615)) ;
#77340 = CARTESIAN_POINT('Ctrl Pts',(-18.6794263981933,-41.2381624578062,
122.092694865088)) ;
#77341 = CARTESIAN_POINT('Ctrl Pts',(-18.825393369095,-41.0581733773874,122.356520462696)) ;
#77342 = CARTESIAN_POINT('Ctrl Pts',(-18.4623191157902,-41.2481252879188,
122.239006352242)) ;
#77343 = CARTESIAN_POINT('Ctrl Pts',(-18.6517079609517,-41.0681362075001,
122.473569619426)) ;
#77344 = CARTESIAN_POINT('Ctrl Pts',(-18.2745423236798,-41.2580295003191,
122.419265967133)) ;
#77345 = CARTESIAN_POINT('Ctrl Pts',(-18.5014870946545,-41.0780404199004,
122.617776816636)) ;
#77346 = CARTESIAN_POINT('Ctrl Pts',(-18.118713573879,-41.268090214407,122.632804079634)) ;
#77347 = CARTESIAN_POINT('Ctrl Pts',(-18.3768240055462,-41.0881011339882,
122.788607593364)) ;
#77348 = CARTESIAN_POINT('Ctrl Pts',(-18.0045368874471,-41.2779297173898,
122.864848022262)) ;
#77349 = CARTESIAN_POINT('Ctrl Pts',(-18.2854831831512,-41.097940636971,122.974241688555)) ;
#77350 = CARTESIAN_POINT('Ctrl Pts',(-17.9304874745659,-41.2879958559562,
123.118755220542)) ;
#77351 = CARTESIAN_POINT('Ctrl Pts',(-18.2262435039461,-41.1080067755374,
123.177367738535)) ;
#77352 = CARTESIAN_POINT('Ctrl Pts',(-17.9022632242414,-41.2978783704422,
123.376958924442)) ;
#77353 = CARTESIAN_POINT('Ctrl Pts',(-18.2036641643928,-41.1178892900235,
123.383929797729)) ;
#77354 = CARTESIAN_POINT('Ctrl Pts',(-17.9189692033118,-41.3078706697977,
123.638973965505)) ;
#77355 = CARTESIAN_POINT('Ctrl Pts',(-18.2170287674167,-41.127881589379,123.593541666519)) ;
#77356 = CARTESIAN_POINT('Ctrl Pts',(-17.9806273076424,-41.3178237367511,
123.893199304598)) ;
#77357 = CARTESIAN_POINT('Ctrl Pts',(-18.2663549772125,-41.1378346563324,
123.796921581805)) ;
#77358 = CARTESIAN_POINT('Ctrl Pts',(-18.0864278199348,-41.3278584449564,
124.134724121219)) ;
#77359 = CARTESIAN_POINT('Ctrl Pts',(-18.3509952924776,-41.1478693645376,
123.990141608418)) ;
#77360 = CARTESIAN_POINT('Ctrl Pts',(-18.230286207724,-41.3377466658605,124.351140926616)) ;
#77361 = CARTESIAN_POINT('Ctrl Pts',(-18.4660813609323,-41.1577575854418,
124.163274450491)) ;
#77362 = CARTESIAN_POINT('Ctrl Pts',(-18.411128139942,-41.347741088891,124.541587743778)) ;
#77363 = CARTESIAN_POINT('Ctrl Pts',(-18.6107545669795,-41.1677520084722,
124.31563199722)) ;
#77364 = CARTESIAN_POINT('Ctrl Pts',(-18.6213277143798,-41.3576864283371,
124.696900401369)) ;
#77365 = CARTESIAN_POINT('Ctrl Pts',(-18.7789136746949,-41.1776973479184,
124.439882070568)) ;
#77366 = CARTESIAN_POINT('Ctrl Pts',(-18.8551198560188,-41.3676337729485,
124.813866561851)) ;
#77367 = CARTESIAN_POINT('Ctrl Pts',(-18.9659467888428,-41.1876446925297,
124.533455168981)) ;
#77368 = CARTESIAN_POINT('Ctrl Pts',(-19.1082663812301,-41.3776816683594,
124.888923688578)) ;
#77369 = CARTESIAN_POINT('Ctrl Pts',(-19.1684641030672,-41.1976925879407,
124.593501257939)) ;
#77370 = CARTESIAN_POINT('Ctrl Pts',(-19.365357688919,-41.3875293138388,124.918508593986)) ;
#77371 = CARTESIAN_POINT('Ctrl Pts',(-19.374135991281,-41.2075402334201,124.617169451887)) ;
#77372 = CARTESIAN_POINT('Ctrl Pts',(-19.6267063239591,-41.3974910277528,
124.903644555677)) ;
#77373 = CARTESIAN_POINT('Ctrl Pts',(-19.5832145704097,-41.2175019473341,
124.605278846852)) ;
#77374 = CARTESIAN_POINT('Ctrl Pts',(-19.8831669773534,-41.4075196520438,
124.842893155748)) ;
#77375 = CARTESIAN_POINT('Ctrl Pts',(-19.7883832884811,-41.227530571625,124.556678216363)) ;
#77376 = CARTESIAN_POINT('Ctrl Pts',(-20.1223364380346,-41.4174300127005,
124.739853154609)) ;
#77377 = CARTESIAN_POINT('Ctrl Pts',(-19.9797184280272,-41.2374409322817,
124.474246990679)) ;
#77378 = CARTESIAN_POINT('Ctrl Pts',(-20.3409126899482,-41.4273647112738,
124.597063389215)) ;
#77379 = CARTESIAN_POINT('Ctrl Pts',(-20.1545793763586,-41.247375630855,124.360016063863)) ;
#77380 = CARTESIAN_POINT('Ctrl Pts',(-20.5332339905812,-41.437406536128,124.416390285372)) ;
#77381 = CARTESIAN_POINT('Ctrl Pts',(-20.3084369714252,-41.2574174557092,
124.215477948896)) ;
#77382 = CARTESIAN_POINT('Ctrl Pts',(-20.6889942203536,-41.4472911098724,
124.208484214608)) ;
#77383 = CARTESIAN_POINT('Ctrl Pts',(-20.4330452122912,-41.2673020294536,
124.049154187181)) ;
#77384 = CARTESIAN_POINT('Ctrl Pts',(-20.8079337347241,-41.4572929592355,
123.974137087489)) ;
#77385 = CARTESIAN_POINT('Ctrl Pts',(-20.5281974668487,-41.2773038788168,
123.861676944645)) ;
#77386 = CARTESIAN_POINT('Ctrl Pts',(-20.8839492757702,-41.4672122608096,
123.724761737212)) ;
#77387 = CARTESIAN_POINT('Ctrl Pts',(-20.5890105118696,-41.2872231803909,
123.662177488703)) ;
#77388 = CARTESIAN_POINT('Ctrl Pts',(-20.9159063784772,-41.4772563691549,
123.462776779807)) ;
#77389 = CARTESIAN_POINT('Ctrl Pts',(-20.6145770325687,-41.2972672887361,
123.452589454882)) ;
#77390 = CARTESIAN_POINT('Ctrl Pts',(-20.9021882405905,-41.4871407925971,
123.20337470008)) ;
#77391 = CARTESIAN_POINT('Ctrl Pts',(-20.6036034091239,-41.3071517121784,
123.245068567429)) ;
#77392 = CARTESIAN_POINT('Ctrl Pts',(-20.8434269168873,-41.4971571545066,
122.946788139657)) ;
#77393 = CARTESIAN_POINT('Ctrl Pts',(-20.5565953052322,-41.3171680740879,
123.039799101921)) ;
#77394 = CARTESIAN_POINT('Ctrl Pts',(-20.7401692463216,-41.507193810012,122.704103736662)) ;
#77395 = CARTESIAN_POINT('Ctrl Pts',(-20.4739898809288,-41.3272047295932,
122.845651168886)) ;
#77396 = CARTESIAN_POINT('Ctrl Pts',(-20.5998669969204,-41.5170239402013,
122.487161714468)) ;
#77397 = CARTESIAN_POINT('Ctrl Pts',(-20.3617495279934,-41.3370348597826,
122.672097974141)) ;
#77398 = CARTESIAN_POINT('Ctrl Pts',(-20.4197517581222,-41.5270999932912,
122.293140547017)) ;
#77399 = CARTESIAN_POINT('Ctrl Pts',(-20.2176578409717,-41.3471109128724,
122.516880105175)) ;
#77400 = CARTESIAN_POINT('Ctrl Pts',(-20.2133740001991,-41.536952222477,122.136713686601)) ;
#77401 = CARTESIAN_POINT('Ctrl Pts',(-20.0525570462563,-41.3569631420582,
122.391738386618)) ;
#77402 = CARTESIAN_POINT('Ctrl Pts',(-19.9779921556305,-41.5470254302763,
122.015693380282)) ;
#77403 = CARTESIAN_POINT('Ctrl Pts',(-19.8642517827859,-41.3670363498575,
122.294921027755)) ;
#77404 = CARTESIAN_POINT('Ctrl Pts',(-19.7309096530858,-41.5568669416277,
121.939233606191)) ;
#77405 = CARTESIAN_POINT('Ctrl Pts',(-19.6665870925325,-41.3768778612089,
122.233752494711)) ;
#77406 = CARTESIAN_POINT('Ctrl Pts',(-19.4713417220691,-41.5668278796652,
121.905469506119)) ;
#77407 = CARTESIAN_POINT('Ctrl Pts',(-19.4589332355636,-41.3868387992465,
122.206739977289)) ;
#77408 = CARTESIAN_POINT('Ctrl Pts',(-19.2078592032228,-41.5768657415902,
121.91790709068)) ;
#77409 = CARTESIAN_POINT('Ctrl Pts',(-19.2481470590052,-41.3968766611714,
122.216688878807)) ;
#77410 = CARTESIAN_POINT('Ctrl Pts',(-18.9545877189853,-41.5867399275872,
121.974495320647)) ;
#77411 = CARTESIAN_POINT('Ctrl Pts',(-19.0455303831215,-41.4067508471685,
122.261958038974)) ;
#77412 = CARTESIAN_POINT('Ctrl Pts',(-18.7103088483372,-41.5968100871651,
122.076174219081)) ;
#77413 = CARTESIAN_POINT('Ctrl Pts',(-18.8501065384056,-41.4168210067464,
122.343300089057)) ;
#77414 = CARTESIAN_POINT('Ctrl Pts',(-18.4925316286567,-41.606641834591,122.215244290438)) ;
#77415 = CARTESIAN_POINT('Ctrl Pts',(-18.675884926045,-41.4266527541722,122.454554491954)) ;
#77416 = CARTESIAN_POINT('Ctrl Pts',(-18.2978201733215,-41.6166779146623,
122.393114575324)) ;
#77417 = CARTESIAN_POINT('Ctrl Pts',(-18.5201147167768,-41.4366888342435,
122.596849707631)) ;
#77418 = CARTESIAN_POINT('Ctrl Pts',(-18.1377661291007,-41.6266949615148,
122.602121409373)) ;
#77419 = CARTESIAN_POINT('Ctrl Pts',(-18.3920704452954,-41.446705881096,122.764054368868)) ;
#77420 = CARTESIAN_POINT('Ctrl Pts',(-18.0176363963573,-41.6365772196814,
122.832366722348)) ;
#77421 = CARTESIAN_POINT('Ctrl Pts',(-18.2959657432194,-41.4565881392626,
122.948249322725)) ;
#77422 = CARTESIAN_POINT('Ctrl Pts',(-17.9381960768741,-41.6465649024777,
123.082493245772)) ;
#77423 = CARTESIAN_POINT('Ctrl Pts',(-18.2324121300775,-41.466575822059,123.148349941612)) ;
#77424 = CARTESIAN_POINT('Ctrl Pts',(-17.9033168941864,-41.6565115591945,
123.341584277104)) ;
#77425 = CARTESIAN_POINT('Ctrl Pts',(-18.2045073339234,-41.4765224787757,
123.355622202973)) ;
#77426 = CARTESIAN_POINT('Ctrl Pts',(-17.9143411682113,-41.6665686172746,
123.605613842763)) ;
#77427 = CARTESIAN_POINT('Ctrl Pts',(-18.2133253006572,-41.4865795368559,
123.56684609059)) ;
#77428 = CARTESIAN_POINT('Ctrl Pts',(-17.9693550454836,-41.6763867968241,
123.857706729687)) ;
#77429 = CARTESIAN_POINT('Ctrl Pts',(-18.2573346904217,-41.4963977164053,
123.768519739504)) ;
#77430 = CARTESIAN_POINT('Ctrl Pts',(-18.0688075004659,-41.6864227312631,
124.101962974005)) ;
#77431 = CARTESIAN_POINT('Ctrl Pts',(-18.3368951443602,-41.5064336508443,
123.963925444336)) ;
#77432 = CARTESIAN_POINT('Ctrl Pts',(-18.2096507194061,-41.6964473856921,
124.324600663838)) ;
#77433 = CARTESIAN_POINT('Ctrl Pts',(-18.4495684418936,-41.5164583052733,
124.142036426713)) ;
#77434 = CARTESIAN_POINT('Ctrl Pts',(-18.3835301011871,-41.7062994052716,
124.516428432838)) ;
#77435 = CARTESIAN_POINT('Ctrl Pts',(-18.5886701972633,-41.5263103248528,
124.295499139978)) ;
#77436 = CARTESIAN_POINT('Ctrl Pts',(-18.5906854587567,-41.7162903189865,
124.677682956485)) ;
#77437 = CARTESIAN_POINT('Ctrl Pts',(-18.7543933282232,-41.5363012385678,
124.424504019859)) ;
#77438 = CARTESIAN_POINT('Ctrl Pts',(-18.8209758180989,-41.7262083078261,
124.799801737025)) ;
#77439 = CARTESIAN_POINT('Ctrl Pts',(-18.9386244015868,-41.5462192274073,
124.522200358764)) ;
#77440 = CARTESIAN_POINT('Ctrl Pts',(-19.0716562721094,-41.7362364185569,
124.881015168281)) ;
#77441 = CARTESIAN_POINT('Ctrl Pts',(-19.1391682539512,-41.5562473381381,
124.587172769983)) ;
#77442 = CARTESIAN_POINT('Ctrl Pts',(-19.3289219205446,-41.7461216164653,
124.917060930271)) ;
#77443 = CARTESIAN_POINT('Ctrl Pts',(-19.3449799461922,-41.5661325360465,
124.616011040601)) ;
#77444 = CARTESIAN_POINT('Ctrl Pts',(-19.5912951011669,-41.7561108917333,
124.908434150121)) ;
#77445 = CARTESIAN_POINT('Ctrl Pts',(-19.554878426075,-41.5761218113145,124.609111482984)) ;
#77446 = CARTESIAN_POINT('Ctrl Pts',(-19.849396039096,-41.7661523499028,124.853543537004)) ;
#77447 = CARTESIAN_POINT('Ctrl Pts',(-19.7613596181265,-41.586163269484,124.565200709918)) ;
#77448 = CARTESIAN_POINT('Ctrl Pts',(-20.0891213276133,-41.7759838136911,
124.75717410497)) ;
#77449 = CARTESIAN_POINT('Ctrl Pts',(-19.9531398219293,-41.5959947332723,
124.488107167589)) ;
#77450 = CARTESIAN_POINT('Ctrl Pts',(-20.3126159521527,-41.785988745995,124.618753527339)) ;
#77451 = CARTESIAN_POINT('Ctrl Pts',(-20.1319364892421,-41.6059996655762,
124.377372384104)) ;
#77452 = CARTESIAN_POINT('Ctrl Pts',(-20.5082790001234,-41.7959751098897,
124.443796510955)) ;
#77453 = CARTESIAN_POINT('Ctrl Pts',(-20.2884681052533,-41.615986029471,124.237408279578)) ;
#77454 = CARTESIAN_POINT('Ctrl Pts',(-20.671089662106,-41.8060047387756,124.236556568572)) ;
#77455 = CARTESIAN_POINT('Ctrl Pts',(-20.4187181302531,-41.6260156583568,
124.071617471286)) ;
#77456 = CARTESIAN_POINT('Ctrl Pts',(-20.7938478464056,-41.815879960884,124.007888084139)) ;
#77457 = CARTESIAN_POINT('Ctrl Pts',(-20.5169261213944,-41.6358908804652,
123.88868407081)) ;
#77458 = CARTESIAN_POINT('Ctrl Pts',(-20.87634772346,-41.8258811732811,123.758394357576)) ;
#77459 = CARTESIAN_POINT('Ctrl Pts',(-20.5829278694143,-41.6458920928623,
123.689089793448)) ;
#77460 = CARTESIAN_POINT('Ctrl Pts',(-20.9141799975385,-41.8357897525166,
123.500723797929)) ;
#77461 = CARTESIAN_POINT('Ctrl Pts',(-20.6131956146695,-41.6558006720979,
123.482954012209)) ;
#77462 = CARTESIAN_POINT('Ctrl Pts',(-20.9065096443948,-41.8458446050726,
123.236647196733)) ;
#77463 = CARTESIAN_POINT('Ctrl Pts',(-20.607061323779,-41.6658555246539,123.271692585024)) ;
#77464 = CARTESIAN_POINT('Ctrl Pts',(-20.854419806544,-41.8557031873474,122.982817801562)) ;
#77465 = CARTESIAN_POINT('Ctrl Pts',(-20.5653915448547,-41.6757141069286,
123.068629169974)) ;
#77466 = CARTESIAN_POINT('Ctrl Pts',(-20.7572019523048,-41.86577131679,122.736787999783)) ;
#77467 = CARTESIAN_POINT('Ctrl Pts',(-20.4876191232104,-41.6857822363713,
122.871804461378)) ;
#77468 = CARTESIAN_POINT('Ctrl Pts',(-20.6216170476979,-41.8756267884792,
122.516096462848)) ;
#77469 = CARTESIAN_POINT('Ctrl Pts',(-20.3791532034229,-41.6956377080604,
122.695250586501)) ;
#77470 = CARTESIAN_POINT('Ctrl Pts',(-20.4479526498512,-41.8856216368654,
122.319060072971)) ;
#77471 = CARTESIAN_POINT('Ctrl Pts',(-20.2402233360119,-41.7056325564467,
122.537620125504)) ;
#77472 = CARTESIAN_POINT('Ctrl Pts',(-20.241600860006,-41.8956529336499,122.155008415719)) ;
#77473 = CARTESIAN_POINT('Ctrl Pts',(-20.0751431938009,-41.7156638532311,
122.406377179865)) ;
#77474 = CARTESIAN_POINT('Ctrl Pts',(-20.0138985646959,-41.90551946986,122.030978291857)) ;
#77475 = CARTESIAN_POINT('Ctrl Pts',(-19.8929827296992,-41.7255303894412,
122.307151422635)) ;
#77476 = CARTESIAN_POINT('Ctrl Pts',(-19.7652803950065,-41.9155068928208,
121.946967065422)) ;
#77477 = CARTESIAN_POINT('Ctrl Pts',(-19.6940889763465,-41.7355178124021,
122.23994043297)) ;
#77478 = CARTESIAN_POINT('Ctrl Pts',(-19.5069103967406,-41.9254518318406,
121.907424800188)) ;
#77479 = CARTESIAN_POINT('Ctrl Pts',(-19.4873934887718,-41.7454627514218,
122.208304514196)) ;
#77480 = CARTESIAN_POINT('Ctrl Pts',(-19.2430300937738,-41.9354967177006,
121.913529164993)) ;
#77481 = CARTESIAN_POINT('Ctrl Pts',(-19.2762891837712,-41.7555076372818,
122.213185853992)) ;
#77482 = CARTESIAN_POINT('Ctrl Pts',(-18.9887092821682,-41.9453652527868,
121.964316287539)) ;
#77483 = CARTESIAN_POINT('Ctrl Pts',(-19.072832435962,-41.7653761723681,122.253813365681)) ;
#77484 = CARTESIAN_POINT('Ctrl Pts',(-18.7444398718254,-41.9553311207935,
122.058732418044)) ;
#77485 = CARTESIAN_POINT('Ctrl Pts',(-18.8774162150229,-41.7753420403747,
122.329344164061)) ;
#77486 = CARTESIAN_POINT('Ctrl Pts',(-18.5191258959852,-41.965353768246,122.195167959757)) ;
#77487 = CARTESIAN_POINT('Ctrl Pts',(-18.6971639262968,-41.7853646878272,
122.438490705683)) ;
#77488 = CARTESIAN_POINT('Ctrl Pts',(-18.3228580657316,-41.9752774072536,
122.366864085239)) ;
#77489 = CARTESIAN_POINT('Ctrl Pts',(-18.5401483567963,-41.7952883268348,
122.575845826025)) ;
#77490 = CARTESIAN_POINT('Ctrl Pts',(-18.1585632396792,-41.9852201322593,
122.570050124115)) ;
#77491 = CARTESIAN_POINT('Ctrl Pts',(-18.4087108446553,-41.8052310518406,
122.738393149906)) ;
#77492 = CARTESIAN_POINT('Ctrl Pts',(-18.0310264116148,-41.9952657383112,
122.801169420602)) ;
#77493 = CARTESIAN_POINT('Ctrl Pts',(-18.3066794495729,-41.8152766578924,
122.923287501502)) ;
#77494 = CARTESIAN_POINT('Ctrl Pts',(-17.946842431743,-42.0051271608323,123.04628607553)) ;
#77495 = CARTESIAN_POINT('Ctrl Pts',(-18.2393302260419,-41.8251380804135,
123.119379900334)) ;
#77496 = CARTESIAN_POINT('Ctrl Pts',(-17.905523159314,-42.0151207292815,123.305597710685)) ;
#77497 = CARTESIAN_POINT('Ctrl Pts',(-18.2062726013886,-41.8351316488627,
123.326828797274)) ;
#77498 = CARTESIAN_POINT('Ctrl Pts',(-17.9096925518551,-42.0250462000368,
123.56643384869)) ;
#77499 = CARTESIAN_POINT('Ctrl Pts',(-18.2096058544786,-41.845057119618,123.535497626538)) ;
#77500 = CARTESIAN_POINT('Ctrl Pts',(-17.959571383868,-42.0350738739927,123.825153894788)) ;
#77501 = CARTESIAN_POINT('Ctrl Pts',(-18.2495067533621,-41.8550847935739,
123.742474085264)) ;
#77502 = CARTESIAN_POINT('Ctrl Pts',(-18.0520856876344,-42.0449610520343,
124.067987197521)) ;
#77503 = CARTESIAN_POINT('Ctrl Pts',(-18.3235158644063,-41.8649719716156,
123.93674127071)) ;
#77504 = CARTESIAN_POINT('Ctrl Pts',(-18.1870669887321,-42.0549894314025,
124.294288291732)) ;
#77505 = CARTESIAN_POINT('Ctrl Pts',(-18.4314996700195,-41.8750003509838,
124.117783890498)) ;
#77506 = CARTESIAN_POINT('Ctrl Pts',(-18.3569254896537,-42.064883674124,124.491191504036)) ;
#77507 = CARTESIAN_POINT('Ctrl Pts',(-18.5673820062169,-41.8848945937052,
124.275305521873)) ;
#77508 = CARTESIAN_POINT('Ctrl Pts',(-18.6285705557633,-42.0782365907749,
124.7132697805)) ;
#77509 = CARTESIAN_POINT('Ctrl Pts',(-18.7847096513815,-41.8982475103561,
124.452982209414)) ;
#77510 = CARTESIAN_POINT('Ctrl Pts',(-18.9483775262574,-42.0914391085216,
124.857795814256)) ;
#77511 = CARTESIAN_POINT('Ctrl Pts',(-19.0405786175282,-41.9114500281029,
124.568605567899)) ;
#77512 = CARTESIAN_POINT('Ctrl Pts',(-19.2946442504988,-42.1047950138026,
124.914924015867)) ;
#77513 = CARTESIAN_POINT('Ctrl Pts',(-19.3175485758015,-41.9248059333838,
124.614299551762)) ;
#77514 = CARTESIAN_POINT('Ctrl Pts',(-19.5547381910692,-42.1146916624404,
124.912293117232)) ;
#77515 = CARTESIAN_POINT('Ctrl Pts',(-19.5256324094928,-41.9347025820217,
124.612199382613)) ;
#77516 = CARTESIAN_POINT('Ctrl Pts',(-19.8142993016443,-42.1247398004929,
124.86390602354)) ;
#77517 = CARTESIAN_POINT('Ctrl Pts',(-19.7332792909241,-41.9447507200741,
124.573491312428)) ;
#77518 = CARTESIAN_POINT('Ctrl Pts',(-20.0576759369306,-42.1346307606706,
124.772616402123)) ;
#77519 = CARTESIAN_POINT('Ctrl Pts',(-19.9279820995287,-41.9546416802519,
124.500461812852)) ;
#77520 = CARTESIAN_POINT('Ctrl Pts',(-20.2841432703892,-42.1446235965474,
124.639664036418)) ;
#77521 = CARTESIAN_POINT('Ctrl Pts',(-20.1091567936653,-41.9646345161287,
124.394101924367)) ;
#77522 = CARTESIAN_POINT('Ctrl Pts',(-20.4846006079206,-42.154662691549,124.468172605325)) ;
#77523 = CARTESIAN_POINT('Ctrl Pts',(-20.269524451752,-41.9746736111302,124.256910062148)) ;
#77524 = CARTESIAN_POINT('Ctrl Pts',(-20.6493590678742,-42.1645000474001,
124.268925825655)) ;
#77525 = CARTESIAN_POINT('Ctrl Pts',(-20.4013316292031,-41.9845109669814,
124.097515752566)) ;
#77526 = CARTESIAN_POINT('Ctrl Pts',(-20.8232941424942,-42.1778929953309,
123.963015567202)) ;
#77527 = CARTESIAN_POINT('Ctrl Pts',(-20.5404892049295,-41.9979039149121,
123.85277973288)) ;
#77528 = CARTESIAN_POINT('Ctrl Pts',(-20.9119427187392,-42.1910596717578,
123.624389608239)) ;
#77529 = CARTESIAN_POINT('Ctrl Pts',(-20.6114090656495,-42.0110705913391,
123.581847590379)) ;
#77530 = CARTESIAN_POINT('Ctrl Pts',(-20.9103198255733,-42.2044444531646,
123.272710611948)) ;
#77531 = CARTESIAN_POINT('Ctrl Pts',(-20.6101088464383,-42.0244553727458,
123.300551791675)) ;
#77532 = CARTESIAN_POINT('Ctrl Pts',(-20.8642332430024,-42.2143062358084,
123.017641919744)) ;
#77533 = CARTESIAN_POINT('Ctrl Pts',(-20.5732425041568,-42.0343171553897,
123.096486611068)) ;
#77534 = CARTESIAN_POINT('Ctrl Pts',(-20.773744130429,-42.2243053837615,122.771002649434)) ;
#77535 = CARTESIAN_POINT('Ctrl Pts',(-20.5008532527009,-42.0443163033428,
122.899177173043)) ;
#77536 = CARTESIAN_POINT('Ctrl Pts',(-20.6432311627546,-42.2342081763786,
122.545797674222)) ;
#77537 = CARTESIAN_POINT('Ctrl Pts',(-20.3964433972298,-42.0542190959598,
122.71901073462)) ;
#77538 = CARTESIAN_POINT('Ctrl Pts',(-20.4731343577762,-42.2442577562695,
122.343862138683)) ;
#77539 = CARTESIAN_POINT('Ctrl Pts',(-20.2603721024993,-42.0642686758508,
122.557463185732)) ;
#77540 = CARTESIAN_POINT('Ctrl Pts',(-20.2076003347488,-42.257444830079,122.1209956095)) ;
#77541 = CARTESIAN_POINT('Ctrl Pts',(-20.0479240767754,-42.0774557496602,
122.379158188714)) ;
#77542 = CARTESIAN_POINT('Ctrl Pts',(-19.804126587412,-42.2741976200502,121.933081385901)) ;
#77543 = CARTESIAN_POINT('Ctrl Pts',(-19.7251863995672,-42.0942085396314,
122.228834129982)) ;
#77544 = CARTESIAN_POINT('Ctrl Pts',(-19.3673812946802,-42.2906862721449,
121.894819463431)) ;
#77545 = CARTESIAN_POINT('Ctrl Pts',(-19.3757249718531,-42.1106971917261,
122.198219603723)) ;
#77546 = CARTESIAN_POINT('Ctrl Pts',(-19.0216618584833,-42.3040430983283,
121.955010873932)) ;
#77547 = CARTESIAN_POINT('Ctrl Pts',(-19.0992014122385,-42.1240540179095,
122.246369156977)) ;
#77548 = CARTESIAN_POINT('Ctrl Pts',(-18.7769948828995,-42.3139394832062,
122.043336388538)) ;
#77549 = CARTESIAN_POINT('Ctrl Pts',(-18.9034558730959,-42.1339504027875,
122.31702867763)) ;
#77550 = CARTESIAN_POINT('Ctrl Pts',(-18.5489107992709,-42.3239459977267,
122.174062497351)) ;
#77551 = CARTESIAN_POINT('Ctrl Pts',(-18.7209920470431,-42.1439569173079,
122.421605740756)) ;
#77552 = CARTESIAN_POINT('Ctrl Pts',(-18.2820313955466,-42.3371361212431,
122.395439854846)) ;
#77553 = CARTESIAN_POINT('Ctrl Pts',(-18.5074779287399,-42.1571470408243,
122.598716881194)) ;
#77554 = CARTESIAN_POINT('Ctrl Pts',(-18.0248416306268,-42.3539026823926,
122.759167368736)) ;
#77555 = CARTESIAN_POINT('Ctrl Pts',(-18.3017330244153,-42.1739136019739,
122.889684714368)) ;
#77556 = CARTESIAN_POINT('Ctrl Pts',(-17.8860485150125,-42.3736871711007,
123.266512292207)) ;
#77557 = CARTESIAN_POINT('Ctrl Pts',(-18.190691850351,-42.1936980906819,123.295564709079)) ;
#77558 = CARTESIAN_POINT('Ctrl Pts',(-17.9274046620384,-42.3936326186972,
123.79488101199)) ;
#77559 = CARTESIAN_POINT('Ctrl Pts',(-18.2237744875469,-42.2136435382784,
123.718259302305)) ;
#77560 = CARTESIAN_POINT('Ctrl Pts',(-18.1467300052085,-42.4135442808531,
124.276525573027)) ;
#77561 = CARTESIAN_POINT('Ctrl Pts',(-18.3992319711091,-42.2335552004343,
124.103577050796)) ;
#77562 = CARTESIAN_POINT('Ctrl Pts',(-18.5161004763007,-42.433436472872,124.654913018511)) ;
#77563 = CARTESIAN_POINT('Ctrl Pts',(-18.6947270610426,-42.2534473924532,
124.40628936176)) ;
#77564 = CARTESIAN_POINT('Ctrl Pts',(-18.9961947812733,-42.4534776034266,
124.885472692645)) ;
#77565 = CARTESIAN_POINT('Ctrl Pts',(-19.0788009536354,-42.2734885230078,
124.590739459069)) ;
#77566 = CARTESIAN_POINT('Ctrl Pts',(-19.5204288936145,-42.4732959380422,
124.938073342038)) ;
#77567 = CARTESIAN_POINT('Ctrl Pts',(-19.4981894659672,-42.2933068576234,
124.632822663084)) ;
#77568 = CARTESIAN_POINT('Ctrl Pts',(-20.0350303911452,-42.4932685032617,
124.808520139726)) ;
#77569 = CARTESIAN_POINT('Ctrl Pts',(-19.9098714983823,-42.313279422843,124.529182116314)) ;
#77570 = CARTESIAN_POINT('Ctrl Pts',(-20.4730875843371,-42.5131577194334,
124.512279231731)) ;
#77571 = CARTESIAN_POINT('Ctrl Pts',(-20.2603191389922,-42.3331686390146,
124.292190423348)) ;
#77572 = CARTESIAN_POINT('Ctrl Pts',(-20.7853676285857,-42.5331812937561,
124.081500341459)) ;
#77573 = CARTESIAN_POINT('Ctrl Pts',(-20.510144598529,-42.3531922133373,123.947568642154)) ;
#77574 = CARTESIAN_POINT('Ctrl Pts',(-20.930672852745,-42.5529784568443,123.575689148446)) ;
#77575 = CARTESIAN_POINT('Ctrl Pts',(-20.6263909037281,-42.3729893764256,
123.542918090147)) ;
#77576 = CARTESIAN_POINT('Ctrl Pts',(-20.89563526975,-42.5729439506681,123.046309019456)) ;
#77577 = CARTESIAN_POINT('Ctrl Pts',(-20.5983617160724,-42.3929548702494,
123.119413476898)) ;
#77578 = CARTESIAN_POINT('Ctrl Pts',(-20.6814765720691,-42.5928976584095,
122.560980844354)) ;
#77579 = CARTESIAN_POINT('Ctrl Pts',(-20.4270354944749,-42.4129085779908,
122.731150136192)) ;
#77580 = CARTESIAN_POINT('Ctrl Pts',(-20.3156068294738,-42.6128050351361,
122.178926648518)) ;
#77581 = CARTESIAN_POINT('Ctrl Pts',(-20.1343395078316,-42.4328159547174,
122.425505382769)) ;
#77582 = CARTESIAN_POINT('Ctrl Pts',(-19.8430795028779,-42.6326572466847,
121.943950043766)) ;
#77583 = CARTESIAN_POINT('Ctrl Pts',(-19.7563159223275,-42.4526681662659,
122.237523311971)) ;
#77584 = CARTESIAN_POINT('Ctrl Pts',(-19.3129641321362,-42.6527296336304,
121.884197616133)) ;
#77585 = CARTESIAN_POINT('Ctrl Pts',(-19.3322245789558,-42.4727405532116,
122.189721484159)) ;
#77586 = CARTESIAN_POINT('Ctrl Pts',(-18.8004818960258,-42.6725675032707,
122.008159119994)) ;
#77587 = CARTESIAN_POINT('Ctrl Pts',(-18.9222366927177,-42.4925784228519,
122.288891090315)) ;
#77588 = CARTESIAN_POINT('Ctrl Pts',(-18.3595239815555,-42.6924181578238,
122.297834685057)) ;
#77589 = CARTESIAN_POINT('Ctrl Pts',(-18.5694695547567,-42.5124290774051,
122.52063348008)) ;
#77590 = CARTESIAN_POINT('Ctrl Pts',(-18.0413332377422,-42.7124700921642,
122.72531992571)) ;
#77591 = CARTESIAN_POINT('Ctrl Pts',(-18.3149181158026,-42.5324810117455,
122.862621797376)) ;
#77592 = CARTESIAN_POINT('Ctrl Pts',(-17.8898151801749,-42.7323032797303,
123.230332622457)) ;
#77593 = CARTESIAN_POINT('Ctrl Pts',(-18.1937042468816,-42.5523141993116,
123.266634019015)) ;
#77594 = CARTESIAN_POINT('Ctrl Pts',(-17.9188018274487,-42.752232491961,123.759028000025)) ;
#77595 = CARTESIAN_POINT('Ctrl Pts',(-18.2168953694706,-42.5722434115422,
123.689590983492)) ;
#77596 = CARTESIAN_POINT('Ctrl Pts',(-18.1255818945202,-42.7721174571754,
124.245626671877)) ;
#77597 = CARTESIAN_POINT('Ctrl Pts',(-18.3823217704082,-42.5921283767566,
124.078870010309)) ;
#77598 = CARTESIAN_POINT('Ctrl Pts',(-18.4898112909711,-42.79219119832,124.635336040319)) ;
#77599 = CARTESIAN_POINT('Ctrl Pts',(-18.6737062691616,-42.6122021179012,
124.390635650376)) ;
#77600 = CARTESIAN_POINT('Ctrl Pts',(-18.9586591559989,-42.8119843801004,
124.874120892194)) ;
#77601 = CARTESIAN_POINT('Ctrl Pts',(-19.0487871981899,-42.6319952996816,
124.581662463708)) ;
#77602 = CARTESIAN_POINT('Ctrl Pts',(-19.4849952307076,-42.8319470881031,
124.94071639769)) ;
#77603 = CARTESIAN_POINT('Ctrl Pts',(-19.4698566611138,-42.6519580076843,
124.634936088449)) ;
#77604 = CARTESIAN_POINT('Ctrl Pts',(-20.0027532085584,-42.8519300398455,
124.822320272829)) ;
#77605 = CARTESIAN_POINT('Ctrl Pts',(-19.8840626043544,-42.6719409594268,
124.540216680374)) ;
#77606 = CARTESIAN_POINT('Ctrl Pts',(-20.4457748039355,-42.8717406596177,
124.537685736261)) ;
#77607 = CARTESIAN_POINT('Ctrl Pts',(-20.2384794300186,-42.6917515791989,
124.312505791514)) ;
#77608 = CARTESIAN_POINT('Ctrl Pts',(-20.7682626055725,-42.8917243756506,
124.115808826905)) ;
#77609 = CARTESIAN_POINT('Ctrl Pts',(-20.496467127968,-42.7117352952318,123.975002213064)) ;
#77610 = CARTESIAN_POINT('Ctrl Pts',(-20.9266062653621,-42.9116058395479,
123.611535793614)) ;
#77611 = CARTESIAN_POINT('Ctrl Pts',(-20.6231390533387,-42.7316167591292,
123.571582135576)) ;
#77612 = CARTESIAN_POINT('Ctrl Pts',(-20.9036603573347,-42.9315611693923,
123.081759157347)) ;
#77613 = CARTESIAN_POINT('Ctrl Pts',(-20.6047789224965,-42.7515720889735,
123.147760755325)) ;
#77614 = CARTESIAN_POINT('Ctrl Pts',(-20.7024014511909,-42.9514366301977,
122.593252469711)) ;
#77615 = CARTESIAN_POINT('Ctrl Pts',(-20.4437676559676,-42.771447549779,122.756956211372)) ;
#77616 = CARTESIAN_POINT('Ctrl Pts',(-20.3449003201924,-42.9714209502493,
122.200502446614)) ;
#77617 = CARTESIAN_POINT('Ctrl Pts',(-20.1577657851218,-42.7914318698305,
122.442758885575)) ;
#77618 = CARTESIAN_POINT('Ctrl Pts',(-19.8758679528794,-42.9913489830389,
121.954198379495)) ;
#77619 = CARTESIAN_POINT('Ctrl Pts',(-19.7825308096546,-42.8113599026202,
122.24571839476)) ;
#77620 = CARTESIAN_POINT('Ctrl Pts',(-19.4385731677938,-43.0079577449787,
121.894584975547)) ;
#77621 = CARTESIAN_POINT('Ctrl Pts',(-19.4327162628233,-42.82796866456,122.198032510649)) ;
#77622 = CARTESIAN_POINT('Ctrl Pts',(-19.0946716816844,-43.0211453836688,
121.937615803006)) ;
#77623 = CARTESIAN_POINT('Ctrl Pts',(-19.1575750804821,-42.84115630325,122.232458887897)) ;
#77624 = CARTESIAN_POINT('Ctrl Pts',(-18.8437153065947,-43.0311318180289,
122.014331379979)) ;
#77625 = CARTESIAN_POINT('Ctrl Pts',(-18.9568164411077,-42.8511427376102,
122.293831610718)) ;
#77626 = CARTESIAN_POINT('Ctrl Pts',(-18.6094527008609,-43.0411411919883,
122.133980200426)) ;
#77627 = CARTESIAN_POINT('Ctrl Pts',(-18.7693988622901,-42.8611521115695,
122.38956024232)) ;
#77628 = CARTESIAN_POINT('Ctrl Pts',(-18.3305857336054,-43.0544312255535,
122.344252306503)) ;
#77629 = CARTESIAN_POINT('Ctrl Pts',(-18.5463444103637,-42.8744421451348,
122.55774111295)) ;
#77630 = CARTESIAN_POINT('Ctrl Pts',(-18.058791901131,-43.071025213216,122.691613440091)) ;
#77631 = CARTESIAN_POINT('Ctrl Pts',(-18.3288675517154,-42.8910361327973,
122.835684012626)) ;
#77632 = CARTESIAN_POINT('Ctrl Pts',(-17.9215463023581,-43.0876574684915,
123.111805423994)) ;
#77633 = CARTESIAN_POINT('Ctrl Pts',(-18.2190954252728,-42.9076683880728,
123.171796586433)) ;
#77634 = CARTESIAN_POINT('Ctrl Pts',(-17.9026645542889,-43.1008998521594,
123.459298795026)) ;
#77635 = CARTESIAN_POINT('Ctrl Pts',(-18.203983606276,-42.9209107717406,123.449819411052)) ;
#77636 = CARTESIAN_POINT('Ctrl Pts',(-17.933115438378,-43.1108140603868,123.718057560293)) ;
#77637 = CARTESIAN_POINT('Ctrl Pts',(-18.2283482599857,-42.9308249799681,
123.656820588526)) ;
#77638 = CARTESIAN_POINT('Ctrl Pts',(-18.0093888247414,-43.1208706996585,
123.971069080724)) ;
#77639 = CARTESIAN_POINT('Ctrl Pts',(-18.2893690473881,-42.9408816192397,
123.859230933456)) ;
#77640 = CARTESIAN_POINT('Ctrl Pts',(-18.1256799000597,-43.1307165060786,
124.202224696473)) ;
#77641 = CARTESIAN_POINT('Ctrl Pts',(-18.3824021684236,-42.9507274256599,
124.044152714525)) ;
#77642 = CARTESIAN_POINT('Ctrl Pts',(-18.2830849970075,-43.1407615057118,
124.414117164537)) ;
#77643 = CARTESIAN_POINT('Ctrl Pts',(-18.5083351697391,-42.960772425293,124.21367093415)) ;
#77644 = CARTESIAN_POINT('Ctrl Pts',(-18.5370432518798,-43.1540425280845,
124.653504054307)) ;
#77645 = CARTESIAN_POINT('Ctrl Pts',(-18.7114678288813,-42.9740534476658,
124.405150550178)) ;
#77646 = CARTESIAN_POINT('Ctrl Pts',(-18.8452649773072,-43.1672399746092,
124.820961905298)) ;
#77647 = CARTESIAN_POINT('Ctrl Pts',(-18.9580634355738,-42.9872508941904,
124.539134958599)) ;
#77648 = CARTESIAN_POINT('Ctrl Pts',(-19.1881152199905,-43.1806542724161,
124.902985566074)) ;
#77649 = CARTESIAN_POINT('Ctrl Pts',(-19.232360308715,-43.0006651919974,124.604753983446)) ;
#77650 = CARTESIAN_POINT('Ctrl Pts',(-19.4462101896767,-43.1904933378189,
124.918723959431)) ;
#77651 = CARTESIAN_POINT('Ctrl Pts',(-19.4388332239247,-43.0105042574002,
124.617341843955)) ;
#77652 = CARTESIAN_POINT('Ctrl Pts',(-19.70691664246,-43.2004765440966,124.889671060907)) ;
#77653 = CARTESIAN_POINT('Ctrl Pts',(-19.6473989352599,-43.0204874636778,
124.594097446698)) ;
#77654 = CARTESIAN_POINT('Ctrl Pts',(-19.9578281238574,-43.2104277790094,
124.815931888738)) ;
#77655 = CARTESIAN_POINT('Ctrl Pts',(-19.8481272005172,-43.0304386985906,
124.535103914391)) ;
#77656 = CARTESIAN_POINT('Ctrl Pts',(-20.1934350690433,-43.220428778711,124.699450982001)) ;
#77657 = CARTESIAN_POINT('Ctrl Pts',(-20.0366117625381,-43.0404396982923,
124.441917204073)) ;
#77658 = CARTESIAN_POINT('Ctrl Pts',(-20.4056235279115,-43.2304601244984,
124.543033701411)) ;
#77659 = CARTESIAN_POINT('Ctrl Pts',(-20.206361135427,-43.0504710440796,124.316781584499)) ;
#77660 = CARTESIAN_POINT('Ctrl Pts',(-20.5844761556789,-43.2403138892034,
124.355767995635)) ;
#77661 = CARTESIAN_POINT('Ctrl Pts',(-20.3494415434613,-43.0603248087846,
124.166967530126)) ;
#77662 = CARTESIAN_POINT('Ctrl Pts',(-20.7303004788891,-43.2502845428717,
124.138111587117)) ;
#77663 = CARTESIAN_POINT('Ctrl Pts',(-20.4660990801308,-43.0702954624529,
123.992841228193)) ;
#77664 = CARTESIAN_POINT('Ctrl Pts',(-20.8364178790176,-43.2602817865289,
123.897736472971)) ;
#77665 = CARTESIAN_POINT('Ctrl Pts',(-20.5509909214164,-43.0802927061101,
123.800540288638)) ;
#77666 = CARTESIAN_POINT('Ctrl Pts',(-20.8990697974947,-43.270315242473,123.641641842378)) ;
#77667 = CARTESIAN_POINT('Ctrl Pts',(-20.6011102563004,-43.0903261620543,
123.595664077152)) ;
#77668 = CARTESIAN_POINT('Ctrl Pts',(-20.9164201485292,-43.2801707467735,
123.38320598339)) ;
#77669 = CARTESIAN_POINT('Ctrl Pts',(-20.6149882875894,-43.1001816663547,
123.388915428103)) ;
#77670 = CARTESIAN_POINT('Ctrl Pts',(-20.8885847143256,-43.2901701830595,
123.121956715694)) ;
#77671 = CARTESIAN_POINT('Ctrl Pts',(-20.5927177264753,-43.1101811026408,
123.17991632247)) ;
#77672 = CARTESIAN_POINT('Ctrl Pts',(-20.8168337006827,-43.3000646425755,
122.871985466919)) ;
#77673 = CARTESIAN_POINT('Ctrl Pts',(-20.5353148477446,-43.1200755621567,
122.979940136269)) ;
#77674 = CARTESIAN_POINT('Ctrl Pts',(-20.7007964615209,-43.3101277620271,
122.634405971044)) ;
#77675 = CARTESIAN_POINT('Ctrl Pts',(-20.4424830472007,-43.1301386816084,
122.789877488713)) ;
#77676 = CARTESIAN_POINT('Ctrl Pts',(-20.548903419078,-43.3199673964391,122.425092863754)) ;
#77677 = CARTESIAN_POINT('Ctrl Pts',(-20.3209670269666,-43.1399783160204,
122.622428563072)) ;
#77678 = CARTESIAN_POINT('Ctrl Pts',(-20.3590408300739,-43.3300306039249,
122.241063679027)) ;
#77679 = CARTESIAN_POINT('Ctrl Pts',(-20.1690754107749,-43.1500415235061,
122.475206756355)) ;
#77680 = CARTESIAN_POINT('Ctrl Pts',(-20.1436111274477,-43.3399247113041,
122.095429795612)) ;
#77681 = CARTESIAN_POINT('Ctrl Pts',(-19.9967306388888,-43.1599356308853,
122.358701616965)) ;
#77682 = CARTESIAN_POINT('Ctrl Pts',(-19.9053553865349,-43.3498670434965,
121.988285686003)) ;
#77683 = CARTESIAN_POINT('Ctrl Pts',(-19.8061253596654,-43.1698779630777,
122.272988371083)) ;
#77684 = CARTESIAN_POINT('Ctrl Pts',(-19.6505873376489,-43.3598676698115,
121.923617759832)) ;
#77685 = CARTESIAN_POINT('Ctrl Pts',(-19.6023104651923,-43.1798785893927,
122.221256110046)) ;
#77686 = CARTESIAN_POINT('Ctrl Pts',(-19.387412643394,-43.3699094040934,121.904584247436)) ;
#77687 = CARTESIAN_POINT('Ctrl Pts',(-19.391770525899,-43.1899203236746,122.206031467427)) ;
#77688 = CARTESIAN_POINT('Ctrl Pts',(-19.1304837624311,-43.3797348300425,
121.930388446554)) ;
#77689 = CARTESIAN_POINT('Ctrl Pts',(-19.1862281367957,-43.1997457496237,
122.226676884756)) ;
#77690 = CARTESIAN_POINT('Ctrl Pts',(-18.8760169234249,-43.3897916565701,
122.001672515935)) ;
#77691 = CARTESIAN_POINT('Ctrl Pts',(-18.9826551632411,-43.2098025761514,
122.283706165014)) ;
#77692 = CARTESIAN_POINT('Ctrl Pts',(-18.6409865992332,-43.3997190896917,
122.11493089705)) ;
#77693 = CARTESIAN_POINT('Ctrl Pts',(-18.7946320604858,-43.219730009273,122.374314665372)) ;
#77694 = CARTESIAN_POINT('Ctrl Pts',(-18.4282774407741,-43.4096690820979,
122.26701392931)) ;
#77695 = CARTESIAN_POINT('Ctrl Pts',(-18.6244661072569,-43.2296800016792,
122.495982618452)) ;
#77696 = CARTESIAN_POINT('Ctrl Pts',(-18.2436237168823,-43.4197242831719,
122.456000772631)) ;
#77697 = CARTESIAN_POINT('Ctrl Pts',(-18.4767445661238,-43.2397352027532,
122.647173618493)) ;
#77698 = CARTESIAN_POINT('Ctrl Pts',(-18.0976352136823,-43.4295465572242,
122.668893815901)) ;
#77699 = CARTESIAN_POINT('Ctrl Pts',(-18.3599557989295,-43.2495574768055,
122.817488687827)) ;
#77700 = CARTESIAN_POINT('Ctrl Pts',(-17.9878760753137,-43.4396024511835,
122.90925930799)) ;
#77701 = CARTESIAN_POINT('Ctrl Pts',(-18.272150254971,-43.2596133707647,123.009781985742)) ;
#77702 = CARTESIAN_POINT('Ctrl Pts',(-17.9227225616892,-43.4495431730286,
123.162245934155)) ;
#77703 = CARTESIAN_POINT('Ctrl Pts',(-18.2200294874287,-43.2695540926099,
123.212171536294)) ;
#77704 = CARTESIAN_POINT('Ctrl Pts',(-17.9017472035659,-43.4594475171152,
123.421680109374)) ;
#77705 = CARTESIAN_POINT('Ctrl Pts',(-18.2032511636437,-43.2794584366965,
123.41971860684)) ;
#77706 = CARTESIAN_POINT('Ctrl Pts',(-17.9266517283389,-43.4694941844147,
123.684496298944)) ;
#77707 = CARTESIAN_POINT('Ctrl Pts',(-18.2231767399461,-43.2895051039959,
123.629971456514)) ;
#77708 = CARTESIAN_POINT('Ctrl Pts',(-17.9955444786617,-43.4793897428646,
123.935293204417)) ;
#77709 = CARTESIAN_POINT('Ctrl Pts',(-18.2782926706353,-43.2994006624459,
123.830608021522)) ;
#77710 = CARTESIAN_POINT('Ctrl Pts',(-18.1087774585217,-43.4894518215693,
124.174200467504)) ;
#77711 = CARTESIAN_POINT('Ctrl Pts',(-18.3688808575243,-43.3094627411505,
124.021733139343)) ;
#77712 = CARTESIAN_POINT('Ctrl Pts',(-18.2583544804656,-43.4992945200351,
124.385256639801)) ;
#77713 = CARTESIAN_POINT('Ctrl Pts',(-18.4885436261305,-43.3193054396163,
124.19057641101)) ;
#77714 = CARTESIAN_POINT('Ctrl Pts',(-18.4445910637564,-43.5092852939295,
124.570269448504)) ;
#77715 = CARTESIAN_POINT('Ctrl Pts',(-18.6375340693141,-43.3292962135108,
124.338585274364)) ;
#77716 = CARTESIAN_POINT('Ctrl Pts',(-18.6588280253522,-43.5192131631644,
124.719179491555)) ;
#77717 = CARTESIAN_POINT('Ctrl Pts',(-18.8089243549263,-43.3392240827457,
124.457711595414)) ;
#77718 = CARTESIAN_POINT('Ctrl Pts',(-18.8969249830117,-43.5292018921343,
124.829722059104)) ;
#77719 = CARTESIAN_POINT('Ctrl Pts',(-18.9994025173376,-43.3492128117156,
124.546144008221)) ;
#77720 = CARTESIAN_POINT('Ctrl Pts',(-19.1519853154848,-43.5392412941181,
124.897107997011)) ;
#77721 = CARTESIAN_POINT('Ctrl Pts',(-19.2034513317484,-43.3592522136993,
124.600051019993)) ;
#77722 = CARTESIAN_POINT('Ctrl Pts',(-19.4096395220042,-43.5490814618548,
124.919256070224)) ;
#77723 = CARTESIAN_POINT('Ctrl Pts',(-19.4095740497206,-43.3690923814361,
124.617767680726)) ;
#77724 = CARTESIAN_POINT('Ctrl Pts',(-19.6726790144128,-43.5591296722293,
124.896233588378)) ;
#77725 = CARTESIAN_POINT('Ctrl Pts',(-19.6200056228297,-43.3791405918106,
124.599348022425)) ;
#77726 = CARTESIAN_POINT('Ctrl Pts',(-19.9250688422625,-43.5690768425171,
124.828171804115)) ;
#77727 = CARTESIAN_POINT('Ctrl Pts',(-19.8219167126913,-43.3890877620984,
124.544896996661)) ;
#77728 = CARTESIAN_POINT('Ctrl Pts',(-20.1612764163258,-43.5789876907722,
124.718431010674)) ;
#77729 = CARTESIAN_POINT('Ctrl Pts',(-20.0108816130576,-43.3989986103534,
124.457103131757)) ;
#77730 = CARTESIAN_POINT('Ctrl Pts',(-20.3778135164168,-43.5890440184499,
124.566965650314)) ;
#77731 = CARTESIAN_POINT('Ctrl Pts',(-20.1841104958632,-43.4090549380312,
124.335929390239)) ;
#77732 = CARTESIAN_POINT('Ctrl Pts',(-20.5611126310766,-43.5988944312185,
124.384166137537)) ;
#77733 = CARTESIAN_POINT('Ctrl Pts',(-20.3307480642774,-43.4189053507997,
124.189689229524)) ;
#77734 = CARTESIAN_POINT('Ctrl Pts',(-20.7130674437035,-43.6089213170522,
124.168903399336)) ;
#77735 = CARTESIAN_POINT('Ctrl Pts',(-20.4523107179373,-43.4289322366334,
124.017478157488)) ;
#77736 = CARTESIAN_POINT('Ctrl Pts',(-20.8247441402527,-43.618949932683,123.930180059056)) ;
#77737 = CARTESIAN_POINT('Ctrl Pts',(-20.5416506341111,-43.4389608522643,
123.82649874937)) ;
#77738 = CARTESIAN_POINT('Ctrl Pts',(-20.8924859436322,-43.6287951560605,
123.680497788529)) ;
#77739 = CARTESIAN_POINT('Ctrl Pts',(-20.5958423726042,-43.4488060756417,
123.626753399107)) ;
#77740 = CARTESIAN_POINT('Ctrl Pts',(-20.9168945753088,-43.6387858381621,
123.419083293923)) ;
#77741 = CARTESIAN_POINT('Ctrl Pts',(-20.6153678869585,-43.4587967577433,
123.417621830856)) ;
#77742 = CARTESIAN_POINT('Ctrl Pts',(-20.8948561360982,-43.6488237267945,
123.15622317163)) ;
#77743 = CARTESIAN_POINT('Ctrl Pts',(-20.5977356311787,-43.4688346463758,
123.207333751848)) ;
#77744 = CARTESIAN_POINT('Ctrl Pts',(-20.8292438814433,-43.6586680618977,
122.905971997086)) ;
#77745 = CARTESIAN_POINT('Ctrl Pts',(-20.5452447033601,-43.4786789814789,
123.00713407774)) ;
#77746 = CARTESIAN_POINT('Ctrl Pts',(-20.7201211840923,-43.6686530240952,
122.667383970139)) ;
#77747 = CARTESIAN_POINT('Ctrl Pts',(-20.4579454445687,-43.4886639436764,
122.816264379379)) ;
#77748 = CARTESIAN_POINT('Ctrl Pts',(-20.5719738573376,-43.6785919656286,
122.452232949028)) ;
#77749 = CARTESIAN_POINT('Ctrl Pts',(-20.3394267805854,-43.4986028852098,
122.644144644649)) ;
#77750 = CARTESIAN_POINT('Ctrl Pts',(-20.3868068905276,-43.6886338506,122.264249292285)) ;
#77751 = CARTESIAN_POINT('Ctrl Pts',(-20.1912922023766,-43.5086447701812,
122.493758541871)) ;
#77752 = CARTESIAN_POINT('Ctrl Pts',(-20.175193466136,-43.6985203985083,122.113473137237)) ;
#77753 = CARTESIAN_POINT('Ctrl Pts',(-20.0220013410477,-43.5185313180895,
122.373139073177)) ;
#77754 = CARTESIAN_POINT('Ctrl Pts',(-19.9382875920077,-43.7085143240083,
122.000193047027)) ;
#77755 = CARTESIAN_POINT('Ctrl Pts',(-19.8324762632877,-43.5285252435895,
122.282516123217)) ;
#77756 = CARTESIAN_POINT('Ctrl Pts',(-19.6867374287738,-43.7184504151347,
121.930037797463)) ;
#77757 = CARTESIAN_POINT('Ctrl Pts',(-19.631236272687,-43.538461334716,122.226393150879)) ;
#77758 = CARTESIAN_POINT('Ctrl Pts',(-19.4244597082905,-43.7284796841147,
121.904445450398)) ;
#77759 = CARTESIAN_POINT('Ctrl Pts',(-19.4214139225834,-43.5484906036959,
122.205920422987)) ;
#77760 = CARTESIAN_POINT('Ctrl Pts',(-19.1654713412094,-43.738362066674,121.924160359711)) ;
#77761 = CARTESIAN_POINT('Ctrl Pts',(-19.2142241183985,-43.5583729862552,
122.221693371168)) ;
#77762 = CARTESIAN_POINT('Ctrl Pts',(-18.9095644693569,-43.7484145837619,
121.989548406025)) ;
#77763 = CARTESIAN_POINT('Ctrl Pts',(-19.0094986897132,-43.5684255033431,
122.274004889728)) ;
#77764 = CARTESIAN_POINT('Ctrl Pts',(-18.6725555427022,-43.7583087045857,
122.096577505289)) ;
#77765 = CARTESIAN_POINT('Ctrl Pts',(-18.8198926461261,-43.578319624167,122.359628808823)) ;
#77766 = CARTESIAN_POINT('Ctrl Pts',(-18.4541166119818,-43.7683706840062,
122.245521781362)) ;
#77767 = CARTESIAN_POINT('Ctrl Pts',(-18.6451418602276,-43.5883816035874,
122.478785221664)) ;
#77768 = CARTESIAN_POINT('Ctrl Pts',(-18.2688956918236,-43.7782152172351,
122.426149066482)) ;
#77769 = CARTESIAN_POINT('Ctrl Pts',(-18.4969665901332,-43.5982261368164,
122.623287037953)) ;
#77770 = CARTESIAN_POINT('Ctrl Pts',(-18.1153222214093,-43.7881752961414,
122.638095379922)) ;
#77771 = CARTESIAN_POINT('Ctrl Pts',(-18.3741086705153,-43.6081862157226,
122.792844257825)) ;
#77772 = CARTESIAN_POINT('Ctrl Pts',(-18.0004538038229,-43.798213572714,122.875554226938)) ;
#77773 = CARTESIAN_POINT('Ctrl Pts',(-18.2822147043336,-43.6182244922952,
122.982811851236)) ;
#77774 = CARTESIAN_POINT('Ctrl Pts',(-17.9292494151495,-43.8080869592518,
123.125095646761)) ;
#77775 = CARTESIAN_POINT('Ctrl Pts',(-18.225252205665,-43.6280978788331,123.182444339761)) ;
#77776 = CARTESIAN_POINT('Ctrl Pts',(-17.9020001551184,-43.8181599020189,
123.388344568529)) ;
#77777 = CARTESIAN_POINT('Ctrl Pts',(-18.2034535746662,-43.6381708216001,
123.393043900429)) ;
#77778 = CARTESIAN_POINT('Ctrl Pts',(-17.9200947061093,-43.8279813161472,
123.64585694239)) ;
#77779 = CARTESIAN_POINT('Ctrl Pts',(-18.2179298642884,-43.6479922357285,
123.599052510802)) ;
#77780 = CARTESIAN_POINT('Ctrl Pts',(-17.9839061110821,-43.8380559462195,
123.902752660062)) ;
#77781 = CARTESIAN_POINT('Ctrl Pts',(-18.2689797188223,-43.6580668658008,
123.804569272354)) ;
#77782 = CARTESIAN_POINT('Ctrl Pts',(-18.0892674356352,-43.8479225835364,
124.139701464769)) ;
#77783 = CARTESIAN_POINT('Ctrl Pts',(-18.353269010714,-43.6679335031176,123.99412714447)) ;
#77784 = CARTESIAN_POINT('Ctrl Pts',(-18.2358881550093,-43.8579461289082,
124.358516056975)) ;
#77785 = CARTESIAN_POINT('Ctrl Pts',(-18.4705660406864,-43.6779570484894,
124.169178557313)) ;
#77786 = CARTESIAN_POINT('Ctrl Pts',(-18.4187926357284,-43.8679718804254,
124.548170374681)) ;
#77787 = CARTESIAN_POINT('Ctrl Pts',(-18.6168901651521,-43.6879828000066,
124.320901587011)) ;
#77788 = CARTESIAN_POINT('Ctrl Pts',(-18.6279123308631,-43.8778254674347,
124.700856473508)) ;
#77789 = CARTESIAN_POINT('Ctrl Pts',(-18.7841853999482,-43.697836387016,124.443049376181)) ;
#77790 = CARTESIAN_POINT('Ctrl Pts',(-18.8629865023104,-43.8878024276627,
124.816974766351)) ;
#77791 = CARTESIAN_POINT('Ctrl Pts',(-18.9722446774819,-43.7078133472439,
124.535943532528)) ;
#77792 = CARTESIAN_POINT('Ctrl Pts',(-19.1158727505967,-43.8978235706912,
124.890405499209)) ;
#77793 = CARTESIAN_POINT('Ctrl Pts',(-19.1745538313907,-43.7178344902724,
124.594687628449)) ;
#77794 = CARTESIAN_POINT('Ctrl Pts',(-19.3740398930862,-43.9077061767111,
124.918943559818)) ;
#77795 = CARTESIAN_POINT('Ctrl Pts',(-19.3810867133437,-43.7277170962923,
124.617517603467)) ;
#77796 = CARTESIAN_POINT('Ctrl Pts',(-19.6380282810984,-43.9177746473438,
124.901808569006)) ;
#77797 = CARTESIAN_POINT('Ctrl Pts',(-19.5922777253755,-43.737785566925,124.603809182427)) ;
#77798 = CARTESIAN_POINT('Ctrl Pts',(-19.8891040806478,-43.9276047305275,
124.840852015911)) ;
#77799 = CARTESIAN_POINT('Ctrl Pts',(-19.7931370891346,-43.7476156501087,
124.555043909552)) ;
#77800 = CARTESIAN_POINT('Ctrl Pts',(-20.1315321755266,-43.9376712902079,
124.735084209489)) ;
#77801 = CARTESIAN_POINT('Ctrl Pts',(-19.9870797585783,-43.7576822097891,
124.470429312396)) ;
#77802 = CARTESIAN_POINT('Ctrl Pts',(-20.3480256593749,-43.947561540037,124.591215461455)) ;
#77803 = CARTESIAN_POINT('Ctrl Pts',(-20.1602736880261,-43.7675724596183,
124.355334538994)) ;
#77804 = CARTESIAN_POINT('Ctrl Pts',(-20.5385520108474,-43.9575537057859,
124.410544001572)) ;
#77805 = CARTESIAN_POINT('Ctrl Pts',(-20.3126945474677,-43.7775646253671,
124.210797386208)) ;
#77806 = CARTESIAN_POINT('Ctrl Pts',(-20.6941599748475,-43.967516549382,124.199999732242)) ;
#77807 = CARTESIAN_POINT('Ctrl Pts',(-20.4371805360489,-43.7875274689632,
124.042362141687)) ;
#77808 = CARTESIAN_POINT('Ctrl Pts',(-20.8107661786946,-43.9774207182097,
123.967284902369)) ;
#77809 = CARTESIAN_POINT('Ctrl Pts',(-20.5304651300537,-43.797431637791,123.856190933871)) ;
#77810 = CARTESIAN_POINT('Ctrl Pts',(-20.8861267322825,-43.9874815931041,
123.713900101294)) ;
#77811 = CARTESIAN_POINT('Ctrl Pts',(-20.5907535610701,-43.8074925126853,
123.653482792957)) ;
#77812 = CARTESIAN_POINT('Ctrl Pts',(-20.9160480544074,-43.9973204964335,
123.457038808337)) ;
#77813 = CARTESIAN_POINT('Ctrl Pts',(-20.6146904768429,-43.8173314160147,
123.44799493269)) ;
#77814 = CARTESIAN_POINT('Ctrl Pts',(-20.9008215570039,-44.0073888728073,
123.192934464744)) ;
#77815 = CARTESIAN_POINT('Ctrl Pts',(-20.6025093217577,-43.8273997923886,
123.236711133605)) ;
#77816 = CARTESIAN_POINT('Ctrl Pts',(-20.8409996768118,-44.01726948944,122.940227571299)) ;
#77817 = CARTESIAN_POINT('Ctrl Pts',(-20.5546520629352,-43.8372804090212,
123.034546490848)) ;
#77818 = CARTESIAN_POINT('Ctrl Pts',(-20.7375752827161,-44.027260649669,122.698940269749)) ;
#77819 = CARTESIAN_POINT('Ctrl Pts',(-20.4719127723535,-43.8472715692502,
122.841516743795)) ;
#77820 = CARTESIAN_POINT('Ctrl Pts',(-20.5943672383573,-44.0372137231011,
122.48002524176)) ;
#77821 = CARTESIAN_POINT('Ctrl Pts',(-20.357346713871,-43.8572246426823,122.666384965214)) ;
#77822 = CARTESIAN_POINT('Ctrl Pts',(-20.4138140211053,-44.0472495587137,
122.28781904811)) ;
#77823 = CARTESIAN_POINT('Ctrl Pts',(-20.212904171313,-43.867260478295,122.512619815452)) ;
#77824 = CARTESIAN_POINT('Ctrl Pts',(-20.205771627624,-44.0571396854439,122.132010547395)) ;
#77825 = CARTESIAN_POINT('Ctrl Pts',(-20.0464710629452,-43.8771506050251,
122.387973367554)) ;
#77826 = CARTESIAN_POINT('Ctrl Pts',(-19.9716606493193,-44.0671318672132,
122.01311881931)) ;
#77827 = CARTESIAN_POINT('Ctrl Pts',(-19.8591825691405,-43.8871427867944,
122.292859783673)) ;
#77828 = CARTESIAN_POINT('Ctrl Pts',(-19.7215859697083,-44.0770778071876,
121.937116648919)) ;
#77829 = CARTESIAN_POINT('Ctrl Pts',(-19.6591233631449,-43.8970887267689,
122.232057912344)) ;
#77830 = CARTESIAN_POINT('Ctrl Pts',(-19.4621316011736,-44.0870249909471,
121.905158079353)) ;
#77831 = CARTESIAN_POINT('Ctrl Pts',(-19.4515603759915,-43.9070359105284,
122.206490695908)) ;
#77832 = CARTESIAN_POINT('Ctrl Pts',(-19.1984633098355,-44.0970729292374,
121.919166261337)) ;
#77833 = CARTESIAN_POINT('Ctrl Pts',(-19.2406255245606,-43.9170838488187,
122.217696907762)) ;
#77834 = CARTESIAN_POINT('Ctrl Pts',(-18.9462999516844,-44.106920564051,121.977344862688)) ;
#77835 = CARTESIAN_POINT('Ctrl Pts',(-19.0388958389278,-43.9269314836323,
122.264239147175)) ;
#77836 = CARTESIAN_POINT('Ctrl Pts',(-18.705003034918,-44.1168822777489,122.078833023543)) ;
#77837 = CARTESIAN_POINT('Ctrl Pts',(-18.8458584060323,-43.9368931973302,
122.345428976242)) ;
#77838 = CARTESIAN_POINT('Ctrl Pts',(-18.4836721334417,-44.1269109135701,
122.221925766964)) ;
#77839 = CARTESIAN_POINT('Ctrl Pts',(-18.6687933369296,-43.9469218331514,
122.459902775154)) ;
#77840 = CARTESIAN_POINT('Ctrl Pts',(-18.2927904239881,-44.1368212283219,
122.399078178107)) ;
#77841 = CARTESIAN_POINT('Ctrl Pts',(-18.5160881141208,-43.9568321479032,
122.601623829949)) ;
#77842 = CARTESIAN_POINT('Ctrl Pts',(-18.1346189320246,-44.1467560989846,
122.60679979721)) ;
#77843 = CARTESIAN_POINT('Ctrl Pts',(-18.3895506742922,-43.9667670185658,
122.767800273057)) ;
#77844 = CARTESIAN_POINT('Ctrl Pts',(-18.0138706730866,-44.1567972813863,
122.841409864092)) ;
#77845 = CARTESIAN_POINT('Ctrl Pts',(-18.2929514212946,-43.9768082009676,
122.955488165132)) ;
#77846 = CARTESIAN_POINT('Ctrl Pts',(-17.9366823754351,-44.1666842528511,
123.089522739993)) ;
#77847 = CARTESIAN_POINT('Ctrl Pts',(-18.2312003631439,-43.9866951724323,
123.153977453905)) ;
#77848 = CARTESIAN_POINT('Ctrl Pts',(-17.9030484193325,-44.1766836851137,
123.350101781406)) ;
#77849 = CARTESIAN_POINT('Ctrl Pts',(-18.2042924372665,-43.9966946046949,
123.36244046689)) ;
#77850 = CARTESIAN_POINT('Ctrl Pts',(-17.91490147005,-44.1866037503703,123.610552838721)) ;
#77851 = CARTESIAN_POINT('Ctrl Pts',(-18.213774030704,-44.0066146699516,123.570800751409)) ;
#77852 = CARTESIAN_POINT('Ctrl Pts',(-17.9724055289825,-44.1966406029545,
123.867950986187)) ;
#77853 = CARTESIAN_POINT('Ctrl Pts',(-18.2597764896288,-44.0166515225357,
123.776719574248)) ;
#77854 = CARTESIAN_POINT('Ctrl Pts',(-18.072489495882,-44.2065532622945,124.108457083353)) ;
#77855 = CARTESIAN_POINT('Ctrl Pts',(-18.33984264497,-44.0265641818757,123.969124165985)) ;
#77856 = CARTESIAN_POINT('Ctrl Pts',(-18.2134492761072,-44.2165444742093,
124.329987229875)) ;
#77857 = CARTESIAN_POINT('Ctrl Pts',(-18.4526095642665,-44.0365553937906,
124.146348659042)) ;
#77858 = CARTESIAN_POINT('Ctrl Pts',(-18.3920400927289,-44.2265861156124,
124.524226386367)) ;
#77859 = CARTESIAN_POINT('Ctrl Pts',(-18.5954817048883,-44.0465970351937,
124.301740649263)) ;
#77860 = CARTESIAN_POINT('Ctrl Pts',(-18.5968513118153,-44.2364149098195,
124.681658511615)) ;
#77861 = CARTESIAN_POINT('Ctrl Pts',(-18.7593291698146,-44.0564258294008,
124.427686424433)) ;
#77862 = CARTESIAN_POINT('Ctrl Pts',(-18.831525371307,-44.2464913209408,124.804205426274)) ;
#77863 = CARTESIAN_POINT('Ctrl Pts',(-18.9470682569457,-44.066502240522,124.525725008789)) ;
#77864 = CARTESIAN_POINT('Ctrl Pts',(-19.078357884535,-44.2563434539832,124.882525082064)) ;
#77865 = CARTESIAN_POINT('Ctrl Pts',(-19.1445330139973,-44.0763543735645,
124.588381422117)) ;
#77866 = CARTESIAN_POINT('Ctrl Pts',(-19.3406710042033,-44.2664166883245,
124.917774928985)) ;
#77867 = CARTESIAN_POINT('Ctrl Pts',(-19.3543836827224,-44.0864276079058,
124.616582420438)) ;
#77868 = CARTESIAN_POINT('Ctrl Pts',(-19.5990935689859,-44.2762581896512,
124.907117526499)) ;
#77869 = CARTESIAN_POINT('Ctrl Pts',(-19.5611207373312,-44.0962691092324,
124.608057610087)) ;
#77870 = CARTESIAN_POINT('Ctrl Pts',(-19.8549900005476,-44.286219141246,124.852048008069)) ;
#77871 = CARTESIAN_POINT('Ctrl Pts',(-19.7658378370726,-44.1062300608272,
124.56400332464)) ;
#77872 = CARTESIAN_POINT('Ctrl Pts',(-20.0991093096475,-44.2962569589666,
124.752132918125)) ;
#77873 = CARTESIAN_POINT('Ctrl Pts',(-19.9611338268518,-44.1162678785479,
124.484072297486)) ;
#77874 = CARTESIAN_POINT('Ctrl Pts',(-20.3188305768952,-44.3061313082237,
124.614027246314)) ;
#77875 = CARTESIAN_POINT('Ctrl Pts',(-20.1369108352661,-44.1261422278049,
124.373589272937)) ;
#77876 = CARTESIAN_POINT('Ctrl Pts',(-20.5149750944299,-44.3162008589659,
124.43646009171)) ;
#77877 = CARTESIAN_POINT('Ctrl Pts',(-20.2938275119669,-44.1362117785471,
124.231536305792)) ;
#77878 = CARTESIAN_POINT('Ctrl Pts',(-20.6736665783671,-44.3260348784745,
124.232462693765)) ;
#77879 = CARTESIAN_POINT('Ctrl Pts',(-20.4207810991636,-44.1460457980557,
124.068340001014)) ;
#77880 = CARTESIAN_POINT('Ctrl Pts',(-20.7975823821295,-44.336069033054,123.999722159429)) ;
#77881 = CARTESIAN_POINT('Ctrl Pts',(-20.5199150654758,-44.1560799526353,
123.88214817752)) ;
#77882 = CARTESIAN_POINT('Ctrl Pts',(-20.8784453197295,-44.3460849588765,
123.749227159085)) ;
#77883 = CARTESIAN_POINT('Ctrl Pts',(-20.5846066615164,-44.1660958784577,
123.681752589755)) ;
#77884 = CARTESIAN_POINT('Ctrl Pts',(-20.9145638047595,-44.3559672140707,
123.49205122072)) ;
#77885 = CARTESIAN_POINT('Ctrl Pts',(-20.613502746607,-44.175978133652,123.476012754182)) ;
#77886 = CARTESIAN_POINT('Ctrl Pts',(-20.9057075528945,-44.3659560205816,
123.229734225028)) ;
#77887 = CARTESIAN_POINT('Ctrl Pts',(-20.6064192252653,-44.1859669401629,
123.266159268691)) ;
#77888 = CARTESIAN_POINT('Ctrl Pts',(-20.8518375941901,-44.3759045878444,
122.973864298025)) ;
#77889 = CARTESIAN_POINT('Ctrl Pts',(-20.563324813657,-44.1959155074256,123.061463372867)) ;
#77890 = CARTESIAN_POINT('Ctrl Pts',(-20.753082557148,-44.3859593931464,122.728813985301)) ;
#77891 = CARTESIAN_POINT('Ctrl Pts',(-20.4843220736738,-44.2059703127276,
122.86542241497)) ;
#77892 = CARTESIAN_POINT('Ctrl Pts',(-20.616855401544,-44.3957781764099,122.509662800828)) ;
#77893 = CARTESIAN_POINT('Ctrl Pts',(-20.3753421837085,-44.2157890959912,
122.690101516828)) ;
#77894 = CARTESIAN_POINT('Ctrl Pts',(-20.4413805689647,-44.4058139487705,
122.312790934057)) ;
#77895 = CARTESIAN_POINT('Ctrl Pts',(-20.2349635031074,-44.2258248683518,
122.532602849493)) ;
#77896 = CARTESIAN_POINT('Ctrl Pts',(-20.2341379247197,-44.4158386477992,
122.150140067288)) ;
#77897 = CARTESIAN_POINT('Ctrl Pts',(-20.0691703136329,-44.2358495673804,
122.402480945821)) ;
#77898 = CARTESIAN_POINT('Ctrl Pts',(-20.0060783373224,-44.4256906510582,
122.027581366455)) ;
#77899 = CARTESIAN_POINT('Ctrl Pts',(-19.8867241261111,-44.2457015706395,
122.304432930007)) ;
#77900 = CARTESIAN_POINT('Ctrl Pts',(-19.7568956897804,-44.4356815854555,
121.94497080337)) ;
#77901 = CARTESIAN_POINT('Ctrl Pts',(-19.6873786743973,-44.2556925050367,
122.238342904726)) ;
#77902 = CARTESIAN_POINT('Ctrl Pts',(-19.4990141869597,-44.4455995078866,
121.906980973372)) ;
#77903 = CARTESIAN_POINT('Ctrl Pts',(-19.4810741764347,-44.2656104274678,
122.207949395468)) ;
#77904 = CARTESIAN_POINT('Ctrl Pts',(-19.2356052976656,-44.4556278635689,
121.914367687835)) ;
#77905 = CARTESIAN_POINT('Ctrl Pts',(-19.2703469878274,-44.2756387831502,
122.213857026739)) ;
#77906 = CARTESIAN_POINT('Ctrl Pts',(-18.9811319609968,-44.4655121480795,
121.966499520209)) ;
#77907 = CARTESIAN_POINT('Ctrl Pts',(-19.0667685443539,-44.2855230676607,
122.255560647816)) ;
#77908 = CARTESIAN_POINT('Ctrl Pts',(-18.7367176525128,-44.4755048319874,
122.062515901557)) ;
#77909 = CARTESIAN_POINT('Ctrl Pts',(-18.871236522365,-44.2955157515686,122.332371983472)) ;
#77910 = CARTESIAN_POINT('Ctrl Pts',(-18.5121188960051,-44.4855335689951,
122.200401078734)) ;
#77911 = CARTESIAN_POINT('Ctrl Pts',(-18.6915565682666,-44.3055444885763,
122.442678613519)) ;
#77912 = CARTESIAN_POINT('Ctrl Pts',(-18.3174591680508,-44.495418965624,122.372439116278)) ;
#77913 = CARTESIAN_POINT('Ctrl Pts',(-18.5358279827225,-44.3154298852052,
122.580307299376)) ;
#77914 = CARTESIAN_POINT('Ctrl Pts',(-18.1536797929993,-44.5054068510379,
122.57750876057)) ;
#77915 = CARTESIAN_POINT('Ctrl Pts',(-18.4048030832296,-44.3254177706191,
122.744361731314)) ;
#77916 = CARTESIAN_POINT('Ctrl Pts',(-18.0283271818047,-44.5153575536985,
122.807042074276)) ;
#77917 = CARTESIAN_POINT('Ctrl Pts',(-18.3045194438468,-44.3353684732797,
122.927987235333)) ;
#77918 = CARTESIAN_POINT('Ctrl Pts',(-17.9441368873553,-44.5253978717959,
123.057070192347)) ;
#77919 = CARTESIAN_POINT('Ctrl Pts',(-18.2371653982975,-44.3454087913771,
123.128009182656)) ;
#77920 = CARTESIAN_POINT('Ctrl Pts',(-17.9050280765353,-44.5352724371291,
123.313629339721)) ;
#77921 = CARTESIAN_POINT('Ctrl Pts',(-18.2058765291738,-44.3552833567104,
123.333255668068)) ;
#77922 = CARTESIAN_POINT('Ctrl Pts',(-17.9108009162363,-44.5452720971902,
123.576303554654)) ;
#77923 = CARTESIAN_POINT('Ctrl Pts',(-18.2104928246366,-44.3652830167714,
123.543394997243)) ;
#77924 = CARTESIAN_POINT('Ctrl Pts',(-17.9614015775647,-44.5551810923579,
123.83178501251)) ;
#77925 = CARTESIAN_POINT('Ctrl Pts',(-18.2509713159387,-44.3751920119392,
123.747780179525)) ;
#77926 = CARTESIAN_POINT('Ctrl Pts',(-18.0570243117927,-44.5652358335212,
124.078057381531)) ;
#77927 = CARTESIAN_POINT('Ctrl Pts',(-18.3274676754747,-44.3852467531024,
123.944798879371)) ;
#77928 = CARTESIAN_POINT('Ctrl Pts',(-18.1910740417786,-44.5750944454349,
124.299808917712)) ;
#77929 = CARTESIAN_POINT('Ctrl Pts',(-18.4347054549292,-44.3951053650162,
124.122200713057)) ;
#77930 = CARTESIAN_POINT('Ctrl Pts',(-18.3650377632803,-44.5851625677143,
124.49910396342)) ;
#77931 = CARTESIAN_POINT('Ctrl Pts',(-18.5738749680476,-44.4051734872955,
124.281638189971)) ;
#77932 = CARTESIAN_POINT('Ctrl Pts',(-18.5666736485411,-44.5950180384175,
124.661680062397)) ;
#77933 = CARTESIAN_POINT('Ctrl Pts',(-18.7351820039692,-44.4150289579987,
124.411700348019)) ;
#77934 = CARTESIAN_POINT('Ctrl Pts',(-18.7962745857529,-44.6050128979108,
124.78921896705)) ;
#77935 = CARTESIAN_POINT('Ctrl Pts',(-18.9188616496907,-44.4250238174921,
124.513733295613)) ;
#77936 = CARTESIAN_POINT('Ctrl Pts',(-19.045634886817,-44.6150441512528,124.874734939546)) ;
#77937 = CARTESIAN_POINT('Ctrl Pts',(-19.1183492174815,-44.435055070834,124.582148031688)) ;
#77938 = CARTESIAN_POINT('Ctrl Pts',(-19.3017226630641,-44.6249108501259,
124.915389460371)) ;
#77939 = CARTESIAN_POINT('Ctrl Pts',(-19.3232187005312,-44.4449217697071,
124.614673670169)) ;
#77940 = CARTESIAN_POINT('Ctrl Pts',(-19.5641051552201,-44.6348976658771,
124.911339609396)) ;
#77941 = CARTESIAN_POINT('Ctrl Pts',(-19.5331246292621,-44.4549085854583,
124.611435943813)) ;
#77942 = CARTESIAN_POINT('Ctrl Pts',(-19.820862633576,-44.6448448710725,124.862095013868)) ;
#77943 = CARTESIAN_POINT('Ctrl Pts',(-19.7385308356951,-44.4648557906538,
124.572042423977)) ;
#77944 = CARTESIAN_POINT('Ctrl Pts',(-20.0674296682217,-44.6548878591988,
124.768031081774)) ;
#77945 = CARTESIAN_POINT('Ctrl Pts',(-19.9357852426788,-44.4748987787801,
124.496793284832)) ;
#77946 = CARTESIAN_POINT('Ctrl Pts',(-20.2900606909921,-44.6647552138203,
124.635070010774)) ;
#77947 = CARTESIAN_POINT('Ctrl Pts',(-20.1138908853131,-44.4847661334015,
124.390426455139)) ;
#77948 = CARTESIAN_POINT('Ctrl Pts',(-20.4886282484317,-44.6747211071184,
124.464326907959)) ;
#77949 = CARTESIAN_POINT('Ctrl Pts',(-20.2727462890408,-44.4947320266996,
124.253833725483)) ;
#77950 = CARTESIAN_POINT('Ctrl Pts',(-20.6553026894902,-44.6847448844945,
124.26032841296)) ;
#77951 = CARTESIAN_POINT('Ctrl Pts',(-20.4060875193306,-44.5047558040757,
124.090636341466)) ;
#77952 = CARTESIAN_POINT('Ctrl Pts',(-20.7828007334858,-44.6946704324262,
124.032794984421)) ;
#77953 = CARTESIAN_POINT('Ctrl Pts',(-20.5080877807566,-44.5146813520074,
123.908610839297)) ;
#77954 = CARTESIAN_POINT('Ctrl Pts',(-20.8695762748802,-44.7046109088472,
123.786387153768)) ;
#77955 = CARTESIAN_POINT('Ctrl Pts',(-20.5775102739201,-44.5246218284284,
123.711485441995)) ;
#77956 = CARTESIAN_POINT('Ctrl Pts',(-20.9124006494163,-44.7146571185101,
123.525895807859)) ;
#77957 = CARTESIAN_POINT('Ctrl Pts',(-20.6117719585213,-44.5346680380913,
123.503092741529)) ;
#77958 = CARTESIAN_POINT('Ctrl Pts',(-20.9096780312337,-44.7245183751719,
123.266743788831)) ;
#77959 = CARTESIAN_POINT('Ctrl Pts',(-20.6095960943389,-44.5445292947531,
123.295771314812)) ;
#77960 = CARTESIAN_POINT('Ctrl Pts',(-20.8618140136245,-44.7345120034472,
123.008558951092)) ;
#77961 = CARTESIAN_POINT('Ctrl Pts',(-20.5713071019526,-44.5545229230284,
123.089223095259)) ;
#77962 = CARTESIAN_POINT('Ctrl Pts',(-20.7705763698278,-44.7444374007574,
122.764165937538)) ;
#77963 = CARTESIAN_POINT('Ctrl Pts',(-20.498319127258,-44.5644483203386,122.893707997254)) ;
#77964 = CARTESIAN_POINT('Ctrl Pts',(-20.6369673170005,-44.7544653086676,
122.537064718107)) ;
#77965 = CARTESIAN_POINT('Ctrl Pts',(-20.3914338502099,-44.5744762282489,
122.712025924337)) ;
#77966 = CARTESIAN_POINT('Ctrl Pts',(-20.468527288973,-44.7643516243368,122.339213894273)) ;
#77967 = CARTESIAN_POINT('Ctrl Pts',(-20.2566836019861,-44.584362543918,122.553743877924)) ;
#77968 = CARTESIAN_POINT('Ctrl Pts',(-20.2655021978524,-44.7743832192406,
122.171124667689)) ;
#77969 = CARTESIAN_POINT('Ctrl Pts',(-20.0942650101056,-44.5943941388218,
122.419270793338)) ;
#77970 = CARTESIAN_POINT('Ctrl Pts',(-20.0398318506842,-44.7842654621923,
122.042531241713)) ;
#77971 = CARTESIAN_POINT('Ctrl Pts',(-19.9137298912166,-44.6042763817735,
122.316394121493)) ;
#77972 = CARTESIAN_POINT('Ctrl Pts',(-19.7909809655127,-44.7943249332221,
121.953425884344)) ;
#77973 = CARTESIAN_POINT('Ctrl Pts',(-19.7146500072838,-44.6143358528034,
122.24510773456)) ;
#77974 = CARTESIAN_POINT('Ctrl Pts',(-19.535389413835,-44.8041913778853,121.90976454012)) ;
#77975 = CARTESIAN_POINT('Ctrl Pts',(-19.5101771563229,-44.6242022974665,
122.210176441665)) ;
#77976 = CARTESIAN_POINT('Ctrl Pts',(-19.2734974473608,-44.8141575023339,
121.910332881199)) ;
#77977 = CARTESIAN_POINT('Ctrl Pts',(-19.300663601662,-44.6341684219152,122.210628864892)) ;
#77978 = CARTESIAN_POINT('Ctrl Pts',(-19.0140941941799,-44.8241877457251,
121.957079096009)) ;
#77979 = CARTESIAN_POINT('Ctrl Pts',(-19.0931406459017,-44.6441986653064,
122.248023646285)) ;
#77980 = CARTESIAN_POINT('Ctrl Pts',(-18.7699778546142,-44.8340807806781,
122.046571668305)) ;
#77981 = CARTESIAN_POINT('Ctrl Pts',(-18.8978469009694,-44.6540917002594,
122.319615481204)) ;
#77982 = CARTESIAN_POINT('Ctrl Pts',(-18.5415249218086,-44.844131694915,122.179088598148)) ;
#77983 = CARTESIAN_POINT('Ctrl Pts',(-18.7150830028236,-44.6641426144963,
122.425627556527)) ;
#77984 = CARTESIAN_POINT('Ctrl Pts',(-18.3427444001269,-44.8540215211396,
122.346531093199)) ;
#77985 = CARTESIAN_POINT('Ctrl Pts',(-18.5560590226922,-44.6740324407208,
122.55957796272)) ;
#77986 = CARTESIAN_POINT('Ctrl Pts',(-18.1174461021074,-44.8673563361865,
122.614979486974)) ;
#77987 = CARTESIAN_POINT('Ctrl Pts',(-18.3758085267228,-44.6873672557678,
122.774344354257)) ;
#77988 = CARTESIAN_POINT('Ctrl Pts',(-17.9686335760007,-44.880633427358,122.934896659111)) ;
#77989 = CARTESIAN_POINT('Ctrl Pts',(-18.2567530298792,-44.7006443469392,
123.030306574973)) ;
#77990 = CARTESIAN_POINT('Ctrl Pts',(-17.9076731561745,-44.8938817159563,
123.277709414337)) ;
#77991 = CARTESIAN_POINT('Ctrl Pts',(-18.2079946998203,-44.7138926355375,
123.304511413503)) ;
#77992 = CARTESIAN_POINT('Ctrl Pts',(-17.907462316396,-44.9039365574504,123.541899571291)) ;
#77993 = CARTESIAN_POINT('Ctrl Pts',(-18.2078213171443,-44.7239474770316,
123.515872463229)) ;
#77994 = CARTESIAN_POINT('Ctrl Pts',(-17.9516919898159,-44.9137675467579,
123.796479325877)) ;
#77995 = CARTESIAN_POINT('Ctrl Pts',(-18.2432033587368,-44.7337784663392,
123.719534329518)) ;
#77996 = CARTESIAN_POINT('Ctrl Pts',(-18.0414310832695,-44.9238441110811,
124.045563596341)) ;
#77997 = CARTESIAN_POINT('Ctrl Pts',(-18.3149935556506,-44.7438550306624,
123.918803730498)) ;
#77998 = CARTESIAN_POINT('Ctrl Pts',(-18.1701298254972,-44.9336934362151,
124.270160085641)) ;
#77999 = CARTESIAN_POINT('Ctrl Pts',(-18.4179464132743,-44.7537043557963,
124.098479058977)) ;
#78000 = CARTESIAN_POINT('Ctrl Pts',(-18.3940753258165,-44.9470414358523,
124.540160290247)) ;
#78001 = CARTESIAN_POINT('Ctrl Pts',(-18.5971230250769,-44.7670523554336,
124.314496251429)) ;
#78002 = CARTESIAN_POINT('Ctrl Pts',(-18.7539725180516,-44.9636261953889,
124.794623795702)) ;
#78003 = CARTESIAN_POINT('Ctrl Pts',(-18.8849990055932,-44.7836371149701,
124.518050456276)) ;
#78004 = CARTESIAN_POINT('Ctrl Pts',(-19.1783954642858,-44.980194746737,124.911954796684)) ;
#78005 = CARTESIAN_POINT('Ctrl Pts',(-19.2246019623236,-44.8002056663183,
124.611932785891)) ;
#78006 = CARTESIAN_POINT('Ctrl Pts',(-19.5295000394713,-44.993554571556,124.914496420858)) ;
#78007 = CARTESIAN_POINT('Ctrl Pts',(-19.5054328311711,-44.8135654911373,
124.613960044086)) ;
#78008 = CARTESIAN_POINT('Ctrl Pts',(-19.7862085515655,-45.0034599803866,
124.871351922851)) ;
#78009 = CARTESIAN_POINT('Ctrl Pts',(-19.7108114579357,-44.8234708999679,
124.579447577859)) ;
#78010 = CARTESIAN_POINT('Ctrl Pts',(-20.032977047638,-45.0134200069707,124.784181635909)) ;
#78011 = CARTESIAN_POINT('Ctrl Pts',(-19.9082219143351,-44.833430926552,124.509714796774)) ;
#78012 = CARTESIAN_POINT('Ctrl Pts',(-20.3365929404085,-45.026677591156,124.613239797364)) ;
#78013 = CARTESIAN_POINT('Ctrl Pts',(-20.151128683135,-44.8466885107373,124.372952796465)) ;
#78014 = CARTESIAN_POINT('Ctrl Pts',(-20.6530388479444,-45.0433288026507,
124.303846929817)) ;
#78015 = CARTESIAN_POINT('Ctrl Pts',(-20.4042740591769,-44.8633397222319,
124.125452733239)) ;
#78016 = CARTESIAN_POINT('Ctrl Pts',(-20.8822225929633,-45.063247016761,123.826665489828)) ;
#78017 = CARTESIAN_POINT('Ctrl Pts',(-20.5876289589755,-44.8832579363422,
123.743704995004)) ;
#78018 = CARTESIAN_POINT('Ctrl Pts',(-20.9358462101618,-45.0831247799818,
123.300999284686)) ;
#78019 = CARTESIAN_POINT('Ctrl Pts',(-20.6305301436153,-44.9031356995631,
123.323172734801)) ;
#78020 = CARTESIAN_POINT('Ctrl Pts',(-20.8055712372193,-45.103137447769,122.785395465284)) ;
#78021 = CARTESIAN_POINT('Ctrl Pts',(-20.5263138314019,-44.9231483673502,
122.910688665346)) ;
#78022 = CARTESIAN_POINT('Ctrl Pts',(-20.5104525720228,-45.1229499704356,
122.349160972127)) ;
#78023 = CARTESIAN_POINT('Ctrl Pts',(-20.2902207745244,-44.9429608900168,
122.561698343085)) ;
#78024 = CARTESIAN_POINT('Ctrl Pts',(-20.0811678726187,-45.1429332704355,
122.036595982183)) ;
#78025 = CARTESIAN_POINT('Ctrl Pts',(-19.946794629083,-44.9629441900167,122.311643931763)) ;
#78026 = CARTESIAN_POINT('Ctrl Pts',(-19.57298082711,-45.1628275475368,121.890260817319)) ;
#78027 = CARTESIAN_POINT('Ctrl Pts',(-19.5402450431835,-44.982838467118,122.194572859151)) ;
#78028 = CARTESIAN_POINT('Ctrl Pts',(-19.0443792387932,-45.1827603092946,
121.925363493161)) ;
#78029 = CARTESIAN_POINT('Ctrl Pts',(-19.1173630609288,-45.0027712288758,
122.222652560923)) ;
#78030 = CARTESIAN_POINT('Ctrl Pts',(-18.5588123388125,-45.2027263150593,
122.139444767392)) ;
#78031 = CARTESIAN_POINT('Ctrl Pts',(-18.7289082955966,-45.0227372346405,
122.393915435072)) ;
#78032 = CARTESIAN_POINT('Ctrl Pts',(-18.1768400074988,-45.2226048472241,
122.504512707819)) ;
#78033 = CARTESIAN_POINT('Ctrl Pts',(-18.4233281318735,-45.0426157668054,
122.685968958821)) ;
#78034 = CARTESIAN_POINT('Ctrl Pts',(-17.9412382745813,-45.2425445138845,
122.97916517489)) ;
#78035 = CARTESIAN_POINT('Ctrl Pts',(-18.2348448067827,-45.0625554334657,
123.065690634958)) ;
#78036 = CARTESIAN_POINT('Ctrl Pts',(-17.8817201356207,-45.2624393885298,
123.504633155358)) ;
#78037 = CARTESIAN_POINT('Ctrl Pts',(-18.1872285519615,-45.0824503081111,
123.48606590208)) ;
#78038 = CARTESIAN_POINT('Ctrl Pts',(-18.0046155636141,-45.2823465278232,
124.01913650114)) ;
#78039 = CARTESIAN_POINT('Ctrl Pts',(-18.2855439122614,-45.1023574474044,
123.897669917515)) ;
#78040 = CARTESIAN_POINT('Ctrl Pts',(-18.295159268459,-45.3022570759017,124.461637555443)) ;
#78041 = CARTESIAN_POINT('Ctrl Pts',(-18.5179788419764,-45.1222679954829,
124.251671936744)) ;
#78042 = CARTESIAN_POINT('Ctrl Pts',(-18.7231289192016,-45.3223256612588,
124.779793280971)) ;
#78043 = CARTESIAN_POINT('Ctrl Pts',(-18.8603532666718,-45.1423365808401,
124.506196853283)) ;
#78044 = CARTESIAN_POINT('Ctrl Pts',(-19.2267990765267,-45.3421074585736,
124.931211593248)) ;
#78045 = CARTESIAN_POINT('Ctrl Pts',(-19.2632917257971,-45.1621183781549,
124.627332840506)) ;
#78046 = CARTESIAN_POINT('Ctrl Pts',(-19.7575625515269,-45.3621150055181,
124.902127405281)) ;
#78047 = CARTESIAN_POINT('Ctrl Pts',(-19.6879025560016,-45.1821259250994,
124.604065538221)) ;
#78048 = CARTESIAN_POINT('Ctrl Pts',(-20.2423289587941,-45.381936743821,124.695488931226)) ;
#78049 = CARTESIAN_POINT('Ctrl Pts',(-20.0757176520892,-45.2019476634022,
124.438753696871)) ;
#78050 = CARTESIAN_POINT('Ctrl Pts',(-20.6310564600135,-45.4019167637251,
124.333814619523)) ;
#78051 = CARTESIAN_POINT('Ctrl Pts',(-20.3866992414769,-45.2219276833064,
124.149413465804)) ;
#78052 = CARTESIAN_POINT('Ctrl Pts',(-20.8717000556849,-45.4218342149874,
123.862278018849)) ;
#78053 = CARTESIAN_POINT('Ctrl Pts',(-20.579213919715,-45.2418451345686,123.77218297004)) ;
#78054 = CARTESIAN_POINT('Ctrl Pts',(-20.9380767681867,-45.4417091361601,
123.338188475179)) ;
#78055 = CARTESIAN_POINT('Ctrl Pts',(-20.6323140215928,-45.2617200557413,
123.352909817565)) ;
#78056 = CARTESIAN_POINT('Ctrl Pts',(-20.8204289202188,-45.4617335047109,
122.819174892969)) ;
#78057 = CARTESIAN_POINT('Ctrl Pts',(-20.5381943820615,-45.2817444242922,
122.937699557393)) ;
#78058 = CARTESIAN_POINT('Ctrl Pts',(-20.5348026192867,-45.4816001890844,
122.374971928314)) ;
#78059 = CARTESIAN_POINT('Ctrl Pts',(-20.3096913007445,-45.3016111086656,
122.582336913759)) ;
#78060 = CARTESIAN_POINT('Ctrl Pts',(-20.1137378287957,-45.5015440109306,
122.053072103638)) ;
#78061 = CARTESIAN_POINT('Ctrl Pts',(-19.9728377986509,-45.3215549305118,
122.324818360673)) ;
#78062 = CARTESIAN_POINT('Ctrl Pts',(-19.6089136734413,-45.5214513801821,
121.894620584334)) ;
#78063 = CARTESIAN_POINT('Ctrl Pts',(-19.5689770139582,-45.3414622997634,
122.198058922414)) ;
#78064 = CARTESIAN_POINT('Ctrl Pts',(-19.0811541092008,-45.5413260779288,
121.916926618905)) ;
#78065 = CARTESIAN_POINT('Ctrl Pts',(-19.1467684454857,-45.3613369975101,
122.215906404225)) ;
#78066 = CARTESIAN_POINT('Ctrl Pts',(-18.58996630322,-45.5613080204505,122.1189694923)) ;
#78067 = CARTESIAN_POINT('Ctrl Pts',(-18.7538191655351,-45.3813189400318,
122.377543293856)) ;
#78068 = CARTESIAN_POINT('Ctrl Pts',(-18.1991325995825,-45.5812106873614,
122.475351878696)) ;
#78069 = CARTESIAN_POINT('Ctrl Pts',(-18.4411535104022,-45.4012216069426,
122.662651767787)) ;
#78070 = CARTESIAN_POINT('Ctrl Pts',(-17.9525130135342,-45.6010660449001,
122.941989689351)) ;
#78071 = CARTESIAN_POINT('Ctrl Pts',(-18.2438603264457,-45.4210769644813,
123.035964382293)) ;
#78072 = CARTESIAN_POINT('Ctrl Pts',(-17.8797853305759,-45.6211300836161,
123.470193368156)) ;
#78073 = CARTESIAN_POINT('Ctrl Pts',(-18.1856815073262,-45.4411410031973,
123.458527308833)) ;
#78074 = CARTESIAN_POINT('Ctrl Pts',(-17.9907738385285,-45.6409852633412,
123.986308188062)) ;
#78075 = CARTESIAN_POINT('Ctrl Pts',(-18.2744755604141,-45.4609961829224,
123.871419313323)) ;
#78076 = CARTESIAN_POINT('Ctrl Pts',(-18.2724161799127,-45.6609653680056,
124.43626592713)) ;
#78077 = CARTESIAN_POINT('Ctrl Pts',(-18.4997930441946,-45.4809762875868,
124.231383659367)) ;
#78078 = CARTESIAN_POINT('Ctrl Pts',(-18.6870078951733,-45.6807744731754,
124.761025281419)) ;
#78079 = CARTESIAN_POINT('Ctrl Pts',(-18.8314673456426,-45.5007853927566,
124.491189117074)) ;
#78080 = CARTESIAN_POINT('Ctrl Pts',(-19.1916999501291,-45.7007670935161,
124.926741074953)) ;
#78081 = CARTESIAN_POINT('Ctrl Pts',(-19.235230041018,-45.5207780130973,124.623756847041)) ;
#78082 = CARTESIAN_POINT('Ctrl Pts',(-19.6312118173509,-45.7173065760202,
124.913196410059)) ;
#78083 = CARTESIAN_POINT('Ctrl Pts',(-19.5868155436623,-45.5373174956014,
124.612921459841)) ;
#78084 = CARTESIAN_POINT('Ctrl Pts',(-19.967499356913,-45.7306708940844,124.812112387731)) ;
#78085 = CARTESIAN_POINT('Ctrl Pts',(-19.8558719099428,-45.5506818136656,
124.532044502846)) ;
#78086 = CARTESIAN_POINT('Ctrl Pts',(-20.2779790595161,-45.7438884965859,
124.656227492498)) ;
#78087 = CARTESIAN_POINT('Ctrl Pts',(-20.1042094374621,-45.5638994161671,
124.407362610249)) ;
#78088 = CARTESIAN_POINT('Ctrl Pts',(-20.6088613726439,-45.7605460908637,
124.362235325812)) ;
#78089 = CARTESIAN_POINT('Ctrl Pts',(-20.3689615158667,-45.5805570104449,
124.172135807522)) ;
#78090 = CARTESIAN_POINT('Ctrl Pts',(-20.8603771682476,-45.7804117929054,
123.897882286003)) ;
#78091 = CARTESIAN_POINT('Ctrl Pts',(-20.5701552926539,-45.6004227124867,
123.800652558022)) ;
#78092 = CARTESIAN_POINT('Ctrl Pts',(-20.9262145452714,-45.7970415195954,
123.460911151539)) ;
#78093 = CARTESIAN_POINT('Ctrl Pts',(-20.6228240067414,-45.6170524391767,
123.451100564137)) ;
#78094 = CARTESIAN_POINT('Ctrl Pts',(-20.8869828200651,-45.8103306347333,
123.113835882206)) ;
#78095 = CARTESIAN_POINT('Ctrl Pts',(-20.5914361114732,-45.6303415543145,
123.17341573683)) ;
#78096 = CARTESIAN_POINT('Ctrl Pts',(-20.8131372217182,-45.8202949817104,
122.862628158014)) ;
#78097 = CARTESIAN_POINT('Ctrl Pts',(-20.532359431995,-45.6403059012916,122.97245700907)) ;
#78098 = CARTESIAN_POINT('Ctrl Pts',(-20.6973720959794,-45.8302233497119,
122.628822672063)) ;
#78099 = CARTESIAN_POINT('Ctrl Pts',(-20.4397374777452,-45.6502342692931,
122.785404651052)) ;
#78100 = CARTESIAN_POINT('Ctrl Pts',(-20.4910362460861,-45.8435067828006,
122.34720320038)) ;
#78101 = CARTESIAN_POINT('Ctrl Pts',(-20.2747057229162,-45.6635177023819,
122.560148879039)) ;
#78102 = CARTESIAN_POINT('Ctrl Pts',(-20.1458260850277,-45.8601588605409,
122.070280119453)) ;
#78103 = CARTESIAN_POINT('Ctrl Pts',(-19.9984819208062,-45.6801697801222,
122.338567916265)) ;
#78104 = CARTESIAN_POINT('Ctrl Pts',(-19.7294257177757,-45.8767102298418,
121.928426697249)) ;
#78105 = CARTESIAN_POINT('Ctrl Pts',(-19.6654083759465,-45.696721149423,122.22511130924)) ;
#78106 = CARTESIAN_POINT('Ctrl Pts',(-19.3810452958552,-45.8899976579907,
121.904492705502)) ;
#78107 = CARTESIAN_POINT('Ctrl Pts',(-19.386670912546,-45.710008577572,122.205956446535)) ;
#78108 = CARTESIAN_POINT('Ctrl Pts',(-19.1186091401468,-45.9000421976908,
121.932658290934)) ;
#78109 = CARTESIAN_POINT('Ctrl Pts',(-19.1767289258844,-45.7200531172721,
122.228493281736)) ;
#78110 = CARTESIAN_POINT('Ctrl Pts',(-18.8700233534811,-45.9098850395147,
122.004195045043)) ;
#78111 = CARTESIAN_POINT('Ctrl Pts',(-18.9778591118884,-45.7298959590959,
122.285724283644)) ;
#78112 = CARTESIAN_POINT('Ctrl Pts',(-18.6340661749748,-45.9198693237616,
122.118877741104)) ;
#78113 = CARTESIAN_POINT('Ctrl Pts',(-18.7890948938155,-45.7398802433429,
122.377472601013)) ;
#78114 = CARTESIAN_POINT('Ctrl Pts',(-18.4223444457329,-45.9298189691608,
122.272320772544)) ;
#78115 = CARTESIAN_POINT('Ctrl Pts',(-18.6197187508759,-45.749829888742,122.500228781122)) ;
#78116 = CARTESIAN_POINT('Ctrl Pts',(-18.2393318882481,-45.9398187308492,
122.460918444128)) ;
#78117 = CARTESIAN_POINT('Ctrl Pts',(-18.4733104024896,-45.7598296504304,
122.65110845724)) ;
#78118 = CARTESIAN_POINT('Ctrl Pts',(-18.0917505486385,-45.9498500768081,
122.679344429102)) ;
#78119 = CARTESIAN_POINT('Ctrl Pts',(-18.3552472195982,-45.7698609963893,
122.825850469655)) ;
#78120 = CARTESIAN_POINT('Ctrl Pts',(-17.9858757131845,-45.9597050312852,
122.915697061974)) ;
#78121 = CARTESIAN_POINT('Ctrl Pts',(-18.2705494534768,-45.7797159508665,
123.014933412963)) ;
#78122 = CARTESIAN_POINT('Ctrl Pts',(-17.9213083460047,-45.9696775692857,
123.169658598785)) ;
#78123 = CARTESIAN_POINT('Ctrl Pts',(-18.218897762685,-45.789688488867,123.218103106479)) ;
#78124 = CARTESIAN_POINT('Ctrl Pts',(-17.9017881316043,-45.9796725630207,
123.431630618321)) ;
#78125 = CARTESIAN_POINT('Ctrl Pts',(-18.2032838339912,-45.7996834826019,
123.427680825471)) ;
#78126 = CARTESIAN_POINT('Ctrl Pts',(-17.9284695514912,-45.9897066218148,
123.693939039822)) ;
#78127 = CARTESIAN_POINT('Ctrl Pts',(-18.2246312126076,-45.809717541396,123.637527304085)) ;
#78128 = CARTESIAN_POINT('Ctrl Pts',(-17.9986278341986,-45.9995619646378,
123.943270201428)) ;
#78129 = CARTESIAN_POINT('Ctrl Pts',(-18.2807599457767,-45.819572884219,123.83699144443)) ;
#78130 = CARTESIAN_POINT('Ctrl Pts',(-18.1123057056129,-46.0095614439834,
124.180132595311)) ;
#78131 = CARTESIAN_POINT('Ctrl Pts',(-18.3717042256828,-45.8295723635646,
124.026480327799)) ;
#78132 = CARTESIAN_POINT('Ctrl Pts',(-18.2635910838051,-46.0194558927387,
124.391666206139)) ;
#78133 = CARTESIAN_POINT('Ctrl Pts',(-18.4927342046914,-45.8394668123199,
124.195705758367)) ;
#78134 = CARTESIAN_POINT('Ctrl Pts',(-18.452459857194,-46.0295190121732,124.576699295131)) ;
#78135 = CARTESIAN_POINT('Ctrl Pts',(-18.6438307990039,-45.8495299317544,
124.343730662622)) ;
#78136 = CARTESIAN_POINT('Ctrl Pts',(-18.6656547762832,-46.0393586574144,
124.72309430415)) ;
#78137 = CARTESIAN_POINT('Ctrl Pts',(-18.8143877068013,-45.8593695769957,
124.460844668667)) ;
#78138 = CARTESIAN_POINT('Ctrl Pts',(-18.9061641632202,-46.0494218216005,
124.832954725834)) ;
#78139 = CARTESIAN_POINT('Ctrl Pts',(-19.0067961563735,-45.8694327411817,
124.5487310367)) ;
#78140 = CARTESIAN_POINT('Ctrl Pts',(-19.1579188976932,-46.0593160913493,
124.898075179744)) ;
#78141 = CARTESIAN_POINT('Ctrl Pts',(-19.2082002369437,-45.8793270109305,
124.600825207935)) ;
#78142 = CARTESIAN_POINT('Ctrl Pts',(-19.4182795982726,-46.0692578173631,
124.919290922773)) ;
#78143 = CARTESIAN_POINT('Ctrl Pts',(-19.4164887608804,-45.8892687369444,
124.617795648672)) ;
#78144 = CARTESIAN_POINT('Ctrl Pts',(-19.6800549446115,-46.0792607060225,
124.894933738413)) ;
#78145 = CARTESIAN_POINT('Ctrl Pts',(-19.6259087706948,-45.8992716256037,
124.598307788373)) ;
#78146 = CARTESIAN_POINT('Ctrl Pts',(-19.9343703358669,-46.0893005548165,
124.824788939951)) ;
#78147 = CARTESIAN_POINT('Ctrl Pts',(-19.8293605316926,-45.9093114743977,
124.542189846149)) ;
#78148 = CARTESIAN_POINT('Ctrl Pts',(-20.1678185634453,-46.0991247702773,
124.714495173591)) ;
#78149 = CARTESIAN_POINT('Ctrl Pts',(-20.0161177505501,-45.9191356898586,
124.453953133522)) ;
#78150 = CARTESIAN_POINT('Ctrl Pts',(-20.3837390423847,-46.1091816137709,
124.56213586375)) ;
#78151 = CARTESIAN_POINT('Ctrl Pts',(-20.1888529869787,-45.9291925333521,
124.332063944319)) ;
#78152 = CARTESIAN_POINT('Ctrl Pts',(-20.5673296044637,-46.1191102231669,
124.376727071072)) ;
#78153 = CARTESIAN_POINT('Ctrl Pts',(-20.3357237457142,-45.9391211427481,
124.183735605175)) ;
#78154 = CARTESIAN_POINT('Ctrl Pts',(-20.7168895336448,-46.1290621072048,
124.162174745033)) ;
#78155 = CARTESIAN_POINT('Ctrl Pts',(-20.4553698831515,-45.949073026786,124.012092764765)) ;
#78156 = CARTESIAN_POINT('Ctrl Pts',(-20.8275975548222,-46.1391150600124,
123.92232919589)) ;
#78157 = CARTESIAN_POINT('Ctrl Pts',(-20.5439344348876,-45.9591259795936,
123.820215369618)) ;
#78158 = CARTESIAN_POINT('Ctrl Pts',(-20.8939114403287,-46.1489379364785,
123.672837152812)) ;
#78159 = CARTESIAN_POINT('Ctrl Pts',(-20.5969834127684,-45.9689488560598,
123.620621818295)) ;
#78160 = CARTESIAN_POINT('Ctrl Pts',(-20.9168785395535,-46.1589936690487,
123.409601144835)) ;
#78161 = CARTESIAN_POINT('Ctrl Pts',(-20.6153551246797,-45.9790045886299,
123.410032751232)) ;
#78162 = CARTESIAN_POINT('Ctrl Pts',(-20.8935915401081,-46.1689344340363,
123.14939855817)) ;
#78163 = CARTESIAN_POINT('Ctrl Pts',(-20.5967235160762,-45.9889453536176,
123.201871130652)) ;
#78164 = CARTESIAN_POINT('Ctrl Pts',(-20.8265158341053,-46.178838766942,122.897909377588)) ;
#78165 = CARTESIAN_POINT('Ctrl Pts',(-20.5430611920399,-45.9988496865232,
123.000680697245)) ;
#78166 = CARTESIAN_POINT('Ctrl Pts',(-20.7150751052144,-46.1888854358227,
122.65859044673)) ;
#78167 = CARTESIAN_POINT('Ctrl Pts',(-20.4539067994353,-46.0088963554039,
122.809226303556)) ;
#78168 = CARTESIAN_POINT('Ctrl Pts',(-20.5662066576584,-46.1987809991285,
122.445321690462)) ;
#78169 = CARTESIAN_POINT('Ctrl Pts',(-20.3348107319398,-46.0187919187097,
122.638612781793)) ;
#78170 = CARTESIAN_POINT('Ctrl Pts',(-20.3795364262212,-46.2088430568288,
122.2580991555)) ;
#78171 = CARTESIAN_POINT('Ctrl Pts',(-20.1854730795545,-46.02885397641,122.488836010064)) ;
#78172 = CARTESIAN_POINT('Ctrl Pts',(-20.1679385536173,-46.2186858344563,
122.109285146135)) ;
#78173 = CARTESIAN_POINT('Ctrl Pts',(-20.0161942548949,-46.0386967540375,
122.369786757822)) ;
#78174 = CARTESIAN_POINT('Ctrl Pts',(-19.9305238988676,-46.2286763127081,
121.997288664803)) ;
#78175 = CARTESIAN_POINT('Ctrl Pts',(-19.8262618842319,-46.0486872322894,
122.280191270744)) ;
#78176 = CARTESIAN_POINT('Ctrl Pts',(-19.6787697821967,-46.2386052853517,
121.928664786083)) ;
#78177 = CARTESIAN_POINT('Ctrl Pts',(-19.6248584943409,-46.0586162049329,
122.225294020736)) ;
#78178 = CARTESIAN_POINT('Ctrl Pts',(-19.4173499655244,-46.2485964222312,
121.904240994582)) ;
#78179 = CARTESIAN_POINT('Ctrl Pts',(-19.4157226100633,-46.0686073418125,
122.205756739917)) ;
#78180 = CARTESIAN_POINT('Ctrl Pts',(-19.1548721753353,-46.2586185397202,
121.925962509157)) ;
#78181 = CARTESIAN_POINT('Ctrl Pts',(-19.2057405118503,-46.0786294593014,
122.22313574868)) ;
#78182 = CARTESIAN_POINT('Ctrl Pts',(-18.903182216174,-46.2685190501224,121.991878228726)) ;
#78183 = CARTESIAN_POINT('Ctrl Pts',(-19.0043894985658,-46.0885299697036,
122.275869893625)) ;
#78184 = CARTESIAN_POINT('Ctrl Pts',(-18.6644805817481,-46.2785080428685,
122.101090338697)) ;
#78185 = CARTESIAN_POINT('Ctrl Pts',(-18.8134290284549,-46.0985189624497,
122.363241059296)) ;
#78186 = CARTESIAN_POINT('Ctrl Pts',(-18.4489924496805,-46.2884732869191,
122.249880282416)) ;
#78187 = CARTESIAN_POINT('Ctrl Pts',(-18.6410397168517,-46.1084842065003,
122.482274286718)) ;
#78188 = CARTESIAN_POINT('Ctrl Pts',(-18.263300225065,-46.2983775514323,122.432284741279)) ;
#78189 = CARTESIAN_POINT('Ctrl Pts',(-18.4924874591841,-46.1183884710135,
122.628198618205)) ;
#78190 = CARTESIAN_POINT('Ctrl Pts',(-18.1099129936779,-46.3084356431305,
122.647513729993)) ;
#78191 = CARTESIAN_POINT('Ctrl Pts',(-18.3697789069092,-46.1284465627118,
122.800382913545)) ;
#78192 = CARTESIAN_POINT('Ctrl Pts',(-17.998387777928,-46.3182855835589,122.881119052178)) ;
#78193 = CARTESIAN_POINT('Ctrl Pts',(-18.2805605437885,-46.1382965031402,
122.98726711269)) ;
#78194 = CARTESIAN_POINT('Ctrl Pts',(-17.9272509866256,-46.3283125947325,
123.134829512523)) ;
#78195 = CARTESIAN_POINT('Ctrl Pts',(-18.2236525328705,-46.1483235143137,
123.190235911234)) ;
#78196 = CARTESIAN_POINT('Ctrl Pts',(-17.9019257693424,-46.3383411813445,
123.397163125625)) ;
#78197 = CARTESIAN_POINT('Ctrl Pts',(-18.2033939634236,-46.1583521009257,
123.400103012758)) ;
#78198 = CARTESIAN_POINT('Ctrl Pts',(-17.9216676871515,-46.3481863954572,
123.655117412468)) ;
#78199 = CARTESIAN_POINT('Ctrl Pts',(-18.2191889474225,-46.1681973150384,
123.606465432505)) ;
#78200 = CARTESIAN_POINT('Ctrl Pts',(-17.986172659598,-46.3581771436368,123.909622518297)) ;
#78201 = CARTESIAN_POINT('Ctrl Pts',(-18.2707942272682,-46.178188063218,123.810069025763)) ;
#78202 = CARTESIAN_POINT('Ctrl Pts',(-18.0949209307698,-46.3682147772222,
124.149940691099)) ;
#78203 = CARTESIAN_POINT('Ctrl Pts',(-18.3577942543388,-46.1882256968035,
124.002323042482)) ;
#78204 = CARTESIAN_POINT('Ctrl Pts',(-18.2405394895008,-46.3780600664351,
124.36379877282)) ;
#78205 = CARTESIAN_POINT('Ctrl Pts',(-18.4742897414031,-46.1980709860163,
124.173407939844)) ;
#78206 = CARTESIAN_POINT('Ctrl Pts',(-18.4231399413535,-46.3880414672409,
124.552075901783)) ;
#78207 = CARTESIAN_POINT('Ctrl Pts',(-18.6203708816344,-46.2080523868222,
124.324028590119)) ;
#78208 = CARTESIAN_POINT('Ctrl Pts',(-18.6350962163198,-46.3979937002309,
124.705303329943)) ;
#78209 = CARTESIAN_POINT('Ctrl Pts',(-18.7899363575204,-46.2180046198121,
124.446609255118)) ;
#78210 = CARTESIAN_POINT('Ctrl Pts',(-18.8714017008393,-46.4079925116875,
124.820247929174)) ;
#78211 = CARTESIAN_POINT('Ctrl Pts',(-18.9789811859863,-46.2280034312688,
124.538563781757)) ;
#78212 = CARTESIAN_POINT('Ctrl Pts',(-19.125198539865,-46.4180316156182,124.892209201569)) ;
#78213 = CARTESIAN_POINT('Ctrl Pts',(-19.1820191456136,-46.2380425351995,
124.596131542575)) ;
#78214 = CARTESIAN_POINT('Ctrl Pts',(-19.3820108279092,-46.4278565580375,
124.918993385685)) ;
#78215 = CARTESIAN_POINT('Ctrl Pts',(-19.387468008186,-46.2478674776188,124.61755756467)) ;
#78216 = CARTESIAN_POINT('Ctrl Pts',(-19.6455932892847,-46.4379112455134,
124.900789356812)) ;
#78217 = CARTESIAN_POINT('Ctrl Pts',(-19.5983341049394,-46.2579221650947,
124.602993203772)) ;
#78218 = CARTESIAN_POINT('Ctrl Pts',(-19.8990733415678,-46.4478540478703,
124.83736478161)) ;
#78219 = CARTESIAN_POINT('Ctrl Pts',(-19.8011174177466,-46.2678649674515,
124.552252461191)) ;
#78220 = CARTESIAN_POINT('Ctrl Pts',(-20.1370762828853,-46.45775784381,124.732039091005)) ;
#78221 = CARTESIAN_POINT('Ctrl Pts',(-19.9915187270784,-46.2777687633913,
124.467991228943)) ;
#78222 = CARTESIAN_POINT('Ctrl Pts',(-20.3561848751974,-46.4678046231851,
124.584777991466)) ;
#78223 = CARTESIAN_POINT('Ctrl Pts',(-20.1668051376118,-46.2878155427663,
124.350181357414)) ;
#78224 = CARTESIAN_POINT('Ctrl Pts',(-20.5437352890552,-46.4777002814797,
124.404584546191)) ;
#78225 = CARTESIAN_POINT('Ctrl Pts',(-20.3168442299365,-46.2977112010609,
124.206026364736)) ;
#78226 = CARTESIAN_POINT('Ctrl Pts',(-20.6997061795062,-46.4877618487303,
124.191114977076)) ;
#78227 = CARTESIAN_POINT('Ctrl Pts',(-20.4416202696434,-46.3077727683115,
124.035249895047)) ;
#78228 = CARTESIAN_POINT('Ctrl Pts',(-20.8137834733619,-46.4976064931676,
123.958907813351)) ;
#78229 = CARTESIAN_POINT('Ctrl Pts',(-20.5328807279198,-46.3176174127489,
123.849484665839)) ;
#78230 = CARTESIAN_POINT('Ctrl Pts',(-20.8875519245094,-46.5075665394103,
123.70778216214)) ;
#78231 = CARTESIAN_POINT('Ctrl Pts',(-20.5918946247474,-46.3275774589915,
123.648584272298)) ;
#78232 = CARTESIAN_POINT('Ctrl Pts',(-20.9163089328195,-46.5176048354286,
123.445571143075)) ;
#78233 = CARTESIAN_POINT('Ctrl Pts',(-20.6148993352014,-46.3376157550099,
123.438815228034)) ;
#78234 = CARTESIAN_POINT('Ctrl Pts',(-20.8998770458328,-46.527478176847,123.186591367231)) ;
#78235 = CARTESIAN_POINT('Ctrl Pts',(-20.6017530884054,-46.3474890964282,
123.231632356186)) ;
#78236 = CARTESIAN_POINT('Ctrl Pts',(-20.8374336991102,-46.5375512806463,
122.92940409919)) ;
#78237 = CARTESIAN_POINT('Ctrl Pts',(-20.5517975371544,-46.3575622002275,
123.025882403029)) ;
#78238 = CARTESIAN_POINT('Ctrl Pts',(-20.7341962066847,-46.5473720957652,
122.692815045751)) ;
#78239 = CARTESIAN_POINT('Ctrl Pts',(-20.4692073631793,-46.3673830153464,
122.836612591769)) ;
#78240 = CARTESIAN_POINT('Ctrl Pts',(-20.5880342150586,-46.5574489608432,
122.472055591204)) ;
#78241 = CARTESIAN_POINT('Ctrl Pts',(-20.3522770187593,-46.3774598804244,
122.660005096316)) ;
#78242 = CARTESIAN_POINT('Ctrl Pts',(-20.4094709147566,-46.5673137004984,
122.2840805988)) ;
#78243 = CARTESIAN_POINT('Ctrl Pts',(-20.2094265518685,-46.3873246200797,
122.509626284042)) ;
#78244 = CARTESIAN_POINT('Ctrl Pts',(-20.1980943114243,-46.5773361037398,
122.126973882659)) ;
#78245 = CARTESIAN_POINT('Ctrl Pts',(-20.0403249282567,-46.397347023321,122.383941308971)) ;
#78246 = CARTESIAN_POINT('Ctrl Pts',(-19.9622532730963,-46.5873618280283,
122.009494285036)) ;
#78247 = CARTESIAN_POINT('Ctrl Pts',(-19.8516517311113,-46.4073727476095,
122.289958211651)) ;
#78248 = CARTESIAN_POINT('Ctrl Pts',(-19.7140632034565,-46.5972166110496,
121.935594664528)) ;
#78249 = CARTESIAN_POINT('Ctrl Pts',(-19.6531005311567,-46.4172275306308,
122.230839367749)) ;
#78250 = CARTESIAN_POINT('Ctrl Pts',(-19.4536310994498,-46.6071954547728,
121.90485653267)) ;
#78251 = CARTESIAN_POINT('Ctrl Pts',(-19.4447550642986,-46.4272063743541,
122.206249292798)) ;
#78252 = CARTESIAN_POINT('Ctrl Pts',(-19.1908123744506,-46.6172143470095,
121.920317600712)) ;
#78253 = CARTESIAN_POINT('Ctrl Pts',(-19.2345001020312,-46.4372252665907,
122.218618661177)) ;
#78254 = CARTESIAN_POINT('Ctrl Pts',(-18.9379696063757,-46.6270975560505,
121.97984075854)) ;
#78255 = CARTESIAN_POINT('Ctrl Pts',(-19.0322268301204,-46.4471084756317,
122.266237355114)) ;
#78256 = CARTESIAN_POINT('Ctrl Pts',(-18.6949496716239,-46.6371658653907,
122.084353103982)) ;
#78257 = CARTESIAN_POINT('Ctrl Pts',(-18.8378107414872,-46.4571767849719,
122.349847736102)) ;
#78258 = CARTESIAN_POINT('Ctrl Pts',(-18.4787605240188,-46.6469959907234,
122.225836194855)) ;
#78259 = CARTESIAN_POINT('Ctrl Pts',(-18.6648606358559,-46.4670069103046,
122.463033810365)) ;
#78260 = CARTESIAN_POINT('Ctrl Pts',(-18.2857214965471,-46.6570625431004,
122.406651152133)) ;
#78261 = CARTESIAN_POINT('Ctrl Pts',(-18.5104293493474,-46.4770734626816,
122.607686172701)) ;
#78262 = CARTESIAN_POINT('Ctrl Pts',(-18.1298739185928,-46.6669527799941,
122.614687511518)) ;
#78263 = CARTESIAN_POINT('Ctrl Pts',(-18.3857520197668,-46.4869636995753,
122.774114761019)) ;
#78264 = CARTESIAN_POINT('Ctrl Pts',(-18.0108157652608,-46.6769450047881,
122.848713195594)) ;
#78265 = CARTESIAN_POINT('Ctrl Pts',(-18.2905057011773,-46.4969559243693,
122.96133522007)) ;
#78266 = CARTESIAN_POINT('Ctrl Pts',(-17.9346569101183,-46.686907625139,123.099193972025)) ;
#78267 = CARTESIAN_POINT('Ctrl Pts',(-18.2295789196735,-46.5069185447203,
123.161719551088)) ;
#78268 = CARTESIAN_POINT('Ctrl Pts',(-17.9026865141076,-46.6968126279022,
123.357534213857)) ;
#78269 = CARTESIAN_POINT('Ctrl Pts',(-18.2040027337092,-46.5168235474834,
123.368391006395)) ;
#78270 = CARTESIAN_POINT('Ctrl Pts',(-17.9164439567275,-46.7068703903003,
123.621460054298)) ;
#78271 = CARTESIAN_POINT('Ctrl Pts',(-18.2150087894346,-46.5268813098816,
123.579531944023)) ;
#78272 = CARTESIAN_POINT('Ctrl Pts',(-17.9743972614119,-46.7167209096791,
123.873771940595)) ;
#78273 = CARTESIAN_POINT('Ctrl Pts',(-18.2613712111539,-46.5367318292604,
123.781380349578)) ;
#78274 = CARTESIAN_POINT('Ctrl Pts',(-18.0765858906852,-46.7267524866773,
124.116760874198)) ;
#78275 = CARTESIAN_POINT('Ctrl Pts',(-18.343122043701,-46.5467634062585,123.97577162832)) ;
#78276 = CARTESIAN_POINT('Ctrl Pts',(-18.2195527491153,-46.7367622217822,
124.337596889002)) ;
#78277 = CARTESIAN_POINT('Ctrl Pts',(-18.4574955266173,-46.5567731413635,
124.15244040257)) ;
#78278 = CARTESIAN_POINT('Ctrl Pts',(-18.3966970018278,-46.7466717984085,
124.528446109124)) ;
#78279 = CARTESIAN_POINT('Ctrl Pts',(-18.5992104071735,-46.5666827179897,
124.30511928162)) ;
#78280 = CARTESIAN_POINT('Ctrl Pts',(-18.6042842737798,-46.7565991842651,
124.686473857412)) ;
#78281 = CARTESIAN_POINT('Ctrl Pts',(-18.7652796215495,-46.5766101038464,
124.431541287681)) ;
#78282 = CARTESIAN_POINT('Ctrl Pts',(-18.8389799600408,-46.7666441187554,
124.807271873862)) ;
#78283 = CARTESIAN_POINT('Ctrl Pts',(-18.9530362508393,-46.5866550383367,
124.528179918756)) ;
#78284 = CARTESIAN_POINT('Ctrl Pts',(-19.0870750670497,-46.7765300509434,
124.884401576639)) ;
#78285 = CARTESIAN_POINT('Ctrl Pts',(-19.1515114465665,-46.5965409705246,
124.589883612155)) ;
#78286 = CARTESIAN_POINT('Ctrl Pts',(-19.3475046537305,-46.7865233568964,
124.918084459539)) ;
#78287 = CARTESIAN_POINT('Ctrl Pts',(-19.3598549143501,-46.6065342764777,
124.616830206673)) ;
#78288 = CARTESIAN_POINT('Ctrl Pts',(-19.6085865454019,-46.7964689946783,
124.905990634187)) ;
#78289 = CARTESIAN_POINT('Ctrl Pts',(-19.5687199653506,-46.6164799142595,
124.607155453148)) ;
#78290 = CARTESIAN_POINT('Ctrl Pts',(-19.8637733414105,-46.8064162630242,
124.849258887839)) ;
#78291 = CARTESIAN_POINT('Ctrl Pts',(-19.7728690447604,-46.6264271826054,
124.561770566073)) ;
#78292 = CARTESIAN_POINT('Ctrl Pts',(-20.1075420667497,-46.8164641651613,
124.747800719741)) ;
#78293 = CARTESIAN_POINT('Ctrl Pts',(-19.9678843424592,-46.6364750847425,
124.480604273047)) ;
#78294 = CARTESIAN_POINT('Ctrl Pts',(-20.3256846822347,-46.8263118600015,
124.608569806592)) ;
#78295 = CARTESIAN_POINT('Ctrl Pts',(-20.1423977064483,-46.6463227795827,
124.369220481856)) ;
#78296 = CARTESIAN_POINT('Ctrl Pts',(-20.5190914281009,-46.8362733697459,
124.432171593208)) ;
#78297 = CARTESIAN_POINT('Ctrl Pts',(-20.297123242795,-46.6562842893271,124.2281026054)) ;
#78298 = CARTESIAN_POINT('Ctrl Pts',(-20.679753909111,-46.8463027613547,124.223227378261)) ;
#78299 = CARTESIAN_POINT('Ctrl Pts',(-20.42565368723,-46.666313680936,124.060947484944)) ;
#78300 = CARTESIAN_POINT('Ctrl Pts',(-20.8003366055936,-46.8562102569095,
123.992472885765)) ;
#78301 = CARTESIAN_POINT('Ctrl Pts',(-20.5221200032968,-46.6762211764908,
123.876344781865)) ;
#78302 = CARTESIAN_POINT('Ctrl Pts',(-20.8798121650525,-46.8661556485725,
123.743517316014)) ;
#78303 = CARTESIAN_POINT('Ctrl Pts',(-20.5857009581305,-46.6861665681538,
123.6771809766)) ;
#78304 = CARTESIAN_POINT('Ctrl Pts',(-20.9152146258605,-46.8761575661699,
123.483036674984)) ;
#78305 = CARTESIAN_POINT('Ctrl Pts',(-20.614023626857,-46.6961684857511,123.468796661138)) ;
#78306 = CARTESIAN_POINT('Ctrl Pts',(-20.9043274470116,-46.8861976337221,
123.219443241595)) ;
#78307 = CARTESIAN_POINT('Ctrl Pts',(-20.605314478917,-46.7062085533033,123.257921751627)) ;
#78308 = CARTESIAN_POINT('Ctrl Pts',(-20.8496146261628,-46.8960219451619,
122.967111685202)) ;
#78309 = CARTESIAN_POINT('Ctrl Pts',(-20.5615452065626,-46.7160328647431,
123.056057541106)) ;
#78310 = CARTESIAN_POINT('Ctrl Pts',(-20.7499690604386,-46.906078186318,122.722378927974)) ;
#78311 = CARTESIAN_POINT('Ctrl Pts',(-20.481829431188,-46.7260891058992,122.860270789842)) ;
#78312 = CARTESIAN_POINT('Ctrl Pts',(-20.6108065948764,-46.9160091080536,
122.501569334486)) ;
#78313 = CARTESIAN_POINT('Ctrl Pts',(-20.3705003850126,-46.7360200276349,
122.683623170689)) ;
#78314 = CARTESIAN_POINT('Ctrl Pts',(-20.4356383206303,-46.9259523441298,
122.307725777392)) ;
#78315 = CARTESIAN_POINT('Ctrl Pts',(-20.2303667445202,-46.7459632637111,
122.528548091162)) ;
#78316 = CARTESIAN_POINT('Ctrl Pts',(-20.2287819479569,-46.9359336281423,
122.146383450033)) ;
#78317 = CARTESIAN_POINT('Ctrl Pts',(-20.0648823935122,-46.7559445477236,
122.399473615786)) ;
#78318 = CARTESIAN_POINT('Ctrl Pts',(-19.9954418662729,-46.945977929768,122.02306909361)) ;
#78319 = CARTESIAN_POINT('Ctrl Pts',(-19.8782105832335,-46.7659888493492,
122.300821320702)) ;
#78320 = CARTESIAN_POINT('Ctrl Pts',(-19.7497569427487,-46.9558060109874,
121.943291660732)) ;
#78321 = CARTESIAN_POINT('Ctrl Pts',(-19.6816640439892,-46.7758169305687,
122.236998801319)) ;
#78322 = CARTESIAN_POINT('Ctrl Pts',(-19.4875976586558,-46.9658826138366,
121.906362635557)) ;
#78323 = CARTESIAN_POINT('Ctrl Pts',(-19.4719364151813,-46.7858935334178,
122.207454534728)) ;
#78324 = CARTESIAN_POINT('Ctrl Pts',(-19.2287886486828,-46.9757346929551,
121.915184765321)) ;
#78325 = CARTESIAN_POINT('Ctrl Pts',(-19.2648901580032,-46.7957456125364,
122.214511170181)) ;
#78326 = CARTESIAN_POINT('Ctrl Pts',(-18.9698079849052,-46.985807951264,121.969772870526)) ;
#78327 = CARTESIAN_POINT('Ctrl Pts',(-19.0577050887598,-46.8058188708453,
122.258180656131)) ;
#78328 = CARTESIAN_POINT('Ctrl Pts',(-18.7298606158463,-46.9956494106443,
122.066316849494)) ;
#78329 = CARTESIAN_POINT('Ctrl Pts',(-18.8657477611846,-46.8156603302256,
122.335414457744)) ;
#78330 = CARTESIAN_POINT('Ctrl Pts',(-18.507158497472,-47.0056105060567,122.203869923483)) ;
#78331 = CARTESIAN_POINT('Ctrl Pts',(-18.6875856641331,-46.8256214256379,
122.445455650075)) ;
#78332 = CARTESIAN_POINT('Ctrl Pts',(-18.3105700405973,-47.0156477904534,
122.379722097199)) ;
#78333 = CARTESIAN_POINT('Ctrl Pts',(-18.5303140387269,-46.8356587100347,
122.586136582411)) ;
#78334 = CARTESIAN_POINT('Ctrl Pts',(-18.1497383799776,-47.0255241291887,
122.583459652744)) ;
#78335 = CARTESIAN_POINT('Ctrl Pts',(-18.4016482050606,-46.8455350487699,
122.749125213228)) ;
#78336 = CARTESIAN_POINT('Ctrl Pts',(-18.0243973838488,-47.0355862553419,
122.816248967661)) ;
#78337 = CARTESIAN_POINT('Ctrl Pts',(-18.3013741678358,-46.8555971749232,
122.935356256442)) ;
#78338 = CARTESIAN_POINT('Ctrl Pts',(-17.942900261106,-47.0454544293185,123.062469015804)) ;
#78339 = CARTESIAN_POINT('Ctrl Pts',(-18.2361754986026,-46.8654653488997,
123.132331099916)) ;
#78340 = CARTESIAN_POINT('Ctrl Pts',(-17.9043551711864,-47.0554599778223,
123.322528432359)) ;
#78341 = CARTESIAN_POINT('Ctrl Pts',(-18.2053380449325,-46.8754708974035,
123.340378359643)) ;
#78342 = CARTESIAN_POINT('Ctrl Pts',(-17.9116262441301,-47.0654426097179,
123.584808795431)) ;
#78343 = CARTESIAN_POINT('Ctrl Pts',(-18.2111535111412,-46.8854535292991,
123.55020250964)) ;
#78344 = CARTESIAN_POINT('Ctrl Pts',(-17.9649058187744,-47.0754865521397,
123.843296984573)) ;
#78345 = CARTESIAN_POINT('Ctrl Pts',(-18.2537758946358,-46.8954974717209,
123.756993455038)) ;
#78346 = CARTESIAN_POINT('Ctrl Pts',(-18.0598529384755,-47.0853147001668,
124.083485382838)) ;
#78347 = CARTESIAN_POINT('Ctrl Pts',(-18.3297319083217,-46.9053256197481,
123.949143731469)) ;
#78348 = CARTESIAN_POINT('Ctrl Pts',(-18.1965689478695,-47.0953045675412,
124.307600675778)) ;
#78349 = CARTESIAN_POINT('Ctrl Pts',(-18.4391033021549,-46.9153154871225,
124.128436666438)) ;
#78350 = CARTESIAN_POINT('Ctrl Pts',(-18.3715713483997,-47.1053483064967,
124.505180389763)) ;
#78351 = CARTESIAN_POINT('Ctrl Pts',(-18.5791042261939,-46.925359226078,124.286501476418)) ;
#78352 = CARTESIAN_POINT('Ctrl Pts',(-18.5733188648225,-47.1151700550347,
124.666164420657)) ;
#78353 = CARTESIAN_POINT('Ctrl Pts',(-18.7405004989235,-46.9351809746159,
124.41528928464)) ;
#78354 = CARTESIAN_POINT('Ctrl Pts',(-18.8045645527925,-47.1252050326444,
124.792922450464)) ;
#78355 = CARTESIAN_POINT('Ctrl Pts',(-18.9254963238758,-46.9452159522256,
124.516697207204)) ;
#78356 = CARTESIAN_POINT('Ctrl Pts',(-19.0542980945305,-47.1352299454021,
124.87682516273)) ;
#78357 = CARTESIAN_POINT('Ctrl Pts',(-19.1252826902165,-46.9552408649833,
124.583820828544)) ;
#78358 = CARTESIAN_POINT('Ctrl Pts',(-19.3102255315823,-47.1450818884959,
124.915973694031)) ;
#78359 = CARTESIAN_POINT('Ctrl Pts',(-19.3300235960743,-46.9650928080772,
124.615141143761)) ;
#78360 = CARTESIAN_POINT('Ctrl Pts',(-19.5726863790216,-47.155072849825,124.910409512918)) ;
#78361 = CARTESIAN_POINT('Ctrl Pts',(-19.5399921733102,-46.9750837694063,
124.61069150596)) ;
#78362 = CARTESIAN_POINT('Ctrl Pts',(-19.8284072327493,-47.1649907246935,
124.859887472804)) ;
#78363 = CARTESIAN_POINT('Ctrl Pts',(-19.7445687433349,-46.9850016442747,
124.570275659941)) ;
#78364 = CARTESIAN_POINT('Ctrl Pts',(-20.0741511052673,-47.1750192436947,
124.764752235733)) ;
#78365 = CARTESIAN_POINT('Ctrl Pts',(-19.9411644966269,-46.9950301632759,
124.494169084387)) ;
#78366 = CARTESIAN_POINT('Ctrl Pts',(-20.2964844790249,-47.1849029224925,
124.630459757741)) ;
#78367 = CARTESIAN_POINT('Ctrl Pts',(-20.1190316002392,-47.0049138420738,
124.386736915918)) ;
#78368 = CARTESIAN_POINT('Ctrl Pts',(-20.4946972414239,-47.1948978659322,
124.45812275425)) ;
#78369 = CARTESIAN_POINT('Ctrl Pts',(-20.2776029447661,-47.0149087855135,
124.248868788224)) ;
#78370 = CARTESIAN_POINT('Ctrl Pts',(-20.6601527761512,-47.2049247197547,
124.253049913834)) ;
#78371 = CARTESIAN_POINT('Ctrl Pts',(-20.4099687724888,-47.0249356393359,
124.084811622413)) ;
#78372 = CARTESIAN_POINT('Ctrl Pts',(-20.7859931801088,-47.2148088840936,
124.025810555401)) ;
#78373 = CARTESIAN_POINT('Ctrl Pts',(-20.5106424360365,-47.0348198036749,
123.90302151066)) ;
#78374 = CARTESIAN_POINT('Ctrl Pts',(-20.8716717235175,-47.224796982136,123.777738571877)) ;
#78375 = CARTESIAN_POINT('Ctrl Pts',(-20.5791870192374,-47.0448079017172,
123.704564663885)) ;
#78376 = CARTESIAN_POINT('Ctrl Pts',(-20.9129754353913,-47.2347480885931,
123.519483140435)) ;
#78377 = CARTESIAN_POINT('Ctrl Pts',(-20.6122318336066,-47.0547590081743,
123.497960883868)) ;
#78378 = CARTESIAN_POINT('Ctrl Pts',(-20.9086243004651,-47.2447931397612,
123.255561025819)) ;
#78379 = CARTESIAN_POINT('Ctrl Pts',(-20.6087528155346,-47.0648040593424,
123.286823089854)) ;
#78380 = CARTESIAN_POINT('Ctrl Pts',(-20.8595658746091,-47.2546549001195,
123.001088343686)) ;
#78381 = CARTESIAN_POINT('Ctrl Pts',(-20.5695080656259,-47.0746658197007,
123.083245164195)) ;
#78382 = CARTESIAN_POINT('Ctrl Pts',(-20.7668750533367,-47.2646177169499,
122.756231591788)) ;
#78383 = CARTESIAN_POINT('Ctrl Pts',(-20.4953573697405,-47.0846286365312,
122.887359233057)) ;
#78384 = CARTESIAN_POINT('Ctrl Pts',(-20.6317297454447,-47.2746523982307,
122.529807845328)) ;
#78385 = CARTESIAN_POINT('Ctrl Pts',(-20.3872427942103,-47.0946633178119,
122.706219207797)) ;
#78386 = CARTESIAN_POINT('Ctrl Pts',(-20.4621990513722,-47.2845374280114,
122.332938363935)) ;
#78387 = CARTESIAN_POINT('Ctrl Pts',(-20.2516200615866,-47.1045483475927,
122.548722648107)) ;
#78388 = CARTESIAN_POINT('Ctrl Pts',(-20.2574099722964,-47.2946030214095,
122.165588379843)) ;
#78389 = CARTESIAN_POINT('Ctrl Pts',(-20.0877899799016,-47.1146139409907,
122.414841027643)) ;
#78390 = CARTESIAN_POINT('Ctrl Pts',(-20.0319196600013,-47.304442189771,122.038978242799)) ;
#78391 = CARTESIAN_POINT('Ctrl Pts',(-19.9073992209969,-47.1244531093522,
122.313551415424)) ;
#78392 = CARTESIAN_POINT('Ctrl Pts',(-19.782518300832,-47.3145047875124,121.951182502159)) ;
#78393 = CARTESIAN_POINT('Ctrl Pts',(-19.7078787262288,-47.1345157070937,
122.243312822989)) ;
#78394 = CARTESIAN_POINT('Ctrl Pts',(-19.5258624977705,-47.3244017999194,
121.909002520916)) ;
#78395 = CARTESIAN_POINT('Ctrl Pts',(-19.502554784226,-47.1444127195006,122.209566874311)) ;
#78396 = CARTESIAN_POINT('Ctrl Pts',(-19.2648924723444,-47.334333121745,121.911168475281)) ;
#78397 = CARTESIAN_POINT('Ctrl Pts',(-19.2937789864561,-47.1543440413262,
122.211297494334)) ;
#78398 = CARTESIAN_POINT('Ctrl Pts',(-19.0054588236184,-47.3443748844995,
121.959423773116)) ;
#78399 = CARTESIAN_POINT('Ctrl Pts',(-19.0862316578282,-47.1643858040807,
122.249899661236)) ;
#78400 = CARTESIAN_POINT('Ctrl Pts',(-18.7620408415113,-47.3542630833902,
122.050409572589)) ;
#78401 = CARTESIAN_POINT('Ctrl Pts',(-18.8914968446578,-47.1742740029714,
122.322686186617)) ;
#78402 = CARTESIAN_POINT('Ctrl Pts',(-18.5355442147044,-47.36425702199,122.183311500813)) ;
#78403 = CARTESIAN_POINT('Ctrl Pts',(-18.7102985172249,-47.1842679415713,
122.429005819235)) ;
#78404 = CARTESIAN_POINT('Ctrl Pts',(-18.3366094811182,-47.3741978430269,
122.352654795941)) ;
#78405 = CARTESIAN_POINT('Ctrl Pts',(-18.551149473623,-47.1942087626082,122.564478686452)) ;
#78406 = CARTESIAN_POINT('Ctrl Pts',(-18.1695526329319,-47.3841572253151,
122.554106931981)) ;
#78407 = CARTESIAN_POINT('Ctrl Pts',(-18.417502400572,-47.2041681448964,122.725638889882)) ;
#78408 = CARTESIAN_POINT('Ctrl Pts',(-18.0393553531157,-47.3941549849675,
122.782338451479)) ;
#78409 = CARTESIAN_POINT('Ctrl Pts',(-18.3133427031119,-47.2141659045487,
122.908222957332)) ;
#78410 = CARTESIAN_POINT('Ctrl Pts',(-17.9507774144696,-47.4041911211698,
123.030750867637)) ;
#78411 = CARTESIAN_POINT('Ctrl Pts',(-18.2424783105885,-47.224202040751,123.106952144432)) ;
#78412 = CARTESIAN_POINT('Ctrl Pts',(-17.9071905132183,-47.4140419186607,
123.285921661665)) ;
#78413 = CARTESIAN_POINT('Ctrl Pts',(-18.2076066786079,-47.2340528382419,
123.311088103092)) ;
#78414 = CARTESIAN_POINT('Ctrl Pts',(-17.9078079176154,-47.424002783737,123.547672833058)) ;
#78415 = CARTESIAN_POINT('Ctrl Pts',(-18.2080983638521,-47.2440137033182,
123.520488944659)) ;
#78416 = CARTESIAN_POINT('Ctrl Pts',(-17.9544972056364,-47.4340316513674,
123.807067402993)) ;
#78417 = CARTESIAN_POINT('Ctrl Pts',(-18.2454476048845,-47.2540425709486,
123.728004959381)) ;
#78418 = CARTESIAN_POINT('Ctrl Pts',(-18.04435585215,-47.4439418875038,124.051493099934)) ;
#78419 = CARTESIAN_POINT('Ctrl Pts',(-18.3173323750563,-47.263952807085,123.923546127263)) ;
#78420 = CARTESIAN_POINT('Ctrl Pts',(-18.1750338401963,-47.4538768408183,
124.277524030933)) ;
#78421 = CARTESIAN_POINT('Ctrl Pts',(-18.4218727658216,-47.2738877603996,
124.10437190683)) ;
#78422 = CARTESIAN_POINT('Ctrl Pts',(-18.3449402388799,-47.4639177712279,
124.479398422779)) ;
#78423 = CARTESIAN_POINT('Ctrl Pts',(-18.5577961461573,-47.2839286908091,
124.265872834734)) ;
#78424 = CARTESIAN_POINT('Ctrl Pts',(-18.5441394208456,-47.4738056680095,
124.64626268792)) ;
#78425 = CARTESIAN_POINT('Ctrl Pts',(-18.717153951654,-47.2938165875907,124.399365886383)) ;
#78426 = CARTESIAN_POINT('Ctrl Pts',(-18.7713398491189,-47.4837951196682,
124.777752129338)) ;
#78427 = CARTESIAN_POINT('Ctrl Pts',(-18.8989131176986,-47.3038060392494,
124.504559363541)) ;
#78428 = CARTESIAN_POINT('Ctrl Pts',(-19.0172406223809,-47.4937542100335,
124.867323859669)) ;
#78429 = CARTESIAN_POINT('Ctrl Pts',(-19.0956328934438,-47.3137651296148,
124.576218838424)) ;
#78430 = CARTESIAN_POINT('Ctrl Pts',(-19.2732681589841,-47.5036515223399,
124.913214982572)) ;
#78431 = CARTESIAN_POINT('Ctrl Pts',(-19.3004544847699,-47.3236624419211,
124.612933948275)) ;
#78432 = CARTESIAN_POINT('Ctrl Pts',(-19.5375180334374,-47.5137079482401,
124.913840319069)) ;
#78433 = CARTESIAN_POINT('Ctrl Pts',(-19.5118543105369,-47.3337188678213,
124.613436469234)) ;
#78434 = CARTESIAN_POINT('Ctrl Pts',(-19.7931038035364,-47.5235779508299,
124.86953541512)) ;
#78435 = CARTESIAN_POINT('Ctrl Pts',(-19.7163232953093,-47.3435888704111,
124.577994777982)) ;
#78436 = CARTESIAN_POINT('Ctrl Pts',(-20.0405538778999,-47.5335818840071,
124.780842159474)) ;
#78437 = CARTESIAN_POINT('Ctrl Pts',(-19.9142841000956,-47.3535928035883,
124.507042257219)) ;
#78438 = CARTESIAN_POINT('Ctrl Pts',(-20.2684557085734,-47.543569144471,124.650592871709)) ;
#78439 = CARTESIAN_POINT('Ctrl Pts',(-20.096606520165,-47.3635800640522,124.402844965088)) ;
#78440 = CARTESIAN_POINT('Ctrl Pts',(-20.470938720647,-47.5535961960567,124.48200287069)) ;
#78441 = CARTESIAN_POINT('Ctrl Pts',(-20.2585947483738,-47.3736071156379,
124.267974120626)) ;
#78442 = CARTESIAN_POINT('Ctrl Pts',(-20.6389889195146,-47.5634872858828,
124.283677447636)) ;
#78443 = CARTESIAN_POINT('Ctrl Pts',(-20.3930350147794,-47.383498205464,124.109317524504)) ;
#78444 = CARTESIAN_POINT('Ctrl Pts',(-20.8155222737349,-47.5767850406638,
123.982153460003)) ;
#78445 = CARTESIAN_POINT('Ctrl Pts',(-20.5342723572746,-47.3967959602451,
123.86808831075)) ;
#78446 = CARTESIAN_POINT('Ctrl Pts',(-20.9091627272302,-47.589983100272,123.644050843678)) ;
#78447 = CARTESIAN_POINT('Ctrl Pts',(-20.6091851817961,-47.4099940198532,
123.597577609492)) ;
#78448 = CARTESIAN_POINT('Ctrl Pts',(-20.9119614688863,-47.6033798408412,
123.292030999212)) ;
#78449 = CARTESIAN_POINT('Ctrl Pts',(-20.6114219138469,-47.4233907604224,
123.316008249511)) ;
#78450 = CARTESIAN_POINT('Ctrl Pts',(-20.8692234170747,-47.6132507529146,
123.036128094881)) ;
#78451 = CARTESIAN_POINT('Ctrl Pts',(-20.5772346237464,-47.4332616724959,
123.111276038365)) ;
#78452 = CARTESIAN_POINT('Ctrl Pts',(-20.7809529679851,-47.6233243146827,
122.786617518481)) ;
#78453 = CARTESIAN_POINT('Ctrl Pts',(-20.5066201804174,-47.443335234264,122.911669620032)) ;
#78454 = CARTESIAN_POINT('Ctrl Pts',(-20.6541739490914,-47.6331457272711,
122.561735103864)) ;
#78455 = CARTESIAN_POINT('Ctrl Pts',(-20.405198506557,-47.4531566468523,122.731761296753)) ;
#78456 = CARTESIAN_POINT('Ctrl Pts',(-20.4863320286393,-47.6432197445021,
122.357091382096)) ;
#78457 = CARTESIAN_POINT('Ctrl Pts',(-20.2709276233739,-47.4632306640834,
122.568046598626)) ;
#78458 = CARTESIAN_POINT('Ctrl Pts',(-20.2240587467642,-47.6563785314667,
122.13161591523)) ;
#78459 = CARTESIAN_POINT('Ctrl Pts',(-20.0611061721674,-47.4763894510479,
122.387657331464)) ;
#78460 = CARTESIAN_POINT('Ctrl Pts',(-19.9043966118388,-47.6697446345609,
121.976897634907)) ;
#78461 = CARTESIAN_POINT('Ctrl Pts',(-19.8053424387584,-47.4897555541421,
122.263873680573)) ;
#78462 = CARTESIAN_POINT('Ctrl Pts',(-19.5604802160081,-47.6830585694499,
121.912018372338)) ;
#78463 = CARTESIAN_POINT('Ctrl Pts',(-19.5302562121692,-47.5030694890312,
122.211981762191)) ;
#78464 = CARTESIAN_POINT('Ctrl Pts',(-19.3003815270674,-47.6929586088974,
121.90833318309)) ;
#78465 = CARTESIAN_POINT('Ctrl Pts',(-19.322167620802,-47.5129695284786,122.209028724385)) ;
#78466 = CARTESIAN_POINT('Ctrl Pts',(-19.041800524058,-47.7029230120319,121.949706845945)) ;
#78467 = CARTESIAN_POINT('Ctrl Pts',(-19.1153050560258,-47.5229339316132,
122.242126300754)) ;
#78468 = CARTESIAN_POINT('Ctrl Pts',(-18.7927924421726,-47.712952979153,122.036134213091)) ;
#78469 = CARTESIAN_POINT('Ctrl Pts',(-18.9160968262407,-47.5329638987343,
122.311266676217)) ;
#78470 = CARTESIAN_POINT('Ctrl Pts',(-18.5654632173557,-47.7228552557621,
122.162745640251)) ;
#78471 = CARTESIAN_POINT('Ctrl Pts',(-18.734234498539,-47.5428661753434,122.412551849973)) ;
#78472 = CARTESIAN_POINT('Ctrl Pts',(-18.2943866085651,-47.7361211849313,
122.382011147365)) ;
#78473 = CARTESIAN_POINT('Ctrl Pts',(-18.5173605390981,-47.5561321045125,
122.587974585937)) ;
#78474 = CARTESIAN_POINT('Ctrl Pts',(-18.0346303796322,-47.7527427160376,
122.739250673767)) ;
#78475 = CARTESIAN_POINT('Ctrl Pts',(-18.3095657843141,-47.5727536356189,
122.873754271504)) ;
#78476 = CARTESIAN_POINT('Ctrl Pts',(-17.8876997700459,-47.7726175446823,
123.246720784375)) ;
#78477 = CARTESIAN_POINT('Ctrl Pts',(-18.192010176043,-47.5926284642636,123.27971738618)) ;
#78478 = CARTESIAN_POINT('Ctrl Pts',(-17.9170005926413,-47.7892907527842,
123.688848718137)) ;
#78479 = CARTESIAN_POINT('Ctrl Pts',(-18.2154597786599,-47.6093016723655,
123.63347188355)) ;
#78480 = CARTESIAN_POINT('Ctrl Pts',(-18.0293936751226,-47.8025418777655,
124.018462677724)) ;
#78481 = CARTESIAN_POINT('Ctrl Pts',(-18.305361509496,-47.6225527973467,123.897116801206)) ;
#78482 = CARTESIAN_POINT('Ctrl Pts',(-18.1961054879698,-47.8157841965863,
124.323995100804)) ;
#78483 = CARTESIAN_POINT('Ctrl Pts',(-18.4387378061925,-47.6357951161676,
124.141559984397)) ;
#78484 = CARTESIAN_POINT('Ctrl Pts',(-18.5033373266332,-47.8325174369258,
124.645448284641)) ;
#78485 = CARTESIAN_POINT('Ctrl Pts',(-18.6845128198436,-47.652528356507,124.398713602975)) ;
#78486 = CARTESIAN_POINT('Ctrl Pts',(-18.9757346113062,-47.8523465851138,
124.87933604937)) ;
#78487 = CARTESIAN_POINT('Ctrl Pts',(-19.0624327890952,-47.672357504695,124.585830613588)) ;
#78488 = CARTESIAN_POINT('Ctrl Pts',(-19.5017537469011,-47.8722712802144,
124.9395166783)) ;
#78489 = CARTESIAN_POINT('Ctrl Pts',(-19.4832476587856,-47.6922821997956,
124.633977069387)) ;
#78490 = CARTESIAN_POINT('Ctrl Pts',(-20.0168758619817,-47.8921945087978,
124.816493222179)) ;
#78491 = CARTESIAN_POINT('Ctrl Pts',(-19.8953467115458,-47.7122054283791,
124.535561030838)) ;
#78492 = CARTESIAN_POINT('Ctrl Pts',(-20.4591503181284,-47.9121216479239,
124.525228376987)) ;
#78493 = CARTESIAN_POINT('Ctrl Pts',(-20.2491681384619,-47.7321325675052,
124.302550855083)) ;
#78494 = CARTESIAN_POINT('Ctrl Pts',(-20.7752836477804,-47.9319981105396,
124.101934449812)) ;
#78495 = CARTESIAN_POINT('Ctrl Pts',(-20.5020771966928,-47.7520090301208,
123.963916114928)) ;
#78496 = CARTESIAN_POINT('Ctrl Pts',(-20.9290246639703,-47.9519753391449,
123.59372436111)) ;
#78497 = CARTESIAN_POINT('Ctrl Pts',(-20.6250718773028,-47.7719862587261,
123.557348393509)) ;
#78498 = CARTESIAN_POINT('Ctrl Pts',(-20.8997496415045,-47.9719101971186,
123.064652071542)) ;
#78499 = CARTESIAN_POINT('Ctrl Pts',(-20.6016537118098,-47.7919211166998,
123.134089837888)) ;
#78500 = CARTESIAN_POINT('Ctrl Pts',(-20.6926191392944,-47.9918066460494,
122.578134849527)) ;
#78501 = CARTESIAN_POINT('Ctrl Pts',(-20.4359502844163,-47.8118175656306,
122.744874452236)) ;
#78502 = CARTESIAN_POINT('Ctrl Pts',(-20.331839327964,-48.011727930116,122.1905714448)) ;
#78503 = CARTESIAN_POINT('Ctrl Pts',(-20.147326663776,-47.8317388496972,122.434822343269)) ;
#78504 = CARTESIAN_POINT('Ctrl Pts',(-19.8595433796949,-48.0316845797869,
121.949105900336)) ;
#78505 = CARTESIAN_POINT('Ctrl Pts',(-19.7694899560227,-47.8516954993682,
122.241648817227)) ;
#78506 = CARTESIAN_POINT('Ctrl Pts',(-19.3354077539435,-48.0515618728986,
121.883411775876)) ;
#78507 = CARTESIAN_POINT('Ctrl Pts',(-19.3501800444516,-47.8715727924798,
122.189092575261)) ;
#78508 = CARTESIAN_POINT('Ctrl Pts',(-18.8196458601966,-48.071448345127,121.999233714831)) ;
#78509 = CARTESIAN_POINT('Ctrl Pts',(-18.9375691001692,-47.8914592647082,
122.281750583357)) ;
#78510 = CARTESIAN_POINT('Ctrl Pts',(-18.3709126385294,-48.091509911051,122.287270877135)) ;
#78511 = CARTESIAN_POINT('Ctrl Pts',(-18.578583226595,-47.9115208306322,122.512179806311)) ;
#78512 = CARTESIAN_POINT('Ctrl Pts',(-18.0514008753301,-48.1113503185918,
122.70674475677)) ;
#78513 = CARTESIAN_POINT('Ctrl Pts',(-18.3229724703465,-47.931361238173,122.847760542803)) ;
#78514 = CARTESIAN_POINT('Ctrl Pts',(-17.892005383859,-48.1312016425647,123.209726070952)) ;
#78515 = CARTESIAN_POINT('Ctrl Pts',(-18.1954566722783,-47.9512125621459,
123.250147612826)) ;
#78516 = CARTESIAN_POINT('Ctrl Pts',(-17.914844951633,-48.1512549125161,123.742150506215)) ;
#78517 = CARTESIAN_POINT('Ctrl Pts',(-18.2137292815851,-47.9712658320974,
123.676086505446)) ;
#78518 = CARTESIAN_POINT('Ctrl Pts',(-18.1156214422084,-48.1710755698994,
124.229345578923)) ;
#78519 = CARTESIAN_POINT('Ctrl Pts',(-18.3743523078456,-47.9910864894807,
124.065843886977)) ;
#78520 = CARTESIAN_POINT('Ctrl Pts',(-18.4724496627576,-48.1910469912299,
124.622086302339)) ;
#78521 = CARTESIAN_POINT('Ctrl Pts',(-18.659816387674,-48.0110579108112,124.380035522052)) ;
#78522 = CARTESIAN_POINT('Ctrl Pts',(-18.9403084788602,-48.2109404835936,
124.868804641601)) ;
#78523 = CARTESIAN_POINT('Ctrl Pts',(-19.03410518183,-48.0309514031749,124.577408955661)) ;
#78524 = CARTESIAN_POINT('Ctrl Pts',(-19.4674642242585,-48.2309645698347,
124.941135895806)) ;
#78525 = CARTESIAN_POINT('Ctrl Pts',(-19.4558298576854,-48.050975489416,124.635271999274)) ;
#78526 = CARTESIAN_POINT('Ctrl Pts',(-19.9821868641335,-48.2507694489476,
124.830704772389)) ;
#78527 = CARTESIAN_POINT('Ctrl Pts',(-19.867609211054,-48.0707803685288,124.546924581979)) ;
#78528 = CARTESIAN_POINT('Ctrl Pts',(-20.432501328611,-48.2707284646455,124.55033776454)) ;
#78529 = CARTESIAN_POINT('Ctrl Pts',(-20.227859532346,-48.0907393842267,124.32262844544)) ;
#78530 = CARTESIAN_POINT('Ctrl Pts',(-20.75958556185,-48.2907144882745,124.131795730235)) ;
#78531 = CARTESIAN_POINT('Ctrl Pts',(-20.4895249857821,-48.1107254078558,
123.987793147059)) ;
#78532 = CARTESIAN_POINT('Ctrl Pts',(-20.9237469670183,-48.310522984035,123.631516939099)) ;
#78533 = CARTESIAN_POINT('Ctrl Pts',(-20.6208517088242,-48.1305339036163,
123.587567868658)) ;
#78534 = CARTESIAN_POINT('Ctrl Pts',(-20.90785637785,-48.3305056231406,123.100761863408)) ;
#78535 = CARTESIAN_POINT('Ctrl Pts',(-20.6081359619185,-48.1505165427219,
123.162963825818)) ;
#78536 = CARTESIAN_POINT('Ctrl Pts',(-20.7125774922686,-48.3503870709346,
122.609609792236)) ;
#78537 = CARTESIAN_POINT('Ctrl Pts',(-20.4519095117402,-48.1703979905159,
122.770042764306)) ;
#78538 = CARTESIAN_POINT('Ctrl Pts',(-20.3605699835349,-48.3703435376721,
122.212992650378)) ;
#78539 = CARTESIAN_POINT('Ctrl Pts',(-20.1703007092997,-48.1903544572534,
122.452751209908)) ;
#78540 = CARTESIAN_POINT('Ctrl Pts',(-19.8961915070814,-48.3902209346277,
121.960894036754)) ;
#78541 = CARTESIAN_POINT('Ctrl Pts',(-19.7987956286007,-48.210231854209,122.2510753083)) ;
#78542 = CARTESIAN_POINT('Ctrl Pts',(-19.3710944052857,-48.410202880803,121.881710834877)) ;
#78543 = CARTESIAN_POINT('Ctrl Pts',(-19.3787173826546,-48.2302138003843,
122.1877323754)) ;
#78544 = CARTESIAN_POINT('Ctrl Pts',(-18.8517658004978,-48.4301319798398,
121.986485154986)) ;
#78545 = CARTESIAN_POINT('Ctrl Pts',(-18.9632548451584,-48.250142899421,122.271556232587)) ;
#78546 = CARTESIAN_POINT('Ctrl Pts',(-18.3995108076941,-48.4500606030523,
122.262000851755)) ;
#78547 = CARTESIAN_POINT('Ctrl Pts',(-18.6014532429342,-48.2700715226336,
122.491970142446)) ;
#78548 = CARTESIAN_POINT('Ctrl Pts',(-18.0691275875029,-48.4698949271588,
122.672852581585)) ;
#78549 = CARTESIAN_POINT('Ctrl Pts',(-18.337147399175,-48.28990584674,122.820662663942)) ;
#78550 = CARTESIAN_POINT('Ctrl Pts',(-17.9257131669283,-48.4865472145422,
123.091471777947)) ;
#78551 = CARTESIAN_POINT('Ctrl Pts',(-18.2224260058625,-48.3065581341234,
123.155533896471)) ;
#78552 = CARTESIAN_POINT('Ctrl Pts',(-17.9020712050021,-48.4998077155644,
123.439203218315)) ;
#78553 = CARTESIAN_POINT('Ctrl Pts',(-18.2035092593179,-48.3198186351457,
123.433741819018)) ;
#78554 = CARTESIAN_POINT('Ctrl Pts',(-17.9295520561369,-48.5098091927657,
123.700586123917)) ;
#78555 = CARTESIAN_POINT('Ctrl Pts',(-18.2254971398453,-48.3298201123469,
123.642843255364)) ;
#78556 = CARTESIAN_POINT('Ctrl Pts',(-18.0026504045817,-48.5198412136252,
123.953887639464)) ;
#78557 = CARTESIAN_POINT('Ctrl Pts',(-18.2839780158191,-48.3398521332064,
123.845485394046)) ;
#78558 = CARTESIAN_POINT('Ctrl Pts',(-18.1163811920468,-48.5297047573507,
124.186799307469)) ;
#78559 = CARTESIAN_POINT('Ctrl Pts',(-18.3749628126578,-48.349715676932,124.031812191722)) ;
#78560 = CARTESIAN_POINT('Ctrl Pts',(-18.2698960729777,-48.5396734710209,
124.399078392918)) ;
#78561 = CARTESIAN_POINT('Ctrl Pts',(-18.4977838735188,-48.3596843906021,
124.201640071483)) ;
#78562 = CARTESIAN_POINT('Ctrl Pts',(-18.5219675225245,-48.5530192184246,
124.64288817391)) ;
#78563 = CARTESIAN_POINT('Ctrl Pts',(-18.6994062245984,-48.3730301380058,
124.396656830868)) ;
#78564 = CARTESIAN_POINT('Ctrl Pts',(-18.8271260676844,-48.5661697734973,
124.813370161001)) ;
#78565 = CARTESIAN_POINT('Ctrl Pts',(-18.9435542458751,-48.3861806930785,
124.533062412033)) ;
#78566 = CARTESIAN_POINT('Ctrl Pts',(-19.1680417733559,-48.5795551540471,
124.899907926096)) ;
#78567 = CARTESIAN_POINT('Ctrl Pts',(-19.2163009890961,-48.3995660736284,
124.602291912706)) ;
#78568 = CARTESIAN_POINT('Ctrl Pts',(-19.4272046606689,-48.5894430900399,
124.91913276081)) ;
#78569 = CARTESIAN_POINT('Ctrl Pts',(-19.4236288223874,-48.4094540096212,
124.617669122976)) ;
#78570 = CARTESIAN_POINT('Ctrl Pts',(-19.688447434272,-48.5994342798526,124.893240945858)) ;
#78571 = CARTESIAN_POINT('Ctrl Pts',(-19.6326235030201,-48.4194451994339,
124.596953556144)) ;
#78572 = CARTESIAN_POINT('Ctrl Pts',(-19.9403393905488,-48.6093863783909,
124.82274784363)) ;
#78573 = CARTESIAN_POINT('Ctrl Pts',(-19.834136251256,-48.4293972979721,124.540556882283)) ;
#78574 = CARTESIAN_POINT('Ctrl Pts',(-20.1782692262565,-48.6194326348414,
124.708388111994)) ;
#78575 = CARTESIAN_POINT('Ctrl Pts',(-20.0244791282803,-48.4394435544226,
124.449067115827)) ;
#78576 = CARTESIAN_POINT('Ctrl Pts',(-20.3886560574177,-48.6292820822355,
124.557608789949)) ;
#78577 = CARTESIAN_POINT('Ctrl Pts',(-20.1927872963318,-48.4492930018168,
124.328441805435)) ;
#78578 = CARTESIAN_POINT('Ctrl Pts',(-20.5723260959942,-48.6392447347306,
124.371049479752)) ;
#78579 = CARTESIAN_POINT('Ctrl Pts',(-20.3397216706453,-48.4592556543119,
124.179192818539)) ;
#78580 = CARTESIAN_POINT('Ctrl Pts',(-20.7214277474001,-48.6492678203728,
124.153918077439)) ;
#78581 = CARTESIAN_POINT('Ctrl Pts',(-20.4590011009063,-48.469278739954,124.005486461818)) ;
#78582 = CARTESIAN_POINT('Ctrl Pts',(-20.8297802316799,-48.6591929361297,
123.916635975677)) ;
#78583 = CARTESIAN_POINT('Ctrl Pts',(-20.5456810096503,-48.479203855711,123.815659897724)) ;
#78584 = CARTESIAN_POINT('Ctrl Pts',(-20.8960112319061,-48.6692454145295,
123.660930444422)) ;
#78585 = CARTESIAN_POINT('Ctrl Pts',(-20.5986636102316,-48.4892563341108,
123.611094951253)) ;
#78586 = CARTESIAN_POINT('Ctrl Pts',(-20.916598068242,-48.6790969132322,123.402843889694)) ;
#78587 = CARTESIAN_POINT('Ctrl Pts',(-20.6151308203117,-48.4991078328135,
123.404625622349)) ;
#78588 = CARTESIAN_POINT('Ctrl Pts',(-20.892445735592,-48.6890686524347,123.141945824764)) ;
#78589 = CARTESIAN_POINT('Ctrl Pts',(-20.5958067228006,-48.509079572016,123.195907470545)) ;
#78590 = CARTESIAN_POINT('Ctrl Pts',(-20.8231457687366,-48.6990638602004,
122.888545055551)) ;
#78591 = CARTESIAN_POINT('Ctrl Pts',(-20.5403646013204,-48.5190747797817,
122.993187508509)) ;
#78592 = CARTESIAN_POINT('Ctrl Pts',(-20.7102015280108,-48.7090978616695,
122.650301300799)) ;
#78593 = CARTESIAN_POINT('Ctrl Pts',(-20.4500071819512,-48.5291087812508,
122.802593499085)) ;
#78594 = CARTESIAN_POINT('Ctrl Pts',(-20.5606310889798,-48.7189532197619,
122.438836911288)) ;
#78595 = CARTESIAN_POINT('Ctrl Pts',(-20.3303491093556,-48.5389641393431,
122.633423436185)) ;
#78596 = CARTESIAN_POINT('Ctrl Pts',(-20.3742255769114,-48.7289526953552,
122.253690036809)) ;
#78597 = CARTESIAN_POINT('Ctrl Pts',(-20.1812231766611,-48.5489636149364,
122.485307572519)) ;
#78598 = CARTESIAN_POINT('Ctrl Pts',(-20.1608603227047,-48.7388471438503,
122.104999075686)) ;
#78599 = CARTESIAN_POINT('Ctrl Pts',(-20.0105298816174,-48.5588580634315,
122.366356738769)) ;
#78600 = CARTESIAN_POINT('Ctrl Pts',(-19.9209501104199,-48.748910268078,121.993860313516)) ;
#78601 = CARTESIAN_POINT('Ctrl Pts',(-19.8186007515957,-48.5689211876593,
122.277447732973)) ;
#78602 = CARTESIAN_POINT('Ctrl Pts',(-19.6710512311484,-48.7587498944066,
121.927273469852)) ;
#78603 = CARTESIAN_POINT('Ctrl Pts',(-19.6186814015643,-48.5787608139879,
122.224180469347)) ;
#78604 = CARTESIAN_POINT('Ctrl Pts',(-19.4076398792597,-48.7688131294496,
121.904256633468)) ;
#78605 = CARTESIAN_POINT('Ctrl Pts',(-19.4079520936183,-48.5888240490308,
122.205769170456)) ;
#78606 = CARTESIAN_POINT('Ctrl Pts',(-19.1486188793757,-48.7787071346836,
121.927163232739)) ;
#78607 = CARTESIAN_POINT('Ctrl Pts',(-19.2007357506879,-48.5987180542649,
122.224096613958)) ;
#78608 = CARTESIAN_POINT('Ctrl Pts',(-18.8961432338801,-48.7886498478994,
121.994321818682)) ;
#78609 = CARTESIAN_POINT('Ctrl Pts',(-18.9987559919676,-48.6086607674806,
122.27782549784)) ;
#78610 = CARTESIAN_POINT('Ctrl Pts',(-18.6575880746569,-48.7986555876975,
122.104972809837)) ;
#78611 = CARTESIAN_POINT('Ctrl Pts',(-18.8079128155078,-48.6186665072788,
122.366348201292)) ;
#78612 = CARTESIAN_POINT('Ctrl Pts',(-18.4417397385288,-48.808676489844,122.255816146029)) ;
#78613 = CARTESIAN_POINT('Ctrl Pts',(-18.6352354003947,-48.6286874094252,
122.487024632224)) ;
#78614 = CARTESIAN_POINT('Ctrl Pts',(-18.2575608010827,-48.8185672598928,
122.439229061403)) ;
#78615 = CARTESIAN_POINT('Ctrl Pts',(-18.4878939926653,-48.6385781794741,
122.633756241431)) ;
#78616 = CARTESIAN_POINT('Ctrl Pts',(-18.1061936758401,-48.8285586706726,
122.653759103607)) ;
#78617 = CARTESIAN_POINT('Ctrl Pts',(-18.3668020674057,-48.6485695902538,
122.805381400602)) ;
#78618 = CARTESIAN_POINT('Ctrl Pts',(-17.9949337391282,-48.838507016337,122.890328842187)) ;
#78619 = CARTESIAN_POINT('Ctrl Pts',(-18.2777961188115,-48.6585179359183,
122.994637890624)) ;
#78620 = CARTESIAN_POINT('Ctrl Pts',(-17.9259246878583,-48.8484518743983,
123.14241755187)) ;
#78621 = CARTESIAN_POINT('Ctrl Pts',(-18.2225909149543,-48.6684627939795,
123.196309167332)) ;
#78622 = CARTESIAN_POINT('Ctrl Pts',(-17.9018586344331,-48.8585067097912,
123.405524737978)) ;
#78623 = CARTESIAN_POINT('Ctrl Pts',(-18.2033401477523,-48.6785176293724,
123.406795195145)) ;
#78624 = CARTESIAN_POINT('Ctrl Pts',(-17.9228907004356,-48.8683290818927,
123.662811089187)) ;
#78625 = CARTESIAN_POINT('Ctrl Pts',(-18.2201677808873,-48.6883400014739,
123.612623483924)) ;
#78626 = CARTESIAN_POINT('Ctrl Pts',(-17.9893599290001,-48.8783849493364,
123.918552606294)) ;
#78627 = CARTESIAN_POINT('Ctrl Pts',(-18.2733451048243,-48.6983958689176,
123.817216284864)) ;
#78628 = CARTESIAN_POINT('Ctrl Pts',(-18.0984022474381,-48.8883256791943,
124.155949320451)) ;
#78629 = CARTESIAN_POINT('Ctrl Pts',(-18.360580702555,-48.7083365987755,124.007132560782)) ;
#78630 = CARTESIAN_POINT('Ctrl Pts',(-18.2457897777886,-48.8982300177454,
124.370478803573)) ;
#78631 = CARTESIAN_POINT('Ctrl Pts',(-18.4784920796112,-48.7182409373267,
124.178754699922)) ;
#78632 = CARTESIAN_POINT('Ctrl Pts',(-18.4309099578096,-48.9082766991739,
124.558689346478)) ;
#78633 = CARTESIAN_POINT('Ctrl Pts',(-18.6265896773682,-48.7282876187551,
124.329321820861)) ;
#78634 = CARTESIAN_POINT('Ctrl Pts',(-18.6425771224203,-48.9181722066431,
124.709824664165)) ;
#78635 = CARTESIAN_POINT('Ctrl Pts',(-18.7959241464339,-48.7381831262244,
124.450228239053)) ;
#78636 = CARTESIAN_POINT('Ctrl Pts',(-18.881153587665,-48.9282344751418,124.823761366659)) ;
#78637 = CARTESIAN_POINT('Ctrl Pts',(-18.986786280884,-48.748245394723,124.541375925979)) ;
#78638 = CARTESIAN_POINT('Ctrl Pts',(-19.1303382919455,-48.9380764654124,
124.893166471183)) ;
#78639 = CARTESIAN_POINT('Ctrl Pts',(-19.18613388542,-48.7580873849936,124.596897991502)) ;
#78640 = CARTESIAN_POINT('Ctrl Pts',(-19.3916192445902,-48.9480698822934,
124.919216288569)) ;
#78641 = CARTESIAN_POINT('Ctrl Pts',(-19.3951586909665,-48.7680808018746,
124.617736026515)) ;
#78642 = CARTESIAN_POINT('Ctrl Pts',(-19.6517180268425,-48.9579943701455,
124.899657271401)) ;
#78643 = CARTESIAN_POINT('Ctrl Pts',(-19.6032371787446,-48.7780052897268,
124.602087041937)) ;
#78644 = CARTESIAN_POINT('Ctrl Pts',(-19.9064040385357,-48.967994004054,124.835026142102)) ;
#78645 = CARTESIAN_POINT('Ctrl Pts',(-19.8069854638334,-48.7880049236352,
124.550380450082)) ;
#78646 = CARTESIAN_POINT('Ctrl Pts',(-20.1457345660607,-48.9779801143107,
124.727283799791)) ;
#78647 = CARTESIAN_POINT('Ctrl Pts',(-19.9984490348426,-48.797991033892,124.464185028181)) ;
#78648 = CARTESIAN_POINT('Ctrl Pts',(-20.3635957586943,-48.9880160654979,
124.578693439251)) ;
#78649 = CARTESIAN_POINT('Ctrl Pts',(-20.1727370240025,-48.8080269850791,
124.345311205248)) ;
#78650 = CARTESIAN_POINT('Ctrl Pts',(-20.5492835774954,-48.9978727038327,
124.398066759138)) ;
#78651 = CARTESIAN_POINT('Ctrl Pts',(-20.321285535719,-48.8178836234139,124.200809123624)) ;
#78652 = CARTESIAN_POINT('Ctrl Pts',(-20.7032232577426,-49.0078716639107,
124.185175408086)) ;
#78653 = CARTESIAN_POINT('Ctrl Pts',(-20.4444358521844,-48.8278825834919,
124.030495143245)) ;
#78654 = CARTESIAN_POINT('Ctrl Pts',(-20.8169628557573,-49.0177668942244,
123.951284539001)) ;
#78655 = CARTESIAN_POINT('Ctrl Pts',(-20.5354258074483,-48.8377778138057,
123.84338226399)) ;
#78656 = CARTESIAN_POINT('Ctrl Pts',(-20.8895070311637,-49.0278274066931,
123.697088016927)) ;
#78657 = CARTESIAN_POINT('Ctrl Pts',(-20.5934596252462,-48.8478383262744,
123.640024411145)) ;
#78658 = CARTESIAN_POINT('Ctrl Pts',(-20.9163903856303,-49.0376766982393,
123.439638200356)) ;
#78659 = CARTESIAN_POINT('Ctrl Pts',(-20.6149646209664,-48.8576876178205,
123.434065220729)) ;
#78660 = CARTESIAN_POINT('Ctrl Pts',(-20.8985020838412,-49.0477038841715,
123.17674881798)) ;
#78661 = CARTESIAN_POINT('Ctrl Pts',(-20.6006524960591,-48.8677148037527,
123.223753784893)) ;
#78662 = CARTESIAN_POINT('Ctrl Pts',(-20.8345541010976,-49.0577324206308,
122.921071960527)) ;
#78663 = CARTESIAN_POINT('Ctrl Pts',(-20.5494925272255,-48.8777433402121,
123.019212637237)) ;
#78664 = CARTESIAN_POINT('Ctrl Pts',(-20.7296054274072,-49.0675776605958,
122.684606145175)) ;
#78665 = CARTESIAN_POINT('Ctrl Pts',(-20.4655325601765,-48.887588580177,122.830041421681)) ;
#78666 = CARTESIAN_POINT('Ctrl Pts',(-20.583631751647,-49.077568355519,122.466374760931)) ;
#78667 = CARTESIAN_POINT('Ctrl Pts',(-20.3487525572943,-48.8975792751002,
122.655457213119)) ;
#78668 = CARTESIAN_POINT('Ctrl Pts',(-20.4007099669967,-49.0876061762776,
122.276320211613)) ;
#78669 = CARTESIAN_POINT('Ctrl Pts',(-20.202413975225,-48.9076170958588,122.503414537184)) ;
#78670 = CARTESIAN_POINT('Ctrl Pts',(-20.1919240684328,-49.0974507700545,
122.123545795029)) ;
#78671 = CARTESIAN_POINT('Ctrl Pts',(-20.0353851785869,-48.9174616896358,
122.381196695483)) ;
#78672 = CARTESIAN_POINT('Ctrl Pts',(-19.9567693977437,-49.1074347654306,
122.007237918763)) ;
#78673 = CARTESIAN_POINT('Ctrl Pts',(-19.8472610587631,-48.9274456850118,
122.288151648235)) ;
#78674 = CARTESIAN_POINT('Ctrl Pts',(-19.7058304590674,-49.117383813992,121.933802444952)) ;
#78675 = CARTESIAN_POINT('Ctrl Pts',(-19.646509912876,-48.9373947335732,122.229404623023)) ;
#78676 = CARTESIAN_POINT('Ctrl Pts',(-19.4445921214441,-49.1273862529665,
121.904618015558)) ;
#78677 = CARTESIAN_POINT('Ctrl Pts',(-19.437519186954,-48.9473971725478,122.206058321962)) ;
#78678 = CARTESIAN_POINT('Ctrl Pts',(-19.181792231299,-49.1374074942629,121.921624060286)) ;
#78679 = CARTESIAN_POINT('Ctrl Pts',(-19.2272793333639,-48.9574184138441,
122.219664472921)) ;
#78680 = CARTESIAN_POINT('Ctrl Pts',(-18.9291459750835,-49.1473001727024,
121.982897915604)) ;
#78681 = CARTESIAN_POINT('Ctrl Pts',(-19.025163319022,-48.9673110922836,122.268684604712)) ;
#78682 = CARTESIAN_POINT('Ctrl Pts',(-18.6884670363389,-49.15729022665,122.087747388098)) ;
#78683 = CARTESIAN_POINT('Ctrl Pts',(-18.8326207934705,-48.9773011462313,
122.352565175257)) ;
#78684 = CARTESIAN_POINT('Ctrl Pts',(-18.4704519829709,-49.1672485877985,
122.232485671744)) ;
#78685 = CARTESIAN_POINT('Ctrl Pts',(-18.6582097022475,-48.9872595073797,
122.468356610712)) ;
#78686 = CARTESIAN_POINT('Ctrl Pts',(-18.2815383414992,-49.1771482146833,
122.411369259827)) ;
#78687 = CARTESIAN_POINT('Ctrl Pts',(-18.5070800263305,-48.9971591342646,
122.611463763631)) ;
#78688 = CARTESIAN_POINT('Ctrl Pts',(-18.124334533003,-49.1871961114867,122.623486945932)) ;
#78689 = CARTESIAN_POINT('Ctrl Pts',(-18.3813177411218,-49.0072070310679,
122.781158694447)) ;
#78690 = CARTESIAN_POINT('Ctrl Pts',(-18.0079271716233,-49.1970914691227,
122.856062333949)) ;
#78691 = CARTESIAN_POINT('Ctrl Pts',(-18.2881931003449,-49.0171023887039,
122.967218812396)) ;
#78692 = CARTESIAN_POINT('Ctrl Pts',(-17.932406893039,-49.2071531215793,123.109426695874)) ;
#78693 = CARTESIAN_POINT('Ctrl Pts',(-18.2277777834536,-49.0271640411606,
123.169910844373)) ;
#78694 = CARTESIAN_POINT('Ctrl Pts',(-17.9026375540909,-49.2169977258513,
123.366423552931)) ;
#78695 = CARTESIAN_POINT('Ctrl Pts',(-18.2039634417627,-49.0370086454325,
123.375507396247)) ;
#78696 = CARTESIAN_POINT('Ctrl Pts',(-17.9171858177311,-49.2269578475493,
123.627756075223)) ;
#78697 = CARTESIAN_POINT('Ctrl Pts',(-18.2156028245757,-49.0469687671305,
123.584573004918)) ;
#78698 = CARTESIAN_POINT('Ctrl Pts',(-17.9778519476595,-49.2369958819118,
123.884464098771)) ;
#78699 = CARTESIAN_POINT('Ctrl Pts',(-18.2641366483863,-49.0570068014931,
123.789939339049)) ;
#78700 = CARTESIAN_POINT('Ctrl Pts',(-18.0800477462609,-49.2468701944983,
124.12301444571)) ;
#78701 = CARTESIAN_POINT('Ctrl Pts',(-18.3458936691752,-49.0668811140795,
123.980778477681)) ;
#78702 = CARTESIAN_POINT('Ctrl Pts',(-18.2248917332872,-49.256939675281,124.34442449373)) ;
#78703 = CARTESIAN_POINT('Ctrl Pts',(-18.4617697106575,-49.0769505948622,
124.157906347072)) ;
#78704 = CARTESIAN_POINT('Ctrl Pts',(-18.4016886196437,-49.2667740112981,
124.53295491212)) ;
#78705 = CARTESIAN_POINT('Ctrl Pts',(-18.6032069775405,-49.0867849308793,
124.308729299601)) ;
#78706 = CARTESIAN_POINT('Ctrl Pts',(-18.6122540928525,-49.2768069690263,
124.691612235834)) ;
#78707 = CARTESIAN_POINT('Ctrl Pts',(-18.7716597901353,-49.0968178886076,
124.435654741883)) ;
#78708 = CARTESIAN_POINT('Ctrl Pts',(-18.8472145112235,-49.2868273676015,
124.8105056569)) ;
#78709 = CARTESIAN_POINT('Ctrl Pts',(-18.9596285027308,-49.1068382871827,
124.530768800945)) ;
#78710 = CARTESIAN_POINT('Ctrl Pts',(-19.0951813191126,-49.2966929413727,
124.886249263536)) ;
#78711 = CARTESIAN_POINT('Ctrl Pts',(-19.158001200267,-49.116703860954,124.59136281955)) ;
#78712 = CARTESIAN_POINT('Ctrl Pts',(-19.3577881565879,-49.3067618160288,
124.91843560293)) ;
#78713 = CARTESIAN_POINT('Ctrl Pts',(-19.3680870720684,-49.12677273561,124.617111322248)) ;
#78714 = CARTESIAN_POINT('Ctrl Pts',(-19.6161749842787,-49.3166072469343,
124.904881658566)) ;
#78715 = CARTESIAN_POINT('Ctrl Pts',(-19.5747953751554,-49.1366181665155,
124.606267622671)) ;
#78716 = CARTESIAN_POINT('Ctrl Pts',(-19.8718870581338,-49.326586871805,124.846704436952)) ;
#78717 = CARTESIAN_POINT('Ctrl Pts',(-19.7793647044864,-49.1465977913862,
124.55972551948)) ;
#78718 = CARTESIAN_POINT('Ctrl Pts',(-20.1143655070177,-49.3366055547191,
124.744152692603)) ;
#78719 = CARTESIAN_POINT('Ctrl Pts',(-19.9733472699668,-49.1566164743003,
124.477683643661)) ;
#78720 = CARTESIAN_POINT('Ctrl Pts',(-20.3326993755422,-49.3464888199029,
124.603431043447)) ;
#78721 = CARTESIAN_POINT('Ctrl Pts',(-20.148013421792,-49.1664997394842,124.365106482365)) ;
#78722 = CARTESIAN_POINT('Ctrl Pts',(-20.5267164376053,-49.3565571139943,
124.423600519454)) ;
#78723 = CARTESIAN_POINT('Ctrl Pts',(-20.3032270348823,-49.1765680335755,
124.221241540364)) ;
#78724 = CARTESIAN_POINT('Ctrl Pts',(-20.6830755385478,-49.3663872441796,
124.217913860269)) ;
#78725 = CARTESIAN_POINT('Ctrl Pts',(-20.4283133065888,-49.1863981637609,
124.056692994351)) ;
#78726 = CARTESIAN_POINT('Ctrl Pts',(-20.8044543032016,-49.3764537923947,
123.982913211167)) ;
#78727 = CARTESIAN_POINT('Ctrl Pts',(-20.5254162463695,-49.196464711976,123.868692079819)) ;
#78728 = CARTESIAN_POINT('Ctrl Pts',(-20.8816750148595,-49.3863440410833,
123.734710364359)) ;
#78729 = CARTESIAN_POINT('Ctrl Pts',(-20.5871922922867,-49.2063549606646,
123.670130518056)) ;
#78730 = CARTESIAN_POINT('Ctrl Pts',(-20.9155298640661,-49.3963362228594,
123.474333218866)) ;
#78731 = CARTESIAN_POINT('Ctrl Pts',(-20.6142760088709,-49.2163471424406,
123.461828953088)) ;
#78732 = CARTESIAN_POINT('Ctrl Pts',(-20.9034492217782,-49.4062990034872,
123.212805454259)) ;
#78733 = CARTESIAN_POINT('Ctrl Pts',(-20.6046113070106,-49.2263099230684,
123.252607116101)) ;
#78734 = CARTESIAN_POINT('Ctrl Pts',(-20.8471090806343,-49.4162034081609,
122.958679801281)) ;
#78735 = CARTESIAN_POINT('Ctrl Pts',(-20.5595393178523,-49.2362143277422,
123.04930733304)) ;
#78736 = CARTESIAN_POINT('Ctrl Pts',(-20.7457693980936,-49.42626340264,122.714534227901)) ;
#78737 = CARTESIAN_POINT('Ctrl Pts',(-20.4784673873757,-49.2462743222212,
122.853990658576)) ;
#78738 = CARTESIAN_POINT('Ctrl Pts',(-20.6067290421162,-49.4361120246098,
122.496219298876)) ;
#78739 = CARTESIAN_POINT('Ctrl Pts',(-20.3672356811197,-49.256122944191,122.679339680775)) ;
#78740 = CARTESIAN_POINT('Ctrl Pts',(-20.429127558002,-49.4461424640216,122.301465539504)) ;
#78741 = CARTESIAN_POINT('Ctrl Pts',(-20.2251545164189,-49.2661533836029,
122.523536525192)) ;
#78742 = CARTESIAN_POINT('Ctrl Pts',(-20.2204806965802,-49.4561521796563,
122.141233524229)) ;
#78743 = CARTESIAN_POINT('Ctrl Pts',(-20.0582370435673,-49.2761630992376,
122.395350947196)) ;
#78744 = CARTESIAN_POINT('Ctrl Pts',(-19.9896519589879,-49.466062932349,122.02066491153)) ;
#78745 = CARTESIAN_POINT('Ctrl Pts',(-19.8735747112757,-49.2860738519302,
122.298896350739)) ;
#78746 = CARTESIAN_POINT('Ctrl Pts',(-19.7410945155474,-49.4759922052954,
121.94122468313)) ;
#78747 = CARTESIAN_POINT('Ctrl Pts',(-19.674729389547,-49.2960031248766,122.235344147617)) ;
#78748 = CARTESIAN_POINT('Ctrl Pts',(-19.4795590978959,-49.4860348966881,
121.905973034216)) ;
#78749 = CARTESIAN_POINT('Ctrl Pts',(-19.4655009066754,-49.3060458162693,
122.207142650007)) ;
#78750 = CARTESIAN_POINT('Ctrl Pts',(-19.2199428620433,-49.4959214299056,
121.916333239369)) ;
#78751 = CARTESIAN_POINT('Ctrl Pts',(-19.2578087796181,-49.3159323494868,
122.215430581112)) ;
#78752 = CARTESIAN_POINT('Ctrl Pts',(-18.9632658837111,-49.5059145748376,
121.97176876514)) ;
#78753 = CARTESIAN_POINT('Ctrl Pts',(-19.0524672904058,-49.3259254944189,
122.259778662686)) ;
#78754 = CARTESIAN_POINT('Ctrl Pts',(-18.7212920166706,-49.5158602556741,
122.070557018446)) ;
#78755 = CARTESIAN_POINT('Ctrl Pts',(-18.8588885297617,-49.3358711752553,
122.338808821512)) ;
#78756 = CARTESIAN_POINT('Ctrl Pts',(-18.4998162839576,-49.5258075128226,
122.209435357168)) ;
#78757 = CARTESIAN_POINT('Ctrl Pts',(-18.6817081096544,-49.3458184324039,
122.449910892272)) ;
#78758 = CARTESIAN_POINT('Ctrl Pts',(-18.3040709556288,-49.5358554166946,
122.386637839502)) ;
#78759 = CARTESIAN_POINT('Ctrl Pts',(-18.5251114670603,-49.3558663362759,
122.591672756877)) ;
#78760 = CARTESIAN_POINT('Ctrl Pts',(-18.1451172425397,-49.5457031157926,
122.590856449705)) ;
#78761 = CARTESIAN_POINT('Ctrl Pts',(-18.3979488685203,-49.3657140353738,
122.755046516047)) ;
#78762 = CARTESIAN_POINT('Ctrl Pts',(-18.0219137175214,-49.5556646067713,
122.821817640646)) ;
#78763 = CARTESIAN_POINT('Ctrl Pts',(-18.2993856846161,-49.3756755263525,
122.939814861468)) ;
#78764 = CARTESIAN_POINT('Ctrl Pts',(-17.9404590218548,-49.5656940691852,
123.072489705615)) ;
#78765 = CARTESIAN_POINT('Ctrl Pts',(-18.2342214104261,-49.3857049887665,
123.140352429838)) ;
#78766 = CARTESIAN_POINT('Ctrl Pts',(-17.9040753302903,-49.5756013002851,
123.330287135658)) ;
#78767 = CARTESIAN_POINT('Ctrl Pts',(-18.2051140105785,-49.3956122198664,
123.346589589261)) ;
#78768 = CARTESIAN_POINT('Ctrl Pts',(-17.9125098781886,-49.5855476789625,
123.59151601534)) ;
#78769 = CARTESIAN_POINT('Ctrl Pts',(-18.2118609481446,-49.4055585985438,
123.555572243342)) ;
#78770 = CARTESIAN_POINT('Ctrl Pts',(-17.9664056108719,-49.5955524477714,
123.848870528839)) ;
#78771 = CARTESIAN_POINT('Ctrl Pts',(-18.2549768267066,-49.4155633673526,
123.761455926636)) ;
#78772 = CARTESIAN_POINT('Ctrl Pts',(-18.0645967712818,-49.6055735687916,
124.093218904673)) ;
#78773 = CARTESIAN_POINT('Ctrl Pts',(-18.3335291813953,-49.4255844883728,
123.95693488968)) ;
#78774 = CARTESIAN_POINT('Ctrl Pts',(-18.20166916916,-49.6154644346442,124.314070124089)) ;
#78775 = CARTESIAN_POINT('Ctrl Pts',(-18.4431860779359,-49.4354753542255,
124.133615557219)) ;
#78776 = CARTESIAN_POINT('Ctrl Pts',(-18.3764527036545,-49.6254552434035,
124.509963683003)) ;
#78777 = CARTESIAN_POINT('Ctrl Pts',(-18.5830121977067,-49.4454661629847,
124.290330807483)) ;
#78778 = CARTESIAN_POINT('Ctrl Pts',(-18.5818191090548,-49.6354059015838,
124.671858407303)) ;
#78779 = CARTESIAN_POINT('Ctrl Pts',(-18.747304497956,-49.4554168211651,124.41984693504)) ;
#78780 = CARTESIAN_POINT('Ctrl Pts',(-18.8116465770786,-49.6453421112259,
124.795748611769)) ;
#78781 = CARTESIAN_POINT('Ctrl Pts',(-18.9311656103158,-49.4653530308072,
124.518959622352)) ;
#78782 = CARTESIAN_POINT('Ctrl Pts',(-19.060609101934,-49.6553252779508,124.878578886169)) ;
#78783 = CARTESIAN_POINT('Ctrl Pts',(-19.1303351363198,-49.475336197532,124.585224676569)) ;
#78784 = CARTESIAN_POINT('Ctrl Pts',(-19.3217571085301,-49.6653690751611,
124.91666347962)) ;
#78785 = CARTESIAN_POINT('Ctrl Pts',(-19.3392535710715,-49.4853799947423,
124.615693198187)) ;
#78786 = CARTESIAN_POINT('Ctrl Pts',(-19.5799756953144,-49.6751972913293,
124.909602893017)) ;
#78787 = CARTESIAN_POINT('Ctrl Pts',(-19.5458273138333,-49.4952082109106,
124.610045737877)) ;
#78788 = CARTESIAN_POINT('Ctrl Pts',(-19.8393726054502,-49.6852738587986,
124.85664781928)) ;
#78789 = CARTESIAN_POINT('Ctrl Pts',(-19.7533453820382,-49.5052847783798,
124.567682597387)) ;
#78790 = CARTESIAN_POINT('Ctrl Pts',(-20.0802989167195,-49.695125944488,124.761703259133)) ;
#78791 = CARTESIAN_POINT('Ctrl Pts',(-19.9460858927394,-49.5151368640692,
124.491728274294)) ;
#78792 = CARTESIAN_POINT('Ctrl Pts',(-20.3060674976868,-49.7051992118934,
124.62357472207)) ;
#78793 = CARTESIAN_POINT('Ctrl Pts',(-20.1267015988155,-49.5252101314746,
124.381226205106)) ;
#78794 = CARTESIAN_POINT('Ctrl Pts',(-20.4998566128569,-49.715040628317,124.452283158296)) ;
#78795 = CARTESIAN_POINT('Ctrl Pts',(-20.2817328184751,-49.5350515478982,
124.244194445969)) ;
#78796 = CARTESIAN_POINT('Ctrl Pts',(-20.6636690760732,-49.7250018864597,
124.248115309329)) ;
#78797 = CARTESIAN_POINT('Ctrl Pts',(-20.412783592269,-49.545012806041,124.080861225897)) ;
#78798 = CARTESIAN_POINT('Ctrl Pts',(-20.7900512078552,-49.7350385628917,
124.01661886947)) ;
#78799 = CARTESIAN_POINT('Ctrl Pts',(-20.5138903779245,-49.5550494824729,
123.895664546268)) ;
#78800 = CARTESIAN_POINT('Ctrl Pts',(-20.8734168717332,-49.7449171707555,
123.770739635638)) ;
#78801 = CARTESIAN_POINT('Ctrl Pts',(-20.5805838585332,-49.5649280903367,
123.698962322209)) ;
#78802 = CARTESIAN_POINT('Ctrl Pts',(-20.9135969835831,-49.7549773993943,
123.509473505383)) ;
#78803 = CARTESIAN_POINT('Ctrl Pts',(-20.6127292533526,-49.5749883189755,
123.489949387837)) ;
#78804 = CARTESIAN_POINT('Ctrl Pts',(-20.9079881466067,-49.7648443835551,
123.25020659995)) ;
#78805 = CARTESIAN_POINT('Ctrl Pts',(-20.6082434986379,-49.5848553031363,
123.282536664813)) ;
#78806 = CARTESIAN_POINT('Ctrl Pts',(-20.8572486897129,-49.7748499498078,
122.992248524987)) ;
#78807 = CARTESIAN_POINT('Ctrl Pts',(-20.5676533267145,-49.594860869389,123.076169999909)) ;
#78808 = CARTESIAN_POINT('Ctrl Pts',(-20.762604793853,-49.7848337382224,122.74750089323)) ;
#78809 = CARTESIAN_POINT('Ctrl Pts',(-20.4919395690296,-49.6048446578036,
122.88037156088)) ;
#78810 = CARTESIAN_POINT('Ctrl Pts',(-20.6258474890098,-49.794879595025,122.521714953376)) ;
#78811 = CARTESIAN_POINT('Ctrl Pts',(-20.3825347960662,-49.6148905146063,
122.699742010315)) ;
#78812 = CARTESIAN_POINT('Ctrl Pts',(-20.4560100049864,-49.8047054722409,
122.327215170004)) ;
#78813 = CARTESIAN_POINT('Ctrl Pts',(-20.246666541654,-49.6247163918222,122.544142037423)) ;
#78814 = CARTESIAN_POINT('Ctrl Pts',(-20.2521537954512,-49.8146959480823,
122.161777820805)) ;
#78815 = CARTESIAN_POINT('Ctrl Pts',(-20.0835826717048,-49.6347068676635,
122.411791024612)) ;
#78816 = CARTESIAN_POINT('Ctrl Pts',(-20.0211126978838,-49.8247395239811,
122.034178353224)) ;
#78817 = CARTESIAN_POINT('Ctrl Pts',(-19.8987503848234,-49.6447504435623,
122.30971013817)) ;
#78818 = CARTESIAN_POINT('Ctrl Pts',(-19.777116224908,-49.8345613162791,121.95001127881)) ;
#78819 = CARTESIAN_POINT('Ctrl Pts',(-19.7035546511395,-49.6545722358604,
122.242375346219)) ;
#78820 = CARTESIAN_POINT('Ctrl Pts',(-19.5167805110233,-49.844596281905,121.907971037186)) ;
#78821 = CARTESIAN_POINT('Ctrl Pts',(-19.4952862619387,-49.6646072014862,
122.208741497832)) ;
#78822 = CARTESIAN_POINT('Ctrl Pts',(-19.2533683214203,-49.8546211988381,
121.912502122714)) ;
#78823 = CARTESIAN_POINT('Ctrl Pts',(-19.2845564644904,-49.6746321184193,
122.212364842142)) ;
#78824 = CARTESIAN_POINT('Ctrl Pts',(-18.9991000929057,-49.8644731372142,
121.961278882202)) ;
#78825 = CARTESIAN_POINT('Ctrl Pts',(-19.0811423664437,-49.6844840567954,
122.251384496068)) ;
#78826 = CARTESIAN_POINT('Ctrl Pts',(-18.7536426684916,-49.8744641132389,
122.05437660085)) ;
#78827 = CARTESIAN_POINT('Ctrl Pts',(-18.8847759503893,-49.6944750328202,
122.325861028897)) ;
#78828 = CARTESIAN_POINT('Ctrl Pts',(-18.5295831348585,-49.8843819340426,
122.187580190372)) ;
#78829 = CARTESIAN_POINT('Ctrl Pts',(-18.7055278321113,-49.7043928536238,
122.432422178777)) ;
#78830 = CARTESIAN_POINT('Ctrl Pts',(-18.3298664401023,-49.8944106546072,
122.359492881443)) ;
#78831 = CARTESIAN_POINT('Ctrl Pts',(-18.5457533183806,-49.7144215741884,
122.569951033302)) ;
#78832 = CARTESIAN_POINT('Ctrl Pts',(-18.1652873216249,-49.9042935812163,
122.560433756627)) ;
#78833 = CARTESIAN_POINT('Ctrl Pts',(-18.4140890357409,-49.7243045007976,
122.730702147218)) ;
#78834 = CARTESIAN_POINT('Ctrl Pts',(-18.0361983460719,-49.9142978663359,
122.789426912429)) ;
#78835 = CARTESIAN_POINT('Ctrl Pts',(-18.3108162891678,-49.7343087859171,
122.913895707216)) ;
#78836 = CARTESIAN_POINT('Ctrl Pts',(-17.9490142971123,-49.9242815475437,
123.036925185825)) ;
#78837 = CARTESIAN_POINT('Ctrl Pts',(-18.2410673737591,-49.7442924671249,
123.111893582383)) ;
#78838 = CARTESIAN_POINT('Ctrl Pts',(-17.9061915788502,-49.9343225462736,
123.297274155858)) ;
#78839 = CARTESIAN_POINT('Ctrl Pts',(-18.2068074268591,-49.7543334658549,
123.32017254399)) ;
#78840 = CARTESIAN_POINT('Ctrl Pts',(-17.9087977232919,-49.9441549911407,
123.555650792529)) ;
#78841 = CARTESIAN_POINT('Ctrl Pts',(-18.2088904958492,-49.764165910722,123.526873108748)) ;
#78842 = CARTESIAN_POINT('Ctrl Pts',(-17.9562480237733,-49.9541499895711,
123.813979871575)) ;
#78843 = CARTESIAN_POINT('Ctrl Pts',(-18.2468487951362,-49.7741609091523,
123.733536626353)) ;
#78844 = CARTESIAN_POINT('Ctrl Pts',(-18.0487030673203,-49.9641815383207,
124.060868718032)) ;
#78845 = CARTESIAN_POINT('Ctrl Pts',(-18.3208110873252,-49.7841924579019,
123.93104838714)) ;
#78846 = CARTESIAN_POINT('Ctrl Pts',(-18.1801084382228,-49.9740469166262,
124.284334653775)) ;
#78847 = CARTESIAN_POINT('Ctrl Pts',(-18.4259334333969,-49.7940578362074,
124.109821606921)) ;
#78848 = CARTESIAN_POINT('Ctrl Pts',(-18.349414443886,-49.9840087640865,124.48401461094)) ;
#78849 = CARTESIAN_POINT('Ctrl Pts',(-18.56137656749,-49.8040196836677,124.269566724914)) ;
#78850 = CARTESIAN_POINT('Ctrl Pts',(-18.5525546908774,-49.9940437049007,
124.652146083555)) ;
#78851 = CARTESIAN_POINT('Ctrl Pts',(-18.7238875347409,-49.814054624482,124.404073431929)) ;
#78852 = CARTESIAN_POINT('Ctrl Pts',(-18.7782043026968,-50.0039286659178,
124.780909685904)) ;
#78853 = CARTESIAN_POINT('Ctrl Pts',(-18.9044058329455,-49.8239395854991,
124.507085842024)) ;
#78854 = CARTESIAN_POINT('Ctrl Pts',(-19.0271970939987,-50.0139942748367,
124.870056934582)) ;
#78855 = CARTESIAN_POINT('Ctrl Pts',(-19.1035994992475,-49.8340051944179,
124.578405575516)) ;
#78856 = CARTESIAN_POINT('Ctrl Pts',(-19.2820603187376,-50.0238334498784,
124.913884244328)) ;
#78857 = CARTESIAN_POINT('Ctrl Pts',(-19.3074891770789,-49.8438443694597,
124.613469338266)) ;
#78858 = CARTESIAN_POINT('Ctrl Pts',(-19.5464617510488,-50.0338960053783,
124.91313355718)) ;
#78859 = CARTESIAN_POINT('Ctrl Pts',(-19.5190104339783,-49.8539069249596,
124.61287087145)) ;
#78860 = CARTESIAN_POINT('Ctrl Pts',(-19.8024340996591,-50.0437931800712,
124.86696663086)) ;
#78861 = CARTESIAN_POINT('Ctrl Pts',(-19.7237883101448,-49.8638040996525,
124.575939415286)) ;
#78862 = CARTESIAN_POINT('Ctrl Pts',(-20.0476128623271,-50.0537238949946,
124.777581121099)) ;
#78863 = CARTESIAN_POINT('Ctrl Pts',(-19.9199318279951,-49.8737348145758,
124.504433101703)) ;
#78864 = CARTESIAN_POINT('Ctrl Pts',(-20.2759720547415,-50.0637679230722,
124.645229703626)) ;
#78865 = CARTESIAN_POINT('Ctrl Pts',(-20.1026202614428,-49.8837788426534,
124.398553782836)) ;
#78866 = CARTESIAN_POINT('Ctrl Pts',(-20.4748580560747,-50.0736541249255,
124.478049523045)) ;
#78867 = CARTESIAN_POINT('Ctrl Pts',(-20.2617301731961,-49.8936650445067,
124.264811487387)) ;
#78868 = CARTESIAN_POINT('Ctrl Pts',(-20.6437749691382,-50.0836472913923,
124.277011182786)) ;
#78869 = CARTESIAN_POINT('Ctrl Pts',(-20.396865308046,-49.9036582109736,124.103982270604)) ;
#78870 = CARTESIAN_POINT('Ctrl Pts',(-20.7746102356371,-50.0935867623795,
124.050904663403)) ;
#78871 = CARTESIAN_POINT('Ctrl Pts',(-20.5015353032639,-49.9135976819608,
123.92309830424)) ;
#78872 = CARTESIAN_POINT('Ctrl Pts',(-20.8649209946815,-50.1036032767337,
123.803687665005)) ;
#78873 = CARTESIAN_POINT('Ctrl Pts',(-20.5737859376745,-49.9236141963149,
123.725325490292)) ;
#78874 = CARTESIAN_POINT('Ctrl Pts',(-20.9107662308834,-50.1135333032105,
123.546758707782)) ;
#78875 = CARTESIAN_POINT('Ctrl Pts',(-20.610464245172,-49.9335442227918,123.519782903442)) ;
#78876 = CARTESIAN_POINT('Ctrl Pts',(-20.911194011502,-50.12358583872,123.282611468906)) ;
#78877 = CARTESIAN_POINT('Ctrl Pts',(-20.6108086511653,-49.9435967583012,
123.308465098402)) ;
#78878 = CARTESIAN_POINT('Ctrl Pts',(-20.8668229607976,-50.1334322419396,
123.027681885346)) ;
#78879 = CARTESIAN_POINT('Ctrl Pts',(-20.5753140241265,-49.9534431615209,
123.104521371413)) ;
#78880 = CARTESIAN_POINT('Ctrl Pts',(-20.7786326899319,-50.1433942847937,
122.781207115412)) ;
#78881 = CARTESIAN_POINT('Ctrl Pts',(-20.5047639491462,-49.963405204375,122.907340893886)) ;
#78882 = CARTESIAN_POINT('Ctrl Pts',(-20.6478070136151,-50.1534228355844,
122.552412487801)) ;
#78883 = CARTESIAN_POINT('Ctrl Pts',(-20.400105350936,-49.9734337551656,122.724304121501)) ;
#78884 = CARTESIAN_POINT('Ctrl Pts',(-20.4813154003197,-50.163333161302,122.352163354397)) ;
#78885 = CARTESIAN_POINT('Ctrl Pts',(-20.2669138792127,-49.9833440808833,
122.564103520818)) ;
#78886 = CARTESIAN_POINT('Ctrl Pts',(-20.2825162867926,-50.1732680731316,
122.182913771869)) ;
#78887 = CARTESIAN_POINT('Ctrl Pts',(-20.107876126385,-49.9932789927128,122.42870221035)) ;
#78888 = CARTESIAN_POINT('Ctrl Pts',(-20.0548359116222,-50.1833090798997,
122.04955872531)) ;
#78889 = CARTESIAN_POINT('Ctrl Pts',(-19.9257329909012,-50.0033199994809,
122.322016258521)) ;
#78890 = CARTESIAN_POINT('Ctrl Pts',(-19.8112788264557,-50.1931967127318,
121.958995011296)) ;
#78891 = CARTESIAN_POINT('Ctrl Pts',(-19.7308882259912,-50.0132076323131,
122.249563225972)) ;
#78892 = CARTESIAN_POINT('Ctrl Pts',(-19.5531495649776,-50.2031871438299,
121.911155500874)) ;
#78893 = CARTESIAN_POINT('Ctrl Pts',(-19.5243852785124,-50.0231980634112,
122.211289414015)) ;
#78894 = CARTESIAN_POINT('Ctrl Pts',(-19.2915318676023,-50.2131425803871,
121.909011127538)) ;
#78895 = CARTESIAN_POINT('Ctrl Pts',(-19.3150912261265,-50.0331534999684,
122.209571651062)) ;
#78896 = CARTESIAN_POINT('Ctrl Pts',(-19.0346123538188,-50.2230535284865,
121.951656547233)) ;
#78897 = CARTESIAN_POINT('Ctrl Pts',(-19.1095552462161,-50.0430644480677,
122.243685801554)) ;
#78898 = CARTESIAN_POINT('Ctrl Pts',(-18.7863546985277,-50.2330656045842,
122.038872975881)) ;
#78899 = CARTESIAN_POINT('Ctrl Pts',(-18.9109485915979,-50.0530765241654,
122.31345662738)) ;
#78900 = CARTESIAN_POINT('Ctrl Pts',(-18.556965523036,-50.2430929266591,122.16850540643)) ;
#78901 = CARTESIAN_POINT('Ctrl Pts',(-18.727435583092,-50.0631038462404,122.417161230504)) ;
#78902 = CARTESIAN_POINT('Ctrl Pts',(-18.3565173091168,-50.2529517016133,
122.332725267608)) ;
#78903 = CARTESIAN_POINT('Ctrl Pts',(-18.5670778973102,-50.0729626211945,
122.548532925854)) ;
#78904 = CARTESIAN_POINT('Ctrl Pts',(-18.1268538969883,-50.2663778944257,
122.600443072319)) ;
#78905 = CARTESIAN_POINT('Ctrl Pts',(-18.3833334664102,-50.086388814007,122.762717346392)) ;
#78906 = CARTESIAN_POINT('Ctrl Pts',(-17.975652168658,-50.2794619102071,122.913754436158)) ;
#78907 = CARTESIAN_POINT('Ctrl Pts',(-18.2623681321715,-50.0994728297884,
123.013391525604)) ;
#78908 = CARTESIAN_POINT('Ctrl Pts',(-17.9092019313838,-50.2929353589624,
123.261460162953)) ;
#78909 = CARTESIAN_POINT('Ctrl Pts',(-18.2092179634923,-50.1129462785436,
123.291511896051)) ;
#78910 = CARTESIAN_POINT('Ctrl Pts',(-17.9058612706005,-50.3027683167682,
123.519872041666)) ;
#78911 = CARTESIAN_POINT('Ctrl Pts',(-18.2065406001334,-50.1227792363495,
123.498250245797)) ;
#78912 = CARTESIAN_POINT('Ctrl Pts',(-17.9468858270987,-50.3127315902189,
123.778444889139)) ;
#78913 = CARTESIAN_POINT('Ctrl Pts',(-18.2393587805037,-50.1327425098001,
123.705106558061)) ;
#78914 = CARTESIAN_POINT('Ctrl Pts',(-18.0333597050335,-50.3227686640368,
124.027627149713)) ;
#78915 = CARTESIAN_POINT('Ctrl Pts',(-18.3085355866663,-50.1427795836181,
123.904453627933)) ;
#78916 = CARTESIAN_POINT('Ctrl Pts',(-18.1593001785433,-50.3326436670485,
124.254558222545)) ;
#78917 = CARTESIAN_POINT('Ctrl Pts',(-18.409286108333,-50.1526545866297,124.085999460383)) ;
#78918 = CARTESIAN_POINT('Ctrl Pts',(-18.325884168104,-50.3427113466747,124.46004911197)) ;
#78919 = CARTESIAN_POINT('Ctrl Pts',(-18.5425518166163,-50.1627222662559,
124.250393776869)) ;
#78920 = CARTESIAN_POINT('Ctrl Pts',(-18.5210703742666,-50.3525521968924,
124.62974311494)) ;
#78921 = CARTESIAN_POINT('Ctrl Pts',(-18.6986983036897,-50.1725631164736,
124.386149592484)) ;
#78922 = CARTESIAN_POINT('Ctrl Pts',(-18.8210606852306,-50.3658883953684,
124.810877501162)) ;
#78923 = CARTESIAN_POINT('Ctrl Pts',(-18.9386954921332,-50.1858993149496,
124.531065583499)) ;
#78924 = CARTESIAN_POINT('Ctrl Pts',(-19.1585310682842,-50.3791059191828,
124.908576997296)) ;
#78925 = CARTESIAN_POINT('Ctrl Pts',(-19.2087060042156,-50.199116838764,124.609228123008)) ;
#78926 = CARTESIAN_POINT('Ctrl Pts',(-19.5088595130128,-50.392440845674,124.91604614796)) ;
#78927 = CARTESIAN_POINT('Ctrl Pts',(-19.4889209379206,-50.2124517652553,
124.615199985815)) ;
#78928 = CARTESIAN_POINT('Ctrl Pts',(-19.7681867122677,-50.4024239462686,
124.876091752278)) ;
#78929 = CARTESIAN_POINT('Ctrl Pts',(-19.696392649381,-50.2224348658499,124.583239677521)) ;
#78930 = CARTESIAN_POINT('Ctrl Pts',(-20.0179829922509,-50.4124687221682,
124.790847910307)) ;
#78931 = CARTESIAN_POINT('Ctrl Pts',(-19.896227454566,-50.2324796417495,124.515046638421)) ;
#78932 = CARTESIAN_POINT('Ctrl Pts',(-20.2442444734349,-50.4222866453541,
124.666833014675)) ;
#78933 = CARTESIAN_POINT('Ctrl Pts',(-20.0772393601815,-50.2422975649354,
124.415835165722)) ;
#78934 = CARTESIAN_POINT('Ctrl Pts',(-20.4505999319598,-50.4323359593095,
124.502045800935)) ;
#78935 = CARTESIAN_POINT('Ctrl Pts',(-20.2423227107125,-50.2523468788908,
124.284011299718)) ;
#78936 = CARTESIAN_POINT('Ctrl Pts',(-20.681214714332,-50.4456396999321,124.239319481613)) ;
#78937 = CARTESIAN_POINT('Ctrl Pts',(-20.4268261522775,-50.2656506195133,
124.073810794489)) ;
#78938 = CARTESIAN_POINT('Ctrl Pts',(-20.8766371021415,-50.4621298954088,
123.846918741784)) ;
#78939 = CARTESIAN_POINT('Ctrl Pts',(-20.5831565547659,-50.28214081499,123.759929216494)) ;
#78940 = CARTESIAN_POINT('Ctrl Pts',(-20.9269267934179,-50.4788490603334,
123.405534034858)) ;
#78941 = CARTESIAN_POINT('Ctrl Pts',(-20.6233943759952,-50.2988599799146,
123.406758446571)) ;
#78942 = CARTESIAN_POINT('Ctrl Pts',(-20.8757804022393,-50.4920100540035,
123.063406602107)) ;
#78943 = CARTESIAN_POINT('Ctrl Pts',(-20.5824794341171,-50.3120209735847,
123.13310677555)) ;
#78944 = CARTESIAN_POINT('Ctrl Pts',(-20.7933286315034,-50.5020062761088,
122.814013822148)) ;
#78945 = CARTESIAN_POINT('Ctrl Pts',(-20.5165192334636,-50.32201719569,122.933581356952)) ;
#78946 = CARTESIAN_POINT('Ctrl Pts',(-20.6679470249481,-50.5120301156425,
122.582347913138)) ;
#78947 = CARTESIAN_POINT('Ctrl Pts',(-20.4162173324879,-50.3320410352238,
122.748251908727)) ;
#78948 = CARTESIAN_POINT('Ctrl Pts',(-20.4530703196355,-50.5252234376358,
122.310222407872)) ;
#78949 = CARTESIAN_POINT('Ctrl Pts',(-20.2443087067898,-50.345234357217,122.530542413722)) ;
#78950 = CARTESIAN_POINT('Ctrl Pts',(-20.0984605249762,-50.5418826094131,
122.045150356545)) ;
#78951 = CARTESIAN_POINT('Ctrl Pts',(-19.9606321286751,-50.3618935289943,
122.318489942363)) ;
#78952 = CARTESIAN_POINT('Ctrl Pts',(-19.591771529195,-50.5617927848988,121.892456854746)) ;
#78953 = CARTESIAN_POINT('Ctrl Pts',(-19.5552782569538,-50.38180370448,122.196329454903)) ;
#78954 = CARTESIAN_POINT('Ctrl Pts',(-19.0638261203275,-50.5816827727432,
121.920703930823)) ;
#78955 = CARTESIAN_POINT('Ctrl Pts',(-19.132921841017,-50.4016936923244,122.218924915738)) ;
#78956 = CARTESIAN_POINT('Ctrl Pts',(-18.5747132438271,-50.601688220758,122.12899945868)) ;
#78957 = CARTESIAN_POINT('Ctrl Pts',(-18.7416302351988,-50.4216991403392,
122.385558456999)) ;
#78958 = CARTESIAN_POINT('Ctrl Pts',(-18.188781745609,-50.6215246147853,122.488396022967)) ;
#78959 = CARTESIAN_POINT('Ctrl Pts',(-18.4328823682395,-50.4415355343665,
122.673074725378)) ;
#78960 = CARTESIAN_POINT('Ctrl Pts',(-17.9465286196628,-50.6415324086819,
122.961624501233)) ;
#78961 = CARTESIAN_POINT('Ctrl Pts',(-18.2390777138567,-50.4615433282632,
123.051656336489)) ;
#78962 = CARTESIAN_POINT('Ctrl Pts',(-17.8806923532301,-50.6613590449759,
123.484550765064)) ;
#78963 = CARTESIAN_POINT('Ctrl Pts',(-18.1864063185633,-50.4813699645572,
123.469998611925)) ;
#78964 = CARTESIAN_POINT('Ctrl Pts',(-17.9971845805368,-50.6813379879298,
124.002602226852)) ;
#78965 = CARTESIAN_POINT('Ctrl Pts',(-18.2795984569262,-50.501348907511,123.884440399758)) ;
#78966 = CARTESIAN_POINT('Ctrl Pts',(-18.2835587249482,-50.7012697897989,
124.448196582392)) ;
#78967 = CARTESIAN_POINT('Ctrl Pts',(-18.5086966003631,-50.5212807093801,
124.240917422711)) ;
#78968 = CARTESIAN_POINT('Ctrl Pts',(-18.7016353947585,-50.7210940902964,
124.769140330271)) ;
#78969 = CARTESIAN_POINT('Ctrl Pts',(-18.843158485295,-50.5411050098776,124.497674650865)) ;
#78970 = CARTESIAN_POINT('Ctrl Pts',(-19.2109425558759,-50.7411900916362,
124.929317666307)) ;
#78971 = CARTESIAN_POINT('Ctrl Pts',(-19.2506040110265,-50.5612010112175,
124.625816398005)) ;
#78972 = CARTESIAN_POINT('Ctrl Pts',(-19.7359254653231,-50.7609485077402,
124.907008256573)) ;
#78973 = CARTESIAN_POINT('Ctrl Pts',(-19.6705889099247,-50.5809594273214,
124.607973339329)) ;
#78974 = CARTESIAN_POINT('Ctrl Pts',(-20.2295077366304,-50.7810422006242,
124.703903011823)) ;
#78975 = CARTESIAN_POINT('Ctrl Pts',(-20.0654722041603,-50.6010531202055,
124.445475287471)) ;
#78976 = CARTESIAN_POINT('Ctrl Pts',(-20.4872438679076,-50.7941531665309,
124.46905554134)) ;
#78977 = CARTESIAN_POINT('Ctrl Pts',(-20.2716279488377,-50.6141640861122,
124.257625239002)) ;
#78978 = CARTESIAN_POINT('Ctrl Pts',(-20.5950497967993,-50.8008665413188,
124.330315451458)) ;
#78979 = CARTESIAN_POINT('Ctrl Pts',(-20.357892637621,-50.6208774609001,124.146615798218)) ;
#78980 = CARTESIAN_POINT('Ctrl Pts',(-18.357854658548,-12.0237682964362,124.08784748689)) ;
#78981 = CARTESIAN_POINT('Ctrl Pts',(-18.3365087757883,-12.0362829650914,
124.094103730057)) ;
#78982 = CARTESIAN_POINT('Ctrl Pts',(-18.3147575215239,-12.0487813483325,
124.09965999913)) ;
#78983 = CARTESIAN_POINT('Ctrl Pts',(-18.2929280361859,-12.0610923942012,
124.104426038987)) ;
#78984 = CARTESIAN_POINT('Ctrl Pts',(-18.2713540954504,-12.0732593220902,
124.109136285693)) ;
#78985 = CARTESIAN_POINT('Ctrl Pts',(-18.249704020901,-12.0852432736665,124.113074478837)) ;
#78986 = CARTESIAN_POINT('Ctrl Pts',(-18.2283156882755,-12.0968791175651,
124.116199920138)) ;
#78987 = CARTESIAN_POINT('Ctrl Pts',(-18.2227099783691,-12.0999287786375,
124.117019073158)) ;
#78988 = CARTESIAN_POINT('Ctrl Pts',(-18.2171223536073,-12.1029545273125,
124.117782654151)) ;
#78989 = CARTESIAN_POINT('Ctrl Pts',(-18.2115591098138,-12.1059533903454,
124.118490483479)) ;
#78990 = CARTESIAN_POINT('Ctrl Pts',(-18.18871992723,-12.1182648372088,124.121396385838)) ;
#78991 = CARTESIAN_POINT('Ctrl Pts',(-18.1654844706787,-12.1305575882187,
124.123462876928)) ;
#78992 = CARTESIAN_POINT('Ctrl Pts',(-18.1422288201718,-12.1426193191337,
124.124534691556)) ;
#78993 = CARTESIAN_POINT('Ctrl Pts',(-18.1247251875183,-12.1516977195438,
124.125341405156)) ;
#78994 = CARTESIAN_POINT('Ctrl Pts',(-18.1072106532554,-12.1606452459923,
124.125585421888)) ;
#78995 = CARTESIAN_POINT('Ctrl Pts',(-18.0898543520415,-12.1693713464509,
124.125218065099)) ;
#78996 = CARTESIAN_POINT('Ctrl Pts',(-20.5005102612951,-12.2002209833368,
122.802143462197)) ;
#78997 = CARTESIAN_POINT('Ctrl Pts',(-20.541093837296,-12.219219492016,122.806247489297)) ;
#78998 = CARTESIAN_POINT('Ctrl Pts',(-20.5830951416339,-12.2380808775341,
122.814354667494)) ;
#78999 = CARTESIAN_POINT('Ctrl Pts',(-20.6474219049173,-12.2647855663232,
122.837495408728)) ;
#79000 = CARTESIAN_POINT('Ctrl Pts',(-20.6724144804817,-12.2745814626532,
122.849334969911)) ;
#79001 = CARTESIAN_POINT('Ctrl Pts',(-20.7094156327346,-12.2874767103628,
122.874746786746)) ;
#79002 = CARTESIAN_POINT('Ctrl Pts',(-20.7230455646647,-12.2917830191842,
122.886284215876)) ;
#79003 = CARTESIAN_POINT('Ctrl Pts',(-20.7432461326241,-12.2970233590185,
122.908954347183)) ;
#79004 = CARTESIAN_POINT('Ctrl Pts',(-20.7506335985086,-12.2985684592622,
122.919056120632)) ;
#79005 = CARTESIAN_POINT('Ctrl Pts',(-20.7590911123199,-12.2996582019218,
122.933919924051)) ;
#79006 = CARTESIAN_POINT('Ctrl Pts',(-20.7611608911784,-12.2998488756498,
122.937926648299)) ;
#79007 = CARTESIAN_POINT('Ctrl Pts',(-20.7653472287969,-12.3000477257932,
122.94693639312)) ;
#79008 = CARTESIAN_POINT('Ctrl Pts',(-20.7673793575462,-12.3000112231311,
122.951954892876)) ;
#79009 = CARTESIAN_POINT('Ctrl Pts',(-20.7693310884309,-12.2998090284859,
122.957583705285)) ;
#79010 = CARTESIAN_POINT('Ctrl Pts',(-20.7695054962804,-12.2997892287744,
122.958095078672)) ;
#79011 = CARTESIAN_POINT('Ctrl Pts',(-20.7696845881009,-12.2997670653285,
122.958629049888)) ;
#79012 = CARTESIAN_POINT('Ctrl Pts',(-20.7696918833559,-12.2997661592856,
122.958650816641)) ;
#79013 = CARTESIAN_POINT('Ctrl Pts',(-20.769705894931,-12.2997644129052,122.958692652767)) ;
#79014 = CARTESIAN_POINT('Ctrl Pts',(-20.7697126114251,-12.2997635730312,
122.958712720312)) ;
#79015 = CARTESIAN_POINT('Ctrl Pts',(-20.7697224091429,-12.2997623438578,
122.958742013309)) ;
#79016 = CARTESIAN_POINT('Ctrl Pts',(-20.7697254935453,-12.2997619563241,
122.958751237791)) ;
#79017 = CARTESIAN_POINT('Ctrl Pts',(-20.7697308745325,-12.2997612792286,
122.958767335535)) ;
#79018 = CARTESIAN_POINT('Ctrl Pts',(-20.7697331715033,-12.2997609898763,
122.958774208704)) ;
#79019 = CARTESIAN_POINT('Ctrl Pts',(-20.7697378791215,-12.2997603961915,
122.958788298387)) ;
#79020 = CARTESIAN_POINT('Ctrl Pts',(-20.7697402897172,-12.2997600918325,
122.958795514906)) ;
#79021 = CARTESIAN_POINT('Ctrl Pts',(-20.7697463513703,-12.2997593256021,
122.958813665796)) ;
#79022 = CARTESIAN_POINT('Ctrl Pts',(-20.7697500017654,-12.2997588633541,
122.958824600409)) ;
#79023 = CARTESIAN_POINT('Ctrl Pts',(-20.7697641085656,-12.2997570738623,
122.958866872028)) ;
#79024 = CARTESIAN_POINT('Ctrl Pts',(-20.7697745563457,-12.2997557418272,
122.958898211664)) ;
#79025 = CARTESIAN_POINT('Ctrl Pts',(-20.7716678466195,-12.2995131409472,
122.964583297981)) ;
#79026 = CARTESIAN_POINT('Ctrl Pts',(-20.7732253610465,-12.2990951061691,
122.970317141544)) ;
#79027 = CARTESIAN_POINT('Ctrl Pts',(-20.7766185838289,-12.2974760939754,
122.986230079433)) ;
#79028 = CARTESIAN_POINT('Ctrl Pts',(-20.7777752979968,-12.2959381602225,
122.996417279488)) ;
#79029 = CARTESIAN_POINT('Ctrl Pts',(-20.7784284793249,-12.2910064741822,
123.021765385816)) ;
#79030 = CARTESIAN_POINT('Ctrl Pts',(-20.7768380405423,-12.2871205346287,
123.036695790602)) ;
#79031 = CARTESIAN_POINT('Ctrl Pts',(-20.7692015154357,-12.2758025819446,
123.072886879007)) ;
#79032 = CARTESIAN_POINT('Ctrl Pts',(-20.7612984889414,-12.2675400841427,
123.093650774925)) ;
#79033 = CARTESIAN_POINT('Ctrl Pts',(-20.7293644524945,-12.2382702301405,
123.157267294964)) ;
#79034 = CARTESIAN_POINT('Ctrl Pts',(-20.6937666914365,-12.2110963893297,
123.201398141947)) ;
#79035 = CARTESIAN_POINT('Ctrl Pts',(-20.6477460536494,-12.1788358604101,
123.242468690928)) ;
#79036 = CARTESIAN_POINT('Origin',(-5.63784594171726E-6,12.,130.056019952763)) ;
#79037 = CARTESIAN_POINT('',(-21.1595576762002,12.3,122.812674418818)) ;
#79038 = CARTESIAN_POINT('',(-21.1596428393339,11.6999371236922,122.812655579117)) ;
#79039 = CARTESIAN_POINT('Ctrl Pts',(-21.1595576760718,12.3,122.812674418862)) ;
#79040 = CARTESIAN_POINT('Ctrl Pts',(-21.1231857045382,12.3022605407561,122.701878867478)) ;
#79041 = CARTESIAN_POINT('Ctrl Pts',(-21.0335185861001,12.2002215949571,122.572974429341)) ;
#79042 = CARTESIAN_POINT('Ctrl Pts',(-21.0066064330477,12.0208669735961,122.543615355704)) ;
#79043 = CARTESIAN_POINT('Ctrl Pts',(-21.0129499559569,11.937009842197,122.550313273341)) ;
#79044 = CARTESIAN_POINT('Ctrl Pts',(-21.0334141863148,11.8415941256325,122.576365669548)) ;
#79045 = CARTESIAN_POINT('Ctrl Pts',(-21.0906762596813,11.7344433920243,122.653153592077)) ;
#79046 = CARTESIAN_POINT('Ctrl Pts',(-21.1409524880335,11.6999402726311,122.758036674297)) ;
#79047 = CARTESIAN_POINT('Ctrl Pts',(-21.1596428393339,11.6999371236922,122.812655579117)) ;
#79048 = CARTESIAN_POINT('',(-5.63784594223766E-6,11.7,130.056019952763)) ;
#79049 = CARTESIAN_POINT('Ctrl Pts',(-21.1596428393339,11.6999371236922,122.812655579117)) ;
#79050 = CARTESIAN_POINT('Ctrl Pts',(-21.1783331906335,11.6999339747533,122.867274483935)) ;
#79051 = CARTESIAN_POINT('Ctrl Pts',(-21.2028183674824,11.7344244983881,122.98086702099)) ;
#79052 = CARTESIAN_POINT('Ctrl Pts',(-21.2047930541468,11.8416345270515,123.076798355982)) ;
#79053 = CARTESIAN_POINT('Ctrl Pts',(-21.2043581510169,11.9369444204252,123.109719701306)) ;
#79054 = CARTESIAN_POINT('Ctrl Pts',(-21.2039085683262,12.0210152953098,123.119325478645)) ;
#79055 = CARTESIAN_POINT('Ctrl Pts',(-21.205181447895,12.1418774804202,123.09162894974)) ;
#79056 = CARTESIAN_POINT('Ctrl Pts',(-21.2026565890277,12.2655504187303,122.980780809732)) ;
#79057 = CARTESIAN_POINT('Ctrl Pts',(-21.1785313959741,12.3001251310309,122.867342837561)) ;
#79058 = CARTESIAN_POINT('Ctrl Pts',(-21.1595576760718,12.3,122.812674418862)) ;
#79059 = CARTESIAN_POINT('Ctrl Pts',(-21.1595576760718,12.3,122.812674418862)) ;
#79060 = CARTESIAN_POINT('Ctrl Pts',(-21.1231857045382,12.3022605407561,122.701878867478)) ;
#79061 = CARTESIAN_POINT('Ctrl Pts',(-21.0335185861001,12.2002215949571,122.572974429341)) ;
#79062 = CARTESIAN_POINT('Ctrl Pts',(-21.0066064330477,12.0208669735961,122.543615355704)) ;
#79063 = CARTESIAN_POINT('Ctrl Pts',(-21.0129499559569,11.937009842197,122.550313273341)) ;
#79064 = CARTESIAN_POINT('Ctrl Pts',(-21.0334141863148,11.8415941256325,122.576365669548)) ;
#79065 = CARTESIAN_POINT('Ctrl Pts',(-21.0906762596813,11.7344433920243,122.653153592077)) ;
#79066 = CARTESIAN_POINT('Ctrl Pts',(-21.1660906022086,11.6826887129352,122.810478215405)) ;
#79067 = CARTESIAN_POINT('Ctrl Pts',(-21.2028183674824,11.7344244983881,122.98086702099)) ;
#79068 = CARTESIAN_POINT('Ctrl Pts',(-21.2047930541468,11.8416345270515,123.076798355982)) ;
#79069 = CARTESIAN_POINT('Ctrl Pts',(-21.2043581510169,11.9369444204252,123.109719701306)) ;
#79070 = CARTESIAN_POINT('Ctrl Pts',(-21.2039085683262,12.0210152953098,123.119325478645)) ;
#79071 = CARTESIAN_POINT('Ctrl Pts',(-21.205181447895,12.1418774804202,123.09162894974)) ;
#79072 = CARTESIAN_POINT('Ctrl Pts',(-21.2026565890277,12.2655504187303,122.980780809732)) ;
#79073 = CARTESIAN_POINT('Ctrl Pts',(-21.1785313959741,12.3001251310309,122.867342837561)) ;
#79074 = CARTESIAN_POINT('Ctrl Pts',(-21.1595576760718,12.3,122.812674418862)) ;
#79075 = CARTESIAN_POINT('Ctrl Pts',(-21.3014729215226,12.4500000043639,122.764093940449)) ;
#79076 = CARTESIAN_POINT('Ctrl Pts',(-21.2417386817332,12.4533908072994,122.58468313231)) ;
#79077 = CARTESIAN_POINT('Ctrl Pts',(-21.1183669661588,12.3003323944147,122.368106075024)) ;
#79078 = CARTESIAN_POINT('Ctrl Pts',(-21.0828841600767,12.0313004597594,122.317703938634)) ;
#79079 = CARTESIAN_POINT('Ctrl Pts',(-21.0912110587446,11.9055147635765,122.329236338449)) ;
#79080 = CARTESIAN_POINT('Ctrl Pts',(-21.1188098709144,11.7623911882616,122.373395814998)) ;
#79081 = CARTESIAN_POINT('Ctrl Pts',(-21.1966797848952,11.6016650881281,122.503047298049)) ;
#79082 = CARTESIAN_POINT('Ctrl Pts',(-21.3085421953233,11.5240330679577,122.761739092861)) ;
#79083 = CARTESIAN_POINT('Ctrl Pts',(-21.3785516269951,11.6016367477315,123.03446770917)) ;
#79084 = CARTESIAN_POINT('Ctrl Pts',(-21.3966874043036,11.7624517905451,123.184919968199)) ;
#79085 = CARTESIAN_POINT('Ctrl Pts',(-21.4016453124917,11.905416630659,123.236367319138)) ;
#79086 = CARTESIAN_POINT('Ctrl Pts',(-21.4027247828246,12.0315229430405,123.251325161369)) ;
#79087 = CARTESIAN_POINT('Ctrl Pts',(-21.3995856881047,12.2128162203883,123.208193040234)) ;
#79088 = CARTESIAN_POINT('Ctrl Pts',(-21.3783532801531,12.3983256286576,123.034306001354)) ;
#79089 = CARTESIAN_POINT('Ctrl Pts',(-21.3321155076486,12.450187696004,122.852788427119)) ;
#79090 = CARTESIAN_POINT('Ctrl Pts',(-21.3014729215226,12.4500000043639,122.764093940449)) ;
#79091 = CARTESIAN_POINT('',(-21.1595576760718,12.3,122.812674418862)) ;
#79092 = CARTESIAN_POINT('Origin',(-5.63784594171726E-6,12.,130.056019952763)) ;
#79093 = CARTESIAN_POINT('',(-17.6588963672735,11.6999371505335,124.011011800868)) ;
#79094 = CARTESIAN_POINT('',(-5.63784594223766E-6,11.7,130.056019952763)) ;
#79095 = CARTESIAN_POINT('',(-17.6589816018599,12.3,124.010992891173)) ;
#79096 = CARTESIAN_POINT('Ctrl Pts',(-17.6588963672735,11.6999371505335,124.011011800868)) ;
#79097 = CARTESIAN_POINT('Ctrl Pts',(-17.6402059616163,11.6999340236683,123.956392954847)) ;
#79098 = CARTESIAN_POINT('Ctrl Pts',(-17.6157209902082,11.734424479462,123.842800166528)) ;
#79099 = CARTESIAN_POINT('Ctrl Pts',(-17.6137462730154,11.841634502012,123.746868949177)) ;
#79100 = CARTESIAN_POINT('Ctrl Pts',(-17.6141812884147,11.9369442552144,123.713947499122)) ;
#79101 = CARTESIAN_POINT('Ctrl Pts',(-17.614630652896,12.0210152204092,123.704342009584)) ;
#79102 = CARTESIAN_POINT('Ctrl Pts',(-17.6133579093719,12.1418772592244,123.732038413223)) ;
#79103 = CARTESIAN_POINT('Ctrl Pts',(-17.615882601329,12.265550626992,123.842886461929)) ;
#79104 = CARTESIAN_POINT('Ctrl Pts',(-17.6400079287178,12.3001250268061,123.956324488906)) ;
#79105 = CARTESIAN_POINT('Ctrl Pts',(-17.6589816021521,12.3,124.010992891073)) ;
#79106 = CARTESIAN_POINT('Ctrl Pts',(-17.6589816021521,12.3,124.010992891073)) ;
#79107 = CARTESIAN_POINT('Ctrl Pts',(-17.695354537387,12.3022593030227,124.121784712804)) ;
#79108 = CARTESIAN_POINT('Ctrl Pts',(-17.7850200523455,12.20022254417,124.250695376743)) ;
#79109 = CARTESIAN_POINT('Ctrl Pts',(-17.811932580282,12.0208678335766,124.280054163229)) ;
#79110 = CARTESIAN_POINT('Ctrl Pts',(-17.8055896930183,11.9370093101012,124.273352046235)) ;
#79111 = CARTESIAN_POINT('Ctrl Pts',(-17.7851245667583,11.8415943650359,124.247302411162)) ;
#79112 = CARTESIAN_POINT('Ctrl Pts',(-17.7278634241582,11.7344432406589,124.170513242669)) ;
#79113 = CARTESIAN_POINT('Ctrl Pts',(-17.6775867729323,11.6999402773988,124.065630646894)) ;
#79114 = CARTESIAN_POINT('Ctrl Pts',(-17.6588963672735,11.6999371505335,124.011011800868)) ;
#79115 = CARTESIAN_POINT('Ctrl Pts',(-17.6589816021521,12.3,124.010992891073)) ;
#79116 = CARTESIAN_POINT('Ctrl Pts',(-17.695354537387,12.3022593030227,124.121784712804)) ;
#79117 = CARTESIAN_POINT('Ctrl Pts',(-17.7850200523455,12.20022254417,124.250695376743)) ;
#79118 = CARTESIAN_POINT('Ctrl Pts',(-17.811932580282,12.0208678335766,124.280054163229)) ;
#79119 = CARTESIAN_POINT('Ctrl Pts',(-17.8055896930183,11.9370093101012,124.273352046235)) ;
#79120 = CARTESIAN_POINT('Ctrl Pts',(-17.7851245667583,11.8415943650359,124.247302411162)) ;
#79121 = CARTESIAN_POINT('Ctrl Pts',(-17.7278634241582,11.7344432406589,124.170513242669)) ;
#79122 = CARTESIAN_POINT('Ctrl Pts',(-17.6524484473213,11.6826887957701,124.01318934901)) ;
#79123 = CARTESIAN_POINT('Ctrl Pts',(-17.6157209902082,11.734424479462,123.842800166528)) ;
#79124 = CARTESIAN_POINT('Ctrl Pts',(-17.6137462730154,11.841634502012,123.746868949177)) ;
#79125 = CARTESIAN_POINT('Ctrl Pts',(-17.6141812884147,11.9369442552144,123.713947499122)) ;
#79126 = CARTESIAN_POINT('Ctrl Pts',(-17.614630652896,12.0210152204092,123.704342009584)) ;
#79127 = CARTESIAN_POINT('Ctrl Pts',(-17.6133579093719,12.1418772592244,123.732038413223)) ;
#79128 = CARTESIAN_POINT('Ctrl Pts',(-17.615882601329,12.265550626992,123.842886461929)) ;
#79129 = CARTESIAN_POINT('Ctrl Pts',(-17.6400079287178,12.3001250268061,123.956324488906)) ;
#79130 = CARTESIAN_POINT('Ctrl Pts',(-17.6589816021521,12.3,124.010992891073)) ;
#79131 = CARTESIAN_POINT('Ctrl Pts',(-17.5170663566028,12.4500000035941,124.059573369615)) ;
#79132 = CARTESIAN_POINT('Ctrl Pts',(-17.5768010750503,12.4533889497169,124.238978500622)) ;
#79133 = CARTESIAN_POINT('Ctrl Pts',(-17.7001719976827,12.3003338187364,124.455565035223)) ;
#79134 = CARTESIAN_POINT('Ctrl Pts',(-17.735655182611,12.0313017495778,124.505966784337)) ;
#79135 = CARTESIAN_POINT('Ctrl Pts',(-17.727328311671,11.9055139654912,124.494427918119)) ;
#79136 = CARTESIAN_POINT('Ctrl Pts',(-17.6997289374594,11.7623915473154,124.450272614137)) ;
#79137 = CARTESIAN_POINT('Ctrl Pts',(-17.6218598761679,11.6016648611214,124.320619335508)) ;
#79138 = CARTESIAN_POINT('Ctrl Pts',(-17.5099968647986,11.5240331921794,124.061928577266)) ;
#79139 = CARTESIAN_POINT('Ctrl Pts',(-17.4399877214087,11.6016367193622,123.789199422435)) ;
#79140 = CARTESIAN_POINT('Ctrl Pts',(-17.4218519288077,11.7624517529768,123.638747342328)) ;
#79141 = CARTESIAN_POINT('Ctrl Pts',(-17.4168941310285,11.9054163828466,123.587299846138)) ;
#79142 = CARTESIAN_POINT('Ctrl Pts',(-17.415814460062,12.0315228305656,123.572342418142)) ;
#79143 = CARTESIAN_POINT('Ctrl Pts',(-17.4189536889037,12.2128158889338,123.615474365746)) ;
#79144 = CARTESIAN_POINT('Ctrl Pts',(-17.4401858916256,12.3983259401867,123.789361234211)) ;
#79145 = CARTESIAN_POINT('Ctrl Pts',(-17.486423826463,12.4501875413069,123.970878916215)) ;
#79146 = CARTESIAN_POINT('Ctrl Pts',(-17.5170663566028,12.4500000035941,124.059573369615)) ;
#79147 = CARTESIAN_POINT('',(-17.6589816021521,12.3,124.010992891073)) ;
#79148 = CARTESIAN_POINT('Origin',(-5.63784594070025E-6,-12.,130.056019952763)) ;
#79149 = CARTESIAN_POINT('',(-17.6589027590969,-11.6999371236917,124.011030194063)) ;
#79150 = CARTESIAN_POINT('',(-5.63784594017984E-6,-11.7,130.056019952763)) ;
#79151 = CARTESIAN_POINT('',(-17.65898160186,-12.3,124.010992891173)) ;
#79152 = CARTESIAN_POINT('Ctrl Pts',(-17.6589027590969,-11.6999371236917,
124.011030194063)) ;
#79153 = CARTESIAN_POINT('Ctrl Pts',(-17.6776053053521,-11.6999339747542,
124.065644924303)) ;
#79154 = CARTESIAN_POINT('Ctrl Pts',(-17.72786935392,-11.7344244983967,124.170412828578)) ;
#79155 = CARTESIAN_POINT('Ctrl Pts',(-17.7850982943228,-11.8416345270247,
124.247429507382)) ;
#79156 = CARTESIAN_POINT('Ctrl Pts',(-17.8056170712146,-11.9369444204012,
124.27317798136)) ;
#79157 = CARTESIAN_POINT('Ctrl Pts',(-17.8118590245238,-12.021015295271,124.280493109677)) ;
#79158 = CARTESIAN_POINT('Ctrl Pts',(-17.7938799763284,-12.1418774804083,
124.259386907686)) ;
#79159 = CARTESIAN_POINT('Ctrl Pts',(-17.7279443615378,-12.2655504187416,
124.17024556063)) ;
#79160 = CARTESIAN_POINT('Ctrl Pts',(-17.6774905688518,-12.3001251310252,
124.065820404267)) ;
#79161 = CARTESIAN_POINT('Ctrl Pts',(-17.6589816021521,-12.3,124.010992891073)) ;
#79162 = CARTESIAN_POINT('Ctrl Pts',(-17.6589816021521,-12.3,124.010992891073)) ;
#79163 = CARTESIAN_POINT('Ctrl Pts',(-17.6198247664454,-12.302260540837,123.901150655369)) ;
#79164 = CARTESIAN_POINT('Ctrl Pts',(-17.6116850160222,-12.2002215949029,
123.744337739047)) ;
#79165 = CARTESIAN_POINT('Ctrl Pts',(-17.6149593962428,-12.0208669736416,
123.704645200407)) ;
#79166 = CARTESIAN_POINT('Ctrl Pts',(-17.6140513077368,-11.9370098422088,
123.713825492269)) ;
#79167 = CARTESIAN_POINT('Ctrl Pts',(-17.6138457601763,-11.8415941256522,
123.746953574365)) ;
#79168 = CARTESIAN_POINT('Ctrl Pts',(-17.6156540763921,-11.7344433920138,
123.842724447157)) ;
#79169 = CARTESIAN_POINT('Ctrl Pts',(-17.6402002128438,-11.6999402726293,
123.956415463829)) ;
#79170 = CARTESIAN_POINT('Ctrl Pts',(-17.6589027590969,-11.6999371236917,
124.011030194063)) ;
#79171 = CARTESIAN_POINT('Origin',(-5.63784594070025E-6,-12.,130.056019952763)) ;
#79172 = CARTESIAN_POINT('',(-21.1595576754736,-12.3,122.812674419067)) ;
#79173 = CARTESIAN_POINT('',(-21.1596366183962,-11.6999371505325,122.812637127424)) ;
#79174 = CARTESIAN_POINT('Ctrl Pts',(-21.1595576755874,-12.3,122.812674419028)) ;
#79175 = CARTESIAN_POINT('Ctrl Pts',(-21.1987114653594,-12.3022593030704,
122.922514297446)) ;
#79176 = CARTESIAN_POINT('Ctrl Pts',(-21.2068562966847,-12.2002225441948,
123.079331151619)) ;
#79177 = CARTESIAN_POINT('Ctrl Pts',(-21.2035814449539,-12.020867833611,123.1190236928)) ;
#79178 = CARTESIAN_POINT('Ctrl Pts',(-21.2044864574362,-11.937009310127,123.109840472177)) ;
#79179 = CARTESIAN_POINT('Ctrl Pts',(-21.204694405188,-11.8415943650587,123.076714022891)) ;
#79180 = CARTESIAN_POINT('Ctrl Pts',(-21.2028845898013,-11.7344432406558,
122.980942735961)) ;
#79181 = CARTESIAN_POINT('Ctrl Pts',(-21.1783390856595,-11.6999402773968,
122.867251844514)) ;
#79182 = CARTESIAN_POINT('Ctrl Pts',(-21.1596366183962,-11.6999371505325,
122.812637127424)) ;
#79183 = CARTESIAN_POINT('',(-5.63784594017984E-6,-11.7,130.056019952763)) ;
#79184 = CARTESIAN_POINT('Ctrl Pts',(-21.1596366183962,-11.6999371505325,
122.812637127424)) ;
#79185 = CARTESIAN_POINT('Ctrl Pts',(-21.1409341511322,-11.6999340236682,
122.758022410332)) ;
#79186 = CARTESIAN_POINT('Ctrl Pts',(-21.0906697862186,-11.7344244794726,
122.653254433413)) ;
#79187 = CARTESIAN_POINT('Ctrl Pts',(-21.0334409420522,-11.8416345019856,
122.576237828854)) ;
#79188 = CARTESIAN_POINT('Ctrl Pts',(-21.0129220122535,-11.9369442551916,
122.550489340921)) ;
#79189 = CARTESIAN_POINT('Ctrl Pts',(-21.0066804077936,-12.0210152203759,
122.543174306292)) ;
#79190 = CARTESIAN_POINT('Ctrl Pts',(-21.0246592715631,-12.1418772592091,
122.564280492712)) ;
#79191 = CARTESIAN_POINT('Ctrl Pts',(-21.0905949626881,-12.2655506269821,
122.653421665207)) ;
#79192 = CARTESIAN_POINT('Ctrl Pts',(-21.141048681955,-12.3001250267877,122.757846947397)) ;
#79193 = CARTESIAN_POINT('Ctrl Pts',(-21.1595576755874,-12.3,122.812674419028)) ;
#79194 = CARTESIAN_POINT('Ctrl Pts',(-21.1595576755874,-12.3,122.812674419028)) ;
#79195 = CARTESIAN_POINT('Ctrl Pts',(-21.1987114653594,-12.3022593030704,
122.922514297446)) ;
#79196 = CARTESIAN_POINT('Ctrl Pts',(-21.2068562966847,-12.2002225441948,
123.079331151619)) ;
#79197 = CARTESIAN_POINT('Ctrl Pts',(-21.2035814449539,-12.020867833611,123.1190236928)) ;
#79198 = CARTESIAN_POINT('Ctrl Pts',(-21.2044864574362,-11.937009310127,123.109840472177)) ;
#79199 = CARTESIAN_POINT('Ctrl Pts',(-21.204694405188,-11.8415943650587,123.076714022891)) ;
#79200 = CARTESIAN_POINT('Ctrl Pts',(-21.2028845898013,-11.7344432406558,
122.980942735961)) ;
#79201 = CARTESIAN_POINT('Ctrl Pts',(-21.166066333588,-11.6826887957666,122.810406398789)) ;
#79202 = CARTESIAN_POINT('Ctrl Pts',(-21.0906697862186,-11.7344244794726,
122.653254433413)) ;
#79203 = CARTESIAN_POINT('Ctrl Pts',(-21.0334409420522,-11.8416345019856,
122.576237828854)) ;
#79204 = CARTESIAN_POINT('Ctrl Pts',(-21.0129220122535,-11.9369442551916,
122.550489340921)) ;
#79205 = CARTESIAN_POINT('Ctrl Pts',(-21.0066804077936,-12.0210152203759,
122.543174306292)) ;
#79206 = CARTESIAN_POINT('Ctrl Pts',(-21.0246592715631,-12.1418772592091,
122.564280492712)) ;
#79207 = CARTESIAN_POINT('Ctrl Pts',(-21.0905949626881,-12.2655506269821,
122.653421665207)) ;
#79208 = CARTESIAN_POINT('Ctrl Pts',(-21.141048681955,-12.3001250267877,122.757846947397)) ;
#79209 = CARTESIAN_POINT('Ctrl Pts',(-21.1595576755874,-12.3,122.812674419028)) ;
#79210 = CARTESIAN_POINT('Ctrl Pts',(-21.3014729215271,-12.4500000013844,
122.764093940462)) ;
#79211 = CARTESIAN_POINT('Ctrl Pts',(-21.3642139707748,-12.4533889553457,
122.942469943529)) ;
#79212 = CARTESIAN_POINT('Ctrl Pts',(-21.3994544235377,-12.3003338159049,
123.189225332334)) ;
#79213 = CARTESIAN_POINT('Ctrl Pts',(-21.4023026040227,-12.031301750527,123.250798708205)) ;
#79214 = CARTESIAN_POINT('Ctrl Pts',(-21.4018113001397,-11.9055139651401,
123.236577567789)) ;
#79215 = CARTESIAN_POINT('Ctrl Pts',(-21.3965611953891,-11.7623915476468,
123.184771653818)) ;
#79216 = CARTESIAN_POINT('Ctrl Pts',(-21.3786395141694,-11.6016648610055,
123.034597166172)) ;
#79217 = CARTESIAN_POINT('Ctrl Pts',(-21.3085026878959,-11.5240331923606,
122.761622685277)) ;
#79218 = CARTESIAN_POINT('Ctrl Pts',(-21.1966891219787,-11.6016367190622,
122.503204035368)) ;
#79219 = CARTESIAN_POINT('Ctrl Pts',(-21.118819138729,-11.7624517530713,122.373200185185)) ;
#79220 = CARTESIAN_POINT('Ctrl Pts',(-21.0912084270103,-11.9054163827587,
122.329507242695)) ;
#79221 = CARTESIAN_POINT('Ctrl Pts',(-21.0828952761476,-12.0315228306677,
122.317025982144)) ;
#79222 = CARTESIAN_POINT('Ctrl Pts',(-21.1068470535444,-12.212815888551,122.353033370586)) ;
#79223 = CARTESIAN_POINT('Ctrl Pts',(-21.1966316872743,-12.3983259410573,
122.503453345861)) ;
#79224 = CARTESIAN_POINT('Ctrl Pts',(-21.2713327489301,-12.450187539844,122.675227520146)) ;
#79225 = CARTESIAN_POINT('Ctrl Pts',(-21.3014729215271,-12.4500000013844,
122.764093940462)) ;
#79226 = CARTESIAN_POINT('',(-21.1595576755874,-12.3,122.812674419028)) ;
#79227 = CARTESIAN_POINT('Ctrl Pts',(-17.6589816021521,-12.3,124.010992891073)) ;
#79228 = CARTESIAN_POINT('Ctrl Pts',(-17.6198247664454,-12.302260540837,123.901150655369)) ;
#79229 = CARTESIAN_POINT('Ctrl Pts',(-17.6116850160222,-12.2002215949029,
123.744337739047)) ;
#79230 = CARTESIAN_POINT('Ctrl Pts',(-17.6149593962428,-12.0208669736416,
123.704645200407)) ;
#79231 = CARTESIAN_POINT('Ctrl Pts',(-17.6140513077368,-11.9370098422088,
123.713825492269)) ;
#79232 = CARTESIAN_POINT('Ctrl Pts',(-17.6138457601763,-11.8415941256522,
123.746953574365)) ;
#79233 = CARTESIAN_POINT('Ctrl Pts',(-17.6156540763921,-11.7344433920138,
123.842724447157)) ;
#79234 = CARTESIAN_POINT('Ctrl Pts',(-17.6524732810711,-11.682688712935,124.013260972172)) ;
#79235 = CARTESIAN_POINT('Ctrl Pts',(-17.72786935392,-11.7344244983967,124.170412828578)) ;
#79236 = CARTESIAN_POINT('Ctrl Pts',(-17.7850982943228,-11.8416345270247,
124.247429507382)) ;
#79237 = CARTESIAN_POINT('Ctrl Pts',(-17.8056170712146,-11.9369444204012,
124.27317798136)) ;
#79238 = CARTESIAN_POINT('Ctrl Pts',(-17.8118590245238,-12.021015295271,124.280493109677)) ;
#79239 = CARTESIAN_POINT('Ctrl Pts',(-17.7938799763284,-12.1418774804083,
124.259386907686)) ;
#79240 = CARTESIAN_POINT('Ctrl Pts',(-17.7279443615378,-12.2655504187416,
124.17024556063)) ;
#79241 = CARTESIAN_POINT('Ctrl Pts',(-17.6774905688518,-12.3001251310252,
124.065820404267)) ;
#79242 = CARTESIAN_POINT('Ctrl Pts',(-17.6589816021521,-12.3,124.010992891073)) ;
#79243 = CARTESIAN_POINT('Ctrl Pts',(-17.5170663564952,-12.4500000035939,
124.059573369301)) ;
#79244 = CARTESIAN_POINT('Ctrl Pts',(-17.4543214499664,-12.4533908062079,
123.881193173708)) ;
#79245 = CARTESIAN_POINT('Ctrl Pts',(-17.4190874317839,-12.3003323949396,
123.634444787988)) ;
#79246 = CARTESIAN_POINT('Ctrl Pts',(-17.4162387146148,-12.0313004596384,
123.572871338394)) ;
#79247 = CARTESIAN_POINT('Ctrl Pts',(-17.4167260337872,-11.905514763682,123.587087385896)) ;
#79248 = CARTESIAN_POINT('Ctrl Pts',(-17.4219791397424,-11.76239118819,123.638896252699)) ;
#79249 = CARTESIAN_POINT('Ctrl Pts',(-17.4398990467708,-11.6016650883087,
123.789069843982)) ;
#79250 = CARTESIAN_POINT('Ctrl Pts',(-17.5100369831582,-11.5240330679591,
124.062044775725)) ;
#79251 = CARTESIAN_POINT('Ctrl Pts',(-17.6218499912451,-11.6016367475424,
124.320463176737)) ;
#79252 = CARTESIAN_POINT('Ctrl Pts',(-17.6997200962288,-11.7624517905878,
124.450467158943)) ;
#79253 = CARTESIAN_POINT('Ctrl Pts',(-17.7273306316869,-11.9054166305896,
124.494160054312)) ;
#79254 = CARTESIAN_POINT('Ctrl Pts',(-17.7356441949461,-12.0315229428807,
124.50664151924)) ;
#79255 = CARTESIAN_POINT('Ctrl Pts',(-17.7116922052291,-12.2128162206925,
124.470634075889)) ;
#79256 = CARTESIAN_POINT('Ctrl Pts',(-17.6219076292031,-12.3983256278298,
124.320213840095)) ;
#79257 = CARTESIAN_POINT('Ctrl Pts',(-17.5472065053376,-12.4501876978419,
124.148439850519)) ;
#79258 = CARTESIAN_POINT('Ctrl Pts',(-17.5170663564952,-12.4500000035939,
124.059573369301)) ;
#79259 = CARTESIAN_POINT('',(-17.6589816021521,-12.3,124.010992891073)) ;
#79260 = CARTESIAN_POINT('Origin',(-5.63784594070025E-6,12.,130.056019952763)) ;
#79261 = CARTESIAN_POINT('',(3.7844009271522,11.7,131.3514993817)) ;
#79262 = CARTESIAN_POINT('Origin',(3.7844009271522,12.,131.3514993817)) ;
#79263 = CARTESIAN_POINT('',(-22.5645297816473,11.7,122.331723857726)) ;
#79264 = CARTESIAN_POINT('',(-5.63784594017984E-6,11.7,130.056019952763)) ;
#79265 = CARTESIAN_POINT('',(-22.5645297816474,12.3,122.331723857726)) ;
#79266 = CARTESIAN_POINT('Origin',(-22.5645297816474,12.,122.331723857726)) ;
#79267 = CARTESIAN_POINT('Origin',(-22.5645297816474,12.,122.331723857726)) ;
#79268 = CARTESIAN_POINT('Origin',(6.05149556563793,0.999999999999999,124.728771423451)) ;
#79269 = CARTESIAN_POINT('Origin',(-22.7064450278348,12.3,122.283143379141)) ;
#79270 = CARTESIAN_POINT('',(-22.7064450278348,12.1500000035778,122.283143379141)) ;
#79271 = CARTESIAN_POINT('Ctrl Pts',(-22.7064450278348,12.1500000035778,122.283143379141)) ;
#79272 = CARTESIAN_POINT('Ctrl Pts',(-22.6937453390508,12.1502314747086,122.246044537944)) ;
#79273 = CARTESIAN_POINT('Ctrl Pts',(-22.6683574552983,12.1175431645324,122.171880431747)) ;
#79274 = CARTESIAN_POINT('Ctrl Pts',(-22.6525723366187,12.0000444315862,122.125768308755)) ;
#79275 = CARTESIAN_POINT('Ctrl Pts',(-22.6683514162181,11.8823598076173,122.171862790143)) ;
#79276 = CARTESIAN_POINT('Ctrl Pts',(-22.7064423304138,11.8336812214274,122.283135499326)) ;
#79277 = CARTESIAN_POINT('Ctrl Pts',(-22.7445380204197,11.8823694052799,122.394422159798)) ;
#79278 = CARTESIAN_POINT('Ctrl Pts',(-22.7603151873203,12.0000313447684,122.440511053734)) ;
#79279 = CARTESIAN_POINT('Ctrl Pts',(-22.74452995505,12.1175454374094,122.394398598916)) ;
#79280 = CARTESIAN_POINT('Ctrl Pts',(-22.7191521346486,12.1502048378774,122.320263890184)) ;
#79281 = CARTESIAN_POINT('Ctrl Pts',(-22.7064450278348,12.1500000035778,122.283143379141)) ;
#79282 = CARTESIAN_POINT('Ctrl Pts',(-22.5645297816474,12.3,122.331723857726)) ;
#79283 = CARTESIAN_POINT('Ctrl Pts',(-22.7064450278348,12.1500000035778,122.283143379141)) ;
#79284 = CARTESIAN_POINT('Ctrl Pts',(-22.5391304026157,12.3004629406991,122.257526171057)) ;
#79285 = CARTESIAN_POINT('Ctrl Pts',(-22.6937453390508,12.1502314747086,122.246044537944)) ;
#79286 = CARTESIAN_POINT('Ctrl Pts',(-22.4883546371039,12.2350863374522,122.109197964485)) ;
#79287 = CARTESIAN_POINT('Ctrl Pts',(-22.6683574552983,12.1175431645324,122.171880431747)) ;
#79288 = CARTESIAN_POINT('Ctrl Pts',(-22.456784402798,12.0000888605178,122.016973727421)) ;
#79289 = CARTESIAN_POINT('Ctrl Pts',(-22.6525723366187,12.0000444315862,122.125768308755)) ;
#79290 = CARTESIAN_POINT('Ctrl Pts',(-22.4883425568402,11.7647196121379,122.109162675133)) ;
#79291 = CARTESIAN_POINT('Ctrl Pts',(-22.6683514162181,11.8823598076173,122.171862790143)) ;
#79292 = CARTESIAN_POINT('Ctrl Pts',(-22.5645243863183,11.6673624555447,122.331708096674)) ;
#79293 = CARTESIAN_POINT('Ctrl Pts',(-22.7064423304138,11.8336812214274,122.283135499326)) ;
#79294 = CARTESIAN_POINT('Ctrl Pts',(-22.6407157694817,11.7647388086052,122.554281426824)) ;
#79295 = CARTESIAN_POINT('Ctrl Pts',(-22.7445380204197,11.8823694052799,122.394422159798)) ;
#79296 = CARTESIAN_POINT('Ctrl Pts',(-22.6722700958943,12.0000626848499,122.646459193111)) ;
#79297 = CARTESIAN_POINT('Ctrl Pts',(-22.7603151873203,12.0000313447684,122.440511053734)) ;
#79298 = CARTESIAN_POINT('Ctrl Pts',(-22.640699636509,12.2350908868498,122.554234298536)) ;
#79299 = CARTESIAN_POINT('Ctrl Pts',(-22.74452995505,12.1175454374094,122.394398598916)) ;
#79300 = CARTESIAN_POINT('Ctrl Pts',(-22.5899439964264,12.3004096643473,122.405964883176)) ;
#79301 = CARTESIAN_POINT('Ctrl Pts',(-22.7191521346486,12.1502048378774,122.320263890184)) ;
#79302 = CARTESIAN_POINT('Ctrl Pts',(-22.5645297816474,12.3,122.331723857726)) ;
#79303 = CARTESIAN_POINT('Ctrl Pts',(-22.7064450278348,12.1500000035778,122.283143379141)) ;
#79304 = CARTESIAN_POINT('',(-22.5645297816474,12.3,122.331723857726)) ;
#79305 = CARTESIAN_POINT('Origin',(22.7064337521429,-12.,137.828896526385)) ;
#79306 = CARTESIAN_POINT('',(3.78440092715221,-12.3,131.3514993817)) ;
#79307 = CARTESIAN_POINT('Origin',(3.7844009271522,-12.,131.3514993817)) ;
#79308 = CARTESIAN_POINT('',(-22.7064450278348,-12.3,122.283143379141)) ;
#79309 = CARTESIAN_POINT('',(22.7064337521429,-12.3,137.828896526385)) ;
#79310 = CARTESIAN_POINT('Origin',(-22.7064450278348,-12.,122.283143379141)) ;
#79311 = CARTESIAN_POINT('Origin',(-22.7064450278348,-12.3,122.283143379141)) ;
#79312 = CARTESIAN_POINT('Origin',(3.78440656499815,14.,131.351482912198)) ;
#79313 = CARTESIAN_POINT('Origin',(-19.4092696390626,-30.19753203383,123.411833654984)) ;
#79314 = CARTESIAN_POINT('',(-18.259825879779,13.5907660201144,123.80531165987)) ;
#79315 = CARTESIAN_POINT('',(-18.259825879779,13.6088050314641,123.80531165987)) ;
#79316 = CARTESIAN_POINT('',(-18.259825879779,-30.19753203383,123.80531165987)) ;
#79317 = CARTESIAN_POINT('',(-19.3053878987246,13.6947924674767,122.201356690909)) ;
#79318 = CARTESIAN_POINT('Ctrl Pts',(-19.3053878987355,13.694792467579,122.201356691093)) ;
#79319 = CARTESIAN_POINT('Ctrl Pts',(-19.2790015565985,13.6935493748007,122.203621136616)) ;
#79320 = CARTESIAN_POINT('Ctrl Pts',(-19.2527011620726,13.6923108864917,122.206747112924)) ;
#79321 = CARTESIAN_POINT('Ctrl Pts',(-19.2199880841637,13.6907569978569,122.211724480067)) ;
#79322 = CARTESIAN_POINT('Ctrl Pts',(-19.2134652193957,13.6904465142337,122.212771451581)) ;
#79323 = CARTESIAN_POINT('Ctrl Pts',(-19.2018448836823,13.6898920627905,122.214733957618)) ;
#79324 = CARTESIAN_POINT('Ctrl Pts',(-19.1967441127338,13.6896482264073,122.215628983934)) ;
#79325 = CARTESIAN_POINT('Ctrl Pts',(-19.1867026363573,13.6891672331473,122.217457204583)) ;
#79326 = CARTESIAN_POINT('Ctrl Pts',(-19.1817616917867,13.6889300932055,122.218388511836)) ;
#79327 = CARTESIAN_POINT('Ctrl Pts',(-19.170187435375,13.6883734502378,122.220644606035)) ;
#79328 = CARTESIAN_POINT('Ctrl Pts',(-19.1635591325312,13.6880537931767,122.221994171274)) ;
#79329 = CARTESIAN_POINT('Ctrl Pts',(-19.1335591030364,13.6866029476454,122.228363745616)) ;
#79330 = CARTESIAN_POINT('Ctrl Pts',(-19.110327483493,13.6854677830628,122.234017497673)) ;
#79331 = CARTESIAN_POINT('Ctrl Pts',(-19.0748968568967,13.6837233529636,122.243755912942)) ;
#79332 = CARTESIAN_POINT('Ctrl Pts',(-19.0625704385601,13.6831141537349,122.247355044169)) ;
#79333 = CARTESIAN_POINT('Ctrl Pts',(-19.0412403253723,13.6820565260515,122.253951832279)) ;
#79334 = CARTESIAN_POINT('Ctrl Pts',(-19.0322104100108,13.6816076912566,122.2568608285)) ;
#79335 = CARTESIAN_POINT('Ctrl Pts',(-19.0183025659665,13.6809146446045,122.261521744582)) ;
#79336 = CARTESIAN_POINT('Ctrl Pts',(-19.0134002434702,13.6806700133047,122.263199611754)) ;
#79337 = CARTESIAN_POINT('Ctrl Pts',(-19.0024541715424,13.680122974838,122.2670244107)) ;
#79338 = CARTESIAN_POINT('Ctrl Pts',(-18.9964163838097,13.6798206715914,122.269187944209)) ;
#79339 = CARTESIAN_POINT('Ctrl Pts',(-18.9798855947754,13.6789912693134,122.275259587945)) ;
#79340 = CARTESIAN_POINT('Ctrl Pts',(-18.9694290404278,13.6784647192872,122.279265106809)) ;
#79341 = CARTESIAN_POINT('Ctrl Pts',(-18.9448557167229,13.6772214310784,122.28906988723)) ;
#79342 = CARTESIAN_POINT('Ctrl Pts',(-18.930789934561,13.676505161048,122.294991705033)) ;
#79343 = CARTESIAN_POINT('Ctrl Pts',(-18.9094825532098,13.6754097066074,122.304438726192)) ;
#79344 = CARTESIAN_POINT('Ctrl Pts',(-18.9021582627929,13.6750312228838,122.307773552056)) ;
#79345 = CARTESIAN_POINT('Ctrl Pts',(-18.8917919371076,13.6744922007744,122.312618366463)) ;
#79346 = CARTESIAN_POINT('Ctrl Pts',(-18.8887222491793,13.6743321618287,122.314068726864)) ;
#79347 = CARTESIAN_POINT('Ctrl Pts',(-18.8810902940327,13.673933144125,122.317713868788)) ;
#79348 = CARTESIAN_POINT('Ctrl Pts',(-18.8765356006337,13.6736940262475,122.319924331301)) ;
#79349 = CARTESIAN_POINT('Ctrl Pts',(-18.8536896123915,13.6724900149245,122.331188813133)) ;
#79350 = CARTESIAN_POINT('Ctrl Pts',(-18.8356147093884,13.6715227048952,122.340674254182)) ;
#79351 = CARTESIAN_POINT('Ctrl Pts',(-18.811959369325,13.6702410508436,122.353858771432)) ;
#79352 = CARTESIAN_POINT('Ctrl Pts',(-18.8061582505,13.6699254410493,122.357154999757)) ;
#79353 = CARTESIAN_POINT('Ctrl Pts',(-18.7937117196621,13.6692455629943,122.364363461565)) ;
#79354 = CARTESIAN_POINT('Ctrl Pts',(-18.7870757996362,13.6688813880778,122.368291521219)) ;
#79355 = CARTESIAN_POINT('Ctrl Pts',(-18.7756444743745,13.6682511221836,122.37520597176)) ;
#79356 = CARTESIAN_POINT('Ctrl Pts',(-18.7708316770778,13.6679848572748,122.378163121457)) ;
#79357 = CARTESIAN_POINT('Ctrl Pts',(-18.7595696537421,13.6673596131151,122.385191560434)) ;
#79358 = CARTESIAN_POINT('Ctrl Pts',(-18.7531377884541,13.6670008331259,122.38929022978)) ;
#79359 = CARTESIAN_POINT('Ctrl Pts',(-18.7263820034781,13.6655008841968,122.406696592065)) ;
#79360 = CARTESIAN_POINT('Ctrl Pts',(-18.7064210224811,13.6643642512426,122.420551724848)) ;
#79361 = CARTESIAN_POINT('Ctrl Pts',(-18.6767567000718,13.6626373161165,122.442488778044)) ;
#79362 = CARTESIAN_POINT('Ctrl Pts',(-18.6667418496699,13.6620472269139,122.45013870501)) ;
#79363 = CARTESIAN_POINT('Ctrl Pts',(-18.6516129483,13.6611432125891,122.462072269252)) ;
#79364 = CARTESIAN_POINT('Ctrl Pts',(-18.6464121468389,13.6608301163655,122.466244528018)) ;
#79365 = CARTESIAN_POINT('Ctrl Pts',(-18.6366900289319,13.6602402178117,122.47417635375)) ;
#79366 = CARTESIAN_POINT('Ctrl Pts',(-18.6321611485509,13.659963505509,122.477926345771)) ;
#79367 = CARTESIAN_POINT('Ctrl Pts',(-18.6244737906184,13.6594904298314,122.484386249689)) ;
#79368 = CARTESIAN_POINT('Ctrl Pts',(-18.621301684346,13.6592942226465,122.487079787436)) ;
#79369 = CARTESIAN_POINT('Ctrl Pts',(-18.6139230797762,13.658835460276,122.493410728789)) ;
#79370 = CARTESIAN_POINT('Ctrl Pts',(-18.6097275973186,13.6585727898024,122.497060817645)) ;
#79371 = CARTESIAN_POINT('Ctrl Pts',(-18.5973742601353,13.6577939240769,122.507958187457)) ;
#79372 = CARTESIAN_POINT('Ctrl Pts',(-18.5892888471,13.6572770052471,122.515286686829)) ;
#79373 = CARTESIAN_POINT('Ctrl Pts',(-18.5637199521017,13.6556195581763,122.539097206545)) ;
#79374 = CARTESIAN_POINT('Ctrl Pts',(-18.5466262454901,13.654476487476,122.555989302032)) ;
#79375 = CARTESIAN_POINT('Ctrl Pts',(-18.523486285956,13.6528853022747,122.580254400298)) ;
#79376 = CARTESIAN_POINT('Ctrl Pts',(-18.5170087993465,13.652434788866,122.587208406547)) ;
#79377 = CARTESIAN_POINT('Ctrl Pts',(-18.505730095759,13.6516413298043,122.599605331651)) ;
#79378 = CARTESIAN_POINT('Ctrl Pts',(-18.5008948212632,13.6512981445459,122.605016608537)) ;
#79379 = CARTESIAN_POINT('Ctrl Pts',(-18.4960368415869,13.6509502176703,122.61055232771)) ;
#79380 = CARTESIAN_POINT('Ctrl Pts',(-18.4959653887577,13.6509450995473,122.610633770936)) ;
#79381 = CARTESIAN_POINT('Ctrl Pts',(-18.4958216195361,13.650934800045,122.610797685917)) ;
#79382 = CARTESIAN_POINT('Ctrl Pts',(-18.4957493034679,13.6509296186715,122.61088015785)) ;
#79383 = CARTESIAN_POINT('Ctrl Pts',(-18.4956033009723,13.6509191562993,122.61104671002)) ;
#79384 = CARTESIAN_POINT('Ctrl Pts',(-18.4955296150436,13.6509138753085,122.611130790565)) ;
#79385 = CARTESIAN_POINT('Ctrl Pts',(-18.4953803125252,13.6509031734559,122.611301202115)) ;
#79386 = CARTESIAN_POINT('Ctrl Pts',(-18.4953046965139,13.6508977525956,122.61138753372)) ;
#79387 = CARTESIAN_POINT('Ctrl Pts',(-18.495150898894,13.6508867253586,122.611563176305)) ;
#79388 = CARTESIAN_POINT('Ctrl Pts',(-18.4950727181454,13.650881118989,122.611652488023)) ;
#79389 = CARTESIAN_POINT('Ctrl Pts',(-18.4949130543925,13.6508696677346,122.611834937817)) ;
#79390 = CARTESIAN_POINT('Ctrl Pts',(-18.4948315724147,13.6508638228506,122.611928077016)) ;
#79391 = CARTESIAN_POINT('Ctrl Pts',(-18.4946644310987,13.6508518315636,122.612119189324)) ;
#79392 = CARTESIAN_POINT('Ctrl Pts',(-18.4945787733826,13.6508456851806,122.612217163619)) ;
#79393 = CARTESIAN_POINT('Ctrl Pts',(-18.4908484797438,13.6505779734918,122.616485213669)) ;
#79394 = CARTESIAN_POINT('Ctrl Pts',(-18.4872323786622,13.6503166335513,122.620680155562)) ;
#79395 = CARTESIAN_POINT('Ctrl Pts',(-18.4792695286078,13.6497369943918,122.630046391917)) ;
#79396 = CARTESIAN_POINT('Ctrl Pts',(-18.4749369697328,13.6494188087734,122.635229512879)) ;
#79397 = CARTESIAN_POINT('Ctrl Pts',(-18.4584470181595,13.6481965312508,122.655294493191)) ;
#79398 = CARTESIAN_POINT('Ctrl Pts',(-18.4466001150082,13.647294652107,122.670427861931)) ;
#79399 = CARTESIAN_POINT('Ctrl Pts',(-18.4296220647914,13.6459607527988,122.693209213516)) ;
#79400 = CARTESIAN_POINT('Ctrl Pts',(-18.4242109104843,13.6455289737106,122.700644679848)) ;
#79401 = CARTESIAN_POINT('Ctrl Pts',(-18.4155583177141,13.6448266814834,122.712822433335)) ;
#79402 = CARTESIAN_POINT('Ctrl Pts',(-18.4122651750663,13.6445564929113,122.717527543225)) ;
#79403 = CARTESIAN_POINT('Ctrl Pts',(-18.4073550932428,13.6441490076542,122.724649841005)) ;
#79404 = CARTESIAN_POINT('Ctrl Pts',(-18.4057132684771,13.644011961902,122.727049774961)) ;
#79405 = CARTESIAN_POINT('Ctrl Pts',(-18.4021410832575,13.6437120665719,122.732311848014)) ;
#79406 = CARTESIAN_POINT('Ctrl Pts',(-18.4002142742678,13.6435491915603,122.735176367436)) ;
#79407 = CARTESIAN_POINT('Ctrl Pts',(-18.396115383237,13.6432003403124,122.741326486652)) ;
#79408 = CARTESIAN_POINT('Ctrl Pts',(-18.3939470158841,13.6430143445044,122.744614515806)) ;
#79409 = CARTESIAN_POINT('Ctrl Pts',(-18.3826132896108,13.6420345896768,122.761983734693)) ;
#79410 = CARTESIAN_POINT('Ctrl Pts',(-18.3737247711066,13.6412398806722,122.77624337438)) ;
#79411 = CARTESIAN_POINT('Ctrl Pts',(-18.3578985921804,13.6397765946518,122.802846674507)) ;
#79412 = CARTESIAN_POINT('Ctrl Pts',(-18.350875427845,13.6391079725304,122.815136146935)) ;
#79413 = CARTESIAN_POINT('Ctrl Pts',(-18.3398105772798,13.6380224992468,122.835308199664)) ;
#79414 = CARTESIAN_POINT('Ctrl Pts',(-18.3356375516177,13.6376051463502,122.843117181785)) ;
#79415 = CARTESIAN_POINT('Ctrl Pts',(-18.327643930231,13.6367896562752,122.858477238561)) ;
#79416 = CARTESIAN_POINT('Ctrl Pts',(-18.3238161303173,13.6363915084997,122.866024000894)) ;
#79417 = CARTESIAN_POINT('Ctrl Pts',(-18.3149411037336,13.6354496403047,122.88398437991)) ;
#79418 = CARTESIAN_POINT('Ctrl Pts',(-18.3099632008601,13.6349062543894,122.894431339147)) ;
#79419 = CARTESIAN_POINT('Ctrl Pts',(-18.2956934700033,13.633301241689,122.925514670719)) ;
#79420 = CARTESIAN_POINT('Ctrl Pts',(-18.2868281617792,13.6322406103379,122.946341262557)) ;
#79421 = CARTESIAN_POINT('Ctrl Pts',(-18.2753976843105,13.6307720674936,122.975422687535)) ;
#79422 = CARTESIAN_POINT('Ctrl Pts',(-18.2723310610967,13.6303667541518,122.98347538022)) ;
#79423 = CARTESIAN_POINT('Ctrl Pts',(-18.267028754269,13.6296449177385,122.997856966129)) ;
#79424 = CARTESIAN_POINT('Ctrl Pts',(-18.2647593636358,13.6293285924177,123.004173052405)) ;
#79425 = CARTESIAN_POINT('Ctrl Pts',(-18.2615783781736,13.6288742876962,123.013262227138)) ;
#79426 = CARTESIAN_POINT('Ctrl Pts',(-18.2606242585385,13.6287365493174,123.016020311112)) ;
#79427 = CARTESIAN_POINT('Ctrl Pts',(-18.2595004286607,13.6285725369429,123.019307264429)) ;
#79428 = CARTESIAN_POINT('Ctrl Pts',(-18.2593211307022,13.6285463155574,123.01983284811)) ;
#79429 = CARTESIAN_POINT('Ctrl Pts',(-18.2589566920424,13.6284929069755,123.020903544316)) ;
#79430 = CARTESIAN_POINT('Ctrl Pts',(-18.2587715783088,13.6284657196391,123.021448665889)) ;
#79431 = CARTESIAN_POINT('Ctrl Pts',(-18.2584418935593,13.6284171940844,123.022421790307)) ;
#79432 = CARTESIAN_POINT('Ctrl Pts',(-18.2582971736603,13.6283958566734,123.022849742647)) ;
#79433 = CARTESIAN_POINT('Ctrl Pts',(-18.2580414169979,13.628358083488,123.023607435025)) ;
#79434 = CARTESIAN_POINT('Ctrl Pts',(-18.2579302831241,13.6283416482388,123.023937142227)) ;
#79435 = CARTESIAN_POINT('Ctrl Pts',(-18.2545355857349,13.6278389528537,123.034022696292)) ;
#79436 = CARTESIAN_POINT('Ctrl Pts',(-18.2513760090569,13.6273520380258,123.043819803597)) ;
#79437 = CARTESIAN_POINT('Ctrl Pts',(-18.2443860235532,13.6262291937492,123.066475791756)) ;
#79438 = CARTESIAN_POINT('Ctrl Pts',(-18.2406433585346,13.6255929325413,123.079360338553)) ;
#79439 = CARTESIAN_POINT('Ctrl Pts',(-18.2304888521251,13.6237608650259,123.116610903915)) ;
#79440 = CARTESIAN_POINT('Ctrl Pts',(-18.2246204691796,13.6225650397346,123.141117983595)) ;
#79441 = CARTESIAN_POINT('Ctrl Pts',(-18.2181089382832,13.6210446163846,123.172604666996)) ;
#79442 = CARTESIAN_POINT('Ctrl Pts',(-18.2167581942384,13.6207158728074,123.17943146443)) ;
#79443 = CARTESIAN_POINT('Ctrl Pts',(-18.2152737832695,13.6203385587359,123.18728774374)) ;
#79444 = CARTESIAN_POINT('Ctrl Pts',(-18.2150826942761,13.620289663212,123.188306227561)) ;
#79445 = CARTESIAN_POINT('Ctrl Pts',(-18.2142021764829,13.6200628449607,123.193032649327)) ;
#79446 = CARTESIAN_POINT('Ctrl Pts',(-18.2135287120729,13.6198850141926,123.196743544139)) ;
#79447 = CARTESIAN_POINT('Ctrl Pts',(-18.2116164479277,13.6193670423708,123.207567033146)) ;
#79448 = CARTESIAN_POINT('Ctrl Pts',(-18.2104237530695,13.6190271646022,123.214687614956)) ;
#79449 = CARTESIAN_POINT('Ctrl Pts',(-18.2085783113974,13.6184721435695,123.226341859156)) ;
#79450 = CARTESIAN_POINT('Ctrl Pts',(-18.2078876103002,13.6182568361054,123.230869316774)) ;
#79451 = CARTESIAN_POINT('Ctrl Pts',(-18.2052015149846,13.617387620246,123.249169814321)) ;
#79452 = CARTESIAN_POINT('Ctrl Pts',(-18.2034172405489,13.6167345433705,123.262972760568)) ;
#79453 = CARTESIAN_POINT('Ctrl Pts',(-18.2006525764722,13.6155665999296,123.287693524581)) ;
#79454 = CARTESIAN_POINT('Ctrl Pts',(-18.1995820592074,13.6150519101811,123.298599677515)) ;
#79455 = CARTESIAN_POINT('Ctrl Pts',(-18.1982208540007,13.6142911221513,123.314705734439)) ;
#79456 = CARTESIAN_POINT('Ctrl Pts',(-18.1978158199284,13.6140458528795,123.319895433881)) ;
#79457 = CARTESIAN_POINT('Ctrl Pts',(-18.1970577169954,13.6135451521361,123.330485979255)) ;
#79458 = CARTESIAN_POINT('Ctrl Pts',(-18.1967073600709,13.6132897117557,123.335886912264)) ;
#79459 = CARTESIAN_POINT('Ctrl Pts',(-18.1950267723857,13.6119228512249,123.364781718951)) ;
#79460 = CARTESIAN_POINT('Ctrl Pts',(-18.1943432320815,13.61080917445,123.388308161591)) ;
#79461 = CARTESIAN_POINT('Ctrl Pts',(-18.1943434021578,13.609157782117,123.423247243905)) ;
#79462 = CARTESIAN_POINT('Ctrl Pts',(-18.194504127961,13.6086189937792,123.434654376293)) ;
#79463 = CARTESIAN_POINT('Ctrl Pts',(-18.1950044016075,13.6077812304192,123.452406709026)) ;
#79464 = CARTESIAN_POINT('Ctrl Pts',(-18.1952331124391,13.607481816352,123.458754352997)) ;
#79465 = CARTESIAN_POINT('Ctrl Pts',(-18.1958107050816,13.6068612975726,123.471915735628)) ;
#79466 = CARTESIAN_POINT('Ctrl Pts',(-18.1961672260551,13.606540240931,123.478728922459)) ;
#79467 = CARTESIAN_POINT('Ctrl Pts',(-18.1973597663866,13.605616062619,123.498350087162)) ;
#79468 = CARTESIAN_POINT('Ctrl Pts',(-18.1983413870918,13.6050137915715,123.511148327642)) ;
#79469 = CARTESIAN_POINT('Ctrl Pts',(-18.2012391874975,13.6035427352008,123.542421767675)) ;
#79470 = CARTESIAN_POINT('Ctrl Pts',(-18.2033765847497,13.6026750236002,123.56087314896)) ;
#79471 = CARTESIAN_POINT('Ctrl Pts',(-18.2076194582323,13.6012333141427,123.591366190679)) ;
#79472 = CARTESIAN_POINT('Ctrl Pts',(-18.209485124377,13.600660581677,123.60343794615)) ;
#79473 = CARTESIAN_POINT('Ctrl Pts',(-18.2123924361722,13.5998452096326,123.620537218982)) ;
#79474 = CARTESIAN_POINT('Ctrl Pts',(-18.2132844079912,13.5996037878829,123.625589457785)) ;
#79475 = CARTESIAN_POINT('Ctrl Pts',(-18.2148941212654,13.5991826940958,123.634381443263)) ;
#79476 = CARTESIAN_POINT('Ctrl Pts',(-18.2155974947312,13.5990031494525,123.638123750475)) ;
#79477 = CARTESIAN_POINT('Ctrl Pts',(-18.2170190896535,13.5986488044543,123.645496269393)) ;
#79478 = CARTESIAN_POINT('Ctrl Pts',(-18.2177363267868,13.5984740148728,123.649126629111)) ;
#79479 = CARTESIAN_POINT('Ctrl Pts',(-18.2193309282037,13.5980938559592,123.657008293661)) ;
#79480 = CARTESIAN_POINT('Ctrl Pts',(-18.2202145129041,13.5978884315067,123.661258284551)) ;
#79481 = CARTESIAN_POINT('Ctrl Pts',(-18.2224492113203,13.5973814111263,123.671725255282)) ;
#79482 = CARTESIAN_POINT('Ctrl Pts',(-18.2238264152357,13.5970795796651,123.677936518863)) ;
#79483 = CARTESIAN_POINT('Ctrl Pts',(-18.234673827614,13.5947801931096,123.725102814226)) ;
#79484 = CARTESIAN_POINT('Ctrl Pts',(-18.2462119199981,13.5927605622578,123.765542013498)) ;
#79485 = CARTESIAN_POINT('Ctrl Pts',(-18.259825879779,13.5907660201144,123.80531165987)) ;
#79486 = CARTESIAN_POINT('',(-18.9360879630843,13.6947924664109,122.292840804082)) ;
#79487 = CARTESIAN_POINT('Origin',(-19.4092696481994,13.6947924276734,123.411833733891)) ;
#79488 = CARTESIAN_POINT('Ctrl Pts',(-18.259825879779,13.6088050314641,123.80531165987)) ;
#79489 = CARTESIAN_POINT('Ctrl Pts',(-18.2564562893653,13.6092962280985,123.795468276951)) ;
#79490 = CARTESIAN_POINT('Ctrl Pts',(-18.2532163611542,13.6097873550664,123.785591544476)) ;
#79491 = CARTESIAN_POINT('Ctrl Pts',(-18.2459652224294,13.6109330714525,123.762489366047)) ;
#79492 = CARTESIAN_POINT('Ctrl Pts',(-18.2420547455701,13.6115880006948,123.749244356245)) ;
#79493 = CARTESIAN_POINT('Ctrl Pts',(-18.2336384625199,13.613086132159,123.718838447372)) ;
#79494 = CARTESIAN_POINT('Ctrl Pts',(-18.2292810266786,13.613929052619,123.701639598016)) ;
#79495 = CARTESIAN_POINT('Ctrl Pts',(-18.2239139371324,13.6150630225712,123.67832199731)) ;
#79496 = CARTESIAN_POINT('Ctrl Pts',(-18.2225721890224,13.6153559808195,123.672281997486)) ;
#79497 = CARTESIAN_POINT('Ctrl Pts',(-18.2203539340453,13.615857027945,123.661923158797)) ;
#79498 = CARTESIAN_POINT('Ctrl Pts',(-18.2194546811356,13.6160652740971,123.65760932423)) ;
#79499 = CARTESIAN_POINT('Ctrl Pts',(-18.2177570205037,13.6164686039618,123.649237694831)) ;
#79500 = CARTESIAN_POINT('Ctrl Pts',(-18.2169558232867,13.6166637067782,123.64518052803)) ;
#79501 = CARTESIAN_POINT('Ctrl Pts',(-18.2154082507614,13.617050237762,123.637127692457)) ;
#79502 = CARTESIAN_POINT('Ctrl Pts',(-18.2146611815556,13.6172416691909,123.633132211637)) ;
#79503 = CARTESIAN_POINT('Ctrl Pts',(-18.2129141051487,13.6177013032481,123.623521773489)) ;
#79504 = CARTESIAN_POINT('Ctrl Pts',(-18.2119335561518,13.6179693390961,123.617903371218)) ;
#79505 = CARTESIAN_POINT('Ctrl Pts',(-18.2060579317768,13.6196410747871,123.582778325726)) ;
#79506 = CARTESIAN_POINT('Ctrl Pts',(-18.202214341137,13.6210342463854,123.553106455399)) ;
#79507 = CARTESIAN_POINT('Ctrl Pts',(-18.1983381607293,13.623004567995,123.511044929049)) ;
#79508 = CARTESIAN_POINT('Ctrl Pts',(-18.1973936704148,13.6235802564231,123.49875060712)) ;
#79509 = CARTESIAN_POINT('Ctrl Pts',(-18.1962670461933,13.6244391662219,123.48043973661)) ;
#79510 = CARTESIAN_POINT('Ctrl Pts',(-18.1959422151088,13.6247211671628,123.474432749139)) ;
#79511 = CARTESIAN_POINT('Ctrl Pts',(-18.1955975267177,13.6250685924995,123.467040687546)) ;
#79512 = CARTESIAN_POINT('Ctrl Pts',(-18.1955354054134,13.6251336119667,123.465657653257)) ;
#79513 = CARTESIAN_POINT('Ctrl Pts',(-18.1954492384305,13.6252273999616,123.463663235883)) ;
#79514 = CARTESIAN_POINT('Ctrl Pts',(-18.1954232903798,13.6252561500617,123.463051935274)) ;
#79515 = CARTESIAN_POINT('Ctrl Pts',(-18.1953670456238,13.6253196076563,123.461702833796)) ;
#79516 = CARTESIAN_POINT('Ctrl Pts',(-18.1953369597583,13.625354317194,123.460965024485)) ;
#79517 = CARTESIAN_POINT('Ctrl Pts',(-18.1952866275414,13.6254137239474,123.459702430108)) ;
#79518 = CARTESIAN_POINT('Ctrl Pts',(-18.195266048772,13.6254384178796,123.459177658353)) ;
#79519 = CARTESIAN_POINT('Ctrl Pts',(-18.1952314934586,13.6254805861963,123.458281637977)) ;
#79520 = CARTESIAN_POINT('Ctrl Pts',(-18.1952173469225,13.6254980588921,123.457910395917)) ;
#79521 = CARTESIAN_POINT('Ctrl Pts',(-18.1951934799149,13.6255278996214,123.457276421153)) ;
#79522 = CARTESIAN_POINT('Ctrl Pts',(-18.195183674439,13.6255402668077,123.457013691635)) ;
#79523 = CARTESIAN_POINT('Ctrl Pts',(-18.1951034828839,13.6256423030949,123.454846147898)) ;
#79524 = CARTESIAN_POINT('Ctrl Pts',(-18.1950374944242,13.6257320159899,123.452941175793)) ;
#79525 = CARTESIAN_POINT('Ctrl Pts',(-18.1948724114947,13.6259729329115,123.447827735397)) ;
#79526 = CARTESIAN_POINT('Ctrl Pts',(-18.1947815494378,13.6261242199306,123.444619021083)) ;
#79527 = CARTESIAN_POINT('Ctrl Pts',(-18.1946260758413,13.6264254778985,123.438234424099)) ;
#79528 = CARTESIAN_POINT('Ctrl Pts',(-18.1945612010521,13.6265754449172,123.435058573375)) ;
#79529 = CARTESIAN_POINT('Ctrl Pts',(-18.1944213280746,13.6269759534525,123.426583664769)) ;
#79530 = CARTESIAN_POINT('Ctrl Pts',(-18.1943685459481,13.6272267195798,123.421284321665)) ;
#79531 = CARTESIAN_POINT('Ctrl Pts',(-18.1942833764605,13.6284078058714,123.396357802433)) ;
#79532 = CARTESIAN_POINT('Ctrl Pts',(-18.1946919357149,13.6293425243796,123.376732255174)) ;
#79533 = CARTESIAN_POINT('Ctrl Pts',(-18.1962526191702,13.6309963678789,123.342108738325)) ;
#79534 = CARTESIAN_POINT('Ctrl Pts',(-18.1972081455711,13.6317144393419,123.32710590241)) ;
#79535 = CARTESIAN_POINT('Ctrl Pts',(-18.1992965550747,13.6329274508423,123.301745061226)) ;
#79536 = CARTESIAN_POINT('Ctrl Pts',(-18.2002847244539,13.633423138966,123.291376854638)) ;
#79537 = CARTESIAN_POINT('Ctrl Pts',(-18.2019976366522,13.6341784956299,123.275560424387)) ;
#79538 = CARTESIAN_POINT('Ctrl Pts',(-18.2026262317556,13.6344390207153,123.27010232765)) ;
#79539 = CARTESIAN_POINT('Ctrl Pts',(-18.2037437577747,13.6348758282347,123.260945744652)) ;
#79540 = CARTESIAN_POINT('Ctrl Pts',(-18.204212738107,13.6350523041372,123.257244918266)) ;
#79541 = CARTESIAN_POINT('Ctrl Pts',(-18.2051125264461,13.6353787046762,123.250397505548)) ;
#79542 = CARTESIAN_POINT('Ctrl Pts',(-18.2055386416694,13.6355286752487,123.247250338092)) ;
#79543 = CARTESIAN_POINT('Ctrl Pts',(-18.2064284190062,13.6358327684773,123.240867042304)) ;
#79544 = CARTESIAN_POINT('Ctrl Pts',(-18.2068928124685,13.6359868824479,123.237631042295)) ;
#79545 = CARTESIAN_POINT('Ctrl Pts',(-18.2080180331836,13.6363497851968,123.230009157782)) ;
#79546 = CARTESIAN_POINT('Ctrl Pts',(-18.2086898284105,13.6365584629146,123.225624936459)) ;
#79547 = CARTESIAN_POINT('Ctrl Pts',(-18.2109085125464,13.6372231778854,123.211656862707)) ;
#79548 = CARTESIAN_POINT('Ctrl Pts',(-18.2125462712004,13.6376783420359,123.202087808503)) ;
#79549 = CARTESIAN_POINT('Ctrl Pts',(-18.2180623851035,13.6391088997323,123.172029585398)) ;
#79550 = CARTESIAN_POINT('Ctrl Pts',(-18.2223536006575,13.6400811046775,123.151620229648)) ;
#79551 = CARTESIAN_POINT('Ctrl Pts',(-18.2294474806769,13.6415183580902,123.121724966207)) ;
#79552 = CARTESIAN_POINT('Ctrl Pts',(-18.2318440194524,13.6419809828871,123.112146675963)) ;
#79553 = CARTESIAN_POINT('Ctrl Pts',(-18.2361796364587,13.6427804358337,123.095673857986)) ;
#79554 = CARTESIAN_POINT('Ctrl Pts',(-18.238063424983,13.6431168898146,123.088765279786)) ;
#79555 = CARTESIAN_POINT('Ctrl Pts',(-18.2419533084532,13.6437905745017,123.074980904348)) ;
#79556 = CARTESIAN_POINT('Ctrl Pts',(-18.243959351904,13.6441277922126,123.068105382182)) ;
#79557 = CARTESIAN_POINT('Ctrl Pts',(-18.2482774810884,13.6448330024152,123.053777824394)) ;
#79558 = CARTESIAN_POINT('Ctrl Pts',(-18.2506007962213,13.6452010358916,123.046329508825)) ;
#79559 = CARTESIAN_POINT('Ctrl Pts',(-18.2599595808061,13.6466403538199,123.017312449718)) ;
#79560 = CARTESIAN_POINT('Ctrl Pts',(-18.2675268759253,13.6477135559427,122.995920143408)) ;
#79561 = CARTESIAN_POINT('Ctrl Pts',(-18.279967349156,13.6493493626998,122.963655473976)) ;
#79562 = CARTESIAN_POINT('Ctrl Pts',(-18.284408754828,13.649911866091,122.952622009087)) ;
#79563 = CARTESIAN_POINT('Ctrl Pts',(-18.2925336316627,13.6509038972777,122.933263473938)) ;
#79564 = CARTESIAN_POINT('Ctrl Pts',(-18.2961500094947,13.6513335568294,122.924911259401)) ;
#79565 = CARTESIAN_POINT('Ctrl Pts',(-18.3037111180125,13.6522084660053,122.907973042786)) ;
#79566 = CARTESIAN_POINT('Ctrl Pts',(-18.3076628452589,13.6526536996475,122.899390846101)) ;
#79567 = CARTESIAN_POINT('Ctrl Pts',(-18.3240877969109,13.6544578782878,122.864788056701)) ;
#79568 = CARTESIAN_POINT('Ctrl Pts',(-18.3373860627355,13.6558145092602,122.839169604252)) ;
#79569 = CARTESIAN_POINT('Ctrl Pts',(-18.3563577046227,13.6576311507509,122.805602270166)) ;
#79570 = CARTESIAN_POINT('Ctrl Pts',(-18.3612326411174,13.6580885406466,122.797213053388)) ;
#79571 = CARTESIAN_POINT('Ctrl Pts',(-18.3705490569635,13.6589459487467,122.781613739776)) ;
#79572 = CARTESIAN_POINT('Ctrl Pts',(-18.3749664481735,13.659345833808,122.77438993363)) ;
#79573 = CARTESIAN_POINT('Ctrl Pts',(-18.383588437236,13.6601141598129,122.760615917939)) ;
#79574 = CARTESIAN_POINT('Ctrl Pts',(-18.387781179161,13.6604825122246,122.754058773662)) ;
#79575 = CARTESIAN_POINT('Ctrl Pts',(-18.3976194324177,13.6613351856627,122.73899340026)) ;
#79576 = CARTESIAN_POINT('Ctrl Pts',(-18.4033097695088,13.6618198828758,122.730515162381)) ;
#79577 = CARTESIAN_POINT('Ctrl Pts',(-18.4202130063289,13.6632335594721,122.706003909944)) ;
#79578 = CARTESIAN_POINT('Ctrl Pts',(-18.4317072109679,13.6641623326182,122.690168663861)) ;
#79579 = CARTESIAN_POINT('Ctrl Pts',(-18.4471883399265,13.6653693068245,122.669889685581)) ;
#79580 = CARTESIAN_POINT('Ctrl Pts',(-18.4508325225009,13.6656504282505,122.665188107336)) ;
#79581 = CARTESIAN_POINT('Ctrl Pts',(-18.4572200824706,13.6661380218222,122.657070958923)) ;
#79582 = CARTESIAN_POINT('Ctrl Pts',(-18.4599476723875,13.6663446364539,122.653643118703)) ;
#79583 = CARTESIAN_POINT('Ctrl Pts',(-18.4636318105319,13.6666215935145,122.649064205802)) ;
#79584 = CARTESIAN_POINT('Ctrl Pts',(-18.464572027648,13.666692092101,122.647900046385)) ;
#79585 = CARTESIAN_POINT('Ctrl Pts',(-18.4658206461076,13.6667854740941,122.646359860348)) ;
#79586 = CARTESIAN_POINT('Ctrl Pts',(-18.4661271252323,13.6668083759759,122.645982278287)) ;
#79587 = CARTESIAN_POINT('Ctrl Pts',(-18.4667143615206,13.6668522210344,122.645259690702)) ;
#79588 = CARTESIAN_POINT('Ctrl Pts',(-18.4669950815863,13.6668731645636,122.644914655173)) ;
#79589 = CARTESIAN_POINT('Ctrl Pts',(-18.4675599706263,13.6669152768415,122.64422112339)) ;
#79590 = CARTESIAN_POINT('Ctrl Pts',(-18.4678441437124,13.6669364455462,122.643872630588)) ;
#79591 = CARTESIAN_POINT('Ctrl Pts',(-18.4684370675434,13.666980579879,122.643146328095)) ;
#79592 = CARTESIAN_POINT('Ctrl Pts',(-18.468745852542,13.667003545173,122.642768546466)) ;
#79593 = CARTESIAN_POINT('Ctrl Pts',(-18.4694093438442,13.6670528500513,122.641957798217)) ;
#79594 = CARTESIAN_POINT('Ctrl Pts',(-18.4697641219677,13.6670791889417,122.641524890455)) ;
#79595 = CARTESIAN_POINT('Ctrl Pts',(-18.4705455851007,13.6671371499667,122.640572675589)) ;
#79596 = CARTESIAN_POINT('Ctrl Pts',(-18.470972402171,13.6671687708286,122.640053477041)) ;
#79597 = CARTESIAN_POINT('Ctrl Pts',(-18.4719322138242,13.6672397978661,122.638887894127)) ;
#79598 = CARTESIAN_POINT('Ctrl Pts',(-18.4724654466735,13.6672792017572,122.638241706278)) ;
#79599 = CARTESIAN_POINT('Ctrl Pts',(-18.4765703910961,13.667582113637,122.633277677682)) ;
#79600 = CARTESIAN_POINT('Ctrl Pts',(-18.4801712756447,13.6678453409675,122.628984034479)) ;
#79601 = CARTESIAN_POINT('Ctrl Pts',(-18.4899014074659,13.668550155612,122.617543663116)) ;
#79602 = CARTESIAN_POINT('Ctrl Pts',(-18.4960842433719,13.6689912538493,122.610443007093)) ;
#79603 = CARTESIAN_POINT('Ctrl Pts',(-18.5240798442053,13.6709605208992,122.579036278452)) ;
#79604 = CARTESIAN_POINT('Ctrl Pts',(-18.5467846894472,13.6724847048018,122.555543893391)) ;
#79605 = CARTESIAN_POINT('Ctrl Pts',(-18.5755388343141,13.6743523945134,122.528097754247)) ;
#79606 = CARTESIAN_POINT('Ctrl Pts',(-18.5807119573899,13.6746859996298,122.523245806392)) ;
#79607 = CARTESIAN_POINT('Ctrl Pts',(-18.589823996568,13.6752695688853,122.514848250222)) ;
#79608 = CARTESIAN_POINT('Ctrl Pts',(-18.5937441841526,13.6755193482774,122.511282596168)) ;
#79609 = CARTESIAN_POINT('Ctrl Pts',(-18.6015539987737,13.67601446339,122.504271901532)) ;
#79610 = CARTESIAN_POINT('Ctrl Pts',(-18.6054426484631,13.6762597855394,122.500825937737)) ;
#79611 = CARTESIAN_POINT('Ctrl Pts',(-18.6141667967013,13.676807500341,122.493194298984)) ;
#79612 = CARTESIAN_POINT('Ctrl Pts',(-18.6190134795332,13.6771099844421,122.489021649032)) ;
#79613 = CARTESIAN_POINT('Ctrl Pts',(-18.6320838473187,13.6779208912446,122.477947475206)) ;
#79614 = CARTESIAN_POINT('Ctrl Pts',(-18.640366430774,13.6784297276285,122.471116371774)) ;
#79615 = CARTESIAN_POINT('Ctrl Pts',(-18.6688459104096,13.6801616749723,122.448255203425)) ;
#79616 = CARTESIAN_POINT('Ctrl Pts',(-18.6894622650883,13.6813849840397,122.4327585348)) ;
#79617 = CARTESIAN_POINT('Ctrl Pts',(-18.7184348985361,13.6830594541009,122.412390805274)) ;
#79618 = CARTESIAN_POINT('Ctrl Pts',(-18.7263792448967,13.6835143183134,122.406945920495)) ;
#79619 = CARTESIAN_POINT('Ctrl Pts',(-18.7419195041533,13.684396193969,122.396564359429)) ;
#79620 = CARTESIAN_POINT('Ctrl Pts',(-18.7495075505735,13.6848232259129,122.391617044542)) ;
#79621 = CARTESIAN_POINT('Ctrl Pts',(-18.7853774019248,13.6868261288562,122.36879789083)) ;
#79622 = CARTESIAN_POINT('Ctrl Pts',(-18.8143341811245,13.6883969627492,122.352014367238)) ;
#79623 = CARTESIAN_POINT('Ctrl Pts',(-18.8497577460213,13.6902829323459,122.333392446661)) ;
#79624 = CARTESIAN_POINT('Ctrl Pts',(-18.855593582267,13.6905925376429,122.330384709293)) ;
#79625 = CARTESIAN_POINT('Ctrl Pts',(-18.8663637957803,13.6911621852468,122.3249438696)) ;
#79626 = CARTESIAN_POINT('Ctrl Pts',(-18.8712908755244,13.6914221133452,122.322496696073)) ;
#79627 = CARTESIAN_POINT('Ctrl Pts',(-18.8959361022421,13.6927185803656,122.31046393456)) ;
#79628 = CARTESIAN_POINT('Ctrl Pts',(-18.9158945839319,13.6937564904598,122.30137985629)) ;
#79629 = CARTESIAN_POINT('Ctrl Pts',(-18.9360879635506,13.6947924657244,122.292840805121)) ;
#79630 = CARTESIAN_POINT('Origin',(-19.4092696390626,-30.19753203383,123.411833654984)) ;
#79631 = CARTESIAN_POINT('',(-18.259825879779,13.2308616644972,123.80531165987)) ;
#79632 = CARTESIAN_POINT('',(-18.259825879779,13.2488777185652,123.80531165987)) ;
#79633 = CARTESIAN_POINT('',(-18.259825879779,-30.19753203383,123.80531165987)) ;
#79634 = CARTESIAN_POINT('Ctrl Pts',(-18.259825879779,13.5907660201144,123.80531165987)) ;
#79635 = CARTESIAN_POINT('Ctrl Pts',(-18.2670498048973,13.5897076635949,123.82641448021)) ;
#79636 = CARTESIAN_POINT('Ctrl Pts',(-18.2749563117422,13.5886447944099,123.847601447194)) ;
#79637 = CARTESIAN_POINT('Ctrl Pts',(-18.2834835869921,13.5875842682099,123.868617697009)) ;
#79638 = CARTESIAN_POINT('Ctrl Pts',(-18.2913328258975,13.5866080685136,123.887962864235)) ;
#79639 = CARTESIAN_POINT('Ctrl Pts',(-18.2997074255637,13.5856338540164,123.907163230561)) ;
#79640 = CARTESIAN_POINT('Ctrl Pts',(-18.3085224981892,13.5846669715988,123.926033643261)) ;
#79641 = CARTESIAN_POINT('Ctrl Pts',(-18.3242374298226,13.582943277225,123.959674573753)) ;
#79642 = CARTESIAN_POINT('Ctrl Pts',(-18.3415966595897,13.5811956620891,123.992803532846)) ;
#79643 = CARTESIAN_POINT('Ctrl Pts',(-18.3605241308919,13.5794267489625,124.02516778511)) ;
#79644 = CARTESIAN_POINT('Ctrl Pts',(-18.3770062101987,13.5778863759261,124.053350639755)) ;
#79645 = CARTESIAN_POINT('Ctrl Pts',(-18.3946766021965,13.5763298527071,124.080953537037)) ;
#79646 = CARTESIAN_POINT('Ctrl Pts',(-18.4134553013666,13.5747589111888,124.10782194578)) ;
#79647 = CARTESIAN_POINT('Ctrl Pts',(-18.4540898318688,13.5713596091144,124.165961498721)) ;
#79648 = CARTESIAN_POINT('Ctrl Pts',(-18.4997513226257,13.568019599761,124.220445584582)) ;
#79649 = CARTESIAN_POINT('Ctrl Pts',(-18.5498882588795,13.5647273358169,124.270617410932)) ;
#79650 = CARTESIAN_POINT('Ctrl Pts',(-18.5948655602435,13.5617738815645,124.315626011823)) ;
#79651 = CARTESIAN_POINT('Ctrl Pts',(-18.6433284015354,13.5587726665132,124.357044740922)) ;
#79652 = CARTESIAN_POINT('Ctrl Pts',(-18.6947613526575,13.5557426318646,124.394444363629)) ;
#79653 = CARTESIAN_POINT('Ctrl Pts',(-18.7001312190031,13.555426280562,124.398349077843)) ;
#79654 = CARTESIAN_POINT('Ctrl Pts',(-18.705533431782,13.5551096151131,124.40221001865)) ;
#79655 = CARTESIAN_POINT('Ctrl Pts',(-18.7109673834869,13.5547926570741,124.406026722725)) ;
#79656 = CARTESIAN_POINT('Ctrl Pts',(-18.7581903583382,13.5520381788752,124.439195239911)) ;
#79657 = CARTESIAN_POINT('Ctrl Pts',(-18.8077515425201,13.5493260681322,124.468976363899)) ;
#79658 = CARTESIAN_POINT('Ctrl Pts',(-18.8591950807205,13.5466198502772,124.495099031681)) ;
#79659 = CARTESIAN_POINT('Ctrl Pts',(-18.8709542339264,13.5460012530446,124.501070247179)) ;
#79660 = CARTESIAN_POINT('Ctrl Pts',(-18.8828116330102,13.5453829637183,124.50685049238)) ;
#79661 = CARTESIAN_POINT('Ctrl Pts',(-18.8947616420897,13.5447645466604,124.51243686102)) ;
#79662 = CARTESIAN_POINT('Ctrl Pts',(-18.9476600207136,13.5420270374701,124.537165699424)) ;
#79663 = CARTESIAN_POINT('Ctrl Pts',(-19.0023100478866,13.5392673299222,124.55806150127)) ;
#79664 = CARTESIAN_POINT('Ctrl Pts',(-19.0582017493017,13.5365087036994,124.574931773315)) ;
#79665 = CARTESIAN_POINT('Ctrl Pts',(-19.0700891535024,13.5359219814469,124.578519850573)) ;
#79666 = CARTESIAN_POINT('Ctrl Pts',(-19.0820326607393,13.5353353081087,124.581926006936)) ;
#79667 = CARTESIAN_POINT('Ctrl Pts',(-19.0940272594464,13.534748907658,124.585148675846)) ;
#79668 = CARTESIAN_POINT('Ctrl Pts',(-19.1560279959301,13.5317177716688,124.601806827629)) ;
#79669 = CARTESIAN_POINT('Ctrl Pts',(-19.2192945917692,13.5286932114462,124.613531456762)) ;
#79670 = CARTESIAN_POINT('Ctrl Pts',(-19.2831523162566,13.5256682002,124.620196314525)) ;
#79671 = CARTESIAN_POINT('Ctrl Pts',(-19.2894573643986,13.5253695230754,124.620854375072)) ;
#79672 = CARTESIAN_POINT('Ctrl Pts',(-19.2957681666485,13.5250708415538,124.621463150064)) ;
#79673 = CARTESIAN_POINT('Ctrl Pts',(-19.30208406715,13.5247721488717,124.622022544893)) ;
#79674 = CARTESIAN_POINT('Ctrl Pts',(-19.3724201145366,13.5214458040943,124.628252158739)) ;
#79675 = CARTESIAN_POINT('Ctrl Pts',(-19.4431858765432,13.5181307274801,124.628339299033)) ;
#79676 = CARTESIAN_POINT('Ctrl Pts',(-19.5135678275382,13.5147860917316,124.622274807608)) ;
#79677 = CARTESIAN_POINT('Ctrl Pts',(-19.5467219612299,13.5132105670525,124.619418067256)) ;
#79678 = CARTESIAN_POINT('Ctrl Pts',(-19.5797175096476,13.5116375405296,124.615198391511)) ;
#79679 = CARTESIAN_POINT('Ctrl Pts',(-19.6123170938337,13.5100766230102,124.609672386699)) ;
#79680 = CARTESIAN_POINT('Ctrl Pts',(-19.645053057037,13.5085091754567,124.604123264074)) ;
#79681 = CARTESIAN_POINT('Ctrl Pts',(-19.6773891298795,13.5069539384338,124.597257065943)) ;
#79682 = CARTESIAN_POINT('Ctrl Pts',(-19.7091004801917,13.5054206439141,124.589181251403)) ;
#79683 = CARTESIAN_POINT('Ctrl Pts',(-19.7129404738416,13.5052349740778,124.588203334151)) ;
#79684 = CARTESIAN_POINT('Ctrl Pts',(-19.7167713319802,13.505049625991,124.587207737506)) ;
#79685 = CARTESIAN_POINT('Ctrl Pts',(-19.7205926771953,13.5048646169337,124.586194699133)) ;
#79686 = CARTESIAN_POINT('Ctrl Pts',(-19.7377483977952,13.5040340288771,124.581646718692)) ;
#79687 = CARTESIAN_POINT('Ctrl Pts',(-19.755025123028,13.5031929130004,124.576659824249)) ;
#79688 = CARTESIAN_POINT('Ctrl Pts',(-19.7721228851667,13.5023530749188,124.571309147557)) ;
#79689 = CARTESIAN_POINT('Ctrl Pts',(-19.7823793181949,13.5018492813248,124.568099437614)) ;
#79690 = CARTESIAN_POINT('Ctrl Pts',(-19.7925715867773,13.5013459475377,124.564759803787)) ;
#79691 = CARTESIAN_POINT('Ctrl Pts',(-19.802637638995,13.500845621912,124.561315065323)) ;
#79692 = CARTESIAN_POINT('Ctrl Pts',(-19.8235243601466,13.499807462999,124.554167348404)) ;
#79693 = CARTESIAN_POINT('Ctrl Pts',(-19.8444590456297,13.4987524949004,124.546362707362)) ;
#79694 = CARTESIAN_POINT('Ctrl Pts',(-19.8651875154715,13.4976925462973,124.537970763003)) ;
#79695 = CARTESIAN_POINT('Ctrl Pts',(-19.8823207002362,13.4968164423014,124.531034373856)) ;
#79696 = CARTESIAN_POINT('Ctrl Pts',(-19.89931310562,13.495936935673,124.523697697217)) ;
#79697 = CARTESIAN_POINT('Ctrl Pts',(-19.9160308813858,13.4950607059879,124.516025186995)) ;
#79698 = CARTESIAN_POINT('Ctrl Pts',(-19.9489281682582,13.4933364587125,124.50092719948)) ;
#79699 = CARTESIAN_POINT('Ctrl Pts',(-19.9813803950063,13.4916076553557,124.484248940504)) ;
#79700 = CARTESIAN_POINT('Ctrl Pts',(-20.0131369162587,13.489881514982,124.466058587158)) ;
#79701 = CARTESIAN_POINT('Ctrl Pts',(-20.0426880424715,13.4882752498737,124.449131499229)) ;
#79702 = CARTESIAN_POINT('Ctrl Pts',(-20.0716364343538,13.4866712907194,124.430895680783)) ;
#79703 = CARTESIAN_POINT('Ctrl Pts',(-20.0997951305476,13.4850754545887,124.411443799838)) ;
#79704 = CARTESIAN_POINT('Ctrl Pts',(-20.1579255419641,13.4817810332065,124.371287613829)) ;
#79705 = CARTESIAN_POINT('Ctrl Pts',(-20.2124359544786,13.4784584750556,124.326139804631)) ;
#79706 = CARTESIAN_POINT('Ctrl Pts',(-20.2626925415402,13.475090394799,124.276538949065)) ;
#79707 = CARTESIAN_POINT('Ctrl Pts',(-20.3070989856034,13.4721143775988,124.232711905747)) ;
#79708 = CARTESIAN_POINT('Ctrl Pts',(-20.3480830615047,13.4691715788273,124.185503789056)) ;
#79709 = CARTESIAN_POINT('Ctrl Pts',(-20.385229376745,13.4662550237275,124.135400159535)) ;
#79710 = CARTESIAN_POINT('Ctrl Pts',(-20.3902765523376,13.4658587430838,124.128592436767)) ;
#79711 = CARTESIAN_POINT('Ctrl Pts',(-20.3952529375974,13.4654629469358,124.121731309245)) ;
#79712 = CARTESIAN_POINT('Ctrl Pts',(-20.4001575465819,13.465067617788,124.114818043728)) ;
#79713 = CARTESIAN_POINT('Ctrl Pts',(-20.4342018669983,13.462323522954,124.066831052892)) ;
#79714 = CARTESIAN_POINT('Ctrl Pts',(-20.4647325078032,13.459550472373,124.016402693801)) ;
#79715 = CARTESIAN_POINT('Ctrl Pts',(-20.4914654231896,13.4567592247756,123.96400951547)) ;
#79716 = CARTESIAN_POINT('Ctrl Pts',(-20.4967440010575,13.4562080758426,123.953664161528)) ;
#79717 = CARTESIAN_POINT('Ctrl Pts',(-20.501874650527,13.4556562174276,123.943242282805)) ;
#79718 = CARTESIAN_POINT('Ctrl Pts',(-20.5068553925641,13.4551037323577,123.932747668806)) ;
#79719 = CARTESIAN_POINT('Ctrl Pts',(-20.5318356253654,13.4523328187946,123.880113362731)) ;
#79720 = CARTESIAN_POINT('Ctrl Pts',(-20.5530104114493,13.4495960832782,123.8257128765)) ;
#79721 = CARTESIAN_POINT('Ctrl Pts',(-20.5701853289561,13.446858214099,123.77005238292)) ;
#79722 = CARTESIAN_POINT('Ctrl Pts',(-20.5739111713719,13.4462642741797,123.75797766828)) ;
#79723 = CARTESIAN_POINT('Ctrl Pts',(-20.5774489589816,13.4456702809093,123.745843724806)) ;
#79724 = CARTESIAN_POINT('Ctrl Pts',(-20.5807970102927,13.4450758737854,123.733655833437)) ;
#79725 = CARTESIAN_POINT('Ctrl Pts',(-20.5973713129412,13.4421333013296,123.673320497615)) ;
#79726 = CARTESIAN_POINT('Ctrl Pts',(-20.6092661588775,13.4391667165855,123.611755506316)) ;
#79727 = CARTESIAN_POINT('Ctrl Pts',(-20.6163604562517,13.4362229685556,123.549593065344)) ;
#79728 = CARTESIAN_POINT('Ctrl Pts',(-20.6172697869142,13.4358456457278,123.541625227143)) ;
#79729 = CARTESIAN_POINT('Ctrl Pts',(-20.6181003156493,13.4354686980963,123.533647586815)) ;
#79730 = CARTESIAN_POINT('Ctrl Pts',(-20.6188518480512,13.4350922243203,123.525661488941)) ;
#79731 = CARTESIAN_POINT('Ctrl Pts',(-20.6254307212966,13.4317965936244,123.455751628091)) ;
#79732 = CARTESIAN_POINT('Ctrl Pts',(-20.6259390008459,13.4285013031375,123.385373714551)) ;
#79733 = CARTESIAN_POINT('Ctrl Pts',(-20.6203564137095,13.4251593702564,123.315320856039)) ;
#79734 = CARTESIAN_POINT('Ctrl Pts',(-20.6175374876002,13.4234718620055,123.279947681009)) ;
#79735 = CARTESIAN_POINT('Ctrl Pts',(-20.613167621542,13.4217961608826,123.24474822006)) ;
#79736 = CARTESIAN_POINT('Ctrl Pts',(-20.607312809919,13.4201356010657,123.209995955708)) ;
#79737 = CARTESIAN_POINT('Ctrl Pts',(-20.601457998296,13.4184750412487,123.175243691355)) ;
#79738 = CARTESIAN_POINT('Ctrl Pts',(-20.594118544722,13.4168296227376,123.140939361691)) ;
#79739 = CARTESIAN_POINT('Ctrl Pts',(-20.5854193236931,13.4152026797105,123.107337652665)) ;
#79740 = CARTESIAN_POINT('Ctrl Pts',(-20.5807421216615,13.4143279414774,123.089271439471)) ;
#79741 = CARTESIAN_POINT('Ctrl Pts',(-20.5755898553748,13.4134404278288,123.071103158856)) ;
#79742 = CARTESIAN_POINT('Ctrl Pts',(-20.5700329379717,13.4125540267447,123.053121430505)) ;
#79743 = CARTESIAN_POINT('Ctrl Pts',(-20.5664270513197,13.4119788406107,123.041453077436)) ;
#79744 = CARTESIAN_POINT('Ctrl Pts',(-20.5626518230741,13.4114041229464,123.029863049017)) ;
#79745 = CARTESIAN_POINT('Ctrl Pts',(-20.558737719952,13.4108336684169,123.018426706518)) ;
#79746 = CARTESIAN_POINT('Ctrl Pts',(-20.5518064668773,13.4098234843242,122.998174765872)) ;
#79747 = CARTESIAN_POINT('Ctrl Pts',(-20.5442541788444,13.4087998151319,122.977868574445)) ;
#79748 = CARTESIAN_POINT('Ctrl Pts',(-20.5361542599015,13.4077755235017,122.957766537256)) ;
#79749 = CARTESIAN_POINT('Ctrl Pts',(-20.5297700128418,13.406968190629,122.941922382182)) ;
#79750 = CARTESIAN_POINT('Ctrl Pts',(-20.5230465750099,13.4061604710741,122.926204877764)) ;
#79751 = CARTESIAN_POINT('Ctrl Pts',(-20.5160412115277,13.4053586630578,122.910732285531)) ;
#79752 = CARTESIAN_POINT('Ctrl Pts',(-20.5014374448478,13.4036871698909,122.87847726729)) ;
#79753 = CARTESIAN_POINT('Ctrl Pts',(-20.4853106051582,13.4020080189064,122.846621324877)) ;
#79754 = CARTESIAN_POINT('Ctrl Pts',(-20.4677249928207,13.400320627094,122.815412528442)) ;
#79755 = CARTESIAN_POINT('Ctrl Pts',(-20.4508165739698,13.3986982140109,122.785405532278)) ;
#79756 = CARTESIAN_POINT('Ctrl Pts',(-20.4325600323781,13.3970681825614,122.755997236008)) ;
#79757 = CARTESIAN_POINT('Ctrl Pts',(-20.4130548688169,13.3954300145273,122.727391467059)) ;
#79758 = CARTESIAN_POINT('Ctrl Pts',(-20.373208780757,13.3920834859253,122.668954223763)) ;
#79759 = CARTESIAN_POINT('Ctrl Pts',(-20.3283321095217,13.388742198361,122.614105775861)) ;
#79760 = CARTESIAN_POINT('Ctrl Pts',(-20.2789586274543,13.3854302875451,122.563489998466)) ;
#79761 = CARTESIAN_POINT('Ctrl Pts',(-20.2347494510225,13.3824647918284,122.518168466757)) ;
#79762 = CARTESIAN_POINT('Ctrl Pts',(-20.1870441586748,13.3794885282217,122.47635664903)) ;
#79763 = CARTESIAN_POINT('Ctrl Pts',(-20.1363457553147,13.3764859557234,122.438485712437)) ;
#79764 = CARTESIAN_POINT('Ctrl Pts',(-20.1306349606425,13.3761477384643,122.434219835632)) ;
#79765 = CARTESIAN_POINT('Ctrl Pts',(-20.1248862229821,13.3758091873893,122.430003920129)) ;
#79766 = CARTESIAN_POINT('Ctrl Pts',(-20.1191002882995,13.3754702802864,122.425838550793)) ;
#79767 = CARTESIAN_POINT('Ctrl Pts',(-20.0721275737193,13.3727188861751,122.392022285028)) ;
#79768 = CARTESIAN_POINT('Ctrl Pts',(-20.0227645008983,13.3699925972803,122.361586840403)) ;
#79769 = CARTESIAN_POINT('Ctrl Pts',(-19.9714671039411,13.3672751518641,122.334810021739)) ;
#79770 = CARTESIAN_POINT('Ctrl Pts',(-19.9599262553494,13.3666637831014,122.328785793838)) ;
#79771 = CARTESIAN_POINT('Ctrl Pts',(-19.9482876062243,13.3660528619572,122.322946570311)) ;
#79772 = CARTESIAN_POINT('Ctrl Pts',(-19.9365565347091,13.3654422032513,122.317295201679)) ;
#79773 = CARTESIAN_POINT('Ctrl Pts',(-19.8838657555059,13.3626993947195,122.29191175598)) ;
#79774 = CARTESIAN_POINT('Ctrl Pts',(-19.8293730012894,13.3599341452415,122.270352805618)) ;
#79775 = CARTESIAN_POINT('Ctrl Pts',(-19.7735878256428,13.3571721468246,122.252817626186)) ;
#79776 = CARTESIAN_POINT('Ctrl Pts',(-19.7621124657137,13.356603986456,122.24921052998)) ;
#79777 = CARTESIAN_POINT('Ctrl Pts',(-19.7505824797019,13.3560359636562,122.245773535587)) ;
#79778 = CARTESIAN_POINT('Ctrl Pts',(-19.7390024009182,13.3554683020607,122.242508122105)) ;
#79779 = CARTESIAN_POINT('Ctrl Pts',(-19.6765654013214,13.3524076072702,122.224901797997)) ;
#79780 = CARTESIAN_POINT('Ctrl Pts',(-19.6127730746103,13.349358790227,122.212316229204)) ;
#79781 = CARTESIAN_POINT('Ctrl Pts',(-19.5483163855901,13.3462943624021,122.204890450701)) ;
#79782 = CARTESIAN_POINT('Ctrl Pts',(-19.5427998573992,13.3460320932297,122.204254915165)) ;
#79783 = CARTESIAN_POINT('Ctrl Pts',(-19.5372784701475,13.3457697097115,122.203657143319)) ;
#79784 = CARTESIAN_POINT('Ctrl Pts',(-19.5317526615641,13.345507194615,122.203097205098)) ;
#79785 = CARTESIAN_POINT('Ctrl Pts',(-19.4612306537588,13.3421568991061,122.195951107477)) ;
#79786 = CARTESIAN_POINT('Ctrl Pts',(-19.390200308206,13.338828645327,122.194989532534)) ;
#79787 = CARTESIAN_POINT('Ctrl Pts',(-19.3194902776855,13.3354839544011,122.200229114569)) ;
#79788 = CARTESIAN_POINT('Ctrl Pts',(-19.2841463339745,13.333812132639,122.202848085189)) ;
#79789 = CARTESIAN_POINT('Ctrl Pts',(-19.248961668752,13.3321383322381,122.207015164986)) ;
#79790 = CARTESIAN_POINT('Ctrl Pts',(-19.2142000902938,13.3304754178574,122.212669876667)) ;
#79791 = CARTESIAN_POINT('Ctrl Pts',(-19.1794385118355,13.3288125034767,122.218324588348)) ;
#79792 = CARTESIAN_POINT('Ctrl Pts',(-19.1451007148001,13.3271604751162,122.225466660224)) ;
#79793 = CARTESIAN_POINT('Ctrl Pts',(-19.111433296722,13.3255321974351,122.233979924988)) ;
#79794 = CARTESIAN_POINT('Ctrl Pts',(-19.0924695578372,13.3246150426742,122.238775164399)) ;
#79795 = CARTESIAN_POINT('Ctrl Pts',(-19.073423771037,13.3236891386708,122.244082894318)) ;
#79796 = CARTESIAN_POINT('Ctrl Pts',(-19.0545747338385,13.3227643623052,122.249836486187)) ;
#79797 = CARTESIAN_POINT('Ctrl Pts',(-19.0415327578809,13.3221244934886,122.253817496253)) ;
#79798 = CARTESIAN_POINT('Ctrl Pts',(-19.028584767259,13.3214851645282,122.258010882909)) ;
#79799 = CARTESIAN_POINT('Ctrl Pts',(-19.0158187797981,13.3208496471916,122.26238060356)) ;
#79800 = CARTESIAN_POINT('Ctrl Pts',(-18.9963862256864,13.3198822543386,122.269032249839)) ;
#79801 = CARTESIAN_POINT('Ctrl Pts',(-18.9768916946246,13.3188995497272,122.276260202074)) ;
#79802 = CARTESIAN_POINT('Ctrl Pts',(-18.9575999785989,13.3179143486395,122.28398596407)) ;
#79803 = CARTESIAN_POINT('Ctrl Pts',(-18.9432404840646,13.3171810292388,122.289736517157)) ;
#79804 = CARTESIAN_POINT('Ctrl Pts',(-18.9289931167333,13.3164463267048,122.29576181833)) ;
#79805 = CARTESIAN_POINT('Ctrl Pts',(-18.9149602389802,13.3157155258924,122.302011996755)) ;
#79806 = CARTESIAN_POINT('Ctrl Pts',(-18.8831716085858,13.3140600452897,122.316170504749)) ;
#79807 = CARTESIAN_POINT('Ctrl Pts',(-18.8517338620342,13.3123990969106,122.331814182501)) ;
#79808 = CARTESIAN_POINT('Ctrl Pts',(-18.820896479701,13.3107371594226,122.348883552003)) ;
#79809 = CARTESIAN_POINT('Ctrl Pts',(-18.7900590973678,13.3090752219345,122.365952921505)) ;
#79810 = CARTESIAN_POINT('Ctrl Pts',(-18.7598227168092,13.3074122953375,122.384447785143)) ;
#79811 = CARTESIAN_POINT('Ctrl Pts',(-18.7304179291922,13.3057528582991,122.404259215009)) ;
#79812 = CARTESIAN_POINT('Ctrl Pts',(-18.6719105203943,13.3024510367574,122.443678490575)) ;
#79813 = CARTESIAN_POINT('Ctrl Pts',(-18.6169579423831,13.2991176447074,122.488113239888)) ;
#79814 = CARTESIAN_POINT('Ctrl Pts',(-18.5661897539316,13.2957819799608,122.537040991908)) ;
#79815 = CARTESIAN_POINT('Ctrl Pts',(-18.5208952077543,13.2928059545105,122.580693530847)) ;
#79816 = CARTESIAN_POINT('Ctrl Pts',(-18.4790410742417,13.2898555176067,122.627821648461)) ;
#79817 = CARTESIAN_POINT('Ctrl Pts',(-18.4410561529531,13.2868881760101,122.677934110496)) ;
#79818 = CARTESIAN_POINT('Ctrl Pts',(-18.4363890213519,13.28652358466,122.684091328867)) ;
#79819 = CARTESIAN_POINT('Ctrl Pts',(-18.4317802523929,13.2861587381074,122.690293558696)) ;
#79820 = CARTESIAN_POINT('Ctrl Pts',(-18.4272306008306,13.2857935575323,122.696539852779)) ;
#79821 = CARTESIAN_POINT('Ctrl Pts',(-18.3928946404529,13.2830375605983,122.743680277318)) ;
#79822 = CARTESIAN_POINT('Ctrl Pts',(-18.3619793344174,13.2802762462414,122.793264184408)) ;
#79823 = CARTESIAN_POINT('Ctrl Pts',(-18.3347692281603,13.2775362339647,122.844828572947)) ;
#79824 = CARTESIAN_POINT('Ctrl Pts',(-18.3289888657802,13.2769541611226,122.855782622478)) ;
#79825 = CARTESIAN_POINT('Ctrl Pts',(-18.3233755523965,13.2763730496085,122.866825952029)) ;
#79826 = CARTESIAN_POINT('Ctrl Pts',(-18.3179317557798,13.275793154619,122.877953967605)) ;
#79827 = CARTESIAN_POINT('Ctrl Pts',(-18.2920118289675,13.2730320603415,122.930938560821)) ;
#79828 = CARTESIAN_POINT('Ctrl Pts',(-18.2699705362575,13.2702660520453,122.985779701527)) ;
#79829 = CARTESIAN_POINT('Ctrl Pts',(-18.2520148528673,13.2674654035193,123.041959006065)) ;
#79830 = CARTESIAN_POINT('Ctrl Pts',(-18.2485203934141,13.2669203531024,123.052892385628)) ;
#79831 = CARTESIAN_POINT('Ctrl Pts',(-18.2451805305577,13.2663739906762,123.063876390402)) ;
#79832 = CARTESIAN_POINT('Ctrl Pts',(-18.2419965766553,13.265826097125,123.074907114232)) ;
#79833 = CARTESIAN_POINT('Ctrl Pts',(-18.2247812063434,13.2628636828863,123.134549307986)) ;
#79834 = CARTESIAN_POINT('Ctrl Pts',(-18.212156748074,13.259927864432,123.195458074127)) ;
#79835 = CARTESIAN_POINT('Ctrl Pts',(-18.2042480633993,13.257032547975,123.257014734077)) ;
#79836 = CARTESIAN_POINT('Ctrl Pts',(-18.2031228234541,13.2566206051722,123.265772955642)) ;
#79837 = CARTESIAN_POINT('Ctrl Pts',(-18.2020929619901,13.2562094822643,123.274544276068)) ;
#79838 = CARTESIAN_POINT('Ctrl Pts',(-18.2011587547338,13.255799219304,123.28332689543)) ;
#79839 = CARTESIAN_POINT('Ctrl Pts',(-18.193725128791,13.2525346959724,123.35321150261)) ;
#79840 = CARTESIAN_POINT('Ctrl Pts',(-18.1923663812627,13.2492233617159,123.423646288282)) ;
#79841 = CARTESIAN_POINT('Ctrl Pts',(-18.197112972822,13.2458562753417,123.493822145477)) ;
#79842 = CARTESIAN_POINT('Ctrl Pts',(-18.1995075328647,13.244157647939,123.52922445501)) ;
#79843 = CARTESIAN_POINT('Ctrl Pts',(-18.2034542366403,13.24247686509,123.564473609004)) ;
#79844 = CARTESIAN_POINT('Ctrl Pts',(-18.2088967701383,13.240815458859,123.59931931213)) ;
#79845 = CARTESIAN_POINT('Ctrl Pts',(-18.2143393036362,13.239154052628,123.634165015255)) ;
#79846 = CARTESIAN_POINT('Ctrl Pts',(-18.2212774273562,13.237512023015,123.668606637015)) ;
#79847 = CARTESIAN_POINT('Ctrl Pts',(-18.2296037713618,13.235890902084,123.702409525742)) ;
#79848 = CARTESIAN_POINT('Ctrl Pts',(-18.2344872337623,13.2349401026566,123.722235170229)) ;
#79849 = CARTESIAN_POINT('Ctrl Pts',(-18.2399200625566,13.2339772581505,123.742120798444)) ;
#79850 = CARTESIAN_POINT('Ctrl Pts',(-18.2458383478562,13.2330133138735,123.761795833979)) ;
#79851 = CARTESIAN_POINT('Ctrl Pts',(-18.2502473234648,13.2322951993201,123.77645324696)) ;
#79852 = CARTESIAN_POINT('Ctrl Pts',(-18.2549246370229,13.2315764744071,123.790993952581)) ;
#79853 = CARTESIAN_POINT('Ctrl Pts',(-18.259825879779,13.2308616644972,123.80531165987)) ;
#79854 = CARTESIAN_POINT('Ctrl Pts',(-18.259825879779,13.2488777185653,123.80531165987)) ;
#79855 = CARTESIAN_POINT('Ctrl Pts',(-18.2541317465942,13.2497016709429,123.788677729199)) ;
#79856 = CARTESIAN_POINT('Ctrl Pts',(-18.2487422399998,13.250529359594,123.771741871465)) ;
#79857 = CARTESIAN_POINT('Ctrl Pts',(-18.2437569527338,13.2513511967269,123.754800233664)) ;
#79858 = CARTESIAN_POINT('Ctrl Pts',(-18.2412772804615,13.251759976932,123.746373495694)) ;
#79859 = CARTESIAN_POINT('Ctrl Pts',(-18.2388968414335,13.2521673094432,123.737945589492)) ;
#79860 = CARTESIAN_POINT('Ctrl Pts',(-18.2366232729461,13.2525720143994,123.729554280879)) ;
#79861 = CARTESIAN_POINT('Ctrl Pts',(-18.2282379267472,13.2540646420395,123.698605563838)) ;
#79862 = CARTESIAN_POINT('Ctrl Pts',(-18.2209951205408,13.255586209498,123.667003461305)) ;
#79863 = CARTESIAN_POINT('Ctrl Pts',(-18.215009722541,13.2571241718318,123.634968474936)) ;
#79864 = CARTESIAN_POINT('Ctrl Pts',(-18.2090513348184,13.2586551938101,123.603078052698)) ;
#79865 = CARTESIAN_POINT('Ctrl Pts',(-18.2043392572502,13.2602024630274,123.570759231022)) ;
#79866 = CARTESIAN_POINT('Ctrl Pts',(-18.2009378272616,13.2617536036098,123.538246188677)) ;
#79867 = CARTESIAN_POINT('Ctrl Pts',(-18.2004500251613,13.2619760540604,123.533583464354)) ;
#79868 = CARTESIAN_POINT('Ctrl Pts',(-18.1999890932779,13.2621985841322,123.528916764725)) ;
#79869 = CARTESIAN_POINT('Ctrl Pts',(-18.1995551349332,13.2624211573227,123.524246797382)) ;
#79870 = CARTESIAN_POINT('Ctrl Pts',(-18.1930200675268,13.2657729324878,123.453920804724)) ;
#79871 = CARTESIAN_POINT('Ctrl Pts',(-18.1926313247632,13.2690704371052,123.383157341937)) ;
#79872 = CARTESIAN_POINT('Ctrl Pts',(-18.1983875184517,13.2724062706453,123.312786261935)) ;
#79873 = CARTESIAN_POINT('Ctrl Pts',(-18.2036324476591,13.2754458158226,123.248665533407)) ;
#79874 = CARTESIAN_POINT('Ctrl Pts',(-18.213969116443,13.2784896509119,123.185031555617)) ;
#79875 = CARTESIAN_POINT('Ctrl Pts',(-18.2292826636117,13.2815090524663,123.122564517586)) ;
#79876 = CARTESIAN_POINT('Ctrl Pts',(-18.230849736092,13.2818180351619,123.116172113844)) ;
#79877 = CARTESIAN_POINT('Ctrl Pts',(-18.232468881758,13.2821267619913,123.109791922641)) ;
#79878 = CARTESIAN_POINT('Ctrl Pts',(-18.2341399470166,13.282435202174,123.10342466848)) ;
#79879 = CARTESIAN_POINT('Ctrl Pts',(-18.2492276240946,13.2852200400791,123.045936144818)) ;
#79880 = CARTESIAN_POINT('Ctrl Pts',(-18.268526186191,13.2880215829812,122.98960118557)) ;
#79881 = CARTESIAN_POINT('Ctrl Pts',(-18.2918470092261,13.2908335603714,122.93495572258)) ;
#79882 = CARTESIAN_POINT('Ctrl Pts',(-18.296154129185,13.2913529041323,122.924863258693)) ;
#79883 = CARTESIAN_POINT('Ctrl Pts',(-18.3005983157538,13.2918726038172,122.914828374478)) ;
#79884 = CARTESIAN_POINT('Ctrl Pts',(-18.3051781978976,13.292392619923,122.904854379638)) ;
#79885 = CARTESIAN_POINT('Ctrl Pts',(-18.3294212425568,13.2951452614277,122.852058260708)) ;
#79886 = CARTESIAN_POINT('Ctrl Pts',(-18.3574408850354,13.2978714559953,122.801033976254)) ;
#79887 = CARTESIAN_POINT('Ctrl Pts',(-18.3889760997798,13.3006089004558,122.75225273517)) ;
#79888 = CARTESIAN_POINT('Ctrl Pts',(-18.395950847592,13.3012143501068,122.741463626636)) ;
#79889 = CARTESIAN_POINT('Ctrl Pts',(-18.403097392957,13.301820350076,122.730784143262)) ;
#79890 = CARTESIAN_POINT('Ctrl Pts',(-18.4104126119089,13.3024273082157,122.720219213702)) ;
#79891 = CARTESIAN_POINT('Ctrl Pts',(-18.4448681629127,13.3052861532175,122.670457139358)) ;
#79892 = CARTESIAN_POINT('Ctrl Pts',(-18.4830184064348,13.3081529411829,122.623312068044)) ;
#79893 = CARTESIAN_POINT('Ctrl Pts',(-18.5244875760069,13.3109950558311,122.579243361395)) ;
#79894 = CARTESIAN_POINT('Ctrl Pts',(-18.5316297482361,13.3114845489298,122.571653474834)) ;
#79895 = CARTESIAN_POINT('Ctrl Pts',(-18.5388702725273,13.3119733101524,122.564154761581)) ;
#79896 = CARTESIAN_POINT('Ctrl Pts',(-18.5462071080853,13.3124611728706,122.556749469826)) ;
#79897 = CARTESIAN_POINT('Ctrl Pts',(-18.5956168411068,13.315746671975,122.506878720283)) ;
#79898 = CARTESIAN_POINT('Ctrl Pts',(-18.649288677809,13.3190556659508,122.461354165491)) ;
#79899 = CARTESIAN_POINT('Ctrl Pts',(-18.7066052679516,13.3223924544114,122.420718788959)) ;
#79900 = CARTESIAN_POINT('Ctrl Pts',(-18.7382703284698,13.3242358929042,122.398269413415)) ;
#79901 = CARTESIAN_POINT('Ctrl Pts',(-18.7709693636302,13.3260622110372,122.377372531742)) ;
#79902 = CARTESIAN_POINT('Ctrl Pts',(-18.8044599660106,13.3278792028658,122.35814909333)) ;
#79903 = CARTESIAN_POINT('Ctrl Pts',(-18.8321965201051,13.3293840158152,122.342228449882)) ;
#79904 = CARTESIAN_POINT('Ctrl Pts',(-18.8604753323463,13.3308824318777,122.327454862663)) ;
#79905 = CARTESIAN_POINT('Ctrl Pts',(-18.889148703445,13.3323788784877,122.313871857645)) ;
#79906 = CARTESIAN_POINT('Ctrl Pts',(-18.9106960849462,13.3335034238329,122.303664540547)) ;
#79907 = CARTESIAN_POINT('Ctrl Pts',(-18.9326603708187,13.334638759352,122.294041202817)) ;
#79908 = CARTESIAN_POINT('Ctrl Pts',(-18.9548108444622,13.3357694147718,122.285106935635)) ;
#79909 = CARTESIAN_POINT('Ctrl Pts',(-18.9751066148332,13.3368053981615,122.276920752438)) ;
#79910 = CARTESIAN_POINT('Ctrl Pts',(-18.9955581376258,13.3378374523875,122.269312619075)) ;
#79911 = CARTESIAN_POINT('Ctrl Pts',(-19.0159746201976,13.3388536769403,122.262327272131)) ;
#79912 = CARTESIAN_POINT('Ctrl Pts',(-19.0310757895312,13.3396053333041,122.257160519891)) ;
#79913 = CARTESIAN_POINT('Ctrl Pts',(-19.0465094020696,13.340366364494,122.252217020429)) ;
#79914 = CARTESIAN_POINT('Ctrl Pts',(-19.0619560302779,13.3411223178931,122.247608954491)) ;
#79915 = CARTESIAN_POINT('Ctrl Pts',(-19.0697273679117,13.34150264485,122.245290595057)) ;
#79916 = CARTESIAN_POINT('Ctrl Pts',(-19.0775017289523,13.3418816865233,122.243056359391)) ;
#79917 = CARTESIAN_POINT('Ctrl Pts',(-19.0852370091252,13.342257602426,122.24091574547)) ;
#79918 = CARTESIAN_POINT('Ctrl Pts',(-19.1156522742549,13.3437357107289,122.232498811823)) ;
#79919 = CARTESIAN_POINT('Ctrl Pts',(-19.1467267842854,13.34523529048,122.225179703659)) ;
#79920 = CARTESIAN_POINT('Ctrl Pts',(-19.1782417556261,13.3467486313542,122.219075501309)) ;
#79921 = CARTESIAN_POINT('Ctrl Pts',(-19.2096032257156,13.3482546011375,122.213001030944)) ;
#79922 = CARTESIAN_POINT('Ctrl Pts',(-19.2414002980428,13.3497741983166,122.208129889525)) ;
#79923 = CARTESIAN_POINT('Ctrl Pts',(-19.2734003828313,13.3512998246835,122.204528622569)) ;
#79924 = CARTESIAN_POINT('Ctrl Pts',(-19.2789378517144,13.3515638273757,122.203905439729)) ;
#79925 = CARTESIAN_POINT('Ctrl Pts',(-19.2844813710085,13.3518280106103,122.203320159961)) ;
#79926 = CARTESIAN_POINT('Ctrl Pts',(-19.290029704004,13.3520923350148,122.202772972482)) ;
#79927 = CARTESIAN_POINT('Ctrl Pts',(-19.360440713544,13.3554467386142,122.19582890067)) ;
#79928 = CARTESIAN_POINT('Ctrl Pts',(-19.4313297110453,13.3587503674759,122.19504973569)) ;
#79929 = CARTESIAN_POINT('Ctrl Pts',(-19.5018619235022,13.3620953493016,122.200440834737)) ;
#79930 = CARTESIAN_POINT('Ctrl Pts',(-19.5670909451669,13.3651888279318,122.205426586697)) ;
#79931 = CARTESIAN_POINT('Ctrl Pts',(-19.6318412542396,13.3682908758495,122.215679365529)) ;
#79932 = CARTESIAN_POINT('Ctrl Pts',(-19.6954027317278,13.3713529115821,122.231082305476)) ;
#79933 = CARTESIAN_POINT('Ctrl Pts',(-19.7007491392792,13.3716104715321,122.232377907744)) ;
#79934 = CARTESIAN_POINT('Ctrl Pts',(-19.7060871405538,13.3718677483895,122.233709918135)) ;
#79935 = CARTESIAN_POINT('Ctrl Pts',(-19.711416315147,13.3721247132427,122.235078250401)) ;
#79936 = CARTESIAN_POINT('Ctrl Pts',(-19.769383977558,13.3749198274948,122.249962173134)) ;
#79937 = CARTESIAN_POINT('Ctrl Pts',(-19.826202342528,13.3777373491628,122.269121127388)) ;
#79938 = CARTESIAN_POINT('Ctrl Pts',(-19.881325845597,13.3805764700006,122.29236555184)) ;
#79939 = CARTESIAN_POINT('Ctrl Pts',(-19.8908402239965,13.3810665054386,122.296377565547)) ;
#79940 = CARTESIAN_POINT('Ctrl Pts',(-19.9003041537587,13.3815571843407,122.300511172329)) ;
#79941 = CARTESIAN_POINT('Ctrl Pts',(-19.909714882751,13.3820485025508,122.304765249621)) ;
#79942 = CARTESIAN_POINT('Ctrl Pts',(-19.9625480806773,13.3848068342658,122.328648256744)) ;
#79943 = CARTESIAN_POINT('Ctrl Pts',(-20.0136392374553,13.3875266827007,122.356303461624)) ;
#79944 = CARTESIAN_POINT('Ctrl Pts',(-20.0625177211307,13.3902529020074,122.387473933324)) ;
#79945 = CARTESIAN_POINT('Ctrl Pts',(-20.0734076217942,13.3908602910916,122.394418570615)) ;
#79946 = CARTESIAN_POINT('Ctrl Pts',(-20.0841877897517,13.3914679964118,122.40153751896)) ;
#79947 = CARTESIAN_POINT('Ctrl Pts',(-20.094853191974,13.3920765140131,122.408827629049)) ;
#79948 = CARTESIAN_POINT('Ctrl Pts',(-20.1447883901869,13.3949255811559,122.442959777532)) ;
#79949 = CARTESIAN_POINT('Ctrl Pts',(-20.1921329756688,13.3977924704886,122.480797749689)) ;
#79950 = CARTESIAN_POINT('Ctrl Pts',(-20.2364258868668,13.4006366507319,122.521969374432)) ;
#79951 = CARTESIAN_POINT('Ctrl Pts',(-20.2440550764245,13.4011265438011,122.529060941029)) ;
#79952 = CARTESIAN_POINT('Ctrl Pts',(-20.2515938080061,13.401615763137,122.536251313755)) ;
#79953 = CARTESIAN_POINT('Ctrl Pts',(-20.2590398232441,13.402104101619,122.543538468909)) ;
#79954 = CARTESIAN_POINT('Ctrl Pts',(-20.3092384544237,13.4053963220306,122.592666116681)) ;
#79955 = CARTESIAN_POINT('Ctrl Pts',(-20.3551122685804,13.4087006073066,122.646087327709)) ;
#79956 = CARTESIAN_POINT('Ctrl Pts',(-20.3961083195075,13.4120397603772,122.703176251959)) ;
#79957 = CARTESIAN_POINT('Ctrl Pts',(-20.4194907060249,13.4139442698597,122.735737322171)) ;
#79958 = CARTESIAN_POINT('Ctrl Pts',(-20.4412263130121,13.4158353105015,122.769414004562)) ;
#79959 = CARTESIAN_POINT('Ctrl Pts',(-20.4611878719886,13.4177137178806,122.803957082543)) ;
#79960 = CARTESIAN_POINT('Ctrl Pts',(-20.4764077561463,13.419145927797,122.830294787226)) ;
#79961 = CARTESIAN_POINT('Ctrl Pts',(-20.4905971960194,13.4205707934319,122.857135520827)) ;
#79962 = CARTESIAN_POINT('Ctrl Pts',(-20.5037186695672,13.4219886851572,122.884361176354)) ;
#79963 = CARTESIAN_POINT('Ctrl Pts',(-20.5144322700877,13.4231463848218,122.906590752641)) ;
#79964 = CARTESIAN_POINT('Ctrl Pts',(-20.5245108043189,13.424312442704,122.929244377532)) ;
#79965 = CARTESIAN_POINT('Ctrl Pts',(-20.533852008639,13.4254760024545,122.952094174275)) ;
#79966 = CARTESIAN_POINT('Ctrl Pts',(-20.5428664550124,13.4265988605586,122.97414467872)) ;
#79967 = CARTESIAN_POINT('Ctrl Pts',(-20.5511944078365,13.427719392245,122.996377332141)) ;
#79968 = CARTESIAN_POINT('Ctrl Pts',(-20.5587873005049,13.4288278410515,123.018571602254)) ;
#79969 = CARTESIAN_POINT('Ctrl Pts',(-20.5635331084435,13.4295206580548,123.032443751895)) ;
#79970 = CARTESIAN_POINT('Ctrl Pts',(-20.568102944472,13.4302253268598,123.04663484588)) ;
#79971 = CARTESIAN_POINT('Ctrl Pts',(-20.5723778495344,13.4309244835595,123.060799202518)) ;
#79972 = CARTESIAN_POINT('Ctrl Pts',(-20.5742105953237,13.4312242274085,123.06687177363)) ;
#79973 = CARTESIAN_POINT('Ctrl Pts',(-20.5759897537802,13.4315229581185,123.072939221501)) ;
#79974 = CARTESIAN_POINT('Ctrl Pts',(-20.5777087635802,13.4318193074104,123.078973461537)) ;
#79975 = CARTESIAN_POINT('Ctrl Pts',(-20.5862099243874,13.4332848679824,123.108815085998)) ;
#79976 = CARTESIAN_POINT('Ctrl Pts',(-20.5936629775568,13.4347626950335,123.139331795925)) ;
#79977 = CARTESIAN_POINT('Ctrl Pts',(-20.5999462560564,13.4362509313631,123.17030707295)) ;
#79978 = CARTESIAN_POINT('Ctrl Pts',(-20.6061951543524,13.4377310245127,123.201112862608)) ;
#79979 = CARTESIAN_POINT('Ctrl Pts',(-20.6112868051342,13.4392214133396,123.232371646335)) ;
#79980 = CARTESIAN_POINT('Ctrl Pts',(-20.6151500417308,13.4407202709629,123.263852742209)) ;
#79981 = CARTESIAN_POINT('Ctrl Pts',(-20.6160279965581,13.4410608996697,123.271007100841)) ;
#79982 = CARTESIAN_POINT('Ctrl Pts',(-20.6168427143569,13.4414019657611,123.278172888928)) ;
#79983 = CARTESIAN_POINT('Ctrl Pts',(-20.6175937276234,13.4417434477945,123.285347319404)) ;
#79984 = CARTESIAN_POINT('Ctrl Pts',(-20.6249761933209,13.4451002185878,123.355872021493)) ;
#79985 = CARTESIAN_POINT('Ctrl Pts',(-20.6261691568536,13.4484538465774,123.426893770811)) ;
#79986 = CARTESIAN_POINT('Ctrl Pts',(-20.621164396608,13.4517681683501,123.497606568652)) ;
#79987 = CARTESIAN_POINT('Ctrl Pts',(-20.6164600480809,13.4548835473062,123.564074816888)) ;
#79988 = CARTESIAN_POINT('Ctrl Pts',(-20.6062896907596,13.4580234506368,123.630062366585)) ;
#79989 = CARTESIAN_POINT('Ctrl Pts',(-20.5907777971686,13.4611842724295,123.694825471852)) ;
#79990 = CARTESIAN_POINT('Ctrl Pts',(-20.5899123609554,13.4613606203155,123.698438721018)) ;
#79991 = CARTESIAN_POINT('Ctrl Pts',(-20.5890303112337,13.4615370333149,123.702048161313)) ;
#79992 = CARTESIAN_POINT('Ctrl Pts',(-20.5881316743378,13.4617135108015,123.705653664296)) ;
#79993 = CARTESIAN_POINT('Ctrl Pts',(-20.5740434312057,13.4644802097312,123.762178388433)) ;
#79994 = CARTESIAN_POINT('Ctrl Pts',(-20.5558944562323,13.4672125201831,123.817653148817)) ;
#79995 = CARTESIAN_POINT('Ctrl Pts',(-20.5338558989619,13.4699542231989,123.871563619345)) ;
#79996 = CARTESIAN_POINT('Ctrl Pts',(-20.5290538725615,13.4705516184868,123.88331028223)) ;
#79997 = CARTESIAN_POINT('Ctrl Pts',(-20.5240673663107,13.4711494597049,123.894982741291)) ;
#79998 = CARTESIAN_POINT('Ctrl Pts',(-20.5188984612438,13.4717481997614,123.906575782835)) ;
#79999 = CARTESIAN_POINT('Ctrl Pts',(-20.4954340221929,13.4744662027781,123.959202831152)) ;
#80000 = CARTESIAN_POINT('Ctrl Pts',(-20.468235883307,13.4771958570766,124.010126937028)) ;
#80001 = CARTESIAN_POINT('Ctrl Pts',(-20.4375558260374,13.479905711605,124.058883431865)) ;
#80002 = CARTESIAN_POINT('Ctrl Pts',(-20.4305098026622,13.4805280604547,124.070080914298)) ;
#80003 = CARTESIAN_POINT('Ctrl Pts',(-20.4232803172227,13.4811493649787,124.081164173257)) ;
#80004 = CARTESIAN_POINT('Ctrl Pts',(-20.4158707580077,13.4817692441999,124.092127770366)) ;
#80005 = CARTESIAN_POINT('Ctrl Pts',(-20.3808596839067,13.4846982493829,124.143932108473)) ;
#80006 = CARTESIAN_POINT('Ctrl Pts',(-20.3418719851168,13.4876453239122,124.192992666741)) ;
#80007 = CARTESIAN_POINT('Ctrl Pts',(-20.299305823346,13.4906079428639,124.238804928216)) ;
#80008 = CARTESIAN_POINT('Ctrl Pts',(-20.2941076490582,13.4909697375153,124.244399515789)) ;
#80009 = CARTESIAN_POINT('Ctrl Pts',(-20.2888561590993,13.4913317639848,124.249945699095)) ;
#80010 = CARTESIAN_POINT('Ctrl Pts',(-20.2835521217904,13.4916940176739,124.255442590736)) ;
#80011 = CARTESIAN_POINT('Ctrl Pts',(-20.2344266246723,13.4950491774371,124.306354286624)) ;
#80012 = CARTESIAN_POINT('Ctrl Pts',(-20.1809262171979,13.4983581432627,124.352897140689)) ;
#80013 = CARTESIAN_POINT('Ctrl Pts',(-20.1236843419261,13.5016986778291,124.394512406366)) ;
#80014 = CARTESIAN_POINT('Ctrl Pts',(-20.0904562899518,13.503637808154,124.418669445322)) ;
#80015 = CARTESIAN_POINT('Ctrl Pts',(-20.0560448598183,13.5055781736,124.44110534709)) ;
#80016 = CARTESIAN_POINT('Ctrl Pts',(-20.0207051752874,13.5075076020376,124.461687207213)) ;
#80017 = CARTESIAN_POINT('Ctrl Pts',(-19.9950132719789,13.5089102939268,124.476650191948)) ;
#80018 = CARTESIAN_POINT('Ctrl Pts',(-19.9688313835272,13.5103072053112,124.490634187891)) ;
#80019 = CARTESIAN_POINT('Ctrl Pts',(-19.9422641111465,13.5116936591906,124.503604138563)) ;
#80020 = CARTESIAN_POINT('Ctrl Pts',(-19.9195299530059,13.512880076121,124.514702790522)) ;
#80021 = CARTESIAN_POINT('Ctrl Pts',(-19.8963628780932,13.5140730034568,124.52512850839)) ;
#80022 = CARTESIAN_POINT('Ctrl Pts',(-19.8729916778398,13.515263555876,124.534779676322)) ;
#80023 = CARTESIAN_POINT('Ctrl Pts',(-19.8496204775865,13.5164541082953,124.544430844253)) ;
#80024 = CARTESIAN_POINT('Ctrl Pts',(-19.826045673914,13.5176422857981,124.553307341802)) ;
#80025 = CARTESIAN_POINT('Ctrl Pts',(-19.8025139576554,13.5188192030627,124.561357383308)) ;
#80026 = CARTESIAN_POINT('Ctrl Pts',(-19.7895816065837,13.5194660027725,124.565781453434)) ;
#80027 = CARTESIAN_POINT('Ctrl Pts',(-19.7763375942247,13.520125198213,124.570063774942)) ;
#80028 = CARTESIAN_POINT('Ctrl Pts',(-19.7631512999327,13.5207777077975,124.574078752279)) ;
#80029 = CARTESIAN_POINT('Ctrl Pts',(-19.7583580644925,13.5210148958957,124.575538201858)) ;
#80030 = CARTESIAN_POINT('Ctrl Pts',(-19.7535726125751,13.5212512005702,124.576962802294)) ;
#80031 = CARTESIAN_POINT('Ctrl Pts',(-19.7488131806747,13.5214857053212,124.578348155295)) ;
#80032 = CARTESIAN_POINT('Ctrl Pts',(-19.7194810128453,13.5229309477061,124.58688602443)) ;
#80033 = CARTESIAN_POINT('Ctrl Pts',(-19.689468046598,13.5243872978826,124.594417550275)) ;
#80034 = CARTESIAN_POINT('Ctrl Pts',(-19.6589894692077,13.5258535219998,124.600818895649)) ;
#80035 = CARTESIAN_POINT('Ctrl Pts',(-19.628689447621,13.5273111563845,124.607182739358)) ;
#80036 = CARTESIAN_POINT('Ctrl Pts',(-19.597929815092,13.5287785493577,124.61242936282)) ;
#80037 = CARTESIAN_POINT('Ctrl Pts',(-19.5669400142052,13.5302544886269,124.616485450686)) ;
#80038 = CARTESIAN_POINT('Ctrl Pts',(-19.5590953627818,13.5306281028082,124.617512194794)) ;
#80039 = CARTESIAN_POINT('Ctrl Pts',(-19.5512360288153,13.5310022646201,124.618462903704)) ;
#80040 = CARTESIAN_POINT('Ctrl Pts',(-19.5433658496564,13.5313769543985,124.619336906487)) ;
#80041 = CARTESIAN_POINT('Ctrl Pts',(-19.4728496206335,13.534734147379,124.627167907427)) ;
#80042 = CARTESIAN_POINT('Ctrl Pts',(-19.40179126521,13.5380934253591,124.628806009374)) ;
#80043 = CARTESIAN_POINT('Ctrl Pts',(-19.3310038383664,13.5414077514449,124.624236377072)) ;
#80044 = CARTESIAN_POINT('Ctrl Pts',(-19.2641668580587,13.5445371143447,124.619921763055)) ;
#80045 = CARTESIAN_POINT('Ctrl Pts',(-19.1977803711769,13.5476779798217,124.610082037491)) ;
#80046 = CARTESIAN_POINT('Ctrl Pts',(-19.132598939239,13.5508697467509,124.594837974479)) ;
#80047 = CARTESIAN_POINT('Ctrl Pts',(-19.1291457887477,13.5510388386412,124.594030381855)) ;
#80048 = CARTESIAN_POINT('Ctrl Pts',(-19.1256960182946,13.5512080733925,124.593207633271)) ;
#80049 = CARTESIAN_POINT('Ctrl Pts',(-19.1222497395156,13.5513774568627,124.592369750726)) ;
#80050 = CARTESIAN_POINT('Ctrl Pts',(-19.0653270435142,13.5541751886781,124.578530320871)) ;
#80051 = CARTESIAN_POINT('Ctrl Pts',(-19.009444848784,13.5569465950344,124.560579032738)) ;
#80052 = CARTESIAN_POINT('Ctrl Pts',(-18.9551249662201,13.5596834935631,124.538687022647)) ;
#80053 = CARTESIAN_POINT('Ctrl Pts',(-18.9436985177004,13.5602592133302,124.534081933047)) ;
#80054 = CARTESIAN_POINT('Ctrl Pts',(-18.9323411408641,13.5608334061555,124.529302643614)) ;
#80055 = CARTESIAN_POINT('Ctrl Pts',(-18.9210575982544,13.5614059958772,124.524351025318)) ;
#80056 = CARTESIAN_POINT('Ctrl Pts',(-18.867195164181,13.5641392754157,124.500714280794)) ;
#80057 = CARTESIAN_POINT('Ctrl Pts',(-18.8150850440426,13.5669062015152,124.473176883449)) ;
#80058 = CARTESIAN_POINT('Ctrl Pts',(-18.7652166588985,13.5697062433898,124.441999493491)) ;
#80059 = CARTESIAN_POINT('Ctrl Pts',(-18.7554793384308,13.5702529806658,124.435911784084)) ;
#80060 = CARTESIAN_POINT('Ctrl Pts',(-18.7458274121111,13.5708009805345,124.429685434137)) ;
#80061 = CARTESIAN_POINT('Ctrl Pts',(-18.7362644137408,13.5713502390443,124.423322588574)) ;
#80062 = CARTESIAN_POINT('Ctrl Pts',(-18.6856315360648,13.5742583791341,124.389633449605)) ;
#80063 = CARTESIAN_POINT('Ctrl Pts',(-18.6375717516268,13.5771200435325,124.352166199987)) ;
#80064 = CARTESIAN_POINT('Ctrl Pts',(-18.592556707396,13.5799635694306,124.311292316254)) ;
#80065 = CARTESIAN_POINT('Ctrl Pts',(-18.5850880158292,13.5804353543251,124.304510707218)) ;
#80066 = CARTESIAN_POINT('Ctrl Pts',(-18.5777030672295,13.5809066399041,124.297635411384)) ;
#80067 = CARTESIAN_POINT('Ctrl Pts',(-18.5704039303823,13.5813775555924,124.290668234917)) ;
#80068 = CARTESIAN_POINT('Ctrl Pts',(-18.5194585604116,13.5846643790162,124.242039829913)) ;
#80069 = CARTESIAN_POINT('Ctrl Pts',(-18.4728077112974,13.5879998975297,124.189040152522)) ;
#80070 = CARTESIAN_POINT('Ctrl Pts',(-18.4310222353521,13.5913395370313,124.132304274245)) ;
#80071 = CARTESIAN_POINT('Ctrl Pts',(-18.4054964725353,13.5933796441231,124.097645662866)) ;
#80072 = CARTESIAN_POINT('Ctrl Pts',(-18.3818506872119,13.5954070301464,124.061674949715)) ;
#80073 = CARTESIAN_POINT('Ctrl Pts',(-18.3602282781819,13.5974254310589,124.024661623705)) ;
#80074 = CARTESIAN_POINT('Ctrl Pts',(-18.3464060730839,13.5987157013218,124.001000717894)) ;
#80075 = CARTESIAN_POINT('Ctrl Pts',(-18.3334097938057,13.6000022998613,123.976914292308)) ;
#80076 = CARTESIAN_POINT('Ctrl Pts',(-18.3212665887893,13.6012862026144,123.952477029753)) ;
#80077 = CARTESIAN_POINT('Ctrl Pts',(-18.3101238971397,13.6024643209503,123.930053223102)) ;
#80078 = CARTESIAN_POINT('Ctrl Pts',(-18.2996490228853,13.6036459044671,123.907224022409)) ;
#80079 = CARTESIAN_POINT('Ctrl Pts',(-18.2899392691066,13.6048221127595,123.884216358921)) ;
#80080 = CARTESIAN_POINT('Ctrl Pts',(-18.2801672790814,13.6060058601504,123.861061224072)) ;
#80081 = CARTESIAN_POINT('Ctrl Pts',(-18.2711704023844,13.6071841631893,123.8377258344)) ;
#80082 = CARTESIAN_POINT('Ctrl Pts',(-18.2629980370417,13.6083480103872,123.814459176388)) ;
#80083 = CARTESIAN_POINT('Ctrl Pts',(-18.2619265327424,13.6085006060219,123.811408612316)) ;
#80084 = CARTESIAN_POINT('Ctrl Pts',(-18.2608691312784,13.6086529531512,123.808359248072)) ;
#80085 = CARTESIAN_POINT('Ctrl Pts',(-18.259825879779,13.6088050314641,123.80531165987)) ;
#80086 = CARTESIAN_POINT('Origin',(-19.4092696390626,-30.19753203383,123.411833654984)) ;
#80087 = CARTESIAN_POINT('',(-18.259825879779,12.870840300276,123.80531165987)) ;
#80088 = CARTESIAN_POINT('',(-18.259825879779,12.8888247888664,123.80531165987)) ;
#80089 = CARTESIAN_POINT('',(-18.259825879779,-30.19753203383,123.80531165987)) ;
#80090 = CARTESIAN_POINT('Ctrl Pts',(-18.259825879779,13.2308616644972,123.80531165987)) ;
#80091 = CARTESIAN_POINT('Ctrl Pts',(-18.2662155410734,13.229929779781,123.823977395204)) ;
#80092 = CARTESIAN_POINT('Ctrl Pts',(-18.2731402046744,13.2289823495695,123.842708806219)) ;
#80093 = CARTESIAN_POINT('Ctrl Pts',(-18.2805158878487,13.2280348698646,123.861234217073)) ;
#80094 = CARTESIAN_POINT('Ctrl Pts',(-18.2856172109641,13.2273795542814,123.874047146313)) ;
#80095 = CARTESIAN_POINT('Ctrl Pts',(-18.2909332321475,13.2267242150223,123.886761815414)) ;
#80096 = CARTESIAN_POINT('Ctrl Pts',(-18.2964225629164,13.2260739790644,123.899293685344)) ;
#80097 = CARTESIAN_POINT('Ctrl Pts',(-18.3103610748771,13.2244228995324,123.931114616938)) ;
#80098 = CARTESIAN_POINT('Ctrl Pts',(-18.3257931498652,13.2227693158545,123.962619901958)) ;
#80099 = CARTESIAN_POINT('Ctrl Pts',(-18.342659690849,13.2211109075677,123.993545881482)) ;
#80100 = CARTESIAN_POINT('Ctrl Pts',(-18.3595262318327,13.2194524992809,124.024471861005)) ;
#80101 = CARTESIAN_POINT('Ctrl Pts',(-18.3778270305652,13.2177892663854,124.054817831129)) ;
#80102 = CARTESIAN_POINT('Ctrl Pts',(-18.3974491913048,13.2161188884183,124.084340366909)) ;
#80103 = CARTESIAN_POINT('Ctrl Pts',(-18.4365917331541,13.2127867966906,124.143232305857)) ;
#80104 = CARTESIAN_POINT('Ctrl Pts',(-18.4807968336201,13.2094316614767,124.198586925243)) ;
#80105 = CARTESIAN_POINT('Ctrl Pts',(-18.5295493467101,13.2061226175737,124.249770468418)) ;
#80106 = CARTESIAN_POINT('Ctrl Pts',(-18.5738592237391,13.2031151145931,124.296289844759)) ;
#80107 = CARTESIAN_POINT('Ctrl Pts',(-18.6218081637929,13.2001058428464,124.339234964246)) ;
#80108 = CARTESIAN_POINT('Ctrl Pts',(-18.6728787352241,13.1970492393281,124.378153650032)) ;
#80109 = CARTESIAN_POINT('Ctrl Pts',(-18.6776608816052,13.1967630250751,124.381797918094)) ;
#80110 = CARTESIAN_POINT('Ctrl Pts',(-18.6824703744847,13.1964763958135,124.385406910975)) ;
#80111 = CARTESIAN_POINT('Ctrl Pts',(-18.6873067735839,13.196189314135,124.388980274973)) ;
#80112 = CARTESIAN_POINT('Ctrl Pts',(-18.7337853611335,13.1934304121803,124.42332088831)) ;
#80113 = CARTESIAN_POINT('Ctrl Pts',(-18.7826889633777,13.1907006475101,124.454321374326)) ;
#80114 = CARTESIAN_POINT('Ctrl Pts',(-18.8335667710696,13.1879971448032,124.481699115624)) ;
#80115 = CARTESIAN_POINT('Ctrl Pts',(-18.8451091827042,13.1873838137161,124.487910176478)) ;
#80116 = CARTESIAN_POINT('Ctrl Pts',(-18.8567530918386,13.1867718342768,124.493934963064)) ;
#80117 = CARTESIAN_POINT('Ctrl Pts',(-18.8684930404656,13.1861611729122,124.499770494371)) ;
#80118 = CARTESIAN_POINT('Ctrl Pts',(-18.921426430588,13.1834078068394,124.526081891895)) ;
#80119 = CARTESIAN_POINT('Ctrl Pts',(-18.9762487783818,13.1806156356083,124.54850969572)) ;
#80120 = CARTESIAN_POINT('Ctrl Pts',(-19.0324403858194,13.1778111404927,124.566842577021)) ;
#80121 = CARTESIAN_POINT('Ctrl Pts',(-19.0431186301153,13.1772781946431,124.570326424416)) ;
#80122 = CARTESIAN_POINT('Ctrl Pts',(-19.0538462651928,13.1767448037479,124.573662534302)) ;
#80123 = CARTESIAN_POINT('Ctrl Pts',(-19.0646196442166,13.1762111495361,124.576849653646)) ;
#80124 = CARTESIAN_POINT('Ctrl Pts',(-19.1256125949851,13.1731898926963,124.594893371665)) ;
#80125 = CARTESIAN_POINT('Ctrl Pts',(-19.1879673326654,13.1702142455434,124.608126440509)) ;
#80126 = CARTESIAN_POINT('Ctrl Pts',(-19.2510277607696,13.1672162128466,124.616410511826)) ;
#80127 = CARTESIAN_POINT('Ctrl Pts',(-19.2583148370614,13.1668697690681,124.617367794571)) ;
#80128 = CARTESIAN_POINT('Ctrl Pts',(-19.2656113243022,13.1665230263658,124.618259047039)) ;
#80129 = CARTESIAN_POINT('Ctrl Pts',(-19.2729161992964,13.1661758798175,124.619084099403)) ;
#80130 = CARTESIAN_POINT('Ctrl Pts',(-19.3434354710218,13.1628246216797,124.627048929993)) ;
#80131 = CARTESIAN_POINT('Ctrl Pts',(-19.4145457118438,13.1594555857011,124.628819748298)) ;
#80132 = CARTESIAN_POINT('Ctrl Pts',(-19.4853787873511,13.1561418975459,124.624373672316)) ;
#80133 = CARTESIAN_POINT('Ctrl Pts',(-19.5211247735273,13.1544696413275,124.622129955389)) ;
#80134 = CARTESIAN_POINT('Ctrl Pts',(-19.5567324960085,13.1527935023082,124.618303626824)) ;
#80135 = CARTESIAN_POINT('Ctrl Pts',(-19.5919531539832,13.1511142506408,124.612946734366)) ;
#80136 = CARTESIAN_POINT('Ctrl Pts',(-19.6257887200428,13.1495010374305,124.607800507717)) ;
#80137 = CARTESIAN_POINT('Ctrl Pts',(-19.659266612977,13.147884951575,124.601242220538)) ;
#80138 = CARTESIAN_POINT('Ctrl Pts',(-19.6921789519876,13.1462666758921,124.593361571178)) ;
#80139 = CARTESIAN_POINT('Ctrl Pts',(-19.7130866415298,13.14523866006,124.588355358458)) ;
#80140 = CARTESIAN_POINT('Ctrl Pts',(-19.7340270137043,13.1442031299505,124.582750069096)) ;
#80141 = CARTESIAN_POINT('Ctrl Pts',(-19.7547385735872,13.1431759272749,124.576607071303)) ;
#80142 = CARTESIAN_POINT('Ctrl Pts',(-19.7709429874757,13.1423722593042,124.571800881943)) ;
#80143 = CARTESIAN_POINT('Ctrl Pts',(-19.7870074624047,13.1415736887748,124.566666606665)) ;
#80144 = CARTESIAN_POINT('Ctrl Pts',(-19.8028133768221,13.1407878025743,124.561254910467)) ;
#80145 = CARTESIAN_POINT('Ctrl Pts',(-19.8206105815958,13.1399029073845,124.555161427808)) ;
#80146 = CARTESIAN_POINT('Ctrl Pts',(-19.8384921936885,13.1390131360211,124.548572668124)) ;
#80147 = CARTESIAN_POINT('Ctrl Pts',(-19.8561768921072,13.1381271180561,124.541576901594)) ;
#80148 = CARTESIAN_POINT('Ctrl Pts',(-19.8677905613895,13.1375452636541,124.536982731147)) ;
#80149 = CARTESIAN_POINT('Ctrl Pts',(-19.8793196061818,13.1369650279592,124.532214063494)) ;
#80150 = CARTESIAN_POINT('Ctrl Pts',(-19.8906888197564,13.1363888549909,124.527307307091)) ;
#80151 = CARTESIAN_POINT('Ctrl Pts',(-19.9223697790245,13.1347833162944,124.513634351728)) ;
#80152 = CARTESIAN_POINT('Ctrl Pts',(-19.9537678031507,13.1331490770808,124.498477050397)) ;
#80153 = CARTESIAN_POINT('Ctrl Pts',(-19.9846098515591,13.1314967446217,124.481894184099)) ;
#80154 = CARTESIAN_POINT('Ctrl Pts',(-20.0154518999675,13.1298444121627,124.465311317801)) ;
#80155 = CARTESIAN_POINT('Ctrl Pts',(-20.045737223135,13.1281739864582,124.447303101419)) ;
#80156 = CARTESIAN_POINT('Ctrl Pts',(-20.0752140367108,13.1264960747798,124.427985196501)) ;
#80157 = CARTESIAN_POINT('Ctrl Pts',(-20.134546358724,13.1231186949368,124.389101205452)) ;
#80158 = CARTESIAN_POINT('Ctrl Pts',(-20.1903651834497,13.119800985813,124.345089512785)) ;
#80159 = CARTESIAN_POINT('Ctrl Pts',(-20.2420112365384,13.1164657148701,124.296473314913)) ;
#80160 = CARTESIAN_POINT('Ctrl Pts',(-20.289587554447,13.1133932649693,124.251688098093)) ;
#80161 = CARTESIAN_POINT('Ctrl Pts',(-20.3334894405665,13.1102924643633,124.203116917199)) ;
#80162 = CARTESIAN_POINT('Ctrl Pts',(-20.3732409589605,13.1072237698501,124.151296426528)) ;
#80163 = CARTESIAN_POINT('Ctrl Pts',(-20.376451305804,13.1069759409836,124.147111385167)) ;
#80164 = CARTESIAN_POINT('Ctrl Pts',(-20.379634604183,13.1067283215206,124.142905169477)) ;
#80165 = CARTESIAN_POINT('Ctrl Pts',(-20.382790614312,13.106480943306,124.138678072198)) ;
#80166 = CARTESIAN_POINT('Ctrl Pts',(-20.4181815626463,13.1037068870598,124.091276138962)) ;
#80167 = CARTESIAN_POINT('Ctrl Pts',(-20.450080551243,13.1009347849525,124.041322143165)) ;
#80168 = CARTESIAN_POINT('Ctrl Pts',(-20.4781886737502,13.0981286305586,123.989291872839)) ;
#80169 = CARTESIAN_POINT('Ctrl Pts',(-20.4834422395951,13.0976041445537,123.979567123311)) ;
#80170 = CARTESIAN_POINT('Ctrl Pts',(-20.488563501437,13.0970784689762,123.969769917912)) ;
#80171 = CARTESIAN_POINT('Ctrl Pts',(-20.4935506797433,13.0965513687291,123.959903468882)) ;
#80172 = CARTESIAN_POINT('Ctrl Pts',(-20.5196526873711,13.0937926194271,123.908264222791)) ;
#80173 = CARTESIAN_POINT('Ctrl Pts',(-20.5420463743133,13.0910584749845,123.854788919448)) ;
#80174 = CARTESIAN_POINT('Ctrl Pts',(-20.5605278743063,13.0883504306551,123.799970707929)) ;
#80175 = CARTESIAN_POINT('Ctrl Pts',(-20.5646923033328,13.0877402281058,123.787618542179)) ;
#80176 = CARTESIAN_POINT('Ctrl Pts',(-20.568658291334,13.0871313507487,123.775198270447)) ;
#80177 = CARTESIAN_POINT('Ctrl Pts',(-20.5724238452424,13.0865238156907,123.762715670384)) ;
#80178 = CARTESIAN_POINT('Ctrl Pts',(-20.590720052164,13.0835719027974,123.702064770356)) ;
#80179 = CARTESIAN_POINT('Ctrl Pts',(-20.6042533504138,13.0805866753739,123.640031126584)) ;
#80180 = CARTESIAN_POINT('Ctrl Pts',(-20.6128804632903,13.0775726118262,123.577263035347)) ;
#80181 = CARTESIAN_POINT('Ctrl Pts',(-20.6138609883362,13.0772300447541,123.57012905131)) ;
#80182 = CARTESIAN_POINT('Ctrl Pts',(-20.614778190337,13.0768871051846,123.562985593044)) ;
#80183 = CARTESIAN_POINT('Ctrl Pts',(-20.615631900232,13.0765437996927,123.555833623426)) ;
#80184 = CARTESIAN_POINT('Ctrl Pts',(-20.6240384845652,13.0731632290955,123.485407315736)) ;
#80185 = CARTESIAN_POINT('Ctrl Pts',(-20.6262623135186,13.069833350483,123.414355351615)) ;
#80186 = CARTESIAN_POINT('Ctrl Pts',(-20.6222745808894,13.0665160349233,123.343533529152)) ;
#80187 = CARTESIAN_POINT('Ctrl Pts',(-20.6202145429152,13.0648023302542,123.306947414373)) ;
#80188 = CARTESIAN_POINT('Ctrl Pts',(-20.6164972921792,13.0630787969676,123.270496808143)) ;
#80189 = CARTESIAN_POINT('Ctrl Pts',(-20.6111745725807,13.0613571613528,123.234434593911)) ;
#80190 = CARTESIAN_POINT('Ctrl Pts',(-20.6062595643491,13.0597674001297,123.201134684621)) ;
#80191 = CARTESIAN_POINT('Ctrl Pts',(-20.5999763082354,13.0581792569958,123.168166269748)) ;
#80192 = CARTESIAN_POINT('Ctrl Pts',(-20.5924035112702,13.0566019647332,123.135717490083)) ;
#80193 = CARTESIAN_POINT('Ctrl Pts',(-20.5873355715961,13.0555463941068,123.114001807146)) ;
#80194 = CARTESIAN_POINT('Ctrl Pts',(-20.5816296818219,13.0544857440984,123.09227307492)) ;
#80195 = CARTESIAN_POINT('Ctrl Pts',(-20.5753455905511,13.0534299520535,123.070787072469)) ;
#80196 = CARTESIAN_POINT('Ctrl Pts',(-20.5701618703803,13.0525590336846,123.053063360401)) ;
#80197 = CARTESIAN_POINT('Ctrl Pts',(-20.5645857062331,13.0516914209316,123.035504758932)) ;
#80198 = CARTESIAN_POINT('Ctrl Pts',(-20.5586761597941,13.0508326916541,123.018246884138)) ;
#80199 = CARTESIAN_POINT('Ctrl Pts',(-20.5529103591577,13.0499948503975,123.001408795718)) ;
#80200 = CARTESIAN_POINT('Ctrl Pts',(-20.546693394412,13.0491462820869,122.984473753146)) ;
#80201 = CARTESIAN_POINT('Ctrl Pts',(-20.5401199674319,13.0482990036882,122.967735207664)) ;
#80202 = CARTESIAN_POINT('Ctrl Pts',(-20.5361498654645,13.0477872794919,122.957625757517)) ;
#80203 = CARTESIAN_POINT('Ctrl Pts',(-20.5320507039911,13.0472760258174,122.947587682286)) ;
#80204 = CARTESIAN_POINT('Ctrl Pts',(-20.5278519379966,13.0467678900933,122.937682269247)) ;
#80205 = CARTESIAN_POINT('Ctrl Pts',(-20.5150841029079,13.045222723457,122.907561352688)) ;
#80206 = CARTESIAN_POINT('Ctrl Pts',(-20.500969811741,13.0436600419622,122.877660814971)) ;
#80207 = CARTESIAN_POINT('Ctrl Pts',(-20.4855559912974,13.0420909675042,122.848226004151)) ;
#80208 = CARTESIAN_POINT('Ctrl Pts',(-20.4702064941635,13.0405284409401,122.81891402754)) ;
#80209 = CARTESIAN_POINT('Ctrl Pts',(-20.4535684798359,13.0389595746585,122.79006450468)) ;
#80210 = CARTESIAN_POINT('Ctrl Pts',(-20.4357371405512,13.0373953518966,122.761902609047)) ;
#80211 = CARTESIAN_POINT('Ctrl Pts',(-20.4336430548303,13.0372116519234,122.758595318295)) ;
#80212 = CARTESIAN_POINT('Ctrl Pts',(-20.4315325643706,13.0370280159926,122.755297485666)) ;
#80213 = CARTESIAN_POINT('Ctrl Pts',(-20.4294058654555,13.0368444618938,122.752009454393)) ;
#80214 = CARTESIAN_POINT('Ctrl Pts',(-20.3911287352109,13.0335407859017,122.69283022579)) ;
#80215 = CARTESIAN_POINT('Ctrl Pts',(-20.3477826778876,13.0302328466101,122.637107690408)) ;
#80216 = CARTESIAN_POINT('Ctrl Pts',(-20.2998744795623,13.0268838791217,122.585474826046)) ;
#80217 = CARTESIAN_POINT('Ctrl Pts',(-20.2568823878123,13.0238785664078,122.539140275395)) ;
#80218 = CARTESIAN_POINT('Ctrl Pts',(-20.2103150811076,13.0208984974685,122.496210972854)) ;
#80219 = CARTESIAN_POINT('Ctrl Pts',(-20.160660763911,13.0179372381888,122.457130940217)) ;
#80220 = CARTESIAN_POINT('Ctrl Pts',(-20.1546424670006,13.0175783220144,122.452394287838)) ;
#80221 = CARTESIAN_POINT('Ctrl Pts',(-20.1485788626903,13.0172196821611,122.447714136001)) ;
#80222 = CARTESIAN_POINT('Ctrl Pts',(-20.142470855856,13.0168613071728,122.443091237322)) ;
#80223 = CARTESIAN_POINT('Ctrl Pts',(-20.0955166488246,13.0141063637269,122.40755353287)) ;
#80224 = CARTESIAN_POINT('Ctrl Pts',(-20.0460100127249,13.0113300555962,122.375458694454)) ;
#80225 = CARTESIAN_POINT('Ctrl Pts',(-19.9944195367589,13.0085420966997,122.347105758613)) ;
#80226 = CARTESIAN_POINT('Ctrl Pts',(-19.9840590476005,13.0079822139427,122.341411872699)) ;
#80227 = CARTESIAN_POINT('Ctrl Pts',(-19.9736146068897,13.0074218613176,122.335868752493)) ;
#80228 = CARTESIAN_POINT('Ctrl Pts',(-19.9630901436767,13.0068611174976,122.33047860471)) ;
#80229 = CARTESIAN_POINT('Ctrl Pts',(-19.9115657163906,13.0041158939557,122.304090154115)) ;
#80230 = CARTESIAN_POINT('Ctrl Pts',(-19.8581843020153,13.0013947918625,122.281404000126)) ;
#80231 = CARTESIAN_POINT('Ctrl Pts',(-19.8034385789658,12.9986707661172,122.262626648871)) ;
#80232 = CARTESIAN_POINT('Ctrl Pts',(-19.7910897472083,12.9980563156404,122.258391096967)) ;
#80233 = CARTESIAN_POINT('Ctrl Pts',(-19.7786715777912,12.9974417164067,122.254354232714)) ;
#80234 = CARTESIAN_POINT('Ctrl Pts',(-19.7661898627449,12.9968266580205,122.250518086325)) ;
#80235 = CARTESIAN_POINT('Ctrl Pts',(-19.7075298248851,12.9939360818386,122.232489434682)) ;
#80236 = CARTESIAN_POINT('Ctrl Pts',(-19.6475485678453,12.9910307279178,122.218923594634)) ;
#80237 = CARTESIAN_POINT('Ctrl Pts',(-19.5868449944418,12.9881433223301,122.209954755408)) ;
#80238 = CARTESIAN_POINT('Ctrl Pts',(-19.5777701226496,12.9877116700558,122.208613960105)) ;
#80239 = CARTESIAN_POINT('Ctrl Pts',(-19.568679128988,12.9872804189036,122.207375809367)) ;
#80240 = CARTESIAN_POINT('Ctrl Pts',(-19.5595740378673,12.9868496782118,122.206240654098)) ;
#80241 = CARTESIAN_POINT('Ctrl Pts',(-19.4898970413724,12.9835534215054,122.197553842661)) ;
#80242 = CARTESIAN_POINT('Ctrl Pts',(-19.4195615991172,12.9802519555717,122.194920530747)) ;
#80243 = CARTESIAN_POINT('Ctrl Pts',(-19.3493791105797,12.9769173597985,122.198384430384)) ;
#80244 = CARTESIAN_POINT('Ctrl Pts',(-19.3116842828543,12.9751263572873,122.200244881656)) ;
#80245 = CARTESIAN_POINT('Ctrl Pts',(-19.2741285272671,12.9733486752165,122.203863529548)) ;
#80246 = CARTESIAN_POINT('Ctrl Pts',(-19.2369706410513,12.9715813245093,122.20918701055)) ;
#80247 = CARTESIAN_POINT('Ctrl Pts',(-19.2042609075386,12.970025542506,122.213873220199)) ;
#80248 = CARTESIAN_POINT('Ctrl Pts',(-19.1718596801468,12.9684777663934,122.219879657425)) ;
#80249 = CARTESIAN_POINT('Ctrl Pts',(-19.139934078093,12.9669359571818,122.227137807232)) ;
#80250 = CARTESIAN_POINT('Ctrl Pts',(-19.1174728567786,12.96585121905,122.232244270341)) ;
#80251 = CARTESIAN_POINT('Ctrl Pts',(-19.0950170794709,12.9647552497427,122.238025766184)) ;
#80252 = CARTESIAN_POINT('Ctrl Pts',(-19.0728179318652,12.9636626863374,122.244423639262)) ;
#80253 = CARTESIAN_POINT('Ctrl Pts',(-19.0535145082355,12.9627126402082,122.249986954419)) ;
#80254 = CARTESIAN_POINT('Ctrl Pts',(-19.0344051671983,12.9617651693813,122.256015449663)) ;
#80255 = CARTESIAN_POINT('Ctrl Pts',(-19.0156454794067,12.9608298976992,122.262439937836)) ;
#80256 = CARTESIAN_POINT('Ctrl Pts',(-18.9996147016043,12.9600306769079,122.267929876877)) ;
#80257 = CARTESIAN_POINT('Ctrl Pts',(-18.9834735656277,12.9592217466141,122.273836898882)) ;
#80258 = CARTESIAN_POINT('Ctrl Pts',(-18.9675274205177,12.9584173094524,122.280060838364)) ;
#80259 = CARTESIAN_POINT('Ctrl Pts',(-18.958652576749,12.9579695991071,122.283524778404)) ;
#80260 = CARTESIAN_POINT('Ctrl Pts',(-18.9498378417739,12.9575232805054,122.287085994564)) ;
#80261 = CARTESIAN_POINT('Ctrl Pts',(-18.9411333105159,12.9570808020558,122.290720692799)) ;
#80262 = CARTESIAN_POINT('Ctrl Pts',(-18.9115402471301,12.9555764944238,122.303077688491)) ;
#80263 = CARTESIAN_POINT('Ctrl Pts',(-18.8821336217213,12.95405373186,122.316737473371)) ;
#80264 = CARTESIAN_POINT('Ctrl Pts',(-18.8531578655204,12.9525179515629,122.331655155192)) ;
#80265 = CARTESIAN_POINT('Ctrl Pts',(-18.8243115077086,12.9509890296715,122.346506218425)) ;
#80266 = CARTESIAN_POINT('Ctrl Pts',(-18.7958927801328,12.9494472060551,122.3626037859)) ;
#80267 = CARTESIAN_POINT('Ctrl Pts',(-18.7681258982293,12.9478978453932,122.379854682488)) ;
#80268 = CARTESIAN_POINT('Ctrl Pts',(-18.7641464874169,12.9476757987626,122.382326994814)) ;
#80269 = CARTESIAN_POINT('Ctrl Pts',(-18.7601804276636,12.9474535973271,122.384822916485)) ;
#80270 = CARTESIAN_POINT('Ctrl Pts',(-18.7562283392693,12.9472312568782,122.387342094819)) ;
#80271 = CARTESIAN_POINT('Ctrl Pts',(-18.6964137833706,12.943866151171,122.425469666436)) ;
#80272 = CARTESIAN_POINT('Ctrl Pts',(-18.6400443839774,12.9405486009369,122.468770151356)) ;
#80273 = CARTESIAN_POINT('Ctrl Pts',(-18.5877897308444,12.9372019724685,122.51672659073)) ;
#80274 = CARTESIAN_POINT('Ctrl Pts',(-18.5396101659096,12.9341163314023,122.560943138851)) ;
#80275 = CARTESIAN_POINT('Ctrl Pts',(-18.4950608892707,12.9310133340656,122.609000108474)) ;
#80276 = CARTESIAN_POINT('Ctrl Pts',(-18.4546266679024,12.9279493121563,122.660366627298)) ;
#80277 = CARTESIAN_POINT('Ctrl Pts',(-18.4512066913697,12.9276901533876,122.664711271093)) ;
#80278 = CARTESIAN_POINT('Ctrl Pts',(-18.4478161310652,12.9274312734485,122.669079570653)) ;
#80279 = CARTESIAN_POINT('Ctrl Pts',(-18.4444552679901,12.927172706425,122.673471192872)) ;
#80280 = CARTESIAN_POINT('Ctrl Pts',(-18.4082581932642,12.9243878950052,122.720769721275)) ;
#80281 = CARTESIAN_POINT('Ctrl Pts',(-18.375571621791,12.9215938819148,122.770694787871)) ;
#80282 = CARTESIAN_POINT('Ctrl Pts',(-18.3467042321094,12.9187651732054,122.82276604254)) ;
#80283 = CARTESIAN_POINT('Ctrl Pts',(-18.3414903806441,12.9182542691295,122.83217083426)) ;
#80284 = CARTESIAN_POINT('Ctrl Pts',(-18.3364009997207,12.9177422332347,122.841645565417)) ;
#80285 = CARTESIAN_POINT('Ctrl Pts',(-18.3314377545054,12.917228915314,122.851187309489)) ;
#80286 = CARTESIAN_POINT('Ctrl Pts',(-18.3047988596977,12.9144738182958,122.902400075654)) ;
#80287 = CARTESIAN_POINT('Ctrl Pts',(-18.2818294855986,12.9117487873613,122.95548336231)) ;
#80288 = CARTESIAN_POINT('Ctrl Pts',(-18.262738061945,12.9090471640161,123.009949046226)) ;
#80289 = CARTESIAN_POINT('Ctrl Pts',(-18.2583816834394,12.9084306938102,123.022377304013)) ;
#80290 = CARTESIAN_POINT('Ctrl Pts',(-18.2542270258558,12.907815442401,123.034877458936)) ;
#80291 = CARTESIAN_POINT('Ctrl Pts',(-18.2502762138882,12.9072013306773,123.047443566635)) ;
#80292 = CARTESIAN_POINT('Ctrl Pts',(-18.2316189672304,12.9043012600087,123.106785538054)) ;
#80293 = CARTESIAN_POINT('Ctrl Pts',(-18.2175379643146,12.9013695518874,123.167515476281)) ;
#80294 = CARTESIAN_POINT('Ctrl Pts',(-18.2081770681978,12.8984127829643,123.229015350927)) ;
#80295 = CARTESIAN_POINT('Ctrl Pts',(-18.2069304814426,12.898019031241,123.237205264396)) ;
#80296 = CARTESIAN_POINT('Ctrl Pts',(-18.2057675283162,12.8976248350859,123.245408813936)) ;
#80297 = CARTESIAN_POINT('Ctrl Pts',(-18.2046884809982,12.8972302100307,123.253624522122)) ;
#80298 = CARTESIAN_POINT('Ctrl Pts',(-18.1954900615473,12.8938661992751,123.323659940141)) ;
#80299 = CARTESIAN_POINT('Ctrl Pts',(-18.1924158000991,12.8905427332555,123.394395417807)) ;
#80300 = CARTESIAN_POINT('Ctrl Pts',(-18.1955062488531,12.8872427554171,123.46497806835)) ;
#80301 = CARTESIAN_POINT('Ctrl Pts',(-18.1972007151705,12.8854334061153,123.503677925057)) ;
#80302 = CARTESIAN_POINT('Ctrl Pts',(-18.2007483633934,12.8836140272436,123.542250460683)) ;
#80303 = CARTESIAN_POINT('Ctrl Pts',(-18.2060983810991,12.8817930848426,123.580430274451)) ;
#80304 = CARTESIAN_POINT('Ctrl Pts',(-18.2104580346587,12.880309224703,123.611542463261)) ;
#80305 = CARTESIAN_POINT('Ctrl Pts',(-18.2160134967859,12.878824326319,123.64239381509)) ;
#80306 = CARTESIAN_POINT('Ctrl Pts',(-18.2227126010336,12.8773429707999,123.672847623171)) ;
#80307 = CARTESIAN_POINT('Ctrl Pts',(-18.2277179246073,12.8762361566011,123.695601585173)) ;
#80308 = CARTESIAN_POINT('Ctrl Pts',(-18.2334066902034,12.8751269962437,123.718322694069)) ;
#80309 = CARTESIAN_POINT('Ctrl Pts',(-18.2397173376852,12.8740258444861,123.740761170446)) ;
#80310 = CARTESIAN_POINT('Ctrl Pts',(-18.245864571975,12.8729532068744,123.76261860612)) ;
#80311 = CARTESIAN_POINT('Ctrl Pts',(-18.2526015019176,12.8718881684698,123.784207516959)) ;
#80312 = CARTESIAN_POINT('Ctrl Pts',(-18.259825879779,12.870840300276,123.80531165987)) ;
#80313 = CARTESIAN_POINT('Ctrl Pts',(-18.259825879779,12.8888247888663,123.80531165987)) ;
#80314 = CARTESIAN_POINT('Ctrl Pts',(-18.2532458294082,12.8897813285136,123.786089752316)) ;
#80315 = CARTESIAN_POINT('Ctrl Pts',(-18.247071181349,12.8907544247006,123.766465209361)) ;
#80316 = CARTESIAN_POINT('Ctrl Pts',(-18.2414031003154,12.8917312466636,123.746697274626)) ;
#80317 = CARTESIAN_POINT('Ctrl Pts',(-18.2371820599301,12.8924586895019,123.731976022344)) ;
#80318 = CARTESIAN_POINT('Ctrl Pts',(-18.2332409732336,12.893188198594,123.717175704504)) ;
#80319 = CARTESIAN_POINT('Ctrl Pts',(-18.2296035771432,12.8939144748306,123.702408737262)) ;
#80320 = CARTESIAN_POINT('Ctrl Pts',(-18.2212772303626,12.8955769904473,123.668605739978)) ;
#80321 = CARTESIAN_POINT('Ctrl Pts',(-18.2143391259864,12.8972454835374,123.634164045277)) ;
#80322 = CARTESIAN_POINT('Ctrl Pts',(-18.2088966327909,12.8989103111607,123.599318432764)) ;
#80323 = CARTESIAN_POINT('Ctrl Pts',(-18.2034541395954,12.900575138784,123.56447282025)) ;
#80324 = CARTESIAN_POINT('Ctrl Pts',(-18.199507497113,12.9022363009406,123.529223921072)) ;
#80325 = CARTESIAN_POINT('Ctrl Pts',(-18.197112973659,12.9038841546903,123.493822157852)) ;
#80326 = CARTESIAN_POINT('Ctrl Pts',(-18.1923664545662,12.9071505955648,123.423647382676)) ;
#80327 = CARTESIAN_POINT('Ctrl Pts',(-18.19372501243,12.9104588638225,123.353212635087)) ;
#80328 = CARTESIAN_POINT('Ctrl Pts',(-18.2011587472781,12.9138225142835,123.283326965522)) ;
#80329 = CARTESIAN_POINT('Ctrl Pts',(-18.2077270055295,12.916794549922,123.221577772801)) ;
#80330 = CARTESIAN_POINT('Ctrl Pts',(-18.2190277864584,12.919718658498,123.160388817979)) ;
#80331 = CARTESIAN_POINT('Ctrl Pts',(-18.2349430601355,12.9226187056347,123.100380637484)) ;
#80332 = CARTESIAN_POINT('Ctrl Pts',(-18.2372015476686,12.9230302424035,123.091865061171)) ;
#80333 = CARTESIAN_POINT('Ctrl Pts',(-18.2395528758531,12.9234412946332,123.083373246407)) ;
#80334 = CARTESIAN_POINT('Ctrl Pts',(-18.241996623602,12.9238519305238,123.074906951587)) ;
#80335 = CARTESIAN_POINT('Ctrl Pts',(-18.2583480343684,12.9265995447674,123.018257952383)) ;
#80336 = CARTESIAN_POINT('Ctrl Pts',(-18.2788154430492,12.9293831647335,122.96284209491)) ;
#80337 = CARTESIAN_POINT('Ctrl Pts',(-18.3032017711111,12.9321792524141,122.909180924394)) ;
#80338 = CARTESIAN_POINT('Ctrl Pts',(-18.3079630592657,12.9327251722065,122.898703894195)) ;
#80339 = CARTESIAN_POINT('Ctrl Pts',(-18.3128735896712,12.9332715672717,122.888293694738)) ;
#80340 = CARTESIAN_POINT('Ctrl Pts',(-18.31793167961,12.9338182624219,122.877954123308)) ;
#80341 = CARTESIAN_POINT('Ctrl Pts',(-18.3435730794007,12.9365896700242,122.825538866186)) ;
#80342 = CARTESIAN_POINT('Ctrl Pts',(-18.3729787867492,12.9393311003956,122.775004910072)) ;
#80343 = CARTESIAN_POINT('Ctrl Pts',(-18.4058732647575,12.9420751350093,122.726821529459)) ;
#80344 = CARTESIAN_POINT('Ctrl Pts',(-18.4128371725788,12.9426560593852,122.716620892714)) ;
#80345 = CARTESIAN_POINT('Ctrl Pts',(-18.4199572833244,12.94323710048,122.706525510553)) ;
#80346 = CARTESIAN_POINT('Ctrl Pts',(-18.4272307252923,12.9438185674378,122.696539681904)) ;
#80347 = CARTESIAN_POINT('Ctrl Pts',(-18.4642301242527,12.9467764418593,122.645742595765)) ;
#80348 = CARTESIAN_POINT('Ctrl Pts',(-18.5051425390423,12.9497506721255,122.597862446162)) ;
#80349 = CARTESIAN_POINT('Ctrl Pts',(-18.5495449045503,12.9527091008555,122.553393629733)) ;
#80350 = CARTESIAN_POINT('Ctrl Pts',(-18.5550400253381,12.9530752282685,122.547890285153)) ;
#80351 = CARTESIAN_POINT('Ctrl Pts',(-18.5605885476501,12.9534411136669,122.542439146153)) ;
#80352 = CARTESIAN_POINT('Ctrl Pts',(-18.5661896262514,12.9538066960978,122.537041114959)) ;
#80353 = CARTESIAN_POINT('Ctrl Pts',(-18.6169576386995,12.9571203245476,122.48811351827)) ;
#80354 = CARTESIAN_POINT('Ctrl Pts',(-18.6719101867737,12.9604271439176,122.443678705657)) ;
#80355 = CARTESIAN_POINT('Ctrl Pts',(-18.7304180440209,12.9637793859921,122.404259137644)) ;
#80356 = CARTESIAN_POINT('Ctrl Pts',(-18.7598230568367,12.965464163487,122.384447560923)) ;
#80357 = CARTESIAN_POINT('Ctrl Pts',(-18.7900595549664,12.9671409241981,122.365952648998)) ;
#80358 = CARTESIAN_POINT('Ctrl Pts',(-18.8208969866602,12.9688031493527,122.348883271387)) ;
#80359 = CARTESIAN_POINT('Ctrl Pts',(-18.851734418354,12.9704653745073,122.331813893776)) ;
#80360 = CARTESIAN_POINT('Ctrl Pts',(-18.8831721463384,12.9721130641054,122.316170247903)) ;
#80361 = CARTESIAN_POINT('Ctrl Pts',(-18.9149607439661,12.973739699374,122.302011771837)) ;
#80362 = CARTESIAN_POINT('Ctrl Pts',(-18.9338084784656,12.9747041454949,122.293617088909)) ;
#80363 = CARTESIAN_POINT('Ctrl Pts',(-18.9530441471631,12.9756793751788,122.285629754367)) ;
#80364 = CARTESIAN_POINT('Ctrl Pts',(-18.9724168258569,12.976654697032,122.278164604653)) ;
#80365 = CARTESIAN_POINT('Ctrl Pts',(-18.9868451849857,12.977381096008,122.272604719893)) ;
#80366 = CARTESIAN_POINT('Ctrl Pts',(-19.001349010063,12.9781075461099,122.267333529315)) ;
#80367 = CARTESIAN_POINT('Ctrl Pts',(-19.0158180196968,12.9788296304523,122.262380863738)) ;
#80368 = CARTESIAN_POINT('Ctrl Pts',(-19.0342731679293,12.9797506453602,122.256063763973)) ;
#80369 = CARTESIAN_POINT('Ctrl Pts',(-19.053109171126,12.9806863048851,122.2501174097)) ;
#80370 = CARTESIAN_POINT('Ctrl Pts',(-19.0720577385372,12.9816216662129,122.244642997795)) ;
#80371 = CARTESIAN_POINT('Ctrl Pts',(-19.0851606201767,12.9822684659684,122.240857457196)) ;
#80372 = CARTESIAN_POINT('Ctrl Pts',(-19.0983169045046,12.9829151231355,122.237296577758)) ;
#80373 = CARTESIAN_POINT('Ctrl Pts',(-19.1114337586695,12.9835566968411,122.233979808178)) ;
#80374 = CARTESIAN_POINT('Ctrl Pts',(-19.1451010559027,12.9852034371626,122.22546658802)) ;
#80375 = CARTESIAN_POINT('Ctrl Pts',(-19.1794387949778,12.9868560446172,122.218324534818)) ;
#80376 = CARTESIAN_POINT('Ctrl Pts',(-19.21420034137,12.9885147179043,122.212669835824)) ;
#80377 = CARTESIAN_POINT('Ctrl Pts',(-19.2489618877623,12.9901733911914,122.207015136831)) ;
#80378 = CARTESIAN_POINT('Ctrl Pts',(-19.2841465466228,12.9918381303111,122.202848063812)) ;
#80379 = CARTESIAN_POINT('Ctrl Pts',(-19.3194904692908,12.9935091339629,122.200229100371)) ;
#80380 = CARTESIAN_POINT('Ctrl Pts',(-19.3902004547269,12.9968521880148,122.194989532921)) ;
#80381 = CARTESIAN_POINT('Ctrl Pts',(-19.4612308056923,13.000197572698,122.195951121451)) ;
#80382 = CARTESIAN_POINT('Ctrl Pts',(-19.5317526856796,13.0035326050172,122.203097207542)) ;
#80383 = CARTESIAN_POINT('Ctrl Pts',(-19.5962898690814,13.0065846165698,122.209636855502)) ;
#80384 = CARTESIAN_POINT('Ctrl Pts',(-19.6602229995032,13.0096473642197,122.221341375042)) ;
#80385 = CARTESIAN_POINT('Ctrl Pts',(-19.7228608896261,13.0127043920223,122.238076259414)) ;
#80386 = CARTESIAN_POINT('Ctrl Pts',(-19.7282510714014,13.0129674586026,122.239516347332)) ;
#80387 = CARTESIAN_POINT('Ctrl Pts',(-19.7336316683635,13.0132304828266,122.240993654563)) ;
#80388 = CARTESIAN_POINT('Ctrl Pts',(-19.7390022433148,13.0134934542082,122.242508077663)) ;
#80389 = CARTESIAN_POINT('Ctrl Pts',(-19.7953263709184,13.0162513774818,122.258390652745)) ;
#80390 = CARTESIAN_POINT('Ctrl Pts',(-19.8504639847626,13.0189973645646,122.278336270964)) ;
#80391 = CARTESIAN_POINT('Ctrl Pts',(-19.9039010481062,13.0217630898227,122.302155474036)) ;
#80392 = CARTESIAN_POINT('Ctrl Pts',(-19.9148591565728,13.0223302451915,122.307039975439)) ;
#80393 = CARTESIAN_POINT('Ctrl Pts',(-19.925745816016,13.0228982305888,122.312087205238)) ;
#80394 = CARTESIAN_POINT('Ctrl Pts',(-19.9365566901172,13.0234673191557,122.317295276546)) ;
#80395 = CARTESIAN_POINT('Ctrl Pts',(-19.9886872531689,13.0262114920266,122.342408850818)) ;
#80396 = CARTESIAN_POINT('Ctrl Pts',(-20.038990378096,13.0289466035877,122.371235502409)) ;
#80397 = CARTESIAN_POINT('Ctrl Pts',(-20.0870043674368,13.0316624975888,122.403507549976)) ;
#80398 = CARTESIAN_POINT('Ctrl Pts',(-20.0978207686876,13.0322743234269,122.410777668966)) ;
#80399 = CARTESIAN_POINT('Ctrl Pts',(-20.1085211047223,13.0328851739874,122.418222459547)) ;
#80400 = CARTESIAN_POINT('Ctrl Pts',(-20.1191002842362,13.033494933158,122.425838547868)) ;
#80401 = CARTESIAN_POINT('Ctrl Pts',(-20.1704527012543,13.0364547664011,122.462807817837)) ;
#80402 = CARTESIAN_POINT('Ctrl Pts',(-20.2188726090177,13.0394380498734,122.503762264382)) ;
#80403 = CARTESIAN_POINT('Ctrl Pts',(-20.2638534759819,13.0424389658114,122.548275688336)) ;
#80404 = CARTESIAN_POINT('Ctrl Pts',(-20.2689325561807,13.0427778186114,122.553301986526)) ;
#80405 = CARTESIAN_POINT('Ctrl Pts',(-20.2739678224269,13.0431168962276,122.558373619549)) ;
#80406 = CARTESIAN_POINT('Ctrl Pts',(-20.2789585710333,13.0434561902842,122.563489940625)) ;
#80407 = CARTESIAN_POINT('Ctrl Pts',(-20.328332389001,13.0468128496365,122.614106055637)) ;
#80408 = CARTESIAN_POINT('Ctrl Pts',(-20.3732090024784,13.0501297950685,122.668954533018)) ;
#80409 = CARTESIAN_POINT('Ctrl Pts',(-20.413054955581,13.0534545350462,122.727391594305)) ;
#80410 = CARTESIAN_POINT('Ctrl Pts',(-20.4333412241692,13.0551472180647,122.757142919809)) ;
#80411 = CARTESIAN_POINT('Ctrl Pts',(-20.4522765989244,13.0568444933791,122.78776252857)) ;
#80412 = CARTESIAN_POINT('Ctrl Pts',(-20.4697500363502,13.0585351659895,122.819020680216)) ;
#80413 = CARTESIAN_POINT('Ctrl Pts',(-20.4865506341453,13.0601607368395,122.849075192149)) ;
#80414 = CARTESIAN_POINT('Ctrl Pts',(-20.501999818948,13.0617802036885,122.879719360213)) ;
#80415 = CARTESIAN_POINT('Ctrl Pts',(-20.5160412745599,13.063383615616,122.910732424749)) ;
#80416 = CARTESIAN_POINT('Ctrl Pts',(-20.5249283323932,13.0643984402128,122.930361080476)) ;
#80417 = CARTESIAN_POINT('Ctrl Pts',(-20.5333601781884,13.0654199755197,122.950384604298)) ;
#80418 = CARTESIAN_POINT('Ctrl Pts',(-20.5412249340041,13.0664387567713,122.970559243378)) ;
#80419 = CARTESIAN_POINT('Ctrl Pts',(-20.5474251735456,13.0672419206518,122.986464072197)) ;
#80420 = CARTESIAN_POINT('Ctrl Pts',(-20.5532738640289,13.068043372866,123.002462265936)) ;
#80421 = CARTESIAN_POINT('Ctrl Pts',(-20.558737602334,13.0688384759608,123.018426362858)) ;
#80422 = CARTESIAN_POINT('Ctrl Pts',(-20.5647703980733,13.0697163903658,123.036053147034)) ;
#80423 = CARTESIAN_POINT('Ctrl Pts',(-20.5704708719528,13.0706067410412,123.054045743056)) ;
#80424 = CARTESIAN_POINT('Ctrl Pts',(-20.5757361798665,13.0714972686474,123.072125390042)) ;
#80425 = CARTESIAN_POINT('Ctrl Pts',(-20.579151634762,13.072074928477,123.083853140787)) ;
#80426 = CARTESIAN_POINT('Ctrl Pts',(-20.5823849749415,13.0726526627545,123.095617130514)) ;
#80427 = CARTESIAN_POINT('Ctrl Pts',(-20.5854194026214,13.0732271253608,123.107337957534)) ;
#80428 = CARTESIAN_POINT('Ctrl Pts',(-20.5941186488215,13.0748740229545,123.140939799685)) ;
#80429 = CARTESIAN_POINT('Ctrl Pts',(-20.6014580999589,13.0765340989596,123.175244208016)) ;
#80430 = CARTESIAN_POINT('Ctrl Pts',(-20.6073128924853,13.0781972778934,123.209996445795)) ;
#80431 = CARTESIAN_POINT('Ctrl Pts',(-20.6131676850117,13.0798604568273,123.244748683574)) ;
#80432 = CARTESIAN_POINT('Ctrl Pts',(-20.617537515338,13.0815267386897,123.279948012451)) ;
#80433 = CARTESIAN_POINT('Ctrl Pts',(-20.6203564173013,13.083186047998,123.31532090111)) ;
#80434 = CARTESIAN_POINT('Ctrl Pts',(-20.6259389565516,13.0864721357949,123.385373191648)) ;
#80435 = CARTESIAN_POINT('Ctrl Pts',(-20.6254307588554,13.089790362517,123.455751084173)) ;
#80436 = CARTESIAN_POINT('Ctrl Pts',(-20.6188518700433,13.0931166999359,123.525661255243)) ;
#80437 = CARTESIAN_POINT('Ctrl Pts',(-20.6129825581758,13.0960842697257,123.588031149073)) ;
#80438 = CARTESIAN_POINT('Ctrl Pts',(-20.6022908582607,13.0990174373957,123.649884042373)) ;
#80439 = CARTESIAN_POINT('Ctrl Pts',(-20.5868916641318,13.1019732940614,123.710584825956)) ;
#80440 = CARTESIAN_POINT('Ctrl Pts',(-20.5849358576223,13.1023487087526,123.718294254558)) ;
#80441 = CARTESIAN_POINT('Ctrl Pts',(-20.5829041831187,13.1027244894353,123.725985111667)) ;
#80442 = CARTESIAN_POINT('Ctrl Pts',(-20.5807969353277,13.1031007530736,123.733656106331)) ;
#80443 = CARTESIAN_POINT('Ctrl Pts',(-20.5653733780598,13.1058547356842,123.789802339353)) ;
#80444 = CARTESIAN_POINT('Ctrl Pts',(-20.5459194132871,13.1086131334078,123.844802121024)) ;
#80445 = CARTESIAN_POINT('Ctrl Pts',(-20.5226186805511,13.1113469816987,123.898146114111)) ;
#80446 = CARTESIAN_POINT('Ctrl Pts',(-20.5175456933214,13.1119421894814,123.909760057706)) ;
#80447 = CARTESIAN_POINT('Ctrl Pts',(-20.5122905486546,13.1125362335941,123.921295583843)) ;
#80448 = CARTESIAN_POINT('Ctrl Pts',(-20.5068554484329,13.1131288151207,123.932747551088)) ;
#80449 = CARTESIAN_POINT('Ctrl Pts',(-20.4816239304041,13.1158797729435,123.985911339469)) ;
#80450 = CARTESIAN_POINT('Ctrl Pts',(-20.4525416222922,13.1186438690752,124.037206847902)) ;
#80451 = CARTESIAN_POINT('Ctrl Pts',(-20.4198836724748,13.1214376143312,124.086151956349)) ;
#80452 = CARTESIAN_POINT('Ctrl Pts',(-20.4134463021852,13.1219883033,124.095799769169)) ;
#80453 = CARTESIAN_POINT('Ctrl Pts',(-20.4068701432227,13.1225401442649,124.105356339859)) ;
#80454 = CARTESIAN_POINT('Ctrl Pts',(-20.4001575102361,13.1230932636784,124.114818094959)) ;
#80455 = CARTESIAN_POINT('Ctrl Pts',(-20.3640599656681,13.1260676930446,124.165699191407)) ;
#80456 = CARTESIAN_POINT('Ctrl Pts',(-20.3240715618893,13.1290113327513,124.213752737903)) ;
#80457 = CARTESIAN_POINT('Ctrl Pts',(-20.280602485974,13.1319272155956,124.258488818542)) ;
#80458 = CARTESIAN_POINT('Ctrl Pts',(-20.2746963362105,13.1323233970283,124.264567116424)) ;
#80459 = CARTESIAN_POINT('Ctrl Pts',(-20.2687259912361,13.1327190660499,124.270584221896)) ;
#80460 = CARTESIAN_POINT('Ctrl Pts',(-20.2626925378787,13.1331142302675,124.276538952679)) ;
#80461 = CARTESIAN_POINT('Ctrl Pts',(-20.2124365464096,13.1364057729999,124.326139220003)) ;
#80462 = CARTESIAN_POINT('Ctrl Pts',(-20.1579262026917,13.139733462171,124.371287158225)) ;
#80463 = CARTESIAN_POINT('Ctrl Pts',(-20.0997951209569,13.1431024819908,124.411443806463)) ;
#80464 = CARTESIAN_POINT('Ctrl Pts',(-20.0695294058607,13.144856548679,124.432351204683)) ;
#80465 = CARTESIAN_POINT('Ctrl Pts',(-20.0383513299908,13.1465967018408,124.451853085651)) ;
#80466 = CARTESIAN_POINT('Ctrl Pts',(-20.0064937701153,13.1483201646471,124.46983612822)) ;
#80467 = CARTESIAN_POINT('Ctrl Pts',(-19.9768591713267,13.1499233674345,124.486564347632)) ;
#80468 = CARTESIAN_POINT('Ctrl Pts',(-19.9466372807795,13.1515121278449,124.501978605502)) ;
#80469 = CARTESIAN_POINT('Ctrl Pts',(-19.9160303243104,13.1530842107175,124.516025442661)) ;
#80470 = CARTESIAN_POINT('Ctrl Pts',(-19.895810249714,13.1541227861468,124.525305296915)) ;
#80471 = CARTESIAN_POINT('Ctrl Pts',(-19.8751876241726,13.1551716918063,124.534092711869)) ;
#80472 = CARTESIAN_POINT('Ctrl Pts',(-19.8544013312711,13.1562211252396,124.542277670704)) ;
#80473 = CARTESIAN_POINT('Ctrl Pts',(-19.8372102335997,13.1570890487667,124.549046959843)) ;
#80474 = CARTESIAN_POINT('Ctrl Pts',(-19.8199077540772,13.1579573332887,124.555404985381)) ;
#80475 = CARTESIAN_POINT('Ctrl Pts',(-19.8026384890018,13.1588204336388,124.561314774439)) ;
#80476 = CARTESIAN_POINT('Ctrl Pts',(-19.7858523723805,13.1596593867193,124.567059223198)) ;
#80477 = CARTESIAN_POINT('Ctrl Pts',(-19.7687146880563,13.1605123080096,124.572508646653)) ;
#80478 = CARTESIAN_POINT('Ctrl Pts',(-19.7515162067081,13.1613635178667,124.577557971888)) ;
#80479 = CARTESIAN_POINT('Ctrl Pts',(-19.7412079405897,13.1618737081301,124.58058438958)) ;
#80480 = CARTESIAN_POINT('Ctrl Pts',(-19.7308781843441,13.1623832835692,124.583468017363)) ;
#80481 = CARTESIAN_POINT('Ctrl Pts',(-19.7205920882092,13.1628888680262,124.586194855273)) ;
#80482 = CARTESIAN_POINT('Ctrl Pts',(-19.6890331133565,13.1644400616915,124.594561120559)) ;
#80483 = CARTESIAN_POINT('Ctrl Pts',(-19.6568234814033,13.1659985862561,124.60173391568)) ;
#80484 = CARTESIAN_POINT('Ctrl Pts',(-19.6241856364059,13.1675616636008,124.607599940749)) ;
#80485 = CARTESIAN_POINT('Ctrl Pts',(-19.5916847617139,13.1691181812238,124.613441348039)) ;
#80486 = CARTESIAN_POINT('Ctrl Pts',(-19.5587598541828,13.1706792134942,124.617986708264)) ;
#80487 = CARTESIAN_POINT('Ctrl Pts',(-19.5256469814756,13.1722420171226,124.621173231058)) ;
#80488 = CARTESIAN_POINT('Ctrl Pts',(-19.5216231627236,13.1724319263039,124.621560451771)) ;
#80489 = CARTESIAN_POINT('Ctrl Pts',(-19.5175965817914,13.1726218616423,124.621927668767)) ;
#80490 = CARTESIAN_POINT('Ctrl Pts',(-19.5135676720988,13.1728118182152,124.622274821002)) ;
#80491 = CARTESIAN_POINT('Ctrl Pts',(-19.4431860182137,13.1761301993118,124.628339277721)) ;
#80492 = CARTESIAN_POINT('Ctrl Pts',(-19.3724202623327,13.1794637724057,124.628252168937)) ;
#80493 = CARTESIAN_POINT('Ctrl Pts',(-19.3020841165369,13.1827969618019,124.622022549267)) ;
#80494 = CARTESIAN_POINT('Ctrl Pts',(-19.2381208971503,13.1858281418898,124.616357374909)) ;
#80495 = CARTESIAN_POINT('Ctrl Pts',(-19.1746816194266,13.1888539155085,124.605623438599)) ;
#80496 = CARTESIAN_POINT('Ctrl Pts',(-19.1124419072866,13.1918776184193,124.58994196653)) ;
#80497 = CARTESIAN_POINT('Ctrl Pts',(-19.1062917947322,13.1921764005407,124.588392428222)) ;
#80498 = CARTESIAN_POINT('Ctrl Pts',(-19.1001533868472,13.1924751624437,124.586794622992)) ;
#80499 = CARTESIAN_POINT('Ctrl Pts',(-19.0940273309136,13.1927739073465,124.585148695047)) ;
#80500 = CARTESIAN_POINT('Ctrl Pts',(-19.0376030709326,13.1955255080902,124.569988816119)) ;
#80501 = CARTESIAN_POINT('Ctrl Pts',(-18.982310761406,13.1982673320755,124.550764643093)) ;
#80502 = CARTESIAN_POINT('Ctrl Pts',(-18.9286648343349,13.2010292632919,124.527658425169)) ;
#80503 = CARTESIAN_POINT('Ctrl Pts',(-18.9172881129165,13.2016149875722,124.522758276757)) ;
#80504 = CARTESIAN_POINT('Ctrl Pts',(-18.9059853714614,13.2022016161536,124.517683712586)) ;
#80505 = CARTESIAN_POINT('Ctrl Pts',(-18.8947614126757,13.2027894340587,124.512436753774)) ;
#80506 = CARTESIAN_POINT('Ctrl Pts',(-18.8425149448965,13.205525670874,124.488012656203)) ;
#80507 = CARTESIAN_POINT('Ctrl Pts',(-18.7920410632873,13.2082605174372,124.459879143387)) ;
#80508 = CARTESIAN_POINT('Ctrl Pts',(-18.7438008678464,13.2109629922146,124.428296743651)) ;
#80509 = CARTESIAN_POINT('Ctrl Pts',(-18.73273725433,13.2115827893817,124.421053500513)) ;
#80510 = CARTESIAN_POINT('Ctrl Pts',(-18.721791021334,13.2122008838315,124.413629037106)) ;
#80511 = CARTESIAN_POINT('Ctrl Pts',(-18.7109675360248,13.2128169018266,124.406026829864)) ;
#80512 = CARTESIAN_POINT('Ctrl Pts',(-18.6588979399802,13.2157804396561,124.369454150288)) ;
#80513 = CARTESIAN_POINT('Ctrl Pts',(-18.6097447256124,13.2187668771422,124.328815918986)) ;
#80514 = CARTESIAN_POINT('Ctrl Pts',(-18.5640274925586,13.2218051835985,124.284537275842)) ;
#80515 = CARTESIAN_POINT('Ctrl Pts',(-18.559277135695,13.2221208859926,124.279936399054)) ;
#80516 = CARTESIAN_POINT('Ctrl Pts',(-18.5545638479963,13.2224371484024,124.275296254488)) ;
#80517 = CARTESIAN_POINT('Ctrl Pts',(-18.5498881932309,13.2227540033275,124.270617345238)) ;
#80518 = CARTESIAN_POINT('Ctrl Pts',(-18.4997504569173,13.2261516854667,124.2204447106)) ;
#80519 = CARTESIAN_POINT('Ctrl Pts',(-18.4540891529611,13.2294902857806,124.165960527441)) ;
#80520 = CARTESIAN_POINT('Ctrl Pts',(-18.4134553008324,13.2327808911029,124.107821945015)) ;
#80521 = CARTESIAN_POINT('Ctrl Pts',(-18.3918974899517,13.2345266829367,124.076977205982)) ;
#80522 = CARTESIAN_POINT('Ctrl Pts',(-18.3718010491922,13.2362874613736,124.045163734806)) ;
#80523 = CARTESIAN_POINT('Ctrl Pts',(-18.3532841579246,13.2380562906017,124.012616943459)) ;
#80524 = CARTESIAN_POINT('Ctrl Pts',(-18.337148907225,13.2395976132042,123.984256316923)) ;
#80525 = CARTESIAN_POINT('Ctrl Pts',(-18.3222124155681,13.2411450487989,123.955339566188)) ;
#80526 = CARTESIAN_POINT('Ctrl Pts',(-18.3085229193702,13.2426940083626,123.926034544882)) ;
#80527 = CARTESIAN_POINT('Ctrl Pts',(-18.298944521022,13.2437777992861,123.905530125755)) ;
#80528 = CARTESIAN_POINT('Ctrl Pts',(-18.2898869625498,13.2448654054133,123.884636235243)) ;
#80529 = CARTESIAN_POINT('Ctrl Pts',(-18.2814571063029,13.2459424605924,123.863591097685)) ;
#80530 = CARTESIAN_POINT('Ctrl Pts',(-18.2737001243048,13.2469335448281,123.844225790803)) ;
#80531 = CARTESIAN_POINT('Ctrl Pts',(-18.2664741872634,13.2479156952537,123.824732962847)) ;
#80532 = CARTESIAN_POINT('Ctrl Pts',(-18.259825879779,13.2488777185653,123.80531165987)) ;
#80533 = CARTESIAN_POINT('Origin',(-19.4092696390626,-30.19753203383,123.411833654984)) ;
#80534 = CARTESIAN_POINT('',(-18.259825879779,12.510900730771,123.80531165987)) ;
#80535 = CARTESIAN_POINT('',(-18.259825879779,12.5288903030032,123.80531165987)) ;
#80536 = CARTESIAN_POINT('',(-18.259825879779,-30.19753203383,123.80531165987)) ;
#80537 = CARTESIAN_POINT('Ctrl Pts',(-18.259825879779,12.870840300276,123.80531165987)) ;
#80538 = CARTESIAN_POINT('Ctrl Pts',(-18.2652438286331,12.8700544476548,123.821138789776)) ;
#80539 = CARTESIAN_POINT('Ctrl Pts',(-18.2710476408713,12.8692618062305,123.837012818616)) ;
#80540 = CARTESIAN_POINT('Ctrl Pts',(-18.2771267299168,12.8684744374755,123.852626496755)) ;
#80541 = CARTESIAN_POINT('Ctrl Pts',(-18.2797352125343,12.8681365846007,123.859326186085)) ;
#80542 = CARTESIAN_POINT('Ctrl Pts',(-18.282393759643,12.867799702525,123.865978162539)) ;
#80543 = CARTESIAN_POINT('Ctrl Pts',(-18.285090905704,12.8674647441515,123.872559247446)) ;
#80544 = CARTESIAN_POINT('Ctrl Pts',(-18.2970887061201,12.865974738189,123.901834096284)) ;
#80545 = CARTESIAN_POINT('Ctrl Pts',(-18.3103663206228,12.8644630347073,123.930961610968)) ;
#80546 = CARTESIAN_POINT('Ctrl Pts',(-18.3248839005837,12.862942247799,123.959696289473)) ;
#80547 = CARTESIAN_POINT('Ctrl Pts',(-18.3393287989552,12.8614290746398,123.988287109145)) ;
#80548 = CARTESIAN_POINT('Ctrl Pts',(-18.3550011089457,12.8599069087778,124.016488416133)) ;
#80549 = CARTESIAN_POINT('Ctrl Pts',(-18.3718124892914,12.858388175797,124.044074557231)) ;
#80550 = CARTESIAN_POINT('Ctrl Pts',(-18.3749875471227,12.8581013424172,124.049284575179)) ;
#80551 = CARTESIAN_POINT('Ctrl Pts',(-18.3782030986378,12.8578146314863,124.0544727119)) ;
#80552 = CARTESIAN_POINT('Ctrl Pts',(-18.3814583607703,12.8575281267115,124.059637539119)) ;
#80553 = CARTESIAN_POINT('Ctrl Pts',(-18.4190899396721,12.8542160656237,124.11934412959)) ;
#80554 = CARTESIAN_POINT('Ctrl Pts',(-18.4618403115692,12.8509002845194,124.175638483707)) ;
#80555 = CARTESIAN_POINT('Ctrl Pts',(-18.5092135497178,12.8475541933109,124.227888145884)) ;
#80556 = CARTESIAN_POINT('Ctrl Pts',(-18.5523033632248,12.8445106511806,124.275413463701)) ;
#80557 = CARTESIAN_POINT('Ctrl Pts',(-18.5991145856276,12.8414987770607,124.319472287255)) ;
#80558 = CARTESIAN_POINT('Ctrl Pts',(-18.6491457361005,12.8384804507046,124.359598155391)) ;
#80559 = CARTESIAN_POINT('Ctrl Pts',(-18.6544581856012,12.8381599562488,124.363858833911)) ;
#80560 = CARTESIAN_POINT('Ctrl Pts',(-18.6598069062294,12.8378393890454,124.368075204618)) ;
#80561 = CARTESIAN_POINT('Ctrl Pts',(-18.6651912734813,12.8375187034571,124.372246733799)) ;
#80562 = CARTESIAN_POINT('Ctrl Pts',(-18.7120795895278,12.8347260991437,124.40857337526)) ;
#80563 = CARTESIAN_POINT('Ctrl Pts',(-18.7615941697354,12.8319149846304,124.44143451251)) ;
#80564 = CARTESIAN_POINT('Ctrl Pts',(-18.8132612855669,12.8291247582724,124.470521493135)) ;
#80565 = CARTESIAN_POINT('Ctrl Pts',(-18.823061917314,12.8285954858215,124.476038944248)) ;
#80566 = CARTESIAN_POINT('Ctrl Pts',(-18.8329399204803,12.8280669649586,124.481420722888)) ;
#80567 = CARTESIAN_POINT('Ctrl Pts',(-18.8428919483362,12.8275394645878,124.486664901056)) ;
#80568 = CARTESIAN_POINT('Ctrl Pts',(-18.8949996559076,12.824777531496,124.514122832886)) ;
#80569 = CARTESIAN_POINT('Ctrl Pts',(-18.9490737869791,12.8220158289773,124.53777063425)) ;
#80570 = CARTESIAN_POINT('Ctrl Pts',(-19.0046041253018,12.8192219391128,124.557386673425)) ;
#80571 = CARTESIAN_POINT('Ctrl Pts',(-19.0152882478231,12.8186843904047,124.561160829539)) ;
#80572 = CARTESIAN_POINT('Ctrl Pts',(-19.0260262156451,12.8181456501742,124.564785878634)) ;
#80573 = CARTESIAN_POINT('Ctrl Pts',(-19.0368143068355,12.8176054875281,124.568260445395)) ;
#80574 = CARTESIAN_POINT('Ctrl Pts',(-19.0954403516193,12.8146700655968,124.587142386879)) ;
#80575 = CARTESIAN_POINT('Ctrl Pts',(-19.1554537398915,12.8117625018629,124.601546016932)) ;
#80576 = CARTESIAN_POINT('Ctrl Pts',(-19.2162518026066,12.8088828516118,124.611329386905)) ;
#80577 = CARTESIAN_POINT('Ctrl Pts',(-19.2254481721147,12.8084472731315,124.612809228223)) ;
#80578 = CARTESIAN_POINT('Ctrl Pts',(-19.2346624728816,12.8080123333077,124.614183453138)) ;
#80579 = CARTESIAN_POINT('Ctrl Pts',(-19.243892594155,12.8075780323319,124.61545167126)) ;
#80580 = CARTESIAN_POINT('Ctrl Pts',(-19.3137968124457,12.8042888588397,124.625056506757)) ;
#80581 = CARTESIAN_POINT('Ctrl Pts',(-19.3844454421074,12.8009600868674,124.62855644456)) ;
#80582 = CARTESIAN_POINT('Ctrl Pts',(-19.4549977610507,12.7975966410503,124.625899071238)) ;
#80583 = CARTESIAN_POINT('Ctrl Pts',(-19.4946799715306,12.7957048681525,124.624404429403)) ;
#80584 = CARTESIAN_POINT('Ctrl Pts',(-19.5342351639706,12.7938301259445,124.620961938844)) ;
#80585 = CARTESIAN_POINT('Ctrl Pts',(-19.5733911893916,12.7919703264446,124.615623509071)) ;
#80586 = CARTESIAN_POINT('Ctrl Pts',(-19.6041976335048,12.7905071082365,124.611423439308)) ;
#80587 = CARTESIAN_POINT('Ctrl Pts',(-19.6347569943669,12.7890531394645,124.606050872099)) ;
#80588 = CARTESIAN_POINT('Ctrl Pts',(-19.6649429132893,12.7876074032817,124.599552928605)) ;
#80589 = CARTESIAN_POINT('Ctrl Pts',(-19.6888698339983,12.7864614380023,124.594402322485)) ;
#80590 = CARTESIAN_POINT('Ctrl Pts',(-19.712749770549,12.7853054287652,124.588500829333)) ;
#80591 = CARTESIAN_POINT('Ctrl Pts',(-19.7363390471498,12.7841509014001,124.581906942594)) ;
#80592 = CARTESIAN_POINT('Ctrl Pts',(-19.7588770859414,12.7830478246512,124.575606907302)) ;
#80593 = CARTESIAN_POINT('Ctrl Pts',(-19.7811494990811,12.7819461006402,124.568675322403)) ;
#80594 = CARTESIAN_POINT('Ctrl Pts',(-19.8029573224534,12.7808557819277,124.561205615679)) ;
#80595 = CARTESIAN_POINT('Ctrl Pts',(-19.817043721936,12.7801515087554,124.556380683308)) ;
#80596 = CARTESIAN_POINT('Ctrl Pts',(-19.8312706523649,12.7794353947332,124.551213688254)) ;
#80597 = CARTESIAN_POINT('Ctrl Pts',(-19.8452968087345,12.7787251458483,124.545820517074)) ;
#80598 = CARTESIAN_POINT('Ctrl Pts',(-19.8514774803503,12.7784121723573,124.543443998579)) ;
#80599 = CARTESIAN_POINT('Ctrl Pts',(-19.8576193910325,12.7781003377312,124.541024208478)) ;
#80600 = CARTESIAN_POINT('Ctrl Pts',(-19.863694495186,12.7777911569645,124.53857406263)) ;
#80601 = CARTESIAN_POINT('Ctrl Pts',(-19.8925245790538,12.7763239051763,124.526946622428)) ;
#80602 = CARTESIAN_POINT('Ctrl Pts',(-19.9212388608835,12.7748458991295,124.514074790318)) ;
#80603 = CARTESIAN_POINT('Ctrl Pts',(-19.9495920023153,12.773356568108,124.499996161163)) ;
#80604 = CARTESIAN_POINT('Ctrl Pts',(-19.9777932858638,12.7718752138624,124.485992936381)) ;
#80605 = CARTESIAN_POINT('Ctrl Pts',(-20.0056366915137,12.7703826556292,124.470795969259)) ;
#80606 = CARTESIAN_POINT('Ctrl Pts',(-20.0328967183668,12.7688783318134,124.45449139463)) ;
#80607 = CARTESIAN_POINT('Ctrl Pts',(-20.0388064558109,12.7685522074544,124.450956704231)) ;
#80608 = CARTESIAN_POINT('Ctrl Pts',(-20.0446888539843,12.768225530131,124.447370136059)) ;
#80609 = CARTESIAN_POINT('Ctrl Pts',(-20.0505417560582,12.767898294121,124.443732859388)) ;
#80610 = CARTESIAN_POINT('Ctrl Pts',(-20.110801109042,12.7645291910702,124.406284780456)) ;
#80611 = CARTESIAN_POINT('Ctrl Pts',(-20.1676603652674,12.7611694127812,124.363632839701)) ;
#80612 = CARTESIAN_POINT('Ctrl Pts',(-20.2204695563796,12.7578667843255,124.31626750565)) ;
#80613 = CARTESIAN_POINT('Ctrl Pts',(-20.2727611706988,12.7545965245506,124.269366393777)) ;
#80614 = CARTESIAN_POINT('Ctrl Pts',(-20.3209020836178,12.7512924797053,124.217997962919)) ;
#80615 = CARTESIAN_POINT('Ctrl Pts',(-20.3642974923925,12.7479375921959,124.162811481188)) ;
#80616 = CARTESIAN_POINT('Ctrl Pts',(-20.4002454991736,12.7451584613536,124.117095953312)) ;
#80617 = CARTESIAN_POINT('Ctrl Pts',(-20.4328852777677,12.742418077025,124.068825008237)) ;
#80618 = CARTESIAN_POINT('Ctrl Pts',(-20.461916599482,12.7396961292568,124.018447430631)) ;
#80619 = CARTESIAN_POINT('Ctrl Pts',(-20.4682779426553,12.7390996960657,124.007408695897)) ;
#80620 = CARTESIAN_POINT('Ctrl Pts',(-20.4744661969473,12.7385041480797,123.996268922871)) ;
#80621 = CARTESIAN_POINT('Ctrl Pts',(-20.4804784836014,12.7379092716233,123.985033015998)) ;
#80622 = CARTESIAN_POINT('Ctrl Pts',(-20.5079240155246,12.7351937156767,123.933742141411)) ;
#80623 = CARTESIAN_POINT('Ctrl Pts',(-20.5316651272719,12.7324521685231,123.88050941552)) ;
#80624 = CARTESIAN_POINT('Ctrl Pts',(-20.5514839489327,12.7296938003856,123.825829266571)) ;
#80625 = CARTESIAN_POINT('Ctrl Pts',(-20.5557379593736,12.7291017305311,123.814092447474)) ;
#80626 = CARTESIAN_POINT('Ctrl Pts',(-20.559811435531,12.7285088856924,123.802289017377)) ;
#80627 = CARTESIAN_POINT('Ctrl Pts',(-20.5637025105913,12.7279153565559,123.790423989276)) ;
#80628 = CARTESIAN_POINT('Ctrl Pts',(-20.5826652147322,12.7250228609757,123.732601147511)) ;
#80629 = CARTESIAN_POINT('Ctrl Pts',(-20.5972647474954,12.7221506683593,123.673397226161)) ;
#80630 = CARTESIAN_POINT('Ctrl Pts',(-20.6073590837758,12.7192993883011,123.61339649519)) ;
#80631 = CARTESIAN_POINT('Ctrl Pts',(-20.6089743525134,12.7188431340797,123.603795338435)) ;
#80632 = CARTESIAN_POINT('Ctrl Pts',(-20.610474368506,12.7183874153358,123.594173804297)) ;
#80633 = CARTESIAN_POINT('Ctrl Pts',(-20.6118586700221,12.717932234567,123.584534317116)) ;
#80634 = CARTESIAN_POINT('Ctrl Pts',(-20.6218395159693,12.7146503706968,123.515033391598)) ;
#80635 = CARTESIAN_POINT('Ctrl Pts',(-20.6257805720531,12.7113409674474,123.444756157452)) ;
#80636 = CARTESIAN_POINT('Ctrl Pts',(-20.6236229978934,12.7079998035975,123.374526604962)) ;
#80637 = CARTESIAN_POINT('Ctrl Pts',(-20.6223527583993,12.7060327433881,123.333180007059)) ;
#80638 = CARTESIAN_POINT('Ctrl Pts',(-20.6189683608956,12.7040831719724,123.291957810843)) ;
#80639 = CARTESIAN_POINT('Ctrl Pts',(-20.6135225780402,12.7021457426414,123.251145276285)) ;
#80640 = CARTESIAN_POINT('Ctrl Pts',(-20.6096329606307,12.7007619454802,123.221995170753)) ;
#80641 = CARTESIAN_POINT('Ctrl Pts',(-20.6046928480253,12.6993843425356,123.193053959686)) ;
#80642 = CARTESIAN_POINT('Ctrl Pts',(-20.5987371476557,12.6980109856402,123.164421161188)) ;
#80643 = CARTESIAN_POINT('Ctrl Pts',(-20.5935681866693,12.6968190471993,123.139570713856)) ;
#80644 = CARTESIAN_POINT('Ctrl Pts',(-20.5875972158044,12.6956183571829,123.114792440979)) ;
#80645 = CARTESIAN_POINT('Ctrl Pts',(-20.5808845007879,12.6944212672785,123.090330137322)) ;
#80646 = CARTESIAN_POINT('Ctrl Pts',(-20.5741717857715,12.6932241773741,123.065867833665)) ;
#80647 = CARTESIAN_POINT('Ctrl Pts',(-20.5667175537136,12.6920306875816,123.041721989206)) ;
#80648 = CARTESIAN_POINT('Ctrl Pts',(-20.5586326678525,12.6908531495887,123.018119895845)) ;
#80649 = CARTESIAN_POINT('Ctrl Pts',(-20.5541414064836,12.6901990116096,123.005008619822)) ;
#80650 = CARTESIAN_POINT('Ctrl Pts',(-20.5493406381397,12.6895333106017,122.991738989093)) ;
#80651 = CARTESIAN_POINT('Ctrl Pts',(-20.5443553865511,12.6888739164767,122.978675205992)) ;
#80652 = CARTESIAN_POINT('Ctrl Pts',(-20.5424583250474,12.6886229940933,122.973703982459)) ;
#80653 = CARTESIAN_POINT('Ctrl Pts',(-20.5405350594797,12.6883729849888,122.968762386795)) ;
#80654 = CARTESIAN_POINT('Ctrl Pts',(-20.5385943316674,12.6881248738665,122.963869778362)) ;
#80655 = CARTESIAN_POINT('Ctrl Pts',(-20.5272753794957,12.68667780957,122.93533450387)) ;
#80656 = CARTESIAN_POINT('Ctrl Pts',(-20.5147339491118,12.6852153862968,122.906884421184)) ;
#80657 = CARTESIAN_POINT('Ctrl Pts',(-20.5010042023758,12.6837414307202,122.878765611155)) ;
#80658 = CARTESIAN_POINT('Ctrl Pts',(-20.4873540842985,12.6822760236703,122.850809882293)) ;
#80659 = CARTESIAN_POINT('Ctrl Pts',(-20.4725295461049,12.6807992176972,122.823182188348)) ;
#80660 = CARTESIAN_POINT('Ctrl Pts',(-20.4566134182114,12.6793147732787,122.796108956468)) ;
#80661 = CARTESIAN_POINT('Ctrl Pts',(-20.4526682092607,12.6789468167352,122.789398181243)) ;
#80662 = CARTESIAN_POINT('Ctrl Pts',(-20.448656161394,12.6785783908704,122.78272137491)) ;
#80663 = CARTESIAN_POINT('Ctrl Pts',(-20.444578985311,12.6782095529563,122.776081774408)) ;
#80664 = CARTESIAN_POINT('Ctrl Pts',(-20.4075827945685,12.6748627272253,122.715834210506)) ;
#80665 = CARTESIAN_POINT('Ctrl Pts',(-20.3654101310523,12.6715220564939,122.658949047217)) ;
#80666 = CARTESIAN_POINT('Ctrl Pts',(-20.3185410461941,12.6682155379078,122.606059862746)) ;
#80667 = CARTESIAN_POINT('Ctrl Pts',(-20.2747485812569,12.6651260685979,122.556642474642)) ;
#80668 = CARTESIAN_POINT('Ctrl Pts',(-20.2269818742819,12.6620310002448,122.510863018777)) ;
#80669 = CARTESIAN_POINT('Ctrl Pts',(-20.1757783500652,12.6588878040927,122.469225416084)) ;
#80670 = CARTESIAN_POINT('Ctrl Pts',(-20.1723499810233,12.6586773491183,122.466437540245)) ;
#80671 = CARTESIAN_POINT('Ctrl Pts',(-20.1689062175314,12.6584666783836,122.463668218323)) ;
#80672 = CARTESIAN_POINT('Ctrl Pts',(-20.1654472267241,12.6582557791229,122.460917595596)) ;
#80673 = CARTESIAN_POINT('Ctrl Pts',(-20.1196759772228,12.6554650452884,122.424519858182)) ;
#80674 = CARTESIAN_POINT('Ctrl Pts',(-20.0713044553254,12.6526971472822,122.391454374463)) ;
#80675 = CARTESIAN_POINT('Ctrl Pts',(-20.0207859716826,12.6499642441057,122.362027162804)) ;
#80676 = CARTESIAN_POINT('Ctrl Pts',(-20.0100535520215,12.6493836513866,122.355775486938)) ;
#80677 = CARTESIAN_POINT('Ctrl Pts',(-19.9992243363149,12.6488046380909,122.349687861134)) ;
#80678 = CARTESIAN_POINT('Ctrl Pts',(-19.9883028378967,12.6482273208029,122.343766966648)) ;
#80679 = CARTESIAN_POINT('Ctrl Pts',(-19.9365861933381,12.6454935463847,122.315729715362)) ;
#80680 = CARTESIAN_POINT('Ctrl Pts',(-19.8828637603558,12.6427273694508,122.291470213793)) ;
#80681 = CARTESIAN_POINT('Ctrl Pts',(-19.8276417803091,12.6399265123786,122.271215117736)) ;
#80682 = CARTESIAN_POINT('Ctrl Pts',(-19.8168671346936,12.6393800226956,122.267263041376)) ;
#80683 = CARTESIAN_POINT('Ctrl Pts',(-19.8060354655735,12.6388322127423,122.26346326699)) ;
#80684 = CARTESIAN_POINT('Ctrl Pts',(-19.7951506272147,12.6382830656004,122.259817266617)) ;
#80685 = CARTESIAN_POINT('Ctrl Pts',(-19.7373273714089,12.6353658449111,122.240448709612)) ;
#80686 = CARTESIAN_POINT('Ctrl Pts',(-19.6780916519949,12.6324929751349,122.225453540607)) ;
#80687 = CARTESIAN_POINT('Ctrl Pts',(-19.6180299855097,12.629644765805,122.214977350395)) ;
#80688 = CARTESIAN_POINT('Ctrl Pts',(-19.6082535311584,12.6291811524867,122.213272103082)) ;
#80689 = CARTESIAN_POINT('Ctrl Pts',(-19.5984552195503,12.6287181925532,122.21168647846)) ;
#80690 = CARTESIAN_POINT('Ctrl Pts',(-19.5886376125502,12.6282558010846,122.210220977716)) ;
#80691 = CARTESIAN_POINT('Ctrl Pts',(-19.5189112904046,12.6249718178806,122.19981274107)) ;
#80692 = CARTESIAN_POINT('Ctrl Pts',(-19.4483672292415,12.6216433959297,122.195489850219)) ;
#80693 = CARTESIAN_POINT('Ctrl Pts',(-19.3778572930884,12.6182833583503,122.197313519044)) ;
#80694 = CARTESIAN_POINT('Ctrl Pts',(-19.3352166590783,12.6162513875317,122.198416376303)) ;
#80695 = CARTESIAN_POINT('Ctrl Pts',(-19.292692077002,12.614235820897,122.201767656007)) ;
#80696 = CARTESIAN_POINT('Ctrl Pts',(-19.2505806312853,12.612237690103,122.207315620709)) ;
#80697 = CARTESIAN_POINT('Ctrl Pts',(-19.2229315759349,12.6109257800514,122.210958240441)) ;
#80698 = CARTESIAN_POINT('Ctrl Pts',(-19.1954604882387,12.6096213862839,122.215546738106)) ;
#80699 = CARTESIAN_POINT('Ctrl Pts',(-19.1682482299057,12.6083248007956,122.221054676159)) ;
#80700 = CARTESIAN_POINT('Ctrl Pts',(-19.1422661761438,12.6070868310008,122.226313612806)) ;
#80701 = CARTESIAN_POINT('Ctrl Pts',(-19.1163797759702,12.6058411342532,122.232443360207)) ;
#80702 = CARTESIAN_POINT('Ctrl Pts',(-19.0908463574102,12.6045965813391,122.239377894716)) ;
#80703 = CARTESIAN_POINT('Ctrl Pts',(-19.0653129388503,12.603352028425,122.246312429225)) ;
#80704 = CARTESIAN_POINT('Ctrl Pts',(-19.0401330527927,12.6021086193443,122.254051484177)) ;
#80705 = CARTESIAN_POINT('Ctrl Pts',(-19.015545705886,12.6008752248834,122.262474111356)) ;
#80706 = CARTESIAN_POINT('Ctrl Pts',(-19.0036139187657,12.6002766812423,122.266561457375)) ;
#80707 = CARTESIAN_POINT('Ctrl Pts',(-18.9915061483425,12.5996650936151,122.270921283469)) ;
#80708 = CARTESIAN_POINT('Ctrl Pts',(-18.9796199090638,12.5990611136394,122.275415155664)) ;
#80709 = CARTESIAN_POINT('Ctrl Pts',(-18.9761299444542,12.5988837767466,122.276734618831)) ;
#80710 = CARTESIAN_POINT('Ctrl Pts',(-18.9726589616602,12.5987070957027,122.278065314125)) ;
#80711 = CARTESIAN_POINT('Ctrl Pts',(-18.9692167198068,12.5985315932456,122.279402939956)) ;
#80712 = CARTESIAN_POINT('Ctrl Pts',(-18.9410916850274,12.5970976403397,122.29033208864)) ;
#80713 = CARTESIAN_POINT('Ctrl Pts',(-18.9130159442305,12.5956536956959,122.302452626089)) ;
#80714 = CARTESIAN_POINT('Ctrl Pts',(-18.8852362505225,12.5942025436577,122.31573379467)) ;
#80715 = CARTESIAN_POINT('Ctrl Pts',(-18.8576318509199,12.5927605486102,122.328931157051)) ;
#80716 = CARTESIAN_POINT('Ctrl Pts',(-18.8303203638607,12.591311436841,122.343274407333)) ;
#80717 = CARTESIAN_POINT('Ctrl Pts',(-18.8035290017548,12.5898579403164,122.358684009208)) ;
#80718 = CARTESIAN_POINT('Ctrl Pts',(-18.7958378539878,12.5894406768527,122.363107730726)) ;
#80719 = CARTESIAN_POINT('Ctrl Pts',(-18.78818944604,12.5890230520307,122.367619028999)) ;
#80720 = CARTESIAN_POINT('Ctrl Pts',(-18.7805888210449,12.5886051304848,122.372215299461)) ;
#80721 = CARTESIAN_POINT('Ctrl Pts',(-18.7198680009331,12.5852663867599,122.408934557692)) ;
#80722 = CARTESIAN_POINT('Ctrl Pts',(-18.6624972427602,12.5819070867189,122.450892105939)) ;
#80723 = CARTESIAN_POINT('Ctrl Pts',(-18.6091191273835,12.5785748167538,122.497609910628)) ;
#80724 = CARTESIAN_POINT('Ctrl Pts',(-18.5777387961616,12.576615816619,122.525074727899)) ;
#80725 = CARTESIAN_POINT('Ctrl Pts',(-18.5478029560891,12.5746631140264,122.554134352609)) ;
#80726 = CARTESIAN_POINT('Ctrl Pts',(-18.5195056024907,12.5727088655747,122.584569576646)) ;
#80727 = CARTESIAN_POINT('Ctrl Pts',(-18.4999106558522,12.5713556155616,122.605644925225)) ;
#80728 = CARTESIAN_POINT('Ctrl Pts',(-18.481100615183,12.5700016242955,122.627379084785)) ;
#80729 = CARTESIAN_POINT('Ctrl Pts',(-18.4631281010885,12.5686442874272,122.649690567234)) ;
#80730 = CARTESIAN_POINT('Ctrl Pts',(-18.4363506617847,12.5666219768359,122.682932681495)) ;
#80731 = CARTESIAN_POINT('Ctrl Pts',(-18.4112434404779,12.5645976075795,122.717694317056)) ;
#80732 = CARTESIAN_POINT('Ctrl Pts',(-18.3880097318216,12.5625726742712,122.753749999248)) ;
#80733 = CARTESIAN_POINT('Ctrl Pts',(-18.3647956860237,12.5605494546788,122.789775167252)) ;
#80734 = CARTESIAN_POINT('Ctrl Pts',(-18.3434523867715,12.5585256719889,122.82709168502)) ;
#80735 = CARTESIAN_POINT('Ctrl Pts',(-18.3241416998298,12.5565028170232,122.865442539042)) ;
#80736 = CARTESIAN_POINT('Ctrl Pts',(-18.3048298827935,12.5544798436765,122.903795637421)) ;
#80737 = CARTESIAN_POINT('Ctrl Pts',(-18.2875512170765,12.5524577981627,122.943182616963)) ;
#80738 = CARTESIAN_POINT('Ctrl Pts',(-18.2724213519401,12.5504381715651,122.983322432084)) ;
#80739 = CARTESIAN_POINT('Ctrl Pts',(-18.2678973567496,12.5498342811186,122.995324675919)) ;
#80740 = CARTESIAN_POINT('Ctrl Pts',(-18.2635651510703,12.5492306069413,123.007394098955)) ;
#80741 = CARTESIAN_POINT('Ctrl Pts',(-18.2594269703917,12.5486271888959,123.019522893739)) ;
#80742 = CARTESIAN_POINT('Ctrl Pts',(-18.2435244538054,12.5463083279707,123.06613235215)) ;
#80743 = CARTESIAN_POINT('Ctrl Pts',(-18.2304408727889,12.543969043762,123.113766337352)) ;
#80744 = CARTESIAN_POINT('Ctrl Pts',(-18.2202951051978,12.5416357742674,123.162062852235)) ;
#80745 = CARTESIAN_POINT('Ctrl Pts',(-18.215944345221,12.5406352097028,123.182773610892)) ;
#80746 = CARTESIAN_POINT('Ctrl Pts',(-18.2121332123063,12.5396357511898,123.203605972904)) ;
#80747 = CARTESIAN_POINT('Ctrl Pts',(-18.2088682788955,12.5386394835517,123.224530503399)) ;
#80748 = CARTESIAN_POINT('Ctrl Pts',(-18.1979762759186,12.5353158782233,123.29433592353)) ;
#80749 = CARTESIAN_POINT('Ctrl Pts',(-18.1931905831683,12.532009642944,123.364997383629)) ;
#80750 = CARTESIAN_POINT('Ctrl Pts',(-18.1945771249853,12.5286466831811,123.435666244636)) ;
#80751 = CARTESIAN_POINT('Ctrl Pts',(-18.1954453231439,12.5265409295443,123.479916316467)) ;
#80752 = CARTESIAN_POINT('Ctrl Pts',(-18.1987345660899,12.524445018058,123.524055666228)) ;
#80753 = CARTESIAN_POINT('Ctrl Pts',(-18.2043922934707,12.5223708167657,123.567771072445)) ;
#80754 = CARTESIAN_POINT('Ctrl Pts',(-18.2078100782309,12.5211178094909,123.594179175752)) ;
#80755 = CARTESIAN_POINT('Ctrl Pts',(-18.2120911794677,12.5198727248409,123.620432721153)) ;
#80756 = CARTESIAN_POINT('Ctrl Pts',(-18.217215114198,12.5186381791136,123.64646508049)) ;
#80757 = CARTESIAN_POINT('Ctrl Pts',(-18.2221197203024,12.5174564777787,123.671383131799)) ;
#80758 = CARTESIAN_POINT('Ctrl Pts',(-18.2278209212937,12.5162682169221,123.69620254406)) ;
#80759 = CARTESIAN_POINT('Ctrl Pts',(-18.2342563280413,12.5150802068191,123.720685747429)) ;
#80760 = CARTESIAN_POINT('Ctrl Pts',(-18.2407347997116,12.5138842467038,123.745332789279)) ;
#80761 = CARTESIAN_POINT('Ctrl Pts',(-18.2479571476,12.5126885407095,123.769638609505)) ;
#80762 = CARTESIAN_POINT('Ctrl Pts',(-18.2558095264191,12.511500036749,123.793377446213)) ;
#80763 = CARTESIAN_POINT('Ctrl Pts',(-18.2571308068481,12.5113000531442,123.797371861291)) ;
#80764 = CARTESIAN_POINT('Ctrl Pts',(-18.2584698156533,12.5111002734513,123.801350270854)) ;
#80765 = CARTESIAN_POINT('Ctrl Pts',(-18.259825879779,12.510900730771,123.80531165987)) ;
#80766 = CARTESIAN_POINT('Ctrl Pts',(-18.259825879779,12.5288903030032,123.80531165987)) ;
#80767 = CARTESIAN_POINT('Ctrl Pts',(-18.2524098048089,12.5299743464015,123.783647523662)) ;
#80768 = CARTESIAN_POINT('Ctrl Pts',(-18.2455076163158,12.5310699985716,123.761472531738)) ;
#80769 = CARTESIAN_POINT('Ctrl Pts',(-18.2392292933661,12.5321671007081,123.739020888121)) ;
#80770 = CARTESIAN_POINT('Ctrl Pts',(-18.2331128960579,12.5332359072362,123.717148299901)) ;
#80771 = CARTESIAN_POINT('Ctrl Pts',(-18.227588592158,12.5343060899024,123.695013616499)) ;
#80772 = CARTESIAN_POINT('Ctrl Pts',(-18.2227126740053,12.5353682558269,123.672847954897)) ;
#80773 = CARTESIAN_POINT('Ctrl Pts',(-18.2144906444783,12.5371593358493,123.635471051005)) ;
#80774 = CARTESIAN_POINT('Ctrl Pts',(-18.2079926912785,12.5389655205004,123.597494755401)) ;
#80775 = CARTESIAN_POINT('Ctrl Pts',(-18.2033107178565,12.5407863761254,123.559173318512)) ;
#80776 = CARTESIAN_POINT('Ctrl Pts',(-18.1994966225247,12.5422697072581,123.527955368222)) ;
#80777 = CARTESIAN_POINT('Ctrl Pts',(-18.1968868214949,12.543762774471,123.496508937966)) ;
#80778 = CARTESIAN_POINT('Ctrl Pts',(-18.1955062474138,12.5452653433241,123.464978035478)) ;
#80779 = CARTESIAN_POINT('Ctrl Pts',(-18.1924157706671,12.5486289108168,123.39439470187)) ;
#80780 = CARTESIAN_POINT('Ctrl Pts',(-18.1954901578647,12.5519576978783,123.323659203646)) ;
#80781 = CARTESIAN_POINT('Ctrl Pts',(-18.2046884819164,12.5552556142764,123.25362451513)) ;
#80782 = CARTESIAN_POINT('Ctrl Pts',(-18.2127932845956,12.5581614655498,123.191915737757)) ;
#80783 = CARTESIAN_POINT('Ctrl Pts',(-18.2256359409674,12.561085567277,123.13089343027)) ;
#80784 = CARTESIAN_POINT('Ctrl Pts',(-18.2430795069021,12.5640439274076,123.071177711639)) ;
#80785 = CARTESIAN_POINT('Ctrl Pts',(-18.2453973836478,12.5644370301813,123.063242770121)) ;
#80786 = CARTESIAN_POINT('Ctrl Pts',(-18.2477964241806,12.5648307378462,123.055330881221)) ;
#80787 = CARTESIAN_POINT('Ctrl Pts',(-18.2502762395728,12.5652250879601,123.047443484941)) ;
#80788 = CARTESIAN_POINT('Ctrl Pts',(-18.2675896731787,12.5679783390837,122.992375711655)) ;
#80789 = CARTESIAN_POINT('Ctrl Pts',(-18.2888214169512,12.5707060852376,122.938576593479)) ;
#80790 = CARTESIAN_POINT('Ctrl Pts',(-18.3137738281503,12.5734075221599,122.886538667041)) ;
#80791 = CARTESIAN_POINT('Ctrl Pts',(-18.3194690820111,12.5740241106306,122.874661289777)) ;
#80792 = CARTESIAN_POINT('Ctrl Pts',(-18.3253579683102,12.5746393285058,122.862875580663)) ;
#80793 = CARTESIAN_POINT('Ctrl Pts',(-18.3314377858075,12.5752531662224,122.851187249312)) ;
#80794 = CARTESIAN_POINT('Ctrl Pts',(-18.3589039783336,12.5780262403996,122.798384026295)) ;
#80795 = CARTESIAN_POINT('Ctrl Pts',(-18.3902368225375,12.5808351609625,122.74763471134)) ;
#80796 = CARTESIAN_POINT('Ctrl Pts',(-18.4251361962623,12.5836604667693,122.699424178035)) ;
#80797 = CARTESIAN_POINT('Ctrl Pts',(-18.431459525935,12.5841723768162,122.690689032866)) ;
#80798 = CARTESIAN_POINT('Ctrl Pts',(-18.4378998236653,12.5846848247728,122.682037160603)) ;
#80799 = CARTESIAN_POINT('Ctrl Pts',(-18.4444551479089,12.5851976948804,122.673471349781)) ;
#80800 = CARTESIAN_POINT('Ctrl Pts',(-18.4842452315836,12.5883107589698,122.621477837839)) ;
#80801 = CARTESIAN_POINT('Ctrl Pts',(-18.5282007356626,12.5913740642443,122.572756774188)) ;
#80802 = CARTESIAN_POINT('Ctrl Pts',(-18.5758383764271,12.594457279894,122.5278437079)) ;
#80803 = CARTESIAN_POINT('Ctrl Pts',(-18.5797969386911,12.59471348698,122.524111550586)) ;
#80804 = CARTESIAN_POINT('Ctrl Pts',(-18.5837809041891,12.5949698315505,122.520405668711)) ;
#80805 = CARTESIAN_POINT('Ctrl Pts',(-18.58778998298,12.5952263535819,122.516726359333)) ;
#80806 = CARTESIAN_POINT('Ctrl Pts',(-18.6400446190422,12.5985698811328,122.468769962743)) ;
#80807 = CARTESIAN_POINT('Ctrl Pts',(-18.6964140289307,12.6019299757216,122.425469517297)) ;
#80808 = CARTESIAN_POINT('Ctrl Pts',(-18.7562282492783,12.6052545103643,122.387342152182)) ;
#80809 = CARTESIAN_POINT('Ctrl Pts',(-18.7837994777867,12.6067869470287,122.369767430153)) ;
#80810 = CARTESIAN_POINT('Ctrl Pts',(-18.8120526841263,12.6083230835739,122.353328360479)) ;
#80811 = CARTESIAN_POINT('Ctrl Pts',(-18.8407669229486,12.6098552748236,122.338124868648)) ;
#80812 = CARTESIAN_POINT('Ctrl Pts',(-18.8696086665945,12.6113942697283,122.322853866111)) ;
#80813 = CARTESIAN_POINT('Ctrl Pts',(-18.898914945886,12.6129292842218,122.30882964563)) ;
#80814 = CARTESIAN_POINT('Ctrl Pts',(-18.9284433577873,12.6144525708304,122.296104304595)) ;
#80815 = CARTESIAN_POINT('Ctrl Pts',(-18.9326689618149,12.6146705576984,122.294283270247)) ;
#80816 = CARTESIAN_POINT('Ctrl Pts',(-18.9368990930012,12.6148883043974,122.292488750564)) ;
#80817 = CARTESIAN_POINT('Ctrl Pts',(-18.9411330215784,12.615105788223,122.290720813449)) ;
#80818 = CARTESIAN_POINT('Ctrl Pts',(-18.956775472796,12.6159092925976,122.284189085392)) ;
#80819 = CARTESIAN_POINT('Ctrl Pts',(-18.9727748193308,12.6167226885707,122.277897489621)) ;
#80820 = CARTESIAN_POINT('Ctrl Pts',(-18.9888360565228,12.6175313828714,122.271973357072)) ;
#80821 = CARTESIAN_POINT('Ctrl Pts',(-18.99777159258,12.6179812932362,122.268677515078)) ;
#80822 = CARTESIAN_POINT('Ctrl Pts',(-19.0067259121831,12.6184297483577,122.265494551706)) ;
#80823 = CARTESIAN_POINT('Ctrl Pts',(-19.0156457967525,12.6188742353227,122.262439829157)) ;
#80824 = CARTESIAN_POINT('Ctrl Pts',(-19.0372180981158,12.6199492051485,122.255052133174)) ;
#80825 = CARTESIAN_POINT('Ctrl Pts',(-19.0592532219469,12.621033427544,122.248189030563)) ;
#80826 = CARTESIAN_POINT('Ctrl Pts',(-19.0815133831771,12.6221207014324,122.24195257863)) ;
#80827 = CARTESIAN_POINT('Ctrl Pts',(-19.1008724951719,12.6230662766579,122.236528890536)) ;
#80828 = CARTESIAN_POINT('Ctrl Pts',(-19.1204012977472,12.6240141598346,122.231578502887)) ;
#80829 = CARTESIAN_POINT('Ctrl Pts',(-19.1399340122772,12.6249602721053,122.227137822195)) ;
#80830 = CARTESIAN_POINT('Ctrl Pts',(-19.1762012395167,12.6267169592603,122.218892620253)) ;
#80831 = CARTESIAN_POINT('Ctrl Pts',(-19.2130824695728,12.6284881998387,122.212263669636)) ;
#80832 = CARTESIAN_POINT('Ctrl Pts',(-19.2503316275509,12.6302618249869,122.207348451845)) ;
#80833 = CARTESIAN_POINT('Ctrl Pts',(-19.2831219408442,12.6318231414685,122.203021601521)) ;
#80834 = CARTESIAN_POINT('Ctrl Pts',(-19.3161967553501,12.6333863058065,122.200022166535)) ;
#80835 = CARTESIAN_POINT('Ctrl Pts',(-19.3493790843881,12.6349430168755,122.198384431677)) ;
#80836 = CARTESIAN_POINT('Ctrl Pts',(-19.4195611623873,12.6382355289092,122.194920550783)) ;
#80837 = CARTESIAN_POINT('Ctrl Pts',(-19.4898965900153,12.64154805959,122.197553795608)) ;
#80838 = CARTESIAN_POINT('Ctrl Pts',(-19.5595738808095,12.6448737795494,122.206240634518)) ;
#80839 = CARTESIAN_POINT('Ctrl Pts',(-19.6205231923216,12.6477829101929,122.213839334822)) ;
#80840 = CARTESIAN_POINT('Ctrl Pts',(-19.6808395885297,12.6506640612106,122.226057302673)) ;
#80841 = CARTESIAN_POINT('Ctrl Pts',(-19.7399214211662,12.6535589646203,122.242767662375)) ;
#80842 = CARTESIAN_POINT('Ctrl Pts',(-19.748705562942,12.6539893717496,122.245252117616)) ;
#80843 = CARTESIAN_POINT('Ctrl Pts',(-19.757462435201,12.6544200828757,122.247835785701)) ;
#80844 = CARTESIAN_POINT('Ctrl Pts',(-19.7661900808373,12.6548512351516,122.250518153353)) ;
#80845 = CARTESIAN_POINT('Ctrl Pts',(-19.8214982695661,12.6575835013827,122.267516654731)) ;
#80846 = CARTESIAN_POINT('Ctrl Pts',(-19.8755571439978,12.6603208780004,122.288460053437)) ;
#80847 = CARTESIAN_POINT('Ctrl Pts',(-19.9278701708427,12.6630421379963,122.313152907669)) ;
#80848 = CARTESIAN_POINT('Ctrl Pts',(-19.9397012183738,12.6636575746915,122.318737412135)) ;
#80849 = CARTESIAN_POINT('Ctrl Pts',(-19.9514430490475,12.6642721870574,122.324513497708)) ;
#80850 = CARTESIAN_POINT('Ctrl Pts',(-19.9630900591537,12.6648857295504,122.330478561421)) ;
#80851 = CARTESIAN_POINT('Ctrl Pts',(-20.0155103716858,12.6676471326004,122.357325838214)) ;
#80852 = CARTESIAN_POINT('Ctrl Pts',(-20.0659434995834,12.670415136917,122.387971786902)) ;
#80853 = CARTESIAN_POINT('Ctrl Pts',(-20.1139149856316,12.6732053908043,122.422126207481)) ;
#80854 = CARTESIAN_POINT('Ctrl Pts',(-20.1235337418823,12.673764864238,122.428974505783)) ;
#80855 = CARTESIAN_POINT('Ctrl Pts',(-20.1330536178746,12.6743252321981,122.435963716956)) ;
#80856 = CARTESIAN_POINT('Ctrl Pts',(-20.1424709209913,12.6748866208308,122.443091286621)) ;
#80857 = CARTESIAN_POINT('Ctrl Pts',(-20.1928674284073,12.6778908807596,122.481234331716)) ;
#80858 = CARTESIAN_POINT('Ctrl Pts',(-20.2402378432288,12.6808711487217,122.523277860457)) ;
#80859 = CARTESIAN_POINT('Ctrl Pts',(-20.2840898649842,12.6838320550256,122.568782370421)) ;
#80860 = CARTESIAN_POINT('Ctrl Pts',(-20.2894033086905,12.6841908209008,122.574296042138)) ;
#80861 = CARTESIAN_POINT('Ctrl Pts',(-20.2946651383711,12.6845493025163,122.579860479491)) ;
#80862 = CARTESIAN_POINT('Ctrl Pts',(-20.2998745118911,12.6849075081088,122.585474860889)) ;
#80863 = CARTESIAN_POINT('Ctrl Pts',(-20.3477823131988,12.6882017319327,122.637107301417)) ;
#80864 = CARTESIAN_POINT('Ctrl Pts',(-20.3911284512309,12.6915271808586,122.692829797445)) ;
#80865 = CARTESIAN_POINT('Ctrl Pts',(-20.4294058110033,12.6948703138278,122.752009370206)) ;
#80866 = CARTESIAN_POINT('Ctrl Pts',(-20.4475133760429,12.6964518230552,122.780004978293)) ;
#80867 = CARTESIAN_POINT('Ctrl Pts',(-20.4644420267259,12.6980235182476,122.808712988296)) ;
#80868 = CARTESIAN_POINT('Ctrl Pts',(-20.4800910780841,12.6995841135068,122.837910888563)) ;
#80869 = CARTESIAN_POINT('Ctrl Pts',(-20.4958052812698,12.7011512060054,122.867230348694)) ;
#80870 = CARTESIAN_POINT('Ctrl Pts',(-20.5102290000787,12.7027071059535,122.897043180513)) ;
#80871 = CARTESIAN_POINT('Ctrl Pts',(-20.523309439146,12.7042505113249,122.927105669496)) ;
#80872 = CARTESIAN_POINT('Ctrl Pts',(-20.524841996152,12.7044313429241,122.930627911974)) ;
#80873 = CARTESIAN_POINT('Ctrl Pts',(-20.5263561703865,12.7046120030052,122.934153567087)) ;
#80874 = CARTESIAN_POINT('Ctrl Pts',(-20.5278519224255,12.7047924894739,122.937682232513)) ;
#80875 = CARTESIAN_POINT('Ctrl Pts',(-20.5348041812293,12.705631390982,122.95408347726)) ;
#80876 = CARTESIAN_POINT('Ctrl Pts',(-20.5414808187029,12.7064832685371,122.970849510673)) ;
#80877 = CARTESIAN_POINT('Ctrl Pts',(-20.5477576521918,12.7073326882528,122.987698134135)) ;
#80878 = CARTESIAN_POINT('Ctrl Pts',(-20.5515482935938,12.7078456611631,122.997873183349)) ;
#80879 = CARTESIAN_POINT('Ctrl Pts',(-20.5551940473909,12.7083577376821,123.008077933982)) ;
#80880 = CARTESIAN_POINT('Ctrl Pts',(-20.5586762065934,12.7088655184933,123.018247020808)) ;
#80881 = CARTESIAN_POINT('Ctrl Pts',(-20.5658397893312,12.7099101375478,123.039167113949)) ;
#80882 = CARTESIAN_POINT('Ctrl Pts',(-20.5725121880288,12.7109660365692,123.060529591782)) ;
#80883 = CARTESIAN_POINT('Ctrl Pts',(-20.5785924632154,12.7120216609084,123.082091287369)) ;
#80884 = CARTESIAN_POINT('Ctrl Pts',(-20.58360867267,12.7128925479371,123.099879623907)) ;
#80885 = CARTESIAN_POINT('Ctrl Pts',(-20.5882226913621,12.7137632480116,123.117803051032)) ;
#80886 = CARTESIAN_POINT('Ctrl Pts',(-20.5924034687724,12.7146272730841,123.135717307983)) ;
#80887 = CARTESIAN_POINT('Ctrl Pts',(-20.6006051681473,12.7163222865232,123.170860855611)) ;
#80888 = CARTESIAN_POINT('Ctrl Pts',(-20.6072936634496,12.7180282649194,123.206614212993)) ;
#80889 = CARTESIAN_POINT('Ctrl Pts',(-20.6123708257249,12.7197467163026,123.242737733281)) ;
#80890 = CARTESIAN_POINT('Ctrl Pts',(-20.6170581982933,12.7213332367715,123.276087937369)) ;
#80891 = CARTESIAN_POINT('Ctrl Pts',(-20.6203725208227,12.7229303885638,123.309753023635)) ;
#80892 = CARTESIAN_POINT('Ctrl Pts',(-20.6222745883944,12.724539358364,123.34353366244)) ;
#80893 = CARTESIAN_POINT('Ctrl Pts',(-20.6262623466444,12.7279126257966,123.414356078574)) ;
#80894 = CARTESIAN_POINT('Ctrl Pts',(-20.6240383934404,12.7312613121533,123.485408065895)) ;
#80895 = CARTESIAN_POINT('Ctrl Pts',(-20.6156319034181,12.7345698810621,123.555833596735)) ;
#80896 = CARTESIAN_POINT('Ctrl Pts',(-20.6081187423961,12.7375268596463,123.618775246799)) ;
#80897 = CARTESIAN_POINT('Ctrl Pts',(-20.5956838500786,12.7405056930328,123.681057206444)) ;
#80898 = CARTESIAN_POINT('Ctrl Pts',(-20.5784645379807,12.7435210083962,123.742029330954)) ;
#80899 = CARTESIAN_POINT('Ctrl Pts',(-20.5765123326015,12.743862863799,123.748941924719)) ;
#80900 = CARTESIAN_POINT('Ctrl Pts',(-20.5744986845941,12.7442051881207,123.755837694971)) ;
#80901 = CARTESIAN_POINT('Ctrl Pts',(-20.5724238354329,12.7445480026765,123.762715702902)) ;
#80902 = CARTESIAN_POINT('Ctrl Pts',(-20.5557105155931,12.7473094416402,123.81811941541)) ;
#80903 = CARTESIAN_POINT('Ctrl Pts',(-20.5350449674215,12.7500407281243,123.872293178228)) ;
#80904 = CARTESIAN_POINT('Ctrl Pts',(-20.5106204324781,12.7527494963095,123.924739422088)) ;
#80905 = CARTESIAN_POINT('Ctrl Pts',(-20.5051200868351,12.7533595042921,123.936550188171)) ;
#80906 = CARTESIAN_POINT('Ctrl Pts',(-20.4994293020387,12.753968370283,123.948273423035)) ;
#80907 = CARTESIAN_POINT('Ctrl Pts',(-20.4935506230553,12.7545761814695,123.959903581031)) ;
#80908 = CARTESIAN_POINT('Ctrl Pts',(-20.4668860643504,12.7573330962648,124.012655743805)) ;
#80909 = CARTESIAN_POINT('Ctrl Pts',(-20.4363847262239,12.760127225549,124.063426780408)) ;
#80910 = CARTESIAN_POINT('Ctrl Pts',(-20.4023365548253,12.7629283003074,124.111736503173)) ;
#80911 = CARTESIAN_POINT('Ctrl Pts',(-20.3959454412135,12.7634540844033,124.12080462384)) ;
#80912 = CARTESIAN_POINT('Ctrl Pts',(-20.3894294835363,12.7639801132181,124.129786098529)) ;
#80913 = CARTESIAN_POINT('Ctrl Pts',(-20.3827907748379,12.7645061865598,124.138677857193)) ;
#80914 = CARTESIAN_POINT('Ctrl Pts',(-20.3436549708646,12.7676074377384,124.191095599836)) ;
#80915 = CARTESIAN_POINT('Ctrl Pts',(-20.3003200443191,12.7706663358612,124.240299227947)) ;
#80916 = CARTESIAN_POINT('Ctrl Pts',(-20.2532605411037,12.7737563344538,124.285747411231)) ;
#80917 = CARTESIAN_POINT('Ctrl Pts',(-20.2495339480594,12.7740010282239,124.289346405528)) ;
#80918 = CARTESIAN_POINT('Ctrl Pts',(-20.2457840194963,12.7742459170217,124.292921867039)) ;
#80919 = CARTESIAN_POINT('Ctrl Pts',(-20.2420110021608,12.7744910373231,124.29647353554)) ;
#80920 = CARTESIAN_POINT('Ctrl Pts',(-20.1903647834785,12.7778463192005,124.345089863483)) ;
#80921 = CARTESIAN_POINT('Ctrl Pts',(-20.1345459269395,12.7812066706123,124.389101475417)) ;
#80922 = CARTESIAN_POINT('Ctrl Pts',(-20.075214192574,12.7845191703928,124.427985094354)) ;
#80923 = CARTESIAN_POINT('Ctrl Pts',(-20.0457376691239,12.7861648491936,124.447302815599)) ;
#80924 = CARTESIAN_POINT('Ctrl Pts',(-20.0154524966392,12.7878143806419,124.465310970758)) ;
#80925 = CARTESIAN_POINT('Ctrl Pts',(-19.9846105575071,12.7894647330416,124.481893804531)) ;
#80926 = CARTESIAN_POINT('Ctrl Pts',(-19.9537686183751,12.7911150854413,124.498476638304)) ;
#80927 = CARTESIAN_POINT('Ctrl Pts',(-19.9223706627251,12.7927662587925,124.513633935522)) ;
#80928 = CARTESIAN_POINT('Ctrl Pts',(-19.890689853112,12.7944152213991,124.527306861112)) ;
#80929 = CARTESIAN_POINT('Ctrl Pts',(-19.8733675535382,12.7953168342243,124.534782885747)) ;
#80930 = CARTESIAN_POINT('Ctrl Pts',(-19.8556736911802,12.7962290946323,124.541935886302)) ;
#80931 = CARTESIAN_POINT('Ctrl Pts',(-19.837877219646,12.7971348160649,124.548645617426)) ;
#80932 = CARTESIAN_POINT('Ctrl Pts',(-19.826205722036,12.7977288172698,124.553046074598)) ;
#80933 = CARTESIAN_POINT('Ctrl Pts',(-19.8144905578315,12.7983200059584,124.557256844807)) ;
#80934 = CARTESIAN_POINT('Ctrl Pts',(-19.8028118584132,12.7989035340819,124.561255430345)) ;
#80935 = CARTESIAN_POINT('Ctrl Pts',(-19.7826198328396,12.7999124319371,124.568168832134)) ;
#80936 = CARTESIAN_POINT('Ctrl Pts',(-19.7620048595353,12.8009244496695,124.574628037106)) ;
#80937 = CARTESIAN_POINT('Ctrl Pts',(-19.7412166057261,12.8019330346865,124.580532550084)) ;
#80938 = CARTESIAN_POINT('Ctrl Pts',(-19.7249347561583,12.8027229822057,124.585157103593)) ;
#80939 = CARTESIAN_POINT('Ctrl Pts',(-19.7085470911927,12.8035108239631,124.589442309953)) ;
#80940 = CARTESIAN_POINT('Ctrl Pts',(-19.6921799650699,12.8042934117004,124.593361328602)) ;
#80941 = CARTESIAN_POINT('Ctrl Pts',(-19.6579132877952,12.8059318594787,124.601566296674)) ;
#80942 = CARTESIAN_POINT('Ctrl Pts',(-19.6230334882165,12.8075974503459,124.608337509049)) ;
#80943 = CARTESIAN_POINT('Ctrl Pts',(-19.5877754174827,12.8092799940258,124.613574718257)) ;
#80944 = CARTESIAN_POINT('Ctrl Pts',(-19.5539179714286,12.8108956987621,124.618603879653)) ;
#80945 = CARTESIAN_POINT('Ctrl Pts',(-19.5197123376266,12.812527036165,124.6222186044)) ;
#80946 = CARTESIAN_POINT('Ctrl Pts',(-19.4853790432398,12.8141649827786,124.624373656255)) ;
#80947 = CARTESIAN_POINT('Ctrl Pts',(-19.4145452746383,12.8175442661676,124.628819790748)) ;
#80948 = CARTESIAN_POINT('Ctrl Pts',(-19.343435013163,12.8208579572261,124.627048899914)) ;
#80949 = CARTESIAN_POINT('Ctrl Pts',(-19.2729158335981,12.8242010480661,124.619084058099)) ;
#80950 = CARTESIAN_POINT('Ctrl Pts',(-19.2097868481366,12.827193793222,124.611953907319)) ;
#80951 = CARTESIAN_POINT('Ctrl Pts',(-19.1472852309664,12.8302092116872,124.599875437733)) ;
#80952 = CARTESIAN_POINT('Ctrl Pts',(-19.0860661233276,12.8331908220591,124.582980692508)) ;
#80953 = CARTESIAN_POINT('Ctrl Pts',(-19.0788994638717,12.8335398664504,124.581002896845)) ;
#80954 = CARTESIAN_POINT('Ctrl Pts',(-19.0717503683076,12.8338884475227,124.578959154462)) ;
#80955 = CARTESIAN_POINT('Ctrl Pts',(-19.0646198790754,12.8342364746619,124.576849723125)) ;
#80956 = CARTESIAN_POINT('Ctrl Pts',(-19.0078934037652,12.8370051981361,124.560068181106)) ;
#80957 = CARTESIAN_POINT('Ctrl Pts',(-18.9524364073411,12.8397779519758,124.539151933304)) ;
#80958 = CARTESIAN_POINT('Ctrl Pts',(-18.8987731161,12.8425868853042,124.514303244646)) ;
#80959 = CARTESIAN_POINT('Ctrl Pts',(-18.8886143406051,12.8431186328434,124.509599242271)) ;
#80960 = CARTESIAN_POINT('Ctrl Pts',(-18.8785197895817,12.8436516769365,124.504754453293)) ;
#80961 = CARTESIAN_POINT('Ctrl Pts',(-18.8684929416447,12.8441862356861,124.499770445251)) ;
#80962 = CARTESIAN_POINT('Ctrl Pts',(-18.816742531374,12.8469451919186,124.474047061129)) ;
#80963 = CARTESIAN_POINT('Ctrl Pts',(-18.7668609318805,12.8496745801071,124.444642998157)) ;
#80964 = CARTESIAN_POINT('Ctrl Pts',(-18.7193050246574,12.8523779218263,124.411831018458)) ;
#80965 = CARTESIAN_POINT('Ctrl Pts',(-18.7085176446678,12.8529911363788,124.404388088359)) ;
#80966 = CARTESIAN_POINT('Ctrl Pts',(-18.6978498211941,12.8536030107243,124.396769986417)) ;
#80967 = CARTESIAN_POINT('Ctrl Pts',(-18.6873066910414,12.8542135859656,124.388980213986)) ;
#80968 = CARTESIAN_POINT('Ctrl Pts',(-18.6357053940623,12.8572019275588,124.350854690087)) ;
#80969 = CARTESIAN_POINT('Ctrl Pts',(-18.5871692007383,12.8602368807547,124.308669656888)) ;
#80970 = CARTESIAN_POINT('Ctrl Pts',(-18.542217609392,12.8632832123375,124.262872240437)) ;
#80971 = CARTESIAN_POINT('Ctrl Pts',(-18.5379626773981,12.8635715655043,124.258537246132)) ;
#80972 = CARTESIAN_POINT('Ctrl Pts',(-18.5337398383119,12.8638600206183,124.254169915882)) ;
#80973 = CARTESIAN_POINT('Ctrl Pts',(-18.5295495179456,12.8641485477988,124.249770648193)) ;
#80974 = CARTESIAN_POINT('Ctrl Pts',(-18.4807966480294,12.8675054577398,124.198586751342)) ;
#80975 = CARTESIAN_POINT('Ctrl Pts',(-18.4365915825538,12.8708059686782,124.143232112355)) ;
#80976 = CARTESIAN_POINT('Ctrl Pts',(-18.39744901714,12.8741441467103,124.084340104869)) ;
#80977 = CARTESIAN_POINT('Ctrl Pts',(-18.377826846205,12.8758175756045,124.054817537164)) ;
#80978 = CARTESIAN_POINT('Ctrl Pts',(-18.3595260505841,12.8774935606388,124.02447155287)) ;
#80979 = CARTESIAN_POINT('Ctrl Pts',(-18.342659499529,12.8791574474389,123.993545530683)) ;
#80980 = CARTESIAN_POINT('Ctrl Pts',(-18.3257929484739,12.8808213342391,123.962619508496)) ;
#80981 = CARTESIAN_POINT('Ctrl Pts',(-18.3103608501574,12.882473122805,123.931114152062)) ;
#80982 = CARTESIAN_POINT('Ctrl Pts',(-18.2964222918482,12.8840981587624,123.899293066508)) ;
#80983 = CARTESIAN_POINT('Ctrl Pts',(-18.2884868930003,12.8850233124389,123.881176917043)) ;
#80984 = CARTESIAN_POINT('Ctrl Pts',(-18.2809156414011,12.8859571442745,123.862677592541)) ;
#80985 = CARTESIAN_POINT('Ctrl Pts',(-18.273826278364,12.88689064817,123.844053819635)) ;
#80986 = CARTESIAN_POINT('Ctrl Pts',(-18.2689213497686,12.8875365129574,123.831168561001)) ;
#80987 = CARTESIAN_POINT('Ctrl Pts',(-18.2642461152496,12.8881822207643,123.818224229348)) ;
#80988 = CARTESIAN_POINT('Ctrl Pts',(-18.259825879779,12.8888247888663,123.80531165987)) ;
#80989 = CARTESIAN_POINT('Origin',(-19.4092696390626,-30.19753203383,123.411833654984)) ;
#80990 = CARTESIAN_POINT('',(-20.3451307049827,12.4073898409302,124.186586679355)) ;
#80991 = CARTESIAN_POINT('Ctrl Pts',(-20.3451203705583,12.4073818757045,124.186578325469)) ;
#80992 = CARTESIAN_POINT('Ctrl Pts',(-20.3351949287717,12.4081071627668,124.198567736058)) ;
#80993 = CARTESIAN_POINT('Ctrl Pts',(-20.325040088624,12.4088341710223,124.210365203265)) ;
#80994 = CARTESIAN_POINT('Ctrl Pts',(-20.3121345010096,12.409742328298,124.224788326587)) ;
#80995 = CARTESIAN_POINT('Ctrl Pts',(-20.309594359267,12.4099203334478,124.227600567204)) ;
#80996 = CARTESIAN_POINT('Ctrl Pts',(-20.3050370056896,12.4102384080975,124.232598888577)) ;
#80997 = CARTESIAN_POINT('Ctrl Pts',(-20.3030248429629,12.4103784012063,124.234789534253)) ;
#80998 = CARTESIAN_POINT('Ctrl Pts',(-20.2989274424902,12.4106625874831,124.23921763062)) ;
#80999 = CARTESIAN_POINT('Ctrl Pts',(-20.2968417606344,12.4108067866048,124.241454640298)) ;
#81000 = CARTESIAN_POINT('Ctrl Pts',(-20.2923176801424,12.4111185917832,124.246270380385)) ;
#81001 = CARTESIAN_POINT('Ctrl Pts',(-20.2898763860514,12.4112862410792,124.248846348195)) ;
#81002 = CARTESIAN_POINT('Ctrl Pts',(-20.2831348621503,12.4117475412132,124.255897626483)) ;
#81003 = CARTESIAN_POINT('Ctrl Pts',(-20.2788115848992,12.4120415369396,124.260350726086)) ;
#81004 = CARTESIAN_POINT('Ctrl Pts',(-20.2545481983232,12.4136813136958,124.284962527665)) ;
#81005 = CARTESIAN_POINT('Ctrl Pts',(-20.2339414290011,12.4150371351338,124.304451306211)) ;
#81006 = CARTESIAN_POINT('Ctrl Pts',(-20.2030097990134,12.4170051085396,124.331718628332)) ;
#81007 = CARTESIAN_POINT('Ctrl Pts',(-20.1932126374959,12.4176189969046,124.340082104741)) ;
#81008 = CARTESIAN_POINT('Ctrl Pts',(-20.1763776108473,12.4186569494554,124.353996881931)) ;
#81009 = CARTESIAN_POINT('Ctrl Pts',(-20.1694079668242,12.4190819065003,124.359628944506)) ;
#81010 = CARTESIAN_POINT('Ctrl Pts',(-20.1621103054176,12.4195219507914,124.365393795902)) ;
#81011 = CARTESIAN_POINT('Ctrl Pts',(-20.1618439056668,12.4195380078138,124.365604059489)) ;
#81012 = CARTESIAN_POINT('Ctrl Pts',(-20.1613584098179,12.4195672584535,124.36598692086)) ;
#81013 = CARTESIAN_POINT('Ctrl Pts',(-20.1611393423655,12.4195804525209,124.366159554839)) ;
#81014 = CARTESIAN_POINT('Ctrl Pts',(-20.1607358942941,12.4196047431953,124.366477263027)) ;
#81015 = CARTESIAN_POINT('Ctrl Pts',(-20.1605515310391,12.4196158400796,124.366622359314)) ;
#81016 = CARTESIAN_POINT('Ctrl Pts',(-20.1602085934314,12.4196364756577,124.36689209486)) ;
#81017 = CARTESIAN_POINT('Ctrl Pts',(-20.1600500300406,12.4196460145262,124.367016748055)) ;
#81018 = CARTESIAN_POINT('Ctrl Pts',(-20.1597522707092,12.4196639227199,124.367250708948)) ;
#81019 = CARTESIAN_POINT('Ctrl Pts',(-20.1596130819206,12.4196722921582,124.367360025719)) ;
#81020 = CARTESIAN_POINT('Ctrl Pts',(-20.1593493191757,12.4196881487995,124.36756708782)) ;
#81021 = CARTESIAN_POINT('Ctrl Pts',(-20.1592247498602,12.4196956360863,124.367664839319)) ;
#81022 = CARTESIAN_POINT('Ctrl Pts',(-20.1589866086921,12.419709946874,124.367851637222)) ;
#81023 = CARTESIAN_POINT('Ctrl Pts',(-20.1588730401842,12.4197167704202,124.367940687664)) ;
#81024 = CARTESIAN_POINT('Ctrl Pts',(-20.158654058468,12.4197299251898,124.368112330879)) ;
#81025 = CARTESIAN_POINT('Ctrl Pts',(-20.1585486475016,12.4197362564463,124.368194926435)) ;
#81026 = CARTESIAN_POINT('Ctrl Pts',(-20.1583436622498,12.4197485663735,124.368355489479)) ;
#81027 = CARTESIAN_POINT('Ctrl Pts',(-20.1582440894389,12.4197545450679,124.368433458853)) ;
#81028 = CARTESIAN_POINT('Ctrl Pts',(-20.1580488011973,12.4197662690306,124.368586327941)) ;
#81029 = CARTESIAN_POINT('Ctrl Pts',(-20.1579530866292,12.4197720143179,124.368661228895)) ;
#81030 = CARTESIAN_POINT('Ctrl Pts',(-20.1577637300843,12.4197833787939,124.368809363099)) ;
#81031 = CARTESIAN_POINT('Ctrl Pts',(-20.1576700887087,12.4197889979836,124.368882596881)) ;
#81032 = CARTESIAN_POINT('Ctrl Pts',(-20.1574831628118,12.4198002133178,124.369028741151)) ;
#81033 = CARTESIAN_POINT('Ctrl Pts',(-20.1573898782531,12.4198058094711,124.369101651847)) ;
#81034 = CARTESIAN_POINT('Ctrl Pts',(-20.1547454393545,12.4199644267504,124.371167908036)) ;
#81035 = CARTESIAN_POINT('Ctrl Pts',(-20.1521863335445,12.4201173195669,124.373151065124)) ;
#81036 = CARTESIAN_POINT('Ctrl Pts',(-20.1469941620041,12.4204263136892,124.377141578164)) ;
#81037 = CARTESIAN_POINT('Ctrl Pts',(-20.1443607566838,12.420582407861,124.379148447169)) ;
#81038 = CARTESIAN_POINT('Ctrl Pts',(-20.1381947792298,12.4209464638494,124.383807702979)) ;
#81039 = CARTESIAN_POINT('Ctrl Pts',(-20.1346558769511,12.4211543225996,124.386451639636)) ;
#81040 = CARTESIAN_POINT('Ctrl Pts',(-20.1233518355119,12.4218149192927,124.394801286129)) ;
#81041 = CARTESIAN_POINT('Ctrl Pts',(-20.11553318429,12.422266828683,124.400433955071)) ;
#81042 = CARTESIAN_POINT('Ctrl Pts',(-20.0913038663772,12.4236534400491,124.417454947616)) ;
#81043 = CARTESIAN_POINT('Ctrl Pts',(-20.0746788275006,12.4245854632615,124.428531977815)) ;
#81044 = CARTESIAN_POINT('Ctrl Pts',(-20.0478927348905,12.4260679981706,124.445440629808)) ;
#81045 = CARTESIAN_POINT('Ctrl Pts',(-20.0379075500964,12.426616925415,124.451543811609)) ;
#81046 = CARTESIAN_POINT('Ctrl Pts',(-20.0221992236386,12.4274748179944,124.460836090356)) ;
#81047 = CARTESIAN_POINT('Ctrl Pts',(-20.0165357731909,12.4277829769006,124.464124787248)) ;
#81048 = CARTESIAN_POINT('Ctrl Pts',(-20.0042389782745,12.4284495607202,124.471133052563)) ;
#81049 = CARTESIAN_POINT('Ctrl Pts',(-19.9975967374022,12.4288080654643,124.474836455182)) ;
#81050 = CARTESIAN_POINT('Ctrl Pts',(-19.9898368802709,12.4292250499094,124.4790679765)) ;
#81051 = CARTESIAN_POINT('Ctrl Pts',(-19.9887526831407,12.4292832689228,124.479657058085)) ;
#81052 = CARTESIAN_POINT('Ctrl Pts',(-19.9862073380042,12.429419850731,124.481035013427)) ;
#81053 = CARTESIAN_POINT('Ctrl Pts',(-19.9847454665762,12.4294982186086,124.481822545253)) ;
#81054 = CARTESIAN_POINT('Ctrl Pts',(-19.9811436218778,12.4296911198525,124.483753395688)) ;
#81055 = CARTESIAN_POINT('Ctrl Pts',(-19.9790018298922,12.4298056648805,124.484893305448)) ;
#81056 = CARTESIAN_POINT('Ctrl Pts',(-19.9742495803081,12.4300594602298,124.487404320452)) ;
#81057 = CARTESIAN_POINT('Ctrl Pts',(-19.9716375168863,12.4301987190576,124.488772353519)) ;
#81058 = CARTESIAN_POINT('Ctrl Pts',(-19.948779499333,12.4314152607861,124.500638094162)) ;
#81059 = CARTESIAN_POINT('Ctrl Pts',(-19.9282466598147,12.4324936651641,124.510573318427)) ;
#81060 = CARTESIAN_POINT('Ctrl Pts',(-19.8975368281539,12.4340841684697,124.524379876922)) ;
#81061 = CARTESIAN_POINT('Ctrl Pts',(-19.8875679291923,12.434597071333,124.528701906152)) ;
#81062 = CARTESIAN_POINT('Ctrl Pts',(-19.8701781872394,12.435485743556,124.535965720148)) ;
#81063 = CARTESIAN_POINT('Ctrl Pts',(-19.8627838517513,12.4358617211218,124.538969161112)) ;
#81064 = CARTESIAN_POINT('Ctrl Pts',(-19.8429676240375,12.4368644695173,124.546791569487)) ;
#81065 = CARTESIAN_POINT('Ctrl Pts',(-19.8304951579678,12.4374907082586,124.551479421536)) ;
#81066 = CARTESIAN_POINT('Ctrl Pts',(-19.8043563752147,12.4387953648757,124.56081610576)) ;
#81067 = CARTESIAN_POINT('Ctrl Pts',(-19.7906792355348,12.4394736846942,124.565428436577)) ;
#81068 = CARTESIAN_POINT('Ctrl Pts',(-19.7673082292067,12.4406274616318,124.572848741369)) ;
#81069 = CARTESIAN_POINT('Ctrl Pts',(-19.7576556409935,12.4411024651437,124.575781615882)) ;
#81070 = CARTESIAN_POINT('Ctrl Pts',(-19.7407866454728,12.4419305084295,124.58067850486)) ;
#81071 = CARTESIAN_POINT('Ctrl Pts',(-19.7335865458731,12.4422832824306,124.582696734997)) ;
#81072 = CARTESIAN_POINT('Ctrl Pts',(-19.7180098829887,12.4430452937906,124.58690826025)) ;
#81073 = CARTESIAN_POINT('Ctrl Pts',(-19.7096275800231,12.4434546271339,124.589078732567)) ;
#81074 = CARTESIAN_POINT('Ctrl Pts',(-19.6746699160501,12.4451592349017,124.597732830853)) ;
#81075 = CARTESIAN_POINT('Ctrl Pts',(-19.6479027753465,12.446460475465,124.603407554339)) ;
#81076 = CARTESIAN_POINT('Ctrl Pts',(-19.6110658098122,12.4482383263109,124.609926018679)) ;
#81077 = CARTESIAN_POINT('Ctrl Pts',(-19.6011428731397,12.448715775322,124.611555151746)) ;
#81078 = CARTESIAN_POINT('Ctrl Pts',(-19.5837658892678,12.4495488284594,124.614186972862)) ;
#81079 = CARTESIAN_POINT('Ctrl Pts',(-19.5763206380909,12.4499047838548,124.615243978531)) ;
#81080 = CARTESIAN_POINT('Ctrl Pts',(-19.5647395600847,12.4504569044709,124.616778602469)) ;
#81081 = CARTESIAN_POINT('Ctrl Pts',(-19.560610302201,12.4506534566962,124.61730419657)) ;
#81082 = CARTESIAN_POINT('Ctrl Pts',(-19.552615905046,12.4510333989522,124.618280042272)) ;
#81083 = CARTESIAN_POINT('Ctrl Pts',(-19.5487511443468,12.4512168095026,124.6187329661)) ;
#81084 = CARTESIAN_POINT('Ctrl Pts',(-19.5397504720133,12.4516433525712,124.619743973136)) ;
#81085 = CARTESIAN_POINT('Ctrl Pts',(-19.5346130399005,12.4518863590588,124.620287881093)) ;
#81086 = CARTESIAN_POINT('Ctrl Pts',(-19.5177162133305,12.4526841952608,124.621967865714)) ;
#81087 = CARTESIAN_POINT('Ctrl Pts',(-19.505943680787,12.4532378123697,124.622965191915)) ;
#81088 = CARTESIAN_POINT('Ctrl Pts',(-19.467090319242,12.4550596706197,124.625686587222)) ;
#81089 = CARTESIAN_POINT('Ctrl Pts',(-19.4399663337638,12.4563231749537,124.626675162395)) ;
#81090 = CARTESIAN_POINT('Ctrl Pts',(-19.4032873085652,12.4580383616142,124.626782711314)) ;
#81091 = CARTESIAN_POINT('Ctrl Pts',(-19.3937426677449,12.4584852406688,124.626698219334)) ;
#81092 = CARTESIAN_POINT('Ctrl Pts',(-19.3786396096712,12.4591938194038,124.62638650644)) ;
#81093 = CARTESIAN_POINT('Ctrl Pts',(-19.3730800437493,12.4594549633874,124.62623356464)) ;
#81094 = CARTESIAN_POINT('Ctrl Pts',(-19.3626132242422,12.4599472966608,124.625873686047)) ;
#81095 = CARTESIAN_POINT('Ctrl Pts',(-19.3577057920009,12.4601784139758,124.625675155148)) ;
#81096 = CARTESIAN_POINT('Ctrl Pts',(-19.3499109047112,12.460546013042,124.625312455789)) ;
#81097 = CARTESIAN_POINT('Ctrl Pts',(-19.3470225932408,12.4606823310212,124.625167724639)) ;
#81098 = CARTESIAN_POINT('Ctrl Pts',(-19.3402806110107,12.4610007912081,124.624805751909)) ;
#81099 = CARTESIAN_POINT('Ctrl Pts',(-19.3364274075621,12.4611829994012,124.62458045589)) ;
#81100 = CARTESIAN_POINT('Ctrl Pts',(-19.3272924955378,12.4616154601858,124.624002646601)) ;
#81101 = CARTESIAN_POINT('Ctrl Pts',(-19.3220118953407,12.4618658442989,124.623633969465)) ;
#81102 = CARTESIAN_POINT('Ctrl Pts',(-19.3010691538164,12.4628604591191,124.622034203137)) ;
#81103 = CARTESIAN_POINT('Ctrl Pts',(-19.2854292205939,12.4636068434062,124.620533889162)) ;
#81104 = CARTESIAN_POINT('Ctrl Pts',(-19.2621492949723,12.4647227455979,124.617844090457)) ;
#81105 = CARTESIAN_POINT('Ctrl Pts',(-19.2544843531212,12.4650909426616,124.616884309909)) ;
#81106 = CARTESIAN_POINT('Ctrl Pts',(-19.2284568809309,12.46634349718,124.613372803311)) ;
#81107 = CARTESIAN_POINT('Ctrl Pts',(-19.2101437085806,12.467228586291,124.610473904923)) ;
#81108 = CARTESIAN_POINT('Ctrl Pts',(-19.1814321557965,12.4686167418677,124.605252802963)) ;
#81109 = CARTESIAN_POINT('Ctrl Pts',(-19.1709857538774,12.4691219684945,124.603210998307)) ;
#81110 = CARTESIAN_POINT('Ctrl Pts',(-19.1566241463862,12.469816499792,124.600207493878)) ;
#81111 = CARTESIAN_POINT('Ctrl Pts',(-19.1526849468642,12.4700069988917,124.599363200647)) ;
#81112 = CARTESIAN_POINT('Ctrl Pts',(-19.1455266584401,12.470353173029,124.597791675751)) ;
#81113 = CARTESIAN_POINT('Ctrl Pts',(-19.1423061980073,12.4705089144514,124.597070892028)) ;
#81114 = CARTESIAN_POINT('Ctrl Pts',(-19.1359887750859,12.4708144342264,124.595629910688)) ;
#81115 = CARTESIAN_POINT('Ctrl Pts',(-19.1328916247853,12.4709642213392,124.594910659636)) ;
#81116 = CARTESIAN_POINT('Ctrl Pts',(-19.1297777194605,12.4711148299593,124.594174622459)) ;
#81117 = CARTESIAN_POINT('Ctrl Pts',(-19.1297581115696,12.4711157783243,124.594169987205)) ;
#81118 = CARTESIAN_POINT('Ctrl Pts',(-19.1297187849672,12.4711176804152,124.594160689468)) ;
#81119 = CARTESIAN_POINT('Ctrl Pts',(-19.1296990663627,12.471118634136,124.594156027003)) ;
#81120 = CARTESIAN_POINT('Ctrl Pts',(-19.1296595142969,12.4711205471336,124.594146673871)) ;
#81121 = CARTESIAN_POINT('Ctrl Pts',(-19.1296396812692,12.4711215063896,124.5941419833)) ;
#81122 = CARTESIAN_POINT('Ctrl Pts',(-19.1295998966232,12.4711234306382,124.594132573054)) ;
#81123 = CARTESIAN_POINT('Ctrl Pts',(-19.1295799451038,12.4711243956262,124.594127853396)) ;
#81124 = CARTESIAN_POINT('Ctrl Pts',(-19.1295399194418,12.4711263315339,124.594118384003)) ;
#81125 = CARTESIAN_POINT('Ctrl Pts',(-19.1295198457925,12.4711273024298,124.594113634378)) ;
#81126 = CARTESIAN_POINT('Ctrl Pts',(-19.1294795723347,12.4711292503245,124.594104104195)) ;
#81127 = CARTESIAN_POINT('Ctrl Pts',(-19.1294593721875,12.4711302273397,124.594099323549)) ;
#81128 = CARTESIAN_POINT('Ctrl Pts',(-19.1294188413759,12.4711321876837,124.594089730272)) ;
#81129 = CARTESIAN_POINT('Ctrl Pts',(-19.1293985113244,12.471133170983,124.594084917779)) ;
#81130 = CARTESIAN_POINT('Ctrl Pts',(-19.1293577174786,12.4711351440512,124.594075260022)) ;
#81131 = CARTESIAN_POINT('Ctrl Pts',(-19.1293372525617,12.4711361338745,124.594070414485)) ;
#81132 = CARTESIAN_POINT('Ctrl Pts',(-19.1292961847695,12.4711381201946,124.59406068962)) ;
#81133 = CARTESIAN_POINT('Ctrl Pts',(-19.1292755817868,12.4711391166967,124.594055810259)) ;
#81134 = CARTESIAN_POINT('Ctrl Pts',(-19.1292342324706,12.4711411166354,124.594046016447)) ;
#81135 = CARTESIAN_POINT('Ctrl Pts',(-19.1292134873069,12.4711421200155,124.594041102264)) ;
#81136 = CARTESIAN_POINT('Ctrl Pts',(-19.1291718507328,12.4711441338501,124.594031238097)) ;
#81137 = CARTESIAN_POINT('Ctrl Pts',(-19.1291509578169,12.4711451443775,124.594026287749)) ;
#81138 = CARTESIAN_POINT('Ctrl Pts',(-19.1291090203986,12.4711471727652,124.594016349961)) ;
#81139 = CARTESIAN_POINT('Ctrl Pts',(-19.1290879772574,12.4711481905597,124.594011362836)) ;
#81140 = CARTESIAN_POINT('Ctrl Pts',(-19.1290457353088,12.4711502336789,124.594001350502)) ;
#81141 = CARTESIAN_POINT('Ctrl Pts',(-19.1290245359253,12.4711512590314,124.593996325147)) ;
#81142 = CARTESIAN_POINT('Ctrl Pts',(-19.1289819772032,12.4711533174743,124.593986235312)) ;
#81143 = CARTESIAN_POINT('Ctrl Pts',(-19.1289606179962,12.4711543505582,124.593981170853)) ;
#81144 = CARTESIAN_POINT('Ctrl Pts',(-19.1289177351044,12.4711564246825,124.593971001709)) ;
#81145 = CARTESIAN_POINT('Ctrl Pts',(-19.1288962111384,12.4711574657365,124.593965896947)) ;
#81146 = CARTESIAN_POINT('Ctrl Pts',(-19.1288529937298,12.4711595560428,124.593955645983)) ;
#81147 = CARTESIAN_POINT('Ctrl Pts',(-19.1288313007526,12.4711606052726,124.593950499881)) ;
#81148 = CARTESIAN_POINT('Ctrl Pts',(-19.1287877406476,12.4711627121565,124.593940165097)) ;
#81149 = CARTESIAN_POINT('Ctrl Pts',(-19.1287658735658,12.4711637698085,124.593934976417)) ;
#81150 = CARTESIAN_POINT('Ctrl Pts',(-19.1287219607313,12.4711658937555,124.593924555373)) ;
#81151 = CARTESIAN_POINT('Ctrl Pts',(-19.1286999147798,12.4711669600602,124.593919322952)) ;
#81152 = CARTESIAN_POINT('Ctrl Pts',(-19.1286556388924,12.4711691015696,124.593908813134)) ;
#81153 = CARTESIAN_POINT('Ctrl Pts',(-19.1286334095222,12.471170176747,124.593903535861)) ;
#81154 = CARTESIAN_POINT('Ctrl Pts',(-19.1285887619197,12.4711723362378,124.593892935148)) ;
#81155 = CARTESIAN_POINT('Ctrl Pts',(-19.1285663436896,12.4711734205512,124.593887611698)) ;
#81156 = CARTESIAN_POINT('Ctrl Pts',(-19.1285213143905,12.4711755985064,124.593876917652)) ;
#81157 = CARTESIAN_POINT('Ctrl Pts',(-19.1284987019365,12.4711766922152,124.593871546716)) ;
#81158 = CARTESIAN_POINT('Ctrl Pts',(-19.1284532782461,12.4711788892488,124.593860756253)) ;
#81159 = CARTESIAN_POINT('Ctrl Pts',(-19.1284304674776,12.471179992551,124.593855336824)) ;
#81160 = CARTESIAN_POINT('Ctrl Pts',(-19.1283846411428,12.4711822090622,124.593844447908)) ;
#81161 = CARTESIAN_POINT('Ctrl Pts',(-19.1283616261888,12.4711833222417,124.593838978554)) ;
#81162 = CARTESIAN_POINT('Ctrl Pts',(-19.1283153861599,12.4711855587652,124.593827988486)) ;
#81163 = CARTESIAN_POINT('Ctrl Pts',(-19.1282921615205,12.4711866820881,124.593822467862)) ;
#81164 = CARTESIAN_POINT('Ctrl Pts',(-19.1282454979295,12.4711889391012,124.593811374218)) ;
#81165 = CARTESIAN_POINT('Ctrl Pts',(-19.1282220575147,12.4711900728621,124.593805800837)) ;
#81166 = CARTESIAN_POINT('Ctrl Pts',(-19.1281749565108,12.4711923510348,124.593794600243)) ;
#81167 = CARTESIAN_POINT('Ctrl Pts',(-19.1281512957772,12.4711934954536,124.593788972983)) ;
#81168 = CARTESIAN_POINT('Ctrl Pts',(-19.1281037476936,12.4711957952535,124.593777663057)) ;
#81169 = CARTESIAN_POINT('Ctrl Pts',(-19.1280798606057,12.4711969506221,124.593771980439)) ;
#81170 = CARTESIAN_POINT('Ctrl Pts',(-19.1280318538365,12.4711992726108,124.593760558334)) ;
#81171 = CARTESIAN_POINT('Ctrl Pts',(-19.1280077343803,12.4712004392201,124.593754818884)) ;
#81172 = CARTESIAN_POINT('Ctrl Pts',(-19.1279592570408,12.4712027839724,124.593743281681)) ;
#81173 = CARTESIAN_POINT('Ctrl Pts',(-19.1279348991688,12.471203962115,124.593737483915)) ;
#81174 = CARTESIAN_POINT('Ctrl Pts',(-19.1278859382947,12.4712063302582,124.593725828436)) ;
#81175 = CARTESIAN_POINT('Ctrl Pts',(-19.127861336301,12.4712075202101,124.593719970948)) ;
#81176 = CARTESIAN_POINT('Ctrl Pts',(-19.1278118816013,12.4712099122421,124.593708194647)) ;
#81177 = CARTESIAN_POINT('Ctrl Pts',(-19.127787028385,12.4712111143468,124.593702275696)) ;
#81178 = CARTESIAN_POINT('Ctrl Pts',(-19.1277370647114,12.4712135310003,124.593690374866)) ;
#81179 = CARTESIAN_POINT('Ctrl Pts',(-19.1277119547266,12.4712147455262,124.593684393082)) ;
#81180 = CARTESIAN_POINT('Ctrl Pts',(-19.1276614715568,12.4712171873103,124.593672365113)) ;
#81181 = CARTESIAN_POINT('Ctrl Pts',(-19.1276360974865,12.4712184146113,124.5936663187)) ;
#81182 = CARTESIAN_POINT('Ctrl Pts',(-19.12758507883,12.4712208822996,124.593654159675)) ;
#81183 = CARTESIAN_POINT('Ctrl Pts',(-19.1275594350107,12.4712221226497,124.593648047227)) ;
#81184 = CARTESIAN_POINT('Ctrl Pts',(-19.1275078705696,12.4712246167403,124.593635754581)) ;
#81185 = CARTESIAN_POINT('Ctrl Pts',(-19.1274819490489,12.4712258705243,124.593629574148)) ;
#81186 = CARTESIAN_POINT('Ctrl Pts',(-19.127429821882,12.4712283918369,124.593617143726)) ;
#81187 = CARTESIAN_POINT('Ctrl Pts',(-19.127403616693,12.4712296593434,124.593610893826)) ;
#81188 = CARTESIAN_POINT('Ctrl Pts',(-19.1273509150534,12.4712322084463,124.593598322708)) ;
#81189 = CARTESIAN_POINT('Ctrl Pts',(-19.1273244183494,12.4712334900549,124.593592001409)) ;
#81190 = CARTESIAN_POINT('Ctrl Pts',(-19.127271125791,12.4712360677437,124.593579285548)) ;
#81191 = CARTESIAN_POINT('Ctrl Pts',(-19.1272443309084,12.4712373637769,124.593572891197)) ;
#81192 = CARTESIAN_POINT('Ctrl Pts',(-19.1271904355227,12.4712399706277,124.593560027624)) ;
#81193 = CARTESIAN_POINT('Ctrl Pts',(-19.1271633338253,12.4712412815032,124.593553558094)) ;
#81194 = CARTESIAN_POINT('Ctrl Pts',(-19.1271088168654,12.471243918423,124.593540542201)) ;
#81195 = CARTESIAN_POINT('Ctrl Pts',(-19.1270814019424,12.471245244451,124.593533995896)) ;
#81196 = CARTESIAN_POINT('Ctrl Pts',(-19.1270262503819,12.47124791207,124.593520824435)) ;
#81197 = CARTESIAN_POINT('Ctrl Pts',(-19.1269985137445,12.4712492536611,124.593514199256)) ;
#81198 = CARTESIAN_POINT('Ctrl Pts',(-19.1269427109486,12.4712519527842,124.593500868111)) ;
#81199 = CARTESIAN_POINT('Ctrl Pts',(-19.1269146446208,12.4712533103244,124.593494162081)) ;
#81200 = CARTESIAN_POINT('Ctrl Pts',(-19.1232261266058,12.4714317203986,124.59261270678)) ;
#81201 = CARTESIAN_POINT('Ctrl Pts',(-19.1195697518813,12.4716085949165,124.591720952851)) ;
#81202 = CARTESIAN_POINT('Ctrl Pts',(-19.1103423316582,12.4720550570206,124.589424996946)) ;
#81203 = CARTESIAN_POINT('Ctrl Pts',(-19.1047769876549,12.4723244160121,124.587998239301)) ;
#81204 = CARTESIAN_POINT('Ctrl Pts',(-19.0879711285919,12.4731383198285,124.58356253251)) ;
#81205 = CARTESIAN_POINT('Ctrl Pts',(-19.0767635106322,12.4736817661215,124.580431520676)) ;
#81206 = CARTESIAN_POINT('Ctrl Pts',(-19.0368958163013,12.4756210993441,124.568673913459)) ;
#81207 = CARTESIAN_POINT('Ctrl Pts',(-19.0085119642555,12.4770157746918,124.559150060454)) ;
#81208 = CARTESIAN_POINT('Ctrl Pts',(-18.9746763427525,12.4787134502845,124.546387936201)) ;
#81209 = CARTESIAN_POINT('Ctrl Pts',(-18.9688611373116,12.4790064217359,124.5441432864)) ;
#81210 = CARTESIAN_POINT('Ctrl Pts',(-18.9588898776629,12.4795109142169,124.540205978949)) ;
#81211 = CARTESIAN_POINT('Ctrl Pts',(-18.9547254475909,12.4797222578357,124.538534861522)) ;
#81212 = CARTESIAN_POINT('Ctrl Pts',(-18.9478449624896,12.4800725258619,124.535729480526)) ;
#81213 = CARTESIAN_POINT('Ctrl Pts',(-18.9451235967112,12.4802113462035,124.534608347498)) ;
#81214 = CARTESIAN_POINT('Ctrl Pts',(-18.9422116026113,12.4803601949877,124.533396284159)) ;
#81215 = CARTESIAN_POINT('Ctrl Pts',(-18.9420168913035,12.4803701492635,124.533315179704)) ;
#81216 = CARTESIAN_POINT('Ctrl Pts',(-18.9416692924694,12.4803879222542,124.533170285704)) ;
#81217 = CARTESIAN_POINT('Ctrl Pts',(-18.9415163966919,12.4803957408314,124.533106515523)) ;
#81218 = CARTESIAN_POINT('Ctrl Pts',(-18.9365214095347,12.4806511971551,124.531021993401)) ;
#81219 = CARTESIAN_POINT('Ctrl Pts',(-18.9316924566339,12.4808990667659,124.52896993135)) ;
#81220 = CARTESIAN_POINT('Ctrl Pts',(-18.9209181544401,12.4814541312749,124.524308767695)) ;
#81221 = CARTESIAN_POINT('Ctrl Pts',(-18.9149801246699,12.4817614309349,124.52168316034)) ;
#81222 = CARTESIAN_POINT('Ctrl Pts',(-18.8979819526725,12.482645017007,124.514003633592)) ;
#81223 = CARTESIAN_POINT('Ctrl Pts',(-18.886976281193,12.4832219170089,124.508831105724)) ;
#81224 = CARTESIAN_POINT('Ctrl Pts',(-18.8555607774336,12.4848813326728,124.493486263975)) ;
#81225 = CARTESIAN_POINT('Ctrl Pts',(-18.8353570774093,12.4859634097558,124.482903333363)) ;
#81226 = CARTESIAN_POINT('Ctrl Pts',(-18.8076378391511,12.4874660048555,124.467374050866)) ;
#81227 = CARTESIAN_POINT('Ctrl Pts',(-18.7998613557678,12.4878897221409,124.462903536099)) ;
#81228 = CARTESIAN_POINT('Ctrl Pts',(-18.7917291756995,12.4883352844162,124.458107947052)) ;
#81229 = CARTESIAN_POINT('Ctrl Pts',(-18.7913234166414,12.4883575224754,124.45786835055)) ;
#81230 = CARTESIAN_POINT('Ctrl Pts',(-18.782935937589,12.4888173425152,124.452909048009)) ;
#81231 = CARTESIAN_POINT('Ctrl Pts',(-18.7750083563902,12.4892544799009,124.448098343911)) ;
#81232 = CARTESIAN_POINT('Ctrl Pts',(-18.750443398737,12.4906176759226,124.432804058551)) ;
#81233 = CARTESIAN_POINT('Ctrl Pts',(-18.7340049644258,12.4915423969222,124.422007006939)) ;
#81234 = CARTESIAN_POINT('Ctrl Pts',(-18.7064803172295,12.4931172500784,124.402956142816)) ;
#81235 = CARTESIAN_POINT('Ctrl Pts',(-18.6952596669294,12.4937670770598,124.394903527791)) ;
#81236 = CARTESIAN_POINT('Ctrl Pts',(-18.6837845615061,12.4944411533968,124.386368179618)) ;
#81237 = CARTESIAN_POINT('Ctrl Pts',(-18.6833905324445,12.4944643114425,124.386074723732)) ;
#81238 = CARTESIAN_POINT('Ctrl Pts',(-18.6826028318842,12.4945106302433,124.385487335101)) ;
#81239 = CARTESIAN_POINT('Ctrl Pts',(-18.6822091605129,12.494533790991,124.385193402452)) ;
#81240 = CARTESIAN_POINT('Ctrl Pts',(-18.6813842104247,12.4945823500495,124.384576678119)) ;
#81241 = CARTESIAN_POINT('Ctrl Pts',(-18.6809529678954,12.4946077486456,124.384253838228)) ;
#81242 = CARTESIAN_POINT('Ctrl Pts',(-18.6799932412372,12.4946643051737,124.383534364191)) ;
#81243 = CARTESIAN_POINT('Ctrl Pts',(-18.6794648657086,12.4946954639981,124.383137585527)) ;
#81244 = CARTESIAN_POINT('Ctrl Pts',(-18.6779865849993,12.4947827010053,124.382025597215)) ;
#81245 = CARTESIAN_POINT('Ctrl Pts',(-18.677037405952,12.4948387854086,124.381309424007)) ;
#81246 = CARTESIAN_POINT('Ctrl Pts',(-18.6722650589083,12.4951211326779,124.377697592794)) ;
#81247 = CARTESIAN_POINT('Ctrl Pts',(-18.6684580193074,12.4953475423961,124.374780715562)) ;
#81248 = CARTESIAN_POINT('Ctrl Pts',(-18.6604677729949,12.4958253390172,124.368583319832)) ;
#81249 = CARTESIAN_POINT('Ctrl Pts',(-18.6562886328926,12.4960767535579,124.365297739247)) ;
#81250 = CARTESIAN_POINT('Ctrl Pts',(-18.6426423991322,12.4969024371642,124.354423587546)) ;
#81251 = CARTESIAN_POINT('Ctrl Pts',(-18.6332674052875,12.4974772121036,124.346720620794)) ;
#81252 = CARTESIAN_POINT('Ctrl Pts',(-18.6128213228358,12.4987461124564,124.329401614334)) ;
#81253 = CARTESIAN_POINT('Ctrl Pts',(-18.6018057200431,12.4994400176587,124.319722911731)) ;
#81254 = CARTESIAN_POINT('Ctrl Pts',(-18.5857958141577,12.5004632501538,124.305134119495)) ;
#81255 = CARTESIAN_POINT('Ctrl Pts',(-18.5806644593845,12.500793525911,124.300376460262)) ;
#81256 = CARTESIAN_POINT('Ctrl Pts',(-18.5713587859075,12.5013967716912,124.29159776347)) ;
#81257 = CARTESIAN_POINT('Ctrl Pts',(-18.5671715935793,12.5016698335591,124.287590679762)) ;
#81258 = CARTESIAN_POINT('Ctrl Pts',(-18.5618209024629,12.5020209113366,124.28239628705)) ;
#81259 = CARTESIAN_POINT('Ctrl Pts',(-18.5606309545955,12.5020991258231,124.28123634692)) ;
#81260 = CARTESIAN_POINT('Ctrl Pts',(-18.5543858940395,12.5025103405062,124.275123734655)) ;
#81261 = CARTESIAN_POINT('Ctrl Pts',(-18.5493717386309,12.5028430273277,124.270129396785)) ;
#81262 = CARTESIAN_POINT('Ctrl Pts',(-18.5284640589082,12.5042413584933,124.248937226405)) ;
#81263 = CARTESIAN_POINT('Ctrl Pts',(-18.5129823544157,12.5053039620752,124.232339575367)) ;
#81264 = CARTESIAN_POINT('Ctrl Pts',(-18.4863040867395,12.5071951944769,124.202081646359)) ;
#81265 = CARTESIAN_POINT('Ctrl Pts',(-18.4749234280842,12.5080231961958,124.18859259609)) ;
#81266 = CARTESIAN_POINT('Ctrl Pts',(-18.4589052683812,12.5092228190037,124.168745283165)) ;
#81267 = CARTESIAN_POINT('Ctrl Pts',(-18.4540293329917,12.5095927906,124.162582352647)) ;
#81268 = CARTESIAN_POINT('Ctrl Pts',(-18.4451010183587,12.5102794371518,124.151069612642)) ;
#81269 = CARTESIAN_POINT('Ctrl Pts',(-18.4410325098955,12.5105959926255,124.145732688638)) ;
#81270 = CARTESIAN_POINT('Ctrl Pts',(-18.4319243444403,12.5113131107076,124.133577345849)) ;
#81271 = CARTESIAN_POINT('Ctrl Pts',(-18.4269114297649,12.5117138190335,124.12673933283)) ;
#81272 = CARTESIAN_POINT('Ctrl Pts',(-18.4154053814133,12.5126478019861,124.110694617467)) ;
#81273 = CARTESIAN_POINT('Ctrl Pts',(-18.4089679150352,12.5131813155171,124.101448958921)) ;
#81274 = CARTESIAN_POINT('Ctrl Pts',(-18.3872211798402,12.5150216325441,124.069270405564)) ;
#81275 = CARTESIAN_POINT('Ctrl Pts',(-18.3725644548256,12.5163287249421,124.045906607494)) ;
#81276 = CARTESIAN_POINT('Ctrl Pts',(-18.3540578587316,12.5180699633502,124.014046222899)) ;
#81277 = CARTESIAN_POINT('Ctrl Pts',(-18.3494923448433,12.5185077432531,124.005975023411)) ;
#81278 = CARTESIAN_POINT('Ctrl Pts',(-18.3402562835985,12.5194109507599,123.989201704953)) ;
#81279 = CARTESIAN_POINT('Ctrl Pts',(-18.3355985429631,12.5198762912002,123.980493304886)) ;
#81280 = CARTESIAN_POINT('Ctrl Pts',(-18.3255776593783,12.5209001906639,123.961195524633)) ;
#81281 = CARTESIAN_POINT('Ctrl Pts',(-18.320262483917,12.5214585425504,123.950582378729)) ;
#81282 = CARTESIAN_POINT('Ctrl Pts',(-18.3071838860961,12.5228738705007,123.923482857499)) ;
#81283 = CARTESIAN_POINT('Ctrl Pts',(-18.2996343075352,12.5237305022439,123.906896621364)) ;
#81284 = CARTESIAN_POINT('Ctrl Pts',(-18.290383698556,12.5248379598755,123.885297464845)) ;
#81285 = CARTESIAN_POINT('Ctrl Pts',(-18.2883383557618,12.52508678507,123.880434535276)) ;
#81286 = CARTESIAN_POINT('Ctrl Pts',(-18.2846466134175,12.5255434556328,123.871494700197)) ;
#81287 = CARTESIAN_POINT('Ctrl Pts',(-18.2829905486527,12.5257512314104,123.867421886359)) ;
#81288 = CARTESIAN_POINT('Ctrl Pts',(-18.2736868532533,12.5269351294952,123.844180231193)) ;
#81289 = CARTESIAN_POINT('Ctrl Pts',(-18.2665099269775,12.5279132636302,123.824837367136)) ;
#81290 = CARTESIAN_POINT('Ctrl Pts',(-18.259825879779,12.5288903030032,123.80531165987)) ;
#81291 = CARTESIAN_POINT('',(-20.0599602754258,12.4073831970672,124.437819810756)) ;
#81292 = CARTESIAN_POINT('Origin',(-19.4092696390626,12.4073831970673,123.411833654984)) ;
#81293 = CARTESIAN_POINT('Ctrl Pts',(-18.259825879779,12.510900730771,123.80531165987)) ;
#81294 = CARTESIAN_POINT('Ctrl Pts',(-18.2708779448963,12.5092744369586,123.837597396604)) ;
#81295 = CARTESIAN_POINT('Ctrl Pts',(-18.2832817189336,12.5076394659094,123.869394206438)) ;
#81296 = CARTESIAN_POINT('Ctrl Pts',(-18.2992643795568,12.5057525469584,123.905762369247)) ;
#81297 = CARTESIAN_POINT('Ctrl Pts',(-18.3015526664204,12.5054869325776,123.910873092127)) ;
#81298 = CARTESIAN_POINT('Ctrl Pts',(-18.3054234465231,12.5050450941351,123.919360385976)) ;
#81299 = CARTESIAN_POINT('Ctrl Pts',(-18.3069862945246,12.5048686558078,123.922745807838)) ;
#81300 = CARTESIAN_POINT('Ctrl Pts',(-18.3098741739523,12.5045461653814,123.928926563957)) ;
#81301 = CARTESIAN_POINT('Ctrl Pts',(-18.3111943424549,12.5044000593755,123.931724132168)) ;
#81302 = CARTESIAN_POINT('Ctrl Pts',(-18.3138334545042,12.5041105663035,123.937261774729)) ;
#81303 = CARTESIAN_POINT('Ctrl Pts',(-18.3151520294746,12.5039671761994,123.940001999279)) ;
#81304 = CARTESIAN_POINT('Ctrl Pts',(-18.3182412047487,12.5036341061789,123.946360622662)) ;
#81305 = CARTESIAN_POINT('Ctrl Pts',(-18.3200195422345,12.5034445157386,123.949975225918)) ;
#81306 = CARTESIAN_POINT('Ctrl Pts',(-18.3254992350252,12.5028667432464,123.960974658897)) ;
#81307 = CARTESIAN_POINT('Ctrl Pts',(-18.3292579646782,12.5024791994803,123.968330658708)) ;
#81308 = CARTESIAN_POINT('Ctrl Pts',(-18.336071983817,12.5017914708978,123.981336893299)) ;
#81309 = CARTESIAN_POINT('Ctrl Pts',(-18.3390976015429,12.5014910431626,123.987002287794)) ;
#81310 = CARTESIAN_POINT('Ctrl Pts',(-18.3426787219295,12.5011409439048,123.993581755835)) ;
#81311 = CARTESIAN_POINT('Ctrl Pts',(-18.3431906737507,12.501091022387,123.994519399683)) ;
#81312 = CARTESIAN_POINT('Ctrl Pts',(-18.3538246731278,12.5000567097751,124.013934726689)) ;
#81313 = CARTESIAN_POINT('Ctrl Pts',(-18.3644243786652,12.4990749671909,124.032146609859)) ;
#81314 = CARTESIAN_POINT('Ctrl Pts',(-18.3834785611712,12.4973778425946,124.063009258256)) ;
#81315 = CARTESIAN_POINT('Ctrl Pts',(-18.3917067937197,12.4966650314769,124.075793633516)) ;
#81316 = CARTESIAN_POINT('Ctrl Pts',(-18.4037481589575,12.4956488473075,124.093752762712)) ;
#81317 = CARTESIAN_POINT('Ctrl Pts',(-18.4073658038323,12.495346838339,124.099056923694)) ;
#81318 = CARTESIAN_POINT('Ctrl Pts',(-18.4125732647053,12.4949166911301,124.106563536787)) ;
#81319 = CARTESIAN_POINT('Ctrl Pts',(-18.414128691141,12.4947887793874,124.108789726105)) ;
#81320 = CARTESIAN_POINT('Ctrl Pts',(-18.4194374626593,12.4943541279479,124.116333851243)) ;
#81321 = CARTESIAN_POINT('Ctrl Pts',(-18.4232260690798,12.4940471694145,124.121626823271)) ;
#81322 = CARTESIAN_POINT('Ctrl Pts',(-18.4321525980218,12.4933313216252,124.133888459256)) ;
#81323 = CARTESIAN_POINT('Ctrl Pts',(-18.4373228367532,12.4929222536337,124.140833150909)) ;
#81324 = CARTESIAN_POINT('Ctrl Pts',(-18.4565933846306,12.4914175510375,124.166147987438)) ;
#81325 = CARTESIAN_POINT('Ctrl Pts',(-18.4711438126358,12.4903196927723,124.184169128002)) ;
#81326 = CARTESIAN_POINT('Ctrl Pts',(-18.49881615561,12.4882995824613,124.21650554077)) ;
#81327 = CARTESIAN_POINT('Ctrl Pts',(-18.5117833978879,12.4873779827832,124.230943439137)) ;
#81328 = CARTESIAN_POINT('Ctrl Pts',(-18.5286842312663,12.4862096697275,124.248877672681)) ;
#81329 = CARTESIAN_POINT('Ctrl Pts',(-18.5323022321512,12.4859613973245,124.252667476463)) ;
#81330 = CARTESIAN_POINT('Ctrl Pts',(-18.5419511153411,12.4853041266909,124.262644518653)) ;
#81331 = CARTESIAN_POINT('Ctrl Pts',(-18.5480236877417,12.4848954183119,124.268791039838)) ;
#81332 = CARTESIAN_POINT('Ctrl Pts',(-18.5574998585772,12.4842651971188,124.278180135829)) ;
#81333 = CARTESIAN_POINT('Ctrl Pts',(-18.5608575642792,12.4840433228017,124.281468598696)) ;
#81334 = CARTESIAN_POINT('Ctrl Pts',(-18.5682245407831,12.4835596122474,124.288600375835)) ;
#81335 = CARTESIAN_POINT('Ctrl Pts',(-18.5722412573361,12.4832978462156,124.292435851528)) ;
#81336 = CARTESIAN_POINT('Ctrl Pts',(-18.58171967871,12.4826846806696,124.301363144904)) ;
#81337 = CARTESIAN_POINT('Ctrl Pts',(-18.5872023114967,12.4823334807318,124.306432425294)) ;
#81338 = CARTESIAN_POINT('Ctrl Pts',(-18.6079289068811,12.4810184089763,124.325244936789)) ;
#81339 = CARTESIAN_POINT('Ctrl Pts',(-18.6234736251106,12.480057459793,124.338651744565)) ;
#81340 = CARTESIAN_POINT('Ctrl Pts',(-18.6603748226619,12.4778267614658,124.368881780136)) ;
#81341 = CARTESIAN_POINT('Ctrl Pts',(-18.6819710535665,12.4765580511313,124.385394811009)) ;
#81342 = CARTESIAN_POINT('Ctrl Pts',(-18.7128568840371,12.4747820521826,124.407409235582)) ;
#81343 = CARTESIAN_POINT('Ctrl Pts',(-18.7216933348196,12.4742781689636,124.41353235549)) ;
#81344 = CARTESIAN_POINT('Ctrl Pts',(-18.7359840832137,12.4734693234892,124.423156767871)) ;
#81345 = CARTESIAN_POINT('Ctrl Pts',(-18.7413871662192,12.4731648753908,124.426733098517)) ;
#81346 = CARTESIAN_POINT('Ctrl Pts',(-18.7470482306654,12.4728472203578,124.430415403002)) ;
#81347 = CARTESIAN_POINT('Ctrl Pts',(-18.7472779247224,12.4728343339784,124.430564699607)) ;
#81348 = CARTESIAN_POINT('Ctrl Pts',(-18.7477292637262,12.4728090172404,124.430857843953)) ;
#81349 = CARTESIAN_POINT('Ctrl Pts',(-18.7479509051141,12.4727965869237,124.431001697082)) ;
#81350 = CARTESIAN_POINT('Ctrl Pts',(-18.7483872392515,12.4727721201238,124.431284691159)) ;
#81351 = CARTESIAN_POINT('Ctrl Pts',(-18.7486019290304,12.4727600836758,124.431423836606)) ;
#81352 = CARTESIAN_POINT('Ctrl Pts',(-18.7490253876303,12.472736346606,124.431698100083)) ;
#81353 = CARTESIAN_POINT('Ctrl Pts',(-18.7492341539641,12.4727246460152,124.431833221816)) ;
#81354 = CARTESIAN_POINT('Ctrl Pts',(-18.7496467346263,12.4727015260305,124.432100080445)) ;
#81355 = CARTESIAN_POINT('Ctrl Pts',(-18.7498505469923,12.4726901066585,124.432231820405)) ;
#81356 = CARTESIAN_POINT('Ctrl Pts',(-18.7502541434033,12.4726674970954,124.432492525083)) ;
#81357 = CARTESIAN_POINT('Ctrl Pts',(-18.750453926018,12.4726563069143,124.432621492332)) ;
#81358 = CARTESIAN_POINT('Ctrl Pts',(-18.750850355263,12.4726341055428,124.432877237574)) ;
#81359 = CARTESIAN_POINT('Ctrl Pts',(-18.7510470005906,12.4726230943717,124.433004017378)) ;
#81360 = CARTESIAN_POINT('Ctrl Pts',(-18.7514380283173,12.4726012019729,124.433255958167)) ;
#81361 = CARTESIAN_POINT('Ctrl Pts',(-18.7516324098492,12.4725903207555,124.433381120493)) ;
#81362 = CARTESIAN_POINT('Ctrl Pts',(-18.75201977778,12.472568639572,124.433630390434)) ;
#81363 = CARTESIAN_POINT('Ctrl Pts',(-18.7522127636392,12.4725578396122,124.433754498881)) ;
#81364 = CARTESIAN_POINT('Ctrl Pts',(-18.7525982166654,12.4725362718256,124.434002227881)) ;
#81365 = CARTESIAN_POINT('Ctrl Pts',(-18.7527906836682,12.4725255039984,124.434125848799)) ;
#81366 = CARTESIAN_POINT('Ctrl Pts',(-18.7531760000206,12.4725039500395,124.434373182528)) ;
#81367 = CARTESIAN_POINT('Ctrl Pts',(-18.7533688493787,12.4724931639124,124.434496895094)) ;
#81368 = CARTESIAN_POINT('Ctrl Pts',(-18.7537558726141,12.4724715206736,124.434745015397)) ;
#81369 = CARTESIAN_POINT('Ctrl Pts',(-18.7539500469856,12.4724606635546,124.434869422446)) ;
#81370 = CARTESIAN_POINT('Ctrl Pts',(-18.7543407243061,12.472438822253,124.435119571591)) ;
#81371 = CARTESIAN_POINT('Ctrl Pts',(-18.754537228102,12.4724278380596,124.435245312406)) ;
#81372 = CARTESIAN_POINT('Ctrl Pts',(-18.7549336540121,12.4724056818063,124.435498820478)) ;
#81373 = CARTESIAN_POINT('Ctrl Pts',(-18.7551335773291,12.472394509734,124.435626585766)) ;
#81374 = CARTESIAN_POINT('Ctrl Pts',(-18.7555380464852,12.4723719105972,124.435884903621)) ;
#81375 = CARTESIAN_POINT('Ctrl Pts',(-18.7557425941155,12.4723604835081,124.436015453539)) ;
#81376 = CARTESIAN_POINT('Ctrl Pts',(-18.7560159732782,12.4723452134236,124.436189819061)) ;
#81377 = CARTESIAN_POINT('Ctrl Pts',(-18.7560847700556,12.4723413708497,124.436233688976)) ;
#81378 = CARTESIAN_POINT('Ctrl Pts',(-18.7600925339082,12.4721175325591,124.438788767859)) ;
#81379 = CARTESIAN_POINT('Ctrl Pts',(-18.764045939796,12.4718973645067,124.441277240356)) ;
#81380 = CARTESIAN_POINT('Ctrl Pts',(-18.7719793798138,12.4714567583463,124.44620729276)) ;
#81381 = CARTESIAN_POINT('Ctrl Pts',(-18.77595933397,12.4712363241106,124.448648852768)) ;
#81382 = CARTESIAN_POINT('Ctrl Pts',(-18.7852393099155,12.4707236865584,124.454268417085)) ;
#81383 = CARTESIAN_POINT('Ctrl Pts',(-18.7905496953622,12.4704313438977,124.45742904317)) ;
#81384 = CARTESIAN_POINT('Ctrl Pts',(-18.8126117980378,12.4692207609752,124.470333000411)) ;
#81385 = CARTESIAN_POINT('Ctrl Pts',(-18.8295711590067,12.4682990129185,124.479715250224)) ;
#81386 = CARTESIAN_POINT('Ctrl Pts',(-18.8734329820549,12.4659403416845,124.502627588803)) ;
#81387 = CARTESIAN_POINT('Ctrl Pts',(-18.9006275205337,12.4645028407894,124.515570733043)) ;
#81388 = CARTESIAN_POINT('Ctrl Pts',(-18.9389095396364,12.4625197033815,124.532075322591)) ;
#81389 = CARTESIAN_POINT('Ctrl Pts',(-18.9496093799162,12.46196959824,124.536508036815)) ;
#81390 = CARTESIAN_POINT('Ctrl Pts',(-18.9689435129936,12.4609830805354,124.544195746187)) ;
#81391 = CARTESIAN_POINT('Ctrl Pts',(-18.9775546023812,12.4605463327404,124.547506641006)) ;
#81392 = CARTESIAN_POINT('Ctrl Pts',(-18.9895041541243,12.4599438014985,124.551945596068)) ;
#81393 = CARTESIAN_POINT('Ctrl Pts',(-18.9928110353211,12.4597774302085,124.553157680835)) ;
#81394 = CARTESIAN_POINT('Ctrl Pts',(-18.996214072409,12.4596065967133,124.554388250743)) ;
#81395 = CARTESIAN_POINT('Ctrl Pts',(-18.9963050038545,12.459602032202,124.554421120127)) ;
#81396 = CARTESIAN_POINT('Ctrl Pts',(-18.9964908640187,12.4595927030888,124.55448827872)) ;
#81397 = CARTESIAN_POINT('Ctrl Pts',(-18.9965857928986,12.4595879385034,124.554522566888)) ;
#81398 = CARTESIAN_POINT('Ctrl Pts',(-18.9967798262084,12.4595782003688,124.554592624093)) ;
#81399 = CARTESIAN_POINT('Ctrl Pts',(-18.9968789312626,12.4595732268151,124.554628392156)) ;
#81400 = CARTESIAN_POINT('Ctrl Pts',(-18.9970815029335,12.4595630614902,124.554701472633)) ;
#81401 = CARTESIAN_POINT('Ctrl Pts',(-18.9971849699443,12.4595578697285,124.554738783882)) ;
#81402 = CARTESIAN_POINT('Ctrl Pts',(-18.9973964592291,12.4595472583568,124.554815016601)) ;
#81403 = CARTESIAN_POINT('Ctrl Pts',(-18.9975044818939,12.4595418387591,124.554853936786)) ;
#81404 = CARTESIAN_POINT('Ctrl Pts',(-18.9976716361686,12.4595334530715,124.554914135112)) ;
#81405 = CARTESIAN_POINT('Ctrl Pts',(-18.9977307640803,12.4595304868965,124.554935424038)) ;
#81406 = CARTESIAN_POINT('Ctrl Pts',(-18.9978625418105,12.4595238764725,124.554982858884)) ;
#81407 = CARTESIAN_POINT('Ctrl Pts',(-18.9979351925447,12.4595202322367,124.555009002494)) ;
#81408 = CARTESIAN_POINT('Ctrl Pts',(-18.9980970183312,12.4595121152772,124.555067218622)) ;
#81409 = CARTESIAN_POINT('Ctrl Pts',(-18.9981861943902,12.4595076425915,124.55509928754)) ;
#81410 = CARTESIAN_POINT('Ctrl Pts',(-18.998384692849,12.459497687352,124.555170644045)) ;
#81411 = CARTESIAN_POINT('Ctrl Pts',(-18.9984940173644,12.4594922048242,124.555209926471)) ;
#81412 = CARTESIAN_POINT('Ctrl Pts',(-18.9987371590971,12.4594800123597,124.555297252653)) ;
#81413 = CARTESIAN_POINT('Ctrl Pts',(-18.9988709789515,12.4594733024872,124.555345288541)) ;
#81414 = CARTESIAN_POINT('Ctrl Pts',(-18.9991682898217,12.4594583963113,124.555451952146)) ;
#81415 = CARTESIAN_POINT('Ctrl Pts',(-18.9993317849728,12.4594502000914,124.555510568293)) ;
#81416 = CARTESIAN_POINT('Ctrl Pts',(-18.9996945609775,12.4594320156238,124.555640542663)) ;
#81417 = CARTESIAN_POINT('Ctrl Pts',(-18.9998938479544,12.4594220274967,124.555711883881)) ;
#81418 = CARTESIAN_POINT('Ctrl Pts',(-19.0002851411589,12.459402418715,124.555851844584)) ;
#81419 = CARTESIAN_POINT('Ctrl Pts',(-19.0004771460836,12.4593927980315,124.555920467837)) ;
#81420 = CARTESIAN_POINT('Ctrl Pts',(-19.0012197128852,12.4593555953361,124.556185653098)) ;
#81421 = CARTESIAN_POINT('Ctrl Pts',(-19.0017703994541,12.4593280158234,124.556381866096)) ;
#81422 = CARTESIAN_POINT('Ctrl Pts',(-19.0038154036166,12.4592256346692,124.557108850624)) ;
#81423 = CARTESIAN_POINT('Ctrl Pts',(-19.0053106166825,12.4591508512919,124.557637093195)) ;
#81424 = CARTESIAN_POINT('Ctrl Pts',(-19.0117012259222,12.4588315326549,124.559880762249)) ;
#81425 = CARTESIAN_POINT('Ctrl Pts',(-19.0166065571016,12.4585872025792,124.561567758131)) ;
#81426 = CARTESIAN_POINT('Ctrl Pts',(-19.0216270026011,12.4583379011671,124.563258465656)) ;
#81427 = CARTESIAN_POINT('Ctrl Pts',(-19.0217314584802,12.4583327145136,124.563293626856)) ;
#81428 = CARTESIAN_POINT('Ctrl Pts',(-19.0219415633262,12.4583222826406,124.563364319038)) ;
#81429 = CARTESIAN_POINT('Ctrl Pts',(-19.0220472124483,12.4583170374209,124.56339984971)) ;
#81430 = CARTESIAN_POINT('Ctrl Pts',(-19.0222598164606,12.4583064828437,124.563471317631)) ;
#81431 = CARTESIAN_POINT('Ctrl Pts',(-19.0223667713187,12.4583011734964,124.563507254468)) ;
#81432 = CARTESIAN_POINT('Ctrl Pts',(-19.0225821018788,12.4582904849767,124.563579572164)) ;
#81433 = CARTESIAN_POINT('Ctrl Pts',(-19.0226904779518,12.4582851057953,124.563615952708)) ;
#81434 = CARTESIAN_POINT('Ctrl Pts',(-19.0229087692449,12.4582742717634,124.563689196187)) ;
#81435 = CARTESIAN_POINT('Ctrl Pts',(-19.0230186846185,12.4582688169156,124.563726058691)) ;
#81436 = CARTESIAN_POINT('Ctrl Pts',(-19.0232401763883,12.458257825533,124.563800305491)) ;
#81437 = CARTESIAN_POINT('Ctrl Pts',(-19.023351752842,12.4582522890066,124.563837689277)) ;
#81438 = CARTESIAN_POINT('Ctrl Pts',(-19.023576692188,12.458241128077,124.563913019051)) ;
#81439 = CARTESIAN_POINT('Ctrl Pts',(-19.0236900554059,12.4582355036699,124.563950964568)) ;
#81440 = CARTESIAN_POINT('Ctrl Pts',(-19.0239186981324,12.4582241605729,124.564027459509)) ;
#81441 = CARTESIAN_POINT('Ctrl Pts',(-19.0240339776838,12.4582184418942,124.564066008315)) ;
#81442 = CARTESIAN_POINT('Ctrl Pts',(-19.0242665875078,12.4582069036251,124.564143752866)) ;
#81443 = CARTESIAN_POINT('Ctrl Pts',(-19.0243839179028,12.4582010840432,124.564182947966)) ;
#81444 = CARTESIAN_POINT('Ctrl Pts',(-19.0246207686207,12.458189337106,124.564262029517)) ;
#81445 = CARTESIAN_POINT('Ctrl Pts',(-19.0247402893849,12.4581834097448,124.564301915371)) ;
#81446 = CARTESIAN_POINT('Ctrl Pts',(-19.0249816658408,12.4581714401052,124.564382424547)) ;
#81447 = CARTESIAN_POINT('Ctrl Pts',(-19.0251035216686,12.4581653978372,124.564423047106)) ;
#81448 = CARTESIAN_POINT('Ctrl Pts',(-19.025349719219,12.4581531909493,124.564505077554)) ;
#81449 = CARTESIAN_POINT('Ctrl Pts',(-19.0254740611223,12.4581470263391,124.564546484623)) ;
#81450 = CARTESIAN_POINT('Ctrl Pts',(-19.0257253879984,12.4581345670296,124.564630133757)) ;
#81451 = CARTESIAN_POINT('Ctrl Pts',(-19.0258523733336,12.4581282723326,124.564672374986)) ;
#81452 = CARTESIAN_POINT('Ctrl Pts',(-19.0261091513439,12.4581155447667,124.564757744178)) ;
#81453 = CARTESIAN_POINT('Ctrl Pts',(-19.0262389442418,12.4581091119085,124.564800871177)) ;
#81454 = CARTESIAN_POINT('Ctrl Pts',(-19.0265015090463,12.4580960995771,124.564888065799)) ;
#81455 = CARTESIAN_POINT('Ctrl Pts',(-19.0266342813408,12.4580895201082,124.564932132425)) ;
#81456 = CARTESIAN_POINT('Ctrl Pts',(-19.0269029846112,12.4580762057221,124.565021262512)) ;
#81457 = CARTESIAN_POINT('Ctrl Pts',(-19.0270389159778,12.4580694708111,124.565066324884)) ;
#81458 = CARTESIAN_POINT('Ctrl Pts',(-19.0364123898857,12.4576050873161,124.568171869593)) ;
#81459 = CARTESIAN_POINT('Ctrl Pts',(-19.045686391355,12.4571482136245,124.571121288879)) ;
#81460 = CARTESIAN_POINT('Ctrl Pts',(-19.0676006511695,12.4560741305134,124.57780186751)) ;
#81461 = CARTESIAN_POINT('Ctrl Pts',(-19.0802681764214,12.4554575338223,124.58143940474)) ;
#81462 = CARTESIAN_POINT('Ctrl Pts',(-19.1221287196726,12.4534313825446,124.592725955992)) ;
#81463 = CARTESIAN_POINT('Ctrl Pts',(-19.1515475027644,12.4520259695632,124.599493465862)) ;
#81464 = CARTESIAN_POINT('Ctrl Pts',(-19.1926036909814,12.4500710253046,124.607340598084)) ;
#81465 = CARTESIAN_POINT('Ctrl Pts',(-19.2040504531208,12.4495265908159,124.609358630735)) ;
#81466 = CARTESIAN_POINT('Ctrl Pts',(-19.2205777903511,12.448739951088,124.61202842498)) ;
#81467 = CARTESIAN_POINT('Ctrl Pts',(-19.2256363232185,12.4484991162218,124.612812799154)) ;
#81468 = CARTESIAN_POINT('Ctrl Pts',(-19.235307100479,12.4480386298423,124.614249817801)) ;
#81469 = CARTESIAN_POINT('Ctrl Pts',(-19.2399184430646,12.4478190270199,124.614907952638)) ;
#81470 = CARTESIAN_POINT('Ctrl Pts',(-19.2495396099516,12.4473608353244,124.616224681586)) ;
#81471 = CARTESIAN_POINT('Ctrl Pts',(-19.2545499899835,12.4471222192283,124.616878574135)) ;
#81472 = CARTESIAN_POINT('Ctrl Pts',(-19.2755098960883,12.44612410801,124.619481124076)) ;
#81473 = CARTESIAN_POINT('Ctrl Pts',(-19.2914931641354,12.4453632273878,124.621144523827)) ;
#81474 = CARTESIAN_POINT('Ctrl Pts',(-19.3400199729492,12.4430558625448,124.625223573964)) ;
#81475 = CARTESIAN_POINT('Ctrl Pts',(-19.3726323283655,12.4415093022874,124.62664571233)) ;
#81476 = CARTESIAN_POINT('Ctrl Pts',(-19.4146372795782,12.4395243298544,124.626784260741)) ;
#81477 = CARTESIAN_POINT('Ctrl Pts',(-19.4240122513541,12.4390817367332,124.626706669822)) ;
#81478 = CARTESIAN_POINT('Ctrl Pts',(-19.4479262366249,12.4379535630246,124.62623189385)) ;
#81479 = CARTESIAN_POINT('Ctrl Pts',(-19.4624607378427,12.4372685471284,124.625682131427)) ;
#81480 = CARTESIAN_POINT('Ctrl Pts',(-19.505739744189,12.4352276028772,124.623266280612)) ;
#81481 = CARTESIAN_POINT('Ctrl Pts',(-19.5344313832049,12.4338729142859,124.620638858866)) ;
#81482 = CARTESIAN_POINT('Ctrl Pts',(-19.5732441652108,12.4320281066831,124.615687820181)) ;
#81483 = CARTESIAN_POINT('Ctrl Pts',(-19.5834688212528,12.4315409686251,124.614250862273)) ;
#81484 = CARTESIAN_POINT('Ctrl Pts',(-19.6033923191214,12.43058891903,124.611191381478)) ;
#81485 = CARTESIAN_POINT('Ctrl Pts',(-19.6130922438604,12.4301240908056,124.609581089074)) ;
#81486 = CARTESIAN_POINT('Ctrl Pts',(-19.6332590674186,12.4291544519405,124.605981102098)) ;
#81487 = CARTESIAN_POINT('Ctrl Pts',(-19.6437214872329,12.4286494617801,124.60397111297)) ;
#81488 = CARTESIAN_POINT('Ctrl Pts',(-19.6763822536025,12.4270679706454,124.597249898521)) ;
#81489 = CARTESIAN_POINT('Ctrl Pts',(-19.698476044724,12.4259914549365,124.592054178708)) ;
#81490 = CARTESIAN_POINT('Ctrl Pts',(-19.7266697639441,12.4246125401667,124.584584682613)) ;
#81491 = CARTESIAN_POINT('Ctrl Pts',(-19.7329147663155,12.4243067478347,124.58287662775)) ;
#81492 = CARTESIAN_POINT('Ctrl Pts',(-19.7431366683324,12.4238056288648,124.579992846724)) ;
#81493 = CARTESIAN_POINT('Ctrl Pts',(-19.7471217202963,12.4236101160344,124.578846534858)) ;
#81494 = CARTESIAN_POINT('Ctrl Pts',(-19.7517716917863,12.4233817979331,124.577483142913)) ;
#81495 = CARTESIAN_POINT('Ctrl Pts',(-19.7524423820719,12.4233488619146,124.577285864766)) ;
#81496 = CARTESIAN_POINT('Ctrl Pts',(-19.7574907149469,12.4231009161189,124.575796202665)) ;
#81497 = CARTESIAN_POINT('Ctrl Pts',(-19.7618612202299,12.422886069044,124.574479734891)) ;
#81498 = CARTESIAN_POINT('Ctrl Pts',(-19.7722985742821,12.4223724823631,124.571271567179)) ;
#81499 = CARTESIAN_POINT('Ctrl Pts',(-19.7783582074024,12.422073901283,124.569356833635)) ;
#81500 = CARTESIAN_POINT('Ctrl Pts',(-19.7943685490549,12.4212837423584,124.564159352773)) ;
#81501 = CARTESIAN_POINT('Ctrl Pts',(-19.8042922959812,12.4207926806324,124.560795267022)) ;
#81502 = CARTESIAN_POINT('Ctrl Pts',(-19.8450857901445,12.4187667234625,124.546375543884)) ;
#81503 = CARTESIAN_POINT('Ctrl Pts',(-19.8755450511598,12.4172357058851,124.534200907544)) ;
#81504 = CARTESIAN_POINT('Ctrl Pts',(-19.9116559119258,12.4153765671281,124.518043304277)) ;
#81505 = CARTESIAN_POINT('Ctrl Pts',(-19.9178140438702,12.4150579857214,124.515225853268)) ;
#81506 = CARTESIAN_POINT('Ctrl Pts',(-19.9285034726263,12.4145021708986,124.510226758634)) ;
#81507 = CARTESIAN_POINT('Ctrl Pts',(-19.9330453820801,12.414265113429,124.508068189605)) ;
#81508 = CARTESIAN_POINT('Ctrl Pts',(-19.9419836110536,12.4137967907583,124.5037520135)) ;
#81509 = CARTESIAN_POINT('Ctrl Pts',(-19.9463805474503,12.4135655406944,124.501595899481)) ;
#81510 = CARTESIAN_POINT('Ctrl Pts',(-19.9560453773763,12.413055288216,124.496783880251)) ;
#81511 = CARTESIAN_POINT('Ctrl Pts',(-19.9613072015799,12.4127762063331,124.494116071267)) ;
#81512 = CARTESIAN_POINT('Ctrl Pts',(-19.9984633144749,12.4107963380609,124.474936003137)) ;
#81513 = CARTESIAN_POINT('Ctrl Pts',(-20.02963087542,12.4090863940919,124.457055018248)) ;
#81514 = CARTESIAN_POINT('Ctrl Pts',(-20.0599602754258,12.4073831970671,124.437819810756)) ;
#81515 = CARTESIAN_POINT('Origin',(-19.4092696390626,12.3398872919312,123.411833654984)) ;
#81516 = CARTESIAN_POINT('',(-19.4092696390626,12.3998836520522,123.411833654984)) ;
#81517 = CARTESIAN_POINT('',(-18.8344050941734,12.0999018514474,123.240115636693)) ;
#81518 = CARTESIAN_POINT('',(-19.2942967300848,12.3398872919312,123.377490051326)) ;
#81519 = CARTESIAN_POINT('Origin',(-19.4092696390626,12.0999018514474,123.411833654984)) ;
#81520 = CARTESIAN_POINT('Origin',(-19.4092696390626,11.9199127710845,123.411833654984)) ;
#81521 = CARTESIAN_POINT('',(-18.1240607872049,12.4705811104891,123.027928413015)) ;
#81522 = CARTESIAN_POINT('Ctrl Pts',(-20.0599602754274,12.4073831970671,124.437819810754)) ;
#81523 = CARTESIAN_POINT('Ctrl Pts',(-20.0004707798595,12.4089443847785,124.479246016639)) ;
#81524 = CARTESIAN_POINT('Ctrl Pts',(-19.9375759144554,12.4104965535012,124.515176126025)) ;
#81525 = CARTESIAN_POINT('Ctrl Pts',(-19.8055230642977,12.4135619883252,124.575655167027)) ;
#81526 = CARTESIAN_POINT('Ctrl Pts',(-19.7366469094468,12.4150958593948,124.600048047181)) ;
#81527 = CARTESIAN_POINT('Ctrl Pts',(-19.5229749245386,12.4197782665643,124.655153900126)) ;
#81528 = CARTESIAN_POINT('Ctrl Pts',(-19.3738301151842,12.4228609961199,124.665868103026)) ;
#81529 = CARTESIAN_POINT('Ctrl Pts',(-19.1462099532735,12.4276127977452,124.64205564411)) ;
#81530 = CARTESIAN_POINT('Ctrl Pts',(-19.0660088189675,12.4292659064182,124.625546210781)) ;
#81531 = CARTESIAN_POINT('Ctrl Pts',(-18.9099376819915,12.4326333165009,124.577450942515)) ;
#81532 = CARTESIAN_POINT('Ctrl Pts',(-18.8339818501442,12.4343499486543,124.545751384892)) ;
#81533 = CARTESIAN_POINT('Ctrl Pts',(-18.6883020808879,12.4377451727855,124.467494661077)) ;
#81534 = CARTESIAN_POINT('Ctrl Pts',(-18.6190403720584,12.4394104855472,124.420918065797)) ;
#81535 = CARTESIAN_POINT('Ctrl Pts',(-18.4905718925471,12.4427709330837,124.315120935469)) ;
#81536 = CARTESIAN_POINT('Ctrl Pts',(-18.4314678570159,12.4444740645654,124.25601094446)) ;
#81537 = CARTESIAN_POINT('Ctrl Pts',(-18.3246877800231,12.4478688624784,124.126126814797)) ;
#81538 = CARTESIAN_POINT('Ctrl Pts',(-18.2775921591984,12.4495305257554,124.055602387271)) ;
#81539 = CARTESIAN_POINT('Ctrl Pts',(-18.1975609831306,12.4529109006071,123.90631896517)) ;
#81540 = CARTESIAN_POINT('Ctrl Pts',(-18.1646626693663,12.4546483109236,123.827609347576)) ;
#81541 = CARTESIAN_POINT('Ctrl Pts',(-18.1149037431104,12.4580007720278,123.665002308302)) ;
#81542 = CARTESIAN_POINT('Ctrl Pts',(-18.0980236143064,12.4596416636239,123.58126056863)) ;
#81543 = CARTESIAN_POINT('Ctrl Pts',(-18.0801681116067,12.4630480670112,123.410618686017)) ;
#81544 = CARTESIAN_POINT('Ctrl Pts',(-18.079700387576,12.4647476001311,123.323794170317)) ;
#81545 = CARTESIAN_POINT('Ctrl Pts',(-18.0942444324001,12.4678125093508,123.166790916998)) ;
#81546 = CARTESIAN_POINT('Ctrl Pts',(-18.1064133510925,12.4692000007385,123.0966580497)) ;
#81547 = CARTESIAN_POINT('Ctrl Pts',(-18.1240607848549,12.4705811104891,123.027928420882)) ;
#81548 = CARTESIAN_POINT('',(-20.8811762570041,12.5498512937297,123.700066866625)) ;
#81549 = CARTESIAN_POINT('Ctrl Pts',(-20.8811762570041,12.5498512937297,123.700066866625)) ;
#81550 = CARTESIAN_POINT('Ctrl Pts',(-20.8239387353199,12.5305321283812,123.791298907814)) ;
#81551 = CARTESIAN_POINT('Ctrl Pts',(-20.7477236709935,12.5080679368041,123.891522335765)) ;
#81552 = CARTESIAN_POINT('Ctrl Pts',(-20.6010201821559,12.4694919241787,124.025328940159)) ;
#81553 = CARTESIAN_POINT('Ctrl Pts',(-20.5520435705854,12.4570505014033,124.063385132327)) ;
#81554 = CARTESIAN_POINT('Ctrl Pts',(-20.451686730373,12.4324340735919,124.130565753573)) ;
#81555 = CARTESIAN_POINT('Ctrl Pts',(-20.3988578773564,12.4199510743856,124.161083210787)) ;
#81556 = CARTESIAN_POINT('Ctrl Pts',(-20.3451307049827,12.4073898409302,124.186586679355)) ;
#81557 = CARTESIAN_POINT('Ctrl Pts',(-18.1240607848549,12.4705811104891,123.027928420882)) ;
#81558 = CARTESIAN_POINT('Ctrl Pts',(-18.1279098458917,12.4708823427136,123.012937882319)) ;
#81559 = CARTESIAN_POINT('Ctrl Pts',(-18.1320193178887,12.471183020255,122.99801403888)) ;
#81560 = CARTESIAN_POINT('Ctrl Pts',(-18.161059296499,12.4731748557988,122.899300917852)) ;
#81561 = CARTESIAN_POINT('Ctrl Pts',(-18.1939563937343,12.4748348374863,122.817970672594)) ;
#81562 = CARTESIAN_POINT('Ctrl Pts',(-18.2750524739676,12.4782125473854,122.662421849023)) ;
#81563 = CARTESIAN_POINT('Ctrl Pts',(-18.3233531703796,12.4799263147624,122.588305207079)) ;
#81564 = CARTESIAN_POINT('Ctrl Pts',(-18.4340812960901,12.4833084828719,122.450081264731)) ;
#81565 = CARTESIAN_POINT('Ctrl Pts',(-18.496341239815,12.4849766794128,122.386340236217)) ;
#81566 = CARTESIAN_POINT('Ctrl Pts',(-18.5984276425599,12.4875069623852,122.300239051129)) ;
#81567 = CARTESIAN_POINT('Ctrl Pts',(-18.6340836690644,12.488357950932,122.273028142518)) ;
#81568 = CARTESIAN_POINT('Ctrl Pts',(-18.7447054878371,12.4908935345292,122.196872452221)) ;
#81569 = CARTESIAN_POINT('Ctrl Pts',(-18.8233958024688,12.492561011236,122.153383232491)) ;
#81570 = CARTESIAN_POINT('Ctrl Pts',(-18.9877409414025,12.4959478846102,122.082090718853)) ;
#81571 = CARTESIAN_POINT('Ctrl Pts',(-19.0732092836722,12.4976141777242,122.054534548675)) ;
#81572 = CARTESIAN_POINT('Ctrl Pts',(-19.2511933598784,12.5009671960115,122.015636377078)) ;
#81573 = CARTESIAN_POINT('Ctrl Pts',(-19.3435306874433,12.502704565731,122.004769570121)) ;
#81574 = CARTESIAN_POINT('Ctrl Pts',(-19.5262352003067,12.5061073744164,122.001418957146)) ;
#81575 = CARTESIAN_POINT('Ctrl Pts',(-19.6161591817334,12.507727171673,122.008516660418)) ;
#81576 = CARTESIAN_POINT('Ctrl Pts',(-19.7978537234547,12.5110837575643,122.040382303008)) ;
#81577 = CARTESIAN_POINT('Ctrl Pts',(-19.8894756330781,12.5128703471317,122.065894447071)) ;
#81578 = CARTESIAN_POINT('Ctrl Pts',(-20.0629268598057,12.5162623626902,122.133678007326)) ;
#81579 = CARTESIAN_POINT('Ctrl Pts',(-20.1447838037588,12.5178649946103,122.175274708415)) ;
#81580 = CARTESIAN_POINT('Ctrl Pts',(-20.3019291037484,12.5212444282736,122.274566651441)) ;
#81581 = CARTESIAN_POINT('Ctrl Pts',(-20.3767707100987,12.522982262924,122.332838750037)) ;
#81582 = CARTESIAN_POINT('Ctrl Pts',(-20.5138479942751,12.5263554079533,122.463352252629)) ;
#81583 = CARTESIAN_POINT('Ctrl Pts',(-20.5758166537567,12.528031334414,122.535122831076)) ;
#81584 = CARTESIAN_POINT('Ctrl Pts',(-20.7402840444869,12.5331385715931,122.767564209032)) ;
#81585 = CARTESIAN_POINT('Ctrl Pts',(-20.8187421074678,12.5364847742368,122.943199468672)) ;
#81586 = CARTESIAN_POINT('Ctrl Pts',(-20.8832644852129,12.5414807225746,123.221724626541)) ;
#81587 = CARTESIAN_POINT('Ctrl Pts',(-20.8958426824975,12.5431677444753,123.317292456651)) ;
#81588 = CARTESIAN_POINT('Ctrl Pts',(-20.9024557483465,12.5465526000103,123.509223945522)) ;
#81589 = CARTESIAN_POINT('Ctrl Pts',(-20.8963747034844,12.5481950593457,123.605216792126)) ;
#81590 = CARTESIAN_POINT('Ctrl Pts',(-20.8811762570041,12.5498512937297,123.700066866625)) ;
#81591 = CARTESIAN_POINT('',(-19.179323821107,11.9199127710845,123.343146447668)) ;
#81592 = CARTESIAN_POINT('Ctrl Pts',(-20.5445227346514,11.9799091312055,123.023213403245)) ;
#81593 = CARTESIAN_POINT('Ctrl Pts',(-20.5894944790636,11.9865359820236,123.154537963808)) ;
#81594 = CARTESIAN_POINT('Ctrl Pts',(-20.6334264843498,11.9997666085046,123.432369739635)) ;
#81595 = CARTESIAN_POINT('Ctrl Pts',(-20.5528870867457,12.0197422297632,123.849423964094)) ;
#81596 = CARTESIAN_POINT('Ctrl Pts',(-20.3351947176899,12.0396595646652,124.212660991227)) ;
#81597 = CARTESIAN_POINT('Ctrl Pts',(-20.0078997286727,12.0595328413812,124.480006144063)) ;
#81598 = CARTESIAN_POINT('Ctrl Pts',(-19.6059596659497,12.0795573315451,124.620366658966)) ;
#81599 = CARTESIAN_POINT('Ctrl Pts',(-19.1834847849121,12.0994251726959,124.61509168873)) ;
#81600 = CARTESIAN_POINT('Ctrl Pts',(-18.7864895436431,12.1193708235754,124.466037582566)) ;
#81601 = CARTESIAN_POINT('Ctrl Pts',(-18.4649120080556,12.1392762241924,124.190860873568)) ;
#81602 = CARTESIAN_POINT('Ctrl Pts',(-18.2561386390073,12.1591504520087,123.823451800427)) ;
#81603 = CARTESIAN_POINT('Ctrl Pts',(-18.1848458732936,12.1791362428864,123.404512149067)) ;
#81604 = CARTESIAN_POINT('Ctrl Pts',(-18.2606755389189,12.1990304855461,122.988387736168)) ;
#81605 = CARTESIAN_POINT('Ctrl Pts',(-18.4728668974967,12.2189092016182,122.622775123101)) ;
#81606 = CARTESIAN_POINT('Ctrl Pts',(-18.7999576817719,12.2389486514628,122.349782388766)) ;
#81607 = CARTESIAN_POINT('Ctrl Pts',(-19.1972059733625,12.2588118130006,122.205994923479)) ;
#81608 = CARTESIAN_POINT('Ctrl Pts',(-19.6218869886643,12.2787911810149,122.206159049441)) ;
#81609 = CARTESIAN_POINT('Ctrl Pts',(-20.018012005359,12.2986017615377,122.349652549516)) ;
#81610 = CARTESIAN_POINT('Ctrl Pts',(-20.3444464973365,12.3185826898233,122.621438196783)) ;
#81611 = CARTESIAN_POINT('Ctrl Pts',(-20.5574196739387,12.3384753616927,122.986936030998)) ;
#81612 = CARTESIAN_POINT('Ctrl Pts',(-20.6337266981278,12.3584016919798,123.403693608248)) ;
#81613 = CARTESIAN_POINT('Ctrl Pts',(-20.5626962923593,12.3783722460721,123.822338681512)) ;
#81614 = CARTESIAN_POINT('Ctrl Pts',(-20.3894978118444,12.3949040851597,124.128191080618)) ;
#81615 = CARTESIAN_POINT('Ctrl Pts',(-20.1931347282858,12.4082438239873,124.328472259114)) ;
#81616 = CARTESIAN_POINT('Ctrl Pts',(-20.0213926648739,12.4182760662059,124.450877135037)) ;
#81617 = CARTESIAN_POINT('Ctrl Pts',(-19.8344384158834,12.4281337668493,124.540321523917)) ;
#81618 = CARTESIAN_POINT('Ctrl Pts',(-19.6322020198109,12.4381256314886,124.597064382826)) ;
#81619 = CARTESIAN_POINT('Ctrl Pts',(-19.4246153604294,12.4480481812487,124.617642782804)) ;
#81620 = CARTESIAN_POINT('Ctrl Pts',(-19.1462130895236,12.4613259547422,124.597251052543)) ;
#81621 = CARTESIAN_POINT('Ctrl Pts',(-18.8783247008221,12.4746732936828,124.503674838352)) ;
#81622 = CARTESIAN_POINT('Ctrl Pts',(-18.6486087635049,12.487880525476,124.347609621771)) ;
#81623 = CARTESIAN_POINT('Ctrl Pts',(-18.4978177576768,12.4978676415657,124.201561862873)) ;
#81624 = CARTESIAN_POINT('Ctrl Pts',(-18.3749666738686,12.5078185471454,124.032184095878)) ;
#81625 = CARTESIAN_POINT('Ctrl Pts',(-18.282681770341,12.5178736491529,123.842034979796)) ;
#81626 = CARTESIAN_POINT('Ctrl Pts',(-18.2257950874506,12.527695322474,123.643518287885)) ;
#81627 = CARTESIAN_POINT('Ctrl Pts',(-18.203381172838,12.5377537935489,123.433271612789)) ;
#81628 = CARTESIAN_POINT('Ctrl Pts',(-18.2179067713694,12.5476784047254,123.225110816846)) ;
#81629 = CARTESIAN_POINT('Ctrl Pts',(-18.2846782509593,12.5609557436258,122.95410104125)) ;
#81630 = CARTESIAN_POINT('Ctrl Pts',(-18.4211173569722,12.5742546228634,122.706459136274)) ;
#81631 = CARTESIAN_POINT('Ctrl Pts',(-18.6137338939602,12.5874934950341,122.50549677162)) ;
#81632 = CARTESIAN_POINT('Ctrl Pts',(-18.7832480563762,12.5975001131707,122.380910631003)) ;
#81633 = CARTESIAN_POINT('Ctrl Pts',(-18.9724531099051,12.6075310582322,122.287792261205)) ;
#81634 = CARTESIAN_POINT('Ctrl Pts',(-19.1713356879387,12.617387231584,122.229594635167)) ;
#81635 = CARTESIAN_POINT('Ctrl Pts',(-19.3802129828016,12.6273865025469,122.206224196748)) ;
#81636 = CARTESIAN_POINT('Ctrl Pts',(-19.5878656312304,12.6372809543042,122.219099840381)) ;
#81637 = CARTESIAN_POINT('Ctrl Pts',(-19.7934896655894,12.6473442701136,122.268715021665)) ;
#81638 = CARTESIAN_POINT('Ctrl Pts',(-19.9832142539162,12.6571831268532,122.351202089314)) ;
#81639 = CARTESIAN_POINT('Ctrl Pts',(-20.1597894985126,12.6672492486708,122.467780794413)) ;
#81640 = CARTESIAN_POINT('Ctrl Pts',(-20.3106265913815,12.677132476395,122.610717001511)) ;
#81641 = CARTESIAN_POINT('Ctrl Pts',(-20.4360240786786,12.6871219376738,122.779153363513)) ;
#81642 = CARTESIAN_POINT('Ctrl Pts',(-20.5299739101893,12.6970856481003,122.966382455643)) ;
#81643 = CARTESIAN_POINT('Ctrl Pts',(-20.5903897211659,12.7070806508312,123.167652541848)) ;
#81644 = CARTESIAN_POINT('Ctrl Pts',(-20.6147102751126,12.7171169818415,123.377230943918)) ;
#81645 = CARTESIAN_POINT('Ctrl Pts',(-20.6028463796374,12.7269632111838,123.58390229972)) ;
#81646 = CARTESIAN_POINT('Ctrl Pts',(-20.5549966972298,12.736948709459,123.788268814636)) ;
#81647 = CARTESIAN_POINT('Ctrl Pts',(-20.4729187888963,12.746883612442,123.980370469917)) ;
#81648 = CARTESIAN_POINT('Ctrl Pts',(-20.3572021787444,12.7569411155372,124.157299797761)) ;
#81649 = CARTESIAN_POINT('Ctrl Pts',(-20.2161112283117,12.7667627719077,124.30808911269)) ;
#81650 = CARTESIAN_POINT('Ctrl Pts',(-20.0473094958752,12.7768188345729,124.435340829882)) ;
#81651 = CARTESIAN_POINT('Ctrl Pts',(-19.8609443815606,12.7867594992761,124.529924426075)) ;
#81652 = CARTESIAN_POINT('Ctrl Pts',(-19.6619130199022,12.7966639032246,124.591112791339)) ;
#81653 = CARTESIAN_POINT('Ctrl Pts',(-19.4523192191116,12.8067103882181,124.617049850997)) ;
#81654 = CARTESIAN_POINT('Ctrl Pts',(-19.2445050876568,12.8166066160299,124.606538219208)) ;
#81655 = CARTESIAN_POINT('Ctrl Pts',(-19.0383681426615,12.8266661995934,124.559383118428)) ;
#81656 = CARTESIAN_POINT('Ctrl Pts',(-18.8475319931247,12.8365182092622,124.478858160451)) ;
#81657 = CARTESIAN_POINT('Ctrl Pts',(-18.6712600278316,12.8464807407018,124.365762068548)) ;
#81658 = CARTESIAN_POINT('Ctrl Pts',(-18.5164450069791,12.8565122889411,124.222542592833)) ;
#81659 = CARTESIAN_POINT('Ctrl Pts',(-18.390477483579,12.8664037001542,124.057089548771)) ;
#81660 = CARTESIAN_POINT('Ctrl Pts',(-18.2936063772451,12.8764199538622,123.870112758873)) ;
#81661 = CARTESIAN_POINT('Ctrl Pts',(-18.2310247387816,12.8864500567069,123.668752580011)) ;
#81662 = CARTESIAN_POINT('Ctrl Pts',(-18.204422386425,12.8963065056606,123.46324083498)) ;
#81663 = CARTESIAN_POINT('Ctrl Pts',(-18.2137782930825,12.9063055164329,123.253271985163)) ;
#81664 = CARTESIAN_POINT('Ctrl Pts',(-18.2587651034631,12.9162007333509,123.050131402828)) ;
#81665 = CARTESIAN_POINT('Ctrl Pts',(-18.339668596568,12.9262612487082,122.854741757177)) ;
#81666 = CARTESIAN_POINT('Ctrl Pts',(-18.4508077453333,12.9361105420953,122.680014237117)) ;
#81667 = CARTESIAN_POINT('Ctrl Pts',(-18.592713145265,12.9461377177753,122.524134235879)) ;
#81668 = CARTESIAN_POINT('Ctrl Pts',(-18.7599030550601,12.9561662934024,122.395673635507)) ;
#81669 = CARTESIAN_POINT('Ctrl Pts',(-18.9432361554979,12.9660113869483,122.299636177384)) ;
#81670 = CARTESIAN_POINT('Ctrl Pts',(-19.143231563781,12.9760026283801,122.235427957992)) ;
#81671 = CARTESIAN_POINT('Ctrl Pts',(-19.3523277949078,12.9860384095234,122.207228144837)) ;
#81672 = CARTESIAN_POINT('Ctrl Pts',(-19.5592861625854,12.9958906152531,122.215330009686)) ;
#81673 = CARTESIAN_POINT('Ctrl Pts',(-19.7640842461694,13.0058527093701,122.259137343665)) ;
#81674 = CARTESIAN_POINT('Ctrl Pts',(-19.9592496485709,13.0158752701972,122.338556584842)) ;
#81675 = CARTESIAN_POINT('Ctrl Pts',(-20.13609931847,13.0258030418487,122.449432047866)) ;
#81676 = CARTESIAN_POINT('Ctrl Pts',(-20.292758411066,13.0358454259736,122.590938523857)) ;
#81677 = CARTESIAN_POINT('Ctrl Pts',(-20.4205737272681,13.0457346500442,122.754925408144)) ;
#81678 = CARTESIAN_POINT('Ctrl Pts',(-20.5192984833546,13.0557238982115,122.940270443942)) ;
#81679 = CARTESIAN_POINT('Ctrl Pts',(-20.5839903547336,13.0656824752535,123.13937958665)) ;
#81680 = CARTESIAN_POINT('Ctrl Pts',(-20.6134664474397,13.0755820443448,123.345414260246)) ;
#81681 = CARTESIAN_POINT('Ctrl Pts',(-20.606545766267,13.0856299564288,123.556518066984)) ;
#81682 = CARTESIAN_POINT('Ctrl Pts',(-20.5638845202153,13.095525310736,123.760161232026)) ;
#81683 = CARTESIAN_POINT('Ctrl Pts',(-20.4852609723389,13.1055869612272,123.956508898549)) ;
#81684 = CARTESIAN_POINT('Ctrl Pts',(-20.3761562249618,13.1154315766896,124.13238749909)) ;
#81685 = CARTESIAN_POINT('Ctrl Pts',(-20.2371197494185,13.125391655591,124.288952093036)) ;
#81686 = CARTESIAN_POINT('Ctrl Pts',(-20.0714719776813,13.1354298499494,124.419691976004)) ;
#81687 = CARTESIAN_POINT('Ctrl Pts',(-19.8888379913786,13.145303565349,124.518402109954)) ;
#81688 = CARTESIAN_POINT('Ctrl Pts',(-19.6879341319038,13.1553752748833,124.585176379889)) ;
#81689 = CARTESIAN_POINT('Ctrl Pts',(-19.4834366764819,13.1652077153358,124.615443529714)) ;
#81690 = CARTESIAN_POINT('Ctrl Pts',(-19.272605892093,13.1752395362612,124.610216779178)) ;
#81691 = CARTESIAN_POINT('Ctrl Pts',(-19.0662333340768,13.1852599061468,124.567919588929)) ;
#81692 = CARTESIAN_POINT('Ctrl Pts',(-18.873132979465,13.1951266772805,124.492120670378)) ;
#81693 = CARTESIAN_POINT('Ctrl Pts',(-18.6925009208601,13.2051974484699,124.381720145738)) ;
#81694 = CARTESIAN_POINT('Ctrl Pts',(-18.537329422245,13.2150406089915,124.244796167475)) ;
#81695 = CARTESIAN_POINT('Ctrl Pts',(-18.4059658449901,13.2250208421779,124.08120074674)) ;
#81696 = CARTESIAN_POINT('Ctrl Pts',(-18.3049709764517,13.2350393622131,123.896379526624)) ;
#81697 = CARTESIAN_POINT('Ctrl Pts',(-18.2380816447624,13.2449226705968,123.699636053287)) ;
#81698 = CARTESIAN_POINT('Ctrl Pts',(-18.2058768832933,13.2549909547676,123.490468235174)) ;
#81699 = CARTESIAN_POINT('Ctrl Pts',(-18.2101289843034,13.2648210814352,123.283817052542)) ;
#81700 = CARTESIAN_POINT('Ctrl Pts',(-18.2508798573275,13.2748876536418,123.076180818645)) ;
#81701 = CARTESIAN_POINT('Ctrl Pts',(-18.3258688030346,13.2847778098825,122.882224404602)) ;
#81702 = CARTESIAN_POINT('Ctrl Pts',(-18.4340995112208,13.2947703374589,122.702192244666)) ;
#81703 = CARTESIAN_POINT('Ctrl Pts',(-18.571661784907,13.3047318273332,122.544287761038)) ;
#81704 = CARTESIAN_POINT('Ctrl Pts',(-18.7334033065214,13.3146410492204,122.412979799339)) ;
#81705 = CARTESIAN_POINT('Ctrl Pts',(-18.9180669225408,13.3246896290307,122.310402899942)) ;
#81706 = CARTESIAN_POINT('Ctrl Pts',(-19.1144428684157,13.3345726035008,122.242506570762)) ;
#81707 = CARTESIAN_POINT('Ctrl Pts',(-19.3218592255467,13.3445675146435,122.208921813123)) ;
#81708 = CARTESIAN_POINT('Ctrl Pts',(-19.5325087212817,13.3545879012171,122.212159433721)) ;
#81709 = CARTESIAN_POINT('Ctrl Pts',(-19.7371141879911,13.3644980050741,122.251364326533)) ;
#81710 = CARTESIAN_POINT('Ctrl Pts',(-19.9323647674742,13.374425717284,122.325127289265)) ;
#81711 = CARTESIAN_POINT('Ctrl Pts',(-20.1138238775436,13.3844688270513,122.43305489869)) ;
#81712 = CARTESIAN_POINT('Ctrl Pts',(-20.2713928547841,13.3943552475068,122.568612065668)) ;
#81713 = CARTESIAN_POINT('Ctrl Pts',(-20.4047144716701,13.4043484251125,122.730961914886)) ;
#81714 = CARTESIAN_POINT('Ctrl Pts',(-20.5072674311864,13.4142940880164,122.913174188626)) ;
#81715 = CARTESIAN_POINT('Ctrl Pts',(-20.5770419820694,13.4242413842216,123.110324466056)) ;
#81716 = CARTESIAN_POINT('Ctrl Pts',(-20.6116395125164,13.4342891497995,123.318702120629)) ;
#81717 = CARTESIAN_POINT('Ctrl Pts',(-20.609736309306,13.4441373630171,123.525730692802)) ;
#81718 = CARTESIAN_POINT('Ctrl Pts',(-20.572167565725,13.4540969358112,123.73171350062)) ;
#81719 = CARTESIAN_POINT('Ctrl Pts',(-20.4984960852348,13.4641335568437,123.929428932147)) ;
#81720 = CARTESIAN_POINT('Ctrl Pts',(-20.393541247342,13.474014071654,124.108708094483)) ;
#81721 = CARTESIAN_POINT('Ctrl Pts',(-20.256803503164,13.4840667229611,124.269810836834)) ;
#81722 = CARTESIAN_POINT('Ctrl Pts',(-20.0967179447139,13.4939621212411,124.402720841087)) ;
#81723 = CARTESIAN_POINT('Ctrl Pts',(-19.913262767579,13.5040122429472,124.507479244964)) ;
#81724 = CARTESIAN_POINT('Ctrl Pts',(-19.717652853567,13.5138965224891,124.577663674712)) ;
#81725 = CARTESIAN_POINT('Ctrl Pts',(-19.510645163499,13.523891303781,124.613591990072)) ;
#81726 = CARTESIAN_POINT('Ctrl Pts',(-19.301497134244,13.5338391489678,124.612953428536)) ;
#81727 = CARTESIAN_POINT('Ctrl Pts',(-19.095840811531,13.5437761123552,124.576354548961)) ;
#81728 = CARTESIAN_POINT('Ctrl Pts',(-18.898621765146,13.5537590770924,124.504501861206)) ;
#81729 = CARTESIAN_POINT('Ctrl Pts',(-18.7160044603142,13.563802928508,124.398546755933)) ;
#81730 = CARTESIAN_POINT('Ctrl Pts',(-18.5576688042803,13.5736311298428,124.265752330225)) ;
#81731 = CARTESIAN_POINT('Ctrl Pts',(-18.421408955207,13.5837077024408,124.103605355622)) ;
#81732 = CARTESIAN_POINT('Ctrl Pts',(-18.3176011922116,13.5935597824484,123.924323629217)) ;
#81733 = CARTESIAN_POINT('Ctrl Pts',(-18.2447623948526,13.6036330674525,123.725509185819)) ;
#81734 = CARTESIAN_POINT('Ctrl Pts',(-18.2084518087594,13.613474419163,123.521808388656)) ;
#81735 = CARTESIAN_POINT('Ctrl Pts',(-18.2072839710603,13.6234359185595,123.312402282748)) ;
#81736 = CARTESIAN_POINT('Ctrl Pts',(-18.2431244045269,13.6334716946895,123.104477458676)) ;
#81737 = CARTESIAN_POINT('Ctrl Pts',(-18.3132663380114,13.643360121327,122.908785005835)) ;
#81738 = CARTESIAN_POINT('Ctrl Pts',(-18.417302510942,13.6533754434019,122.725719693206)) ;
#81739 = CARTESIAN_POINT('Ctrl Pts',(-18.5521194988632,13.6634057923022,122.563574869052)) ;
#81740 = CARTESIAN_POINT('Ctrl Pts',(-18.7097686244556,13.6732491679088,122.429528067973)) ;
#81741 = CARTESIAN_POINT('Ctrl Pts',(-18.8914413453651,13.683278604806,122.322502836408)) ;
#81742 = CARTESIAN_POINT('Ctrl Pts',(-19.0891909781922,13.6933104827389,122.249169480939)) ;
#81743 = CARTESIAN_POINT('Ctrl Pts',(-19.2923910474279,13.7031401058444,122.211639192755)) ;
#81744 = CARTESIAN_POINT('Ctrl Pts',(-19.5023938465683,13.7131295769975,122.209303796898)) ;
#81745 = CARTESIAN_POINT('Ctrl Pts',(-19.7106448780283,13.7231734257599,122.244181273255)) ;
#81746 = CARTESIAN_POINT('Ctrl Pts',(-19.9054181998677,13.7329951312916,122.312725993549)) ;
#81747 = CARTESIAN_POINT('Ctrl Pts',(-20.0894923668064,13.7430301711194,122.415798371662)) ;
#81748 = CARTESIAN_POINT('Ctrl Pts',(-20.2523425461733,13.7530548780108,122.549585334357)) ;
#81749 = CARTESIAN_POINT('Ctrl Pts',(-20.3874635188741,13.7629075823516,122.706578430368)) ;
#81750 = CARTESIAN_POINT('Ctrl Pts',(-20.495034847891,13.7728957045593,122.886895987857)) ;
#81751 = CARTESIAN_POINT('Ctrl Pts',(-20.5692346966723,13.7828241746666,123.08199531323)) ;
#81752 = CARTESIAN_POINT('Ctrl Pts',(-20.6090140370944,13.7928131518338,123.288203351907)) ;
#81753 = CARTESIAN_POINT('Ctrl Pts',(-20.6120399399708,13.8028509591135,123.499202419839)) ;
#81754 = CARTESIAN_POINT('Ctrl Pts',(-20.5793586406497,13.8126972599768,123.703608137573)) ;
#81755 = CARTESIAN_POINT('Ctrl Pts',(-20.5108933551934,13.8227230033561,123.902954081901)) ;
#81756 = CARTESIAN_POINT('Ctrl Pts',(-20.4083206360127,13.8327538697951,124.087214529611)) ;
#81757 = CARTESIAN_POINT('Ctrl Pts',(-20.2782096650615,13.8425912285939,124.247959028834)) ;
#81758 = CARTESIAN_POINT('Ctrl Pts',(-20.1200757165618,13.8525831895276,124.386233235836)) ;
#81759 = CARTESIAN_POINT('Ctrl Pts',(-19.939381440305,13.8626155520842,124.495031216594)) ;
#81760 = CARTESIAN_POINT('Ctrl Pts',(-19.7459291063119,13.8724807126586,124.569766298816)) ;
#81761 = CARTESIAN_POINT('Ctrl Pts',(-19.5405428783788,13.8824426172363,124.610756191596)) ;
#81762 = CARTESIAN_POINT('Ctrl Pts',(-19.3296341401678,13.892477547312,124.615150409139)) ;
#81763 = CARTESIAN_POINT('Ctrl Pts',(-19.1241882630405,13.9023624941656,124.583680284887)) ;
#81764 = CARTESIAN_POINT('Ctrl Pts',(-18.9238050412693,13.9124281704771,124.515772547022)) ;
#81765 = CARTESIAN_POINT('Ctrl Pts',(-18.7422739018673,13.922267090112,124.416547651095)) ;
#81766 = CARTESIAN_POINT('Ctrl Pts',(-18.5769212021709,13.9323305998464,124.284614917872)) ;
#81767 = CARTESIAN_POINT('Ctrl Pts',(-18.4394438907327,13.9422242130082,124.12849967911)) ;
#81768 = CARTESIAN_POINT('Ctrl Pts',(-18.3301649153485,13.9521682198216,123.950314437566)) ;
#81769 = CARTESIAN_POINT('Ctrl Pts',(-18.252931772702,13.9621691741759,123.754727554759)) ;
#81770 = CARTESIAN_POINT('Ctrl Pts',(-18.2110520046167,13.9722079318682,123.547897335282)) ;
#81771 = CARTESIAN_POINT('Ctrl Pts',(-18.2053814422572,13.9820321160382,123.341422790906)) ;
#81772 = CARTESIAN_POINT('Ctrl Pts',(-18.2360559546118,13.9920901816376,123.132225932652)) ;
#81773 = CARTESIAN_POINT('Ctrl Pts',(-18.3020120627055,14.0020202284123,122.934144622133)) ;
#81774 = CARTESIAN_POINT('Ctrl Pts',(-18.4010833690568,14.0119716707494,122.749875876778)) ;
#81775 = CARTESIAN_POINT('Ctrl Pts',(-18.5321101497463,14.0220184679287,122.58421709419)) ;
#81776 = CARTESIAN_POINT('Ctrl Pts',(-18.6866603133442,14.0318664086088,122.446457948608)) ;
#81777 = CARTESIAN_POINT('Ctrl Pts',(-18.8644655336791,14.0418280399514,122.335821830782)) ;
#81778 = CARTESIAN_POINT('Ctrl Pts',(-19.0602066092931,14.0518566993273,122.257452043026)) ;
#81779 = CARTESIAN_POINT('Ctrl Pts',(-19.2641111444034,14.0617670022155,122.214707828412)) ;
#81780 = CARTESIAN_POINT('Ctrl Pts',(-19.4728544922654,14.0717018967777,122.207453402267)) ;
#81781 = CARTESIAN_POINT('Ctrl Pts',(-19.68185738335,14.0817429954446,122.237057210089)) ;
#81782 = CARTESIAN_POINT('Ctrl Pts',(-19.8795330772188,14.091630277949,122.301367079773)) ;
#81783 = CARTESIAN_POINT('Ctrl Pts',(-20.065123390794,14.1016220184595,122.399728598824)) ;
#81784 = CARTESIAN_POINT('Ctrl Pts',(-20.2301072624107,14.1115725676949,122.528359338337)) ;
#81785 = CARTESIAN_POINT('Ctrl Pts',(-20.3702567814711,14.1215082453297,122.683224847717)) ;
#81786 = CARTESIAN_POINT('Ctrl Pts',(-20.4821496428218,14.1314936631225,122.860862878877)) ;
#81787 = CARTESIAN_POINT('Ctrl Pts',(-20.5615945327275,14.141522455993,123.056157709777)) ;
#81788 = CARTESIAN_POINT('Ctrl Pts',(-20.6054790276225,14.1514019672209,123.259164195847)) ;
#81789 = CARTESIAN_POINT('Ctrl Pts',(-20.6140230839649,14.1613955038939,123.469094160262)) ;
#81790 = CARTESIAN_POINT('Ctrl Pts',(-20.5854452308061,14.1714277721577,123.678050018947)) ;
#81791 = CARTESIAN_POINT('Ctrl Pts',(-20.5225143012457,14.1812917341636,123.875665243064)) ;
#81792 = CARTESIAN_POINT('Ctrl Pts',(-20.4242669170228,14.1913617955085,124.06316684514)) ;
#81793 = CARTESIAN_POINT('Ctrl Pts',(-20.2978535530189,14.2012041598572,124.226991191777)) ;
#81794 = CARTESIAN_POINT('Ctrl Pts',(-20.1436081129759,14.2111648323597,124.368614423322)) ;
#81795 = CARTESIAN_POINT('Ctrl Pts',(-19.9655216612941,14.2212029034275,124.481821948191)) ;
#81796 = CARTESIAN_POINT('Ctrl Pts',(-19.773794365022,14.2310765183879,124.561451051005)) ;
#81797 = CARTESIAN_POINT('Ctrl Pts',(-19.5671348212395,14.2411487529692,124.607418823694)) ;
#81798 = CARTESIAN_POINT('Ctrl Pts',(-19.3607741072514,14.250972771418,124.616812784655)) ;
#81799 = CARTESIAN_POINT('Ctrl Pts',(-19.1509484643771,14.261037692394,124.589865490901)) ;
#81800 = CARTESIAN_POINT('Ctrl Pts',(-18.8857421831171,14.2742479906888,124.507190925921)) ;
#81801 = CARTESIAN_POINT('Ctrl Pts',(-18.6462439305007,14.2875634374207,124.356328829034)) ;
#81802 = CARTESIAN_POINT('Ctrl Pts',(-18.4564443867322,14.300853682688,124.151228791517)) ;
#81803 = CARTESIAN_POINT('Ctrl Pts',(-18.3421585188713,14.3109044322951,123.973546353508)) ;
#81804 = CARTESIAN_POINT('Ctrl Pts',(-18.2619973092775,14.3207170392773,123.783433923944)) ;
#81805 = CARTESIAN_POINT('Ctrl Pts',(-18.2145911012313,14.3307881372716,123.577110239697)) ;
#81806 = CARTESIAN_POINT('Ctrl Pts',(-18.2041343827819,14.3406777100464,123.369451442456)) ;
#81807 = CARTESIAN_POINT('Ctrl Pts',(-18.2378552198279,14.3539478168497,123.092490133588)) ;
#81808 = CARTESIAN_POINT('Ctrl Pts',(-18.3698702894281,14.3705645037722,122.76481914799)) ;
#81809 = CARTESIAN_POINT('Ctrl Pts',(-18.6050453051043,14.3871385470885,122.502296262875)) ;
#81810 = CARTESIAN_POINT('Ctrl Pts',(-18.8388900348431,14.4004351145203,122.349191255889)) ;
#81811 = CARTESIAN_POINT('Ctrl Pts',(-19.0327140202685,14.4104651780977,122.266120714729)) ;
#81812 = CARTESIAN_POINT('Ctrl Pts',(-19.2351924737432,14.4203590699469,122.218606671375)) ;
#81813 = CARTESIAN_POINT('Ctrl Pts',(-19.5133780610374,14.4336118257325,122.202020475397)) ;
#81814 = CARTESIAN_POINT('Ctrl Pts',(-19.8616301080899,14.4503399307249,122.274027235168)) ;
#81815 = CARTESIAN_POINT('Ctrl Pts',(-20.2206980583628,14.4701707672034,122.495229511939)) ;
#81816 = CARTESIAN_POINT('Ctrl Pts',(-20.484680559631,14.4900961590936,122.826481287003)) ;
#81817 = CARTESIAN_POINT('Ctrl Pts',(-20.619780680086,14.5100213724456,123.228098196348)) ;
#81818 = CARTESIAN_POINT('Ctrl Pts',(-20.6098292278703,14.5299463859307,123.651592133763)) ;
#81819 = CARTESIAN_POINT('Ctrl Pts',(-20.4568503086671,14.5498228576307,124.045589431713)) ;
#81820 = CARTESIAN_POINT('Ctrl Pts',(-20.1773268323864,14.5698021755395,124.365478490848)) ;
#81821 = CARTESIAN_POINT('Ctrl Pts',(-19.8060956324391,14.5897351791155,124.570044599947)) ;
#81822 = CARTESIAN_POINT('Ctrl Pts',(-19.3882614992928,14.6096304491432,124.635961690786)) ;
#81823 = CARTESIAN_POINT('Ctrl Pts',(-18.9723460744339,14.6295517870491,124.555651059117)) ;
#81824 = CARTESIAN_POINT('Ctrl Pts',(-18.6081837802081,14.6495094103152,124.337753576671)) ;
#81825 = CARTESIAN_POINT('Ctrl Pts',(-18.3412613988883,14.6693892422725,124.010077128848)) ;
#81826 = CARTESIAN_POINT('Ctrl Pts',(-18.201016862601,14.6892710935694,123.611189546996)) ;
#81827 = CARTESIAN_POINT('Ctrl Pts',(-18.2061577113468,14.7093421106732,123.184511307658)) ;
#81828 = CARTESIAN_POINT('Ctrl Pts',(-18.3545971328961,14.7291493344262,122.790298984124)) ;
#81829 = CARTESIAN_POINT('Ctrl Pts',(-18.630222996083,14.749130469995,122.467037934246)) ;
#81830 = CARTESIAN_POINT('Ctrl Pts',(-18.9990324357376,14.7690579633343,122.258519647139)) ;
#81831 = CARTESIAN_POINT('Ctrl Pts',(-19.4145307497255,14.7888786246921,122.18730127194)) ;
#81832 = CARTESIAN_POINT('Ctrl Pts',(-19.8347873100262,14.8089758139139,122.263805837987)) ;
#81833 = CARTESIAN_POINT('Ctrl Pts',(-20.1980424116417,14.8287394929222,122.475491393999)) ;
#81834 = CARTESIAN_POINT('Ctrl Pts',(-20.4713801712505,14.8487967715953,122.802607740335)) ;
#81835 = CARTESIAN_POINT('Ctrl Pts',(-20.6146598483129,14.8685921953427,123.198496247975)) ;
#81836 = CARTESIAN_POINT('Ctrl Pts',(-20.6155550087254,14.8885558400703,123.622927778774)) ;
#81837 = CARTESIAN_POINT('Ctrl Pts',(-20.470426520549,14.9085393313444,124.022283127792)) ;
#81838 = CARTESIAN_POINT('Ctrl Pts',(-20.2007731778919,14.9283468264937,124.345851882021)) ;
#81839 = CARTESIAN_POINT('Ctrl Pts',(-19.8340286108545,14.9483294172138,124.560210061234)) ;
#81840 = CARTESIAN_POINT('Ctrl Pts',(-19.4180417678935,14.968212071205,124.636132917858)) ;
#81841 = CARTESIAN_POINT('Ctrl Pts',(-18.9996611265361,14.9881703160681,124.565621362804)) ;
#81842 = CARTESIAN_POINT('Ctrl Pts',(-18.6317275054773,15.0080459031097,124.35759044417)) ;
#81843 = CARTESIAN_POINT('Ctrl Pts',(-18.3552455446959,15.0280267912449,124.035054764001)) ;
#81844 = CARTESIAN_POINT('Ctrl Pts',(-18.2060499354365,15.0479619323559,123.638243857989)) ;
#81845 = CARTESIAN_POINT('Ctrl Pts',(-18.2009208909891,15.067873950367,123.214932035603)) ;
#81846 = CARTESIAN_POINT('Ctrl Pts',(-18.3399790656831,15.0877621686106,122.815553113942)) ;
#81847 = CARTESIAN_POINT('Ctrl Pts',(-18.5625223680875,15.1043604724575,122.541718610699)) ;
#81848 = CARTESIAN_POINT('Ctrl Pts',(-18.7884689621563,15.1176330623603,122.377905248733)) ;
#81849 = CARTESIAN_POINT('Ctrl Pts',(-18.9775554066951,15.1276404773112,122.285678430504)) ;
#81850 = CARTESIAN_POINT('Ctrl Pts',(-19.1798597516223,15.1376478240438,122.22785769584)) ;
#81851 = CARTESIAN_POINT('Ctrl Pts',(-19.457193918436,15.1509141838454,122.19875899803)) ;
#81852 = CARTESIAN_POINT('Ctrl Pts',(-19.8041247998046,15.1674288414683,122.253102887633)) ;
#81853 = CARTESIAN_POINT('Ctrl Pts',(-20.1135389192194,15.184026274711,122.4226744457)) ;
#81854 = CARTESIAN_POINT('Ctrl Pts',(-20.3161544867179,15.197374271856,122.616914600856)) ;
#81855 = CARTESIAN_POINT('Ctrl Pts',(-20.4392738849815,15.2072700262076,122.784604378727)) ;
#81856 = CARTESIAN_POINT('Ctrl Pts',(-20.5324949089409,15.2172579801389,122.972739458481)) ;
#81857 = CARTESIAN_POINT('Ctrl Pts',(-20.5915500229038,15.2272152038437,123.173594433495)) ;
#81858 = CARTESIAN_POINT('Ctrl Pts',(-20.61491405898,15.2372507504003,123.383260935523)) ;
#81859 = CARTESIAN_POINT('Ctrl Pts',(-20.6018719810459,15.2471378616764,123.590723454185)) ;
#81860 = CARTESIAN_POINT('Ctrl Pts',(-20.5528214869393,15.2571292667773,123.79495655389)) ;
#81861 = CARTESIAN_POINT('Ctrl Pts',(-20.469375655594,15.2670748879921,123.986671291111)) ;
#81862 = CARTESIAN_POINT('Ctrl Pts',(-20.3542146612541,15.2770241362604,124.161292940439)) ;
#81863 = CARTESIAN_POINT('Ctrl Pts',(-20.2089133776194,15.287070631429,124.314566336844)) ;
#81864 = CARTESIAN_POINT('Ctrl Pts',(-20.042609411081,15.2969219742205,124.438017667828)) ;
#81865 = CARTESIAN_POINT('Ctrl Pts',(-19.8554011038652,15.3068937543479,124.532309413521)) ;
#81866 = CARTESIAN_POINT('Ctrl Pts',(-19.6541309470983,15.3168889543256,124.592800416461)) ;
#81867 = CARTESIAN_POINT('Ctrl Pts',(-19.4446258145735,15.3269229460216,124.617258984874)) ;
#81868 = CARTESIAN_POINT('Ctrl Pts',(-19.2377471749459,15.3367783509941,124.605514108099)) ;
#81869 = CARTESIAN_POINT('Ctrl Pts',(-19.0330947230129,15.3467776488399,124.55762545372)) ;
#81870 = CARTESIAN_POINT('Ctrl Pts',(-18.8417260232628,15.3566727614451,124.475969746375)) ;
#81871 = CARTESIAN_POINT('Ctrl Pts',(-18.6645920999811,15.3667334069801,124.360440268439)) ;
#81872 = CARTESIAN_POINT('Ctrl Pts',(-18.5133455015667,15.3765822839693,124.219009644722)) ;
#81873 = CARTESIAN_POINT('Ctrl Pts',(-18.3862687864151,15.3866109950629,124.050778478714)) ;
#81874 = CARTESIAN_POINT('Ctrl Pts',(-18.290833948785,15.396640396319,123.86275858809)) ;
#81875 = CARTESIAN_POINT('Ctrl Pts',(-18.2302119049096,15.406480588115,123.66496496262)) ;
#81876 = CARTESIAN_POINT('Ctrl Pts',(-18.2040500549491,15.416484017308,123.456316143428)) ;
#81877 = CARTESIAN_POINT('Ctrl Pts',(-18.2145657244891,15.4264695297742,123.246616916574)) ;
#81878 = CARTESIAN_POINT('Ctrl Pts',(-18.26178793961,15.4365106261582,123.040892392394)) ;
#81879 = CARTESIAN_POINT('Ctrl Pts',(-18.3421420875874,15.4463538221092,122.850175898891)) ;
#81880 = CARTESIAN_POINT('Ctrl Pts',(-18.4556407659876,15.4563401331636,122.673598929047)) ;
#81881 = CARTESIAN_POINT('Ctrl Pts',(-18.5972860767463,15.4662748184213,122.520057465721)) ;
#81882 = CARTESIAN_POINT('Ctrl Pts',(-18.7655513631646,15.4763323796383,122.392067434468)) ;
#81883 = CARTESIAN_POINT('Ctrl Pts',(-18.9489772344995,15.4861540212469,122.297204603864)) ;
#81884 = CARTESIAN_POINT('Ctrl Pts',(-19.1506365335545,15.4962100848379,122.233796786976)) ;
#81885 = CARTESIAN_POINT('Ctrl Pts',(-19.3579112056646,15.5061507605997,122.207051934583)) ;
#81886 = CARTESIAN_POINT('Ctrl Pts',(-19.5659421426239,15.516055119388,122.216014786074)) ;
#81887 = CARTESIAN_POINT('Ctrl Pts',(-19.772129699741,15.5261017739638,122.261734136277)) ;
#81888 = CARTESIAN_POINT('Ctrl Pts',(-19.9644276677444,15.5359973686067,122.34119219078)) ;
#81889 = CARTESIAN_POINT('Ctrl Pts',(-20.1429244164977,15.5460593152635,122.454662034304)) ;
#81890 = CARTESIAN_POINT('Ctrl Pts',(-20.2957651324477,15.5559089391957,122.594383759069)) ;
#81891 = CARTESIAN_POINT('Ctrl Pts',(-20.4240143606613,15.5658721782255,122.759973311807)) ;
#81892 = CARTESIAN_POINT('Ctrl Pts',(-20.5219183135764,15.5758967530014,122.946614158251)) ;
#81893 = CARTESIAN_POINT('Ctrl Pts',(-20.5853737236392,15.5858153156891,123.145237961311)) ;
#81894 = CARTESIAN_POINT('Ctrl Pts',(-20.6139543239796,15.5958075024131,123.353364337211)) ;
#81895 = CARTESIAN_POINT('Ctrl Pts',(-20.605550036432,15.6058423009973,123.564151643716)) ;
#81896 = CARTESIAN_POINT('Ctrl Pts',(-20.5618195347646,15.6156974916709,123.766687362844)) ;
#81897 = CARTESIAN_POINT('Ctrl Pts',(-20.482721928661,15.6256968398239,123.96141891483)) ;
#81898 = CARTESIAN_POINT('Ctrl Pts',(-20.3723321482436,15.6355919654991,124.137780679672)) ;
#81899 = CARTESIAN_POINT('Ctrl Pts',(-20.2306926367424,15.6456525084472,124.294818439706)) ;
#81900 = CARTESIAN_POINT('Ctrl Pts',(-20.0674780437418,15.6555017827141,124.422264726541)) ;
#81901 = CARTESIAN_POINT('Ctrl Pts',(-19.8815798640716,15.665529007284,124.521651786014)) ;
#81902 = CARTESIAN_POINT('Ctrl Pts',(-19.6810377876268,15.6755574064718,124.586740135574)) ;
#81903 = CARTESIAN_POINT('Ctrl Pts',(-19.4761222669464,15.6854031568852,124.615862634401)) ;
#81904 = CARTESIAN_POINT('Ctrl Pts',(-19.2662142305259,15.695391947286,124.609449912632)) ;
#81905 = CARTESIAN_POINT('Ctrl Pts',(-19.0595807224344,15.7054368756857,124.565927885616)) ;
#81906 = CARTESIAN_POINT('Ctrl Pts',(-18.8677446564262,15.7152613604747,124.489355654725)) ;
#81907 = CARTESIAN_POINT('Ctrl Pts',(-18.6878182095202,15.7253187580159,124.378336126653)) ;
#81908 = CARTESIAN_POINT('Ctrl Pts',(-18.5321217513917,15.7352448496021,124.239371234552)) ;
#81909 = CARTESIAN_POINT('Ctrl Pts',(-18.4021311728377,15.7451996347466,124.075359055294)) ;
#81910 = CARTESIAN_POINT('Ctrl Pts',(-18.3019733000776,15.7552370044043,123.889627359725)) ;
#81911 = CARTESIAN_POINT('Ctrl Pts',(-18.2364143023807,15.7651258145259,123.692335431482)) ;
#81912 = CARTESIAN_POINT('Ctrl Pts',(-18.2054278152639,15.7751151735769,123.484630912349)) ;
#81913 = CARTESIAN_POINT('Ctrl Pts',(-18.2111153581584,15.785073721033,123.275354627164)) ;
#81914 = CARTESIAN_POINT('Ctrl Pts',(-18.2523061623846,15.7949732975841,123.071338434884)) ;
#81915 = CARTESIAN_POINT('Ctrl Pts',(-18.329490776144,15.8050212094148,122.874729160765)) ;
#81916 = CARTESIAN_POINT('Ctrl Pts',(-18.4378567623646,15.8149165572753,122.697113500965)) ;
#81917 = CARTESIAN_POINT('Ctrl Pts',(-18.5776691405104,15.8249782338065,122.538410360444)) ;
#81918 = CARTESIAN_POINT('Ctrl Pts',(-18.739350169092,15.8348227515557,122.409198097224)) ;
#81919 = CARTESIAN_POINT('Ctrl Pts',(-18.9227807641953,15.8447831952704,122.308206346156)) ;
#81920 = CARTESIAN_POINT('Ctrl Pts',(-19.1226076900904,15.8548200280887,122.240451395418)) ;
#81921 = CARTESIAN_POINT('Ctrl Pts',(-19.3278520560388,15.8646988248355,122.208586052293)) ;
#81922 = CARTESIAN_POINT('Ctrl Pts',(-19.5392660873161,15.8747581409638,122.212851544582)) ;
#81923 = CARTESIAN_POINT('Ctrl Pts',(-19.7428659929903,15.8846285877171,122.252995254409)) ;
#81924 = CARTESIAN_POINT('Ctrl Pts',(-19.9389930726343,15.8946212259751,122.328273341098)) ;
#81925 = CARTESIAN_POINT('Ctrl Pts',(-20.1195385569295,15.904653241523,122.437273858021)) ;
#81926 = CARTESIAN_POINT('Ctrl Pts',(-20.2761009241912,15.9145190978296,122.573347765819)) ;
#81927 = CARTESIAN_POINT('Ctrl Pts',(-20.4093380273943,15.9245883872987,122.737816277399)) ;
#81928 = CARTESIAN_POINT('Ctrl Pts',(-20.5097308458922,15.93443194485,122.918789574222)) ;
#81929 = CARTESIAN_POINT('Ctrl Pts',(-20.5787544498906,15.9444120716378,123.116917393126)) ;
#81930 = CARTESIAN_POINT('Ctrl Pts',(-20.6120581104924,15.9544306202378,123.324883620406)) ;
#81931 = CARTESIAN_POINT('Ctrl Pts',(-20.6092324188456,15.964313920761,123.53266749653)) ;
#81932 = CARTESIAN_POINT('Ctrl Pts',(-20.5695642742578,15.9743822078091,123.740549105626)) ;
#81933 = CARTESIAN_POINT('Ctrl Pts',(-20.4963847976889,15.9842123308277,123.933856076758)) ;
#81934 = CARTESIAN_POINT('Ctrl Pts',(-20.3884819599051,15.9942789147531,124.115873458542)) ;
#81935 = CARTESIAN_POINT('Ctrl Pts',(-20.2528965388693,16.0041690277675,124.273541553575)) ;
#81936 = CARTESIAN_POINT('Ctrl Pts',(-20.0906428375853,16.0141617165302,124.406954216609)) ;
#81937 = CARTESIAN_POINT('Ctrl Pts',(-19.9081751563257,16.0241226048859,124.509724874185)) ;
#81938 = CARTESIAN_POINT('Ctrl Pts',(-19.7116275426118,16.0340405497659,124.579282843754)) ;
#81939 = CARTESIAN_POINT('Ctrl Pts',(-19.5041323834058,16.0440483028621,124.614214939347)) ;
#81940 = CARTESIAN_POINT('Ctrl Pts',(-19.29326855203,16.0540793968212,124.612157277847)) ;
#81941 = CARTESIAN_POINT('Ctrl Pts',(-19.0896398485272,16.0639273648492,124.574676420677)) ;
#81942 = CARTESIAN_POINT('Ctrl Pts',(-18.8913605350658,16.073989320975,124.50102077639)) ;
#81943 = CARTESIAN_POINT('Ctrl Pts',(-18.7119475644722,16.0838865325762,124.395627492663)) ;
#81944 = CARTESIAN_POINT('Ctrl Pts',(-18.5525797590912,16.0938176992408,124.260752898042)) ;
#81945 = CARTESIAN_POINT('Ctrl Pts',(-18.4177343388883,16.103859883445,124.098313844903)) ;
#81946 = CARTESIAN_POINT('Ctrl Pts',(-18.3146251501111,16.1137465516981,123.917832423583)) ;
#81947 = CARTESIAN_POINT('Ctrl Pts',(-18.2433394533002,16.1237396636764,123.720221174115)) ;
#81948 = CARTESIAN_POINT('Ctrl Pts',(-18.2076942572138,16.1336853412922,123.514192350361)) ;
#81949 = CARTESIAN_POINT('Ctrl Pts',(-18.2079375236498,16.1436326442772,123.305059089537)) ;
#81950 = CARTESIAN_POINT('Ctrl Pts',(-18.2450857238941,16.1536803680239,123.097121717048)) ;
#81951 = CARTESIAN_POINT('Ctrl Pts',(-18.3161807940119,16.1635287417865,122.902670785188)) ;
#81952 = CARTESIAN_POINT('Ctrl Pts',(-18.4205216585494,16.1734877142322,122.721154060357)) ;
#81953 = CARTESIAN_POINT('Ctrl Pts',(-18.5561610324773,16.1835265761133,122.559473799906)) ;
#81954 = CARTESIAN_POINT('Ctrl Pts',(-18.7150408954212,16.1934051802851,122.425694987581)) ;
#81955 = CARTESIAN_POINT('Ctrl Pts',(-18.8977929392953,16.2034567214885,122.319658585763)) ;
#81956 = CARTESIAN_POINT('Ctrl Pts',(-19.0931360052247,16.2133521194688,122.248009860964)) ;
#81957 = CARTESIAN_POINT('Ctrl Pts',(-19.3010941183184,16.2234033520141,122.210689224517)) ;
#81958 = CARTESIAN_POINT('Ctrl Pts',(-19.5089537512372,16.2332895426384,122.210030667253)) ;
#81959 = CARTESIAN_POINT('Ctrl Pts',(-19.7159989180033,16.2432820819541,122.245467035054)) ;
#81960 = CARTESIAN_POINT('Ctrl Pts',(-19.912880843383,16.2532305278489,122.316077257933)) ;
#81961 = CARTESIAN_POINT('Ctrl Pts',(-20.0944193479257,16.2631673303808,122.419404599673)) ;
#81962 = CARTESIAN_POINT('Ctrl Pts',(-20.2562110345139,16.2731503378321,122.553127840936)) ;
#81963 = CARTESIAN_POINT('Ctrl Pts',(-20.392826960401,16.2831941792469,122.714098614043)) ;
#81964 = CARTESIAN_POINT('Ctrl Pts',(-20.4975783868843,16.2930223778708,122.892232473459)) ;
#81965 = CARTESIAN_POINT('Ctrl Pts',(-20.5717018307411,16.303098971313,123.090636621067)) ;
#81966 = CARTESIAN_POINT('Ctrl Pts',(-20.6095109727593,16.3129509706546,123.294322600127)) ;
#81967 = CARTESIAN_POINT('Ctrl Pts',(-20.6115947138046,16.3230245574784,123.506054671263)) ;
#81968 = CARTESIAN_POINT('Ctrl Pts',(-20.5776393567891,16.3328647825759,123.710139991898)) ;
#81969 = CARTESIAN_POINT('Ctrl Pts',(-20.5085932982019,16.3428304866046,123.907927939968)) ;
#81970 = CARTESIAN_POINT('Ctrl Pts',(-20.4053465774814,16.3528571199112,124.091716983098)) ;
#81971 = CARTESIAN_POINT('Ctrl Pts',(-20.2733735919819,16.362771415623,124.253036040026)) ;
#81972 = CARTESIAN_POINT('Ctrl Pts',(-20.1144503949313,16.3727597043154,124.390304188214)) ;
#81973 = CARTESIAN_POINT('Ctrl Pts',(-19.9330154611805,16.3827984374738,124.498096915543)) ;
#81974 = CARTESIAN_POINT('Ctrl Pts',(-19.7395811105255,16.3926417693013,124.571625597567)) ;
#81975 = CARTESIAN_POINT('Ctrl Pts',(-19.5326001724498,16.4026694951809,124.611656473864)) ;
#81976 = CARTESIAN_POINT('Ctrl Pts',(-19.3217012598712,16.4127018315695,124.614568733438)) ;
#81977 = CARTESIAN_POINT('Ctrl Pts',(-19.1176631418604,16.4225313318701,124.581915860113)) ;
#81978 = CARTESIAN_POINT('Ctrl Pts',(-18.9189922527592,16.4325208357869,124.513822081444)) ;
#81979 = CARTESIAN_POINT('Ctrl Pts',(-18.7344293002481,16.4425646762993,124.411248255595)) ;
#81980 = CARTESIAN_POINT('Ctrl Pts',(-18.5738358373638,16.4523863820673,124.281460870642)) ;
#81981 = CARTESIAN_POINT('Ctrl Pts',(-18.434881893899,16.4624214291997,124.12271871664)) ;
#81982 = CARTESIAN_POINT('Ctrl Pts',(-18.3262087635374,16.4724461066366,123.942138990231)) ;
#81983 = CARTESIAN_POINT('Ctrl Pts',(-18.2514329538547,16.482298921491,123.748970510266)) ;
#81984 = CARTESIAN_POINT('Ctrl Pts',(-18.2104254283557,16.4922866310986,123.543056577685)) ;
#81985 = CARTESIAN_POINT('Ctrl Pts',(-18.2058105603721,16.5022166410927,123.334340206634)) ;
#81986 = CARTESIAN_POINT('Ctrl Pts',(-18.2373758713605,16.5122063963118,123.126705719172)) ;
#81987 = CARTESIAN_POINT('Ctrl Pts',(-18.3050193572529,16.5222330049947,122.927059272191)) ;
#81988 = CARTESIAN_POINT('Ctrl Pts',(-18.4046805568282,16.5321169450166,122.7447319742)) ;
#81989 = CARTESIAN_POINT('Ctrl Pts',(-18.5354936535171,16.5421061725551,122.580436407492)) ;
#81990 = CARTESIAN_POINT('Ctrl Pts',(-18.6939750843828,16.5521490430788,122.440936928317)) ;
#81991 = CARTESIAN_POINT('Ctrl Pts',(-18.8703193515889,16.5619814298342,122.33309621936)) ;
#81992 = CARTESIAN_POINT('Ctrl Pts',(-19.0656339220194,16.5719747230058,122.255709958654)) ;
#81993 = CARTESIAN_POINT('Ctrl Pts',(-19.2723178782231,16.5820067286542,122.213677942991)) ;
#81994 = CARTESIAN_POINT('Ctrl Pts',(-19.4796281167346,16.5918719846232,122.208007210698)) ;
#81995 = CARTESIAN_POINT('Ctrl Pts',(-19.6868865943995,16.6018338645307,122.23813162248)) ;
#81996 = CARTESIAN_POINT('Ctrl Pts',(-19.887099697081,16.6118687978926,122.304588583073)) ;
#81997 = CARTESIAN_POINT('Ctrl Pts',(-20.0701600638373,16.6217537562719,122.403012885151)) ;
#81998 = CARTESIAN_POINT('Ctrl Pts',(-20.2362528490299,16.6318193831945,122.534076877196)) ;
#81999 = CARTESIAN_POINT('Ctrl Pts',(-20.3740988588356,16.6416584888589,122.688345892466)) ;
#82000 = CARTESIAN_POINT('Ctrl Pts',(-20.4857489154389,16.6517213038642,122.868002484053)) ;
#82001 = CARTESIAN_POINT('Ctrl Pts',(-20.5630460687322,16.6616175099129,123.061183032358)) ;
#82002 = CARTESIAN_POINT('Ctrl Pts',(-20.6063783427559,16.6715583329382,123.265604149292)) ;
#82003 = CARTESIAN_POINT('Ctrl Pts',(-20.6136572723222,16.6815629159168,123.475829767627)) ;
#82004 = CARTESIAN_POINT('Ctrl Pts',(-20.5840255687026,16.6915838103616,123.68440137035)) ;
#82005 = CARTESIAN_POINT('Ctrl Pts',(-20.519713862323,16.701475730951,123.88217222093)) ;
#82006 = CARTESIAN_POINT('Ctrl Pts',(-20.4213081374851,16.7114691632964,124.067785900772)) ;
#82007 = CARTESIAN_POINT('Ctrl Pts',(-20.2927295608921,16.7214147681962,124.232664555243)) ;
#82008 = CARTESIAN_POINT('Ctrl Pts',(-20.1377257127213,16.7313620416778,124.37306033678)) ;
#82009 = CARTESIAN_POINT('Ctrl Pts',(-19.9587973051972,16.7414099561541,124.48532564178)) ;
#82010 = CARTESIAN_POINT('Ctrl Pts',(-19.7670526137768,16.7512575965015,124.563399289271)) ;
#82011 = CARTESIAN_POINT('Ctrl Pts',(-19.5624702723363,16.7612193118781,124.608137597195)) ;
#82012 = CARTESIAN_POINT('Ctrl Pts',(-19.351788240765,16.7712479354509,124.616465589517)) ;
#82013 = CARTESIAN_POINT('Ctrl Pts',(-19.1453379706875,16.7811582975173,124.588489764781)) ;
#82014 = CARTESIAN_POINT('Ctrl Pts',(-18.9462095070637,16.7910929911697,124.52545651433)) ;
#82015 = CARTESIAN_POINT('Ctrl Pts',(-18.7591671244395,16.8011348342976,124.42758603691)) ;
#82016 = CARTESIAN_POINT('Ctrl Pts',(-18.5944417057161,16.811019339868,124.300871726085)) ;
#82017 = CARTESIAN_POINT('Ctrl Pts',(-18.4524057695084,16.8210214436532,124.145859468398)) ;
#82018 = CARTESIAN_POINT('Ctrl Pts',(-18.340207999891,16.8309397950682,123.970062273976)) ;
#82019 = CARTESIAN_POINT('Ctrl Pts',(-18.2592729248101,16.8409874510891,123.774984976864)) ;
#82020 = CARTESIAN_POINT('Ctrl Pts',(-18.2140000295948,16.8508586441173,123.572415400728)) ;
#82021 = CARTESIAN_POINT('Ctrl Pts',(-18.2043727844571,16.8609243572608,123.361070125236)) ;
#82022 = CARTESIAN_POINT('Ctrl Pts',(-18.230785233552,16.8707768178334,123.15557468565)) ;
#82023 = CARTESIAN_POINT('Ctrl Pts',(-18.3149326595085,16.884205280556,122.88617187367)) ;
#82024 = CARTESIAN_POINT('Ctrl Pts',(-18.4633057586097,16.8972862280731,122.650748676165)) ;
#82025 = CARTESIAN_POINT('Ctrl Pts',(-18.6709271509889,16.9107607263076,122.458191539496)) ;
#82026 = CARTESIAN_POINT('Ctrl Pts',(-18.8447722117222,16.9205928299171,122.346294262746)) ;
#82027 = CARTESIAN_POINT('Ctrl Pts',(-19.0376048145137,16.9305587330438,122.264442659652)) ;
#82028 = CARTESIAN_POINT('Ctrl Pts',(-19.2431084187965,16.940586142354,122.217330844712)) ;
#82029 = CARTESIAN_POINT('Ctrl Pts',(-19.451166029566,16.9504971737206,122.206685708904)) ;
#82030 = CARTESIAN_POINT('Ctrl Pts',(-19.7276789875147,16.9637414813416,122.240089337459)) ;
#82031 = CARTESIAN_POINT('Ctrl Pts',(-20.0569136948359,16.9804419640128,122.372795307525)) ;
#82032 = CARTESIAN_POINT('Ctrl Pts',(-20.318335465656,16.9969487931686,122.60717328351)) ;
#82033 = CARTESIAN_POINT('Ctrl Pts',(-20.4717078308237,17.0102594214062,122.841129236635)) ;
#82034 = CARTESIAN_POINT('Ctrl Pts',(-20.5546945465041,17.0202519849463,123.0341657377)) ;
#82035 = CARTESIAN_POINT('Ctrl Pts',(-20.6028174013198,17.0302820679478,123.239432150588)) ;
#82036 = CARTESIAN_POINT('Ctrl Pts',(-20.6188287669329,17.0434556719456,123.515992319437)) ;
#82037 = CARTESIAN_POINT('Ctrl Pts',(-20.5476980425484,17.060093377177,123.862375167711)) ;
#82038 = CARTESIAN_POINT('Ctrl Pts',(-20.3266354431392,17.0799751397444,124.222885241376)) ;
#82039 = CARTESIAN_POINT('Ctrl Pts',(-20.0488094967542,17.0966714919609,124.443797368873)) ;
#82040 = CARTESIAN_POINT('Ctrl Pts',(-19.7952426665839,17.10982851975,124.554332583483)) ;
#82041 = CARTESIAN_POINT('Ctrl Pts',(-19.5219785942262,17.1232058743935,124.620786207619)) ;
#82042 = CARTESIAN_POINT('Ctrl Pts',(-19.1705568147902,17.1397367086523,124.612580143332)) ;
#82043 = CARTESIAN_POINT('Ctrl Pts',(-18.7748002339287,17.1597013983954,124.459120979636)) ;
#82044 = CARTESIAN_POINT('Ctrl Pts',(-18.4561699434069,17.1796178918191,124.18016633333)) ;
#82045 = CARTESIAN_POINT('Ctrl Pts',(-18.251376561792,17.1995076111686,123.810101526073)) ;
#82046 = CARTESIAN_POINT('Ctrl Pts',(-18.1851276822054,17.2195143408165,123.389957438637)) ;
#82047 = CARTESIAN_POINT('Ctrl Pts',(-18.265260003141,17.2393523944634,122.975738571344)) ;
#82048 = CARTESIAN_POINT('Ctrl Pts',(-18.4831733622697,17.259345732677,122.610816790265)) ;
#82049 = CARTESIAN_POINT('Ctrl Pts',(-18.8110017559419,17.2792285320836,122.343752288443)) ;
#82050 = CARTESIAN_POINT('Ctrl Pts',(-19.2100490249569,17.2991207130023,122.203910324025)) ;
#82051 = CARTESIAN_POINT('Ctrl Pts',(-19.6333306351389,17.3190228914974,122.207929474009)) ;
#82052 = CARTESIAN_POINT('Ctrl Pts',(-20.0320400933982,17.3390602027011,122.357765014815)) ;
#82053 = CARTESIAN_POINT('Ctrl Pts',(-20.3526643050806,17.358872644242,122.6313021622)) ;
#82054 = CARTESIAN_POINT('Ctrl Pts',(-20.56304176731,17.3789378849769,123.002232875681)) ;
#82055 = CARTESIAN_POINT('Ctrl Pts',(-20.6335141765675,17.3986950898327,123.41657822951)) ;
#82056 = CARTESIAN_POINT('Ctrl Pts',(-20.5580063907539,17.4187283624784,123.83557538103)) ;
#82057 = CARTESIAN_POINT('Ctrl Pts',(-20.3461519216991,17.4385412709322,124.199927820861)) ;
#82058 = CARTESIAN_POINT('Ctrl Pts',(-20.0203445224272,17.4585374170597,124.472800756352)) ;
#82059 = CARTESIAN_POINT('Ctrl Pts',(-19.6233800168032,17.4783991702822,124.617465592322)) ;
#82060 = CARTESIAN_POINT('Ctrl Pts',(-19.1967646853301,17.4984676874103,124.617721492029)) ;
#82061 = CARTESIAN_POINT('Ctrl Pts',(-18.8003376642784,17.5182985604071,124.473776925844)) ;
#82062 = CARTESIAN_POINT('Ctrl Pts',(-18.4747560307729,17.5382204712238,124.202953891927)) ;
#82063 = CARTESIAN_POINT('Ctrl Pts',(-18.2610777332137,17.5581499146591,123.836937868401)) ;
#82064 = CARTESIAN_POINT('Ctrl Pts',(-18.1850738365675,17.5780595847755,123.420547828184)) ;
#82065 = CARTESIAN_POINT('Ctrl Pts',(-18.2548694891289,17.5979329420383,123.003739230976)) ;
#82066 = CARTESIAN_POINT('Ctrl Pts',(-18.4639624788878,17.6179244766563,122.633712881794)) ;
#82067 = CARTESIAN_POINT('Ctrl Pts',(-18.7847202419542,17.637790094067,122.35877951611)) ;
#82068 = CARTESIAN_POINT('Ctrl Pts',(-19.1821148442675,17.6577710238952,122.208575263194)) ;
#82069 = CARTESIAN_POINT('Ctrl Pts',(-19.6060391285895,17.6777094859784,122.203480332858)) ;
#82070 = CARTESIAN_POINT('Ctrl Pts',(-20.0055817549243,17.6976016792001,122.342419869265)) ;
#82071 = CARTESIAN_POINT('Ctrl Pts',(-20.3347847387671,17.7175723942355,122.610483331917)) ;
#82072 = CARTESIAN_POINT('Ctrl Pts',(-20.5517123532575,17.7373820659016,122.97165207797)) ;
#82073 = CARTESIAN_POINT('Ctrl Pts',(-20.6333779860565,17.7573752825927,123.388684203349)) ;
#82074 = CARTESIAN_POINT('Ctrl Pts',(-20.5685930951932,17.7772261947891,123.805942343805)) ;
#82075 = CARTESIAN_POINT('Ctrl Pts',(-20.362939595394,17.7973008011081,124.179847955856)) ;
#82076 = CARTESIAN_POINT('Ctrl Pts',(-20.098611386588,17.8138174329915,124.411232739304)) ;
#82077 = CARTESIAN_POINT('Ctrl Pts',(-19.8472361889034,17.8271561406856,124.5354219874)) ;
#82078 = CARTESIAN_POINT('Ctrl Pts',(-19.6486955377895,17.8369985149939,124.59379753129)) ;
#82079 = CARTESIAN_POINT('Ctrl Pts',(-19.4386609397151,17.8470535349766,124.617501312887)) ;
#82080 = CARTESIAN_POINT('Ctrl Pts',(-19.1610336754665,17.8602856916342,124.600234915123)) ;
#82081 = CARTESIAN_POINT('Ctrl Pts',(-18.8258947387444,17.8769006589793,124.488350086626)) ;
#82082 = CARTESIAN_POINT('Ctrl Pts',(-18.5495768294908,17.8934952459905,124.269022287686)) ;
#82083 = CARTESIAN_POINT('Ctrl Pts',(-18.3833597966674,17.9067288143459,124.045859206005)) ;
#82084 = CARTESIAN_POINT('Ctrl Pts',(-18.2885301550365,17.9167724321545,123.857229906636)) ;
#82085 = CARTESIAN_POINT('Ctrl Pts',(-18.2287562614033,17.9266593563894,123.658135422975)) ;
#82086 = CARTESIAN_POINT('Ctrl Pts',(-18.2038373016727,17.9366500108362,123.449600406301)) ;
#82087 = CARTESIAN_POINT('Ctrl Pts',(-18.2155183704076,17.9466117692902,123.240489064376)) ;
#82088 = CARTESIAN_POINT('Ctrl Pts',(-18.2792425265462,17.9599516343574,122.96736967854)) ;
#82089 = CARTESIAN_POINT('Ctrl Pts',(-18.4130348686305,17.9732604172707,122.718034036451)) ;
#82090 = CARTESIAN_POINT('Ctrl Pts',(-18.6026066029756,17.9864561747147,122.515468776243)) ;
#82091 = CARTESIAN_POINT('Ctrl Pts',(-18.7697372859476,17.9964180583912,122.389261077873)) ;
#82092 = CARTESIAN_POINT('Ctrl Pts',(-18.9579188488401,18.0064611679059,122.293522046831)) ;
#82093 = CARTESIAN_POINT('Ctrl Pts',(-19.1559639974618,18.0163134179051,122.232844543332)) ;
#82094 = CARTESIAN_POINT('Ctrl Pts',(-19.3639322401646,18.0262849548556,122.206660737817)) ;
#82095 = CARTESIAN_POINT('Ctrl Pts',(-19.573840915156,18.0362802203331,122.217029724111)) ;
#82096 = CARTESIAN_POINT('Ctrl Pts',(-19.779447227666,18.0463141932067,122.264110388096)) ;
#82097 = CARTESIAN_POINT('Ctrl Pts',(-19.9704605148367,18.0561696079691,122.34442663518)) ;
#82098 = CARTESIAN_POINT('Ctrl Pts',(-20.1472770470841,18.0661688854779,122.458056104505)) ;
#82099 = CARTESIAN_POINT('Ctrl Pts',(-20.3002748716103,18.0760640696409,122.599059938975)) ;
#82100 = CARTESIAN_POINT('Ctrl Pts',(-20.4285143260641,18.0861244492817,122.767212166188)) ;
#82101 = CARTESIAN_POINT('Ctrl Pts',(-20.5237126864081,18.0959743182898,122.951130297099)) ;
#82102 = CARTESIAN_POINT('Ctrl Pts',(-20.5871207089532,18.1060058794977,123.152253484728)) ;
#82103 = CARTESIAN_POINT('Ctrl Pts',(-20.6141694641062,18.11601632838,123.360978666179)) ;
#82104 = CARTESIAN_POINT('Ctrl Pts',(-20.604896382514,18.125923067797,123.569036040792)) ;
#82105 = CARTESIAN_POINT('Ctrl Pts',(-20.5598938047864,18.1358610838654,123.773047836236)) ;
#82106 = CARTESIAN_POINT('Ctrl Pts',(-20.4797271671721,18.1458663303166,123.967538007628)) ;
#82107 = CARTESIAN_POINT('Ctrl Pts',(-20.366397809523,18.1559003913728,124.145444996922)) ;
#82108 = CARTESIAN_POINT('Ctrl Pts',(-20.2268317398703,18.165745472431,124.298300989317)) ;
#82109 = CARTESIAN_POINT('Ctrl Pts',(-20.060776723632,18.1757312783845,124.426689933067)) ;
#82110 = CARTESIAN_POINT('Ctrl Pts',(-19.8759066270791,18.1856660989387,124.523963672816)) ;
#82111 = CARTESIAN_POINT('Ctrl Pts',(-19.6745058024379,18.1957236240709,124.588245907448)) ;
#82112 = CARTESIAN_POINT('Ctrl Pts',(-19.4699075166441,18.2055452747222,124.616238143895)) ;
#82113 = CARTESIAN_POINT('Ctrl Pts',(-19.2586565390616,18.215601338227,124.608486330295)) ;
#82114 = CARTESIAN_POINT('Ctrl Pts',(-19.0543868823573,18.2255420052909,124.564306968047)) ;
#82115 = CARTESIAN_POINT('Ctrl Pts',(-18.8613551751565,18.2354463989569,124.486226473999)) ;
#82116 = CARTESIAN_POINT('Ctrl Pts',(-18.6823712516307,18.2454929227199,124.374127325452)) ;
#82117 = CARTESIAN_POINT('Ctrl Pts',(-18.5277423264652,18.2553890057363,124.234883369432)) ;
#82118 = CARTESIAN_POINT('Ctrl Pts',(-18.3975181426355,18.2654557049663,124.068106618512)) ;
#82119 = CARTESIAN_POINT('Ctrl Pts',(-18.3003841373162,18.2752793153674,123.885816193792)) ;
#82120 = CARTESIAN_POINT('Ctrl Pts',(-18.2345287994309,18.2853351755449,123.68495762991)) ;
#82121 = CARTESIAN_POINT('Ctrl Pts',(-18.2051746041223,18.2952683218498,123.478179409818)) ;
#82122 = CARTESIAN_POINT('Ctrl Pts',(-18.2117492807388,18.3052135776204,123.269226631086)) ;
#82123 = CARTESIAN_POINT('Ctrl Pts',(-18.2545138769522,18.3151968760589,123.063722386448)) ;
#82124 = CARTESIAN_POINT('Ctrl Pts',(-18.3329825492014,18.3252340562055,122.867858860331)) ;
#82125 = CARTESIAN_POINT('Ctrl Pts',(-18.4419876978032,18.335088608915,122.69165785752)) ;
#82126 = CARTESIAN_POINT('Ctrl Pts',(-18.5817046998285,18.3450881273623,122.534632662835)) ;
#82127 = CARTESIAN_POINT('Ctrl Pts',(-18.7447605670421,18.3549832098244,122.405396558866)) ;
#82128 = CARTESIAN_POINT('Ctrl Pts',(-18.9307947270975,18.3650437553305,122.304828639192)) ;
#82129 = CARTESIAN_POINT('Ctrl Pts',(-19.1272549383344,18.3748930625785,122.239367983502)) ;
#82130 = CARTESIAN_POINT('Ctrl Pts',(-19.335695185128,18.3849201526658,122.207938380251)) ;
#82131 = CARTESIAN_POINT('Ctrl Pts',(-19.5464637126567,18.3949490568028,122.213739548366)) ;
#82132 = CARTESIAN_POINT('Ctrl Pts',(-19.7492771311671,18.4047929219021,122.254862772888)) ;
#82133 = CARTESIAN_POINT('Ctrl Pts',(-19.9450396765661,18.4147887486105,122.331265523239)) ;
#82134 = CARTESIAN_POINT('Ctrl Pts',(-20.1248922159333,18.4248139652595,122.441153309289)) ;
#82135 = CARTESIAN_POINT('Ctrl Pts',(-20.2809828268305,18.4347037974171,122.578506486257)) ;
#82136 = CARTESIAN_POINT('Ctrl Pts',(-20.4123979974566,18.4446946535018,122.742346656916)) ;
#82137 = CARTESIAN_POINT('Ctrl Pts',(-20.512875040643,18.4546397480947,122.925697224082)) ;
#82138 = CARTESIAN_POINT('Ctrl Pts',(-20.5804101851488,18.4645916518628,123.123726283587)) ;
#82139 = CARTESIAN_POINT('Ctrl Pts',(-20.612623320595,18.4746280513322,123.332244177723)) ;
#82140 = CARTESIAN_POINT('Ctrl Pts',(-20.608359655852,18.4845171214209,123.540106555575)) ;
#82141 = CARTESIAN_POINT('Ctrl Pts',(-20.5680335601972,18.4945064107918,123.746199638526)) ;
#82142 = CARTESIAN_POINT('Ctrl Pts',(-20.4926226085068,18.5044649770015,123.941500179011)) ;
#82143 = CARTESIAN_POINT('Ctrl Pts',(-20.3855172625548,18.5143645482183,124.119959380232)) ;
#82144 = CARTESIAN_POINT('Ctrl Pts',(-20.2469737641147,18.5244124626325,124.279390783866)) ;
#82145 = CARTESIAN_POINT('Ctrl Pts',(-20.0854054590516,18.5343078054931,124.410487000382)) ;
#82146 = CARTESIAN_POINT('Ctrl Pts',(-19.9005352475718,18.5443694994405,124.513234875)) ;
#82147 = CARTESIAN_POINT('Ctrl Pts',(-19.7049300850852,18.5542139525247,124.580875665388)) ;
#82148 = CARTESIAN_POINT('Ctrl Pts',(-19.498273946928,18.5641746374831,124.614633531059)) ;
#82149 = CARTESIAN_POINT('Ctrl Pts',(-19.2873015921753,18.5742105699917,124.611621178761)) ;
#82150 = CARTESIAN_POINT('Ctrl Pts',(-19.0830712792715,18.5840991856797,124.572810355091)) ;
#82151 = CARTESIAN_POINT('Ctrl Pts',(-18.8860431848826,18.5941135948222,124.498576084643)) ;
#82152 = CARTESIAN_POINT('Ctrl Pts',(-18.7048498408381,18.60414740378,124.390593284749)) ;
#82153 = CARTESIAN_POINT('Ctrl Pts',(-18.5479907947063,18.6139778580362,124.255995839856)) ;
#82154 = CARTESIAN_POINT('Ctrl Pts',(-18.4135763365836,18.6240555256144,124.092282621306)) ;
#82155 = CARTESIAN_POINT('Ctrl Pts',(-18.3118234906073,18.6339073937366,123.911832218199)) ;
#82156 = CARTESIAN_POINT('Ctrl Pts',(-18.2412636801989,18.643980431302,123.712204324392)) ;
#82157 = CARTESIAN_POINT('Ctrl Pts',(-18.2072562008697,18.6538229846528,123.508079026734)) ;
#82158 = CARTESIAN_POINT('Ctrl Pts',(-18.2085295969781,18.6638033801463,123.298272657034)) ;
#82159 = CARTESIAN_POINT('Ctrl Pts',(-18.2467612461067,18.6738218581241,123.091156421006)) ;
#82160 = CARTESIAN_POINT('Ctrl Pts',(-18.3189753825504,18.6837051724301,122.896304492424)) ;
#82161 = CARTESIAN_POINT('Ctrl Pts',(-18.4259403191284,18.6937734749689,122.713693094242)) ;
#82162 = CARTESIAN_POINT('Ctrl Pts',(-18.559602694153,18.7036035222423,122.556032920979)) ;
#82163 = CARTESIAN_POINT('Ctrl Pts',(-18.7222140012075,18.7136703936578,122.420633660617)) ;
#82164 = CARTESIAN_POINT('Ctrl Pts',(-18.902732128757,18.7235594324569,122.317446999546)) ;
#82165 = CARTESIAN_POINT('Ctrl Pts',(-19.1003669108627,18.733556130591,122.246036925525)) ;
#82166 = CARTESIAN_POINT('Ctrl Pts',(-19.3065324036651,18.7435085563029,122.210267846884)) ;
#82167 = CARTESIAN_POINT('Ctrl Pts',(-19.515513806108,18.7534498585359,122.210548414054)) ;
#82168 = CARTESIAN_POINT('Ctrl Pts',(-19.7222190007818,18.7634330976198,122.247050242627)) ;
#82169 = CARTESIAN_POINT('Ctrl Pts',(-19.9203917966261,18.7734718991884,122.319582333041)) ;
#82170 = CARTESIAN_POINT('Ctrl Pts',(-20.0997259540497,18.78332000531,122.423079562139)) ;
#82171 = CARTESIAN_POINT('Ctrl Pts',(-20.2618814355052,18.7933802008854,122.558833866396)) ;
#82172 = CARTESIAN_POINT('Ctrl Pts',(-20.3956744733974,18.8032778841968,122.718208717392)) ;
#82173 = CARTESIAN_POINT('Ctrl Pts',(-20.500699852914,18.8132089245708,122.898646703033)) ;
#82174 = CARTESIAN_POINT('Ctrl Pts',(-20.5733935792951,18.8232511422274,123.096852695664)) ;
#82175 = CARTESIAN_POINT('Ctrl Pts',(-20.6101416824105,18.8331378029614,123.301436586852)) ;
#82176 = CARTESIAN_POINT('Ctrl Pts',(-20.6111685252256,18.8431309115638,123.511509895884)) ;
#82177 = CARTESIAN_POINT('Ctrl Pts',(-20.5757926368399,18.8530766102021,123.717585377804)) ;
#82178 = CARTESIAN_POINT('Ctrl Pts',(-20.5055613870211,18.8630238324731,123.914572351637)) ;
#82179 = CARTESIAN_POINT('Ctrl Pts',(-20.4009471133785,18.8730718580533,124.098082373486)) ;
#82180 = CARTESIAN_POINT('Ctrl Pts',(-20.2688858623514,18.8829191051962,124.257508865836)) ;
#82181 = CARTESIAN_POINT('Ctrl Pts',(-20.1097243653322,18.8928822822869,124.393663555677)) ;
#82182 = CARTESIAN_POINT('Ctrl Pts',(-19.9279708858338,18.9029120033203,124.500552461279)) ;
#82183 = CARTESIAN_POINT('Ctrl Pts',(-19.7329558262972,18.9128164708532,124.573584982313)) ;
#82184 = CARTESIAN_POINT('Ctrl Pts',(-19.5257968131938,18.922840956683,124.612170961109)) ;
#82185 = CARTESIAN_POINT('Ctrl Pts',(-19.3175695516905,18.9327447918069,124.614349948157)) ;
#82186 = CARTESIAN_POINT('Ctrl Pts',(-19.1091146460019,18.9427959825169,124.579889389743)) ;
#82187 = CARTESIAN_POINT('Ctrl Pts',(-18.9130619745761,18.9526804251752,124.510943593051)) ;
#82188 = CARTESIAN_POINT('Ctrl Pts',(-18.729812387142,18.962673433027,124.408243899049)) ;
#82189 = CARTESIAN_POINT('Ctrl Pts',(-18.5679260209722,18.9726217527433,124.275805077291)) ;
#82190 = CARTESIAN_POINT('Ctrl Pts',(-18.43144613634,18.9825585914528,124.117671370071)) ;
#82191 = CARTESIAN_POINT('Ctrl Pts',(-18.3237491330142,18.9925415803724,123.937505527869)) ;
#82192 = CARTESIAN_POINT('Ctrl Pts',(-18.2488966397258,19.0025854597365,123.74009037589)) ;
#82193 = CARTESIAN_POINT('Ctrl Pts',(-18.209813065763,19.0124135250949,123.537170735293)) ;
#82194 = CARTESIAN_POINT('Ctrl Pts',(-18.2063851574917,19.0224906136498,123.325393194983)) ;
#82195 = CARTESIAN_POINT('Ctrl Pts',(-18.2389095766539,19.0323407658061,123.120827998228)) ;
#82196 = CARTESIAN_POINT('Ctrl Pts',(-18.3079229039894,19.0424212462584,122.920512664248)) ;
#82197 = CARTESIAN_POINT('Ctrl Pts',(-18.4078474700848,19.0522357440273,122.739938974569)) ;
#82198 = CARTESIAN_POINT('Ctrl Pts',(-18.5406432867953,19.0623040400474,122.575174067644)) ;
#82199 = CARTESIAN_POINT('Ctrl Pts',(-18.6974620235744,19.0722028725302,122.438290128418)) ;
#82200 = CARTESIAN_POINT('Ctrl Pts',(-18.8783200381135,19.0822557525447,122.329027971715)) ;
#82201 = CARTESIAN_POINT('Ctrl Pts',(-19.0718217296824,19.0921255680409,122.254003566536)) ;
#82202 = CARTESIAN_POINT('Ctrl Pts',(-19.2795065095552,19.1021982491237,122.212846725004)) ;
#82203 = CARTESIAN_POINT('Ctrl Pts',(-19.486188422999,19.1120307276946,122.208399680051)) ;
#82204 = CARTESIAN_POINT('Ctrl Pts',(-19.6946842168501,19.1220613616807,122.239936675267)) ;
#82205 = CARTESIAN_POINT('Ctrl Pts',(-19.8943771096132,19.1320929188999,122.307793559759)) ;
#82206 = CARTESIAN_POINT('Ctrl Pts',(-20.0757189797169,19.1419226277716,122.406859095438)) ;
#82207 = CARTESIAN_POINT('Ctrl Pts',(-20.2401349998331,19.1519120765737,122.537526739617)) ;
#82208 = CARTESIAN_POINT('Ctrl Pts',(-20.3797167257988,19.1619559289737,122.695962343136)) ;
#82209 = CARTESIAN_POINT('Ctrl Pts',(-20.4876019773481,19.1717776423058,122.872018751571)) ;
#82210 = CARTESIAN_POINT('Ctrl Pts',(-20.5654043920265,19.1818126472945,123.068115049024)) ;
#82211 = CARTESIAN_POINT('Ctrl Pts',(-20.6073616916099,19.1918374857421,123.274657345158)) ;
#82212 = CARTESIAN_POINT('Ctrl Pts',(-20.6131682474204,19.2016896986973,123.48170036684)) ;
#82213 = CARTESIAN_POINT('Ctrl Pts',(-20.5828695009904,19.2116796548911,123.689507417309)) ;
#82214 = CARTESIAN_POINT('Ctrl Pts',(-20.5173663448206,19.2216077651743,123.887689668796)) ;
#82215 = CARTESIAN_POINT('Ctrl Pts',(-20.418139793369,19.2315963652539,124.072765163294)) ;
#82216 = CARTESIAN_POINT('Ctrl Pts',(-20.2875636494693,19.2416229571814,124.238246501146)) ;
#82217 = CARTESIAN_POINT('Ctrl Pts',(-20.1326099243232,19.2515080852456,124.376719379815)) ;
#82218 = CARTESIAN_POINT('Ctrl Pts',(-19.9543134180587,19.2614992027191,124.487770824645)) ;
#82219 = CARTESIAN_POINT('Ctrl Pts',(-19.7583197917987,19.2715398185709,124.566149257661)) ;
#82220 = CARTESIAN_POINT('Ctrl Pts',(-19.5560396568112,19.2813728094246,124.608747665679)) ;
#82221 = CARTESIAN_POINT('Ctrl Pts',(-19.3460913751893,19.2913659408749,124.616289970547)) ;
#82222 = CARTESIAN_POINT('Ctrl Pts',(-19.1372600744288,19.3013979893103,124.586714092898)) ;
#82223 = CARTESIAN_POINT('Ctrl Pts',(-18.9400108934153,19.3112632358527,124.522664185443)) ;
#82224 = CARTESIAN_POINT('Ctrl Pts',(-18.7547919716297,19.3212251106795,124.42490173768)) ;
#82225 = CARTESIAN_POINT('Ctrl Pts',(-18.5883738308643,19.3312600737908,124.295260107016)) ;
#82226 = CARTESIAN_POINT('Ctrl Pts',(-18.4488190485599,19.3411449182532,124.141239793615)) ;
#82227 = CARTESIAN_POINT('Ctrl Pts',(-18.3361799509214,19.3512109710939,123.962131077529)) ;
#82228 = CARTESIAN_POINT('Ctrl Pts',(-18.2579205679467,19.3610484870029,123.770652745803)) ;
#82229 = CARTESIAN_POINT('Ctrl Pts',(-18.2128628982536,19.3711172351118,123.563864379788)) ;
#82230 = CARTESIAN_POINT('Ctrl Pts',(-18.2046274737914,19.3809977521428,123.356276336326)) ;
#82231 = CARTESIAN_POINT('Ctrl Pts',(-18.2324438381508,19.3909889390772,123.148111150481)) ;
#82232 = CARTESIAN_POINT('Ctrl Pts',(-18.295726868169,19.4009420053522,122.948631988173)) ;
#82233 = CARTESIAN_POINT('Ctrl Pts',(-18.3935294192508,19.4109778428848,122.7617040229)) ;
#82234 = CARTESIAN_POINT('Ctrl Pts',(-18.52033969625,19.4208679690962,122.596912733029)) ;
#82235 = CARTESIAN_POINT('Ctrl Pts',(-18.6751751290804,19.4308601510042,122.454963151658)) ;
#82236 = CARTESIAN_POINT('Ctrl Pts',(-18.8515331266452,19.4408060909428,122.342630531984)) ;
#82237 = CARTESIAN_POINT('Ctrl Pts',(-19.0445885211167,19.4507532747068,122.262219660309)) ;
#82238 = CARTESIAN_POINT('Ctrl Pts',(-19.2507744026111,19.4608012130143,122.216323259587)) ;
#82239 = CARTESIAN_POINT('Ctrl Pts',(-19.4575916167922,19.4706488477546,122.206936574078)) ;
#82240 = CARTESIAN_POINT('Ctrl Pts',(-19.665347647943,19.4806105617284,122.233259207866)) ;
#82241 = CARTESIAN_POINT('Ctrl Pts',(-19.8666638852989,19.4906391965192,122.295933848434)) ;
#82242 = CARTESIAN_POINT('Ctrl Pts',(-20.0518399911396,19.5005495151164,122.391400478421)) ;
#82243 = CARTESIAN_POINT('Ctrl Pts',(-20.2183835123299,19.5104843714279,122.517455349615)) ;
#82244 = CARTESIAN_POINT('Ctrl Pts',(-20.3618707138859,19.5205256073886,122.672277289521)) ;
#82245 = CARTESIAN_POINT('Ctrl Pts',(-20.4746969570894,19.5304123789686,122.846864648244)) ;
#82246 = CARTESIAN_POINT('Ctrl Pts',(-20.5566359414748,19.5404125576748,123.040441264708)) ;
#82247 = CARTESIAN_POINT('Ctrl Pts',(-20.6035192091407,19.5503298358844,123.243629797779)) ;
#82248 = CARTESIAN_POINT('Ctrl Pts',(-20.6144848722906,19.560377082298,123.454540489081)) ;
#82249 = CARTESIAN_POINT('Ctrl Pts',(-20.5893212879762,19.5702509712793,123.660622657951)) ;
#82250 = CARTESIAN_POINT('Ctrl Pts',(-20.5277315386694,19.5803129888599,123.862966123418)) ;
#82251 = CARTESIAN_POINT('Ctrl Pts',(-20.4337174008764,19.5901840505942,124.047986023597)) ;
#82252 = CARTESIAN_POINT('Ctrl Pts',(-20.3079299585367,19.6001781139545,124.216278196079)) ;
#82253 = CARTESIAN_POINT('Ctrl Pts',(-20.1539324806393,19.6102102719879,124.36037634443)) ;
#82254 = CARTESIAN_POINT('Ctrl Pts',(-19.9804428606357,19.620074148228,124.474010290571)) ;
#82255 = CARTESIAN_POINT('Ctrl Pts',(-19.7859181324196,19.6301446628663,124.557511621058)) ;
#82256 = CARTESIAN_POINT('Ctrl Pts',(-19.5845187702975,19.6399852998073,124.604891310649)) ;
#82257 = CARTESIAN_POINT('Ctrl Pts',(-19.3753708163134,19.6499524286475,124.617420938823)) ;
#82258 = CARTESIAN_POINT('Ctrl Pts',(-19.1662428926851,19.659966401772,124.593109655886)) ;
#82259 = CARTESIAN_POINT('Ctrl Pts',(-18.8985886193499,19.6732511356353,124.513253218145)) ;
#82260 = CARTESIAN_POINT('Ctrl Pts',(-18.6588872460886,19.68647640035,124.36624963569)) ;
#82261 = CARTESIAN_POINT('Ctrl Pts',(-18.4660700314843,19.6997869229049,124.163476334807)) ;
#82262 = CARTESIAN_POINT('Ctrl Pts',(-18.3496595586421,19.7098155678071,123.987691638222)) ;
#82263 = CARTESIAN_POINT('Ctrl Pts',(-18.2666103147507,19.719696600161,123.797282030804)) ;
#82264 = CARTESIAN_POINT('Ctrl Pts',(-18.2169671329577,19.7296775728411,123.593407967415)) ;
#82265 = CARTESIAN_POINT('Ctrl Pts',(-18.2036560520165,19.7396587004271,123.384012355789)) ;
#82266 = CARTESIAN_POINT('Ctrl Pts',(-18.2339327364672,19.7529018906885,123.107170942939)) ;
#82267 = CARTESIAN_POINT('Ctrl Pts',(-18.3623905339946,19.7695698860493,122.776996583947)) ;
#82268 = CARTESIAN_POINT('Ctrl Pts',(-18.5937075192732,19.7860903860613,122.512484152482)) ;
#82269 = CARTESIAN_POINT('Ctrl Pts',(-18.8258990467803,19.7994034023773,122.356364032903)) ;
#82270 = CARTESIAN_POINT('Ctrl Pts',(-19.0164084560592,19.8093199606103,122.271584830569)) ;
#82271 = CARTESIAN_POINT('Ctrl Pts',(-19.2209351105263,19.8193476289132,122.220706890432)) ;
#82272 = CARTESIAN_POINT('Ctrl Pts',(-19.4974375044467,19.8325282186578,122.200845480391)) ;
#82273 = CARTESIAN_POINT('Ctrl Pts',(-19.8469032671938,19.8492763577772,122.268339890241)) ;
#82274 = CARTESIAN_POINT('Ctrl Pts',(-20.2084084237355,19.8690711002878,122.484283560404)) ;
#82275 = CARTESIAN_POINT('Ctrl Pts',(-20.4779908187138,19.8891154930966,122.814197860746)) ;
#82276 = CARTESIAN_POINT('Ctrl Pts',(-20.6171058432914,19.9089546753953,123.212554236894)) ;
#82277 = CARTESIAN_POINT('Ctrl Pts',(-20.6129557723522,19.9288799990882,123.636097670843)) ;
#82278 = CARTESIAN_POINT('Ctrl Pts',(-20.464422658849,19.9488036371397,124.032909206255)) ;
#82279 = CARTESIAN_POINT('Ctrl Pts',(-20.18955447349,19.9687285106052,124.355231228581)) ;
#82280 = CARTESIAN_POINT('Ctrl Pts',(-19.8222578423576,19.9886071176841,124.564437264234)) ;
#82281 = CARTESIAN_POINT('Ctrl Pts',(-19.403615042977,20.0085845605161,124.636299305193)) ;
#82282 = CARTESIAN_POINT('Ctrl Pts',(-18.9865389485054,20.0285164086008,124.560857289686)) ;
#82283 = CARTESIAN_POINT('Ctrl Pts',(-18.6207630528678,20.0484116769434,124.348399240722)) ;
#82284 = CARTESIAN_POINT('Ctrl Pts',(-18.3486870871748,20.0683341753555,124.023705533677)) ;
#82285 = CARTESIAN_POINT('Ctrl Pts',(-18.203574404514,20.0882936572315,123.624866923908)) ;
#82286 = CARTESIAN_POINT('Ctrl Pts',(-18.2031996447165,20.1081714096908,123.202277453472)) ;
#82287 = CARTESIAN_POINT('Ctrl Pts',(-18.346002051333,20.1280532004254,122.804297838567)) ;
#82288 = CARTESIAN_POINT('Ctrl Pts',(-18.6192053764453,20.1481265392764,122.476459381856)) ;
#82289 = CARTESIAN_POINT('Ctrl Pts',(-18.98301587099,20.1679310065122,122.264237767861)) ;
#82290 = CARTESIAN_POINT('Ctrl Pts',(-19.4008364759886,20.18791434692,122.18732233124)) ;
#82291 = CARTESIAN_POINT('Ctrl Pts',(-19.8183361021273,20.207829311518,122.258043575574)) ;
#82292 = CARTESIAN_POINT('Ctrl Pts',(-20.1864344857312,20.2276978462343,122.465512799918)) ;
#82293 = CARTESIAN_POINT('Ctrl Pts',(-20.4635252494409,20.2477502304461,122.789401507206)) ;
#82294 = CARTESIAN_POINT('Ctrl Pts',(-20.6120084813329,20.2675241942353,123.182939564041)) ;
#82295 = CARTESIAN_POINT('Ctrl Pts',(-20.6176872102052,20.2875785732566,123.609141239229)) ;
#82296 = CARTESIAN_POINT('Ctrl Pts',(-20.4791319362288,20.3073753108299,124.00674845248)) ;
#82297 = CARTESIAN_POINT('Ctrl Pts',(-20.2119684125399,20.3273431231813,124.336599903747)) ;
#82298 = CARTESIAN_POINT('Ctrl Pts',(-19.8479480817942,20.3473020992464,124.554908135789)) ;
#82299 = CARTESIAN_POINT('Ctrl Pts',(-19.4327659312794,20.3671970175238,124.635876929889)) ;
#82300 = CARTESIAN_POINT('Ctrl Pts',(-19.0147876905116,20.3870933299741,124.570821089718)) ;
#82301 = CARTESIAN_POINT('Ctrl Pts',(-18.6435959691219,20.4070012633482,124.367296800333)) ;
#82302 = CARTESIAN_POINT('Ctrl Pts',(-18.3636276837222,20.4269511536367,124.048670511752)) ;
#82303 = CARTESIAN_POINT('Ctrl Pts',(-18.2093280562878,20.446828384138,123.655155581433)) ;
#82304 = CARTESIAN_POINT('Ctrl Pts',(-18.198304793453,20.466811053009,123.230434093372)) ;
#82305 = CARTESIAN_POINT('Ctrl Pts',(-18.3328373858692,20.4867439395894,122.828470917943)) ;
#82306 = CARTESIAN_POINT('Ctrl Pts',(-18.5959298066078,20.5066566856073,122.496768356092)) ;
#82307 = CARTESIAN_POINT('Ctrl Pts',(-18.895676555151,20.5232264069491,122.311681507848)) ;
#82308 = CARTESIAN_POINT('Ctrl Pts',(-19.1634853018324,20.5365264182541,122.231185644961)) ;
#82309 = CARTESIAN_POINT('Ctrl Pts',(-19.4404546522305,20.549796606004,122.198099948954)) ;
#82310 = CARTESIAN_POINT('Ctrl Pts',(-19.7904975982779,20.5664239883694,122.248239271014)) ;
#82311 = CARTESIAN_POINT('Ctrl Pts',(-20.1021496586214,20.5830462781146,122.414851991892)) ;
#82312 = CARTESIAN_POINT('Ctrl Pts',(-20.305538571328,20.5962914925091,122.60507349097)) ;
#82313 = CARTESIAN_POINT('Ctrl Pts',(-20.4311937815454,20.6062034574698,122.77131708526)) ;
#82314 = CARTESIAN_POINT('Ctrl Pts',(-20.5272486919017,20.6162620806342,122.959681415796)) ;
#82315 = CARTESIAN_POINT('Ctrl Pts',(-20.5881005962991,20.62610219475,123.157431298094)) ;
#82316 = CARTESIAN_POINT('Ctrl Pts',(-20.6144821793486,20.6361679797077,123.367363458734)) ;
#82317 = CARTESIAN_POINT('Ctrl Pts',(-20.6041090188649,20.6460512974956,123.574910030849)) ;
#82318 = CARTESIAN_POINT('Ctrl Pts',(-20.5578169159025,20.6560407353541,123.779732824598)) ;
#82319 = CARTESIAN_POINT('Ctrl Pts',(-20.4767917351146,20.6660044494069,123.972907172998)) ;
#82320 = CARTESIAN_POINT('Ctrl Pts',(-20.363282775576,20.6759994610661,124.149756048535)) ;
#82321 = CARTESIAN_POINT('Ctrl Pts',(-20.2199777436041,20.6860357527603,124.304604665341)) ;
#82322 = CARTESIAN_POINT('Ctrl Pts',(-20.0553288276782,20.6958821304538,124.430086219133)) ;
#82323 = CARTESIAN_POINT('Ctrl Pts',(-19.8690272051789,20.7058670746045,124.526746885253)) ;
#82324 = CARTESIAN_POINT('Ctrl Pts',(-19.6697103598208,20.7158040457344,124.589424857213)) ;
#82325 = CARTESIAN_POINT('Ctrl Pts',(-19.4602253401753,20.7258538303662,124.616732469471)) ;
#82326 = CARTESIAN_POINT('Ctrl Pts',(-19.253324082945,20.7357042924436,124.607595743279)) ;
#82327 = CARTESIAN_POINT('Ctrl Pts',(-19.0485802151792,20.7456763059641,124.562661428666)) ;
#82328 = CARTESIAN_POINT('Ctrl Pts',(-18.8542534350798,20.7556714530835,124.482625689863)) ;
#82329 = CARTESIAN_POINT('Ctrl Pts',(-18.6762666846949,20.7657054228196,124.36943917364)) ;
#82330 = CARTESIAN_POINT('Ctrl Pts',(-18.5231567953254,20.7755609684902,124.229814819193)) ;
#82331 = CARTESIAN_POINT('Ctrl Pts',(-18.394575811181,20.7855597255034,124.063565093148)) ;
#82332 = CARTESIAN_POINT('Ctrl Pts',(-18.2976014743614,20.7954568607406,123.87944119294)) ;
#82333 = CARTESIAN_POINT('Ctrl Pts',(-18.2330490484476,20.8055099565802,123.678215684589)) ;
#82334 = CARTESIAN_POINT('Ctrl Pts',(-18.2048744104078,20.8153934653108,123.472337923428)) ;
#82335 = CARTESIAN_POINT('Ctrl Pts',(-18.2124727925747,20.8253883379569,123.262357979921)) ;
#82336 = CARTESIAN_POINT('Ctrl Pts',(-18.2568500096631,20.8354082995926,123.056422212533)) ;
#82337 = CARTESIAN_POINT('Ctrl Pts',(-18.3352337461589,20.8453136633924,122.863498944733)) ;
#82338 = CARTESIAN_POINT('Ctrl Pts',(-18.4459506865734,20.855254251,122.686271481203)) ;
#82339 = CARTESIAN_POINT('Ctrl Pts',(-18.5865697971061,20.8652570691006,122.529879035352)) ;
#82340 = CARTESIAN_POINT('Ctrl Pts',(-18.7529194184332,20.8752917808248,122.400158067132)) ;
#82341 = CARTESIAN_POINT('Ctrl Pts',(-18.9355983712862,20.8851366875621,122.302840177009)) ;
#82342 = CARTESIAN_POINT('Ctrl Pts',(-19.1350505907235,20.8951225401311,122.237440608609)) ;
#82343 = CARTESIAN_POINT('Ctrl Pts',(-19.3418166620123,20.9050573485441,122.20766040024)) ;
#82344 = CARTESIAN_POINT('Ctrl Pts',(-19.5531166794157,20.9151148756252,122.214501576206)) ;
#82345 = CARTESIAN_POINT('Ctrl Pts',(-19.755282382907,20.9249365306223,122.256609777774)) ;
#82346 = CARTESIAN_POINT('Ctrl Pts',(-19.9517518328601,20.9349925747953,122.334626535932)) ;
#82347 = CARTESIAN_POINT('Ctrl Pts',(-20.1294511445661,20.9449333148405,122.444634048167)) ;
#82348 = CARTESIAN_POINT('Ctrl Pts',(-20.2852058392503,20.9548374359133,122.582819935686)) ;
#82349 = CARTESIAN_POINT('Ctrl Pts',(-20.4163627073902,20.9648849770676,122.748380027201)) ;
#82350 = CARTESIAN_POINT('Ctrl Pts',(-20.5154483160002,20.974783728668,122.931410768418)) ;
#82351 = CARTESIAN_POINT('Ctrl Pts',(-20.5823152000268,20.9848322076338,123.131775211427)) ;
#82352 = CARTESIAN_POINT('Ctrl Pts',(-20.6129012298034,20.9947197047175,123.337400837279)) ;
#82353 = CARTESIAN_POINT('Ctrl Pts',(-20.6076505386233,21.0047127950156,123.547403033291)) ;
#82354 = CARTESIAN_POINT('Ctrl Pts',(-20.5661097269182,21.0146649650759,123.752476419101)) ;
#82355 = CARTESIAN_POINT('Ctrl Pts',(-20.489974800567,21.0246033849904,123.947032286064)) ;
#82356 = CARTESIAN_POINT('Ctrl Pts',(-20.3808873584294,21.034588515076,124.126405174509)) ;
#82357 = CARTESIAN_POINT('Ctrl Pts',(-20.2413837740045,21.0446252044901,124.284693816363)) ;
#82358 = CARTESIAN_POINT('Ctrl Pts',(-20.0796866049328,21.0544798884826,124.414245633382)) ;
#82359 = CARTESIAN_POINT('Ctrl Pts',(-19.8954680695033,21.0644793725304,124.515444105572)) ;
#82360 = CARTESIAN_POINT('Ctrl Pts',(-19.6985589416017,21.0743744613073,124.582645268236)) ;
#82361 = CARTESIAN_POINT('Ctrl Pts',(-19.4895929842184,21.0844350159535,124.615139996336)) ;
#82362 = CARTESIAN_POINT('Ctrl Pts',(-19.2825548193412,21.0942842803264,124.611063574309)) ;
#82363 = CARTESIAN_POINT('Ctrl Pts',(-19.0756156897001,21.1043115327742,124.570906278873)) ;
#82364 = CARTESIAN_POINT('Ctrl Pts',(-18.8789572087526,21.1143398303444,124.494897176349)) ;
#82365 = CARTESIAN_POINT('Ctrl Pts',(-18.7015724696845,21.1241859593504,124.388226917804)) ;
#82366 = CARTESIAN_POINT('Ctrl Pts',(-18.5427085112095,21.1341798647124,124.250730179564)) ;
#82367 = CARTESIAN_POINT('Ctrl Pts',(-18.4100202913512,21.1442039623955,124.0870024506)) ;
#82368 = CARTESIAN_POINT('Ctrl Pts',(-18.3089182683856,21.1540937902495,123.905319990407)) ;
#82369 = CARTESIAN_POINT('Ctrl Pts',(-18.2399098881066,21.1640857716799,123.706924554748)) ;
#82370 = CARTESIAN_POINT('Ctrl Pts',(-18.2065962274029,21.1740327764458,123.500477641717)) ;
#82371 = CARTESIAN_POINT('Ctrl Pts',(-18.2092510439381,21.1839824278356,123.291312971923)) ;
#82372 = CARTESIAN_POINT('Ctrl Pts',(-18.2486917570198,21.194019430813,123.084028422543)) ;
#82373 = CARTESIAN_POINT('Ctrl Pts',(-18.3222881608881,21.203908339248,122.889587468432)) ;
#82374 = CARTESIAN_POINT('Ctrl Pts',(-18.429273753743,21.2138976717255,122.708880714178)) ;
#82375 = CARTESIAN_POINT('Ctrl Pts',(-18.5657078725449,21.2238562271626,122.550089089031)) ;
#82376 = CARTESIAN_POINT('Ctrl Pts',(-18.7263705845267,21.2337557983631,122.417776071601)) ;
#82377 = CARTESIAN_POINT('Ctrl Pts',(-18.9102889857896,21.2438037236151,122.313916744243)) ;
#82378 = CARTESIAN_POINT('Ctrl Pts',(-19.1064181843842,21.2536990231411,122.244464755994)) ;
#82379 = CARTESIAN_POINT('Ctrl Pts',(-19.3150200723039,21.263760879589,122.209527188093)) ;
#82380 = CARTESIAN_POINT('Ctrl Pts',(-19.5219709540585,21.2736047260057,122.21125922334)) ;
#82381 = CARTESIAN_POINT('Ctrl Pts',(-19.7280504821707,21.2835676751337,122.248639614342)) ;
#82382 = CARTESIAN_POINT('Ctrl Pts',(-19.9258060478764,21.2936017115617,122.322083795872)) ;
#82383 = CARTESIAN_POINT('Ctrl Pts',(-20.1052484653061,21.3034891385198,122.426997625945)) ;
#82384 = CARTESIAN_POINT('Ctrl Pts',(-20.2660567351159,21.3135035728562,122.562908279566)) ;
#82385 = CARTESIAN_POINT('Ctrl Pts',(-20.4006745778762,21.3235385174911,122.725323864246)) ;
#82386 = CARTESIAN_POINT('Ctrl Pts',(-20.5034505638933,21.3333708675221,122.904698004707)) ;
#82387 = CARTESIAN_POINT('Ctrl Pts',(-20.5752878328286,21.3434463066393,123.103919084727)) ;
#82388 = CARTESIAN_POINT('Ctrl Pts',(-20.6107746375596,21.3532987718739,123.308030795076)) ;
#82389 = CARTESIAN_POINT('Ctrl Pts',(-20.6104406096869,21.3633716494508,123.51975852017)) ;
#82390 = CARTESIAN_POINT('Ctrl Pts',(-20.5741595231419,21.3732142456433,123.723492699423)) ;
#82391 = CARTESIAN_POINT('Ctrl Pts',(-20.502730586389,21.3831946297586,123.920769607282)) ;
#82392 = CARTESIAN_POINT('Ctrl Pts',(-20.3973760350854,21.3932131104074,124.103140698037)) ;
#82393 = CARTESIAN_POINT('Ctrl Pts',(-20.2641044764514,21.4030964254077,124.262579989455)) ;
#82394 = CARTESIAN_POINT('Ctrl Pts',(-20.1021843288943,21.4131647224982,124.398852256054)) ;
#82395 = CARTESIAN_POINT('Ctrl Pts',(-19.9234578599345,21.4229947908705,124.502677758348)) ;
#82396 = CARTESIAN_POINT('Ctrl Pts',(-19.7249073454882,21.4330615833389,124.575830411415)) ;
#82397 = CARTESIAN_POINT('Ctrl Pts',(-19.5202525728482,21.4429509168274,124.612656973868)) ;
#82398 = CARTESIAN_POINT('Ctrl Pts',(-19.310016393334,21.4529530482435,124.613728175413)) ;
#82399 = CARTESIAN_POINT('Ctrl Pts',(-19.1043135048021,21.4628769178645,124.578676680394)) ;
#82400 = CARTESIAN_POINT('Ctrl Pts',(-18.9055379557793,21.4729204333817,124.507558457858)) ;
#82401 = CARTESIAN_POINT('Ctrl Pts',(-18.7248962511209,21.48280264627,124.404861344333)) ;
#82402 = CARTESIAN_POINT('Ctrl Pts',(-18.5618819358323,21.4928707234894,124.26991318281)) ;
#82403 = CARTESIAN_POINT('Ctrl Pts',(-18.4277131737804,21.5027092282236,124.112452199386)) ;
#82404 = CARTESIAN_POINT('Ctrl Pts',(-18.3203059133888,21.512771996653,123.930225116019)) ;
#82405 = CARTESIAN_POINT('Ctrl Pts',(-18.2475914284263,21.5226689899357,123.735266065714)) ;
#82406 = CARTESIAN_POINT('Ctrl Pts',(-18.2090196028703,21.5326002175705,123.530079755485)) ;
#82407 = CARTESIAN_POINT('Ctrl Pts',(-18.2068659043944,21.5426423762126,123.318975217952)) ;
#82408 = CARTESIAN_POINT('Ctrl Pts',(-18.2407188945203,21.5525290857437,123.11389200301)) ;
#82409 = CARTESIAN_POINT('Ctrl Pts',(-18.3100668942293,21.5625220581723,122.915594081842)) ;
#82410 = CARTESIAN_POINT('Ctrl Pts',(-18.4123921025152,21.5724682527089,122.73324535457)) ;
#82411 = CARTESIAN_POINT('Ctrl Pts',(-18.5444723633924,21.5824136275604,122.571139711593)) ;
#82412 = CARTESIAN_POINT('Ctrl Pts',(-18.7046180543727,21.5924685469203,122.433199194873)) ;
#82413 = CARTESIAN_POINT('Ctrl Pts',(-18.8819052439076,21.6022900663638,122.32730254651)) ;
#82414 = CARTESIAN_POINT('Ctrl Pts',(-19.0795341491452,21.6123558351307,122.251751647162)) ;
#82415 = CARTESIAN_POINT('Ctrl Pts',(-19.2839834267402,21.6222577567857,122.212371550904)) ;
#82416 = CARTESIAN_POINT('Ctrl Pts',(-19.4950721221416,21.6323008156068,122.208856215622)) ;
#82417 = CARTESIAN_POINT('Ctrl Pts',(-19.7007257257666,21.6422068096495,122.241706225376)) ;
#82418 = CARTESIAN_POINT('Ctrl Pts',(-19.8983768302514,21.6521445827313,122.309400724326)) ;
#82419 = CARTESIAN_POINT('Ctrl Pts',(-20.0830478955549,21.6621849464636,122.411625303527)) ;
#82420 = CARTESIAN_POINT('Ctrl Pts',(-20.2447725573388,21.6720722901871,122.542225508942)) ;
#82421 = CARTESIAN_POINT('Ctrl Pts',(-20.3830581794245,21.6820645207558,122.700338520228)) ;
#82422 = CARTESIAN_POINT('Ctrl Pts',(-20.491278690877,21.6920130485394,122.879326392428)) ;
#82423 = CARTESIAN_POINT('Ctrl Pts',(-20.5669519629379,21.7019498322627,123.074021956924)) ;
#82424 = CARTESIAN_POINT('Ctrl Pts',(-20.608129406161,21.7119328330596,123.279844256603)) ;
#82425 = CARTESIAN_POINT('Ctrl Pts',(-20.6125825117782,21.7219767199004,123.490926869864)) ;
#82426 = CARTESIAN_POINT('Ctrl Pts',(-20.5814885190451,21.7318047434749,123.695222689568)) ;
#82427 = CARTESIAN_POINT('Ctrl Pts',(-20.5138274657763,21.7418819916886,123.895933180593)) ;
#82428 = CARTESIAN_POINT('Ctrl Pts',(-20.4147141986854,21.7517315469939,124.077802382472)) ;
#82429 = CARTESIAN_POINT('Ctrl Pts',(-20.2825949519492,21.7618142551916,124.24349248853)) ;
#82430 = CARTESIAN_POINT('Ctrl Pts',(-20.1280211029921,21.771626848118,124.380174263147)) ;
#82431 = CARTESIAN_POINT('Ctrl Pts',(-19.9477576074203,21.781694040376,124.490980583927)) ;
#82432 = CARTESIAN_POINT('Ctrl Pts',(-19.754162533042,21.7915928698386,124.567467527028)) ;
#82433 = CARTESIAN_POINT('Ctrl Pts',(-19.5471445495349,21.8016468610288,124.60990198465)) ;
#82434 = CARTESIAN_POINT('Ctrl Pts',(-19.3396514700833,21.811518585812,124.615828020924)) ;
#82435 = CARTESIAN_POINT('Ctrl Pts',(-19.1302180432198,21.8215890279422,124.585090725879)) ;
#82436 = CARTESIAN_POINT('Ctrl Pts',(-18.9339576769579,21.8314221063725,124.520098546332)) ;
#82437 = CARTESIAN_POINT('Ctrl Pts',(-18.7480491234729,21.8414525798739,124.420590536606)) ;
#82438 = CARTESIAN_POINT('Ctrl Pts',(-18.5825887690176,21.8514841791725,124.289804551159)) ;
#82439 = CARTESIAN_POINT('Ctrl Pts',(-18.444868573602,21.8613138802107,124.135752800917)) ;
#82440 = CARTESIAN_POINT('Ctrl Pts',(-18.333675525086,21.8713033182672,123.957587871481)) ;
#82441 = CARTESIAN_POINT('Ctrl Pts',(-18.2551799356059,21.8813472214833,123.761568593398)) ;
#82442 = CARTESIAN_POINT('Ctrl Pts',(-18.2124473458304,21.8911687422968,123.559558751751)) ;
#82443 = CARTESIAN_POINT('Ctrl Pts',(-18.2047822894588,21.9012044665439,123.348720043273)) ;
#82444 = CARTESIAN_POINT('Ctrl Pts',(-18.2343460999651,21.9112266204764,123.140091270568)) ;
#82445 = CARTESIAN_POINT('Ctrl Pts',(-18.2983110659554,21.9210888522337,122.942886802025)) ;
#82446 = CARTESIAN_POINT('Ctrl Pts',(-18.3959903010469,21.9310479226916,122.757690814069)) ;
#82447 = CARTESIAN_POINT('Ctrl Pts',(-18.5255720615345,21.9410830950677,122.591216505646)) ;
#82448 = CARTESIAN_POINT('Ctrl Pts',(-18.67949002609,21.950963480226,122.451700734787)) ;
#82449 = CARTESIAN_POINT('Ctrl Pts',(-18.858352008295,21.9610201948199,122.339007613317)) ;
#82450 = CARTESIAN_POINT('Ctrl Pts',(-19.0506455514497,21.970899463392,122.260495049301)) ;
#82451 = CARTESIAN_POINT('Ctrl Pts',(-19.2558150150403,21.9808904208777,122.215517103777)) ;
#82452 = CARTESIAN_POINT('Ctrl Pts',(-19.4667419989655,21.9909310795129,122.207269166707)) ;
#82453 = CARTESIAN_POINT('Ctrl Pts',(-19.6716113086595,22.0007640592209,122.234836706723)) ;
#82454 = CARTESIAN_POINT('Ctrl Pts',(-19.8719733239983,22.0107571924706,122.298006116924)) ;
#82455 = CARTESIAN_POINT('Ctrl Pts',(-20.0588577669836,22.0207892448539,122.395778372292)) ;
#82456 = CARTESIAN_POINT('Ctrl Pts',(-20.2232889178433,22.0306544738052,122.522158713069)) ;
#82457 = CARTESIAN_POINT('Ctrl Pts',(-20.3650985185716,22.0406164150485,122.67628155435)) ;
#82458 = CARTESIAN_POINT('Ctrl Pts',(-20.4785231195851,22.0506511300852,122.854145179665)) ;
#82459 = CARTESIAN_POINT('Ctrl Pts',(-20.5584654837704,22.0605369004293,123.046012221598)) ;
#82460 = CARTESIAN_POINT('Ctrl Pts',(-20.6046775906511,22.070599497818,123.252424729211)) ;
#82461 = CARTESIAN_POINT('Ctrl Pts',(-20.6142383738852,22.0804499096533,123.4593067714)) ;
#82462 = CARTESIAN_POINT('Ctrl Pts',(-20.5877974801273,22.0904770789392,123.668438866555)) ;
#82463 = CARTESIAN_POINT('Ctrl Pts',(-20.5249128796181,22.1005045596534,123.86966118125)) ;
#82464 = CARTESIAN_POINT('Ctrl Pts',(-20.4301887585523,22.1103476122327,124.053631108362)) ;
#82465 = CARTESIAN_POINT('Ctrl Pts',(-20.3034636441155,22.1203415156713,124.22121369691)) ;
#82466 = CARTESIAN_POINT('Ctrl Pts',(-20.1487862388261,22.1303686384477,124.364442189682)) ;
#82467 = CARTESIAN_POINT('Ctrl Pts',(-19.9741429312409,22.1402593433397,124.477302554671)) ;
#82468 = CARTESIAN_POINT('Ctrl Pts',(-19.7807209988621,22.1502513701901,124.55922910085)) ;
#82469 = CARTESIAN_POINT('Ctrl Pts',(-19.5769360895709,22.1601973516786,124.606050630884)) ;
#82470 = CARTESIAN_POINT('Ctrl Pts',(-19.3681010795256,22.1701445243005,124.617200647158)) ;
#82471 = CARTESIAN_POINT('Ctrl Pts',(-19.1584464253659,22.1801924656267,124.591432575702)) ;
#82472 = CARTESIAN_POINT('Ctrl Pts',(-18.9604177789619,22.1900400994344,124.531049438807)) ;
#82473 = CARTESIAN_POINT('Ctrl Pts',(-18.7734573964872,22.2000018141195,124.436702699596)) ;
#82474 = CARTESIAN_POINT('Ctrl Pts',(-18.6047340277275,22.210030446998,124.310256642053)) ;
#82475 = CARTESIAN_POINT('Ctrl Pts',(-18.4621942277681,22.2199407725331,124.158312602361)) ;
#82476 = CARTESIAN_POINT('Ctrl Pts',(-18.3474585546691,22.2298756030049,123.983782776444)) ;
#82477 = CARTESIAN_POINT('Ctrl Pts',(-18.2640502980382,22.2399169353868,123.78985928878)) ;
#82478 = CARTESIAN_POINT('Ctrl Pts',(-18.2162240860105,22.2498098088257,123.58745557848)) ;
#82479 = CARTESIAN_POINT('Ctrl Pts',(-18.2036438426885,22.2597789746436,123.378240631757)) ;
#82480 = CARTESIAN_POINT('Ctrl Pts',(-18.2280682146378,22.2698077083601,123.168844828151)) ;
#82481 = CARTESIAN_POINT('Ctrl Pts',(-18.3069945528939,22.2830002271312,122.902886750421)) ;
#82482 = CARTESIAN_POINT('Ctrl Pts',(-18.4552999005184,22.2963600951739,122.66069779592)) ;
#82483 = CARTESIAN_POINT('Ctrl Pts',(-18.6570215898245,22.3095854323228,122.469325661276)) ;
#82484 = CARTESIAN_POINT('Ctrl Pts',(-18.8316797652282,22.3195666581634,122.353021542224)) ;
#82485 = CARTESIAN_POINT('Ctrl Pts',(-19.025082549416,22.3296022251463,122.26873651452)) ;
#82486 = CARTESIAN_POINT('Ctrl Pts',(-19.22658820499,22.3394653031084,122.219744511049)) ;
#82487 = CARTESIAN_POINT('Ctrl Pts',(-19.437838742601,22.3495356019095,122.206163829392)) ;
#82488 = CARTESIAN_POINT('Ctrl Pts',(-19.6435055191939,22.3593779004773,122.228957325514)) ;
#82489 = CARTESIAN_POINT('Ctrl Pts',(-19.8446819369498,22.3693385986471,122.287067922869)) ;
#82490 = CARTESIAN_POINT('Ctrl Pts',(-20.0339845517462,22.3793766328265,122.380317508446)) ;
#82491 = CARTESIAN_POINT('Ctrl Pts',(-20.2016926105113,22.389250369673,122.502684369457)) ;
#82492 = CARTESIAN_POINT('Ctrl Pts',(-20.3484344011402,22.3993221535983,122.655289347127)) ;
#82493 = CARTESIAN_POINT('Ctrl Pts',(-20.4637741168611,22.4091542747995,122.826843880767)) ;
#82494 = CARTESIAN_POINT('Ctrl Pts',(-20.5497920261545,22.4191872988249,123.019422041315)) ;
#82495 = CARTESIAN_POINT('Ctrl Pts',(-20.6004603771645,22.4292031790216,123.223814284378)) ;
#82496 = CARTESIAN_POINT('Ctrl Pts',(-20.6150640004931,22.4390866981158,123.431083471758)) ;
#82497 = CARTESIAN_POINT('Ctrl Pts',(-20.5934940797132,22.4490771104794,123.639987608933)) ;
#82498 = CARTESIAN_POINT('Ctrl Pts',(-20.517218240559,22.4623402736829,123.908212352652)) ;
#82499 = CARTESIAN_POINT('Ctrl Pts',(-20.3727555418363,22.4756178439341,124.150777416786)) ;
#82500 = CARTESIAN_POINT('Ctrl Pts',(-20.1718123791193,22.4889481464407,124.346093847646)) ;
#82501 = CARTESIAN_POINT('Ctrl Pts',(-19.9998410836339,22.4988468282571,124.463290434871)) ;
#82502 = CARTESIAN_POINT('Ctrl Pts',(-19.8085085382788,22.5088363433046,124.549850694843)) ;
#82503 = CARTESIAN_POINT('Ctrl Pts',(-19.6058755849689,22.5187843950796,124.601655303795)) ;
#82504 = CARTESIAN_POINT('Ctrl Pts',(-19.3975125848243,22.5287257983581,124.61774036324)) ;
#82505 = CARTESIAN_POINT('Ctrl Pts',(-19.1194367253564,22.5420124631391,124.590882659697)) ;
#82506 = CARTESIAN_POINT('Ctrl Pts',(-18.788660398813,22.5586228847939,124.46721791432)) ;
#82507 = CARTESIAN_POINT('Ctrl Pts',(-18.4662722077278,22.5785341470447,124.192767698316)) ;
#82508 = CARTESIAN_POINT('Ctrl Pts',(-18.2564052347418,22.5984782762096,123.824248386877)) ;
#82509 = CARTESIAN_POINT('Ctrl Pts',(-18.1850298158601,22.6184014388147,123.406724093783)) ;
#82510 = CARTESIAN_POINT('Ctrl Pts',(-18.2596165922756,22.6382915612213,122.990368848326)) ;
#82511 = CARTESIAN_POINT('Ctrl Pts',(-18.4732461365668,22.6582965148214,122.622623863024)) ;
#82512 = CARTESIAN_POINT('Ctrl Pts',(-18.7967224378562,22.678134771837,122.351774793471)) ;
#82513 = CARTESIAN_POINT('Ctrl Pts',(-19.1960527549602,22.6981290726235,122.206072274783)) ;
#82514 = CARTESIAN_POINT('Ctrl Pts',(-19.6188774272319,22.718014314668,122.205770397816)) ;
#82515 = CARTESIAN_POINT('Ctrl Pts',(-20.0166123098937,22.7378892611439,122.348576418114)) ;
#82516 = CARTESIAN_POINT('Ctrl Pts',(-20.3441438839441,22.757922331085,122.620968086443)) ;
#82517 = CARTESIAN_POINT('Ctrl Pts',(-20.5570158705556,22.7778108379854,122.986324841109)) ;
#82518 = CARTESIAN_POINT('Ctrl Pts',(-20.6337660265927,22.7976656977667,123.401523678932)) ;
#82519 = CARTESIAN_POINT('Ctrl Pts',(-20.5628771685772,22.8177165315544,123.821821293036)) ;
#82520 = CARTESIAN_POINT('Ctrl Pts',(-20.3561026233615,22.8374824734436,124.18784828046)) ;
#82521 = CARTESIAN_POINT('Ctrl Pts',(-20.0335851048464,22.857495204903,124.465242814785)) ;
#82522 = CARTESIAN_POINT('Ctrl Pts',(-19.6377262813745,22.8773880398465,124.61457533021)) ;
#82523 = CARTESIAN_POINT('Ctrl Pts',(-19.2145951458485,22.8972950631861,124.620562118106)) ;
#82524 = CARTESIAN_POINT('Ctrl Pts',(-18.8143052784339,22.9172103280868,124.48212442822)) ;
#82525 = CARTESIAN_POINT('Ctrl Pts',(-18.4838083763501,22.9372420202465,124.213504451096)) ;
#82526 = CARTESIAN_POINT('Ctrl Pts',(-18.2668145194159,22.9570850668195,123.851613055632)) ;
#82527 = CARTESIAN_POINT('Ctrl Pts',(-18.1851080185163,22.9770016147193,123.436153668619)) ;
#82528 = CARTESIAN_POINT('Ctrl Pts',(-18.2502202177031,22.9969338577106,123.017334018235)) ;
#82529 = CARTESIAN_POINT('Ctrl Pts',(-18.4538258820045,23.0168376925199,122.646347008578)) ;
#82530 = CARTESIAN_POINT('Ctrl Pts',(-18.7714168386275,23.0367380927074,122.366744945612)) ;
#82531 = CARTESIAN_POINT('Ctrl Pts',(-19.1662858522202,23.0566877690867,122.211749727135)) ;
#82532 = CARTESIAN_POINT('Ctrl Pts',(-19.5899723211097,23.0766202933071,122.200906811496)) ;
#82533 = CARTESIAN_POINT('Ctrl Pts',(-19.9918128358523,23.0965403022933,122.334876915876)) ;
#82534 = CARTESIAN_POINT('Ctrl Pts',(-20.3243318262341,23.1164972084694,122.598424755681)) ;
#82535 = CARTESIAN_POINT('Ctrl Pts',(-20.5465556585454,23.1363830479709,122.95823999004)) ;
#82536 = CARTESIAN_POINT('Ctrl Pts',(-20.6329370108439,23.1563542201068,123.373906265248)) ;
#82537 = CARTESIAN_POINT('Ctrl Pts',(-20.573322927364,23.1761684170912,123.791036823515)) ;
#82538 = CARTESIAN_POINT('Ctrl Pts',(-20.3738396316099,23.1961496030594,124.166064107875)) ;
#82539 = CARTESIAN_POINT('Ctrl Pts',(-20.1119254262802,23.2127251084487,124.401936038304)) ;
#82540 = CARTESIAN_POINT('Ctrl Pts',(-19.8627907757275,23.2260345563123,124.529374358132)) ;
#82541 = CARTESIAN_POINT('Ctrl Pts',(-19.5941634496156,23.2394022540889,124.611788229656)) ;
#82542 = CARTESIAN_POINT('Ctrl Pts',(-19.2437165005351,23.2558928257548,124.624712070297)) ;
#82543 = CARTESIAN_POINT('Ctrl Pts',(-18.84025681319,23.2758130980876,124.49601281634)) ;
#82544 = CARTESIAN_POINT('Ctrl Pts',(-18.5605856338908,23.2924301338086,124.280092561327)) ;
#82545 = CARTESIAN_POINT('Ctrl Pts',(-18.3909771122857,23.3057209840897,124.057986573605)) ;
#82546 = CARTESIAN_POINT('Ctrl Pts',(-18.2945642892611,23.3156900292442,123.871929208905)) ;
#82547 = CARTESIAN_POINT('Ctrl Pts',(-18.2319237623496,23.3255934198777,123.673347940635)) ;
#82548 = CARTESIAN_POINT('Ctrl Pts',(-18.2044109627458,23.3356512059904,123.463725251977)) ;
#82549 = CARTESIAN_POINT('Ctrl Pts',(-18.2133455814225,23.3455032426402,123.256767963458)) ;
#82550 = CARTESIAN_POINT('Ctrl Pts',(-18.2735481031819,23.3588683667834,122.982370270208)) ;
#82551 = CARTESIAN_POINT('Ctrl Pts',(-18.4029731145721,23.3720944297464,122.732648890195)) ;
#82552 = CARTESIAN_POINT('Ctrl Pts',(-18.5911585972298,23.3853980780287,122.525747425895)) ;
#82553 = CARTESIAN_POINT('Ctrl Pts',(-18.7572840249593,23.3953896091917,122.397160356993)) ;
#82554 = CARTESIAN_POINT('Ctrl Pts',(-18.9442034218826,23.405429056991,122.299171365096)) ;
#82555 = CARTESIAN_POINT('Ctrl Pts',(-19.1413113103794,23.4152728325048,122.236069997522)) ;
#82556 = CARTESIAN_POINT('Ctrl Pts',(-19.3492334705242,23.4252584738925,122.207338845479)) ;
#82557 = CARTESIAN_POINT('Ctrl Pts',(-19.5580294441203,23.4351952582543,122.214996284707)) ;
#82558 = CARTESIAN_POINT('Ctrl Pts',(-19.7645715963343,23.4452450927216,122.259384713795)) ;
#82559 = CARTESIAN_POINT('Ctrl Pts',(-19.9564788390194,23.4550955422248,122.33725097854)) ;
#82560 = CARTESIAN_POINT('Ctrl Pts',(-20.1343708523743,23.4650675562069,122.448127375331)) ;
#82561 = CARTESIAN_POINT('Ctrl Pts',(-20.290697050754,23.475062714054,122.588593746515)) ;
#82562 = CARTESIAN_POINT('Ctrl Pts',(-20.4205292525816,23.4850966404177,122.75482783176)) ;
#82563 = CARTESIAN_POINT('Ctrl Pts',(-20.5180699407723,23.4949523488501,122.937651926998)) ;
#82564 = CARTESIAN_POINT('Ctrl Pts',(-20.5835848064832,23.5049504981887,123.137338609662)) ;
#82565 = CARTESIAN_POINT('Ctrl Pts',(-20.6133315592433,23.5148499013623,123.343349263886)) ;
#82566 = CARTESIAN_POINT('Ctrl Pts',(-20.6068042976346,23.5249010982508,123.554533941708)) ;
#82567 = CARTESIAN_POINT('Ctrl Pts',(-20.5644542845727,23.5347834220636,123.757945272623)) ;
#82568 = CARTESIAN_POINT('Ctrl Pts',(-20.4869988626981,23.5447783177202,123.953265935445)) ;
#82569 = CARTESIAN_POINT('Ctrl Pts',(-20.3762451240115,23.5547994171028,124.132491954)) ;
#82570 = CARTESIAN_POINT('Ctrl Pts',(-20.2377780768666,23.5647066849648,124.288078659894)) ;
#82571 = CARTESIAN_POINT('Ctrl Pts',(-20.0741559214403,23.5746450287901,124.417986713011)) ;
#82572 = CARTESIAN_POINT('Ctrl Pts',(-19.8892906509235,23.5846484480906,124.518297171664)) ;
#82573 = CARTESIAN_POINT('Ctrl Pts',(-19.6891176969412,23.5946829987977,124.584849929833)) ;
#82574 = CARTESIAN_POINT('Ctrl Pts',(-19.4844008635135,23.6045279484033,124.615406104231)) ;
#82575 = CARTESIAN_POINT('Ctrl Pts',(-19.2745631998316,23.6145137905162,124.61026978037)) ;
#82576 = CARTESIAN_POINT('Ctrl Pts',(-19.0697563432002,23.6244485978853,124.56912101187)) ;
#82577 = CARTESIAN_POINT('Ctrl Pts',(-18.8729354133231,23.6345061395986,124.491945311398)) ;
#82578 = CARTESIAN_POINT('Ctrl Pts',(-18.6965271286141,23.6443277371107,124.384596044604)) ;
#82579 = CARTESIAN_POINT('Ctrl Pts',(-18.5375052095962,23.6543839965912,124.245310916362)) ;
#82580 = CARTESIAN_POINT('Ctrl Pts',(-18.4068828190707,23.6643239328916,124.082183811168)) ;
#82581 = CARTESIAN_POINT('Ctrl Pts',(-18.3063569600864,23.674231053636,123.89977336365)) ;
#82582 = CARTESIAN_POINT('Ctrl Pts',(-18.2381821022871,23.6842739595613,123.699954793719)) ;
#82583 = CARTESIAN_POINT('Ctrl Pts',(-18.2061315885862,23.6941817406604,123.494134504047)) ;
#82584 = CARTESIAN_POINT('Ctrl Pts',(-18.2099782470609,23.7041921096629,123.283713238738)) ;
#82585 = CARTESIAN_POINT('Ctrl Pts',(-18.2508047879774,23.7142229482317,123.076824775959)) ;
#82586 = CARTESIAN_POINT('Ctrl Pts',(-18.3252380545856,23.7240757878714,122.883518206758)) ;
#82587 = CARTESIAN_POINT('Ctrl Pts',(-18.4332307035632,23.7340637890363,122.703457541296)) ;
#82588 = CARTESIAN_POINT('Ctrl Pts',(-18.5700431604149,23.7439926080155,122.545803259153)) ;
#82589 = CARTESIAN_POINT('Ctrl Pts',(-18.7328941586295,23.7539803107378,122.413240963306)) ;
#82590 = CARTESIAN_POINT('Ctrl Pts',(-18.9173305893805,23.7640163105405,122.310793634948)) ;
#82591 = CARTESIAN_POINT('Ctrl Pts',(-19.1130661829979,23.7738711803419,122.242836707875)) ;
#82592 = CARTESIAN_POINT('Ctrl Pts',(-19.3205318093657,23.7838706107654,122.209140766422)) ;
#82593 = CARTESIAN_POINT('Ctrl Pts',(-19.528576529855,23.7937657282307,122.211727967725)) ;
#82594 = CARTESIAN_POINT('Ctrl Pts',(-19.7363643552713,23.8038262217477,122.251054379042)) ;
#82595 = CARTESIAN_POINT('Ctrl Pts',(-19.9300969389221,23.8136757019489,122.324201642346)) ;
#82596 = CARTESIAN_POINT('Ctrl Pts',(-20.1116481535929,23.8237021522127,122.431297541146)) ;
#82597 = CARTESIAN_POINT('Ctrl Pts',(-20.2715506779212,23.8337334426908,122.568801980816)) ;
#82598 = CARTESIAN_POINT('Ctrl Pts',(-20.4029659176429,23.8435748303426,122.728604738249)) ;
#82599 = CARTESIAN_POINT('Ctrl Pts',(-20.5066563597952,23.8535782312338,122.911544076918)) ;
#82600 = CARTESIAN_POINT('Ctrl Pts',(-20.5768109022022,23.863562614025,123.109415512319)) ;
#82601 = CARTESIAN_POINT('Ctrl Pts',(-20.6115256239944,23.8736017040384,123.31757326113)) ;
#82602 = CARTESIAN_POINT('Ctrl Pts',(-20.6098969878997,23.8834475129475,123.524571599926)) ;
#82603 = CARTESIAN_POINT('Ctrl Pts',(-20.5722509348656,23.8934319357665,123.731041364494)) ;
#82604 = CARTESIAN_POINT('Ctrl Pts',(-20.4997173978823,23.9033715610077,123.927042140903)) ;
#82605 = CARTESIAN_POINT('Ctrl Pts',(-20.3931719092889,23.9134112505264,124.109223158577)) ;
#82606 = CARTESIAN_POINT('Ctrl Pts',(-20.2587341754022,23.923299438945,124.267797397072)) ;
#82607 = CARTESIAN_POINT('Ctrl Pts',(-20.0974322378108,23.933288964947,124.402272331516)) ;
#82608 = CARTESIAN_POINT('Ctrl Pts',(-19.915715878204,23.9432474663022,124.506233907612)) ;
#82609 = CARTESIAN_POINT('Ctrl Pts',(-19.7200317103862,23.9531470603059,124.577135525943)) ;
#82610 = CARTESIAN_POINT('Ctrl Pts',(-19.5119585755635,23.9631949484272,124.613440422247)) ;
#82611 = CARTESIAN_POINT('Ctrl Pts',(-19.3038930888951,23.9730903736727,124.613234238601)) ;
#82612 = CARTESIAN_POINT('Ctrl Pts',(-19.0956394147176,23.9831517643733,124.576334613564)) ;
#82613 = CARTESIAN_POINT('Ctrl Pts',(-18.9011714992526,23.9929973480599,124.505414746921)) ;
#82614 = CARTESIAN_POINT('Ctrl Pts',(-18.7195046967717,24.0029603213691,124.401196093712)) ;
#82615 = CARTESIAN_POINT('Ctrl Pts',(-18.5578392061729,24.0129859881949,124.265939513218)) ;
#82616 = CARTESIAN_POINT('Ctrl Pts',(-18.4235465432553,24.0229004660612,124.106543727124)) ;
#82617 = CARTESIAN_POINT('Ctrl Pts',(-18.3178150664723,24.0328889807362,123.925094508878)) ;
#82618 = CARTESIAN_POINT('Ctrl Pts',(-18.2452273820998,24.0429330916517,123.72682449614)) ;
#82619 = CARTESIAN_POINT('Ctrl Pts',(-18.2084622185153,24.0527612292462,123.523473719363)) ;
#82620 = CARTESIAN_POINT('Ctrl Pts',(-18.2074439800112,24.0628377973052,123.311677825631)) ;
#82621 = CARTESIAN_POINT('Ctrl Pts',(-18.2423298172474,24.0726899592093,123.107467672833)) ;
#82622 = CARTESIAN_POINT('Ctrl Pts',(-18.3135158921644,24.0827629211662,122.908064117061)) ;
#82623 = CARTESIAN_POINT('Ctrl Pts',(-18.4159003186132,24.0926054831691,122.728227437951)) ;
#82624 = CARTESIAN_POINT('Ctrl Pts',(-18.5492445179135,24.1025859196629,122.566240438821)) ;
#82625 = CARTESIAN_POINT('Ctrl Pts',(-18.7095634324068,24.1126042249873,122.429654343682)) ;
#82626 = CARTESIAN_POINT('Ctrl Pts',(-18.8885295576989,24.1224881889067,122.324026226446)) ;
#82627 = CARTESIAN_POINT('Ctrl Pts',(-19.0866747117363,24.1325540656453,122.249802038306)) ;
#82628 = CARTESIAN_POINT('Ctrl Pts',(-19.2900277987292,24.1423931665062,122.211839217238)) ;
#82629 = CARTESIAN_POINT('Ctrl Pts',(-19.5009280452446,24.1524262493719,122.209188900034)) ;
#82630 = CARTESIAN_POINT('Ctrl Pts',(-19.7087891088746,24.1624479346474,122.243680922594)) ;
#82631 = CARTESIAN_POINT('Ctrl Pts',(-19.9045118842529,24.1723146297458,122.312331343585)) ;
#82632 = CARTESIAN_POINT('Ctrl Pts',(-20.0873424230859,24.1822745194804,122.414410683436)) ;
#82633 = CARTESIAN_POINT('Ctrl Pts',(-20.2506734219996,24.1923095073059,122.547919076296)) ;
#82634 = CARTESIAN_POINT('Ctrl Pts',(-20.3865972542028,24.2021962113802,122.70520302407)) ;
#82635 = CARTESIAN_POINT('Ctrl Pts',(-20.4949915148063,24.2122613556131,122.886893116054)) ;
#82636 = CARTESIAN_POINT('Ctrl Pts',(-20.5687253538472,24.2221006463416,123.080191844963)) ;
#82637 = CARTESIAN_POINT('Ctrl Pts',(-20.608936234929,24.2321632037801,123.28785666925)) ;
#82638 = CARTESIAN_POINT('Ctrl Pts',(-20.6121978969833,24.2420602550322,123.495909815713)) ;
#82639 = CARTESIAN_POINT('Ctrl Pts',(-20.5798621410768,24.2519914617804,123.702170633504)) ;
#82640 = CARTESIAN_POINT('Ctrl Pts',(-20.5112278003848,24.2620336459993,123.901818282665)) ;
#82641 = CARTESIAN_POINT('Ctrl Pts',(-20.4106814466933,24.2719202741102,124.083739096484)) ;
#82642 = CARTESIAN_POINT('Ctrl Pts',(-20.2789510205555,24.2819135466426,124.247385519698)) ;
#82643 = CARTESIAN_POINT('Ctrl Pts',(-20.1215139965701,24.291858622184,124.384961385471)) ;
#82644 = CARTESIAN_POINT('Ctrl Pts',(-19.9427040338153,24.3018081729123,124.493512747479)) ;
#82645 = CARTESIAN_POINT('Ctrl Pts',(-19.7459483455522,24.3118475077603,124.569858328381)) ;
#82646 = CARTESIAN_POINT('Ctrl Pts',(-19.5420958305893,24.3217336467042,124.610447517326)) ;
#82647 = CARTESIAN_POINT('Ctrl Pts',(-19.3319860419115,24.3317317596779,124.615343457489)) ;
#82648 = CARTESIAN_POINT('Ctrl Pts',(-19.1257788093217,24.3416515220303,124.584048457345)) ;
#82649 = CARTESIAN_POINT('Ctrl Pts',(-18.9257658349345,24.351690917643,124.516694244747)) ;
#82650 = CARTESIAN_POINT('Ctrl Pts',(-18.7429093393127,24.3616001034313,124.416883437135)) ;
#82651 = CARTESIAN_POINT('Ctrl Pts',(-18.5793682381325,24.3715352875888,124.286955899813)) ;
#82652 = CARTESIAN_POINT('Ctrl Pts',(-18.4395549919539,24.3815763449747,124.128807119473)) ;
#82653 = CARTESIAN_POINT('Ctrl Pts',(-18.3308792199516,24.391463503008,123.951607976595)) ;
#82654 = CARTESIAN_POINT('Ctrl Pts',(-18.2534953332544,24.4014557826839,123.756326943082)) ;
#82655 = CARTESIAN_POINT('Ctrl Pts',(-18.2114309361531,24.4114042997289,123.551439509569)) ;
#82656 = CARTESIAN_POINT('Ctrl Pts',(-18.2052935477801,24.4213410772993,123.342645056263)) ;
#82657 = CARTESIAN_POINT('Ctrl Pts',(-18.2353874902954,24.4313241134463,123.134912265281)) ;
#82658 = CARTESIAN_POINT('Ctrl Pts',(-18.3018447177131,24.44136786504,122.934516737873)) ;
#82659 = CARTESIAN_POINT('Ctrl Pts',(-18.3995391049124,24.4511963942526,122.75241027329)) ;
#82660 = CARTESIAN_POINT('Ctrl Pts',(-18.5304447148588,24.4612717551613,122.585941029605)) ;
#82661 = CARTESIAN_POINT('Ctrl Pts',(-18.6848541226501,24.4711283540485,122.447684982794)) ;
#82662 = CARTESIAN_POINT('Ctrl Pts',(-18.864422486662,24.4811913480664,122.335908343508)) ;
#82663 = CARTESIAN_POINT('Ctrl Pts',(-19.0571387654209,24.4910692823558,122.258444824587)) ;
#82664 = CARTESIAN_POINT('Ctrl Pts',(-19.2627623039169,24.5010699299139,122.214785947123)) ;
#82665 = CARTESIAN_POINT('Ctrl Pts',(-19.4711725797811,24.5109877763519,122.207393835235)) ;
#82666 = CARTESIAN_POINT('Ctrl Pts',(-19.6803970457402,24.5210388933576,122.236738188576)) ;
#82667 = CARTESIAN_POINT('Ctrl Pts',(-19.8778824426931,24.5309096286682,122.30059393333)) ;
#82668 = CARTESIAN_POINT('Ctrl Pts',(-20.0649514483934,24.5409803359112,122.399666053777)) ;
#82669 = CARTESIAN_POINT('Ctrl Pts',(-20.2281337107902,24.5508133433631,122.5266026047)) ;
#82670 = CARTESIAN_POINT('Ctrl Pts',(-20.370009757199,24.5608438356654,122.682600129859)) ;
#82671 = CARTESIAN_POINT('Ctrl Pts',(-20.4821469112332,24.5708754307388,122.861226309303)) ;
#82672 = CARTESIAN_POINT('Ctrl Pts',(-20.5603565453377,24.580705129877,123.05249064484)) ;
#82673 = CARTESIAN_POINT('Ctrl Pts',(-20.6054976015341,24.5906945797586,123.257597896419)) ;
#82674 = CARTESIAN_POINT('Ctrl Pts',(-20.6138517558197,24.6007384375743,123.468583732253)) ;
#82675 = CARTESIAN_POINT('Ctrl Pts',(-20.5864978778444,24.6105601281645,123.67324702507)) ;
#82676 = CARTESIAN_POINT('Ctrl Pts',(-20.5231546982953,24.6205952187049,123.874478649542)) ;
#82677 = CARTESIAN_POINT('Ctrl Pts',(-20.4254304035954,24.6306197376876,124.061214681155)) ;
#82678 = CARTESIAN_POINT('Ctrl Pts',(-20.2991788046576,24.6404795830978,124.22559646436)) ;
#82679 = CARTESIAN_POINT('Ctrl Pts',(-20.145129895565,24.6504393594134,124.367416560908)) ;
#82680 = CARTESIAN_POINT('Ctrl Pts',(-19.9674334411512,24.6604675567281,124.480860594718)) ;
#82681 = CARTESIAN_POINT('Ctrl Pts',(-19.7751577797198,24.6703750990184,124.560990106468)) ;
#82682 = CARTESIAN_POINT('Ctrl Pts',(-19.5693703328522,24.6804077495822,124.607155032494)) ;
#82683 = CARTESIAN_POINT('Ctrl Pts',(-19.3617967555664,24.6902917060089,124.61680553169)) ;
#82684 = CARTESIAN_POINT('Ctrl Pts',(-19.1534319522652,24.7002814073707,124.590503034334)) ;
#82685 = CARTESIAN_POINT('Ctrl Pts',(-18.9519051623861,24.7103224026468,124.527673623599)) ;
#82686 = CARTESIAN_POINT('Ctrl Pts',(-18.7680835662665,24.7201552919151,124.43311943108)) ;
#82687 = CARTESIAN_POINT('Ctrl Pts',(-18.6004240956916,24.7301484502826,124.306526655359)) ;
#82688 = CARTESIAN_POINT('Ctrl Pts',(-18.4570479654996,24.7401804926347,124.15183839261)) ;
#82689 = CARTESIAN_POINT('Ctrl Pts',(-18.3444058754051,24.7500457365931,123.977707914406)) ;
#82690 = CARTESIAN_POINT('Ctrl Pts',(-18.2623662492347,24.7600076278391,123.785008651907)) ;
#82691 = CARTESIAN_POINT('Ctrl Pts',(-18.2150227218341,24.7700425278576,123.57943498646)) ;
#82692 = CARTESIAN_POINT('Ctrl Pts',(-18.2039108265899,24.7799276082722,123.371890119944)) ;
#82693 = CARTESIAN_POINT('Ctrl Pts',(-18.2294765748112,24.789992780397,123.161866623619)) ;
#82694 = CARTESIAN_POINT('Ctrl Pts',(-18.2896850160126,24.7998400151205,122.963774156201)) ;
#82695 = CARTESIAN_POINT('Ctrl Pts',(-18.3846631838683,24.8098708264382,122.775510299179)) ;
#82696 = CARTESIAN_POINT('Ctrl Pts',(-18.5109890530779,24.8198804423517,122.607182357342)) ;
#82697 = CARTESIAN_POINT('Ctrl Pts',(-18.6629344097243,24.8297912217554,122.46464599339)) ;
#82698 = CARTESIAN_POINT('Ctrl Pts',(-18.8373840507773,24.8397204875445,122.349990527342)) ;
#82699 = CARTESIAN_POINT('Ctrl Pts',(-19.0313351917403,24.8497631808571,122.266594739761)) ;
#82700 = CARTESIAN_POINT('Ctrl Pts',(-19.2336139838106,24.8596497135518,122.218758538381)) ;
#82701 = CARTESIAN_POINT('Ctrl Pts',(-19.443319684323,24.8696428586551,122.206287816751)) ;
#82702 = CARTESIAN_POINT('Ctrl Pts',(-19.6510167260348,24.8795885393292,122.230384480415)) ;
#82703 = CARTESIAN_POINT('Ctrl Pts',(-19.851538316644,24.8895357969559,122.289780441045)) ;
#82704 = CARTESIAN_POINT('Ctrl Pts',(-20.0404730206876,24.8995836990774,122.384240048737)) ;
#82705 = CARTESIAN_POINT('Ctrl Pts',(-20.2068658067481,24.9094314046991,122.507427675113)) ;
#82706 = CARTESIAN_POINT('Ctrl Pts',(-20.3514609472444,24.9193928713332,122.658908390859)) ;
#82707 = CARTESIAN_POINT('Ctrl Pts',(-20.4681229399216,24.9294224246014,122.834556316667)) ;
#82708 = CARTESIAN_POINT('Ctrl Pts',(-20.5515899926402,24.9393293166288,123.025376823584)) ;
#82709 = CARTESIAN_POINT('Ctrl Pts',(-20.6012474613026,24.9492769607418,123.2285093331)) ;
#82710 = CARTESIAN_POINT('Ctrl Pts',(-20.6150856722324,24.9592770037707,123.438313378773)) ;
#82711 = CARTESIAN_POINT('Ctrl Pts',(-20.5918280692934,24.9693157697647,123.648058183156)) ;
#82712 = CARTESIAN_POINT('Ctrl Pts',(-20.5341801448491,24.9791408317869,123.846419031211)) ;
#82713 = CARTESIAN_POINT('Ctrl Pts',(-20.4411614002517,24.9891953791133,124.036215807253)) ;
#82714 = CARTESIAN_POINT('Ctrl Pts',(-20.317675914931,24.9991386225625,124.204890724799)) ;
#82715 = CARTESIAN_POINT('Ctrl Pts',(-20.1678533868408,25.0090407941704,124.349428618332)) ;
#82716 = CARTESIAN_POINT('Ctrl Pts',(-19.992519998126,25.0190936297806,124.46741219479)) ;
#82717 = CARTESIAN_POINT('Ctrl Pts',(-19.8028366542702,25.0289666874661,124.551709330501)) ;
#82718 = CARTESIAN_POINT('Ctrl Pts',(-19.5990412584524,25.0389619489918,124.602912199608)) ;
#82719 = CARTESIAN_POINT('Ctrl Pts',(-19.3887859636416,25.0489873184123,124.617620931804)) ;
#82720 = CARTESIAN_POINT('Ctrl Pts',(-19.1819727421528,25.0588771509389,124.596169235394)) ;
#82721 = CARTESIAN_POINT('Ctrl Pts',(-18.91306138402,25.0721751217483,124.519808852697)) ;
#82722 = CARTESIAN_POINT('Ctrl Pts',(-18.6717643622118,25.0853735168574,124.37640217607)) ;
#82723 = CARTESIAN_POINT('Ctrl Pts',(-18.4752738616247,25.0987689591369,124.174746619851)) ;
#82724 = CARTESIAN_POINT('Ctrl Pts',(-18.3582246189825,25.1086447973759,124.003215132547)) ;
#82725 = CARTESIAN_POINT('Ctrl Pts',(-18.2710748662201,25.1187061999736,123.810519405556)) ;
#82726 = CARTESIAN_POINT('Ctrl Pts',(-18.2196533575529,25.1285712569087,123.609567294506)) ;
#82727 = CARTESIAN_POINT('Ctrl Pts',(-18.203298763142,25.1385833528575,123.399749571812)) ;
#82728 = CARTESIAN_POINT('Ctrl Pts',(-18.2303147257671,25.151860662003,123.121871212669)) ;
#82729 = CARTESIAN_POINT('Ctrl Pts',(-18.353792179079,25.1684596875103,122.791296798162)) ;
#82730 = CARTESIAN_POINT('Ctrl Pts',(-18.5827030592161,25.1850587355433,122.522606055033)) ;
#82731 = CARTESIAN_POINT('Ctrl Pts',(-18.8116926955832,25.1983021475742,122.364286012288)) ;
#82732 = CARTESIAN_POINT('Ctrl Pts',(-19.0034239801853,25.2083395752627,122.276149971483)) ;
#82733 = CARTESIAN_POINT('Ctrl Pts',(-19.2048452374266,25.2182438772183,122.223388078408)) ;
#82734 = CARTESIAN_POINT('Ctrl Pts',(-19.4827947851968,25.2315107171934,122.199905674607)) ;
#82735 = CARTESIAN_POINT('Ctrl Pts',(-19.8307375228141,25.2481369152834,122.262279578136)) ;
#82736 = CARTESIAN_POINT('Ctrl Pts',(-20.1971584545413,25.2680560306668,122.474694751445)) ;
#82737 = CARTESIAN_POINT('Ctrl Pts',(-20.4241107571781,25.284662453801,122.745253295824)) ;
#82738 = CARTESIAN_POINT('Ctrl Pts',(-20.5421825344432,25.2979586742967,122.998571370006)) ;
#82739 = CARTESIAN_POINT('Ctrl Pts',(-20.6149656243915,25.3112275066382,123.267944727549)) ;
#82740 = CARTESIAN_POINT('Ctrl Pts',(-20.6152703491861,25.3279187546713,123.62274741247)) ;
#82741 = CARTESIAN_POINT('Ctrl Pts',(-20.4723050652647,25.3477284863441,124.019012656486)) ;
#82742 = CARTESIAN_POINT('Ctrl Pts',(-20.2011038052829,25.3677060936726,124.345923721756)) ;
#82743 = CARTESIAN_POINT('Ctrl Pts',(-19.8352019120776,25.3876324027305,124.559424851809)) ;
#82744 = CARTESIAN_POINT('Ctrl Pts',(-19.4208025912353,25.4074492628952,124.636316300838)) ;
#82745 = CARTESIAN_POINT('Ctrl Pts',(-18.9994694110562,25.4275490784892,124.56558046184)) ;
#82746 = CARTESIAN_POINT('Ctrl Pts',(-18.6335309608518,25.4473060423717,124.358919220961)) ;
#82747 = CARTESIAN_POINT('Ctrl Pts',(-18.3557823809738,25.4673429684412,124.036055619481)) ;
#82748 = CARTESIAN_POINT('Ctrl Pts',(-18.2066757307838,25.4872125508227,123.640645139258)) ;
#82749 = CARTESIAN_POINT('Ctrl Pts',(-18.2003787294005,25.5071171225759,123.217548778513)) ;
#82750 = CARTESIAN_POINT('Ctrl Pts',(-18.3392640178439,25.5270697247744,122.816604069234)) ;
#82751 = CARTESIAN_POINT('Ctrl Pts',(-18.6060642919708,25.5469792157446,122.488044084388)) ;
#82752 = CARTESIAN_POINT('Ctrl Pts',(-18.9674597166613,25.5668305844441,122.269771258974)) ;
#82753 = CARTESIAN_POINT('Ctrl Pts',(-19.3863524336457,25.5869107805801,122.187636260904)) ;
#82754 = CARTESIAN_POINT('Ctrl Pts',(-19.8024618699774,25.6067117241555,122.252489134257)) ;
#82755 = CARTESIAN_POINT('Ctrl Pts',(-20.1751760188317,25.626695700665,122.456396660156)) ;
#82756 = CARTESIAN_POINT('Ctrl Pts',(-20.4545282376597,25.6466116636406,122.774650868096)) ;
#82757 = CARTESIAN_POINT('Ctrl Pts',(-20.6092750951516,25.6664820984625,123.167879992123)) ;
#82758 = CARTESIAN_POINT('Ctrl Pts',(-20.619928125435,25.6865323836956,123.5939462739)) ;
#82759 = CARTESIAN_POINT('Ctrl Pts',(-20.486892040256,25.7063063524549,123.992971139945)) ;
#82760 = CARTESIAN_POINT('Ctrl Pts',(-20.2223888179771,25.7263628105744,124.3272695752)) ;
#82761 = CARTESIAN_POINT('Ctrl Pts',(-19.8640907327752,25.7461576935654,124.548347804245)) ;
#82762 = CARTESIAN_POINT('Ctrl Pts',(-19.4487334488014,25.7661243488678,124.635759281327)) ;
#82763 = CARTESIAN_POINT('Ctrl Pts',(-19.0285707776427,25.7860833189443,124.57548876472)) ;
#82764 = CARTESIAN_POINT('Ctrl Pts',(-18.6553224410746,25.8059794065344,124.376406038216)) ;
#82765 = CARTESIAN_POINT('Ctrl Pts',(-18.3720204939912,25.825877576446,124.062217957459)) ;
#82766 = CARTESIAN_POINT('Ctrl Pts',(-18.2124360297774,25.8457834118131,123.670170482707)) ;
#82767 = CARTESIAN_POINT('Ctrl Pts',(-18.1961936546643,25.865733336751,123.246330110804)) ;
#82768 = CARTESIAN_POINT('Ctrl Pts',(-18.3247479467419,25.8856125266614,122.843621262067)) ;
#82769 = CARTESIAN_POINT('Ctrl Pts',(-18.5841089761526,25.905593850942,122.507162548675)) ;
#82770 = CARTESIAN_POINT('Ctrl Pts',(-18.9420162535925,25.9255236351503,122.280112542374)) ;
#82771 = CARTESIAN_POINT('Ctrl Pts',(-19.355512500182,25.9454436245411,122.188825953052)) ;
#82772 = CARTESIAN_POINT('Ctrl Pts',(-19.7742961210267,25.9652988198951,122.243020652397)) ;
#82773 = CARTESIAN_POINT('Ctrl Pts',(-20.1526865313049,25.9853448215545,122.439009324516)) ;
#82774 = CARTESIAN_POINT('Ctrl Pts',(-20.390612650393,26.0018445687643,122.696940363315)) ;
#82775 = CARTESIAN_POINT('Ctrl Pts',(-20.5216824453276,26.0152331732124,122.946016191372)) ;
#82776 = CARTESIAN_POINT('Ctrl Pts',(-20.5849012114667,26.0250950015473,123.143472116702)) ;
#82777 = CARTESIAN_POINT('Ctrl Pts',(-20.6138255653156,26.0350611443048,123.351002200631)) ;
#82778 = CARTESIAN_POINT('Ctrl Pts',(-20.6032059167686,26.0484228904298,123.631608353229)) ;
#82779 = CARTESIAN_POINT('Ctrl Pts',(-20.5008843919957,26.0648772193849,123.966371529301)) ;
#82780 = CARTESIAN_POINT('Ctrl Pts',(-20.2867255145907,26.0816444644332,124.251158212897)) ;
#82781 = CARTESIAN_POINT('Ctrl Pts',(-20.0681057939674,26.0948310297072,124.421840339604)) ;
#82782 = CARTESIAN_POINT('Ctrl Pts',(-19.8829958353414,26.1048204884518,124.520903003192)) ;
#82783 = CARTESIAN_POINT('Ctrl Pts',(-19.6841239965598,26.1147742609329,124.586158608731)) ;
#82784 = CARTESIAN_POINT('Ctrl Pts',(-19.4750313009823,26.1248220774656,124.615997658308)) ;
#82785 = CARTESIAN_POINT('Ctrl Pts',(-19.268213655038,26.1346636105881,124.609461722499)) ;
#82786 = CARTESIAN_POINT('Ctrl Pts',(-19.0626573797531,26.1446498528078,124.566942370509)) ;
#82787 = CARTESIAN_POINT('Ctrl Pts',(-18.8684723237742,26.1545864762327,124.489834641604)) ;
#82788 = CARTESIAN_POINT('Ctrl Pts',(-18.6887022886735,26.1646363536156,124.378870956204)) ;
#82789 = CARTESIAN_POINT('Ctrl Pts',(-18.5339300885659,26.1744867923932,124.241258963112)) ;
#82790 = CARTESIAN_POINT('Ctrl Pts',(-18.4034137260128,26.1844588063619,124.077232557393)) ;
#82791 = CARTESIAN_POINT('Ctrl Pts',(-18.3031245373039,26.1944539749881,123.892541814178)) ;
#82792 = CARTESIAN_POINT('Ctrl Pts',(-18.2364238757988,26.2044878582493,123.692438349081)) ;
#82793 = CARTESIAN_POINT('Ctrl Pts',(-18.2057140200122,26.2143437283126,123.487510340136)) ;
#82794 = CARTESIAN_POINT('Ctrl Pts',(-18.2107938710183,26.2243412742298,123.277414606972)) ;
#82795 = CARTESIAN_POINT('Ctrl Pts',(-18.2518456721577,26.234249401129,123.073191376682)) ;
#82796 = CARTESIAN_POINT('Ctrl Pts',(-18.3281770957647,26.2442597726512,122.8770614784)) ;
#82797 = CARTESIAN_POINT('Ctrl Pts',(-18.4380159389114,26.2542902153986,122.697063925177)) ;
#82798 = CARTESIAN_POINT('Ctrl Pts',(-18.5745552026189,26.2641381679519,122.541414211324)) ;
#82799 = CARTESIAN_POINT('Ctrl Pts',(-18.7394363077977,26.2742008369729,122.408905152099)) ;
#82800 = CARTESIAN_POINT('Ctrl Pts',(-18.921826397574,26.2840952124368,122.30885227749)) ;
#82801 = CARTESIAN_POINT('Ctrl Pts',(-19.1195394226765,26.2940370107549,122.241151657766)) ;
#82802 = CARTESIAN_POINT('Ctrl Pts',(-19.3273054139925,26.3040395044822,122.208523084326)) ;
#82803 = CARTESIAN_POINT('Ctrl Pts',(-19.5382116556896,26.3140743029892,122.212809760869)) ;
#82804 = CARTESIAN_POINT('Ctrl Pts',(-19.7413463318015,26.3239191869685,122.252542608404)) ;
#82805 = CARTESIAN_POINT('Ctrl Pts',(-19.9373601105037,26.3339050437866,122.327621631711)) ;
#82806 = CARTESIAN_POINT('Ctrl Pts',(-20.1165785345523,26.3438398579613,122.434952365593)) ;
#82807 = CARTESIAN_POINT('Ctrl Pts',(-20.2762122406521,26.3538973577467,122.57355737854)) ;
#82808 = CARTESIAN_POINT('Ctrl Pts',(-20.4065114699198,26.363719116165,122.733766867349)) ;
#82809 = CARTESIAN_POINT('Ctrl Pts',(-20.5097347077751,26.373774773949,122.91823428775)) ;
#82810 = CARTESIAN_POINT('Ctrl Pts',(-20.5782258754457,26.383716956129,123.11572137009)) ;
#82811 = CARTESIAN_POINT('Ctrl Pts',(-20.611887127279,26.3936221648237,123.321218154667)) ;
#82812 = CARTESIAN_POINT('Ctrl Pts',(-20.6092537918309,26.4036639557861,123.532308255734)) ;
#82813 = CARTESIAN_POINT('Ctrl Pts',(-20.5705521085007,26.4135717302584,123.736982032277)) ;
#82814 = CARTESIAN_POINT('Ctrl Pts',(-20.4964939722591,26.423583230486,123.934001629512)) ;
#82815 = CARTESIAN_POINT('Ctrl Pts',(-20.3887491018075,26.4336159908787,124.115324540984)) ;
#82816 = CARTESIAN_POINT('Ctrl Pts',(-20.2539283340151,26.4434665600136,124.272523602686)) ;
#82817 = CARTESIAN_POINT('Ctrl Pts',(-20.0918867892734,26.4534551695435,124.406059625645)) ;
#82818 = CARTESIAN_POINT('Ctrl Pts',(-19.9101964278376,26.4633838255676,124.508820930747)) ;
#82819 = CARTESIAN_POINT('Ctrl Pts',(-19.7123664532002,26.4733715717454,124.579225540424)) ;
#82820 = CARTESIAN_POINT('Ctrl Pts',(-19.5042772626285,26.4834075606811,124.614026057559)) ;
#82821 = CARTESIAN_POINT('Ctrl Pts',(-19.2970856363154,26.4932624304947,124.612543958121)) ;
#82822 = CARTESIAN_POINT('Ctrl Pts',(-19.0903087732055,26.5032618717365,124.574850514142)) ;
#82823 = CARTESIAN_POINT('Ctrl Pts',(-18.8951319150959,26.5131569459166,124.502774164513)) ;
#82824 = CARTESIAN_POINT('Ctrl Pts',(-18.7124927509316,26.5232176017563,124.396160185279)) ;
#82825 = CARTESIAN_POINT('Ctrl Pts',(-18.5544270389059,26.5330664759519,124.262395151652)) ;
#82826 = CARTESIAN_POINT('Ctrl Pts',(-18.4191734787532,26.5430951879151,124.100664920014)) ;
#82827 = CARTESIAN_POINT('Ctrl Pts',(-18.3145428642339,26.5531245884982,123.917602937838)) ;
#82828 = CARTESIAN_POINT('Ctrl Pts',(-18.2441983040916,26.5629647821151,123.723055464282)) ;
#82829 = CARTESIAN_POINT('Ctrl Pts',(-18.2077335903667,26.5729682046903,123.515958814128)) ;
#82830 = CARTESIAN_POINT('Ctrl Pts',(-18.207849921292,26.5829537417834,123.305996098969)) ;
#82831 = CARTESIAN_POINT('Ctrl Pts',(-18.2448224488325,26.5929947462702,123.098185943807)) ;
#82832 = CARTESIAN_POINT('Ctrl Pts',(-18.3156375537416,26.6028382852114,122.90372091966)) ;
#82833 = CARTESIAN_POINT('Ctrl Pts',(-18.420226223306,26.6128233162022,122.721750391998)) ;
#82834 = CARTESIAN_POINT('Ctrl Pts',(-18.5541826435393,26.6227627787242,122.561338902929)) ;
#82835 = CARTESIAN_POINT('Ctrl Pts',(-18.7155638287665,26.632802510948,122.425330530865)) ;
#82836 = CARTESIAN_POINT('Ctrl Pts',(-18.8953261605119,26.6426906912652,122.320904791171)) ;
#82837 = CARTESIAN_POINT('Ctrl Pts',(-19.0923360261154,26.6526802069677,122.248179866433)) ;
#82838 = CARTESIAN_POINT('Ctrl Pts',(-19.2983696770575,26.6626387576224,122.211042571254)) ;
#82839 = CARTESIAN_POINT('Ctrl Pts',(-19.5064961437083,26.6725381647274,122.209729675331)) ;
#82840 = CARTESIAN_POINT('Ctrl Pts',(-19.71472754712,26.6825867511437,122.245179243824)) ;
#82841 = CARTESIAN_POINT('Ctrl Pts',(-19.9106882517753,26.6924795701081,122.314976938035)) ;
#82842 = CARTESIAN_POINT('Ctrl Pts',(-20.0947008341311,26.7025506876379,122.419616599627)) ;
#82843 = CARTESIAN_POINT('Ctrl Pts',(-20.2538532375806,26.712366381604,122.551030478766)) ;
#82844 = CARTESIAN_POINT('Ctrl Pts',(-20.3913677952363,26.7224327591013,122.711830832678)) ;
#82845 = CARTESIAN_POINT('Ctrl Pts',(-20.4970805265388,26.7323317451832,122.891149607162)) ;
#82846 = CARTESIAN_POINT('Ctrl Pts',(-20.5712377391384,26.7423859251767,123.089035348672)) ;
#82847 = CARTESIAN_POINT('Ctrl Pts',(-20.6094217290172,26.7522567381094,123.293057137242)) ;
#82848 = CARTESIAN_POINT('Ctrl Pts',(-20.6116385923756,26.7623306389632,123.504781122853)) ;
#82849 = CARTESIAN_POINT('Ctrl Pts',(-20.578165667762,26.7721507943498,123.708548577239)) ;
#82850 = CARTESIAN_POINT('Ctrl Pts',(-20.5082435307415,26.7822295013021,123.908510180151)) ;
#82851 = CARTESIAN_POINT('Ctrl Pts',(-20.4070109643156,26.7920810898409,124.089251320675)) ;
#82852 = CARTESIAN_POINT('Ctrl Pts',(-20.2731855773229,26.8021542063659,124.253326774915)) ;
#82853 = CARTESIAN_POINT('Ctrl Pts',(-20.1165101097309,26.8119967234617,124.388517173998)) ;
#82854 = CARTESIAN_POINT('Ctrl Pts',(-19.9366356777944,26.8219771850156,124.496525247979)) ;
#82855 = CARTESIAN_POINT('Ctrl Pts',(-19.7398462584671,26.8319954350064,124.57156869515)) ;
#82856 = CARTESIAN_POINT('Ctrl Pts',(-19.5358433260639,26.8418795952002,124.61119618925)) ;
#82857 = CARTESIAN_POINT('Ctrl Pts',(-19.3242969450418,26.8519447421752,124.614819303363)) ;
#82858 = CARTESIAN_POINT('Ctrl Pts',(-19.1199162618972,26.861786565816,124.582500420025)) ;
#82859 = CARTESIAN_POINT('Ctrl Pts',(-18.9203548754396,26.8718160382768,124.514444221525)) ;
#82860 = CARTESIAN_POINT('Ctrl Pts',(-18.7359669740694,26.8818428935388,124.412277169318)) ;
#82861 = CARTESIAN_POINT('Ctrl Pts',(-18.5748099018744,26.8916861436494,124.282461811643)) ;
#82862 = CARTESIAN_POINT('Ctrl Pts',(-18.4355916287619,26.9017345832325,124.123583549416)) ;
#82863 = CARTESIAN_POINT('Ctrl Pts',(-18.3274329259316,26.9116840774804,123.944547242474)) ;
#82864 = CARTESIAN_POINT('Ctrl Pts',(-18.2517329022827,26.9215919332064,123.750483492684)) ;
#82865 = CARTESIAN_POINT('Ctrl Pts',(-18.210480034894,26.9316514098564,123.543086574013)) ;
#82866 = CARTESIAN_POINT('Ctrl Pts',(-18.2056838568797,26.9414922192651,123.33623203913)) ;
#82867 = CARTESIAN_POINT('Ctrl Pts',(-18.2373097308937,26.9515543695659,123.127093653458)) ;
#82868 = CARTESIAN_POINT('Ctrl Pts',(-18.3038768892104,26.9614515306884,122.929948768524)) ;
#82869 = CARTESIAN_POINT('Ctrl Pts',(-18.403389671936,26.9713827050925,122.746410731173)) ;
#82870 = CARTESIAN_POINT('Ctrl Pts',(-18.5348933081084,26.9814249088175,122.581254032342)) ;
#82871 = CARTESIAN_POINT('Ctrl Pts',(-18.6905332850335,26.9913114912479,122.443483739432)) ;
#82872 = CARTESIAN_POINT('Ctrl Pts',(-18.8694457274301,27.0013049269963,122.333371768838)) ;
#82873 = CARTESIAN_POINT('Ctrl Pts',(-19.0638389728186,27.0112493953544,122.256431782156)) ;
#82874 = CARTESIAN_POINT('Ctrl Pts',(-19.2687173761859,27.0212012116,122.213994239668)) ;
#82875 = CARTESIAN_POINT('Ctrl Pts',(-19.4796376595632,27.0312386477145,122.207914896292)) ;
#82876 = CARTESIAN_POINT('Ctrl Pts',(-19.6852953955237,27.0411236068908,122.237889880641)) ;
#82877 = CARTESIAN_POINT('Ctrl Pts',(-19.8849208638732,27.0511217251028,122.303615150814)) ;
#82878 = CARTESIAN_POINT('Ctrl Pts',(-20.0687824125727,27.0610426576147,122.402131159829)) ;
#82879 = CARTESIAN_POINT('Ctrl Pts',(-20.2347433918381,27.0710839578368,122.532576220351)) ;
#82880 = CARTESIAN_POINT('Ctrl Pts',(-20.3736041394949,27.0809908762268,122.687807501135)) ;
#82881 = CARTESIAN_POINT('Ctrl Pts',(-20.4842302839769,27.0909266679358,122.864990331019)) ;
#82882 = CARTESIAN_POINT('Ctrl Pts',(-20.5630380544402,27.1009675625137,123.060813866335)) ;
#82883 = CARTESIAN_POINT('Ctrl Pts',(-20.6061312160508,27.1108547642276,123.264168808546)) ;
#82884 = CARTESIAN_POINT('Ctrl Pts',(-20.6136841214982,27.1208470319892,123.474087454112)) ;
#82885 = CARTESIAN_POINT('Ctrl Pts',(-20.5847396470279,27.130795553011,123.681235938774)) ;
#82886 = CARTESIAN_POINT('Ctrl Pts',(-20.5206329047438,27.1407323265887,123.880040230082)) ;
#82887 = CARTESIAN_POINT('Ctrl Pts',(-20.4227398930541,27.1507153747297,124.065715829988)) ;
#82888 = CARTESIAN_POINT('Ctrl Pts',(-20.2930387357381,27.1607590823398,124.232307363465)) ;
#82889 = CARTESIAN_POINT('Ctrl Pts',(-20.1400188875306,27.1705877754931,124.371201746397)) ;
#82890 = CARTESIAN_POINT('Ctrl Pts',(-19.9609581955699,27.1806625246225,124.484270421944)) ;
#82891 = CARTESIAN_POINT('Ctrl Pts',(-19.7689924114484,27.1905278504181,124.562839081487)) ;
#82892 = CARTESIAN_POINT('Ctrl Pts',(-19.5632221468659,27.200550024775,124.608103782849)) ;
#82893 = CARTESIAN_POINT('Ctrl Pts',(-19.352593328768,27.2105760779819,124.616438890928)) ;
#82894 = CARTESIAN_POINT('Ctrl Pts',(-19.1472929985065,27.2204297748282,124.58889990198)) ;
#82895 = CARTESIAN_POINT('Ctrl Pts',(-18.94756230638,27.2303891795812,124.526053160044)) ;
#82896 = CARTESIAN_POINT('Ctrl Pts',(-18.7604972958979,27.2404274252861,124.428392109811)) ;
#82897 = CARTESIAN_POINT('Ctrl Pts',(-18.5957070248986,27.2503016094481,124.302108734558)) ;
#82898 = CARTESIAN_POINT('Ctrl Pts',(-18.4526111915143,27.260371392586,124.146135557906)) ;
#82899 = CARTESIAN_POINT('Ctrl Pts',(-18.3413269156734,27.2702046476068,123.971898769522)) ;
#82900 = CARTESIAN_POINT('Ctrl Pts',(-18.2598539322131,27.2802350737385,123.777409894901)) ;
#82901 = CARTESIAN_POINT('Ctrl Pts',(-18.2139770900648,27.2902666859255,123.571552166036)) ;
#82902 = CARTESIAN_POINT('Ctrl Pts',(-18.204301463541,27.3000963827801,123.36514186041)) ;
#82903 = CARTESIAN_POINT('Ctrl Pts',(-18.2304203551583,27.3100858246826,123.156756796633)) ;
#82904 = CARTESIAN_POINT('Ctrl Pts',(-18.2931717693521,27.3201297166982,122.955144101719)) ;
#82905 = CARTESIAN_POINT('Ctrl Pts',(-18.387455169837,27.3299512784675,122.771448979149)) ;
#82906 = CARTESIAN_POINT('Ctrl Pts',(-18.5145023629227,27.3399868500917,122.603007681867)) ;
#82907 = CARTESIAN_POINT('Ctrl Pts',(-18.6691989465435,27.3500161243735,122.459740103133)) ;
#82908 = CARTESIAN_POINT('Ctrl Pts',(-18.8426716693766,27.3598499614921,122.347266608957)) ;
#82909 = CARTESIAN_POINT('Ctrl Pts',(-19.0371543589241,27.3699023575803,122.264600969507)) ;
#82910 = CARTESIAN_POINT('Ctrl Pts',(-19.2407489259686,27.3798391245308,122.217766395529)) ;
#82911 = CARTESIAN_POINT('Ctrl Pts',(-19.4492892687206,27.3897733595101,122.206457881068)) ;
#82912 = CARTESIAN_POINT('Ctrl Pts',(-19.6584787766812,27.3997971228369,122.231885053703)) ;
#82913 = CARTESIAN_POINT('Ctrl Pts',(-19.8573566517877,27.4096834642215,122.292260660859)) ;
#82914 = CARTESIAN_POINT('Ctrl Pts',(-20.0448842456016,27.4196725129885,122.386795149275)) ;
#82915 = CARTESIAN_POINT('Ctrl Pts',(-20.2137587561122,27.4297137336859,122.513457846421)) ;
#82916 = CARTESIAN_POINT('Ctrl Pts',(-20.3553226212523,27.4395463738638,122.664084462041)) ;
#82917 = CARTESIAN_POINT('Ctrl Pts',(-20.4709452089178,27.4495403031717,122.839511285258)) ;
#82918 = CARTESIAN_POINT('Ctrl Pts',(-20.5542369544809,27.4595695108523,123.033209537113)) ;
#82919 = CARTESIAN_POINT('Ctrl Pts',(-20.6022223083643,27.4694453225564,123.235220662099)) ;
#82920 = CARTESIAN_POINT('Ctrl Pts',(-20.6147833777703,27.4794445495278,123.44503211102)) ;
#82921 = CARTESIAN_POINT('Ctrl Pts',(-20.5911307346589,27.4893540306835,123.652044209463)) ;
#82922 = CARTESIAN_POINT('Ctrl Pts',(-20.5310228627754,27.4994072609844,123.854644058628)) ;
#82923 = CARTESIAN_POINT('Ctrl Pts',(-20.4384382046183,27.5092778775354,124.040371920306)) ;
#82924 = CARTESIAN_POINT('Ctrl Pts',(-20.3135085837969,27.5192995392675,124.210019678146)) ;
#82925 = CARTESIAN_POINT('Ctrl Pts',(-20.160659918999,27.5293223524486,124.355074881809)) ;
#82926 = CARTESIAN_POINT('Ctrl Pts',(-19.9878844387266,27.5391895169085,124.469859474152)) ;
#82927 = CARTESIAN_POINT('Ctrl Pts',(-19.7955494051919,27.5491829591284,124.554411461735)) ;
#82928 = CARTESIAN_POINT('Ctrl Pts',(-19.5905834066282,27.5592146327288,124.604073130056)) ;
#82929 = CARTESIAN_POINT('Ctrl Pts',(-19.3835855603672,27.5690810678418,124.617490990063)) ;
#82930 = CARTESIAN_POINT('Ctrl Pts',(-19.174870131399,27.5790685183749,124.59482811783)) ;
#82931 = CARTESIAN_POINT('Ctrl Pts',(-18.974033313999,27.5890134482028,124.536610658265)) ;
#82932 = CARTESIAN_POINT('Ctrl Pts',(-18.784566926627,27.5990583432579,124.443394511315)) ;
#82933 = CARTESIAN_POINT('Ctrl Pts',(-18.6171298669107,27.6089204049438,124.321093519021)) ;
#82934 = CARTESIAN_POINT('Ctrl Pts',(-18.4713021073392,27.6189121277306,124.169926560183)) ;
#82935 = CARTESIAN_POINT('Ctrl Pts',(-18.3546885614246,27.6288443419706,123.996714392999)) ;
#82936 = CARTESIAN_POINT('Ctrl Pts',(-18.2694196513225,27.6387836605363,123.805941878918)) ;
#82937 = CARTESIAN_POINT('Ctrl Pts',(-18.218224017845,27.6488278353122,123.601084916452)) ;
#82938 = CARTESIAN_POINT('Ctrl Pts',(-18.2035200669392,27.6586983893772,123.394096892666)) ;
#82939 = CARTESIAN_POINT('Ctrl Pts',(-18.2245812237522,27.6686633717313,123.185662506194)) ;
#82940 = CARTESIAN_POINT('Ctrl Pts',(-18.2821983595158,27.6786940746212,122.982815613202)) ;
#82941 = CARTESIAN_POINT('Ctrl Pts',(-18.3726338777417,27.6885864146464,122.795512202132)) ;
#82942 = CARTESIAN_POINT('Ctrl Pts',(-18.4961446567781,27.6986396478063,122.62404318365)) ;
#82943 = CARTESIAN_POINT('Ctrl Pts',(-18.6449200835009,27.7085208922831,122.479010016898)) ;
#82944 = CARTESIAN_POINT('Ctrl Pts',(-18.8191075113425,27.7185540131541,122.360127402557)) ;
#82945 = CARTESIAN_POINT('Ctrl Pts',(-19.008374966413,27.7284352234292,122.274409098091)) ;
#82946 = CARTESIAN_POINT('Ctrl Pts',(-19.2132499111456,27.7384972991985,122.221874642393)) ;
#82947 = CARTESIAN_POINT('Ctrl Pts',(-19.4198941418905,27.7483543575803,122.205962713999)) ;
#82948 = CARTESIAN_POINT('Ctrl Pts',(-19.6290171196823,27.7583489128693,122.226026761165)) ;
#82949 = CARTESIAN_POINT('Ctrl Pts',(-19.830168372801,27.7682748004048,122.281656744792)) ;
#82950 = CARTESIAN_POINT('Ctrl Pts',(-20.0204729078967,27.7782998204,122.372190057432)) ;
#82951 = CARTESIAN_POINT('Ctrl Pts',(-20.1900415778749,27.7881971975037,122.492787694309)) ;
#82952 = CARTESIAN_POINT('Ctrl Pts',(-20.3377913724602,27.7981874345846,122.642064148753)) ;
#82953 = CARTESIAN_POINT('Ctrl Pts',(-20.4575937503346,27.8082240473934,122.815752536172)) ;
#82954 = CARTESIAN_POINT('Ctrl Pts',(-20.544094957431,27.8180739308114,123.003904294989)) ;
#82955 = CARTESIAN_POINT('Ctrl Pts',(-20.5978342516824,27.8280775477138,123.20720838406)) ;
#82956 = CARTESIAN_POINT('Ctrl Pts',(-20.6153219996542,27.838066959479,123.416522180099)) ;
#82957 = CARTESIAN_POINT('Ctrl Pts',(-20.5960192166938,27.8480857208238,123.626239400183)) ;
#82958 = CARTESIAN_POINT('Ctrl Pts',(-20.5232688311072,27.8613043962049,123.89449979669)) ;
#82959 = CARTESIAN_POINT('Ctrl Pts',(-20.3813539781269,27.8746147034496,124.139307969047)) ;
#82960 = CARTESIAN_POINT('Ctrl Pts',(-20.184222532259,27.8878523696756,124.335730450596)) ;
#82961 = CARTESIAN_POINT('Ctrl Pts',(-20.0135550690303,27.8977720650863,124.45559246094)) ;
#82962 = CARTESIAN_POINT('Ctrl Pts',(-19.8220508423892,27.9078249320848,124.544956156346)) ;
#82963 = CARTESIAN_POINT('Ctrl Pts',(-19.6219767232522,27.9176803404141,124.598870292212)) ;
#82964 = CARTESIAN_POINT('Ctrl Pts',(-19.4118115423759,27.9277189720907,124.617912531858)) ;
#82965 = CARTESIAN_POINT('Ctrl Pts',(-19.1331436916363,27.9410211543577,124.594057320696)) ;
#82966 = CARTESIAN_POINT('Ctrl Pts',(-18.8021121159466,27.9575661674406,124.475054043175)) ;
#82967 = CARTESIAN_POINT('Ctrl Pts',(-18.5297401860013,27.9742181835168,124.248816186926)) ;
#82968 = CARTESIAN_POINT('Ctrl Pts',(-18.3691043653144,27.987441274422,124.021959245793)) ;
#82969 = CARTESIAN_POINT('Ctrl Pts',(-18.279074783477,27.9974022339814,123.832881356621)) ;
#82970 = CARTESIAN_POINT('Ctrl Pts',(-18.2231429975512,28.0074270307325,123.629695199133)) ;
#82971 = CARTESIAN_POINT('Ctrl Pts',(-18.1966274923705,28.0206514781283,123.352901461679)) ;
#82972 = CARTESIAN_POINT('Ctrl Pts',(-18.2547427005857,28.0372852628274,123.004090417878)) ;
#82973 = CARTESIAN_POINT('Ctrl Pts',(-18.4626541562344,28.0571879295523,122.635456474346)) ;
#82974 = CARTESIAN_POINT('Ctrl Pts',(-18.7834264089108,28.0770881573342,122.35955622577)) ;
#82975 = CARTESIAN_POINT('Ctrl Pts',(-19.179357615155,28.0970056448657,122.20926617617)) ;
#82976 = CARTESIAN_POINT('Ctrl Pts',(-19.6030850730905,28.1169351706826,122.202842194496)) ;
#82977 = CARTESIAN_POINT('Ctrl Pts',(-20.0042033525094,28.1368974385688,122.341703258092)) ;
#82978 = CARTESIAN_POINT('Ctrl Pts',(-20.3326268321142,28.156787633521,122.608069857982)) ;
#82979 = CARTESIAN_POINT('Ctrl Pts',(-20.5514322742889,28.1766778782673,122.9700984434)) ;
#82980 = CARTESIAN_POINT('Ctrl Pts',(-20.6334273789311,28.1967522508298,123.388925899664)) ;
#82981 = CARTESIAN_POINT('Ctrl Pts',(-20.5686426235298,28.2165376281901,123.804655209976)) ;
#82982 = CARTESIAN_POINT('Ctrl Pts',(-20.3652778683003,28.2364995022572,124.177163703848)) ;
#82983 = CARTESIAN_POINT('Ctrl Pts',(-20.0460051045629,28.2564794777477,124.457438441996)) ;
#82984 = CARTESIAN_POINT('Ctrl Pts',(-19.653857904935,28.2762919076256,124.611414371596)) ;
#82985 = CARTESIAN_POINT('Ctrl Pts',(-19.2292624618467,28.2962720157159,124.622968506333)) ;
#82986 = CARTESIAN_POINT('Ctrl Pts',(-18.8278348153005,28.3161663993132,124.489281226312)) ;
#82987 = CARTESIAN_POINT('Ctrl Pts',(-18.4954922096611,28.3360933272904,124.226621143619)) ;
#82988 = CARTESIAN_POINT('Ctrl Pts',(-18.2725085979326,28.3559881845916,123.867030766251)) ;
#82989 = CARTESIAN_POINT('Ctrl Pts',(-18.1854382364504,28.3760273781953,123.44997732498)) ;
#82990 = CARTESIAN_POINT('Ctrl Pts',(-18.2454140746476,28.395867346106,123.032367008361)) ;
#82991 = CARTESIAN_POINT('Ctrl Pts',(-18.4440437795509,28.4157821630701,122.658441102044)) ;
#82992 = CARTESIAN_POINT('Ctrl Pts',(-18.7589841342305,28.4357244084664,122.374569023093)) ;
#82993 = CARTESIAN_POINT('Ctrl Pts',(-19.1503541669098,28.4555964565809,122.215058285885)) ;
#82994 = CARTESIAN_POINT('Ctrl Pts',(-19.5753981818252,28.475607521535,122.198881824646)) ;
#82995 = CARTESIAN_POINT('Ctrl Pts',(-19.9769247208087,28.4954190458386,122.326892941792)) ;
#82996 = CARTESIAN_POINT('Ctrl Pts',(-20.3149985662992,28.515514257802,122.587908802987)) ;
#82997 = CARTESIAN_POINT('Ctrl Pts',(-20.5402449088348,28.5352949817218,122.943300074454)) ;
#82998 = CARTESIAN_POINT('Ctrl Pts',(-20.6325412092939,28.5552860573646,123.358060870925)) ;
#82999 = CARTESIAN_POINT('Ctrl Pts',(-20.5777380109827,28.5751679964076,123.777357890785)) ;
#83000 = CARTESIAN_POINT('Ctrl Pts',(-20.3829565395105,28.5951206009108,124.154169126176)) ;
#83001 = CARTESIAN_POINT('Ctrl Pts',(-20.0720353336252,28.6150194696415,124.441191742656)) ;
#83002 = CARTESIAN_POINT('Ctrl Pts',(-19.6822522085535,28.6349128694511,124.605274921211)) ;
#83003 = CARTESIAN_POINT('Ctrl Pts',(-19.2594120114922,28.6548220002911,124.627173959621)) ;
#83004 = CARTESIAN_POINT('Ctrl Pts',(-18.8522721728086,28.6748541000547,124.502181189478)) ;
#83005 = CARTESIAN_POINT('Ctrl Pts',(-18.5715057730066,28.6913861732241,124.290597833785)) ;
#83006 = CARTESIAN_POINT('Ctrl Pts',(-18.3986990200904,28.7047215138301,124.069861172508)) ;
#83007 = CARTESIAN_POINT('Ctrl Pts',(-18.3010384496953,28.7145640723698,123.887414318719)) ;
#83008 = CARTESIAN_POINT('Ctrl Pts',(-18.2349738172095,28.7246159792197,123.686701717407)) ;
#83009 = CARTESIAN_POINT('Ctrl Pts',(-18.1952065179791,28.7378644936106,123.411043235738)) ;
#83010 = CARTESIAN_POINT('Ctrl Pts',(-18.2364118977493,28.7544636685583,123.060489190664)) ;
#83011 = CARTESIAN_POINT('Ctrl Pts',(-18.3945321166907,28.7710524543534,122.745246203248)) ;
#83012 = CARTESIAN_POINT('Ctrl Pts',(-18.5797842873954,28.7843282706954,122.536445736904)) ;
#83013 = CARTESIAN_POINT('Ctrl Pts',(-18.7438859265167,28.7943021214892,122.405910579741)) ;
#83014 = CARTESIAN_POINT('Ctrl Pts',(-18.9292775365355,28.8043311535816,122.305499209113)) ;
#83015 = CARTESIAN_POINT('Ctrl Pts',(-19.1264646932159,28.8142212790835,122.239514293344)) ;
#83016 = CARTESIAN_POINT('Ctrl Pts',(-19.3341633145433,28.824213757355,122.208177518519)) ;
#83017 = CARTESIAN_POINT('Ctrl Pts',(-19.5433408860057,28.8341649724524,122.213247360527)) ;
#83018 = CARTESIAN_POINT('Ctrl Pts',(-19.7503772801932,28.8442134742074,122.255121662075)) ;
#83019 = CARTESIAN_POINT('Ctrl Pts',(-19.9430718587328,28.8540548238242,122.330508467652)) ;
#83020 = CARTESIAN_POINT('Ctrl Pts',(-20.1225389719754,28.8640411148444,122.43938139671)) ;
#83021 = CARTESIAN_POINT('Ctrl Pts',(-20.2797113936261,28.873977726573,122.577040956257)) ;
#83022 = CARTESIAN_POINT('Ctrl Pts',(-20.4119681738559,28.8840276019406,122.741778191217)) ;
#83023 = CARTESIAN_POINT('Ctrl Pts',(-20.5117487555868,28.893878060476,122.923259385367)) ;
#83024 = CARTESIAN_POINT('Ctrl Pts',(-20.5798319599895,28.9038499974288,123.121510222702)) ;
#83025 = CARTESIAN_POINT('Ctrl Pts',(-20.6125111693682,28.9138454543609,123.329122115711)) ;
#83026 = CARTESIAN_POINT('Ctrl Pts',(-20.6083934061051,28.923878261414,123.539989200486)) ;
#83027 = CARTESIAN_POINT('Ctrl Pts',(-20.5686973010357,28.9337381480039,123.74344956962)) ;
#83028 = CARTESIAN_POINT('Ctrl Pts',(-20.493679373233,28.9437272285692,123.939575692006)) ;
#83029 = CARTESIAN_POINT('Ctrl Pts',(-20.3863550998014,28.9536587077783,124.118678011433)) ;
#83030 = CARTESIAN_POINT('Ctrl Pts',(-20.249070224389,28.9636445672243,124.27752143985)) ;
#83031 = CARTESIAN_POINT('Ctrl Pts',(-20.0852249936528,28.9736827178714,124.410502587285)) ;
#83032 = CARTESIAN_POINT('Ctrl Pts',(-19.904447217627,28.9835308083759,124.511458793351)) ;
#83033 = CARTESIAN_POINT('Ctrl Pts',(-19.7047579448723,28.9935917168938,124.581118061351)) ;
#83034 = CARTESIAN_POINT('Ctrl Pts',(-19.4993889431451,29.0034865640518,124.614351432211)) ;
#83035 = CARTESIAN_POINT('Ctrl Pts',(-19.2904222945581,29.0134282360969,124.611964719731)) ;
#83036 = CARTESIAN_POINT('Ctrl Pts',(-19.0837191063688,29.0234307632223,124.573165462231)) ;
#83037 = CARTESIAN_POINT('Ctrl Pts',(-18.8864144001065,29.0334655544098,124.498528920258)) ;
#83038 = CARTESIAN_POINT('Ctrl Pts',(-18.7082976445877,29.0433104342689,124.393092631481)) ;
#83039 = CARTESIAN_POINT('Ctrl Pts',(-18.5487226744575,29.0532963148874,124.256732103658)) ;
#83040 = CARTESIAN_POINT('Ctrl Pts',(-18.4157694205225,29.0632310379806,124.095604648302)) ;
#83041 = CARTESIAN_POINT('Ctrl Pts',(-18.3117412163871,29.0732888782918,123.91155389501)) ;
#83042 = CARTESIAN_POINT('Ctrl Pts',(-18.2425809972532,29.0831093656883,123.716996801485)) ;
#83043 = CARTESIAN_POINT('Ctrl Pts',(-18.2070771108362,29.0931697670334,123.508522429768)) ;
#83044 = CARTESIAN_POINT('Ctrl Pts',(-18.2085773475788,29.1031007325863,123.299723943504)) ;
#83045 = CARTESIAN_POINT('Ctrl Pts',(-18.2458733773094,29.1130395949228,123.094155479002)) ;
#83046 = CARTESIAN_POINT('Ctrl Pts',(-18.3185218478309,29.123025325849,122.897169941289)) ;
#83047 = CARTESIAN_POINT('Ctrl Pts',(-18.4248524145763,29.1330497112764,122.715235116205)) ;
#83048 = CARTESIAN_POINT('Ctrl Pts',(-18.559295617884,29.1429529956297,122.55622987037)) ;
#83049 = CARTESIAN_POINT('Ctrl Pts',(-18.7218419122943,29.1530130002077,122.420962440277)) ;
#83050 = CARTESIAN_POINT('Ctrl Pts',(-18.9014185037897,29.1628562692768,122.318086410997)) ;
#83051 = CARTESIAN_POINT('Ctrl Pts',(-19.0988343275783,29.1728468348845,122.246460342704)) ;
#83052 = CARTESIAN_POINT('Ctrl Pts',(-19.3044348738419,29.1827749666633,122.210453577453)) ;
#83053 = CARTESIAN_POINT('Ctrl Pts',(-19.5144210476911,29.1927628537442,122.210327948367)) ;
#83054 = CARTESIAN_POINT('Ctrl Pts',(-19.722154657313,29.2027988033129,122.247189650964)) ;
#83055 = CARTESIAN_POINT('Ctrl Pts',(-19.9168982115564,29.2126536896917,122.317939837635)) ;
#83056 = CARTESIAN_POINT('Ctrl Pts',(-20.099129259896,29.2226531040396,122.422673271606)) ;
#83057 = CARTESIAN_POINT('Ctrl Pts',(-20.2589220492417,29.2325482692301,122.555925374151)) ;
#83058 = CARTESIAN_POINT('Ctrl Pts',(-20.3953335945201,29.242608587922,122.717517992467)) ;
#83059 = CARTESIAN_POINT('Ctrl Pts',(-20.4995231362164,29.2524587196981,122.896499773068)) ;
#83060 = CARTESIAN_POINT('Ctrl Pts',(-20.5728206243323,29.2624892901484,123.094215207785)) ;
#83061 = CARTESIAN_POINT('Ctrl Pts',(-20.6101551347691,29.2725034408212,123.301419340689)) ;
#83062 = CARTESIAN_POINT('Ctrl Pts',(-20.611271903258,29.2823963743666,123.509400284579)) ;
#83063 = CARTESIAN_POINT('Ctrl Pts',(-20.5761577667123,29.2923858883568,123.716434470495)) ;
#83064 = CARTESIAN_POINT('Ctrl Pts',(-20.505994801406,29.3023396590093,123.91361267384)) ;
#83065 = CARTESIAN_POINT('Ctrl Pts',(-20.4015456777071,29.3123874276698,124.097194226307)) ;
#83066 = CARTESIAN_POINT('Ctrl Pts',(-20.2697350753662,29.3222291541096,124.256700948655)) ;
#83067 = CARTESIAN_POINT('Ctrl Pts',(-20.1102649351783,29.3322146709324,124.393174759304)) ;
#83068 = CARTESIAN_POINT('Ctrl Pts',(-19.9303421124139,29.342154002628,124.499490590629)) ;
#83069 = CARTESIAN_POINT('Ctrl Pts',(-19.7327438419793,29.3521937723255,124.573634332047)) ;
#83070 = CARTESIAN_POINT('Ctrl Pts',(-19.5283969336439,29.3620819335743,124.611863917295)) ;
#83071 = CARTESIAN_POINT('Ctrl Pts',(-19.318408138685,29.3720714880767,124.61444751305)) ;
#83072 = CARTESIAN_POINT('Ctrl Pts',(-19.1118302786596,29.3820299026003,124.580478870266)) ;
#83073 = CARTESIAN_POINT('Ctrl Pts',(-18.9152650511162,29.3919298154297,124.512040426744)) ;
#83074 = CARTESIAN_POINT('Ctrl Pts',(-18.7309320391737,29.4019765150796,124.408967908519)) ;
#83075 = CARTESIAN_POINT('Ctrl Pts',(-18.5695640054962,29.4118763753852,124.277476281909)) ;
#83076 = CARTESIAN_POINT('Ctrl Pts',(-18.4313828878791,29.4219277795906,124.117644015429)) ;
#83077 = CARTESIAN_POINT('Ctrl Pts',(-18.3247938273524,29.4318088165118,123.939309433569)) ;
#83078 = CARTESIAN_POINT('Ctrl Pts',(-18.2496549022467,29.4418086486893,123.743005208198)) ;
#83079 = CARTESIAN_POINT('Ctrl Pts',(-18.2098863976418,29.4517266516742,123.538288197709)) ;
#83080 = CARTESIAN_POINT('Ctrl Pts',(-18.2062893419363,29.4617779575487,123.327044356571)) ;
#83081 = CARTESIAN_POINT('Ctrl Pts',(-18.2385895959843,29.4716477809403,123.122034250536)) ;
#83082 = CARTESIAN_POINT('Ctrl Pts',(-18.3073743398675,29.4817219469906,122.921775475891)) ;
#83083 = CARTESIAN_POINT('Ctrl Pts',(-18.4071229866679,29.4915420311322,122.740968826247)) ;
#83084 = CARTESIAN_POINT('Ctrl Pts',(-18.5399452984231,29.5016207578681,122.575947041892)) ;
#83085 = CARTESIAN_POINT('Ctrl Pts',(-18.6958378157169,29.5114723385176,122.439518093478)) ;
#83086 = CARTESIAN_POINT('Ctrl Pts',(-18.8768647521978,29.521545466816,122.329703299433)) ;
#83087 = CARTESIAN_POINT('Ctrl Pts',(-19.0697539979625,29.5313879447074,122.254755395135)) ;
#83088 = CARTESIAN_POINT('Ctrl Pts',(-19.2754083676275,29.5413685513055,122.213189334731)) ;
#83089 = CARTESIAN_POINT('Ctrl Pts',(-19.485955652892,29.5513862603243,122.2083402379)) ;
#83090 = CARTESIAN_POINT('Ctrl Pts',(-19.6914902361341,29.5612724393617,122.239308647118)) ;
#83091 = CARTESIAN_POINT('Ctrl Pts',(-19.8919142714091,29.571330051934,122.306617589253)) ;
#83092 = CARTESIAN_POINT('Ctrl Pts',(-20.0742975260261,29.5812064453062,122.405879060446)) ;
#83093 = CARTESIAN_POINT('Ctrl Pts',(-20.2389379421708,29.5912014734566,122.536433084805)) ;
#83094 = CARTESIAN_POINT('Ctrl Pts',(-20.3785081408678,29.6012222203026,122.694246134392)) ;
#83095 = CARTESIAN_POINT('Ctrl Pts',(-20.4874550855457,29.611124288969,122.871631043243)) ;
#83096 = CARTESIAN_POINT('Ctrl Pts',(-20.5649217226117,29.6211150287887,123.066861318861)) ;
#83097 = CARTESIAN_POINT('Ctrl Pts',(-20.6070427364269,29.631078224999,123.272029797791)) ;
#83098 = CARTESIAN_POINT('Ctrl Pts',(-20.6133815262534,29.6409824092991,123.4801692879)) ;
#83099 = CARTESIAN_POINT('Ctrl Pts',(-20.5828416910867,29.65104286969,123.68942921765)) ;
#83100 = CARTESIAN_POINT('Ctrl Pts',(-20.5181178762266,29.6608834155608,123.885951528494)) ;
#83101 = CARTESIAN_POINT('Ctrl Pts',(-20.4183117865064,29.6709456362725,124.072440578358)) ;
#83102 = CARTESIAN_POINT('Ctrl Pts',(-20.2895938023547,29.6808427792891,124.235930311958)) ;
#83103 = CARTESIAN_POINT('Ctrl Pts',(-20.1343856079396,29.6907739557063,124.375570798608)) ;
#83104 = CARTESIAN_POINT('Ctrl Pts',(-19.9551846882219,29.7008161694849,124.487181192015)) ;
#83105 = CARTESIAN_POINT('Ctrl Pts',(-19.7624071612754,29.7107027096876,124.564908201709)) ;
#83106 = CARTESIAN_POINT('Ctrl Pts',(-19.5569567804311,29.720696304293,124.608773536135)) ;
#83107 = CARTESIAN_POINT('Ctrl Pts',(-19.3480261376384,29.7306401794506,124.616231476392)) ;
#83108 = CARTESIAN_POINT('Ctrl Pts',(-19.1406146531479,29.7406007155654,124.587525948238)) ;
#83109 = CARTESIAN_POINT('Ctrl Pts',(-18.9405437604366,29.7505973188881,124.523120293792)) ;
#83110 = CARTESIAN_POINT('Ctrl Pts',(-18.7541801252713,29.7606304018426,124.424343499834)) ;
#83111 = CARTESIAN_POINT('Ctrl Pts',(-18.59065350497,29.7704815705442,124.297265216123)) ;
#83112 = CARTESIAN_POINT('Ctrl Pts',(-18.4496497380777,29.7804440612431,124.142406990805)) ;
#83113 = CARTESIAN_POINT('Ctrl Pts',(-18.337145412894,29.7904724896608,123.964090322171)) ;
#83114 = CARTESIAN_POINT('Ctrl Pts',(-18.25819728872,29.8003828570254,123.771290917072)) ;
#83115 = CARTESIAN_POINT('Ctrl Pts',(-18.2132772363488,29.8103177246405,123.567310255916)) ;
#83116 = CARTESIAN_POINT('Ctrl Pts',(-18.2045597770297,29.8203588666195,123.356400641158)) ;
#83117 = CARTESIAN_POINT('Ctrl Pts',(-18.2320230342371,29.8302460028227,123.150352695314)) ;
#83118 = CARTESIAN_POINT('Ctrl Pts',(-18.2951719204759,29.8402382852261,122.950015139329)) ;
#83119 = CARTESIAN_POINT('Ctrl Pts',(-18.3917862051207,29.8501868131913,122.764504981868)) ;
#83120 = CARTESIAN_POINT('Ctrl Pts',(-18.5187400573616,29.8601235443534,122.598627788548)) ;
#83121 = CARTESIAN_POINT('Ctrl Pts',(-18.673140853215,29.8701067552134,122.456430324054)) ;
#83122 = CARTESIAN_POINT('Ctrl Pts',(-18.8511109701876,29.8801498543633,122.342866858803)) ;
#83123 = CARTESIAN_POINT('Ctrl Pts',(-19.0418427105954,29.8899808186382,122.263194741687)) ;
#83124 = CARTESIAN_POINT('Ctrl Pts',(-19.2483822765628,29.9000536710241,122.216595398939)) ;
#83125 = CARTESIAN_POINT('Ctrl Pts',(-19.455549423982,29.9099177987359,122.20680736902)) ;
#83126 = CARTESIAN_POINT('Ctrl Pts',(-19.6646004829869,29.9199400008708,122.233040555836)) ;
#83127 = CARTESIAN_POINT('Ctrl Pts',(-19.8658934126634,29.9299671938392,122.295687403736)) ;
#83128 = CARTESIAN_POINT('Ctrl Pts',(-20.0501683092842,29.9398227878062,122.390377344587)) ;
#83129 = CARTESIAN_POINT('Ctrl Pts',(-20.2172985731652,29.9497799596715,122.516433231891)) ;
#83130 = CARTESIAN_POINT('Ctrl Pts',(-20.3608933907705,29.9598188036699,122.671082973157)) ;
#83131 = CARTESIAN_POINT('Ctrl Pts',(-20.4739034023993,29.9696928275454,122.84524049053)) ;
#83132 = CARTESIAN_POINT('Ctrl Pts',(-20.5565361429159,29.9797626535358,123.040115256471)) ;
#83133 = CARTESIAN_POINT('Ctrl Pts',(-20.6030779857184,29.9895958974331,123.241551209471)) ;
#83134 = CARTESIAN_POINT('Ctrl Pts',(-20.6147495281195,29.9996263252062,123.452092287856)) ;
#83135 = CARTESIAN_POINT('Ctrl Pts',(-20.5890726629342,30.0096579419513,123.661431338415)) ;
#83136 = CARTESIAN_POINT('Ctrl Pts',(-20.5290983151318,30.019487618932,123.859172845459)) ;
#83137 = CARTESIAN_POINT('Ctrl Pts',(-20.434731970837,30.0294771357719,124.046795693821)) ;
#83138 = CARTESIAN_POINT('Ctrl Pts',(-20.3081181710845,30.0395207479117,124.215767057646)) ;
#83139 = CARTESIAN_POINT('Ctrl Pts',(-20.1577705279338,30.049343354247,124.35732849996)) ;
#83140 = CARTESIAN_POINT('Ctrl Pts',(-19.9816087128904,30.0593815841462,124.473517351811)) ;
#83141 = CARTESIAN_POINT('Ctrl Pts',(-19.7882588039469,30.0693926189382,124.556686176543)) ;
#83142 = CARTESIAN_POINT('Ctrl Pts',(-19.5858185488893,30.0792903499053,124.604791885319)) ;
#83143 = CARTESIAN_POINT('Ctrl Pts',(-19.3761865187044,30.0892799777558,124.617404592443)) ;
#83144 = CARTESIAN_POINT('Ctrl Pts',(-19.1682644783533,30.0992357682018,124.593435202836)) ;
#83145 = CARTESIAN_POINT('Ctrl Pts',(-18.9681109878404,30.1091631667638,124.53427778847)) ;
#83146 = CARTESIAN_POINT('Ctrl Pts',(-18.7794620901044,30.1191887618737,124.440297304535)) ;
#83147 = CARTESIAN_POINT('Ctrl Pts',(-18.6122766484749,30.1290746125433,124.316833188977)) ;
#83148 = CARTESIAN_POINT('Ctrl Pts',(-18.4672078423433,30.1390637923875,124.164980782603)) ;
#83149 = CARTESIAN_POINT('Ctrl Pts',(-18.3504739201255,30.149104979491,123.989097076407)) ;
#83150 = CARTESIAN_POINT('Ctrl Pts',(-18.2674956317655,30.158937622967,123.799773764769)) ;
#83151 = CARTESIAN_POINT('Ctrl Pts',(-18.2172642412709,30.1689315726765,123.595763800434)) ;
#83152 = CARTESIAN_POINT('Ctrl Pts',(-18.203613049275,30.178960695453,123.385360236912)) ;
#83153 = CARTESIAN_POINT('Ctrl Pts',(-18.2260199316159,30.1888368263717,123.178935369056)) ;
#83154 = CARTESIAN_POINT('Ctrl Pts',(-18.2843970102494,30.1988348613887,122.977040722259)) ;
#83155 = CARTESIAN_POINT('Ctrl Pts',(-18.3760423177623,30.2087487911474,122.789820231878)) ;
#83156 = CARTESIAN_POINT('Ctrl Pts',(-18.5003433721555,30.2187919788852,122.619168159099)) ;
#83157 = CARTESIAN_POINT('Ctrl Pts',(-18.6502274233987,30.2286918210256,122.474753642193)) ;
#83158 = CARTESIAN_POINT('Ctrl Pts',(-18.8242469442218,30.2386830878336,122.357118257708)) ;
#83159 = CARTESIAN_POINT('Ctrl Pts',(-19.0169820154261,30.2487151899655,122.271468240282)) ;
#83160 = CARTESIAN_POINT('Ctrl Pts',(-19.2182167060322,30.2585820709203,122.221158082751)) ;
#83161 = CARTESIAN_POINT('Ctrl Pts',(-19.4277225488607,30.2685738622084,122.205867869769)) ;
#83162 = CARTESIAN_POINT('Ctrl Pts',(-19.6374978256527,30.27860597812,122.227678696559)) ;
#83163 = CARTESIAN_POINT('Ctrl Pts',(-19.8370434526668,30.28847229492,122.284323901951)) ;
#83164 = CARTESIAN_POINT('Ctrl Pts',(-20.0261335233839,30.2984597763936,122.375543048429)) ;
#83165 = CARTESIAN_POINT('Ctrl Pts',(-20.1958972985317,30.3084047007725,122.49762869755)) ;
#83166 = CARTESIAN_POINT('Ctrl Pts',(-20.3432317615189,30.3184495866832,122.648887741277)) ;
#83167 = CARTESIAN_POINT('Ctrl Pts',(-20.4600715018246,30.3283116903958,122.820180920246)) ;
#83168 = CARTESIAN_POINT('Ctrl Pts',(-20.5468880473964,30.3383032542202,123.011437808103)) ;
#83169 = CARTESIAN_POINT('Ctrl Pts',(-20.5987893919799,30.3482360622831,123.21370328218)) ;
#83170 = CARTESIAN_POINT('Ctrl Pts',(-20.6153024482951,30.3581731645195,123.421971743177)) ;
#83171 = CARTESIAN_POINT('Ctrl Pts',(-20.5948955461052,30.3682256107899,123.63230200216)) ;
#83172 = CARTESIAN_POINT('Ctrl Pts',(-20.5397174330207,30.3780717263715,123.831827122385)) ;
#83173 = CARTESIAN_POINT('Ctrl Pts',(-20.4492191425848,30.3881197460864,124.022684679915)) ;
#83174 = CARTESIAN_POINT('Ctrl Pts',(-20.3279940543757,30.3980616977153,124.192964425444)) ;
#83175 = CARTESIAN_POINT('Ctrl Pts',(-20.1794618084049,30.4080004787144,124.33992376818)) ;
#83176 = CARTESIAN_POINT('Ctrl Pts',(-20.0060825101838,30.4180265274405,124.45976448913)) ;
#83177 = CARTESIAN_POINT('Ctrl Pts',(-19.8172623615967,30.4279133878487,124.546716314081)) ;
#83178 = CARTESIAN_POINT('Ctrl Pts',(-19.6133595978461,30.4379446629805,124.600410230691)) ;
#83179 = CARTESIAN_POINT('Ctrl Pts',(-19.4062767925641,30.4478276402809,124.617843638863)) ;
#83180 = CARTESIAN_POINT('Ctrl Pts',(-19.1957688211311,30.4578844936881,124.598739097093)) ;
#83181 = CARTESIAN_POINT('Ctrl Pts',(-18.9283787606756,30.471052734764,124.526647165086)) ;
#83182 = CARTESIAN_POINT('Ctrl Pts',(-18.6818039728824,30.4844537639905,124.384038008386)) ;
#83183 = CARTESIAN_POINT('Ctrl Pts',(-18.4857400799911,30.4976666807214,124.187208677308)) ;
#83184 = CARTESIAN_POINT('Ctrl Pts',(-18.3657914541072,30.5075950751746,124.016432968705)) ;
#83185 = CARTESIAN_POINT('Ctrl Pts',(-18.2766768590663,30.5175765753027,123.826421058636)) ;
#83186 = CARTESIAN_POINT('Ctrl Pts',(-18.2218764268591,30.5276171185728,123.622585952812)) ;
#83187 = CARTESIAN_POINT('Ctrl Pts',(-18.2033813661449,30.5374664503559,123.416346888214)) ;
#83188 = CARTESIAN_POINT('Ctrl Pts',(-18.2206996447847,30.5474618548276,123.206928595446)) ;
#83189 = CARTESIAN_POINT('Ctrl Pts',(-18.2745929041492,30.5574781822762,123.003367309086)) ;
#83190 = CARTESIAN_POINT('Ctrl Pts',(-18.3909391811523,30.5707018394427,122.750841186866)) ;
#83191 = CARTESIAN_POINT('Ctrl Pts',(-18.5712709267288,30.5839961308321,122.53321318112)) ;
#83192 = CARTESIAN_POINT('Ctrl Pts',(-18.7990626847824,30.5972804817636,122.371616533633)) ;
#83193 = CARTESIAN_POINT('Ctrl Pts',(-18.9884333508581,30.6072528628254,122.281709437163)) ;
#83194 = CARTESIAN_POINT('Ctrl Pts',(-19.1891893065226,30.617161242451,122.226046310469)) ;
#83195 = CARTESIAN_POINT('Ctrl Pts',(-19.3995715448735,30.627215241199,122.205891863364)) ;
#83196 = CARTESIAN_POINT('Ctrl Pts',(-19.606289331107,30.6370774383153,122.2220960198)) ;
#83197 = CARTESIAN_POINT('Ctrl Pts',(-19.8780883135872,30.6504245646895,122.291836907067)) ;
#83198 = CARTESIAN_POINT('Ctrl Pts',(-20.1845056854532,30.6669615303309,122.46430462257)) ;
#83199 = CARTESIAN_POINT('Ctrl Pts',(-20.4154425969608,30.6835961345048,122.732190513853)) ;
#83200 = CARTESIAN_POINT('Ctrl Pts',(-20.5367455747761,30.6968859277475,122.983880923607)) ;
#83201 = CARTESIAN_POINT('Ctrl Pts',(-20.5937491354777,30.7068385590069,123.185188446597)) ;
#83202 = CARTESIAN_POINT('Ctrl Pts',(-20.6151760975103,30.7167905263116,123.393329160038)) ;
#83203 = CARTESIAN_POINT('Ctrl Pts',(-20.5948114579857,30.7301577847754,123.67359407567)) ;
#83204 = CARTESIAN_POINT('Ctrl Pts',(-20.4800577195779,30.7466745967245,124.005597255658)) ;
#83205 = CARTESIAN_POINT('Ctrl Pts',(-20.2120200993978,30.7667004917309,124.336309570418)) ;
#83206 = CARTESIAN_POINT('Ctrl Pts',(-19.8510357660558,30.7865112218611,124.553553066115)) ;
#83207 = CARTESIAN_POINT('Ctrl Pts',(-19.4344068486954,30.8064884379909,124.636126295085)) ;
#83208 = CARTESIAN_POINT('Ctrl Pts',(-19.0157737449017,30.8264153133862,124.570966815067)) ;
#83209 = CARTESIAN_POINT('Ctrl Pts',(-18.645743049627,30.8462367748625,124.36909313754)) ;
#83210 = CARTESIAN_POINT('Ctrl Pts',(-18.3635487087384,30.8663110926718,124.048939440631)) ;
#83211 = CARTESIAN_POINT('Ctrl Pts',(-18.2096219039696,30.8861590616797,123.655865535498)) ;
#83212 = CARTESIAN_POINT('Ctrl Pts',(-18.19815035681,30.9061060957429,123.231985121454)) ;
#83213 = CARTESIAN_POINT('Ctrl Pts',(-18.3318134073363,30.926002046715,122.830579249658)) ;
#83214 = CARTESIAN_POINT('Ctrl Pts',(-18.5938414916461,30.9458975263333,122.498499904225)) ;
#83215 = CARTESIAN_POINT('Ctrl Pts',(-18.9545566345522,30.9658536372981,122.274979619949)) ;
#83216 = CARTESIAN_POINT('Ctrl Pts',(-19.3687579852179,30.9857581853381,122.188333585932)) ;
#83217 = CARTESIAN_POINT('Ctrl Pts',(-19.7873089672698,31.0056323096572,122.247107307915)) ;
#83218 = CARTESIAN_POINT('Ctrl Pts',(-20.1636515298828,31.0256868396562,122.447450777236)) ;
#83219 = CARTESIAN_POINT('Ctrl Pts',(-20.4457199868758,31.0454943534162,122.760325250148)) ;
#83220 = CARTESIAN_POINT('Ctrl Pts',(-20.6062681401233,31.0654777091839,123.153662164199)) ;
#83221 = CARTESIAN_POINT('Ctrl Pts',(-20.6222628204701,31.0853960117678,123.576872257537)) ;
#83222 = CARTESIAN_POINT('Ctrl Pts',(-20.4942581378236,31.1052642272136,123.979554943358)) ;
#83223 = CARTESIAN_POINT('Ctrl Pts',(-20.2337562023119,31.1253145440099,124.31687445342)) ;
#83224 = CARTESIAN_POINT('Ctrl Pts',(-19.8787616566699,31.1450906058923,124.542563564278)) ;
#83225 = CARTESIAN_POINT('Ctrl Pts',(-19.4626826896039,31.1651452115848,124.635079575042)) ;
#83226 = CARTESIAN_POINT('Ctrl Pts',(-19.0452264784568,31.1849389007407,124.580607517285)) ;
#83227 = CARTESIAN_POINT('Ctrl Pts',(-18.6678122022123,31.2049055923351,124.38638898605)) ;
#83228 = CARTESIAN_POINT('Ctrl Pts',(-18.3797967673245,31.224865638086,124.07456737004)) ;
#83229 = CARTESIAN_POINT('Ctrl Pts',(-18.2157691109868,31.2447638982363,123.684593743109)) ;
#83230 = CARTESIAN_POINT('Ctrl Pts',(-18.1941556982586,31.2646588137855,123.262145187816)) ;
#83231 = CARTESIAN_POINT('Ctrl Pts',(-18.3177211897733,31.2845689941991,122.857238651777)) ;
#83232 = CARTESIAN_POINT('Ctrl Pts',(-18.5722267264253,31.3045047933133,122.518239434528)) ;
#83233 = CARTESIAN_POINT('Ctrl Pts',(-18.9271454738372,31.3244426549675,122.286400969285)) ;
#83234 = CARTESIAN_POINT('Ctrl Pts',(-19.3394522016131,31.3443617016051,122.189424102426)) ;
#83235 = CARTESIAN_POINT('Ctrl Pts',(-19.7607105158001,31.3643105996593,122.238978385728)) ;
#83236 = CARTESIAN_POINT('Ctrl Pts',(-20.1390295029159,31.3842164271023,122.428816602022)) ;
#83237 = CARTESIAN_POINT('Ctrl Pts',(-20.3815087264455,31.4007991224676,122.684686241664)) ;
#83238 = CARTESIAN_POINT('Ctrl Pts',(-20.5148524186569,31.4140733361913,122.929906786892)) ;
#83239 = CARTESIAN_POINT('Ctrl Pts',(-20.5818785542684,31.4241200553906,123.130173426279)) ;
#83240 = CARTESIAN_POINT('Ctrl Pts',(-20.6127165674891,31.4339640900363,123.334840458635)) ;
#83241 = CARTESIAN_POINT('Ctrl Pts',(-20.6063535951271,31.4472984749408,123.615037152783)) ;
#83242 = CARTESIAN_POINT('Ctrl Pts',(-20.5072194117263,31.4638856922406,123.953619575348)) ;
#83243 = CARTESIAN_POINT('Ctrl Pts',(-20.2982546759496,31.4805189042785,124.238841010089)) ;
#83244 = CARTESIAN_POINT('Ctrl Pts',(-20.0804678238985,31.4938013465506,124.413704853419)) ;
#83245 = CARTESIAN_POINT('Ctrl Pts',(-19.8981272815586,31.5037072344649,124.514266935638)) ;
#83246 = CARTESIAN_POINT('Ctrl Pts',(-19.6995097079086,31.51369565257,124.582464166109)) ;
#83247 = CARTESIAN_POINT('Ctrl Pts',(-19.4913126461785,31.5237190798087,124.615029422142)) ;
#83248 = CARTESIAN_POINT('Ctrl Pts',(-19.2831319092561,31.5336235109258,124.611113980468)) ;
#83249 = CARTESIAN_POINT('Ctrl Pts',(-19.0093614799214,31.5468866635362,124.558272298217)) ;
#83250 = CARTESIAN_POINT('Ctrl Pts',(-18.7546008901196,31.5602115614401,124.434360421277)) ;
#83251 = CARTESIAN_POINT('Ctrl Pts',(-18.5439610209561,31.5734673050557,124.251809963666)) ;
#83252 = CARTESIAN_POINT('Ctrl Pts',(-18.4117282371194,31.583426678503,124.089512292891)) ;
#83253 = CARTESIAN_POINT('Ctrl Pts',(-18.3095841784395,31.5933705024299,123.907084613389)) ;
#83254 = CARTESIAN_POINT('Ctrl Pts',(-18.2401310523998,31.6034184465772,123.707606289012)) ;
#83255 = CARTESIAN_POINT('Ctrl Pts',(-18.2068457694298,31.6132694177954,123.503187635857)) ;
#83256 = CARTESIAN_POINT('Ctrl Pts',(-18.2090524602005,31.6232412352375,123.293584248886)) ;
#83257 = CARTESIAN_POINT('Ctrl Pts',(-18.2477548018564,31.6332366575296,123.087014130891)) ;
#83258 = CARTESIAN_POINT('Ctrl Pts',(-18.3222090746577,31.6432697226533,122.889672426475)) ;
#83259 = CARTESIAN_POINT('Ctrl Pts',(-18.4278263368555,31.6531350553185,122.71118449622)) ;
#83260 = CARTESIAN_POINT('Ctrl Pts',(-18.5636713658397,31.6630955979161,122.551819036529)) ;
#83261 = CARTESIAN_POINT('Ctrl Pts',(-18.7265249362776,31.6731292834178,122.417766698447)) ;
#83262 = CARTESIAN_POINT('Ctrl Pts',(-18.9073121335119,31.683014115408,122.31523335348)) ;
#83263 = CARTESIAN_POINT('Ctrl Pts',(-19.1067295419793,31.6930815421679,122.244429551725)) ;
#83264 = CARTESIAN_POINT('Ctrl Pts',(-19.3107004385562,31.7029200313267,122.209912169596)) ;
#83265 = CARTESIAN_POINT('Ctrl Pts',(-19.5222334995631,31.7129835125168,122.211086087581)) ;
#83266 = CARTESIAN_POINT('Ctrl Pts',(-19.7268674082678,31.722877670332,122.248520772617)) ;
#83267 = CARTESIAN_POINT('Ctrl Pts',(-19.9229838785611,31.7328195270763,122.320715616212)) ;
#83268 = CARTESIAN_POINT('Ctrl Pts',(-20.1047748415662,31.7428220047477,122.426467352772)) ;
#83269 = CARTESIAN_POINT('Ctrl Pts',(-20.2657146991617,31.752856809052,122.562842382034)) ;
#83270 = CARTESIAN_POINT('Ctrl Pts',(-20.3982636528338,31.7627016858976,122.721817853387)) ;
#83271 = CARTESIAN_POINT('Ctrl Pts',(-20.5029887507993,31.7726875654532,122.90372683207)) ;
#83272 = CARTESIAN_POINT('Ctrl Pts',(-20.5743391712646,31.7826222958117,123.100063805189)) ;
#83273 = CARTESIAN_POINT('Ctrl Pts',(-20.6107539154827,31.7926801081246,123.308316175894)) ;
#83274 = CARTESIAN_POINT('Ctrl Pts',(-20.6108179024331,31.8025007002489,123.514810057198)) ;
#83275 = CARTESIAN_POINT('Ctrl Pts',(-20.5744003087098,31.8125672858587,123.723241387401)) ;
#83276 = CARTESIAN_POINT('Ctrl Pts',(-20.5034740802056,31.8224668664405,123.918955059192)) ;
#83277 = CARTESIAN_POINT('Ctrl Pts',(-20.3981618181735,31.8325184661188,124.102114219325)) ;
#83278 = CARTESIAN_POINT('Ctrl Pts',(-20.2651091877199,31.8423926525358,124.261505376368)) ;
#83279 = CARTESIAN_POINT('Ctrl Pts',(-20.1036202264451,31.8524491284167,124.397897467732)) ;
#83280 = CARTESIAN_POINT('Ctrl Pts',(-19.9238419317425,31.8623420597193,124.502558097825)) ;
#83281 = CARTESIAN_POINT('Ctrl Pts',(-19.7253582983379,31.8724048384319,124.575658467282)) ;
#83282 = CARTESIAN_POINT('Ctrl Pts',(-19.5217145643937,31.8822473640131,124.612477743301)) ;
#83283 = CARTESIAN_POINT('Ctrl Pts',(-19.3117088879781,31.8922381294379,124.613893835916)) ;
#83284 = CARTESIAN_POINT('Ctrl Pts',(-19.1059168167146,31.902166205436,124.579001618329)) ;
#83285 = CARTESIAN_POINT('Ctrl Pts',(-18.9080017658777,31.912154115823,124.508830983756)) ;
#83286 = CARTESIAN_POINT('Ctrl Pts',(-18.7245905230028,31.9221900279479,124.404561296605)) ;
#83287 = CARTESIAN_POINT('Ctrl Pts',(-18.5647630481987,31.9320450407956,124.27270294668)) ;
#83288 = CARTESIAN_POINT('Ctrl Pts',(-18.4281031647553,31.9420439867119,124.113022558058)) ;
#83289 = CARTESIAN_POINT('Ctrl Pts',(-18.3221272962083,31.9519408991599,123.933932731515)) ;
#83290 = CARTESIAN_POINT('Ctrl Pts',(-18.2476926054129,31.9619946972534,123.736138061524)) ;
#83291 = CARTESIAN_POINT('Ctrl Pts',(-18.2093337802235,31.97187561808,123.53195900041)) ;
#83292 = CARTESIAN_POINT('Ctrl Pts',(-18.2066019695323,31.9818801440778,123.321674466972)) ;
#83293 = CARTESIAN_POINT('Ctrl Pts',(-18.2404263440032,31.9918641076953,123.114487622753)) ;
#83294 = CARTESIAN_POINT('Ctrl Pts',(-18.3102693041505,32.0019037482466,122.915329879683)) ;
#83295 = CARTESIAN_POINT('Ctrl Pts',(-18.4114038214133,32.0117477738613,122.734771545471)) ;
#83296 = CARTESIAN_POINT('Ctrl Pts',(-18.5438394915442,32.0217387796786,122.571741129883)) ;
#83297 = CARTESIAN_POINT('Ctrl Pts',(-18.703628596721,32.0317765712108,122.433903138758)) ;
#83298 = CARTESIAN_POINT('Ctrl Pts',(-18.8812503335969,32.0416209709992,122.327667862756)) ;
#83299 = CARTESIAN_POINT('Ctrl Pts',(-19.0771971927256,32.0516057715559,122.25246020401)) ;
#83300 = CARTESIAN_POINT('Ctrl Pts',(-19.2823298265578,32.0615452949671,122.212499589025)) ;
#83301 = CARTESIAN_POINT('Ctrl Pts',(-19.4933471363301,32.0715850140681,122.208776391678)) ;
#83302 = CARTESIAN_POINT('Ctrl Pts',(-19.6987028420245,32.0814731859874,122.24115319859)) ;
#83303 = CARTESIAN_POINT('Ctrl Pts',(-19.8974425339761,32.0914627484044,122.309009013835)) ;
#83304 = CARTESIAN_POINT('Ctrl Pts',(-20.0807345462606,32.1014211205991,122.410164937541)) ;
#83305 = CARTESIAN_POINT('Ctrl Pts',(-20.2430472168791,32.1113211948298,122.540457107242)) ;
#83306 = CARTESIAN_POINT('Ctrl Pts',(-20.3822631435707,32.1213672912034,122.699266977795)) ;
#83307 = CARTESIAN_POINT('Ctrl Pts',(-20.4903109590882,32.1312758752005,122.877375105401)) ;
#83308 = CARTESIAN_POINT('Ctrl Pts',(-20.5669294967305,32.1412864537914,123.073389780507)) ;
#83309 = CARTESIAN_POINT('Ctrl Pts',(-20.608008918276,32.1513156119042,123.28020159049)) ;
#83310 = CARTESIAN_POINT('Ctrl Pts',(-20.6127724602431,32.1611684937423,123.487271842967)) ;
#83311 = CARTESIAN_POINT('Ctrl Pts',(-20.581806621185,32.1711280548933,123.694357054793)) ;
#83312 = CARTESIAN_POINT('Ctrl Pts',(-20.5144687727705,32.1811664894824,123.894350918024)) ;
#83313 = CARTESIAN_POINT('Ctrl Pts',(-20.4154130490164,32.1910397617095,124.07679460432)) ;
#83314 = CARTESIAN_POINT('Ctrl Pts',(-20.2835620235085,32.201113003703,124.242457441947)) ;
#83315 = CARTESIAN_POINT('Ctrl Pts',(-20.1290461275997,32.2109333352361,124.379450085929)) ;
#83316 = CARTESIAN_POINT('Ctrl Pts',(-19.9486477293024,32.2210119964629,124.490491077014)) ;
#83317 = CARTESIAN_POINT('Ctrl Pts',(-19.7560810791827,32.2308635917571,124.566868126149)) ;
#83318 = CARTESIAN_POINT('Ctrl Pts',(-19.5487382565785,32.2409367269859,124.609752347802)) ;
#83319 = CARTESIAN_POINT('Ctrl Pts',(-19.3418894082037,32.2507791625109,124.6158111822)) ;
#83320 = CARTESIAN_POINT('Ctrl Pts',(-19.1341823402658,32.2607599316443,124.58613825041)) ;
#83321 = CARTESIAN_POINT('Ctrl Pts',(-18.9341677743458,32.2707770328882,124.520238624712)) ;
#83322 = CARTESIAN_POINT('Ctrl Pts',(-18.7508181441457,32.2806654804901,124.42222827271)) ;
#83323 = CARTESIAN_POINT('Ctrl Pts',(-18.5845185824704,32.2907211946709,124.291738453968)) ;
#83324 = CARTESIAN_POINT('Ctrl Pts',(-18.4458907267504,32.3005964010847,124.137177696302)) ;
#83325 = CARTESIAN_POINT('Ctrl Pts',(-18.3344556829309,32.3105914535575,123.959039398453)) ;
#83326 = CARTESIAN_POINT('Ctrl Pts',(-18.2557440839217,32.3206133375196,123.763594375523)) ;
#83327 = CARTESIAN_POINT('Ctrl Pts',(-18.2124503446323,32.3305173100489,123.559934275682)) ;
#83328 = CARTESIAN_POINT('Ctrl Pts',(-18.2048119906324,32.3405058067098,123.350081945316)) ;
#83329 = CARTESIAN_POINT('Ctrl Pts',(-18.2337946180017,32.3504696039577,123.142637274561)) ;
#83330 = CARTESIAN_POINT('Ctrl Pts',(-18.2974931064922,32.3603736272658,122.944386171069)) ;
#83331 = CARTESIAN_POINT('Ctrl Pts',(-18.396316975891,32.3704341305874,122.757419493341)) ;
#83332 = CARTESIAN_POINT('Ctrl Pts',(-18.5230894394292,32.3802746657273,122.593899248481)) ;
#83333 = CARTESIAN_POINT('Ctrl Pts',(-18.6795618066723,32.3903368864319,122.451576307416)) ;
#83334 = CARTESIAN_POINT('Ctrl Pts',(-18.8555799493967,32.4002340402081,122.3406038363)) ;
#83335 = CARTESIAN_POINT('Ctrl Pts',(-19.0485759608522,32.4101651735936,122.260971581326)) ;
#83336 = CARTESIAN_POINT('Ctrl Pts',(-19.254802198742,32.4202075487393,122.215784881501)) ;
#83337 = CARTESIAN_POINT('Ctrl Pts',(-19.462464619885,32.4300934865054,122.207066667792)) ;
#83338 = CARTESIAN_POINT('Ctrl Pts',(-19.6707916883363,32.4400893294903,122.234516696651)) ;
#83339 = CARTESIAN_POINT('Ctrl Pts',(-19.8701274150094,32.4500313073689,122.297413048005)) ;
#83340 = CARTESIAN_POINT('Ctrl Pts',(-20.0559495921236,32.4599906818499,122.393870351229)) ;
#83341 = CARTESIAN_POINT('Ctrl Pts',(-20.2229152131252,32.4699872976837,122.521538033646)) ;
#83342 = CARTESIAN_POINT('Ctrl Pts',(-20.3654870895935,32.4800215162572,122.677008263768)) ;
#83343 = CARTESIAN_POINT('Ctrl Pts',(-20.4770646801134,32.4898745834678,122.851527873814)) ;
#83344 = CARTESIAN_POINT('Ctrl Pts',(-20.5580731805413,32.4998348413454,123.044611536658)) ;
#83345 = CARTESIAN_POINT('Ctrl Pts',(-20.6044060160116,32.509863868051,123.250311165375)) ;
#83346 = CARTESIAN_POINT('Ctrl Pts',(-20.6142619776741,32.5197740750854,123.458412229653)) ;
#83347 = CARTESIAN_POINT('Ctrl Pts',(-20.5883124061432,32.529708985733,123.665662879571)) ;
#83348 = CARTESIAN_POINT('Ctrl Pts',(-20.5259286930374,32.5397501159122,123.867323656511)) ;
#83349 = CARTESIAN_POINT('Ctrl Pts',(-20.4310789052782,32.5496372562822,124.052292593451)) ;
#83350 = CARTESIAN_POINT('Ctrl Pts',(-20.3045135514618,32.5596295338181,124.219935537952)) ;
#83351 = CARTESIAN_POINT('Ctrl Pts',(-20.1513762341763,32.5695780770865,124.362403871637)) ;
#83352 = CARTESIAN_POINT('Ctrl Pts',(-19.9762223695005,32.5795147519037,124.476218556103)) ;
#83353 = CARTESIAN_POINT('Ctrl Pts',(-19.7831272891508,32.58949817284,124.55852326293)) ;
#83354 = CARTESIAN_POINT('Ctrl Pts',(-19.5774219840255,32.5995404880293,124.605989529416)) ;
#83355 = CARTESIAN_POINT('Ctrl Pts',(-19.3708457610076,32.6093808054685,124.617131308199)) ;
#83356 = CARTESIAN_POINT('Ctrl Pts',(-19.1614606709902,32.619410509526,124.59224704481)) ;
#83357 = CARTESIAN_POINT('Ctrl Pts',(-18.9599202826958,32.6294314662485,124.530895291569)) ;
#83358 = CARTESIAN_POINT('Ctrl Pts',(-18.7747348077778,32.6392980085521,124.437418884862)) ;
#83359 = CARTESIAN_POINT('Ctrl Pts',(-18.6051744829553,32.6493691084972,124.310654926759)) ;
#83360 = CARTESIAN_POINT('Ctrl Pts',(-18.4634825803537,32.6592111826748,124.159861045774)) ;
#83361 = CARTESIAN_POINT('Ctrl Pts',(-18.348119531362,32.6691719772618,123.985101878547)) ;
#83362 = CARTESIAN_POINT('Ctrl Pts',(-18.2645928499221,32.6792098501627,123.79131595217)) ;
#83363 = CARTESIAN_POINT('Ctrl Pts',(-18.2163931534487,32.6890841357068,123.589374685025)) ;
#83364 = CARTESIAN_POINT('Ctrl Pts',(-18.2037592125035,32.6991538861207,123.378082408074)) ;
#83365 = CARTESIAN_POINT('Ctrl Pts',(-18.2273293206378,32.7089871706553,123.172687254376)) ;
#83366 = CARTESIAN_POINT('Ctrl Pts',(-18.2868043404784,32.7190175114554,122.970385348413)) ;
#83367 = CARTESIAN_POINT('Ctrl Pts',(-18.3810784993133,32.729049435455,122.781715068891)) ;
#83368 = CARTESIAN_POINT('Ctrl Pts',(-18.5037608242304,32.7388779703909,122.615463889597)) ;
#83369 = CARTESIAN_POINT('Ctrl Pts',(-18.6555715412042,32.7488717481556,122.470222039496)) ;
#83370 = CARTESIAN_POINT('Ctrl Pts',(-18.8311254092731,32.7588994586411,122.353490726389)) ;
#83371 = CARTESIAN_POINT('Ctrl Pts',(-19.0214892252655,32.7687878694751,122.269952805632)) ;
#83372 = CARTESIAN_POINT('Ctrl Pts',(-19.2251690251725,32.7787647200106,122.219945127882)) ;
#83373 = CARTESIAN_POINT('Ctrl Pts',(-19.4347962363997,32.7887565165611,122.206021141314)) ;
#83374 = CARTESIAN_POINT('Ctrl Pts',(-19.644506274362,32.7987925226548,122.229058211083)) ;
#83375 = CARTESIAN_POINT('Ctrl Pts',(-19.8434117086824,32.8086432569176,122.286768454023)) ;
#83376 = CARTESIAN_POINT('Ctrl Pts',(-20.0320459418187,32.8186345154458,122.379097172002)) ;
#83377 = CARTESIAN_POINT('Ctrl Pts',(-20.200655836678,32.828552410349,122.501801185391)) ;
#83378 = CARTESIAN_POINT('Ctrl Pts',(-20.3470163616419,32.838580552012,122.653517385148)) ;
#83379 = CARTESIAN_POINT('Ctrl Pts',(-20.4632160383456,32.8484657201279,122.825818799276)) ;
#83380 = CARTESIAN_POINT('Ctrl Pts',(-20.5490902337959,32.8584550836339,123.017471264473)) ;
#83381 = CARTESIAN_POINT('Ctrl Pts',(-20.6002153354156,32.8684962186439,123.222283159047)) ;
#83382 = CARTESIAN_POINT('Ctrl Pts',(-20.6150344431865,32.878328886832,123.428460757677)) ;
#83383 = CARTESIAN_POINT('Ctrl Pts',(-20.594080101708,32.8883227897865,123.637515478041)) ;
#83384 = CARTESIAN_POINT('Ctrl Pts',(-20.5365126192868,32.898352074871,123.840353459571)) ;
#83385 = CARTESIAN_POINT('Ctrl Pts',(-20.4463103933135,32.9082276033129,124.027361177366)) ;
#83386 = CARTESIAN_POINT('Ctrl Pts',(-20.3236864945423,32.9182278859289,124.198101789634)) ;
#83387 = CARTESIAN_POINT('Ctrl Pts',(-20.1746881491512,32.928139901986,124.343816675066)) ;
#83388 = CARTESIAN_POINT('Ctrl Pts',(-20.0004586807909,32.938181977325,124.463012680177)) ;
#83389 = CARTESIAN_POINT('Ctrl Pts',(-19.8108772925301,32.9480818099811,124.548917300338)) ;
#83390 = CARTESIAN_POINT('Ctrl Pts',(-19.6075007747243,32.9580742105591,124.601531936566)) ;
#83391 = CARTESIAN_POINT('Ctrl Pts',(-19.3971732333432,32.9681082323185,124.617729269528)) ;
#83392 = CARTESIAN_POINT('Ctrl Pts',(-19.190754436079,32.9779728431597,124.597773976657)) ;
#83393 = CARTESIAN_POINT('Ctrl Pts',(-18.9882033469982,32.9879652426208,124.542054828575)) ;
#83394 = CARTESIAN_POINT('Ctrl Pts',(-18.7978335009767,32.9979971959537,124.451283463694)) ;
#83395 = CARTESIAN_POINT('Ctrl Pts',(-18.6287589942609,33.0078635548954,124.331111742769)) ;
#83396 = CARTESIAN_POINT('Ctrl Pts',(-18.4811111557562,33.0178510303812,124.181860134254)) ;
#83397 = CARTESIAN_POINT('Ctrl Pts',(-18.362006088434,33.0277959365697,124.009992202084)) ;
#83398 = CARTESIAN_POINT('Ctrl Pts',(-18.2738031023012,33.0378409012299,123.818139922867)) ;
#83399 = CARTESIAN_POINT('Ctrl Pts',(-18.221036924655,33.0477027081348,123.617622978503)) ;
#83400 = CARTESIAN_POINT('Ctrl Pts',(-18.2032624857334,33.0576953804405,123.408320496302)) ;
#83401 = CARTESIAN_POINT('Ctrl Pts',(-18.2220069147815,33.0676240513859,123.200418237419)) ;
#83402 = CARTESIAN_POINT('Ctrl Pts',(-18.276358079909,33.0775765936112,122.998381929429)) ;
#83403 = CARTESIAN_POINT('Ctrl Pts',(-18.3653128439867,33.0875779496071,122.807841826037)) ;
#83404 = CARTESIAN_POINT('Ctrl Pts',(-18.486547387057,33.0976065618818,122.635363535432)) ;
#83405 = CARTESIAN_POINT('Ctrl Pts',(-18.6332437344153,33.1074708964313,122.488761354518)) ;
#83406 = CARTESIAN_POINT('Ctrl Pts',(-18.8051496261247,33.1174632205079,122.368071521827)) ;
#83407 = CARTESIAN_POINT('Ctrl Pts',(-18.9941648077372,33.1273907128737,122.279502904876)) ;
#83408 = CARTESIAN_POINT('Ctrl Pts',(-19.1976621955604,33.1374180714246,122.224574414037)) ;
#83409 = CARTESIAN_POINT('Ctrl Pts',(-19.4046917063012,33.1473044894757,122.205852145858)) ;
#83410 = CARTESIAN_POINT('Ctrl Pts',(-19.6148150213246,33.1573362242111,122.22350700037)) ;
#83411 = CARTESIAN_POINT('Ctrl Pts',(-19.8157514821659,33.1672178054543,122.276392579727)) ;
#83412 = CARTESIAN_POINT('Ctrl Pts',(-20.0078549838356,33.1772797834867,122.364875755103)) ;
#83413 = CARTESIAN_POINT('Ctrl Pts',(-20.1782306268323,33.1871368618484,122.482889582793)) ;
#83414 = CARTESIAN_POINT('Ctrl Pts',(-20.3278335578549,33.1971314349544,122.630382150663)) ;
#83415 = CARTESIAN_POINT('Ctrl Pts',(-20.4488150867353,33.207057231242,122.800439196544)) ;
#83416 = CARTESIAN_POINT('Ctrl Pts',(-20.5393606634792,33.2170825984117,122.99074466967)) ;
#83417 = CARTESIAN_POINT('Ctrl Pts',(-20.5948558871472,33.2269786780656,123.191261925233)) ;
#83418 = CARTESIAN_POINT('Ctrl Pts',(-20.6153122230026,33.2369737577711,123.400394982972)) ;
#83419 = CARTESIAN_POINT('Ctrl Pts',(-20.5987384029199,33.246998845587,123.610498671386)) ;
#83420 = CARTESIAN_POINT('Ctrl Pts',(-20.5297765324198,33.2601826679542,123.878959486108)) ;
#83421 = CARTESIAN_POINT('Ctrl Pts',(-20.3913922331434,33.2735047861002,124.126130635834)) ;
#83422 = CARTESIAN_POINT('Ctrl Pts',(-20.1945244288533,33.2868839957278,124.327020121736)) ;
#83423 = CARTESIAN_POINT('Ctrl Pts',(-20.0266226406426,33.296722232972,124.44783147606)) ;
#83424 = CARTESIAN_POINT('Ctrl Pts',(-19.8359283407029,33.3067951562307,124.539857196587)) ;
#83425 = CARTESIAN_POINT('Ctrl Pts',(-19.6364751988179,33.3166517976858,124.596128291563)) ;
#83426 = CARTESIAN_POINT('Ctrl Pts',(-19.4276788871458,33.3266371731919,124.617742250002)) ;
#83427 = CARTESIAN_POINT('Ctrl Pts',(-19.1491574137072,33.3399212046523,124.597574248406)) ;
#83428 = CARTESIAN_POINT('Ctrl Pts',(-18.8168324643961,33.3564399965226,124.483616296897)) ;
#83429 = CARTESIAN_POINT('Ctrl Pts',(-18.5395293026587,33.3732257135293,124.258981067428)) ;
#83430 = CARTESIAN_POINT('Ctrl Pts',(-18.3774838638889,33.3863388620383,124.035935686859)) ;
#83431 = CARTESIAN_POINT('Ctrl Pts',(-18.2842424548978,33.3963744111184,123.846700489471)) ;
#83432 = CARTESIAN_POINT('Ctrl Pts',(-18.2259657627014,33.4063904672979,123.644335418821)) ;
#83433 = CARTESIAN_POINT('Ctrl Pts',(-18.1960980312473,33.4195685031639,123.368929020654)) ;
#83434 = CARTESIAN_POINT('Ctrl Pts',(-18.2490090481057,33.436170380351,123.019870932776)) ;
#83435 = CARTESIAN_POINT('Ctrl Pts',(-18.4541281933962,33.4562335249669,122.645836797817)) ;
#83436 = CARTESIAN_POINT('Ctrl Pts',(-18.7702598882601,33.4760344150506,122.367699543622)) ;
#83437 = CARTESIAN_POINT('Ctrl Pts',(-19.1646435491626,33.4959775403293,122.212088086197)) ;
#83438 = CARTESIAN_POINT('Ctrl Pts',(-19.5875673811207,33.5158755854489,122.200707738123)) ;
#83439 = CARTESIAN_POINT('Ctrl Pts',(-19.9891371716541,33.5357613450756,122.333269289904)) ;
#83440 = CARTESIAN_POINT('Ctrl Pts',(-20.3238757207542,33.5558265202555,122.597734115346)) ;
#83441 = CARTESIAN_POINT('Ctrl Pts',(-20.5455361210312,33.5756531633583,122.956408577687)) ;
#83442 = CARTESIAN_POINT('Ctrl Pts',(-20.6329532916303,33.5955618728067,123.370482994529)) ;
#83443 = CARTESIAN_POINT('Ctrl Pts',(-20.5737633532293,33.6155137098385,123.79068321241)) ;
#83444 = CARTESIAN_POINT('Ctrl Pts',(-20.3736428975741,33.6355221845416,124.166059601071)) ;
#83445 = CARTESIAN_POINT('Ctrl Pts',(-20.0610026955118,33.6553236433031,124.448078246282)) ;
#83446 = CARTESIAN_POINT('Ctrl Pts',(-19.6682568612891,33.675280531539,124.608739923763)) ;
#83447 = CARTESIAN_POINT('Ctrl Pts',(-19.2436659702764,33.6952643689531,124.624794639191)) ;
#83448 = CARTESIAN_POINT('Ctrl Pts',(-18.8423052598593,33.7150728081741,124.496925818226)) ;
#83449 = CARTESIAN_POINT('Ctrl Pts',(-18.5055647293173,33.7350585175543,124.237926514824)) ;
#83450 = CARTESIAN_POINT('Ctrl Pts',(-18.2784679586642,33.7549280405696,123.881468060406)) ;
#83451 = CARTESIAN_POINT('Ctrl Pts',(-18.1861872054109,33.7749487796868,123.466060026539)) ;
#83452 = CARTESIAN_POINT('Ctrl Pts',(-18.2401103433978,33.7947528446637,123.048276947068)) ;
#83453 = CARTESIAN_POINT('Ctrl Pts',(-18.4356215903281,33.8148148083945,122.66928309307)) ;
#83454 = CARTESIAN_POINT('Ctrl Pts',(-18.7455984770616,33.834647988683,122.383215119623)) ;
#83455 = CARTESIAN_POINT('Ctrl Pts',(-19.1356568043022,33.854567186009,122.21836038993)) ;
#83456 = CARTESIAN_POINT('Ctrl Pts',(-19.5590432936728,33.8745052111223,122.196755239328)) ;
#83457 = CARTESIAN_POINT('Ctrl Pts',(-19.9633828074082,33.8943832571784,122.319991705251)) ;
#83458 = CARTESIAN_POINT('Ctrl Pts',(-20.3031557179913,33.9143679914665,122.575085856202)) ;
#83459 = CARTESIAN_POINT('Ctrl Pts',(-20.534784691646,33.934278808145,122.92960459951)) ;
#83460 = CARTESIAN_POINT('Ctrl Pts',(-20.6316400568924,33.9542777836637,123.343555560692)) ;
#83461 = CARTESIAN_POINT('Ctrl Pts',(-20.58241644095,33.9740827043089,123.761861352156)) ;
#83462 = CARTESIAN_POINT('Ctrl Pts',(-20.392337806412,33.9940666646001,124.141776573077)) ;
#83463 = CARTESIAN_POINT('Ctrl Pts',(-20.0852720969054,34.0139528683241,124.43258612421)) ;
#83464 = CARTESIAN_POINT('Ctrl Pts',(-19.6964740781402,34.0339020466473,124.602080252954)) ;
#83465 = CARTESIAN_POINT('Ctrl Pts',(-19.2741491940426,34.0538038458868,124.628564557594)) ;
#83466 = CARTESIAN_POINT('Ctrl Pts',(-18.8683285859551,34.0736824509392,124.510329663157)) ;
#83467 = CARTESIAN_POINT('Ctrl Pts',(-18.5246879272809,34.0937148106649,124.258609949435)) ;
#83468 = CARTESIAN_POINT('Ctrl Pts',(-18.3288959796527,34.110296536621,123.965412149913)) ;
#83469 = CARTESIAN_POINT('Ctrl Pts',(-18.2390051118599,34.1234907069189,123.702986280917)) ;
#83470 = CARTESIAN_POINT('Ctrl Pts',(-18.195215620379,34.1368028850121,123.426625345839)) ;
#83471 = CARTESIAN_POINT('Ctrl Pts',(-18.2318570276994,34.1533690646054,123.076205474803)) ;
#83472 = CARTESIAN_POINT('Ctrl Pts',(-18.3860722304639,34.1699972594656,122.758154636996)) ;
#83473 = CARTESIAN_POINT('Ctrl Pts',(-18.5689207833389,34.1832858411753,122.546840480982)) ;
#83474 = CARTESIAN_POINT('Ctrl Pts',(-18.7313513303073,34.1932540892789,122.414464338576)) ;
#83475 = CARTESIAN_POINT('Ctrl Pts',(-18.9132140631746,34.2031688455351,122.312607045933)) ;
#83476 = CARTESIAN_POINT('Ctrl Pts',(-19.1118792711937,34.2131819961863,122.242971316891)) ;
#83477 = CARTESIAN_POINT('Ctrl Pts',(-19.3196579103368,34.2231947033883,122.209223879779)) ;
#83478 = CARTESIAN_POINT('Ctrl Pts',(-19.597538352536,34.2364139920796,122.212437336866)) ;
#83479 = CARTESIAN_POINT('Ctrl Pts',(-19.9378288626282,34.2530326730776,122.307523642033)) ;
#83480 = CARTESIAN_POINT('Ctrl Pts',(-20.2246132922364,34.2695975808511,122.512032295996)) ;
#83481 = CARTESIAN_POINT('Ctrl Pts',(-20.4036556912666,34.2829960524619,122.729519755814)) ;
#83482 = CARTESIAN_POINT('Ctrl Pts',(-20.5055966706641,34.2928373079489,122.909568823664)) ;
#83483 = CARTESIAN_POINT('Ctrl Pts',(-20.5761690059698,34.3028236235371,123.107261401867)) ;
#83484 = CARTESIAN_POINT('Ctrl Pts',(-20.6112776484593,34.3127602311235,123.313223850994)) ;
#83485 = CARTESIAN_POINT('Ctrl Pts',(-20.609973583627,34.3228100984918,123.524478235219)) ;
#83486 = CARTESIAN_POINT('Ctrl Pts',(-20.5729077524679,34.3326605931666,123.728238360151)) ;
#83487 = CARTESIAN_POINT('Ctrl Pts',(-20.5006686189369,34.3426323935611,123.925008528361)) ;
#83488 = CARTESIAN_POINT('Ctrl Pts',(-20.3950540866116,34.3526283605869,124.106728445384)) ;
#83489 = CARTESIAN_POINT('Ctrl Pts',(-20.2587448397583,34.3626658199681,124.267788317343)) ;
#83490 = CARTESIAN_POINT('Ctrl Pts',(-20.099944331439,34.3725065208688,124.400411921082)) ;
#83491 = CARTESIAN_POINT('Ctrl Pts',(-19.916925180984,34.3825545421362,124.505877187115)) ;
#83492 = CARTESIAN_POINT('Ctrl Pts',(-19.7202373549352,34.3925019352189,124.576929496361)) ;
#83493 = CARTESIAN_POINT('Ctrl Pts',(-19.5150731826552,34.4024120812653,124.613246050668)) ;
#83494 = CARTESIAN_POINT('Ctrl Pts',(-19.3036249159796,34.4124709951149,124.613150609061)) ;
#83495 = CARTESIAN_POINT('Ctrl Pts',(-19.0998219309053,34.4223117654042,124.577418246397)) ;
#83496 = CARTESIAN_POINT('Ctrl Pts',(-18.9008963305154,34.4323746349828,124.505500646163)) ;
#83497 = CARTESIAN_POINT('Ctrl Pts',(-18.7205944587309,34.4422689581133,124.401729144062)) ;
#83498 = CARTESIAN_POINT('Ctrl Pts',(-18.5599579928676,34.4522107652078,124.268052326554)) ;
#83499 = CARTESIAN_POINT('Ctrl Pts',(-18.4240523663219,34.4622132761631,124.107549499809)) ;
#83500 = CARTESIAN_POINT('Ctrl Pts',(-18.3180449884681,34.4722479969815,123.925171280476)) ;
#83501 = CARTESIAN_POINT('Ctrl Pts',(-18.2463591450484,34.4820931744872,123.73099253113)) ;
#83502 = CARTESIAN_POINT('Ctrl Pts',(-18.2085560221446,34.4920779348883,123.524543622521)) ;
#83503 = CARTESIAN_POINT('Ctrl Pts',(-18.2070790887704,34.5020168412047,123.315570311663)) ;
#83504 = CARTESIAN_POINT('Ctrl Pts',(-18.2423345282347,34.5120590688404,123.107437291874)) ;
#83505 = CARTESIAN_POINT('Ctrl Pts',(-18.3119591424953,34.5219442804248,122.911604455747)) ;
#83506 = CARTESIAN_POINT('Ctrl Pts',(-18.4154468238259,34.5319432106267,122.728669490148)) ;
#83507 = CARTESIAN_POINT('Ctrl Pts',(-18.5479551281842,34.5418606335371,122.567652774081)) ;
#83508 = CARTESIAN_POINT('Ctrl Pts',(-18.7084701842232,34.5519085656159,122.430380022431)) ;
#83509 = CARTESIAN_POINT('Ctrl Pts',(-18.8872472231273,34.5617859414253,122.324675785033)) ;
#83510 = CARTESIAN_POINT('Ctrl Pts',(-19.0850314861629,34.5718398345932,122.250237672887)) ;
#83511 = CARTESIAN_POINT('Ctrl Pts',(-19.2894839508418,34.5817334578465,122.211783907264)) ;
#83512 = CARTESIAN_POINT('Ctrl Pts',(-19.5009836238309,34.5917960514695,122.20934143813)) ;
#83513 = CARTESIAN_POINT('Ctrl Pts',(-19.7052052787397,34.6016386254585,122.242811571831)) ;
#83514 = CARTESIAN_POINT('Ctrl Pts',(-19.9035702129768,34.6116293823415,122.311773012743)) ;
#83515 = CARTESIAN_POINT('Ctrl Pts',(-20.0858114401487,34.6215574440994,122.413537172417)) ;
#83516 = CARTESIAN_POINT('Ctrl Pts',(-20.2488208163427,34.6315454199886,122.545909746572)) ;
#83517 = CARTESIAN_POINT('Ctrl Pts',(-20.3867503190561,34.641581084345,122.705552977548)) ;
#83518 = CARTESIAN_POINT('Ctrl Pts',(-20.4932169413994,34.6514370227647,122.883323165584)) ;
#83519 = CARTESIAN_POINT('Ctrl Pts',(-20.5685573101781,34.6614325141616,123.079465842186)) ;
#83520 = CARTESIAN_POINT('Ctrl Pts',(-20.6084203324499,34.671342319115,123.283961991978)) ;
#83521 = CARTESIAN_POINT('Ctrl Pts',(-20.612551190647,34.6813545413818,123.494414786544)) ;
#83522 = CARTESIAN_POINT('Ctrl Pts',(-20.5796204241671,34.6913824220746,123.70264640733)) ;
#83523 = CARTESIAN_POINT('Ctrl Pts',(-20.5125423139285,34.7012388180572,123.898699508043)) ;
#83524 = CARTESIAN_POINT('Ctrl Pts',(-20.4111153015867,34.7112636152372,124.083444109091)) ;
#83525 = CARTESIAN_POINT('Ctrl Pts',(-20.2786642763012,34.721294545221,124.247549925688)) ;
#83526 = CARTESIAN_POINT('Ctrl Pts',(-20.1229410884498,34.7311391477296,124.383860215577)) ;
#83527 = CARTESIAN_POINT('Ctrl Pts',(-19.9435694586071,34.7411299989537,124.493149983065)) ;
#83528 = CARTESIAN_POINT('Ctrl Pts',(-19.746860411412,34.751167831965,124.5695515535)) ;
#83529 = CARTESIAN_POINT('Ctrl Pts',(-19.543924430635,34.7610122204304,124.610202433286)) ;
#83530 = CARTESIAN_POINT('Ctrl Pts',(-19.3341067512897,34.7709970248,124.61548205464)) ;
#83531 = CARTESIAN_POINT('Ctrl Pts',(-19.1274314289972,34.7809365442828,124.58447308467)) ;
#83532 = CARTESIAN_POINT('Ctrl Pts',(-18.9273406268735,34.7909762752842,124.517347067221)) ;
#83533 = CARTESIAN_POINT('Ctrl Pts',(-18.7446690785949,34.8008644035305,124.418099723713)) ;
#83534 = CARTESIAN_POINT('Ctrl Pts',(-18.5801062236572,34.810854128739,124.287630585747)) ;
#83535 = CARTESIAN_POINT('Ctrl Pts',(-18.4412525822457,34.8208118934405,124.130968222616)) ;
#83536 = CARTESIAN_POINT('Ctrl Pts',(-18.3318983026168,34.8307142348525,123.953816542597)) ;
#83537 = CARTESIAN_POINT('Ctrl Pts',(-18.2538875050456,34.8407584305589,123.757605403826)) ;
#83538 = CARTESIAN_POINT('Ctrl Pts',(-18.2116860598952,34.8506658313181,123.553629678819)) ;
#83539 = CARTESIAN_POINT('Ctrl Pts',(-18.2051086185152,34.8606764311925,123.343275057012)) ;
#83540 = CARTESIAN_POINT('Ctrl Pts',(-18.2356186127828,34.8707067271047,123.134619193214)) ;
#83541 = CARTESIAN_POINT('Ctrl Pts',(-18.3004560794895,34.8805615067544,122.937861249696)) ;
#83542 = CARTESIAN_POINT('Ctrl Pts',(-18.3989387378507,34.8905188349719,122.753132034152)) ;
#83543 = CARTESIAN_POINT('Ctrl Pts',(-18.5293404007521,34.9005578678788,122.587203276214)) ;
#83544 = CARTESIAN_POINT('Ctrl Pts',(-18.683750583713,34.9104309797681,122.448444456777)) ;
#83545 = CARTESIAN_POINT('Ctrl Pts',(-18.8634484884761,34.9205042647952,122.336472021751)) ;
#83546 = CARTESIAN_POINT('Ctrl Pts',(-19.0549066208828,34.9303245845319,122.259103627693)) ;
#83547 = CARTESIAN_POINT('Ctrl Pts',(-19.2620674122068,34.9404032499104,122.214853274735)) ;
#83548 = CARTESIAN_POINT('Ctrl Pts',(-19.4690914445195,34.9502548403942,122.20734023343)) ;
#83549 = CARTESIAN_POINT('Ctrl Pts',(-19.678827834024,34.9603279907131,122.236334586812)) ;
#83550 = CARTESIAN_POINT('Ctrl Pts',(-19.8757733045073,34.9701703706881,122.299862342837)) ;
#83551 = CARTESIAN_POINT('Ctrl Pts',(-20.0615624802536,34.9801513469312,122.397356517618)) ;
#83552 = CARTESIAN_POINT('Ctrl Pts',(-20.2279932750896,34.9901676752865,122.526380482302)) ;
#83553 = CARTESIAN_POINT('Ctrl Pts',(-20.3680015083541,35.0000654722776,122.680305185456)) ;
#83554 = CARTESIAN_POINT('Ctrl Pts',(-20.4807624809088,35.0100780290097,122.858068616556)) ;
#83555 = CARTESIAN_POINT('Ctrl Pts',(-20.5606293993348,35.0201100638562,123.053255739191)) ;
#83556 = CARTESIAN_POINT('Ctrl Pts',(-20.6050415900168,35.0299494646716,123.255303485779)) ;
#83557 = CARTESIAN_POINT('Ctrl Pts',(-20.6140547299555,35.0400152503232,123.466701668536)) ;
#83558 = CARTESIAN_POINT('Ctrl Pts',(-20.5866072578228,35.0499057054378,123.672832352002)) ;
#83559 = CARTESIAN_POINT('Ctrl Pts',(-20.5235800737394,35.0598978240735,123.873208904789)) ;
#83560 = CARTESIAN_POINT('Ctrl Pts',(-20.4268258300591,35.0698606508366,124.058965811028)) ;
#83561 = CARTESIAN_POINT('Ctrl Pts',(-20.3004423219117,35.0797649341095,124.224463820885)) ;
#83562 = CARTESIAN_POINT('Ctrl Pts',(-20.1447351796746,35.0898253680566,124.367564128807)) ;
#83563 = CARTESIAN_POINT('Ctrl Pts',(-19.9705404840006,35.0996659207298,124.479217042603)) ;
#83564 = CARTESIAN_POINT('Ctrl Pts',(-19.775454299902,35.1097281406755,124.560953485022)) ;
#83565 = CARTESIAN_POINT('Ctrl Pts',(-19.5724444891805,35.119625279954,124.606605440931)) ;
#83566 = CARTESIAN_POINT('Ctrl Pts',(-19.3639245804483,35.1295564720891,124.617042217637)) ;
#83567 = CARTESIAN_POINT('Ctrl Pts',(-19.1544758293092,35.1395986267342,124.590591188997)) ;
#83568 = CARTESIAN_POINT('Ctrl Pts',(-18.9558504881667,35.1494853877535,124.52929739217)) ;
#83569 = CARTESIAN_POINT('Ctrl Pts',(-18.7686967842373,35.1594846894707,124.433626676918)) ;
#83570 = CARTESIAN_POINT('Ctrl Pts',(-18.6021840039089,35.1694054876375,124.307986902434)) ;
#83571 = CARTESIAN_POINT('Ctrl Pts',(-18.4584119398437,35.1794395412342,124.153654272285)) ;
#83572 = CARTESIAN_POINT('Ctrl Pts',(-18.3447544017699,35.1893626588006,123.978681426512)) ;
#83573 = CARTESIAN_POINT('Ctrl Pts',(-18.2621745123595,35.1994187822997,123.784088489185)) ;
#83574 = CARTESIAN_POINT('Ctrl Pts',(-18.2155383684478,35.2092642239545,123.582420316723)) ;
#83575 = CARTESIAN_POINT('Ctrl Pts',(-18.2038107386585,35.2192265250787,123.373323341411)) ;
#83576 = CARTESIAN_POINT('Ctrl Pts',(-18.2290111975994,35.2292550043538,123.16399026275)) ;
#83577 = CARTESIAN_POINT('Ctrl Pts',(-18.2893801566425,35.2391653578635,122.964592181347)) ;
#83578 = CARTESIAN_POINT('Ctrl Pts',(-18.3832066496104,35.2491002300407,122.777983945553)) ;
#83579 = CARTESIAN_POINT('Ctrl Pts',(-18.5094937587254,35.2591413676264,122.608837914047)) ;
#83580 = CARTESIAN_POINT('Ctrl Pts',(-18.6607872589449,35.2690285168409,122.46628852353)) ;
#83581 = CARTESIAN_POINT('Ctrl Pts',(-18.8361660023692,35.279020751592,122.350681667072)) ;
#83582 = CARTESIAN_POINT('Ctrl Pts',(-19.0281614512113,35.288969457155,122.267692165554)) ;
#83583 = CARTESIAN_POINT('Ctrl Pts',(-19.2312959711642,35.2989055255787,122.219071218612)) ;
#83584 = CARTESIAN_POINT('Ctrl Pts',(-19.4408495262732,35.3088912097945,122.206154757803)) ;
#83585 = CARTESIAN_POINT('Ctrl Pts',(-19.6505366990128,35.3189316363631,122.230278771778)) ;
#83586 = CARTESIAN_POINT('Ctrl Pts',(-19.8489056511922,35.3287707498269,122.288911025244)) ;
#83587 = CARTESIAN_POINT('Ctrl Pts',(-20.0378790782979,35.3388004840027,122.382455871339)) ;
#83588 = CARTESIAN_POINT('Ctrl Pts',(-20.2072811529409,35.3488225835086,122.507735654977)) ;
#83589 = CARTESIAN_POINT('Ctrl Pts',(-20.3505219702096,35.358691023402,122.657836946013)) ;
#83590 = CARTESIAN_POINT('Ctrl Pts',(-20.4678365484085,35.3687598880876,122.83401133288)) ;
#83591 = CARTESIAN_POINT('Ctrl Pts',(-20.5508879121588,35.3786025611862,123.023544397002)) ;
#83592 = CARTESIAN_POINT('Ctrl Pts',(-20.6010962703193,35.3885631953487,123.226835535581)) ;
#83593 = CARTESIAN_POINT('Ctrl Pts',(-20.6149388902107,35.3986011110268,123.437402313412)) ;
#83594 = CARTESIAN_POINT('Ctrl Pts',(-20.5927617522168,35.4084753858862,123.643828081637)) ;
#83595 = CARTESIAN_POINT('Ctrl Pts',(-20.5339407377704,35.4185451362614,123.847160643849)) ;
#83596 = CARTESIAN_POINT('Ctrl Pts',(-20.4429777575099,35.4283784316359,124.03281763608)) ;
#83597 = CARTESIAN_POINT('Ctrl Pts',(-20.3192176499442,35.4384087291155,124.203541031282)) ;
#83598 = CARTESIAN_POINT('Ctrl Pts',(-20.16722456801,35.4484408155569,124.349771846987)) ;
#83599 = CARTESIAN_POINT('Ctrl Pts',(-19.9959822051023,35.4582687440459,124.465363734723)) ;
#83600 = CARTESIAN_POINT('Ctrl Pts',(-19.8042655640966,35.4682647851566,124.551422946889)) ;
#83601 = CARTESIAN_POINT('Ctrl Pts',(-19.5998043217573,35.4782905972579,124.602646565029)) ;
#83602 = CARTESIAN_POINT('Ctrl Pts',(-19.392483122797,35.4881778321527,124.617652844569)) ;
#83603 = CARTESIAN_POINT('Ctrl Pts',(-19.1838143097851,35.4981546983637,124.596588858927)) ;
#83604 = CARTESIAN_POINT('Ctrl Pts',(-18.9815944245208,35.5081476422355,124.539544119741)) ;
#83605 = CARTESIAN_POINT('Ctrl Pts',(-18.7916564256267,35.5181855649069,124.447621093285)) ;
#83606 = CARTESIAN_POINT('Ctrl Pts',(-18.623585679529,35.5280340291686,124.326680948825)) ;
#83607 = CARTESIAN_POINT('Ctrl Pts',(-18.4767269345962,35.5380258959126,124.176530851777)) ;
#83608 = CARTESIAN_POINT('Ctrl Pts',(-18.3589196028122,35.5479436279538,124.004467615478)) ;
#83609 = CARTESIAN_POINT('Ctrl Pts',(-18.2717855237114,35.557971812849,123.812511474511)) ;
#83610 = CARTESIAN_POINT('Ctrl Pts',(-18.2199640326758,35.5678569708979,123.611253900228)) ;
#83611 = CARTESIAN_POINT('Ctrl Pts',(-18.2031956371269,35.5778463314396,123.401912404642)) ;
#83612 = CARTESIAN_POINT('Ctrl Pts',(-18.2235772732531,35.5878874883739,123.19180201946)) ;
#83613 = CARTESIAN_POINT('Ctrl Pts',(-18.2786256492768,35.5977200718291,122.992558401148)) ;
#83614 = CARTESIAN_POINT('Ctrl Pts',(-18.368354397371,35.6077142917911,122.802574694399)) ;
#83615 = CARTESIAN_POINT('Ctrl Pts',(-18.4904752636947,35.6177423935784,122.630717576888)) ;
#83616 = CARTESIAN_POINT('Ctrl Pts',(-18.6381538687161,35.6276223382014,122.484653315381)) ;
#83617 = CARTESIAN_POINT('Ctrl Pts',(-18.8106615035911,35.6376126647585,122.364871615126)) ;
#83618 = CARTESIAN_POINT('Ctrl Pts',(-19.0004190126746,35.6475535964128,122.277289203109)) ;
#83619 = CARTESIAN_POINT('Ctrl Pts',(-19.203373565365,35.6575407149157,122.223445031076)) ;
#83620 = CARTESIAN_POINT('Ctrl Pts',(-19.4135608775624,35.6675740478129,122.205909966889)) ;
#83621 = CARTESIAN_POINT('Ctrl Pts',(-19.6201740270743,35.6774401522576,122.224414930449)) ;
#83622 = CARTESIAN_POINT('Ctrl Pts',(-19.8244618404045,35.6875062661379,122.279549955093)) ;
#83623 = CARTESIAN_POINT('Ctrl Pts',(-20.0121134212357,35.6973622779064,122.367450472132)) ;
#83624 = CARTESIAN_POINT('Ctrl Pts',(-20.1843772744917,35.7073569815377,122.487755292346)) ;
#83625 = CARTESIAN_POINT('Ctrl Pts',(-20.3333683513366,35.7173883172625,122.637013317977)) ;
#83626 = CARTESIAN_POINT('Ctrl Pts',(-20.4524676775641,35.7272548424662,122.806847353514)) ;
#83627 = CARTESIAN_POINT('Ctrl Pts',(-20.5416380597562,35.737242270512,122.996911535405)) ;
#83628 = CARTESIAN_POINT('Ctrl Pts',(-20.5963428018029,35.7471872001984,123.198733454628)) ;
#83629 = CARTESIAN_POINT('Ctrl Pts',(-20.6152390420274,35.7572321183069,123.409042028494)) ;
#83630 = CARTESIAN_POINT('Ctrl Pts',(-20.5978399960011,35.7670940879208,123.615657169133)) ;
#83631 = CARTESIAN_POINT('Ctrl Pts',(-20.5445360900848,35.7770861559421,123.818824883138)) ;
#83632 = CARTESIAN_POINT('Ctrl Pts',(-20.4572545323624,35.7870170813166,124.008498783823)) ;
#83633 = CARTESIAN_POINT('Ctrl Pts',(-20.3384335820411,35.7969677095401,124.180653507785)) ;
#83634 = CARTESIAN_POINT('Ctrl Pts',(-20.1908529728622,35.8069679485992,124.330416617571)) ;
#83635 = CARTESIAN_POINT('Ctrl Pts',(-20.0188759857956,35.8169964039684,124.452357630872)) ;
#83636 = CARTESIAN_POINT('Ctrl Pts',(-19.8315424729774,35.8268624385517,124.541414625509)) ;
#83637 = CARTESIAN_POINT('Ctrl Pts',(-19.6291530298496,35.8368547602991,124.597623082846)) ;
#83638 = CARTESIAN_POINT('Ctrl Pts',(-19.4213005157174,35.8467870499761,124.61775207134)) ;
#83639 = CARTESIAN_POINT('Ctrl Pts',(-19.211666492633,35.8567886949468,124.601579008395)) ;
#83640 = CARTESIAN_POINT('Ctrl Pts',(-18.9405973697482,35.8701013283629,124.531802097679)) ;
#83641 = CARTESIAN_POINT('Ctrl Pts',(-18.6953541163112,35.8833330777444,124.393908284791)) ;
#83642 = CARTESIAN_POINT('Ctrl Pts',(-18.4950059200478,35.8966563425615,124.19822486619)) ;
#83643 = CARTESIAN_POINT('Ctrl Pts',(-18.3736554135811,35.9065320487792,124.029742314884)) ;
#83644 = CARTESIAN_POINT('Ctrl Pts',(-18.2821355538352,35.9165216398792,123.840747272205)) ;
#83645 = CARTESIAN_POINT('Ctrl Pts',(-18.2250326647968,35.9264487363346,123.639986046386)) ;
#83646 = CARTESIAN_POINT('Ctrl Pts',(-18.2034246484447,35.9364738848392,123.430355376024)) ;
#83647 = CARTESIAN_POINT('Ctrl Pts',(-18.218222177825,35.9463695389859,123.222826192878)) ;
#83648 = CARTESIAN_POINT('Ctrl Pts',(-18.2690819771899,35.9563730733641,123.018783675102)) ;
#83649 = CARTESIAN_POINT('Ctrl Pts',(-18.3544809763552,35.9663582118041,122.826985698645)) ;
#83650 = CARTESIAN_POINT('Ctrl Pts',(-18.4726337060775,35.9763941363995,122.652198310176)) ;
#83651 = CARTESIAN_POINT('Ctrl Pts',(-18.6164712051897,35.9862454118272,122.503192825929)) ;
#83652 = CARTESIAN_POINT('Ctrl Pts',(-18.7860469770092,35.9962376729885,122.379193148442)) ;
#83653 = CARTESIAN_POINT('Ctrl Pts',(-18.9756946417762,36.0062775570061,122.286567052607)) ;
#83654 = CARTESIAN_POINT('Ctrl Pts',(-19.1742898211919,36.0161123315086,122.228953645098)) ;
#83655 = CARTESIAN_POINT('Ctrl Pts',(-19.3848548302103,36.0261887125289,122.206080564844)) ;
#83656 = CARTESIAN_POINT('Ctrl Pts',(-19.5914291862838,36.0360349856795,122.219742059449)) ;
#83657 = CARTESIAN_POINT('Ctrl Pts',(-19.8644347267717,36.0493995069647,122.286166574249)) ;
#83658 = CARTESIAN_POINT('Ctrl Pts',(-20.1107389390427,36.0626057513992,122.421071137189)) ;
#83659 = CARTESIAN_POINT('Ctrl Pts',(-20.3128956661837,36.0758707060764,122.613085888176)) ;
#83660 = CARTESIAN_POINT('Ctrl Pts',(-20.4382108216345,36.0859029866281,122.782748260018)) ;
#83661 = CARTESIAN_POINT('Ctrl Pts',(-20.5310088524388,36.095811720146,122.969242493688)) ;
#83662 = CARTESIAN_POINT('Ctrl Pts',(-20.5907141654176,36.1057492710135,123.169457023205)) ;
#83663 = CARTESIAN_POINT('Ctrl Pts',(-20.6147942216351,36.1157791186074,123.378913624605)) ;
#83664 = CARTESIAN_POINT('Ctrl Pts',(-20.5984716755817,36.1290142585278,123.656761647636)) ;
#83665 = CARTESIAN_POINT('Ctrl Pts',(-20.4868793174588,36.145682722899,123.993019408595)) ;
#83666 = CARTESIAN_POINT('Ctrl Pts',(-20.225147237261,36.1655537347729,124.324870584311)) ;
#83667 = CARTESIAN_POINT('Ctrl Pts',(-19.9231598859888,36.1822608191559,124.511857502732)) ;
#83668 = CARTESIAN_POINT('Ctrl Pts',(-19.6579098007615,36.1954381004665,124.59178022723)) ;
#83669 = CARTESIAN_POINT('Ctrl Pts',(-19.3810457926493,36.2087055609806,124.625650251506)) ;
#83670 = CARTESIAN_POINT('Ctrl Pts',(-19.031245809974,36.2253194516678,124.576426839473)) ;
#83671 = CARTESIAN_POINT('Ctrl Pts',(-18.656546623084,36.2452682510952,124.377542791956)) ;
#83672 = CARTESIAN_POINT('Ctrl Pts',(-18.3727286129065,36.265189362626,124.063195119709)) ;
#83673 = CARTESIAN_POINT('Ctrl Pts',(-18.2127928763886,36.2850558107989,123.672157333383)) ;
#83674 = CARTESIAN_POINT('Ctrl Pts',(-18.1960230951589,36.305082157416,123.246720338443)) ;
#83675 = CARTESIAN_POINT('Ctrl Pts',(-18.3244917453936,36.3249442018056,122.844336519412)) ;
#83676 = CARTESIAN_POINT('Ctrl Pts',(-18.5830321625222,36.3448895044867,122.508241908739)) ;
#83677 = CARTESIAN_POINT('Ctrl Pts',(-18.9399427386742,36.3647848115456,122.281138173914)) ;
#83678 = CARTESIAN_POINT('Ctrl Pts',(-19.3527183542738,36.3846780817132,122.188728150166)) ;
#83679 = CARTESIAN_POINT('Ctrl Pts',(-19.7737310767519,36.4046436743936,122.243004278236)) ;
#83680 = CARTESIAN_POINT('Ctrl Pts',(-20.1494256309747,36.4245189980784,122.436570970355)) ;
#83681 = CARTESIAN_POINT('Ctrl Pts',(-20.4382669875534,36.4444940606534,122.747982616058)) ;
#83682 = CARTESIAN_POINT('Ctrl Pts',(-20.6027131203733,36.4644464702845,123.139055928244)) ;
#83683 = CARTESIAN_POINT('Ctrl Pts',(-20.6245287326153,36.4842825245207,123.560259041129)) ;
#83684 = CARTESIAN_POINT('Ctrl Pts',(-20.5008694423809,36.5042604359382,123.966645206898)) ;
#83685 = CARTESIAN_POINT('Ctrl Pts',(-20.2463345705319,36.5241784854417,124.305097676142)) ;
#83686 = CARTESIAN_POINT('Ctrl Pts',(-19.8929822057688,36.5440466292098,124.536788634087)) ;
#83687 = CARTESIAN_POINT('Ctrl Pts',(-19.4780342144417,36.5640974857971,124.63420462861)) ;
#83688 = CARTESIAN_POINT('Ctrl Pts',(-19.0601853486315,36.583877922253,124.585267888838)) ;
#83689 = CARTESIAN_POINT('Ctrl Pts',(-18.679261467487,36.6039079779308,124.395005365554)) ;
#83690 = CARTESIAN_POINT('Ctrl Pts',(-18.3887179656958,36.6237890831056,124.087851983068)) ;
#83691 = CARTESIAN_POINT('Ctrl Pts',(-18.2193877468624,36.6436695454733,123.700582763927)) ;
#83692 = CARTESIAN_POINT('Ctrl Pts',(-18.19234690507,36.6636546926177,123.276492035899)) ;
#83693 = CARTESIAN_POINT('Ctrl Pts',(-18.3111820310243,36.6835452711541,122.870593167855)) ;
#83694 = CARTESIAN_POINT('Ctrl Pts',(-18.5608264774921,36.7034392910285,122.52912278026)) ;
#83695 = CARTESIAN_POINT('Ctrl Pts',(-18.9123819271041,36.7233607357549,122.292957389509)) ;
#83696 = CARTESIAN_POINT('Ctrl Pts',(-19.3229430451525,36.7432588738103,122.190279959009)) ;
#83697 = CARTESIAN_POINT('Ctrl Pts',(-19.7472711559483,36.7633296290264,122.23504109074)) ;
#83698 = CARTESIAN_POINT('Ctrl Pts',(-20.1256424620349,36.7831151790776,122.419154427526)) ;
#83699 = CARTESIAN_POINT('Ctrl Pts',(-20.4220170617102,36.803098253955,122.723507791332)) ;
#83700 = CARTESIAN_POINT('Ctrl Pts',(-20.5955264961768,36.8230073366009,123.109641754048)) ;
#83701 = CARTESIAN_POINT('Ctrl Pts',(-20.6279926914676,36.8428658957237,123.530692354676)) ;
#83702 = CARTESIAN_POINT('Ctrl Pts',(-20.5133249107813,36.8629093395624,123.941072173113)) ;
#83703 = CARTESIAN_POINT('Ctrl Pts',(-20.3093891442203,36.8794094042916,124.226640227204)) ;
#83704 = CARTESIAN_POINT('Ctrl Pts',(-20.0922744150235,36.8927991441405,124.405775148074)) ;
#83705 = CARTESIAN_POINT('Ctrl Pts',(-19.9119759265063,36.9026560453489,124.507969785609)) ;
#83706 = CARTESIAN_POINT('Ctrl Pts',(-19.7142026391897,36.9126475711954,124.578640987021)) ;
#83707 = CARTESIAN_POINT('Ctrl Pts',(-19.5084997100281,36.9225722516463,124.613748997365)) ;
#83708 = CARTESIAN_POINT('Ctrl Pts',(-19.2980712246021,36.9325828416907,124.612675113319)) ;
#83709 = CARTESIAN_POINT('Ctrl Pts',(-19.0237190251931,36.9458421023944,124.563191736342)) ;
#83710 = CARTESIAN_POINT('Ctrl Pts',(-18.767004640469,36.9591931775447,124.442157944638)) ;
#83711 = CARTESIAN_POINT('Ctrl Pts',(-18.554897868614,36.9723994867795,124.262901619475)) ;
#83712 = CARTESIAN_POINT('Ctrl Pts',(-18.4202072573084,36.9823863203698,124.101894877221)) ;
#83713 = CARTESIAN_POINT('Ctrl Pts',(-18.3157478310431,36.9923390478658,123.920555058414)) ;
#83714 = CARTESIAN_POINT('Ctrl Pts',(-18.2438653347165,37.0023871447074,123.721943582903)) ;
#83715 = CARTESIAN_POINT('Ctrl Pts',(-18.2080589055082,37.0122286015793,123.518146563826)) ;
#83716 = CARTESIAN_POINT('Ctrl Pts',(-18.2077355256996,37.0222148684928,123.308238341924)) ;
#83717 = CARTESIAN_POINT('Ctrl Pts',(-18.2435931027669,37.0321514693932,123.102404826661)) ;
#83718 = CARTESIAN_POINT('Ctrl Pts',(-18.3155367162439,37.0422014121802,122.903771955819)) ;
#83719 = CARTESIAN_POINT('Ctrl Pts',(-18.4186658037517,37.052051611866,122.724179687361)) ;
#83720 = CARTESIAN_POINT('Ctrl Pts',(-18.5526159351476,37.0620245167981,122.562916724889)) ;
#83721 = CARTESIAN_POINT('Ctrl Pts',(-18.7130217569356,37.0720228912777,122.427035007619)) ;
#83722 = CARTESIAN_POINT('Ctrl Pts',(-18.8950290315818,37.0820430651477,122.320985383453)) ;
#83723 = CARTESIAN_POINT('Ctrl Pts',(-19.0902841551798,37.0919441090897,122.248841936887)) ;
#83724 = CARTESIAN_POINT('Ctrl Pts',(-19.296849422935,37.101932912814,122.211043584546)) ;
#83725 = CARTESIAN_POINT('Ctrl Pts',(-19.5063417583613,37.1118983796458,122.209838368908)) ;
#83726 = CARTESIAN_POINT('Ctrl Pts',(-19.7116920048539,37.1218019419188,122.244315913118)) ;
#83727 = CARTESIAN_POINT('Ctrl Pts',(-19.9109467756604,37.1318626197968,122.315177850177)) ;
#83728 = CARTESIAN_POINT('Ctrl Pts',(-20.0910226055792,37.1417029177462,122.417070024375)) ;
#83729 = CARTESIAN_POINT('Ctrl Pts',(-20.2544023733536,37.1517659126557,122.551425194411)) ;
#83730 = CARTESIAN_POINT('Ctrl Pts',(-20.3895668547775,37.1616602068028,122.709563454073)) ;
#83731 = CARTESIAN_POINT('Ctrl Pts',(-20.496191309324,37.1716020044997,122.889298737266)) ;
#83732 = CARTESIAN_POINT('Ctrl Pts',(-20.5705305806763,37.1816045820288,123.086035719177)) ;
#83733 = CARTESIAN_POINT('Ctrl Pts',(-20.6093785758496,37.1916390459499,123.293373240593)) ;
#83734 = CARTESIAN_POINT('Ctrl Pts',(-20.6119178344459,37.2014851844709,123.500360820734)) ;
#83735 = CARTESIAN_POINT('Ctrl Pts',(-20.5784854248412,37.2114663577079,123.707499064364)) ;
#83736 = CARTESIAN_POINT('Ctrl Pts',(-20.5097396929773,37.2214186516652,123.905117967548)) ;
#83737 = CARTESIAN_POINT('Ctrl Pts',(-20.4074820202486,37.2314174467998,124.088793919153)) ;
#83738 = CARTESIAN_POINT('Ctrl Pts',(-20.2740542843056,37.2414565550606,124.252304030072)) ;
#83739 = CARTESIAN_POINT('Ctrl Pts',(-20.1179432203303,37.2512814964997,124.387573712776)) ;
#83740 = CARTESIAN_POINT('Ctrl Pts',(-19.9367725786366,37.2613361835741,124.496449030684)) ;
#83741 = CARTESIAN_POINT('Ctrl Pts',(-19.7414996689974,37.2712789885143,124.571043200501)) ;
#83742 = CARTESIAN_POINT('Ctrl Pts',(-19.5371698877541,37.2811827745108,124.611070181106)) ;
#83743 = CARTESIAN_POINT('Ctrl Pts',(-19.3260077883793,37.2912295910756,124.61493909619)) ;
#83744 = CARTESIAN_POINT('Ctrl Pts',(-19.1204430941798,37.3011251105543,124.582756712364)) ;
#83745 = CARTESIAN_POINT('Ctrl Pts',(-18.9203358363099,37.3111871958787,124.514257554786)) ;
#83746 = CARTESIAN_POINT('Ctrl Pts',(-18.7390960612812,37.3210299068366,124.41436004309)) ;
#83747 = CARTESIAN_POINT('Ctrl Pts',(-18.5752583699515,37.3310206241427,124.282977391372)) ;
#83748 = CARTESIAN_POINT('Ctrl Pts',(-18.4375935777154,37.3409487072392,124.126081569931)) ;
#83749 = CARTESIAN_POINT('Ctrl Pts',(-18.3282968872261,37.350936637351,123.946781561077)) ;
#83750 = CARTESIAN_POINT('Ctrl Pts',(-18.2517622204331,37.3609724634783,123.750174847478)) ;
#83751 = CARTESIAN_POINT('Ctrl Pts',(-18.2109407997604,37.3708278005919,123.547034393052)) ;
#83752 = CARTESIAN_POINT('Ctrl Pts',(-18.2056086311467,37.3808255354421,123.336940852331)) ;
#83753 = CARTESIAN_POINT('Ctrl Pts',(-18.2364910721176,37.3907334394265,123.130938228114)) ;
#83754 = CARTESIAN_POINT('Ctrl Pts',(-18.303026933122,37.400744513975,122.931261324963)) ;
#83755 = CARTESIAN_POINT('Ctrl Pts',(-18.4037673378414,37.4107723695106,122.746069528211)) ;
#83756 = CARTESIAN_POINT('Ctrl Pts',(-18.5326081128245,37.4206299634158,122.583754393451)) ;
#83757 = CARTESIAN_POINT('Ctrl Pts',(-18.6900546247519,37.4306566502539,122.44359153337)) ;
#83758 = CARTESIAN_POINT('Ctrl Pts',(-18.8697607051448,37.4406853194077,122.333319595354)) ;
#83759 = CARTESIAN_POINT('Ctrl Pts',(-19.0621377283289,37.4505305276891,122.256989623599)) ;
#83760 = CARTESIAN_POINT('Ctrl Pts',(-19.2677422232173,37.4605212166522,122.214048076628)) ;
#83761 = CARTESIAN_POINT('Ctrl Pts',(-19.4786785246119,37.4705590929345,122.207898022641)) ;
#83762 = CARTESIAN_POINT('Ctrl Pts',(-19.6835147870489,37.4804034705767,122.237521469835)) ;
#83763 = CARTESIAN_POINT('Ctrl Pts',(-19.882996095527,37.4903882749681,122.302778964749)) ;
#83764 = CARTESIAN_POINT('Ctrl Pts',(-20.0673693745768,37.5003278051867,122.401180197241)) ;
#83765 = CARTESIAN_POINT('Ctrl Pts',(-20.2334482168437,37.5103674932236,122.531409815803)) ;
#83766 = CARTESIAN_POINT('Ctrl Pts',(-20.3723615434971,37.5202557825919,122.686081229765)) ;
#83767 = CARTESIAN_POINT('Ctrl Pts',(-20.4837564567188,37.5302449062767,122.864096075934)) ;
#83768 = CARTESIAN_POINT('Ctrl Pts',(-20.5621702921538,37.5402049159513,123.058246148547)) ;
#83769 = CARTESIAN_POINT('Ctrl Pts',(-20.6059089803281,37.5501053456555,123.261743082962)) ;
#83770 = CARTESIAN_POINT('Ctrl Pts',(-20.6137506150888,37.5601484270623,123.47272578721)) ;
#83771 = CARTESIAN_POINT('Ctrl Pts',(-20.5852316440179,37.5700558209699,123.679059674677)) ;
#83772 = CARTESIAN_POINT('Ctrl Pts',(-20.5210197943171,37.5800675519591,123.879505655746)) ;
#83773 = CARTESIAN_POINT('Ctrl Pts',(-20.4224065041356,37.5900997696738,124.065948303167)) ;
#83774 = CARTESIAN_POINT('Ctrl Pts',(-20.2954706315988,37.59995227892,124.229610493564)) ;
#83775 = CARTESIAN_POINT('Ctrl Pts',(-20.1408283212273,37.609910215463,124.370729363786)) ;
#83776 = CARTESIAN_POINT('Ctrl Pts',(-19.9624090573161,37.6199490854713,124.48343363066)) ;
#83777 = CARTESIAN_POINT('Ctrl Pts',(-19.7704588435921,37.6298222406296,124.562502743437)) ;
#83778 = CARTESIAN_POINT('Ctrl Pts',(-19.5636464572191,37.6398955154793,124.607865012722)) ;
#83779 = CARTESIAN_POINT('Ctrl Pts',(-19.3573352443777,37.6497158326567,124.616683318652)) ;
#83780 = CARTESIAN_POINT('Ctrl Pts',(-19.1473126609859,37.6597945184502,124.589037290867)) ;
#83781 = CARTESIAN_POINT('Ctrl Pts',(-18.9497170068523,37.6696460298333,124.526820882821)) ;
#83782 = CARTESIAN_POINT('Ctrl Pts',(-18.7617822134983,37.6797194761399,124.429288117211)) ;
#83783 = CARTESIAN_POINT('Ctrl Pts',(-18.5974727396535,37.6895607512646,124.303521835439)) ;
#83784 = CARTESIAN_POINT('Ctrl Pts',(-18.4549977309688,37.6995458509214,124.149384967092)) ;
#83785 = CARTESIAN_POINT('Ctrl Pts',(-18.3414230044762,37.7095533270557,123.972266854178)) ;
#83786 = CARTESIAN_POINT('Ctrl Pts',(-18.2608486938713,37.7194759147646,123.779863616156)) ;
#83787 = CARTESIAN_POINT('Ctrl Pts',(-18.2142702298317,37.729462519038,123.575125889961)) ;
#83788 = CARTESIAN_POINT('Ctrl Pts',(-18.2042901761544,37.7395026473721,123.364303674408)) ;
#83789 = CARTESIAN_POINT('Ctrl Pts',(-18.2300893061444,37.7493420819055,123.159042211176)) ;
#83790 = CARTESIAN_POINT('Ctrl Pts',(-18.2923486019064,37.7594061363965,122.956858603344)) ;
#83791 = CARTESIAN_POINT('Ctrl Pts',(-18.3872136998659,37.7692970556336,122.77179660064)) ;
#83792 = CARTESIAN_POINT('Ctrl Pts',(-18.5136767992949,37.7792890489397,122.60407891323)) ;
#83793 = CARTESIAN_POINT('Ctrl Pts',(-18.6670286119021,37.789251912899,122.461423763276)) ;
#83794 = CARTESIAN_POINT('Ctrl Pts',(-18.8415186737119,37.7991561727167,122.347777335576)) ;
#83795 = CARTESIAN_POINT('Ctrl Pts',(-19.0361446776308,37.8092166632881,122.265052855607)) ;
#83796 = CARTESIAN_POINT('Ctrl Pts',(-19.2376613638147,37.8190570129192,122.218146463825)) ;
#83797 = CARTESIAN_POINT('Ctrl Pts',(-19.4488650436602,37.8291199884092,122.206437418726)) ;
#83798 = CARTESIAN_POINT('Ctrl Pts',(-19.6554019408263,37.8390143085526,122.231332716202)) ;
#83799 = CARTESIAN_POINT('Ctrl Pts',(-19.8555475570371,37.8489560216842,122.291445922081)) ;
#83800 = CARTESIAN_POINT('Ctrl Pts',(-20.0434591182195,37.8589589114783,122.385921690692)) ;
#83801 = CARTESIAN_POINT('Ctrl Pts',(-20.2124620853633,37.8689987686388,122.512333026513)) ;
#83802 = CARTESIAN_POINT('Ctrl Pts',(-20.3542123367619,37.8788229494764,122.662567208184)) ;
#83803 = CARTESIAN_POINT('Ctrl Pts',(-20.4706389075393,37.8888799229796,122.839032447305)) ;
#83804 = CARTESIAN_POINT('Ctrl Pts',(-20.5533481466804,37.8988080471667,123.030678526418)) ;
#83805 = CARTESIAN_POINT('Ctrl Pts',(-20.6021910285097,37.9087617422401,123.234157913246)) ;
#83806 = CARTESIAN_POINT('Ctrl Pts',(-20.6147789282106,37.9188079358154,123.4449832549)) ;
#83807 = CARTESIAN_POINT('Ctrl Pts',(-20.5912446252773,37.9286560381753,123.650677870567)) ;
#83808 = CARTESIAN_POINT('Ctrl Pts',(-20.5322977195808,37.9386176264029,123.851625135048)) ;
#83809 = CARTESIAN_POINT('Ctrl Pts',(-20.4384823086868,37.9486462965591,124.040450654678)) ;
#83810 = CARTESIAN_POINT('Ctrl Pts',(-20.3148504533172,37.9585565994409,124.20813777863)) ;
#83811 = CARTESIAN_POINT('Ctrl Pts',(-20.1639729427983,37.9684914832488,124.352574766539)) ;
#83812 = CARTESIAN_POINT('Ctrl Pts',(-19.9883521310107,37.9785326249394,124.469690942097)) ;
#83813 = CARTESIAN_POINT('Ctrl Pts',(-19.7980710765372,37.9884197461034,124.553374463438)) ;
#83814 = CARTESIAN_POINT('Ctrl Pts',(-19.5941095918449,37.9984120889519,124.603607303031)) ;
#83815 = CARTESIAN_POINT('Ctrl Pts',(-19.3854195842662,38.0083603901759,124.617543166151)) ;
#83816 = CARTESIAN_POINT('Ctrl Pts',(-19.177694220947,38.018297967858,124.595361007265)) ;
#83817 = CARTESIAN_POINT('Ctrl Pts',(-18.9759006217927,38.0282845423085,124.53736043578)) ;
#83818 = CARTESIAN_POINT('Ctrl Pts',(-18.7865662327341,38.038313352217,124.444601890689)) ;
#83819 = CARTESIAN_POINT('Ctrl Pts',(-18.6186516542393,38.0481916735238,124.322405716065)) ;
#83820 = CARTESIAN_POINT('Ctrl Pts',(-18.472489585433,38.0581833208712,124.171531238114)) ;
#83821 = CARTESIAN_POINT('Ctrl Pts',(-18.3546061530968,38.068217844309,123.996595612871)) ;
#83822 = CARTESIAN_POINT('Ctrl Pts',(-18.2699432567758,38.0780812011876,123.807284310517)) ;
#83823 = CARTESIAN_POINT('Ctrl Pts',(-18.2183482654027,38.0881514278679,123.601982881661)) ;
#83824 = CARTESIAN_POINT('Ctrl Pts',(-18.2035357134123,38.0979937360026,123.395589024256)) ;
#83825 = CARTESIAN_POINT('Ctrl Pts',(-18.2242703551438,38.107954468026,123.187217212771)) ;
#83826 = CARTESIAN_POINT('Ctrl Pts',(-18.2817100388421,38.1179923572241,122.984164140469)) ;
#83827 = CARTESIAN_POINT('Ctrl Pts',(-18.3717050512653,38.1278666401429,122.797069690323)) ;
#83828 = CARTESIAN_POINT('Ctrl Pts',(-18.4951947344798,38.1379363847604,122.62515584992)) ;
#83829 = CARTESIAN_POINT('Ctrl Pts',(-18.6430558971096,38.147769695106,122.480657473056)) ;
#83830 = CARTESIAN_POINT('Ctrl Pts',(-18.816822434158,38.1577999384587,122.361207113094)) ;
#83831 = CARTESIAN_POINT('Ctrl Pts',(-19.0089987785869,38.1678322264371,122.274295739322)) ;
#83832 = CARTESIAN_POINT('Ctrl Pts',(-19.2090434292556,38.1776594029052,122.222666245532)) ;
#83833 = CARTESIAN_POINT('Ctrl Pts',(-19.4186876276623,38.187664785772,122.205831123598)) ;
#83834 = CARTESIAN_POINT('Ctrl Pts',(-19.627653582682,38.1976474247647,122.225683031831)) ;
#83835 = CARTESIAN_POINT('Ctrl Pts',(-19.8311151594825,38.2076914919014,122.282093509122)) ;
#83836 = CARTESIAN_POINT('Ctrl Pts',(-20.0176420041598,38.2175127107054,122.37064600163)) ;
#83837 = CARTESIAN_POINT('Ctrl Pts',(-20.1899591987326,38.2275495496434,122.492420098757)) ;
#83838 = CARTESIAN_POINT('Ctrl Pts',(-20.3379110188023,38.2375739617412,122.64250885033)) ;
#83839 = CARTESIAN_POINT('Ctrl Pts',(-20.4558734175795,38.2474260461465,122.81276043771)) ;
#83840 = CARTESIAN_POINT('Ctrl Pts',(-20.5439817152443,38.2574169428896,123.00339930315)) ;
#83841 = CARTESIAN_POINT('Ctrl Pts',(-20.5974030969993,38.2673349347906,123.204972777987)) ;
#83842 = CARTESIAN_POINT('Ctrl Pts',(-20.6152555329228,38.2773630502476,123.415021619111)) ;
#83843 = CARTESIAN_POINT('Ctrl Pts',(-20.5967206678449,38.2872482261897,123.622015760556)) ;
#83844 = CARTESIAN_POINT('Ctrl Pts',(-20.5424483507648,38.2972375845966,123.824894040502)) ;
#83845 = CARTESIAN_POINT('Ctrl Pts',(-20.4529119922513,38.3072787321768,124.016061119421)) ;
#83846 = CARTESIAN_POINT('Ctrl Pts',(-20.3343454404401,38.3171113551833,124.18538604575)) ;
#83847 = CARTESIAN_POINT('Ctrl Pts',(-20.1862012398777,38.3271054262941,124.334369805916)) ;
#83848 = CARTESIAN_POINT('Ctrl Pts',(-20.0135915942845,38.3371340839349,124.455455362226)) ;
#83849 = CARTESIAN_POINT('Ctrl Pts',(-19.8254446593735,38.3470184101277,124.54364378584)) ;
#83850 = CARTESIAN_POINT('Ctrl Pts',(-19.6233091252654,38.3569841536184,124.598773682484)) ;
#83851 = CARTESIAN_POINT('Ctrl Pts',(-19.4133488542568,38.3670125327496,124.617784427648)) ;
#83852 = CARTESIAN_POINT('Ctrl Pts',(-19.2058864394032,38.3769133789565,124.600587770816)) ;
#83853 = CARTESIAN_POINT('Ctrl Pts',(-19.0014247677989,38.3869720363736,124.546746007214)) ;
#83854 = CARTESIAN_POINT('Ctrl Pts',(-18.8131022759335,38.3968295991555,124.460160335888)) ;
#83855 = CARTESIAN_POINT('Ctrl Pts',(-18.6390069736978,38.4068980017087,124.339821060971)) ;
#83856 = CARTESIAN_POINT('Ctrl Pts',(-18.4916162320444,38.4167534004483,124.194179107453)) ;
#83857 = CARTESIAN_POINT('Ctrl Pts',(-18.3695561134866,38.4267482675222,124.023151845071)) ;
#83858 = CARTESIAN_POINT('Ctrl Pts',(-18.2791222095453,38.4367795625056,123.832631966761)) ;
#83859 = CARTESIAN_POINT('Ctrl Pts',(-18.2237417212463,38.4466460872322,123.632728866384)) ;
#83860 = CARTESIAN_POINT('Ctrl Pts',(-18.2033366605409,38.4566335579279,123.423780131102)) ;
#83861 = CARTESIAN_POINT('Ctrl Pts',(-18.2193409223718,38.4665783174918,123.215291231871)) ;
#83862 = CARTESIAN_POINT('Ctrl Pts',(-18.2719426702172,38.4766238734406,123.010781908858)) ;
#83863 = CARTESIAN_POINT('Ctrl Pts',(-18.3574578438676,38.4864834618157,122.821937909227)) ;
#83864 = CARTESIAN_POINT('Ctrl Pts',(-18.4758459844247,38.4964844169518,122.648227494575)) ;
#83865 = CARTESIAN_POINT('Ctrl Pts',(-18.6211083978513,38.5063886442293,122.499006540837)) ;
#83866 = CARTESIAN_POINT('Ctrl Pts',(-18.7923421242233,38.5164307211245,122.375568110277)) ;
#83867 = CARTESIAN_POINT('Ctrl Pts',(-18.9798774217074,38.5263383338106,122.284845068347)) ;
#83868 = CARTESIAN_POINT('Ctrl Pts',(-19.1832184871999,38.5363928644264,122.227224428102)) ;
#83869 = CARTESIAN_POINT('Ctrl Pts',(-19.3894682309684,38.5462536509752,122.206072298328)) ;
#83870 = CARTESIAN_POINT('Ctrl Pts',(-19.5990133797797,38.5562474060463,122.220862897589)) ;
#83871 = CARTESIAN_POINT('Ctrl Pts',(-19.8015015919299,38.5661727662863,122.271381257439)) ;
#83872 = CARTESIAN_POINT('Ctrl Pts',(-19.9940600695036,38.5762006956816,122.357136872003)) ;
#83873 = CARTESIAN_POINT('Ctrl Pts',(-20.1665038714254,38.5860869624809,122.473213604027)) ;
#83874 = CARTESIAN_POINT('Ctrl Pts',(-20.3184039133706,38.5961187313791,122.619467213453)) ;
#83875 = CARTESIAN_POINT('Ctrl Pts',(-20.4409492915006,38.6060003272227,122.787261733951)) ;
#83876 = CARTESIAN_POINT('Ctrl Pts',(-20.5341860438392,38.6160622126907,122.977102521833)) ;
#83877 = CARTESIAN_POINT('Ctrl Pts',(-20.5919300802782,38.6259196467096,123.176157000518)) ;
#83878 = CARTESIAN_POINT('Ctrl Pts',(-20.6149768427881,38.6359128897515,123.384951999739)) ;
#83879 = CARTESIAN_POINT('Ctrl Pts',(-20.6015180584844,38.6458436506379,123.593303638436)) ;
#83880 = CARTESIAN_POINT('Ctrl Pts',(-20.5353364781107,38.6591926428351,123.866067846683)) ;
#83881 = CARTESIAN_POINT('Ctrl Pts',(-20.3999665698266,38.6724610156515,124.113595090077)) ;
#83882 = CARTESIAN_POINT('Ctrl Pts',(-20.2075244528949,38.6857439570358,124.315918873025)) ;
#83883 = CARTESIAN_POINT('Ctrl Pts',(-20.0375784179767,38.6957867428781,124.441187515618)) ;
#83884 = CARTESIAN_POINT('Ctrl Pts',(-19.8521844358346,38.7056366854302,124.53344877468)) ;
#83885 = CARTESIAN_POINT('Ctrl Pts',(-19.6507787501863,38.7156339183491,124.593496881762)) ;
#83886 = CARTESIAN_POINT('Ctrl Pts',(-19.4415865793863,38.7256488136837,124.617384098665)) ;
#83887 = CARTESIAN_POINT('Ctrl Pts',(-19.1637205474223,38.7388884903219,124.600727732205)) ;
#83888 = CARTESIAN_POINT('Ctrl Pts',(-18.8297226674719,38.7554357147272,124.490328749291)) ;
#83889 = CARTESIAN_POINT('Ctrl Pts',(-18.5515626228593,38.7720831518583,124.271315968218)) ;
#83890 = CARTESIAN_POINT('Ctrl Pts',(-18.3844931738527,38.7853726493365,124.047426592264)) ;
#83891 = CARTESIAN_POINT('Ctrl Pts',(-18.2905580424256,38.7952460571589,123.862315169489)) ;
#83892 = CARTESIAN_POINT('Ctrl Pts',(-18.2290723693852,38.8052984347516,123.660137301504)) ;
#83893 = CARTESIAN_POINT('Ctrl Pts',(-18.2040857533093,38.8152020882925,123.453418521977)) ;
#83894 = CARTESIAN_POINT('Ctrl Pts',(-18.2149101918065,38.8251463572878,123.244669041056)) ;
#83895 = CARTESIAN_POINT('Ctrl Pts',(-18.2776890698287,38.8384773656205,122.971450399707)) ;
#83896 = CARTESIAN_POINT('Ctrl Pts',(-18.4435331913446,38.8550989461448,122.659461152855)) ;
#83897 = CARTESIAN_POINT('Ctrl Pts',(-18.7042960227545,38.8716416168431,122.423288632422)) ;
#83898 = CARTESIAN_POINT('Ctrl Pts',(-18.9539076969586,38.8849907764061,122.295137393368)) ;
#83899 = CARTESIAN_POINT('Ctrl Pts',(-19.2195502286589,38.8982189265656,122.21266634664)) ;
#83900 = CARTESIAN_POINT('Ctrl Pts',(-19.5728078616279,38.9148496037031,122.198403767171)) ;
#83901 = CARTESIAN_POINT('Ctrl Pts',(-19.9761466167671,38.9347525429912,122.326687068324)) ;
#83902 = CARTESIAN_POINT('Ctrl Pts',(-20.3116532401564,38.9546554095944,122.584476648909)) ;
#83903 = CARTESIAN_POINT('Ctrl Pts',(-20.5398098713944,38.9745685746993,122.941266374104)) ;
#83904 = CARTESIAN_POINT('Ctrl Pts',(-20.6324050392952,38.9946044038406,123.357036057847)) ;
#83905 = CARTESIAN_POINT('Ctrl Pts',(-20.5783888068868,39.0144229787187,123.775059915529)) ;
#83906 = CARTESIAN_POINT('Ctrl Pts',(-20.3841956945606,39.0343932797607,124.152516109212)) ;
#83907 = CARTESIAN_POINT('Ctrl Pts',(-20.0739570774436,39.0542848121252,124.440209333799)) ;
#83908 = CARTESIAN_POINT('Ctrl Pts',(-19.6816966830104,39.0743079099418,124.605463079056)) ;
#83909 = CARTESIAN_POINT('Ctrl Pts',(-19.2612631464682,39.0941046628617,124.62700383692)) ;
#83910 = CARTESIAN_POINT('Ctrl Pts',(-18.8551291542701,39.1140657513505,124.503871232136)) ;
#83911 = CARTESIAN_POINT('Ctrl Pts',(-18.5155747700048,39.1340440202826,124.248566128734)) ;
#83912 = CARTESIAN_POINT('Ctrl Pts',(-18.2848897271834,39.1538640350736,123.895929288)) ;
#83913 = CARTESIAN_POINT('Ctrl Pts',(-18.1867323135785,39.1738024443255,123.48348235109)) ;
#83914 = CARTESIAN_POINT('Ctrl Pts',(-18.2364347214362,39.1938495617179,123.06008016948)) ;
#83915 = CARTESIAN_POINT('Ctrl Pts',(-18.4258541864355,39.2136958075517,122.683047672444)) ;
#83916 = CARTESIAN_POINT('Ctrl Pts',(-18.7315120380653,39.2335447760638,122.391994355)) ;
#83917 = CARTESIAN_POINT('Ctrl Pts',(-19.1222232914194,39.2535950783751,122.2215247231)) ;
#83918 = CARTESIAN_POINT('Ctrl Pts',(-19.5432352942313,39.2734300008063,122.194986111622)) ;
#83919 = CARTESIAN_POINT('Ctrl Pts',(-19.9499550927427,39.2933604020322,122.313413163743)) ;
#83920 = CARTESIAN_POINT('Ctrl Pts',(-20.2916490239367,39.313245347391,122.562710718802)) ;
#83921 = CARTESIAN_POINT('Ctrl Pts',(-20.5292736425933,39.3333179555424,122.917142170104)) ;
#83922 = CARTESIAN_POINT('Ctrl Pts',(-20.6303535167698,39.3531092718706,123.32570516107)) ;
#83923 = CARTESIAN_POINT('Ctrl Pts',(-20.5868689588886,39.3730740616378,123.747941864772)) ;
#83924 = CARTESIAN_POINT('Ctrl Pts',(-20.4007639600174,39.3930570173881,124.129914819336)) ;
#83925 = CARTESIAN_POINT('Ctrl Pts',(-20.0987295327906,39.4128655393642,124.42351592743)) ;
#83926 = CARTESIAN_POINT('Ctrl Pts',(-19.7115171487444,39.4328511141001,124.598356581541)) ;
#83927 = CARTESIAN_POINT('Ctrl Pts',(-19.2898686561888,39.4527337541685,124.630327663352)) ;
#83928 = CARTESIAN_POINT('Ctrl Pts',(-18.8812200067832,39.4726890663004,124.516450733859)) ;
#83929 = CARTESIAN_POINT('Ctrl Pts',(-18.5370775098728,39.4925634229082,124.271087917632)) ;
#83930 = CARTESIAN_POINT('Ctrl Pts',(-18.2958623876815,39.5125456297692,123.921382096351)) ;
#83931 = CARTESIAN_POINT('Ctrl Pts',(-18.1889226838399,39.5324767077192,123.511215629101)) ;
#83932 = CARTESIAN_POINT('Ctrl Pts',(-18.2282858913957,39.5524036825742,123.089434397404)) ;
#83933 = CARTESIAN_POINT('Ctrl Pts',(-18.4076742807777,39.5722361415231,122.707733435929)) ;
#83934 = CARTESIAN_POINT('Ctrl Pts',(-18.6583860005917,39.5888938256983,122.45771230889)) ;
#83935 = CARTESIAN_POINT('Ctrl Pts',(-18.899856660283,39.6021430496054,122.318686767975)) ;
#83936 = CARTESIAN_POINT('Ctrl Pts',(-19.0984023707433,39.6121920710566,122.246593172769)) ;
#83937 = CARTESIAN_POINT('Ctrl Pts',(-19.3025721748883,39.6220520792871,122.210698625699)) ;
#83938 = CARTESIAN_POINT('Ctrl Pts',(-19.5818091090242,39.6353355925117,122.209905164428)) ;
#83939 = CARTESIAN_POINT('Ctrl Pts',(-19.9238636732146,39.6519815115125,122.300943991679)) ;
#83940 = CARTESIAN_POINT('Ctrl Pts',(-20.2129499026306,39.6685354893286,122.501708337776)) ;
#83941 = CARTESIAN_POINT('Ctrl Pts',(-20.3943693157841,39.6818952183002,122.716154682349)) ;
#83942 = CARTESIAN_POINT('Ctrl Pts',(-20.4992257257281,39.6917882700969,122.895780883899)) ;
#83943 = CARTESIAN_POINT('Ctrl Pts',(-20.5722643729361,39.7017782353779,123.092667938302)) ;
#83944 = CARTESIAN_POINT('Ctrl Pts',(-20.6099946155583,39.7117301162387,123.298490471332)) ;
#83945 = CARTESIAN_POINT('Ctrl Pts',(-20.6112491614818,39.7217784679306,123.5097123281)) ;
#83946 = CARTESIAN_POINT('Ctrl Pts',(-20.5767745820442,39.7316197520368,123.713735911497)) ;
#83947 = CARTESIAN_POINT('Ctrl Pts',(-20.5068084652051,39.7416064551624,123.911647798122)) ;
#83948 = CARTESIAN_POINT('Ctrl Pts',(-20.404149955336,39.7515414839799,124.093590220558)) ;
#83949 = CARTESIAN_POINT('Ctrl Pts',(-20.2697572467411,39.7615972788868,124.256736870422)) ;
#83950 = CARTESIAN_POINT('Ctrl Pts',(-20.1128745784745,39.771425642176,124.391246879686)) ;
#83951 = CARTESIAN_POINT('Ctrl Pts',(-19.9310134309257,39.781486612074,124.499192637866)) ;
#83952 = CARTESIAN_POINT('Ctrl Pts',(-19.7359479982454,39.7914008909638,124.572688744676)) ;
#83953 = CARTESIAN_POINT('Ctrl Pts',(-19.5292237033137,39.801409885432,124.611969713177)) ;
#83954 = CARTESIAN_POINT('Ctrl Pts',(-19.3183814454034,39.8114397199958,124.614334357562)) ;
#83955 = CARTESIAN_POINT('Ctrl Pts',(-19.1138104499501,39.821297950068,124.581026337363)) ;
#83956 = CARTESIAN_POINT('Ctrl Pts',(-18.9153042209363,39.8312966558104,124.511985709217)) ;
#83957 = CARTESIAN_POINT('Ctrl Pts',(-18.7335269819325,39.8411913117292,124.410773872078)) ;
#83958 = CARTESIAN_POINT('Ctrl Pts',(-18.5694363601387,39.8512543761131,124.277299024287)) ;
#83959 = CARTESIAN_POINT('Ctrl Pts',(-18.4338684191718,39.861094034393,124.121008559524)) ;
#83960 = CARTESIAN_POINT('Ctrl Pts',(-18.3248828525009,39.8711572014749,123.939715182308)) ;
#83961 = CARTESIAN_POINT('Ctrl Pts',(-18.2504503795783,39.881051446602,123.745455644195)) ;
#83962 = CARTESIAN_POINT('Ctrl Pts',(-18.2101397445367,39.8909932682066,123.540397862087)) ;
#83963 = CARTESIAN_POINT('Ctrl Pts',(-18.2059424849837,39.9009957991247,123.330126961265)) ;
#83964 = CARTESIAN_POINT('Ctrl Pts',(-18.2387400782455,39.9110304255822,123.121743701287)) ;
#83965 = CARTESIAN_POINT('Ctrl Pts',(-18.3056247063555,39.9208759605686,122.925856511835)) ;
#83966 = CARTESIAN_POINT('Ctrl Pts',(-18.4064938974703,39.9308593854076,122.741821100437)) ;
#83967 = CARTESIAN_POINT('Ctrl Pts',(-18.5373982393695,39.9408097757727,122.578645629989)) ;
#83968 = CARTESIAN_POINT('Ctrl Pts',(-18.6952153467067,39.9508074160698,122.439801679769)) ;
#83969 = CARTESIAN_POINT('Ctrl Pts',(-18.8756822321668,39.960846496633,122.330394247099)) ;
#83970 = CARTESIAN_POINT('Ctrl Pts',(-19.0680855968778,39.9706726474021,122.255165125593)) ;
#83971 = CARTESIAN_POINT('Ctrl Pts',(-19.2752888310551,39.9807292223312,122.213206637334)) ;
#83972 = CARTESIAN_POINT('Ctrl Pts',(-19.4842192729442,39.9906697617115,122.20828893783)) ;
#83973 = CARTESIAN_POINT('Ctrl Pts',(-19.6901728378794,40.0005741546879,122.238964162981)) ;
#83974 = CARTESIAN_POINT('Ctrl Pts',(-19.8904453981696,40.0106208088928,122.306001788064)) ;
#83975 = CARTESIAN_POINT('Ctrl Pts',(-20.0733802135455,40.0205163708312,122.405136531576)) ;
#83976 = CARTESIAN_POINT('Ctrl Pts',(-20.2390148331265,40.0305784486768,122.536666604298)) ;
#83977 = CARTESIAN_POINT('Ctrl Pts',(-20.3763608552124,40.0404211470905,122.691467800279)) ;
#83978 = CARTESIAN_POINT('Ctrl Pts',(-20.4867687239541,40.050411922052,122.870114190149)) ;
#83979 = CARTESIAN_POINT('Ctrl Pts',(-20.5639763620447,40.0603397870711,123.064036076896)) ;
#83980 = CARTESIAN_POINT('Ctrl Pts',(-20.6069421627515,40.0703285318373,123.269592676975)) ;
#83981 = CARTESIAN_POINT('Ctrl Pts',(-20.6132830460432,40.0803613174242,123.480421510486)) ;
#83982 = CARTESIAN_POINT('Ctrl Pts',(-20.5836334756742,40.0902280020449,123.685712616004)) ;
#83983 = CARTESIAN_POINT('Ctrl Pts',(-20.5187331389451,40.100189894208,123.884836795131)) ;
#83984 = CARTESIAN_POINT('Ctrl Pts',(-20.4192475497836,40.1102233711206,124.070827756619)) ;
#83985 = CARTESIAN_POINT('Ctrl Pts',(-20.2911532710343,40.1201077123689,124.234483925835)) ;
#83986 = CARTESIAN_POINT('Ctrl Pts',(-20.1338366504222,40.13017065449,124.375890206505)) ;
#83987 = CARTESIAN_POINT('Ctrl Pts',(-19.9581654257089,40.1400210561096,124.485576275425)) ;
#83988 = CARTESIAN_POINT('Ctrl Pts',(-19.7628967023069,40.1500479448992,124.564969159993)) ;
#83989 = CARTESIAN_POINT('Ctrl Pts',(-19.5566424479521,40.1600765598555,124.60872174278)) ;
#83990 = CARTESIAN_POINT('Ctrl Pts',(-19.3498138019929,40.1699217829755,124.61625506074)) ;
#83991 = CARTESIAN_POINT('Ctrl Pts',(-19.1416957832697,40.1799124667815,124.587896764921)) ;
#83992 = CARTESIAN_POINT('Ctrl Pts',(-18.9408691373841,40.1899503488539,124.523084939537)) ;
#83993 = CARTESIAN_POINT('Ctrl Pts',(-18.7577650040935,40.1997947084927,124.426605483624)) ;
#83994 = CARTESIAN_POINT('Ctrl Pts',(-18.5916351108559,40.2097795791075,124.298338376431)) ;
#83995 = CARTESIAN_POINT('Ctrl Pts',(-18.4508347705853,40.2197188624361,124.143903010517)) ;
#83996 = CARTESIAN_POINT('Ctrl Pts',(-18.3379319966298,40.2297594718093,123.96557517779)) ;
#83997 = CARTESIAN_POINT('Ctrl Pts',(-18.2587923174509,40.2396443227225,123.773397813617)) ;
#83998 = CARTESIAN_POINT('Ctrl Pts',(-18.213460031334,40.2496462788913,123.568102243328)) ;
#83999 = CARTESIAN_POINT('Ctrl Pts',(-18.204367545909,40.2595648756118,123.359747486292)) ;
#84000 = CARTESIAN_POINT('Ctrl Pts',(-18.2319750563764,40.2696116976876,123.150373468902)) ;
#84001 = CARTESIAN_POINT('Ctrl Pts',(-18.2942593625659,40.2794859788003,122.952312214751)) ;
#84002 = CARTESIAN_POINT('Ctrl Pts',(-18.3915852031377,40.2895401788449,122.764722269776)) ;
#84003 = CARTESIAN_POINT('Ctrl Pts',(-18.5179539789495,40.2994356084801,122.599419714225)) ;
#84004 = CARTESIAN_POINT('Ctrl Pts',(-18.6735953670539,40.3094972367975,122.456211498221)) ;
#84005 = CARTESIAN_POINT('Ctrl Pts',(-18.8479090387008,40.3193418656274,122.34462186564)) ;
#84006 = CARTESIAN_POINT('Ctrl Pts',(-19.0408896885059,40.329301913233,122.263369317502)) ;
#84007 = CARTESIAN_POINT('Ctrl Pts',(-19.246736340465,40.339340219407,122.216899416783)) ;
#84008 = CARTESIAN_POINT('Ctrl Pts',(-19.454082103357,40.3492135188397,122.20664050289)) ;
#84009 = CARTESIAN_POINT('Ctrl Pts',(-19.6641481133357,40.359286780426,122.233123002106)) ;
#84010 = CARTESIAN_POINT('Ctrl Pts',(-19.861509253522,40.3691070063827,122.293870082184)) ;
#84011 = CARTESIAN_POINT('Ctrl Pts',(-20.050164432258,40.3791860703222,122.390230258189)) ;
#84012 = CARTESIAN_POINT('Ctrl Pts',(-20.2155277669988,40.389036160342,122.514970602576)) ;
#84013 = CARTESIAN_POINT('Ctrl Pts',(-20.3600033921578,40.3991149139558,122.669891379684)) ;
#84014 = CARTESIAN_POINT('Ctrl Pts',(-20.4726264427281,40.4089363812152,122.843004495884)) ;
#84015 = CARTESIAN_POINT('Ctrl Pts',(-20.5557528282333,40.4190019795729,123.037552166323)) ;
#84016 = CARTESIAN_POINT('Ctrl Pts',(-20.6030259622588,40.4289046353476,123.24035156858)) ;
#84017 = CARTESIAN_POINT('Ctrl Pts',(-20.6145983075349,40.4389554611772,123.451291704677)) ;
#84018 = CARTESIAN_POINT('Ctrl Pts',(-20.5900018171462,40.4488296655161,123.657461665772)) ;
#84019 = CARTESIAN_POINT('Ctrl Pts',(-20.5288150242809,40.4589021155552,123.860137172536)) ;
#84020 = CARTESIAN_POINT('Ctrl Pts',(-20.4358132666408,40.4687311323287,124.044705992598)) ;
#84021 = CARTESIAN_POINT('Ctrl Pts',(-20.3094637393586,40.4787979782435,124.214444033496)) ;
#84022 = CARTESIAN_POINT('Ctrl Pts',(-20.1581261325448,40.4886881495453,124.357060562804)) ;
#84023 = CARTESIAN_POINT('Ctrl Pts',(-19.9828174861627,40.4986803431691,124.472776119996)) ;
#84024 = CARTESIAN_POINT('Ctrl Pts',(-19.7905608688836,40.5086431537925,124.555869129345)) ;
#84025 = CARTESIAN_POINT('Ctrl Pts',(-19.5880954730282,40.518547426636,124.604552612878)) ;
#84026 = CARTESIAN_POINT('Ctrl Pts',(-19.3770061385178,40.5286079184406,124.617357350951)) ;
#84027 = CARTESIAN_POINT('Ctrl Pts',(-19.1714136665381,40.5384482501129,124.594104016423)) ;
#84028 = CARTESIAN_POINT('Ctrl Pts',(-18.9684724548646,40.5485112962047,124.534440348117)) ;
#84029 = CARTESIAN_POINT('Ctrl Pts',(-18.7821897791034,40.5584053518998,124.441849138628)) ;
#84030 = CARTESIAN_POINT('Ctrl Pts',(-18.6136871793535,40.5683480522227,124.318199437492)) ;
#84031 = CARTESIAN_POINT('Ctrl Pts',(-18.4682360875354,40.5783537931503,124.166208379419)) ;
#84032 = CARTESIAN_POINT('Ctrl Pts',(-18.3514206949662,40.5883747036659,123.990896048269)) ;
#84033 = CARTESIAN_POINT('Ctrl Pts',(-18.2676944058122,40.5982654391158,123.80055651548)) ;
#84034 = CARTESIAN_POINT('Ctrl Pts',(-18.2174871451412,40.6082569798447,123.596600026153)) ;
#84035 = CARTESIAN_POINT('Ctrl Pts',(-18.2035765211451,40.6182048402663,123.387929661451)) ;
#84036 = CARTESIAN_POINT('Ctrl Pts',(-18.2256975259737,40.6281515094527,123.179981133137)) ;
#84037 = CARTESIAN_POINT('Ctrl Pts',(-18.2843962838863,40.6381995855883,122.977065937708)) ;
#84038 = CARTESIAN_POINT('Ctrl Pts',(-18.3754280473038,40.6480471835939,122.791125024287)) ;
#84039 = CARTESIAN_POINT('Ctrl Pts',(-18.4982372741933,40.6580089066784,122.621498389461)) ;
#84040 = CARTESIAN_POINT('Ctrl Pts',(-18.6498469120804,40.6680375417614,122.474969319783)) ;
#84041 = CARTESIAN_POINT('Ctrl Pts',(-18.8224769707275,40.6779478500794,122.358338766406)) ;
#84042 = CARTESIAN_POINT('Ctrl Pts',(-19.0129988131327,40.6878827472153,122.272737599559)) ;
#84043 = CARTESIAN_POINT('Ctrl Pts',(-19.2176901817854,40.6979238301579,122.221162632871)) ;
#84044 = CARTESIAN_POINT('Ctrl Pts',(-19.4250098113896,40.7078111729861,122.206002229052)) ;
#84045 = CARTESIAN_POINT('Ctrl Pts',(-19.6340061907446,40.7178026879254,122.226929971137)) ;
#84046 = CARTESIAN_POINT('Ctrl Pts',(-19.835373853098,40.7277540791219,122.283688979789)) ;
#84047 = CARTESIAN_POINT('Ctrl Pts',(-20.0236219719852,40.7376866124545,122.374049360346)) ;
#84048 = CARTESIAN_POINT('Ctrl Pts',(-20.1944682418108,40.747683770354,122.496443508176)) ;
#84049 = CARTESIAN_POINT('Ctrl Pts',(-20.3413742173031,40.7576687805175,122.646434347578)) ;
#84050 = CARTESIAN_POINT('Ctrl Pts',(-20.4604016388904,40.7677116070873,122.82078190189)) ;
#84051 = CARTESIAN_POINT('Ctrl Pts',(-20.545965381587,40.7775418413922,123.008934982547)) ;
#84052 = CARTESIAN_POINT('Ctrl Pts',(-20.5989226624239,40.7876178666269,123.213993657036)) ;
#84053 = CARTESIAN_POINT('Ctrl Pts',(-20.6152177266927,40.7974701031178,123.420521265477)) ;
#84054 = CARTESIAN_POINT('Ctrl Pts',(-20.595146371147,40.8075433095519,123.631304261666)) ;
#84055 = CARTESIAN_POINT('Ctrl Pts',(-20.5400095589462,40.8173848190591,123.830735669813)) ;
#84056 = CARTESIAN_POINT('Ctrl Pts',(-20.4507245478584,40.8273457658389,124.020150570781)) ;
#84057 = CARTESIAN_POINT('Ctrl Pts',(-20.3286295016058,40.8373835946389,124.192262277119)) ;
#84058 = CARTESIAN_POINT('Ctrl Pts',(-20.1811994395748,40.8472579043934,124.338439950334)) ;
#84059 = CARTESIAN_POINT('Ctrl Pts',(-20.0072892729552,40.8573276020665,124.459100741627)) ;
#84060 = CARTESIAN_POINT('Ctrl Pts',(-19.8195861561062,40.8671610733539,124.545769392456)) ;
#84061 = CARTESIAN_POINT('Ctrl Pts',(-19.615872314466,40.8771907198839,124.600164946026)) ;
#84062 = CARTESIAN_POINT('Ctrl Pts',(-19.4056431537582,40.8872252342113,124.617731140901)) ;
#84063 = CARTESIAN_POINT('Ctrl Pts',(-19.1998966584607,40.8970505196821,124.599424022294)) ;
#84064 = CARTESIAN_POINT('Ctrl Pts',(-18.9967300700441,40.9070547612307,124.545129020329)) ;
#84065 = CARTESIAN_POINT('Ctrl Pts',(-18.8064674138369,40.9170374063098,124.456466503023)) ;
#84066 = CARTESIAN_POINT('Ctrl Pts',(-18.6336010926336,40.9270826034013,124.335200573966)) ;
#84067 = CARTESIAN_POINT('Ctrl Pts',(-18.4874473673318,40.9369057191614,124.189290879588)) ;
#84068 = CARTESIAN_POINT('Ctrl Pts',(-18.3658653930389,40.9469403309617,124.016894765703)) ;
#84069 = CARTESIAN_POINT('Ctrl Pts',(-18.2766790054836,40.9569653397348,123.825931009398)) ;
#84070 = CARTESIAN_POINT('Ctrl Pts',(-18.2225124709899,40.9668172645764,123.626017271798)) ;
#84071 = CARTESIAN_POINT('Ctrl Pts',(-18.203299075712,40.9768082028991,123.416882417543)) ;
#84072 = CARTESIAN_POINT('Ctrl Pts',(-18.220432722887,40.9867261880456,123.209055352599)) ;
#84073 = CARTESIAN_POINT('Ctrl Pts',(-18.2739197568231,40.9967542889411,123.005147713301)) ;
#84074 = CARTESIAN_POINT('Ctrl Pts',(-18.3606743272535,41.0066395298837,122.816298472625)) ;
#84075 = CARTESIAN_POINT('Ctrl Pts',(-18.4797205533408,41.0166286428503,122.643290607372)) ;
#84076 = CARTESIAN_POINT('Ctrl Pts',(-18.6281007078246,41.0266707071911,122.493120515096)) ;
#84077 = CARTESIAN_POINT('Ctrl Pts',(-18.7964346106993,41.0364999085956,122.373256813908)) ;
#84078 = CARTESIAN_POINT('Ctrl Pts',(-18.9861689447885,41.0465067493538,122.282435666155)) ;
#84079 = CARTESIAN_POINT('Ctrl Pts',(-19.1884902487412,41.0564942735457,122.226152190945)) ;
#84080 = CARTESIAN_POINT('Ctrl Pts',(-19.3983530804929,41.0665239193543,122.205918577425)) ;
#84081 = CARTESIAN_POINT('Ctrl Pts',(-19.605339265154,41.076397950093,122.221929297578)) ;
#84082 = CARTESIAN_POINT('Ctrl Pts',(-19.8089638120336,41.0863972729571,122.274027018011)) ;
#84083 = CARTESIAN_POINT('Ctrl Pts',(-19.9989028196144,41.0963081085327,122.359763952569)) ;
#84084 = CARTESIAN_POINT('Ctrl Pts',(-20.1734602703495,41.1063623565068,122.478901029742)) ;
#84085 = CARTESIAN_POINT('Ctrl Pts',(-20.3219594050165,41.1162211007695,122.62353974216)) ;
#84086 = CARTESIAN_POINT('Ctrl Pts',(-20.4457241103997,41.1262891868425,122.795209530907)) ;
#84087 = CARTESIAN_POINT('Ctrl Pts',(-20.535863063905,41.136144670022,122.981787012691)) ;
#84088 = CARTESIAN_POINT('Ctrl Pts',(-20.5936332050625,41.1461395158162,123.183805523602)) ;
#84089 = CARTESIAN_POINT('Ctrl Pts',(-20.6150774326418,41.1561708114787,123.393606067351)) ;
#84090 = CARTESIAN_POINT('Ctrl Pts',(-20.6003488779222,41.1660373547686,123.600515251708)) ;
#84091 = CARTESIAN_POINT('Ctrl Pts',(-20.5496364134409,41.176024750532,123.804239891869)) ;
#84092 = CARTESIAN_POINT('Ctrl Pts',(-20.4647624232787,41.185969791262,123.995347573894)) ;
#84093 = CARTESIAN_POINT('Ctrl Pts',(-20.3467582709289,41.1960142974787,124.170441035072)) ;
#84094 = CARTESIAN_POINT('Ctrl Pts',(-20.2028932956802,41.205877803616,124.319807442047)) ;
#84095 = CARTESIAN_POINT('Ctrl Pts',(-20.0333415512162,41.2158706644521,124.443797445221)) ;
#84096 = CARTESIAN_POINT('Ctrl Pts',(-19.8460833020742,41.225796858171,124.535960566689)) ;
#84097 = CARTESIAN_POINT('Ctrl Pts',(-19.6438582487859,41.2358157842036,124.594776911831)) ;
#84098 = CARTESIAN_POINT('Ctrl Pts',(-19.4366299850422,41.2457307835712,124.617551938462)) ;
#84099 = CARTESIAN_POINT('Ctrl Pts',(-19.2257234112187,41.2557855551285,124.603768112369)) ;
#84100 = CARTESIAN_POINT('Ctrl Pts',(-19.0243302973375,41.265644517426,124.55466833159)) ;
#84101 = CARTESIAN_POINT('Ctrl Pts',(-18.8318135036879,41.2756387612639,124.470587736357)) ;
#84102 = CARTESIAN_POINT('Ctrl Pts',(-18.6579190557029,41.2855639906881,124.35520482749)) ;
#84103 = CARTESIAN_POINT('Ctrl Pts',(-18.5051729929965,41.2955919545796,124.209940587375)) ;
#84104 = CARTESIAN_POINT('Ctrl Pts',(-18.3815316967757,41.30547821421,124.042837487095)) ;
#84105 = CARTESIAN_POINT('Ctrl Pts',(-18.2873498166845,41.3155099772878,123.854175099983)) ;
#84106 = CARTESIAN_POINT('Ctrl Pts',(-18.2280402925463,41.3253916035819,123.655039695236)) ;
#84107 = CARTESIAN_POINT('Ctrl Pts',(-18.2037261419787,41.3354533730681,123.444942864468)) ;
#84108 = CARTESIAN_POINT('Ctrl Pts',(-18.2159492400391,41.3453112405636,123.238034912573)) ;
#84109 = CARTESIAN_POINT('Ctrl Pts',(-18.2640991524596,41.3553028656809,123.033597999841)) ;
#84110 = CARTESIAN_POINT('Ctrl Pts',(-18.3466098748585,41.3652396647892,122.841666401691)) ;
#84111 = CARTESIAN_POINT('Ctrl Pts',(-18.4615560357131,41.3752304943465,122.665869308741)) ;
#84112 = CARTESIAN_POINT('Ctrl Pts',(-18.6059270402561,41.3852537300597,122.512369557892)) ;
#84113 = CARTESIAN_POINT('Ctrl Pts',(-18.7725080465758,41.3951500780889,122.387730247027)) ;
#84114 = CARTESIAN_POINT('Ctrl Pts',(-18.9597602693054,41.4051396405914,122.292617765238)) ;
#84115 = CARTESIAN_POINT('Ctrl Pts',(-19.1618068495338,41.4151799482759,122.231566049931)) ;
#84116 = CARTESIAN_POINT('Ctrl Pts',(-19.3672327140925,41.4250222516231,122.206620712325)) ;
#84117 = CARTESIAN_POINT('Ctrl Pts',(-19.5776398977284,41.4350459599022,122.21764350523)) ;
#84118 = CARTESIAN_POINT('Ctrl Pts',(-19.8485692369757,41.4482681373699,122.280066833461)) ;
#84119 = CARTESIAN_POINT('Ctrl Pts',(-20.0983813608666,41.4615607224292,122.412161972798)) ;
#84120 = CARTESIAN_POINT('Ctrl Pts',(-20.303073356928,41.4748455783508,122.602192135613)) ;
#84121 = CARTESIAN_POINT('Ctrl Pts',(-20.4297314686523,41.4848178055236,122.769227486127)) ;
#84122 = CARTESIAN_POINT('Ctrl Pts',(-20.5251912543411,41.4947264219626,122.954404447147)) ;
#84123 = CARTESIAN_POINT('Ctrl Pts',(-20.5878572647725,41.5047796273463,123.156230096444)) ;
#84124 = CARTESIAN_POINT('Ctrl Pts',(-20.6141674277665,41.5146447611066,123.361965495425)) ;
#84125 = CARTESIAN_POINT('Ctrl Pts',(-20.6014118208167,41.5279838187329,123.642111014814)) ;
#84126 = CARTESIAN_POINT('Ctrl Pts',(-20.494885952926,41.544553006066,123.977938704161)) ;
#84127 = CARTESIAN_POINT('Ctrl Pts',(-20.2793745820825,41.5611981459171,124.258685789852)) ;
#84128 = CARTESIAN_POINT('Ctrl Pts',(-20.0579576947335,41.5744704483905,124.428476506012)) ;
#84129 = CARTESIAN_POINT('Ctrl Pts',(-19.8719402894778,41.5844514118381,124.52554227184)) ;
#84130 = CARTESIAN_POINT('Ctrl Pts',(-19.6726896538698,41.5943932439074,124.588712900572)) ;
#84131 = CARTESIAN_POINT('Ctrl Pts',(-19.39515947758,41.6077128131228,124.625810170929)) ;
#84132 = CARTESIAN_POINT('Ctrl Pts',(-19.0464439657701,41.6242429680556,124.581269960781)) ;
#84133 = CARTESIAN_POINT('Ctrl Pts',(-18.6680926078095,41.6442646935477,124.386344269769)) ;
#84134 = CARTESIAN_POINT('Ctrl Pts',(-18.3816919436633,41.6640760901545,124.077301459505)) ;
#84135 = CARTESIAN_POINT('Ctrl Pts',(-18.2159314047826,41.6840613388633,123.686131291422)) ;
#84136 = CARTESIAN_POINT('Ctrl Pts',(-18.1939891745708,41.7039554014993,123.263631019772)) ;
#84137 = CARTESIAN_POINT('Ctrl Pts',(-18.3171493950975,41.7238870806729,122.858127957561)) ;
#84138 = CARTESIAN_POINT('Ctrl Pts',(-18.5719340628339,41.7438511351449,122.51860266307)) ;
#84139 = CARTESIAN_POINT('Ctrl Pts',(-18.9256476276961,41.7637320369078,122.287092846652)) ;
#84140 = CARTESIAN_POINT('Ctrl Pts',(-19.3381948683728,41.7836706985162,122.189526548591)) ;
#84141 = CARTESIAN_POINT('Ctrl Pts',(-19.7584053445719,41.8035672237715,122.238430566627)) ;
#84142 = CARTESIAN_POINT('Ctrl Pts',(-20.1370057693331,41.8234622622258,122.427169239193)) ;
#84143 = CARTESIAN_POINT('Ctrl Pts',(-20.4294053281451,41.8434260855319,122.734843250388)) ;
#84144 = CARTESIAN_POINT('Ctrl Pts',(-20.5988096520374,41.8633002096609,123.122013415926)) ;
#84145 = CARTESIAN_POINT('Ctrl Pts',(-20.6264542889846,41.8832752853882,123.545855735373)) ;
#84146 = CARTESIAN_POINT('Ctrl Pts',(-20.5073566083067,41.9032288547448,123.953056646348)) ;
#84147 = CARTESIAN_POINT('Ctrl Pts',(-20.2585450342421,41.9230667649326,124.29366905313)) ;
#84148 = CARTESIAN_POINT('Ctrl Pts',(-19.9062556139249,41.9430425935036,124.530937461275)) ;
#84149 = CARTESIAN_POINT('Ctrl Pts',(-19.4952528460471,41.9629606382138,124.632990013257)) ;
#84150 = CARTESIAN_POINT('Ctrl Pts',(-19.0748806212009,41.9828308840015,124.589826715437)) ;
#84151 = CARTESIAN_POINT('Ctrl Pts',(-18.6915025085209,42.0028798871011,124.403663986878)) ;
#84152 = CARTESIAN_POINT('Ctrl Pts',(-18.3981608610353,42.0226591283419,124.102123408947)) ;
#84153 = CARTESIAN_POINT('Ctrl Pts',(-18.2226406675483,42.0426891920508,123.714185684315)) ;
#84154 = CARTESIAN_POINT('Ctrl Pts',(-18.1909502299276,42.0625714769527,123.292557552484)) ;
#84155 = CARTESIAN_POINT('Ctrl Pts',(-18.3038833814422,42.0824537778457,122.885208178774)) ;
#84156 = CARTESIAN_POINT('Ctrl Pts',(-18.5504266417596,42.1024368874641,122.539145783805)) ;
#84157 = CARTESIAN_POINT('Ctrl Pts',(-18.8986862807476,42.122327282842,122.299139021908)) ;
#84158 = CARTESIAN_POINT('Ctrl Pts',(-19.3078323184584,42.1422240728762,122.191754248238)) ;
#84159 = CARTESIAN_POINT('Ctrl Pts',(-19.7296141903488,42.1621411268179,122.230019843799)) ;
#84160 = CARTESIAN_POINT('Ctrl Pts',(-20.1146546190343,42.1821446750214,122.410843614084)) ;
#84161 = CARTESIAN_POINT('Ctrl Pts',(-20.4133983649852,42.202082968674,122.711612553304)) ;
#84162 = CARTESIAN_POINT('Ctrl Pts',(-20.5914741681142,42.2219044561069,123.093609268308)) ;
#84163 = CARTESIAN_POINT('Ctrl Pts',(-20.6292246758247,42.2418828490978,123.516673289908)) ;
#84164 = CARTESIAN_POINT('Ctrl Pts',(-20.5204944696321,42.2617812307115,123.925630779362)) ;
#84165 = CARTESIAN_POINT('Ctrl Pts',(-20.3195273000853,42.2783641614414,124.215224407757)) ;
#84166 = CARTESIAN_POINT('Ctrl Pts',(-20.106668699646,42.2916383970302,124.395804380293)) ;
#84167 = CARTESIAN_POINT('Ctrl Pts',(-19.9243029543144,42.3016848144864,124.502286299798)) ;
#84168 = CARTESIAN_POINT('Ctrl Pts',(-19.7302093566461,42.3115300397057,124.574250347447)) ;
#84169 = CARTESIAN_POINT('Ctrl Pts',(-19.454606237044,42.3248650107451,124.625183227152)) ;
#84170 = CARTESIAN_POINT('Ctrl Pts',(-19.1029744052115,42.3414478675377,124.597295491216)) ;
#84171 = CARTESIAN_POINT('Ctrl Pts',(-18.7810077769034,42.3580908698871,124.450748766499)) ;
#84172 = CARTESIAN_POINT('Ctrl Pts',(-18.5658476550181,42.3713346009188,124.273892948555)) ;
#84173 = CARTESIAN_POINT('Ctrl Pts',(-18.4283770364785,42.3813889955934,124.113388633526)) ;
#84174 = CARTESIAN_POINT('Ctrl Pts',(-18.3228682596185,42.3912300569819,123.935378247258)) ;
#84175 = CARTESIAN_POINT('Ctrl Pts',(-18.2480350846399,42.4012962813384,123.737465749298)) ;
#84176 = CARTESIAN_POINT('Ctrl Pts',(-18.2094758316958,42.4111768942581,123.53331998125)) ;
#84177 = CARTESIAN_POINT('Ctrl Pts',(-18.2065221797275,42.4211701874177,123.323284136936)) ;
#84178 = CARTESIAN_POINT('Ctrl Pts',(-18.2398729765059,42.4311211956413,123.116720768107)) ;
#84179 = CARTESIAN_POINT('Ctrl Pts',(-18.3093895953043,42.4411697100033,122.917259886208)) ;
#84180 = CARTESIAN_POINT('Ctrl Pts',(-18.4101750501696,42.451011216066,122.736545002513)) ;
#84181 = CARTESIAN_POINT('Ctrl Pts',(-18.5423307476065,42.4609968686957,122.573475467159)) ;
#84182 = CARTESIAN_POINT('Ctrl Pts',(-18.7000496641721,42.4709358775406,122.436369799845)) ;
#84183 = CARTESIAN_POINT('Ctrl Pts',(-18.8809998215444,42.4809768028336,122.327702252941)) ;
#84184 = CARTESIAN_POINT('Ctrl Pts',(-19.075104637649,42.4908671245885,122.253109681038)) ;
#84185 = CARTESIAN_POINT('Ctrl Pts',(-19.2812985955346,42.5008630979219,122.212630849789)) ;
#84186 = CARTESIAN_POINT('Ctrl Pts',(-19.4900575848041,42.510794497504,122.208578593669)) ;
#84187 = CARTESIAN_POINT('Ctrl Pts',(-19.6979366117902,42.520800037981,122.24078115684)) ;
#84188 = CARTESIAN_POINT('Ctrl Pts',(-19.8974710231854,42.5308330219123,122.309135094637)) ;
#84189 = CARTESIAN_POINT('Ctrl Pts',(-20.0790398642152,42.5406886527391,122.408984399467)) ;
#84190 = CARTESIAN_POINT('Ctrl Pts',(-20.2429987573532,42.5506880549323,122.540492343443)) ;
#84191 = CARTESIAN_POINT('Ctrl Pts',(-20.3804073367586,42.5605825242934,122.696711264063)) ;
#84192 = CARTESIAN_POINT('Ctrl Pts',(-20.4903548510497,42.5706456384576,122.877413023356)) ;
#84193 = CARTESIAN_POINT('Ctrl Pts',(-20.5657866640294,42.580485284174,123.070066475262)) ;
#84194 = CARTESIAN_POINT('Ctrl Pts',(-20.6078006789638,42.5905484517297,123.277382573781)) ;
#84195 = CARTESIAN_POINT('Ctrl Pts',(-20.6129143402783,42.6004427075246,123.48535102237)) ;
#84196 = CARTESIAN_POINT('Ctrl Pts',(-20.5822609083431,42.6103844859843,123.692072366378)) ;
#84197 = CARTESIAN_POINT('Ctrl Pts',(-20.5158291283224,42.6203871788145,123.891620696624)) ;
#84198 = CARTESIAN_POINT('Ctrl Pts',(-20.4151804975653,42.6304212007683,124.076996124411)) ;
#84199 = CARTESIAN_POINT('Ctrl Pts',(-20.2865490933976,42.6402689918573,124.239226619396)) ;
#84200 = CARTESIAN_POINT('Ctrl Pts',(-20.1299261467673,42.6502505164063,124.378854112824)) ;
#84201 = CARTESIAN_POINT('Ctrl Pts',(-19.9519781253064,42.6601997398973,124.488795047195)) ;
#84202 = CARTESIAN_POINT('Ctrl Pts',(-19.7567858477738,42.6701973961138,124.566794955655)) ;
#84203 = CARTESIAN_POINT('Ctrl Pts',(-19.5500874626473,42.6802376091689,124.609497549118)) ;
#84204 = CARTESIAN_POINT('Ctrl Pts',(-19.3435610750483,42.6900656564452,124.615984151148)) ;
#84205 = CARTESIAN_POINT('Ctrl Pts',(-19.1343128423954,42.7001200034775,124.586163345661)) ;
#84206 = CARTESIAN_POINT('Ctrl Pts',(-18.9357761785149,42.7100611398061,124.520862042553)) ;
#84207 = CARTESIAN_POINT('Ctrl Pts',(-18.7519747196911,42.7199653728858,124.423017051191)) ;
#84208 = CARTESIAN_POINT('Ctrl Pts',(-18.5856939200554,42.7300120697294,124.29280902179)) ;
#84209 = CARTESIAN_POINT('Ctrl Pts',(-18.4464957947498,42.7399076210097,124.138158890315)) ;
#84210 = CARTESIAN_POINT('Ctrl Pts',(-18.3344432793517,42.7499696988492,123.958773213698)) ;
#84211 = CARTESIAN_POINT('Ctrl Pts',(-18.2568373001376,42.7598124079452,123.766927664689)) ;
#84212 = CARTESIAN_POINT('Ctrl Pts',(-18.2125966963191,42.7698031401837,123.561630546517)) ;
#84213 = CARTESIAN_POINT('Ctrl Pts',(-18.2047563020714,42.7797311654124,123.35304849605)) ;
#84214 = CARTESIAN_POINT('Ctrl Pts',(-18.2330695491077,42.789719312063,123.144978918657)) ;
#84215 = CARTESIAN_POINT('Ctrl Pts',(-18.2976873840925,42.799754329903,122.944147828888)) ;
#84216 = CARTESIAN_POINT('Ctrl Pts',(-18.3943257759869,42.8096191270081,122.760659901221)) ;
#84217 = CARTESIAN_POINT('Ctrl Pts',(-18.5221133593397,42.8195798593643,122.594758697312)) ;
#84218 = CARTESIAN_POINT('Ctrl Pts',(-18.6781228108456,42.8296133217613,122.452804639824)) ;
#84219 = CARTESIAN_POINT('Ctrl Pts',(-18.8536233433113,42.8394988559727,122.341445375326)) ;
#84220 = CARTESIAN_POINT('Ctrl Pts',(-19.0492358229451,42.8495636966527,122.26084028791)) ;
#84221 = CARTESIAN_POINT('Ctrl Pts',(-19.2514442585677,42.8594118283815,122.216302493889)) ;
#84222 = CARTESIAN_POINT('Ctrl Pts',(-19.4620358055281,42.8694393253717,122.206847322742)) ;
#84223 = CARTESIAN_POINT('Ctrl Pts',(-19.6710341574969,42.8794677774167,122.234659846651)) ;
#84224 = CARTESIAN_POINT('Ctrl Pts',(-19.8684540618217,42.8893130439808,122.296792882877)) ;
#84225 = CARTESIAN_POINT('Ctrl Pts',(-20.0550738088005,42.8993037169218,122.393179126527)) ;
#84226 = CARTESIAN_POINT('Ctrl Pts',(-20.2226209396394,42.9093415990102,122.521475164468)) ;
#84227 = CARTESIAN_POINT('Ctrl Pts',(-20.3628676291703,42.9191859694499,122.673680087124)) ;
#84228 = CARTESIAN_POINT('Ctrl Pts',(-20.4764790858517,42.9291707968453,122.850155959111)) ;
#84229 = CARTESIAN_POINT('Ctrl Pts',(-20.5574622870053,42.9391102422506,123.042816232772)) ;
#84230 = CARTESIAN_POINT('Ctrl Pts',(-20.6041616186596,42.9491502465365,123.248636423166)) ;
#84231 = CARTESIAN_POINT('Ctrl Pts',(-20.6144023760936,42.9590373557221,123.456265606785)) ;
#84232 = CARTESIAN_POINT('Ctrl Pts',(-20.5884050697669,42.9690374156246,123.664852246182)) ;
#84233 = CARTESIAN_POINT('Ctrl Pts',(-20.5272465507079,42.9789548315393,123.864211860364)) ;
#84234 = CARTESIAN_POINT('Ctrl Pts',(-20.4311397225098,42.9890016462801,124.052262571585)) ;
#84235 = CARTESIAN_POINT('Ctrl Pts',(-20.3061446771948,42.9988771234767,124.218074771365)) ;
#84236 = CARTESIAN_POINT('Ctrl Pts',(-20.1516108795258,43.008933219198,124.362292449822)) ;
#84237 = CARTESIAN_POINT('Ctrl Pts',(-19.9772349402535,43.018826381213,124.475727085091)) ;
#84238 = CARTESIAN_POINT('Ctrl Pts',(-19.7826262183255,43.0288886172357,124.558584692657)) ;
#84239 = CARTESIAN_POINT('Ctrl Pts',(-19.5810180214014,43.0387330828646,124.605386435808)) ;
#84240 = CARTESIAN_POINT('Ctrl Pts',(-19.3719712696387,43.0486931755687,124.617355627248)) ;
#84241 = CARTESIAN_POINT('Ctrl Pts',(-19.162444446929,43.0587314645498,124.592241353779)) ;
#84242 = CARTESIAN_POINT('Ctrl Pts',(-18.9636256595679,43.068604787656,124.53250285335)) ;
#84243 = CARTESIAN_POINT('Ctrl Pts',(-18.774542404624,43.0786779717411,124.437233832824)) ;
#84244 = CARTESIAN_POINT('Ctrl Pts',(-18.6088995227669,43.088498484029,124.313922050298)) ;
#84245 = CARTESIAN_POINT('Ctrl Pts',(-18.4633850579159,43.0985764801448,124.159993820606)) ;
#84246 = CARTESIAN_POINT('Ctrl Pts',(-18.3493042591805,43.1084305551281,123.987014257358)) ;
#84247 = CARTESIAN_POINT('Ctrl Pts',(-18.2650619365002,43.1184944367118,123.792978328618)) ;
#84248 = CARTESIAN_POINT('Ctrl Pts',(-18.2166935633452,43.1283778626855,123.590869297813)) ;
#84249 = CARTESIAN_POINT('Ctrl Pts',(-18.2036737600321,43.1383784666066,123.381065490452)) ;
#84250 = CARTESIAN_POINT('Ctrl Pts',(-18.226966748946,43.1482982509444,123.173787194636)) ;
#84251 = CARTESIAN_POINT('Ctrl Pts',(-18.286681255959,43.1583456013013,122.97121296391)) ;
#84252 = CARTESIAN_POINT('Ctrl Pts',(-18.3788852089591,43.1682229435356,122.785107675015)) ;
#84253 = CARTESIAN_POINT('Ctrl Pts',(-18.5043642202227,43.1782928246102,122.614654111536)) ;
#84254 = CARTESIAN_POINT('Ctrl Pts',(-18.6537874671552,43.1881225298119,122.471849925775)) ;
#84255 = CARTESIAN_POINT('Ctrl Pts',(-18.8296636074183,43.1981891909783,122.354200223767)) ;
#84256 = CARTESIAN_POINT('Ctrl Pts',(-19.0200097582387,43.2080794128456,122.270467347616)) ;
#84257 = CARTESIAN_POINT('Ctrl Pts',(-19.2239389860699,43.2180715889558,122.220108587182)) ;
#84258 = CARTESIAN_POINT('Ctrl Pts',(-19.4329190392225,43.2280344190684,122.206163569416)) ;
#84259 = CARTESIAN_POINT('Ctrl Pts',(-19.6400002172605,43.2379386314687,122.228059005943)) ;
#84260 = CARTESIAN_POINT('Ctrl Pts',(-19.8432008782305,43.2479993455566,122.286655349108)) ;
#84261 = CARTESIAN_POINT('Ctrl Pts',(-20.0291416113698,43.2578388485394,122.377370325286)) ;
#84262 = CARTESIAN_POINT('Ctrl Pts',(-20.2004350392593,43.2679049871058,122.501580201474)) ;
#84263 = CARTESIAN_POINT('Ctrl Pts',(-20.3448645376767,43.2777875015918,122.65097173677)) ;
#84264 = CARTESIAN_POINT('Ctrl Pts',(-20.4627595418713,43.2877798009473,122.824800722048)) ;
#84265 = CARTESIAN_POINT('Ctrl Pts',(-20.5484179727521,43.2977328679007,123.015743378607)) ;
#84266 = CARTESIAN_POINT('Ctrl Pts',(-20.5999443496352,43.307767576106,123.220298980291)) ;
#84267 = CARTESIAN_POINT('Ctrl Pts',(-20.6151020046759,43.3176557970101,123.427639351467)) ;
#84268 = CARTESIAN_POINT('Ctrl Pts',(-20.5941477370278,43.3276502200406,123.636694552893)) ;
#84269 = CARTESIAN_POINT('Ctrl Pts',(-20.5374094838607,43.3375955594868,123.837931569304)) ;
#84270 = CARTESIAN_POINT('Ctrl Pts',(-20.4469569802207,43.3475429040981,124.02649364133)) ;
#84271 = CARTESIAN_POINT('Ctrl Pts',(-20.3237223272501,43.3575907995091,124.198051257851)) ;
#84272 = CARTESIAN_POINT('Ctrl Pts',(-20.1757015005492,43.3674384449884,124.342795665365)) ;
#84273 = CARTESIAN_POINT('Ctrl Pts',(-20.0031972366942,43.3774001589024,124.46152863281)) ;
#84274 = CARTESIAN_POINT('Ctrl Pts',(-19.8112856932042,43.3874287831934,124.548856656598)) ;
#84275 = CARTESIAN_POINT('Ctrl Pts',(-19.6095733525184,43.3973391438501,124.600973582111)) ;
#84276 = CARTESIAN_POINT('Ctrl Pts',(-19.4013914577083,43.4072738424234,124.617866015945)) ;
#84277 = CARTESIAN_POINT('Ctrl Pts',(-19.1912336801749,43.4173156672776,124.597937770818)) ;
#84278 = CARTESIAN_POINT('Ctrl Pts',(-18.9908383852225,43.427200241022,124.542869334189)) ;
#84279 = CARTESIAN_POINT('Ctrl Pts',(-18.8007562631651,43.4372020903851,124.453033623645)) ;
#84280 = CARTESIAN_POINT('Ctrl Pts',(-18.6304420125934,43.4471213919592,124.332653745502)) ;
#84281 = CARTESIAN_POINT('Ctrl Pts',(-18.4817975922359,43.4571655003045,124.182701661743)) ;
#84282 = CARTESIAN_POINT('Ctrl Pts',(-18.3632946073683,43.4670499237467,124.011990264435)) ;
#84283 = CARTESIAN_POINT('Ctrl Pts',(-18.2746464011047,43.4770662856562,123.82097505322)) ;
#84284 = CARTESIAN_POINT('Ctrl Pts',(-18.2209433721218,43.4871029411616,123.616933241554)) ;
#84285 = CARTESIAN_POINT('Ctrl Pts',(-18.2032793807859,43.4969330713509,123.411004635612)) ;
#84286 = CARTESIAN_POINT('Ctrl Pts',(-18.2220212371663,43.5070091244408,123.20004552969)) ;
#84287 = CARTESIAN_POINT('Ctrl Pts',(-18.2757963342158,43.5168613536266,122.999978140461)) ;
#84288 = CARTESIAN_POINT('Ctrl Pts',(-18.3652659387053,43.5269345614259,122.808072789942)) ;
#84289 = CARTESIAN_POINT('Ctrl Pts',(-18.4839781003294,43.5367760727773,122.638602022809)) ;
#84290 = CARTESIAN_POINT('Ctrl Pts',(-18.6315156170314,43.5467370108148,122.49000026879)) ;
#84291 = CARTESIAN_POINT('Ctrl Pts',(-18.8041793234811,43.5567748727398,122.368686470592)) ;
#84292 = CARTESIAN_POINT('Ctrl Pts',(-18.9920325810589,43.5666490587369,122.280289825011)) ;
#84293 = CARTESIAN_POINT('Ctrl Pts',(-19.1963084092414,43.5767192183147,122.22480654154)) ;
#84294 = CARTESIAN_POINT('Ctrl Pts',(-19.402160991638,43.5865509657406,122.205953810568)) ;
#84295 = CARTESIAN_POINT('Ctrl Pts',(-19.6124556385658,43.5965870458119,122.222937574671)) ;
#84296 = CARTESIAN_POINT('Ctrl Pts',(-19.8161059834079,43.6066040926644,122.276596417447)) ;
#84297 = CARTESIAN_POINT('Ctrl Pts',(-20.0049292669574,43.616486350831,122.363254720361)) ;
#84298 = CARTESIAN_POINT('Ctrl Pts',(-20.1777775708207,43.6264740336273,122.482430150644)) ;
#84299 = CARTESIAN_POINT('Ctrl Pts',(-20.3268505663484,43.6364206903441,122.629119310291)) ;
#84300 = CARTESIAN_POINT('Ctrl Pts',(-20.4493262904899,43.6464777484242,122.801435835122)) ;
#84301 = CARTESIAN_POINT('Ctrl Pts',(-20.5381405147354,43.6562959279737,122.987771873157)) ;
#84302 = CARTESIAN_POINT('Ctrl Pts',(-20.5950205298352,43.6663318624127,123.190941554761)) ;
#84303 = CARTESIAN_POINT('Ctrl Pts',(-20.6151355410255,43.6763565168417,123.400737123359)) ;
#84304 = CARTESIAN_POINT('Ctrl Pts',(-20.5992612062192,43.6862085364212,123.607251304135)) ;
#84305 = CARTESIAN_POINT('Ctrl Pts',(-20.5473617823272,43.6961994501361,123.810752814889)) ;
#84306 = CARTESIAN_POINT('Ctrl Pts',(-20.4616503372551,43.7061174389757,124.000855972249)) ;
#84307 = CARTESIAN_POINT('Ctrl Pts',(-20.3429941356077,43.7161455497065,124.17509706111)) ;
#84308 = CARTESIAN_POINT('Ctrl Pts',(-20.1980312028953,43.7260307476149,124.324012626185)) ;
#84309 = CARTESIAN_POINT('Ctrl Pts',(-20.0279376936583,43.7360200228829,124.447192063469)) ;
#84310 = CARTESIAN_POINT('Ctrl Pts',(-19.8378630861795,43.7460614810524,124.539030414508)) ;
#84311 = CARTESIAN_POINT('Ctrl Pts',(-19.6390701324391,43.7558929448407,124.595638016703)) ;
#84312 = CARTESIAN_POINT('Ctrl Pts',(-19.4299206998209,43.7658978771446,124.617705082745)) ;
#84313 = CARTESIAN_POINT('Ctrl Pts',(-19.2204529465553,43.7758842410393,124.603030014934)) ;
#84314 = CARTESIAN_POINT('Ctrl Pts',(-19.0159260256037,43.7859138699252,124.551840171341)) ;
#84315 = CARTESIAN_POINT('Ctrl Pts',(-18.8262138026566,43.7957890920336,124.467467725213)) ;
#84316 = CARTESIAN_POINT('Ctrl Pts',(-18.6517412402782,43.8057903044307,124.350192701147)) ;
#84317 = CARTESIAN_POINT('Ctrl Pts',(-18.5014974685159,43.8156988836662,124.205849690348)) ;
#84318 = CARTESIAN_POINT('Ctrl Pts',(-18.3768780512125,43.8257537362222,124.035148133203)) ;
#84319 = CARTESIAN_POINT('Ctrl Pts',(-18.2853633379775,43.835612318497,123.849147658235)) ;
#84320 = CARTESIAN_POINT('Ctrl Pts',(-18.2262007825756,43.8456804479396,123.645952411411)) ;
#84321 = CARTESIAN_POINT('Ctrl Pts',(-18.203715267376,43.8555359196287,123.439965697177)) ;
#84322 = CARTESIAN_POINT('Ctrl Pts',(-18.2168996593856,43.865530768015,123.230263427159)) ;
#84323 = CARTESIAN_POINT('Ctrl Pts',(-18.2669194322133,43.8755620647995,123.025387399113)) ;
#84324 = CARTESIAN_POINT('Ctrl Pts',(-18.3500573743321,43.8854286010096,122.835344597124)) ;
#84325 = CARTESIAN_POINT('Ctrl Pts',(-18.4660377743392,43.8954160239704,122.660345771646)) ;
#84326 = CARTESIAN_POINT('Ctrl Pts',(-18.6099846193016,43.9053609629902,122.508677841172)) ;
#84327 = CARTESIAN_POINT('Ctrl Pts',(-18.7797941717303,43.9154058488502,122.383164608696)) ;
#84328 = CARTESIAN_POINT('Ctrl Pts',(-18.9654667340032,43.9252743839364,122.290585232131)) ;
#84329 = CARTESIAN_POINT('Ctrl Pts',(-19.1661752384791,43.9352402519431,122.230514467672)) ;
#84330 = CARTESIAN_POINT('Ctrl Pts',(-19.3755016092463,43.9452628993956,122.206300298723)) ;
#84331 = CARTESIAN_POINT('Ctrl Pts',(-19.583752931223,43.9551865384032,122.218617120769)) ;
#84332 = CARTESIAN_POINT('Ctrl Pts',(-19.7872305258696,43.9651292634089,122.266516179803)) ;
#84333 = CARTESIAN_POINT('Ctrl Pts',(-19.9811657967004,43.9751748694608,122.350095113591)) ;
#84334 = CARTESIAN_POINT('Ctrl Pts',(-20.1545571070679,43.9850362919819,122.463777119903)) ;
#84335 = CARTESIAN_POINT('Ctrl Pts',(-20.3078102053902,43.9950298604311,122.607448060503)) ;
#84336 = CARTESIAN_POINT('Ctrl Pts',(-20.4330542345469,44.0049553311864,122.774384345054)) ;
#84337 = CARTESIAN_POINT('Ctrl Pts',(-20.5283647722935,44.0149830051423,122.962392956857)) ;
#84338 = CARTESIAN_POINT('Ctrl Pts',(-20.588933840108,44.0248701831839,123.161260937744)) ;
#84339 = CARTESIAN_POINT('Ctrl Pts',(-20.6145511580893,44.0348985625521,123.37049929144)) ;
#84340 = CARTESIAN_POINT('Ctrl Pts',(-20.6037082962981,44.0447928052736,123.578247921938)) ;
#84341 = CARTESIAN_POINT('Ctrl Pts',(-20.5408575074722,44.0581457219245,123.851835509504)) ;
#84342 = CARTESIAN_POINT('Ctrl Pts',(-20.4095228682182,44.0713482396712,124.100006403082)) ;
#84343 = CARTESIAN_POINT('Ctrl Pts',(-20.2186591011258,44.0847041449522,124.305849465822)) ;
#84344 = CARTESIAN_POINT('Ctrl Pts',(-20.0529407671226,44.09460079359,124.431709382734)) ;
#84345 = CARTESIAN_POINT('Ctrl Pts',(-19.865133373299,44.1046489316425,124.528373373342)) ;
#84346 = CARTESIAN_POINT('Ctrl Pts',(-19.6665214872006,44.1145398918202,124.589983507587)) ;
#84347 = CARTESIAN_POINT('Ctrl Pts',(-19.4581739575967,44.124532727697,124.616965016942)) ;
#84348 = CARTESIAN_POINT('Ctrl Pts',(-19.2473737978853,44.1345718226986,124.606831455382)) ;
#84349 = CARTESIAN_POINT('Ctrl Pts',(-19.0455363706327,44.1444091785497,124.561650521355)) ;
#84350 = CARTESIAN_POINT('Ctrl Pts',(-18.7855906137243,44.1578021264805,124.453535581331)) ;
#84351 = CARTESIAN_POINT('Ctrl Pts',(-18.5635140073878,44.1709688029074,124.282902241153)) ;
#84352 = CARTESIAN_POINT('Ctrl Pts',(-18.3921555813385,44.1843535843142,124.059820793974)) ;
#84353 = CARTESIAN_POINT('Ctrl Pts',(-18.2962312056799,44.194215366958,123.875972393078)) ;
#84354 = CARTESIAN_POINT('Ctrl Pts',(-18.2325177147997,44.2042145149111,123.67569306529)) ;
#84355 = CARTESIAN_POINT('Ctrl Pts',(-18.2046131479773,44.2141173075282,123.469337303131)) ;
#84356 = CARTESIAN_POINT('Ctrl Pts',(-18.213138129981,44.2241668874191,123.258291526556)) ;
#84357 = CARTESIAN_POINT('Ctrl Pts',(-18.2717479171345,44.2373539612286,122.987197784556)) ;
#84358 = CARTESIAN_POINT('Ctrl Pts',(-18.4346577722479,44.2541067511998,122.670626830962)) ;
#84359 = CARTESIAN_POINT('Ctrl Pts',(-18.6920466309599,44.2705954032945,122.432275015599)) ;
#84360 = CARTESIAN_POINT('Ctrl Pts',(-18.9400674710734,44.2839522294779,122.300862352034)) ;
#84361 = CARTESIAN_POINT('Ctrl Pts',(-19.138050968932,44.2938486143558,122.236740395541)) ;
#84362 = CARTESIAN_POINT('Ctrl Pts',(-19.3463245926845,44.3038551288763,122.207560046898)) ;
#84363 = CARTESIAN_POINT('Ctrl Pts',(-19.6235857637495,44.3170452523927,122.216668886464)) ;
#84364 = CARTESIAN_POINT('Ctrl Pts',(-19.9644817452573,44.3338118135422,122.320510300557)) ;
#84365 = CARTESIAN_POINT('Ctrl Pts',(-20.3009628630552,44.3535963022503,122.573194318011)) ;
#84366 = CARTESIAN_POINT('Ctrl Pts',(-20.5338593298856,44.3735417498468,122.927488552972)) ;
#84367 = CARTESIAN_POINT('Ctrl Pts',(-20.6313432869638,44.3934534120027,123.339498229976)) ;
#84368 = CARTESIAN_POINT('Ctrl Pts',(-20.5833486351149,44.4133456040216,123.759794081848)) ;
#84369 = CARTESIAN_POINT('Ctrl Pts',(-20.3928831894929,44.4333867345762,124.140920711645)) ;
#84370 = CARTESIAN_POINT('Ctrl Pts',(-20.0872651790941,44.4532050691918,124.43118843213)) ;
#84371 = CARTESIAN_POINT('Ctrl Pts',(-19.6984334120506,44.4731776344114,124.601580084721)) ;
#84372 = CARTESIAN_POINT('Ctrl Pts',(-19.2762688089198,44.493066850583,124.629069320153)) ;
#84373 = CARTESIAN_POINT('Ctrl Pts',(-18.8676588274966,44.5130904249057,124.509843418797)) ;
#84374 = CARTESIAN_POINT('Ctrl Pts',(-18.5278180218302,44.5328875879939,124.261320788567)) ;
#84375 = CARTESIAN_POINT('Ctrl Pts',(-18.2904318127847,44.5528530818177,123.909483353914)) ;
#84376 = CARTESIAN_POINT('Ctrl Pts',(-18.1878781245095,44.5728067895591,123.497677772688)) ;
#84377 = CARTESIAN_POINT('Ctrl Pts',(-18.2318637933429,44.5927141662857,123.076780022158)) ;
#84378 = CARTESIAN_POINT('Ctrl Pts',(-18.4153836924114,44.6125663778343,122.696570163402)) ;
#84379 = CARTESIAN_POINT('Ctrl Pts',(-18.721213427716,44.63263876478,122.398901462891)) ;
#84380 = CARTESIAN_POINT('Ctrl Pts',(-19.1059665362462,44.6524766344203,122.226015016883)) ;
#84381 = CARTESIAN_POINT('Ctrl Pts',(-19.5267471287715,44.6723272889734,122.192956241741)) ;
#84382 = CARTESIAN_POINT('Ctrl Pts',(-19.9374777977326,44.6923792233138,122.307204924401)) ;
#84383 = CARTESIAN_POINT('Ctrl Pts',(-20.2808528712217,44.7122124108799,122.552178876658)) ;
#84384 = CARTESIAN_POINT('Ctrl Pts',(-20.5217265853229,44.7321416231106,122.900618651357)) ;
#84385 = CARTESIAN_POINT('Ctrl Pts',(-20.6295648496897,44.752026588325,123.309611273299)) ;
#84386 = CARTESIAN_POINT('Ctrl Pts',(-20.5903665879315,44.7721003294696,123.734542133322)) ;
#84387 = CARTESIAN_POINT('Ctrl Pts',(-20.4110379245902,44.79189351125,124.115354659194)) ;
#84388 = CARTESIAN_POINT('Ctrl Pts',(-20.1109493954123,44.8118562192527,124.41549537119)) ;
#84389 = CARTESIAN_POINT('Ctrl Pts',(-19.7255903117033,44.8318391709951,124.594483377586)) ;
#84390 = CARTESIAN_POINT('Ctrl Pts',(-19.3059767207478,44.8516497907673,124.631738883303)) ;
#84391 = CARTESIAN_POINT('Ctrl Pts',(-18.8952790350949,44.8716335068002,124.523139946406)) ;
#84392 = CARTESIAN_POINT('Ctrl Pts',(-18.5479537981365,44.8915149706975,124.28197876055)) ;
#84393 = CARTESIAN_POINT('Ctrl Pts',(-18.302732820425,44.9114703005419,123.935816472258)) ;
#84394 = CARTESIAN_POINT('Ctrl Pts',(-18.1904707648224,44.9313457613473,123.528324077861)) ;
#84395 = CARTESIAN_POINT('Ctrl Pts',(-18.2239253980212,44.9513300813989,123.104770271589)) ;
#84396 = CARTESIAN_POINT('Ctrl Pts',(-18.3996904016786,44.9712581141885,122.719111274452)) ;
#84397 = CARTESIAN_POINT('Ctrl Pts',(-18.6468965811825,44.9878668761283,122.467052957218)) ;
#84398 = CARTESIAN_POINT('Ctrl Pts',(-18.885415024673,45.0010545148184,122.325643231264)) ;
#84399 = CARTESIAN_POINT('Ctrl Pts',(-19.0816687636844,45.0110409491785,122.251110513577)) ;
#84400 = CARTESIAN_POINT('Ctrl Pts',(-19.2884343852017,45.0210503231378,122.211902199266)) ;
#84401 = CARTESIAN_POINT('Ctrl Pts',(-19.5677616357913,45.0343403567031,122.208107593301)) ;
#84402 = CARTESIAN_POINT('Ctrl Pts',(-19.9099464874213,45.0509343443656,122.29446682086)) ;
#84403 = CARTESIAN_POINT('Ctrl Pts',(-20.2026694566148,45.0675665996411,122.492797279563)) ;
#84404 = CARTESIAN_POINT('Ctrl Pts',(-20.384991023903,45.080808983309,122.703234497855)) ;
#84405 = CARTESIAN_POINT('Ctrl Pts',(-20.4925937355116,45.0907231915364,122.881741621572)) ;
#84406 = CARTESIAN_POINT('Ctrl Pts',(-20.568416740875,45.1007798308081,123.07908485721)) ;
#84407 = CARTESIAN_POINT('Ctrl Pts',(-20.6082256043889,45.1106256372282,123.282226390095)) ;
#84408 = CARTESIAN_POINT('Ctrl Pts',(-20.612596696362,45.1206706368614,123.493357737852)) ;
#84409 = CARTESIAN_POINT('Ctrl Pts',(-20.5694219253255,45.1339516592341,123.769153352634)) ;
#84410 = CARTESIAN_POINT('Ctrl Pts',(-20.4566672380709,45.1471491057588,124.026150825483)) ;
#84411 = CARTESIAN_POINT('Ctrl Pts',(-20.280126516246,45.1605634035657,124.246100642346)) ;
#84412 = CARTESIAN_POINT('Ctrl Pts',(-20.1246823586444,45.1704024689685,124.382580114351)) ;
#84413 = CARTESIAN_POINT('Ctrl Pts',(-19.9456254623816,45.1803856752462,124.49202682819)) ;
#84414 = CARTESIAN_POINT('Ctrl Pts',(-19.7508537829088,45.190336910159,124.568420987033)) ;
#84415 = CARTESIAN_POINT('Ctrl Pts',(-19.5448027598535,45.2003379098606,124.610291845591)) ;
#84416 = CARTESIAN_POINT('Ctrl Pts',(-19.3339774210853,45.2103692556479,124.615434704807)) ;
#84417 = CARTESIAN_POINT('Ctrl Pts',(-19.1291027096562,45.220223020353,124.58473277515)) ;
#84418 = CARTESIAN_POINT('Ctrl Pts',(-18.9302085771127,45.2301936740213,124.518626237724)) ;
#84419 = CARTESIAN_POINT('Ctrl Pts',(-18.7452783058747,45.2401909176785,124.418690904311)) ;
#84420 = CARTESIAN_POINT('Ctrl Pts',(-18.5801193737719,45.2502243736227,124.287508830628)) ;
#84421 = CARTESIAN_POINT('Ctrl Pts',(-18.4424514372433,45.2600798779231,124.13263744952)) ;
#84422 = CARTESIAN_POINT('Ctrl Pts',(-18.3319695805143,45.2700793142092,123.953834867365)) ;
#84423 = CARTESIAN_POINT('Ctrl Pts',(-18.2547793585316,45.2799737737251,123.760632288585)) ;
#84424 = CARTESIAN_POINT('Ctrl Pts',(-18.2116609512092,45.2900368931767,123.553551735828)) ;
#84425 = CARTESIAN_POINT('Ctrl Pts',(-18.2050676042058,45.2998765275887,123.346762433404)) ;
#84426 = CARTESIAN_POINT('Ctrl Pts',(-18.2348732954205,45.3099397350745,123.13734193917)) ;
#84427 = CARTESIAN_POINT('Ctrl Pts',(-18.299665433266,45.3198338424537,122.93966000259)) ;
#84428 = CARTESIAN_POINT('Ctrl Pts',(-18.3977574508029,45.3297761746461,122.75511979076)) ;
#84429 = CARTESIAN_POINT('Ctrl Pts',(-18.5271124110106,45.3397768009611,122.589336702802)) ;
#84430 = CARTESIAN_POINT('Ctrl Pts',(-18.6841544889452,45.349818535243,122.448281249036)) ;
#84431 = CARTESIAN_POINT('Ctrl Pts',(-18.8592295883591,45.3596439611921,122.338633546838)) ;
#84432 = CARTESIAN_POINT('Ctrl Pts',(-19.0550454530649,45.3697007877197,122.258943893974)) ;
#84433 = CARTESIAN_POINT('Ctrl Pts',(-19.2591518279753,45.3796282208413,122.215318487918)) ;
#84434 = CARTESIAN_POINT('Ctrl Pts',(-19.468181276108,45.3895782132475,122.20718013329)) ;
#84435 = CARTESIAN_POINT('Ctrl Pts',(-19.6775673120917,45.3996334143215,122.236125936073)) ;
#84436 = CARTESIAN_POINT('Ctrl Pts',(-19.8742295194565,45.4094556883738,122.299140356534)) ;
#84437 = CARTESIAN_POINT('Ctrl Pts',(-20.061457560878,45.4195115823331,122.397284056323)) ;
#84438 = CARTESIAN_POINT('Ctrl Pts',(-20.2266741638109,45.4294523041782,122.52527460033)) ;
#84439 = CARTESIAN_POINT('Ctrl Pts',(-20.3671232504393,45.4393566482648,122.678999529168)) ;
#84440 = CARTESIAN_POINT('Ctrl Pts',(-20.4802264787038,45.4494033155643,122.857355769901)) ;
#84441 = CARTESIAN_POINT('Ctrl Pts',(-20.5596285804351,45.4592988740142,123.04967868684)) ;
#84442 = CARTESIAN_POINT('Ctrl Pts',(-20.6051710365697,45.4693609527189,123.256223873825)) ;
#84443 = CARTESIAN_POINT('Ctrl Pts',(-20.6140833446175,45.4792036511847,123.462979287271)) ;
#84444 = CARTESIAN_POINT('Ctrl Pts',(-20.5870525350675,45.4891944250792,123.671243809474)) ;
#84445 = CARTESIAN_POINT('Ctrl Pts',(-20.5246209778266,45.4991222943141,123.870412109524)) ;
#84446 = CARTESIAN_POINT('Ctrl Pts',(-20.4282957886132,45.5091110232839,124.057023148898)) ;
#84447 = CARTESIAN_POINT('Ctrl Pts',(-20.3000887267814,45.5191504252677,124.224668111442)) ;
#84448 = CARTESIAN_POINT('Ctrl Pts',(-20.1480643821402,45.5289905930044,124.364985804919)) ;
#84449 = CARTESIAN_POINT('Ctrl Pts',(-19.9704897783103,45.5390388033789,124.479388559856)) ;
#84450 = CARTESIAN_POINT('Ctrl Pts',(-19.7775671836577,45.5489859736667,124.560097142958)) ;
#84451 = CARTESIAN_POINT('Ctrl Pts',(-19.5744414701754,45.5588968219218,124.606523876973)) ;
#84452 = CARTESIAN_POINT('Ctrl Pts',(-19.3632945131307,45.5689531495995,124.616929810979)) ;
#84453 = CARTESIAN_POINT('Ctrl Pts',(-19.1577990571512,45.5788035623681,124.591231951628)) ;
#84454 = CARTESIAN_POINT('Ctrl Pts',(-18.9562025286816,45.5888304482018,124.529644846341)) ;
#84455 = CARTESIAN_POINT('Ctrl Pts',(-18.7685671889028,45.5988590638326,124.433479707402)) ;
#84456 = CARTESIAN_POINT('Ctrl Pts',(-18.6033345097439,45.6087042872101,124.308847799277)) ;
#84457 = CARTESIAN_POINT('Ctrl Pts',(-18.4597435271059,45.6186949693117,124.155554328125)) ;
#84458 = CARTESIAN_POINT('Ctrl Pts',(-18.3448064911182,45.6287328579441,123.978575656932)) ;
#84459 = CARTESIAN_POINT('Ctrl Pts',(-18.2635978094481,45.6385771930473,123.788206651437)) ;
#84460 = CARTESIAN_POINT('Ctrl Pts',(-18.215612918174,45.6485621552448,123.583878844602)) ;
#84461 = CARTESIAN_POINT('Ctrl Pts',(-18.2037886155601,45.6585010967782,123.37523545725)) ;
#84462 = CARTESIAN_POINT('Ctrl Pts',(-18.2286862705219,45.6685429817496,123.16561689975)) ;
#84463 = CARTESIAN_POINT('Ctrl Pts',(-18.2885437879519,45.6784295296579,122.966555275257)) ;
#84464 = CARTESIAN_POINT('Ctrl Pts',(-18.3827734140441,45.6884234551579,122.778797314709)) ;
#84465 = CARTESIAN_POINT('Ctrl Pts',(-18.5074028980685,45.6983595462843,122.6111225881)) ;
#84466 = CARTESIAN_POINT('Ctrl Pts',(-18.6606617579988,45.7083888152643,122.466359772254)) ;
#84467 = CARTESIAN_POINT('Ctrl Pts',(-18.834052688656,45.7182711978236,122.351852188486)) ;
#84468 = CARTESIAN_POINT('Ctrl Pts',(-19.0278880707733,45.7283237149114,122.267728229744)) ;
#84469 = CARTESIAN_POINT('Ctrl Pts',(-19.2301906235251,45.7382178357354,122.219193860073)) ;
#84470 = CARTESIAN_POINT('Ctrl Pts',(-19.4413039395695,45.7482798151558,122.206261137265)) ;
#84471 = CARTESIAN_POINT('Ctrl Pts',(-19.6469492061947,45.7581243483847,122.229642983626)) ;
#84472 = CARTESIAN_POINT('Ctrl Pts',(-19.847942922004,45.768084427291,122.288339198138)) ;
#84473 = CARTESIAN_POINT('Ctrl Pts',(-20.0369764458074,45.7781227038636,122.382139593977)) ;
#84474 = CARTESIAN_POINT('Ctrl Pts',(-20.2043294583818,45.7879960904014,122.504984319071)) ;
#84475 = CARTESIAN_POINT('Ctrl Pts',(-20.3506163202273,45.7980690331685,122.658044794021)) ;
#84476 = CARTESIAN_POINT('Ctrl Pts',(-20.4654246764655,45.8078904472968,122.829707697927)) ;
#84477 = CARTESIAN_POINT('Ctrl Pts',(-20.5510305730476,45.8179650773691,123.023395222281)) ;
#84478 = CARTESIAN_POINT('Ctrl Pts',(-20.6005900658558,45.827831714686,123.224841812656)) ;
#84479 = CARTESIAN_POINT('Ctrl Pts',(-20.6151763356349,45.8378552600578,123.435053208665)) ;
#84480 = CARTESIAN_POINT('Ctrl Pts',(-20.592528635638,45.847881011575,123.644618732393)) ;
#84481 = CARTESIAN_POINT('Ctrl Pts',(-20.5351846913682,45.8577345985843,123.843665085029)) ;
#84482 = CARTESIAN_POINT('Ctrl Pts',(-20.4435052217378,45.8677115588123,124.032319507282)) ;
#84483 = CARTESIAN_POINT('Ctrl Pts',(-20.3196371636077,45.8777327018408,124.202720700626)) ;
#84484 = CARTESIAN_POINT('Ctrl Pts',(-20.1704222805544,45.8876153078607,124.347330375355)) ;
#84485 = CARTESIAN_POINT('Ctrl Pts',(-19.9951347291686,45.8976837784934,124.465921431324)) ;
#84486 = CARTESIAN_POINT('Ctrl Pts',(-19.8065276112628,45.9075138616771,124.550478460805)) ;
#84487 = CARTESIAN_POINT('Ctrl Pts',(-19.6014167263255,45.9175804213574,124.602468015969)) ;
#84488 = CARTESIAN_POINT('Ctrl Pts',(-19.3940227475724,45.9274706711867,124.61765622834)) ;
#84489 = CARTESIAN_POINT('Ctrl Pts',(-19.1850008925533,45.9374628369355,124.596848271941)) ;
#84490 = CARTESIAN_POINT('Ctrl Pts',(-18.9834082274553,45.9474256805316,124.540036386113)) ;
#84491 = CARTESIAN_POINT('Ctrl Pts',(-18.7956023361387,45.9573298493593,124.450088171428)) ;
#84492 = CARTESIAN_POINT('Ctrl Pts',(-18.6237362733502,45.9673907242537,124.326851238018)) ;
#84493 = CARTESIAN_POINT('Ctrl Pts',(-18.4788922942551,45.977229627583,124.179140512665)) ;
#84494 = CARTESIAN_POINT('Ctrl Pts',(-18.359037504779,45.9872980039569,124.004715589726)) ;
#84495 = CARTESIAN_POINT('Ctrl Pts',(-18.2729630369527,45.9971786205896,123.815633475423)) ;
#84496 = CARTESIAN_POINT('Ctrl Pts',(-18.22005104732,46.0071697808186,123.612393236317)) ;
#84497 = CARTESIAN_POINT('Ctrl Pts',(-18.2032574682917,46.0171228542507,123.403791948476)) ;
#84498 = CARTESIAN_POINT('Ctrl Pts',(-18.2231668439234,46.0271586898633,123.193765792517)) ;
#84499 = CARTESIAN_POINT('Ctrl Pts',(-18.278298274426,46.0370488165935,122.993273294469)) ;
#84500 = CARTESIAN_POINT('Ctrl Pts',(-18.3680085315035,46.0470409983628,122.803337401315)) ;
#84501 = CARTESIAN_POINT('Ctrl Pts',(-18.48883758189,46.0569869383372,122.632688949944)) ;
#84502 = CARTESIAN_POINT('Ctrl Pts',(-18.6371890134999,46.0669341220967,122.485284985213)) ;
#84503 = CARTESIAN_POINT('Ctrl Pts',(-18.8107407202325,46.076982060387,122.364873623863)) ;
#84504 = CARTESIAN_POINT('Ctrl Pts',(-18.9986732432391,46.0868296952006,122.278026559726)) ;
#84505 = CARTESIAN_POINT('Ctrl Pts',(-19.2009700027035,46.0967914088986,122.223885449461)) ;
#84506 = CARTESIAN_POINT('Ctrl Pts',(-19.411042470006,46.1068200447197,122.205834191344)) ;
#84507 = CARTESIAN_POINT('Ctrl Pts',(-19.6185632505069,46.1167303594715,122.224242554186)) ;
#84508 = CARTESIAN_POINT('Ctrl Pts',(-19.8203927501633,46.1266652301342,122.278012310979)) ;
#84509 = CARTESIAN_POINT('Ctrl Pts',(-20.0117474066158,46.1367064125359,122.367127720079)) ;
#84510 = CARTESIAN_POINT('Ctrl Pts',(-20.1821838321545,46.1465933840007,122.486134507027)) ;
#84511 = CARTESIAN_POINT('Ctrl Pts',(-20.3311988089654,46.1565928162633,122.634375530162)) ;
#84512 = CARTESIAN_POINT('Ctrl Pts',(-20.4513952266997,46.1665128815199,122.804835876269)) ;
#84513 = CARTESIAN_POINT('Ctrl Pts',(-20.5412360542906,46.1765497341041,122.995747933808)) ;
#84514 = CARTESIAN_POINT('Ctrl Pts',(-20.59587728788,46.186462393444,123.196855992653)) ;
#84515 = CARTESIAN_POINT('Ctrl Pts',(-20.6153750507368,46.1964536053589,123.406008416068)) ;
#84516 = CARTESIAN_POINT('Ctrl Pts',(-20.5977036062115,46.2064952467621,123.616357743328)) ;
#84517 = CARTESIAN_POINT('Ctrl Pts',(-20.5454116592005,46.2163240409691,123.816292436209)) ;
#84518 = CARTESIAN_POINT('Ctrl Pts',(-20.4571378572033,46.2264004520904,124.008815850834)) ;
#84519 = CARTESIAN_POINT('Ctrl Pts',(-20.339495499964,46.2362525851328,124.179339841369)) ;
#84520 = CARTESIAN_POINT('Ctrl Pts',(-20.1909503583246,46.2463258194742,124.330227020492)) ;
#84521 = CARTESIAN_POINT('Ctrl Pts',(-20.022359060117,46.2561673208008,124.450184743589)) ;
#84522 = CARTESIAN_POINT('Ctrl Pts',(-19.8335905201032,46.2661282723956,124.540828601706)) ;
#84523 = CARTESIAN_POINT('Ctrl Pts',(-19.6302804392769,46.2761660901162,124.597348545521)) ;
#84524 = CARTESIAN_POINT('Ctrl Pts',(-19.4236714780948,46.2860404393733,124.617764022101)) ;
#84525 = CARTESIAN_POINT('Ctrl Pts',(-19.2126193295471,46.2961099901155,124.601674273063)) ;
#84526 = CARTESIAN_POINT('Ctrl Pts',(-19.0122872962936,46.3059440096241,124.550514499661)) ;
#84527 = CARTESIAN_POINT('Ctrl Pts',(-18.8198464982895,46.3159781642036,124.46413465279)) ;
#84528 = CARTESIAN_POINT('Ctrl Pts',(-18.6459181761566,46.3259940900261,124.345423519706)) ;
#84529 = CARTESIAN_POINT('Ctrl Pts',(-18.4970009615531,46.3358763452203,124.200552798175)) ;
#84530 = CARTESIAN_POINT('Ctrl Pts',(-18.3739944708057,46.3458651517313,124.030382105074)) ;
#84531 = CARTESIAN_POINT('Ctrl Pts',(-18.2826050981716,46.355813718994,123.842218558594)) ;
#84532 = CARTESIAN_POINT('Ctrl Pts',(-18.2248950683396,46.365868524296,123.638888671338)) ;
#84533 = CARTESIAN_POINT('Ctrl Pts',(-18.2035713060587,46.3756873075596,123.433561300174)) ;
#84534 = CARTESIAN_POINT('Ctrl Pts',(-18.2179813445457,46.3857230799201,123.223075302304)) ;
#84535 = CARTESIAN_POINT('Ctrl Pts',(-18.2692515878222,46.3957477789488,123.018648166375)) ;
#84536 = CARTESIAN_POINT('Ctrl Pts',(-18.3533370689887,46.4055997822079,122.829360936852)) ;
#84537 = CARTESIAN_POINT('Ctrl Pts',(-18.4703613694233,46.4155907166051,122.654971104637)) ;
#84538 = CARTESIAN_POINT('Ctrl Pts',(-18.6147606329656,46.4255086390362,122.504524558652)) ;
#84539 = CARTESIAN_POINT('Ctrl Pts',(-18.7849011229507,46.4355369947185,122.380053429102)) ;
#84540 = CARTESIAN_POINT('Ctrl Pts',(-18.9713293231097,46.4454212792291,122.28824983603)) ;
#84541 = CARTESIAN_POINT('Ctrl Pts',(-19.1729140858886,46.455413963137,122.229120010516)) ;
#84542 = CARTESIAN_POINT('Ctrl Pts',(-19.3824991228755,46.4654427001447,122.206173308855)) ;
#84543 = CARTESIAN_POINT('Ctrl Pts',(-19.5899010964574,46.4753280967736,122.219495009534)) ;
#84544 = CARTESIAN_POINT('Ctrl Pts',(-19.7939762357025,46.4853159821875,122.268837874836)) ;
#84545 = CARTESIAN_POINT('Ctrl Pts',(-19.9857528123901,46.4952666848481,122.352485219102)) ;
#84546 = CARTESIAN_POINT('Ctrl Pts',(-20.1615560713129,46.5053070029455,122.469269470923)) ;
#84547 = CARTESIAN_POINT('Ctrl Pts',(-20.312061766034,46.5151815682787,122.612283972297)) ;
#84548 = CARTESIAN_POINT('Ctrl Pts',(-20.4371930749062,46.5251812283398,122.781168558307)) ;
#84549 = CARTESIAN_POINT('Ctrl Pts',(-20.5304591793014,46.5350902235075,122.967483463169)) ;
#84550 = CARTESIAN_POINT('Ctrl Pts',(-20.5907489828305,46.5451449646707,123.170049998762)) ;
#84551 = CARTESIAN_POINT('Ctrl Pts',(-20.6147246473763,46.5550035765845,123.37595414604)) ;
#84552 = CARTESIAN_POINT('Ctrl Pts',(-20.6024582716505,46.5650716988639,123.587231213569)) ;
#84553 = CARTESIAN_POINT('Ctrl Pts',(-20.5546964518429,46.5749271695671,123.788861895035)) ;
#84554 = CARTESIAN_POINT('Ctrl Pts',(-20.4720783495954,46.5849220290604,123.982053985397)) ;
#84555 = CARTESIAN_POINT('Ctrl Pts',(-20.3563663950888,46.5949532824024,124.15836793779)) ;
#84556 = CARTESIAN_POINT('Ctrl Pts',(-20.2144077351763,46.6048199812755,124.309619911489)) ;
#84557 = CARTESIAN_POINT('Ctrl Pts',(-20.0465524126368,46.6148067970267,124.435697555555)) ;
#84558 = CARTESIAN_POINT('Ctrl Pts',(-19.8600955779439,46.6247540022221,124.530446736084)) ;
#84559 = CARTESIAN_POINT('Ctrl Pts',(-19.658107114407,46.6347969903484,124.591866563251)) ;
#84560 = CARTESIAN_POINT('Ctrl Pts',(-19.4521805478414,46.6446643449699,124.616961781733)) ;
#84561 = CARTESIAN_POINT('Ctrl Pts',(-19.2429425710295,46.654630238268,124.606374914884)) ;
#84562 = CARTESIAN_POINT('Ctrl Pts',(-19.0375622495762,46.6646540156441,124.559128817244)) ;
#84563 = CARTESIAN_POINT('Ctrl Pts',(-18.8454096947828,46.6745795635758,124.477797817512)) ;
#84564 = CARTESIAN_POINT('Ctrl Pts',(-18.669747000263,46.6845200399968,124.364570074209)) ;
#84565 = CARTESIAN_POINT('Ctrl Pts',(-18.5149640442547,46.6945662496597,124.220891203878)) ;
#84566 = CARTESIAN_POINT('Ctrl Pts',(-18.3896311544296,46.7044275063215,124.055728940118)) ;
#84567 = CARTESIAN_POINT('Ctrl Pts',(-18.2933092985916,46.7144211345968,123.869046552226)) ;
#84568 = CARTESIAN_POINT('Ctrl Pts',(-18.2311685573197,46.724346531907,123.669818227534)) ;
#84569 = CARTESIAN_POINT('Ctrl Pts',(-18.2042912868287,46.7343744398172,123.460747783017)) ;
#84570 = CARTESIAN_POINT('Ctrl Pts',(-18.2137735619061,46.7442607554864,123.253092008572)) ;
#84571 = CARTESIAN_POINT('Ctrl Pts',(-18.2597106116491,46.7542923503902,123.047294541768)) ;
#84572 = CARTESIAN_POINT('Ctrl Pts',(-18.3393267948155,46.7641745933419,122.855362781302)) ;
#84573 = CARTESIAN_POINT('Ctrl Pts',(-18.4529567609936,46.7742340643717,122.677029439703)) ;
#84574 = CARTESIAN_POINT('Ctrl Pts',(-18.5931277415802,46.7841005090349,122.524119542989)) ;
#84575 = CARTESIAN_POINT('Ctrl Pts',(-18.7589660899219,46.7940666334836,122.396081360997)) ;
#84576 = CARTESIAN_POINT('Ctrl Pts',(-18.9458707343078,46.8040968768747,122.298455537853)) ;
#84577 = CARTESIAN_POINT('Ctrl Pts',(-19.1440685456171,46.8139899118278,122.235347192875)) ;
#84578 = CARTESIAN_POINT('Ctrl Pts',(-19.353458752379,46.8240408260646,122.207116932518)) ;
#84579 = CARTESIAN_POINT('Ctrl Pts',(-19.5612106214837,46.8339306522892,122.215512469215)) ;
#84580 = CARTESIAN_POINT('Ctrl Pts',(-19.8352624788568,46.8472654673361,122.274762009686)) ;
#84581 = CARTESIAN_POINT('Ctrl Pts',(-20.0862026626761,46.8605425585076,122.404067043679)) ;
#84582 = CARTESIAN_POINT('Ctrl Pts',(-20.2927726621347,46.8737908471059,122.590867832793)) ;
#84583 = CARTESIAN_POINT('Ctrl Pts',(-20.4224375530319,46.8838456885999,122.757782588646)) ;
#84584 = CARTESIAN_POINT('Ctrl Pts',(-20.5192876968314,46.8936766779075,122.940402665893)) ;
#84585 = CARTESIAN_POINT('Ctrl Pts',(-20.5846756847044,46.9037532422307,123.141863683039)) ;
#84586 = CARTESIAN_POINT('Ctrl Pts',(-20.6134306387111,46.9136025673647,123.346938432967)) ;
#84587 = CARTESIAN_POINT('Ctrl Pts',(-20.6042235799873,46.9269505670019,123.627443340569)) ;
#84588 = CARTESIAN_POINT('Ctrl Pts',(-20.5014828829124,46.9435353265385,123.964713423941)) ;
#84589 = CARTESIAN_POINT('Ctrl Pts',(-20.2906566355743,46.9601038778866,124.2470189635)) ;
#84590 = CARTESIAN_POINT('Ctrl Pts',(-20.0699818080453,46.9734637027056,124.420721815992)) ;
#84591 = CARTESIAN_POINT('Ctrl Pts',(-19.8865380012834,46.9833691115362,124.51931119778)) ;
#84592 = CARTESIAN_POINT('Ctrl Pts',(-19.6878068412282,46.9933291381203,124.585185778078)) ;
#84593 = CARTESIAN_POINT('Ctrl Pts',(-19.4120461780084,47.0065867223056,124.62597415739)) ;
#84594 = CARTESIAN_POINT('Ctrl Pts',(-19.0603318090092,47.0232379338003,124.585529981602)) ;
#84595 = CARTESIAN_POINT('Ctrl Pts',(-18.6814960970596,47.0431561479106,124.396231532548)) ;
#84596 = CARTESIAN_POINT('Ctrl Pts',(-18.3898810922891,47.0630339111314,124.090210992981)) ;
#84597 = CARTESIAN_POINT('Ctrl Pts',(-18.2194529069462,47.0830465789186,123.700392596067)) ;
#84598 = CARTESIAN_POINT('Ctrl Pts',(-18.1921466433378,47.1028591015852,123.279930301551)) ;
#84599 = CARTESIAN_POINT('Ctrl Pts',(-18.3102874267524,47.1228424015851,122.871872118256)) ;
#84600 = CARTESIAN_POINT('Ctrl Pts',(-18.5598052667018,47.1427366786864,122.530215788296)) ;
#84601 = CARTESIAN_POINT('Ctrl Pts',(-18.9111816446954,47.1626694404441,122.293251063936)) ;
#84602 = CARTESIAN_POINT('Ctrl Pts',(-19.3230996718903,47.1826354462089,122.190530008854)) ;
#84603 = CARTESIAN_POINT('Ctrl Pts',(-19.7435526621383,47.2025139783737,122.234047576491)) ;
#84604 = CARTESIAN_POINT('Ctrl Pts',(-20.1251992562022,47.2224536450341,122.418602153129)) ;
#84605 = CARTESIAN_POINT('Ctrl Pts',(-20.4204439982056,47.2423485196794,122.721609107295)) ;
#84606 = CARTESIAN_POINT('Ctrl Pts',(-20.5949958913168,47.2622556589728,123.107115801826)) ;
#84607 = CARTESIAN_POINT('Ctrl Pts',(-20.6282641793116,47.2821662070513,123.52929662423)) ;
#84608 = CARTESIAN_POINT('Ctrl Pts',(-20.5136941343494,47.3022347924084,123.940242952693)) ;
#84609 = CARTESIAN_POINT('Ctrl Pts',(-20.2695209604141,47.3220165897232,124.28289844978)) ;
#84610 = CARTESIAN_POINT('Ctrl Pts',(-19.9197275897854,47.3420241366677,124.524725500337)) ;
#84611 = CARTESIAN_POINT('Ctrl Pts',(-19.5119619969569,47.3618458749706,124.631757155408)) ;
#84612 = CARTESIAN_POINT('Ctrl Pts',(-19.0889034892236,47.3818258948748,124.593693820885)) ;
#84613 = CARTESIAN_POINT('Ctrl Pts',(-18.7055979157497,47.401743346137,124.41357834132)) ;
#84614 = CARTESIAN_POINT('Ctrl Pts',(-18.4066951513726,47.4216182673097,124.114802948108)) ;
#84615 = CARTESIAN_POINT('Ctrl Pts',(-18.2266177235489,47.4416426358605,123.72901779228)) ;
#84616 = CARTESIAN_POINT('Ctrl Pts',(-18.1894085958522,47.461509320234,123.308171325423)) ;
#84617 = CARTESIAN_POINT('Ctrl Pts',(-18.2977813339801,47.4814531420802,122.898242749511)) ;
#84618 = CARTESIAN_POINT('Ctrl Pts',(-18.5392371408358,47.5013605113317,122.550578280407)) ;
#84619 = CARTESIAN_POINT('Ctrl Pts',(-18.8838107916012,47.5212352090784,122.305940570887)) ;
#84620 = CARTESIAN_POINT('Ctrl Pts',(-19.2933813903598,47.5412171516001,122.192858540616)) ;
#84621 = CARTESIAN_POINT('Ctrl Pts',(-19.7151773385406,47.561119818511,122.226545830922)) ;
#84622 = CARTESIAN_POINT('Ctrl Pts',(-20.099857981226,47.5809751760497,122.400636940011)) ;
#84623 = CARTESIAN_POINT('Ctrl Pts',(-20.4047900928406,47.6010392147657,122.698899589428)) ;
#84624 = CARTESIAN_POINT('Ctrl Pts',(-20.5876551935011,47.6208943944907,123.079589159602)) ;
#84625 = CARTESIAN_POINT('Ctrl Pts',(-20.630201683294,47.6408744991552,123.502119743328)) ;
#84626 = CARTESIAN_POINT('Ctrl Pts',(-20.5273230946429,47.660683604325,123.910681522273)) ;
#84627 = CARTESIAN_POINT('Ctrl Pts',(-20.2895043292247,47.6806762246657,124.262875655293)) ;
#84628 = CARTESIAN_POINT('Ctrl Pts',(-20.005035238579,47.6972157071698,124.469774758122)) ;
#84629 = CARTESIAN_POINT('Ctrl Pts',(-19.7428589411892,47.710580025234,124.570749541603)) ;
#84630 = CARTESIAN_POINT('Ctrl Pts',(-19.4702099350432,47.7237976277355,124.624411960442)) ;
#84631 = CARTESIAN_POINT('Ctrl Pts',(-19.1168449928776,47.7404552220133,124.600779206886)) ;
#84632 = CARTESIAN_POINT('Ctrl Pts',(-18.7302031446882,47.760320924055,124.43052412299)) ;
#84633 = CARTESIAN_POINT('Ctrl Pts',(-18.4743682268421,47.776950650745,124.186579044811)) ;
#84634 = CARTESIAN_POINT('Ctrl Pts',(-18.3289986202607,47.7902397658829,123.947912625341)) ;
#84635 = CARTESIAN_POINT('Ctrl Pts',(-18.2525289132203,47.80020411286,123.752907855463)) ;
#84636 = CARTESIAN_POINT('Ctrl Pts',(-18.2110894697858,47.8101324808615,123.548334684544)) ;
#84637 = CARTESIAN_POINT('Ctrl Pts',(-18.2034573469909,47.8234159139502,123.26919781636)) ;
#84638 = CARTESIAN_POINT('Ctrl Pts',(-18.2859430189476,47.8400679916905,122.924823299534)) ;
#84639 = CARTESIAN_POINT('Ctrl Pts',(-18.4796140200425,47.8566193609914,122.631051222548)) ;
#84640 = CARTESIAN_POINT('Ctrl Pts',(-18.6881382843732,47.8699067891403,122.445096809951)) ;
#84641 = CARTESIAN_POINT('Ctrl Pts',(-18.8678491409432,47.8799513288404,122.334247522911)) ;
#84642 = CARTESIAN_POINT('Ctrl Pts',(-19.0600721113435,47.8897941706643,122.257599498801)) ;
#84643 = CARTESIAN_POINT('Ctrl Pts',(-19.2654626383406,47.8997784549112,122.214420614964)) ;
#84644 = CARTESIAN_POINT('Ctrl Pts',(-19.4745348605085,47.9097281003104,122.207626209341)) ;
#84645 = CARTESIAN_POINT('Ctrl Pts',(-19.682692403788,47.9197278619988,122.237130756495)) ;
#84646 = CARTESIAN_POINT('Ctrl Pts',(-19.8830746242283,47.9297592079577,122.302862418087)) ;
#84647 = CARTESIAN_POINT('Ctrl Pts',(-20.0658794612454,47.9396141624348,122.40037377344)) ;
#84648 = CARTESIAN_POINT('Ctrl Pts',(-20.2312034863803,47.9495867004353,122.529268259751)) ;
#84649 = CARTESIAN_POINT('Ctrl Pts',(-20.3719768873054,47.9595816941703,122.685311409787)) ;
#84650 = CARTESIAN_POINT('Ctrl Pts',(-20.4837075519426,47.9696157529644,122.864217847032)) ;
#84651 = CARTESIAN_POINT('Ctrl Pts',(-20.561590830256,47.9794710957874,123.056234967956)) ;
#84652 = CARTESIAN_POINT('Ctrl Pts',(-20.6058491698567,47.989470575133,123.261705399765)) ;
#84653 = CARTESIAN_POINT('Ctrl Pts',(-20.6139152861985,47.9993650238883,123.469600664788)) ;
#84654 = CARTESIAN_POINT('Ctrl Pts',(-20.5852299955288,48.0094281433228,123.679168568782)) ;
#84655 = CARTESIAN_POINT('Ctrl Pts',(-20.522223787543,48.019267788564,123.876235991037)) ;
#84656 = CARTESIAN_POINT('Ctrl Pts',(-20.4240386262326,48.0293309527501,124.063598469787)) ;
#84657 = CARTESIAN_POINT('Ctrl Pts',(-20.2968105185812,48.0392252224989,124.228190134964)) ;
#84658 = CARTESIAN_POINT('Ctrl Pts',(-20.1426174173993,48.0491669485127,124.369245419551)) ;
#84659 = CARTESIAN_POINT('Ctrl Pts',(-19.9651875449329,48.0591698371721,124.482184152979)) ;
#84660 = CARTESIAN_POINT('Ctrl Pts',(-19.7700259574284,48.0692096859661,124.562519679078)) ;
#84661 = CARTESIAN_POINT('Ctrl Pts',(-19.5683733991087,48.0790339014269,124.607243543306)) ;
#84662 = CARTESIAN_POINT('Ctrl Pts',(-19.3571780841245,48.0890907449205,124.616781601427)) ;
#84663 = CARTESIAN_POINT('Ctrl Pts',(-19.1502186646684,48.0990193543165,124.589576537769)) ;
#84664 = CARTESIAN_POINT('Ctrl Pts',(-18.9504848243982,48.1089712383544,124.527263966995)) ;
#84665 = CARTESIAN_POINT('Ctrl Pts',(-18.7629118785965,48.119024191162,124.429914062262)) ;
#84666 = CARTESIAN_POINT('Ctrl Pts',(-18.5986752513259,48.1288470676282,124.304701794279)) ;
#84667 = CARTESIAN_POINT('Ctrl Pts',(-18.4551028259504,48.1389028001983,124.149549504682)) ;
#84668 = CARTESIAN_POINT('Ctrl Pts',(-18.3422586437204,48.148843565186,123.973638765055)) ;
#84669 = CARTESIAN_POINT('Ctrl Pts',(-18.2613684519812,48.1587478980916,123.781768982557)) ;
#84670 = CARTESIAN_POINT('Ctrl Pts',(-18.2144911981124,48.1687945669723,123.575842264722)) ;
#84671 = CARTESIAN_POINT('Ctrl Pts',(-18.2040462151921,48.1786901302781,123.368035261619)) ;
#84672 = CARTESIAN_POINT('Ctrl Pts',(-18.2302679712022,48.1887521879784,123.158160931143)) ;
#84673 = CARTESIAN_POINT('Ctrl Pts',(-18.2910782469109,48.1985949656059,122.960347491377)) ;
#84674 = CARTESIAN_POINT('Ctrl Pts',(-18.3862593780217,48.2085854438577,122.773151847488)) ;
#84675 = CARTESIAN_POINT('Ctrl Pts',(-18.5117691377216,48.2185144165013,122.606345569241)) ;
#84676 = CARTESIAN_POINT('Ctrl Pts',(-18.6650588076118,48.2285055533808,122.462742642378)) ;
#84677 = CARTESIAN_POINT('Ctrl Pts',(-18.8416404902588,48.2385276708698,122.347792998566)) ;
#84678 = CARTESIAN_POINT('Ctrl Pts',(-19.0330683521124,48.248428181272,122.266070937534)) ;
#84679 = CARTESIAN_POINT('Ctrl Pts',(-19.2375119544187,48.2584171740181,122.218087239322)) ;
#84680 = CARTESIAN_POINT('Ctrl Pts',(-19.4466837042948,48.2683824180687,122.206504347386)) ;
#84681 = CARTESIAN_POINT('Ctrl Pts',(-19.653498629586,48.2782866825819,122.230779258632)) ;
#84682 = CARTESIAN_POINT('Ctrl Pts',(-19.8559842562716,48.2883447742801,122.291642965385)) ;
#84683 = CARTESIAN_POINT('Ctrl Pts',(-20.0410138891386,48.2981947147085,122.384646494879)) ;
#84684 = CARTESIAN_POINT('Ctrl Pts',(-20.2103684268925,48.308221725882,122.510161016601)) ;
#84685 = CARTESIAN_POINT('Ctrl Pts',(-20.3549894371285,48.3182503124941,122.663586480818)) ;
#84686 = CARTESIAN_POINT('Ctrl Pts',(-20.4689725657444,48.3280955266068,122.836337103123)) ;
#84687 = CARTESIAN_POINT('Ctrl Pts',(-20.552967115562,48.3380862747864,123.028853190084)) ;
#84688 = CARTESIAN_POINT('Ctrl Pts',(-20.6020368136756,48.3481239083719,123.234091529741)) ;
#84689 = CARTESIAN_POINT('Ctrl Pts',(-20.6148256880223,48.3579691975847,123.440677314626)) ;
#84690 = CARTESIAN_POINT('Ctrl Pts',(-20.591694430975,48.3679505983906,123.649222812979)) ;
#84691 = CARTESIAN_POINT('Ctrl Pts',(-20.5328217842057,48.3779028313805,123.850002497856)) ;
#84692 = CARTESIAN_POINT('Ctrl Pts',(-20.4397876862182,48.3879016428371,124.038518382421)) ;
#84693 = CARTESIAN_POINT('Ctrl Pts',(-20.314622824821,48.3979407467678,124.208436648988)) ;
#84694 = CARTESIAN_POINT('Ctrl Pts',(-20.1654041702261,48.4077656891871,124.351272582354)) ;
#84695 = CARTESIAN_POINT('Ctrl Pts',(-19.9898488299125,48.4178203766631,124.468988144029)) ;
#84696 = CARTESIAN_POINT('Ctrl Pts',(-19.7985107535511,48.4277631790199,124.55316317497)) ;
#84697 = CARTESIAN_POINT('Ctrl Pts',(-19.5964148607437,48.4376669749596,124.603261723256)) ;
#84698 = CARTESIAN_POINT('Ctrl Pts',(-19.3857034827114,48.4477137543347,124.617586751126)) ;
#84699 = CARTESIAN_POINT('Ctrl Pts',(-19.1787979364258,48.4576094126293,124.595621172365)) ;
#84700 = CARTESIAN_POINT('Ctrl Pts',(-18.975541301345,48.4676709798799,124.537136964074)) ;
#84701 = CARTESIAN_POINT('Ctrl Pts',(-18.7895837084427,48.4775156243172,124.446269114341)) ;
#84702 = CARTESIAN_POINT('Ctrl Pts',(-18.6198326405228,48.4874756705599,124.323679623546)) ;
#84703 = CARTESIAN_POINT('Ctrl Pts',(-18.4731016776164,48.4975139665783,124.172014555145)) ;
#84704 = CARTESIAN_POINT('Ctrl Pts',(-18.3565226797059,48.5073873079966,124.000238817597)) ;
#84705 = CARTESIAN_POINT('Ctrl Pts',(-18.2699091400072,48.5174604117959,123.807037640738)) ;
#84706 = CARTESIAN_POINT('Ctrl Pts',(-18.2191835073536,48.5272812269148,123.606859946643)) ;
#84707 = CARTESIAN_POINT('Ctrl Pts',(-18.2033538660541,48.5373580919928,123.395643623774)) ;
#84708 = CARTESIAN_POINT('Ctrl Pts',(-18.2240803976646,48.547222831648,123.189269074831)) ;
#84709 = CARTESIAN_POINT('Ctrl Pts',(-18.2806840950281,48.5572452348894,122.986320575425)) ;
#84710 = CARTESIAN_POINT('Ctrl Pts',(-18.372181360659,48.5672709591779,122.796429427149)) ;
#84711 = CARTESIAN_POINT('Ctrl Pts',(-18.4928501657698,48.5771257421992,122.628035078555)) ;
#84712 = CARTESIAN_POINT('Ctrl Pts',(-18.6424187453956,48.5871045859224,122.480923741899)) ;
#84713 = CARTESIAN_POINT('Ctrl Pts',(-18.8161460063999,48.5971234781591,122.361848181127)) ;
#84714 = CARTESIAN_POINT('Ctrl Pts',(-19.005167762733,48.6070066872001,122.275518623979)) ;
#84715 = CARTESIAN_POINT('Ctrl Pts',(-19.2100373399335,48.6170749965403,122.222445396054)) ;
#84716 = CARTESIAN_POINT('Ctrl Pts',(-19.4160689419314,48.626905121873,122.205898319748)) ;
#84717 = CARTESIAN_POINT('Ctrl Pts',(-19.6267500732107,48.63697167425,122.225565271417)) ;
#84718 = CARTESIAN_POINT('Ctrl Pts',(-19.827264205147,48.6468619111437,122.280674205092)) ;
#84719 = CARTESIAN_POINT('Ctrl Pts',(-20.0172632939002,48.6568541359377,122.370249356566)) ;
#84720 = CARTESIAN_POINT('Ctrl Pts',(-20.1882096971853,48.6668167562886,122.491258777972)) ;
#84721 = CARTESIAN_POINT('Ctrl Pts',(-20.3350743946117,48.6767217590518,122.638900209885)) ;
#84722 = CARTESIAN_POINT('Ctrl Pts',(-20.4557702176987,48.6867795214499,122.812492107969)) ;
#84723 = CARTESIAN_POINT('Ctrl Pts',(-20.5428321318592,48.6966300408287,123.000408249078)) ;
#84724 = CARTESIAN_POINT('Ctrl Pts',(-20.5973596016546,48.7066616178269,123.204118638861)) ;
#84725 = CARTESIAN_POINT('Ctrl Pts',(-20.6152472704221,48.7166713529318,123.413816470762)) ;
#84726 = CARTESIAN_POINT('Ctrl Pts',(-20.596827642037,48.7265809295581,123.621312650826)) ;
#84727 = CARTESIAN_POINT('Ctrl Pts',(-20.5430718776097,48.7365083154147,123.822985220348)) ;
#84728 = CARTESIAN_POINT('Ctrl Pts',(-20.4539262829434,48.746553249905,124.014413117639)) ;
#84729 = CARTESIAN_POINT('Ctrl Pts',(-20.3349016053117,48.756439182093,124.184803478514)) ;
#84730 = CARTESIAN_POINT('Ctrl Pts',(-20.1867787456366,48.766432488046,124.333775750932)) ;
#84731 = CARTESIAN_POINT('Ctrl Pts',(-20.0158011499558,48.7763781258279,124.454128865026)) ;
#84732 = CARTESIAN_POINT('Ctrl Pts',(-19.8266660386154,48.7863253941738,124.543373159768)) ;
#84733 = CARTESIAN_POINT('Ctrl Pts',(-19.6228207603563,48.7963732963109,124.598744958645)) ;
#84734 = CARTESIAN_POINT('Ctrl Pts',(-19.4166583359961,48.8062209911511,124.617674236778)) ;
#84735 = CARTESIAN_POINT('Ctrl Pts',(-19.2079107140701,48.8161825008955,124.600980619408)) ;
#84736 = CARTESIAN_POINT('Ctrl Pts',(-19.0039065477696,48.8262118925043,124.547658863247)) ;
#84737 = CARTESIAN_POINT('Ctrl Pts',(-18.8145476302912,48.8361193880591,124.460899954782)) ;
#84738 = CARTESIAN_POINT('Ctrl Pts',(-18.6422518271585,48.8460647797221,124.342481564474)) ;
#84739 = CARTESIAN_POINT('Ctrl Pts',(-18.4921671250518,48.8560666973195,124.195169722798)) ;
#84740 = CARTESIAN_POINT('Ctrl Pts',(-18.3698192760209,48.8661067648717,124.023195652858)) ;
#84741 = CARTESIAN_POINT('Ctrl Pts',(-18.2806985265947,48.8759310763115,123.836856177689)) ;
#84742 = CARTESIAN_POINT('Ctrl Pts',(-18.2237077358343,48.8859873174676,123.633290201079)) ;
#84743 = CARTESIAN_POINT('Ctrl Pts',(-18.2034272663934,48.8959182392032,123.425474801886)) ;
#84744 = CARTESIAN_POINT('Ctrl Pts',(-18.2191289139483,48.9058614752794,123.217054132415)) ;
#84745 = CARTESIAN_POINT('Ctrl Pts',(-18.2707970023579,48.9158427592919,123.013643957691)) ;
#84746 = CARTESIAN_POINT('Ctrl Pts',(-18.3578513256861,48.9258870609176,122.821289635891)) ;
#84747 = CARTESIAN_POINT('Ctrl Pts',(-18.4740534699962,48.935715142137,122.650406878368)) ;
#84748 = CARTESIAN_POINT('Ctrl Pts',(-18.621678191689,48.9457917449862,122.498533628722)) ;
#84749 = CARTESIAN_POINT('Ctrl Pts',(-18.7896140891355,48.9556438241047,122.377226241393)) ;
#84750 = CARTESIAN_POINT('Ctrl Pts',(-18.9800970457834,48.9657170824136,122.284765868234)) ;
#84751 = CARTESIAN_POINT('Ctrl Pts',(-19.1791159230783,48.9755585417939,122.228160557319)) ;
#84752 = CARTESIAN_POINT('Ctrl Pts',(-19.3873388554528,48.9855196372063,122.205934289294)) ;
#84753 = CARTESIAN_POINT('Ctrl Pts',(-19.5978306689872,48.995556921603,122.220722311465)) ;
#84754 = CARTESIAN_POINT('Ctrl Pts',(-19.7993884804198,49.0054332603383,122.270668665904)) ;
#84755 = CARTESIAN_POINT('Ctrl Pts',(-19.992754216528,49.0154953864916,122.356380838616)) ;
#84756 = CARTESIAN_POINT('Ctrl Pts',(-20.1649869075803,49.0253635604681,122.472078092719)) ;
#84757 = CARTESIAN_POINT('Ctrl Pts',(-20.3168522787746,49.0353691089719,122.617582456607)) ;
#84758 = CARTESIAN_POINT('Ctrl Pts',(-20.4408428299329,49.0453517408675,122.786952869297)) ;
#84759 = CARTESIAN_POINT('Ctrl Pts',(-20.5338891114472,49.0553956832892,122.976482688953)) ;
#84760 = CARTESIAN_POINT('Ctrl Pts',(-20.5916223966733,49.0652238313164,123.174870972758)) ;
#84761 = CARTESIAN_POINT('Ctrl Pts',(-20.6150709603759,49.0752136986908,123.38357704141)) ;
#84762 = CARTESIAN_POINT('Ctrl Pts',(-20.6013063782785,49.0852574376463,123.594278915098)) ;
#84763 = CARTESIAN_POINT('Ctrl Pts',(-20.5526930823634,49.0950791861842,123.79495727049)) ;
#84764 = CARTESIAN_POINT('Ctrl Pts',(-20.4686518773646,49.105114163794,123.988462046128)) ;
#84765 = CARTESIAN_POINT('Ctrl Pts',(-20.3519125739174,49.1151390765517,124.163938848035)) ;
#84766 = CARTESIAN_POINT('Ctrl Pts',(-20.2093168597284,49.1249910196455,124.314159557755)) ;
#84767 = CARTESIAN_POINT('Ctrl Pts',(-20.0406693363286,49.1349819809746,124.439317919305)) ;
#84768 = CARTESIAN_POINT('Ctrl Pts',(-19.854241583189,49.1448998558431,124.532750813393)) ;
#84769 = CARTESIAN_POINT('Ctrl Pts',(-19.6522481376843,49.1549283748443,124.593089435573)) ;
#84770 = CARTESIAN_POINT('Ctrl Pts',(-19.4458571981503,49.1648120536421,124.617196619252)) ;
#84771 = CARTESIAN_POINT('Ctrl Pts',(-19.2360620898884,49.1748069970819,124.605427828753)) ;
#84772 = CARTESIAN_POINT('Ctrl Pts',(-19.0309256506428,49.1848338509043,124.556904560052)) ;
#84773 = CARTESIAN_POINT('Ctrl Pts',(-18.8399656511367,49.1947180152432,124.474946591072)) ;
#84774 = CARTESIAN_POINT('Ctrl Pts',(-18.664180747488,49.2047061132856,124.360128702838)) ;
#84775 = CARTESIAN_POINT('Ctrl Pts',(-18.5114556865831,49.2146572197427,124.217117734899)) ;
#84776 = CARTESIAN_POINT('Ctrl Pts',(-18.3848137951546,49.2247022709108,124.048141099064)) ;
#84777 = CARTESIAN_POINT('Ctrl Pts',(-18.291067478107,49.2345640312691,123.863220173348)) ;
#84778 = CARTESIAN_POINT('Ctrl Pts',(-18.2296182846069,49.2445268480995,123.662986260319)) ;
#84779 = CARTESIAN_POINT('Ctrl Pts',(-18.2040446119018,49.2545615293803,123.453590802208)) ;
#84780 = CARTESIAN_POINT('Ctrl Pts',(-18.2146977103563,49.2644465591611,123.246021049742)) ;
#84781 = CARTESIAN_POINT('Ctrl Pts',(-18.2621126124949,49.274512152559,123.039825967864)) ;
#84782 = CARTESIAN_POINT('Ctrl Pts',(-18.3425873172727,49.2843513209205,122.849236798402)) ;
#84783 = CARTESIAN_POINT('Ctrl Pts',(-18.4572075820245,49.294413918662,122.67146142508)) ;
#84784 = CARTESIAN_POINT('Ctrl Pts',(-18.5987775243,49.304310931069,122.518966636729)) ;
#84785 = CARTESIAN_POINT('Ctrl Pts',(-18.7648162010161,49.3142422528946,122.392390628733)) ;
#84786 = CARTESIAN_POINT('Ctrl Pts',(-18.952480025907,49.3242840156491,122.295703968439)) ;
#84787 = CARTESIAN_POINT('Ctrl Pts',(-19.1509683025373,49.3341722145398,122.233882221204)) ;
#84788 = CARTESIAN_POINT('Ctrl Pts',(-19.3593098400291,49.3441661531396,122.206854423686)) ;
#84789 = CARTESIAN_POINT('Ctrl Pts',(-19.5680935725974,49.3541069741765,122.216376406783)) ;
#84790 = CARTESIAN_POINT('Ctrl Pts',(-19.77246713365,49.3640663564647,122.261825261247)) ;
#84791 = CARTESIAN_POINT('Ctrl Pts',(-19.9666684170184,49.3740641161171,122.342274287404)) ;
#84792 = CARTESIAN_POINT('Ctrl Pts',(-20.1444533728029,49.3841002523194,122.455885738796)) ;
#84793 = CARTESIAN_POINT('Ctrl Pts',(-20.2971096658251,49.3939510498103,122.595827064741)) ;
#84794 = CARTESIAN_POINT('Ctrl Pts',(-20.4250477465985,49.4039119148866,122.761600407615)) ;
#84795 = CARTESIAN_POINT('Ctrl Pts',(-20.5227053010492,49.413940782517,122.948471659109)) ;
#84796 = CARTESIAN_POINT('Ctrl Pts',(-20.5857337882693,49.4238510186534,123.147044510219)) ;
#84797 = CARTESIAN_POINT('Ctrl Pts',(-20.6139392662548,49.4337859719679,123.354001283637)) ;
#84798 = CARTESIAN_POINT('Ctrl Pts',(-20.6055025813455,49.4438269023775,123.56491960417)) ;
#84799 = CARTESIAN_POINT('Ctrl Pts',(-20.5613836249676,49.4537147991591,123.768066893831)) ;
#84800 = CARTESIAN_POINT('Ctrl Pts',(-20.4822199801657,49.4637042508178,123.962579565154)) ;
#84801 = CARTESIAN_POINT('Ctrl Pts',(-20.3706836503675,49.4736633411831,124.139761384585)) ;
#84802 = CARTESIAN_POINT('Ctrl Pts',(-20.2313302611011,49.4835606534894,124.29429460168)) ;
#84803 = CARTESIAN_POINT('Ctrl Pts',(-20.0645865632603,49.4936170793897,124.42424335629)) ;
#84804 = CARTESIAN_POINT('Ctrl Pts',(-19.8812921299888,49.5034870819794,124.521540983639)) ;
#84805 = CARTESIAN_POINT('Ctrl Pts',(-19.681378547272,49.5134910151567,124.586788973033)) ;
#84806 = CARTESIAN_POINT('Ctrl Pts',(-19.4734493643751,49.5234782756206,124.616182758674)) ;
#84807 = CARTESIAN_POINT('Ctrl Pts',(-19.2627909875329,49.5335053272063,124.608876433656)) ;
#84808 = CARTESIAN_POINT('Ctrl Pts',(-19.0593249390386,49.5433964170324,124.565892080854)) ;
#84809 = CARTESIAN_POINT('Ctrl Pts',(-18.799884789262,49.5566941718134,124.461822818187)) ;
#84810 = CARTESIAN_POINT('Ctrl Pts',(-18.5749111535208,49.5698922314216,124.293969511799)) ;
#84811 = CARTESIAN_POINT('Ctrl Pts',(-18.4005901141605,49.5832889719908,124.072839422484)) ;
#84812 = CARTESIAN_POINT('Ctrl Pts',(-18.3021399347806,49.5931598840642,123.890105721718)) ;
#84813 = CARTESIAN_POINT('Ctrl Pts',(-18.2356163079452,49.6032334458323,123.689098930403)) ;
#84814 = CARTESIAN_POINT('Ctrl Pts',(-18.2055086116115,49.6130548584207,123.484778378006)) ;
#84815 = CARTESIAN_POINT('Ctrl Pts',(-18.2112827916809,49.6231288756517,123.273123424791)) ;
#84816 = CARTESIAN_POINT('Ctrl Pts',(-18.2665397113971,49.6362876626163,123.001992298951)) ;
#84817 = CARTESIAN_POINT('Ctrl Pts',(-18.392790369239,49.6496537657104,122.747437472296)) ;
#84818 = CARTESIAN_POINT('Ctrl Pts',(-18.5783672784974,49.6629677005995,122.537851142176)) ;
#84819 = CARTESIAN_POINT('Ctrl Pts',(-18.7409926332398,49.672867740047,122.407995171193)) ;
#84820 = CARTESIAN_POINT('Ctrl Pts',(-18.9247419738745,49.6828321431815,122.307378326656)) ;
#84821 = CARTESIAN_POINT('Ctrl Pts',(-19.1245307678255,49.6928621103026,122.239933892101)) ;
#84822 = CARTESIAN_POINT('Ctrl Pts',(-19.3303117175903,49.7027643869117,122.208520852537)) ;
#84823 = CARTESIAN_POINT('Ctrl Pts',(-19.6091931851167,49.7160303160808,122.21423648019)) ;
#84824 = CARTESIAN_POINT('Ctrl Pts',(-19.9485295576993,49.7326518471873,122.312721939524)) ;
#84825 = CARTESIAN_POINT('Ctrl Pts',(-20.2902094160068,49.7525266758319,122.561479387571)) ;
#84826 = CARTESIAN_POINT('Ctrl Pts',(-20.4884697069658,49.7691998839338,122.855392710273)) ;
#84827 = CARTESIAN_POINT('Ctrl Pts',(-20.5789967303349,49.7824510089151,123.118823468172)) ;
#84828 = CARTESIAN_POINT('Ctrl Pts',(-20.6234021150388,49.7956933277359,123.393723395703)) ;
#84829 = CARTESIAN_POINT('Ctrl Pts',(-20.5867774609634,49.8124265680754,123.747547976554)) ;
#84830 = CARTESIAN_POINT('Ctrl Pts',(-20.4028093076993,49.8322557162633,124.127010811538)) ;
#84831 = CARTESIAN_POINT('Ctrl Pts',(-20.0997798926132,49.852180411364,124.42294390878)) ;
#84832 = CARTESIAN_POINT('Ctrl Pts',(-19.7138203126562,49.8721036399474,124.597719619346)) ;
#84833 = CARTESIAN_POINT('Ctrl Pts',(-19.2914296712832,49.8920307790735,124.630422663148)) ;
#84834 = CARTESIAN_POINT('Ctrl Pts',(-18.8840520052967,49.9119072416892,124.517817536054)) ;
#84835 = CARTESIAN_POINT('Ctrl Pts',(-18.5377036256357,49.9318844702945,124.27191551634)) ;
#84836 = CARTESIAN_POINT('Ctrl Pts',(-18.2968245024389,49.9518193282682,123.923098282419)) ;
#84837 = CARTESIAN_POINT('Ctrl Pts',(-18.189244149917,49.971715777199,123.513986183938)) ;
#84838 = CARTESIAN_POINT('Ctrl Pts',(-18.2273108184386,49.9916370612656,123.092101326508)) ;
#84839 = CARTESIAN_POINT('Ctrl Pts',(-18.4075015764664,50.0115937109365,122.707903617813)) ;
#84840 = CARTESIAN_POINT('Ctrl Pts',(-18.7066393081926,50.0314710040481,122.409408094434)) ;
#84841 = CARTESIAN_POINT('Ctrl Pts',(-19.0894747132605,50.0513574762766,122.229768593168)) ;
#84842 = CARTESIAN_POINT('Ctrl Pts',(-19.5143647079176,50.0714190422006,122.191861118502)) ;
#84843 = CARTESIAN_POINT('Ctrl Pts',(-19.9220057248458,50.0912594497413,122.300397245321)) ;
#84844 = CARTESIAN_POINT('Ctrl Pts',(-20.269364749244,50.1111107737143,122.540224979063)) ;
#84845 = CARTESIAN_POINT('Ctrl Pts',(-20.5159525618895,50.1311640436657,122.888006920519)) ;
#84846 = CARTESIAN_POINT('Ctrl Pts',(-20.6278796826559,50.150984701049,123.294433905217)) ;
#84847 = CARTESIAN_POINT('Ctrl Pts',(-20.5948465512445,50.1709561223796,123.71765363184)) ;
#84848 = CARTESIAN_POINT('Ctrl Pts',(-20.4200332314794,50.1908496147432,124.10299591866)) ;
#84849 = CARTESIAN_POINT('Ctrl Pts',(-20.1222394668476,50.2108737009843,124.407164798566)) ;
#84850 = CARTESIAN_POINT('Ctrl Pts',(-19.7427028446322,50.2306785800972,124.589700978199)) ;
#84851 = CARTESIAN_POINT('Ctrl Pts',(-19.3205721862812,50.2506375957951,124.633229805539)) ;
#84852 = CARTESIAN_POINT('Ctrl Pts',(-18.9086034727282,50.2706236194241,124.528993219994)) ;
#84853 = CARTESIAN_POINT('Ctrl Pts',(-18.5595577971267,50.2904321151846,124.293209206143)) ;
#84854 = CARTESIAN_POINT('Ctrl Pts',(-18.3093968949596,50.3104147542902,123.949887481206)) ;
#84855 = CARTESIAN_POINT('Ctrl Pts',(-18.1920567395981,50.3302962020842,123.543654845403)) ;
#84856 = CARTESIAN_POINT('Ctrl Pts',(-18.2201436547661,50.3502526688217,123.120348131323)) ;
#84857 = CARTESIAN_POINT('Ctrl Pts',(-18.3901205711742,50.3701300657773,122.733311899486)) ;
#84858 = CARTESIAN_POINT('Ctrl Pts',(-18.6832550770662,50.3901120119526,122.425821701632)) ;
#84859 = CARTESIAN_POINT('Ctrl Pts',(-19.0629300478071,50.4100411109893,122.237453775053)) ;
#84860 = CARTESIAN_POINT('Ctrl Pts',(-19.4839074313654,50.429969734202,122.18990649363)) ;
#84861 = CARTESIAN_POINT('Ctrl Pts',(-19.8941981218103,50.4498040583084,122.287670822097)) ;
#84862 = CARTESIAN_POINT('Ctrl Pts',(-20.1900713511371,50.4664563456918,122.481987303005)) ;
#84863 = CARTESIAN_POINT('Ctrl Pts',(-20.3755130654345,50.479716846714,122.690239021733)) ;
#84864 = CARTESIAN_POINT('Ctrl Pts',(-20.4862810393611,50.4897183239153,122.8689492502)) ;
#84865 = CARTESIAN_POINT('Ctrl Pts',(-20.5642531757108,50.4997503447748,123.064919125253)) ;
#84866 = CARTESIAN_POINT('Ctrl Pts',(-20.6065416927143,50.5096138885003,123.267915656053)) ;
#84867 = CARTESIAN_POINT('Ctrl Pts',(-20.6135616619196,50.5195826021705,123.47738461801)) ;
#84868 = CARTESIAN_POINT('Ctrl Pts',(-20.5737480165566,50.5329283495742,123.755049799615)) ;
#84869 = CARTESIAN_POINT('Ctrl Pts',(-20.4644112173549,50.5460789046468,124.01246056538)) ;
#84870 = CARTESIAN_POINT('Ctrl Pts',(-20.2913080349741,50.5594642851967,124.234313475355)) ;
#84871 = CARTESIAN_POINT('Ctrl Pts',(-20.136897698789,50.5693522211896,124.373521055531)) ;
#84872 = CARTESIAN_POINT('Ctrl Pts',(-19.9590515618089,50.5793434110022,124.485228977949)) ;
#84873 = CARTESIAN_POINT('Ctrl Pts',(-19.7652513978111,50.5892955095405,124.564155971045)) ;
#84874 = CARTESIAN_POINT('Ctrl Pts',(-19.5587718390512,50.599341765991,124.608506610613)) ;
#84875 = CARTESIAN_POINT('Ctrl Pts',(-19.3518494007043,50.6091912133851,124.616330381746)) ;
#84876 = CARTESIAN_POINT('Ctrl Pts',(-19.144275513289,50.6191538658803,124.588436795362)) ;
#84877 = CARTESIAN_POINT('Ctrl Pts',(-18.9435668721036,50.6291769515224,124.524268876107)) ;
#84878 = CARTESIAN_POINT('Ctrl Pts',(-18.758740003588,50.6391020672793,124.427384612171)) ;
#84879 = CARTESIAN_POINT('Ctrl Pts',(-18.5915092232509,50.6491545456791,124.298203194396)) ;
#84880 = CARTESIAN_POINT('Ctrl Pts',(-18.4519664488922,50.6590060443818,124.145139257447)) ;
#84881 = CARTESIAN_POINT('Ctrl Pts',(-18.3393284230792,50.6689777835844,123.968364363511)) ;
#84882 = CARTESIAN_POINT('Ctrl Pts',(-18.2589073168524,50.6789729913501,123.774195216805)) ;
#84883 = CARTESIAN_POINT('Ctrl Pts',(-18.2135079778918,50.6890069928191,123.568211141614)) ;
#84884 = CARTESIAN_POINT('Ctrl Pts',(-18.2043916883253,50.6988623509115,123.361200369958)) ;
#84885 = CARTESIAN_POINT('Ctrl Pts',(-18.2314639870011,50.7088618265048,123.152768262259)) ;
#84886 = CARTESIAN_POINT('Ctrl Pts',(-18.2934523109721,50.7187562749999,122.954165767823)) ;
#84887 = CARTESIAN_POINT('Ctrl Pts',(-18.3906320047257,50.7288193992276,122.766288923649)) ;
#84888 = CARTESIAN_POINT('Ctrl Pts',(-18.515967951093,50.7386590255562,122.601680143843)) ;
#84889 = CARTESIAN_POINT('Ctrl Pts',(-18.671206799712,50.7487222605992,122.457990491376)) ;
#84890 = CARTESIAN_POINT('Ctrl Pts',(-18.8461841647024,50.7586162658332,122.345485242714)) ;
#84891 = CARTESIAN_POINT('Ctrl Pts',(-19.0387184734415,50.768558979049,122.264163925914)) ;
#84892 = CARTESIAN_POINT('Ctrl Pts',(-19.2437750813141,50.7785647188472,122.217162069722)) ;
#84893 = CARTESIAN_POINT('Ctrl Pts',(-19.454181494152,50.7885856209936,122.206701103383)) ;
#84894 = CARTESIAN_POINT('Ctrl Pts',(-19.66053430919,50.7984763910424,122.232355977739)) ;
#84895 = CARTESIAN_POINT('Ctrl Pts',(-19.8613997985619,50.8084678018222,122.293768556927)) ;
#84896 = CARTESIAN_POINT('Ctrl Pts',(-20.0477153832223,50.8184161474867,122.388776879898)) ;
#84897 = CARTESIAN_POINT('Ctrl Pts',(-20.2149291809395,50.8283610055478,122.514309604095)) ;
#84898 = CARTESIAN_POINT('Ctrl Pts',(-20.3591331058569,50.8384158409408,122.668841760372)) ;
#84899 = CARTESIAN_POINT('Ctrl Pts',(-20.4719728911623,50.8482382130423,122.841803139184)) ;
#84900 = CARTESIAN_POINT('Ctrl Pts',(-20.555331401532,50.858294080486,123.036064303744)) ;
#84901 = CARTESIAN_POINT('Ctrl Pts',(-20.6027823192798,50.8682348103439,123.23959968748)) ;
#84902 = CARTESIAN_POINT('Ctrl Pts',(-20.6147815729296,50.878139148895,123.44747770564)) ;
#84903 = CARTESIAN_POINT('Ctrl Pts',(-20.5900240767088,50.8881858303235,123.657216643882)) ;
#84904 = CARTESIAN_POINT('Ctrl Pts',(-20.5303079529691,50.8980813377928,123.856531746283)) ;
#84905 = CARTESIAN_POINT('Ctrl Pts',(-20.4353433394466,50.9081436062914,124.045523747935)) ;
#84906 = CARTESIAN_POINT('Ctrl Pts',(-20.3118409988346,50.917985596562,124.21156392592)) ;
#84907 = CARTESIAN_POINT('Ctrl Pts',(-20.1594362435033,50.9279790134429,124.356126658546)) ;
#84908 = CARTESIAN_POINT('Ctrl Pts',(-19.9854190300829,50.9379035012951,124.471276812575)) ;
#84909 = CARTESIAN_POINT('Ctrl Pts',(-19.7927265192482,50.9479031352036,124.55527997658)) ;
#84910 = CARTESIAN_POINT('Ctrl Pts',(-19.5886058865393,50.9578892454603,124.60450108156)) ;
#84911 = CARTESIAN_POINT('Ctrl Pts',(-19.3780314592793,50.9679251966475,124.61737349996)) ;
#84912 = CARTESIAN_POINT('Ctrl Pts',(-19.1720910866892,50.9777818349823,124.594220179101)) ;
#84913 = CARTESIAN_POINT('Ctrl Pts',(-18.9704025499293,50.9877807950603,124.535105151428)) ;
#84914 = CARTESIAN_POINT('Ctrl Pts',(-18.7838328347708,50.9976760253741,124.4430065962)) ;
#84915 = CARTESIAN_POINT('Ctrl Pts',(-18.6133502426643,51.0077365378427,124.317874563771)) ;
#84916 = CARTESIAN_POINT('Ctrl Pts',(-18.4701391587835,51.0175858293889,124.168301037552)) ;
#84917 = CARTESIAN_POINT('Ctrl Pts',(-18.3525641864338,51.0276130153211,123.993338577093)) ;
#84918 = CARTESIAN_POINT('Ctrl Pts',(-18.267643184674,51.0376415517804,123.80035451897)) ;
#84919 = CARTESIAN_POINT('Ctrl Pts',(-18.218060405156,51.0474867917454,123.599415288978)) ;
#84920 = CARTESIAN_POINT('Ctrl Pts',(-18.2033518857591,51.0574774866686,123.389889933825)) ;
#84921 = CARTESIAN_POINT('Ctrl Pts',(-18.2258151202182,51.0675153074272,123.18006296061)) ;
#84922 = CARTESIAN_POINT('Ctrl Pts',(-18.2829055891925,51.0773599012041,122.981124529681)) ;
#84923 = CARTESIAN_POINT('Ctrl Pts',(-18.374543826743,51.0873438965802,122.792311132886)) ;
#84924 = CARTESIAN_POINT('Ctrl Pts',(-18.497178925122,51.0972929451416,122.622862413352)) ;
#84925 = CARTESIAN_POINT('Ctrl Pts',(-18.6480196169421,51.1072953841161,122.476338494011)) ;
#84926 = CARTESIAN_POINT('Ctrl Pts',(-18.8224928721173,51.1173166254125,122.358249517239)) ;
#84927 = CARTESIAN_POINT('Ctrl Pts',(-19.0122492011059,51.127209303852,122.273123769501)) ;
#84928 = CARTESIAN_POINT('Ctrl Pts',(-19.2158038373338,51.1371993577996,122.221412219631)) ;
#84929 = CARTESIAN_POINT('Ctrl Pts',(-19.4245865714748,51.1471577189481,122.206028609409)) ;
#84930 = CARTESIAN_POINT('Ctrl Pts',(-19.6317117699765,51.1570573458329,122.226497827974)) ;
#84931 = CARTESIAN_POINT('Ctrl Pts',(-19.8350849559763,51.1671052426363,122.283522987711)) ;
#84932 = CARTESIAN_POINT('Ctrl Pts',(-20.022696372349,51.1770006002723,122.373481440644)) ;
#84933 = CARTESIAN_POINT('Ctrl Pts',(-20.1946528304489,51.1870622527289,122.496627883948)) ;
#84934 = CARTESIAN_POINT('Ctrl Pts',(-20.3394665608581,51.1969068570009,122.644499616688)) ;
#84935 = CARTESIAN_POINT('Ctrl Pts',(-20.4583901002709,51.2068669786989,122.816839675595)) ;
#84936 = CARTESIAN_POINT('Ctrl Pts',(-20.5458920206449,51.2169050130614,123.008866436735)) ;
#84937 = CARTESIAN_POINT('Ctrl Pts',(-20.5982377519266,51.2267793256479,123.209773659771)) ;
#84938 = CARTESIAN_POINT('Ctrl Pts',(-20.615219420683,51.2368488064306,123.420755084816)) ;
#84939 = CARTESIAN_POINT('Ctrl Pts',(-20.5958818047259,51.2466831424477,123.626614553327)) ;
#84940 = CARTESIAN_POINT('Ctrl Pts',(-20.5405510012675,51.2567161001759,123.830145681177)) ;
#84941 = CARTESIAN_POINT('Ctrl Pts',(-20.4503035157272,51.2667364987511,124.020498806758)) ;
#84942 = CARTESIAN_POINT('Ctrl Pts',(-20.3306797939829,51.2766020725223,124.189949471815)) ;
#84943 = CARTESIAN_POINT('Ctrl Pts',(-20.1804458345177,51.2866709471784,124.339042785219)) ;
#84944 = CARTESIAN_POINT('Ctrl Pts',(-20.0104561735626,51.2965163780839,124.457150465107)) ;
#84945 = CARTESIAN_POINT('Ctrl Pts',(-19.8202797994579,51.3064960029546,124.545737849271)) ;
#84946 = CARTESIAN_POINT('Ctrl Pts',(-19.616714022503,51.3165146858687,124.599784861309)) ;
#84947 = CARTESIAN_POINT('Ctrl Pts',(-19.4096995310272,51.3263979510525,124.617864751251)) ;
#84948 = CARTESIAN_POINT('Ctrl Pts',(-19.1988827452184,51.3364662451439,124.599299463664)) ;
#84949 = CARTESIAN_POINT('Ctrl Pts',(-18.9991976018258,51.3462963753292,124.545926781667)) ;
#84950 = CARTESIAN_POINT('Ctrl Pts',(-18.8072530956794,51.3563629235443,124.456872690114)) ;
#84951 = CARTESIAN_POINT('Ctrl Pts',(-18.6367526325519,51.366253172233,124.337824103863)) ;
#84952 = CARTESIAN_POINT('Ctrl Pts',(-18.4876976832283,51.376245354009,124.1898183886)) ;
#84953 = CARTESIAN_POINT('Ctrl Pts',(-18.3671179776991,51.3862081346368,124.018565014349)) ;
#84954 = CARTESIAN_POINT('Ctrl Pts',(-18.2781468980494,51.3961125393105,123.830292783191)) ;
#84955 = CARTESIAN_POINT('Ctrl Pts',(-18.2225158405115,51.4061725337896,123.626267180242)) ;
#84956 = CARTESIAN_POINT('Ctrl Pts',(-18.2033820488565,51.4160211557594,123.420089212083)) ;
#84957 = CARTESIAN_POINT('Ctrl Pts',(-18.220176478215,51.4260515951712,123.209899707613)) ;
#84958 = CARTESIAN_POINT('Ctrl Pts',(-18.2735217851603,51.436061310806,123.006313697817)) ;
#84959 = CARTESIAN_POINT('Ctrl Pts',(-18.3603349962703,51.4459720634986,122.816927498495)) ;
#84960 = CARTESIAN_POINT('Ctrl Pts',(-18.4785193359598,51.455901336445,122.644849590924)) ;
#84961 = CARTESIAN_POINT('Ctrl Pts',(-18.6265725102153,51.4659440278377,122.494343311464)) ;
#84962 = CARTESIAN_POINT('Ctrl Pts',(-18.7957733587672,51.4758305610552,122.373613107459)) ;
#84963 = CARTESIAN_POINT('Ctrl Pts',(-18.9852153494115,51.4858237059872,122.282818770106)) ;
#84964 = CARTESIAN_POINT('Ctrl Pts',(-19.1866163697418,51.4957693868237,122.226639312132)) ;
#84965 = CARTESIAN_POINT('Ctrl Pts',(-19.3947137007887,51.5057166439722,122.205852968183)) ;
#84966 = CARTESIAN_POINT('Ctrl Pts',(-19.6053345562994,51.5157645478442,122.221908810466)) ;
#84967 = CARTESIAN_POINT('Ctrl Pts',(-19.8059405043631,51.5256122469422,122.273080725535)) ;
#84968 = CARTESIAN_POINT('Ctrl Pts',(-19.9970579122772,51.5355737379209,122.358685508991)) ;
#84969 = CARTESIAN_POINT('Ctrl Pts',(-20.1714467611568,51.5456032003348,122.477219168564)) ;
#84970 = CARTESIAN_POINT('Ctrl Pts',(-20.3208357337139,51.5555104314347,122.62235338658)) ;
#84971 = CARTESIAN_POINT('Ctrl Pts',(-20.4435745272734,51.5654568101121,122.791629667315)) ;
#84972 = CARTESIAN_POINT('Ctrl Pts',(-20.5356748438808,51.575461578921,122.980744980658)) ;
#84973 = CARTESIAN_POINT('Ctrl Pts',(-20.5933963675229,51.5854826999412,123.183354761338)) ;
#84974 = CARTESIAN_POINT('Ctrl Pts',(-20.6150184502875,51.5953735657938,123.390171536173)) ;
#84975 = CARTESIAN_POINT('Ctrl Pts',(-20.6005649524091,51.6053643745531,123.599699839258)) ;
#84976 = CARTESIAN_POINT('Ctrl Pts',(-20.5501094987751,51.6153150327334,123.802728492899)) ;
#84977 = CARTESIAN_POINT('Ctrl Pts',(-20.4655583773895,51.6252512423755,123.993724149889)) ;
#84978 = CARTESIAN_POINT('Ctrl Pts',(-20.3487803568357,51.6352344091004,124.168144479374)) ;
#84979 = CARTESIAN_POINT('Ctrl Pts',(-20.2023614827982,51.6452782063107,124.32025219371)) ;
#84980 = CARTESIAN_POINT('Ctrl Pts',(-20.0356625555616,51.655106422479,124.442383564606)) ;
#84981 = CARTESIAN_POINT('Ctrl Pts',(-19.8457170220924,51.6651829899482,124.536080304452)) ;
#84982 = CARTESIAN_POINT('Ctrl Pts',(-19.6468633598627,51.6750350756376,124.594176636831)) ;
#84983 = CARTESIAN_POINT('Ctrl Pts',(-19.4364191049559,51.685108343043,124.617542351253)) ;
#84984 = CARTESIAN_POINT('Ctrl Pts',(-19.2299340144037,51.6949497594666,124.604264983939)) ;
#84985 = CARTESIAN_POINT('Ctrl Pts',(-19.0262804084281,51.7049110176093,124.555507886137)) ;
#84986 = CARTESIAN_POINT('Ctrl Pts',(-18.8328905076921,51.7149476940412,124.471123415834)) ;
#84987 = CARTESIAN_POINT('Ctrl Pts',(-18.6596436603667,51.7248263019051,124.356557651577)) ;
#84988 = CARTESIAN_POINT('Ctrl Pts',(-18.506152939823,51.7348865305439,124.211091737001)) ;
#84989 = CARTESIAN_POINT('Ctrl Pts',(-18.3825894189891,51.7447535147047,124.044441759415)) ;
#84990 = CARTESIAN_POINT('Ctrl Pts',(-18.288197260969,51.7547590809574,123.856492609393)) ;
#84991 = CARTESIAN_POINT('Ctrl Pts',(-18.2280368454756,51.764742869372,123.655369944984)) ;
#84992 = CARTESIAN_POINT('Ctrl Pts',(-18.2037955443594,51.7747887261746,123.44558720362)) ;
#84993 = CARTESIAN_POINT('Ctrl Pts',(-18.2158049422002,51.7846146033906,123.239365703502)) ;
#84994 = CARTESIAN_POINT('Ctrl Pts',(-18.2635681761334,51.7946050792319,123.034837434973)) ;
#84995 = CARTESIAN_POINT('Ctrl Pts',(-18.3470677407397,51.8046486551307,122.840901092914)) ;
#84996 = CARTESIAN_POINT('Ctrl Pts',(-18.460050036264,51.8144704474287,122.668070690443)) ;
#84997 = CARTESIAN_POINT('Ctrl Pts',(-18.6040154321595,51.8245054130546,122.513860046172)) ;
#84998 = CARTESIAN_POINT('Ctrl Pts',(-18.7727581101242,51.8345303299877,122.387582237159)) ;
#84999 = CARTESIAN_POINT('Ctrl Pts',(-18.9574116325095,51.8443822683638,122.293758444843)) ;
#85000 = CARTESIAN_POINT('Ctrl Pts',(-19.1582249159221,51.8543732443885,122.232272280437)) ;
#85001 = CARTESIAN_POINT('Ctrl Pts',(-19.3651733728884,51.8642910651922,122.206630479533)) ;
#85002 = CARTESIAN_POINT('Ctrl Pts',(-19.5757113303297,51.8743197857568,122.217393836154)) ;
#85003 = CARTESIAN_POINT('Ctrl Pts',(-19.7782673536523,51.8842027123659,122.263734533123)) ;
#85004 = CARTESIAN_POINT('Ctrl Pts',(-19.9721412663142,51.8942069974854,122.345208741606)) ;
#85005 = CARTESIAN_POINT('Ctrl Pts',(-20.1485965825961,51.9041906786933,122.458925895138)) ;
#85006 = CARTESIAN_POINT('Ctrl Pts',(-20.3033084600691,51.9142316774232,122.602515954827)) ;
#85007 = CARTESIAN_POINT('Ctrl Pts',(-20.4283341936151,51.9240641222903,122.767130738101)) ;
#85008 = CARTESIAN_POINT('Ctrl Pts',(-20.5249880230487,51.9340591207207,122.953701580357)) ;
#85009 = CARTESIAN_POINT('Ctrl Pts',(-20.5875824491008,51.9440906694703,123.155104794156)) ;
#85010 = CARTESIAN_POINT('Ctrl Pts',(-20.6140701866757,51.9539560477758,123.360796237962)) ;
#85011 = CARTESIAN_POINT('Ctrl Pts',(-20.6049369884442,51.9639178952361,123.570032777721)) ;
#85012 = CARTESIAN_POINT('Ctrl Pts',(-20.5589475425777,51.9739528360503,123.775913422753)) ;
#85013 = CARTESIAN_POINT('Ctrl Pts',(-20.4794278314996,51.9838377970674,123.967942136483)) ;
#85014 = CARTESIAN_POINT('Ctrl Pts',(-20.3657283845521,51.9939034059863,124.14637155563)) ;
#85015 = CARTESIAN_POINT('Ctrl Pts',(-20.2260994155027,52.003742581028,124.299028744683)) ;
#85016 = CARTESIAN_POINT('Ctrl Pts',(-20.0585850427289,52.0138051365279,124.428181893886)) ;
#85017 = CARTESIAN_POINT('Ctrl Pts',(-19.874133546261,52.0237023112208,124.524491578189)) ;
#85018 = CARTESIAN_POINT('Ctrl Pts',(-19.6753166357075,52.0336330261442,124.588188263668)) ;
#85019 = CARTESIAN_POINT('Ctrl Pts',(-19.4660674265901,52.0436770542218,124.616477182065)) ;
#85020 = CARTESIAN_POINT('Ctrl Pts',(-19.2583751604447,52.0535632560751,124.608298744114)) ;
#85021 = CARTESIAN_POINT('Ctrl Pts',(-19.0530285450914,52.0635564225419,124.564023365578)) ;
#85022 = CARTESIAN_POINT('Ctrl Pts',(-18.8594658865747,52.0734958935291,124.485230512348)) ;
#85023 = CARTESIAN_POINT('Ctrl Pts',(-18.681171591748,52.0835124078833,124.373224330543)) ;
#85024 = CARTESIAN_POINT('Ctrl Pts',(-18.5262256114229,52.0934424343601,124.233278642585)) ;
#85025 = CARTESIAN_POINT('Ctrl Pts',(-18.3964520684742,52.1034949698696,124.066502860236)) ;
#85026 = CARTESIAN_POINT('Ctrl Pts',(-18.2995181668881,52.1133413730892,123.883591053163)) ;
#85027 = CARTESIAN_POINT('Ctrl Pts',(-18.2344303663657,52.1233034159433,123.684540728996)) ;
#85028 = CARTESIAN_POINT('Ctrl Pts',(-18.2049633408895,52.133331966734,123.475764348543)) ;
#85029 = CARTESIAN_POINT('Ctrl Pts',(-18.2120381030114,52.1432422924516,123.267547761259)) ;
#85030 = CARTESIAN_POINT('Ctrl Pts',(-18.2547347149684,52.1531772042812,123.063088669452)) ;
#85031 = CARTESIAN_POINT('Ctrl Pts',(-18.3332871503977,52.1632182110493,122.867161311579)) ;
#85032 = CARTESIAN_POINT('Ctrl Pts',(-18.4428555005339,52.1731058438815,122.690501470127)) ;
#85033 = CARTESIAN_POINT('Ctrl Pts',(-18.582582312004,52.1830962749795,122.533706157524)) ;
#85034 = CARTESIAN_POINT('Ctrl Pts',(-18.7469172566811,52.1930517115367,122.404087576833)) ;
#85035 = CARTESIAN_POINT('Ctrl Pts',(-18.9302412953445,52.2029626596361,122.305087020515)) ;
#85036 = CARTESIAN_POINT('Ctrl Pts',(-19.1299410619868,52.2129747357338,122.238509440795)) ;
#85037 = CARTESIAN_POINT('Ctrl Pts',(-19.3385091445612,52.2230020578087,122.207996703187)) ;
#85038 = CARTESIAN_POINT('Ctrl Pts',(-19.5457346255432,52.2328608327629,122.213537169316)) ;
#85039 = CARTESIAN_POINT('Ctrl Pts',(-19.8221907945134,52.2462870255753,122.270185645489)) ;
#85040 = CARTESIAN_POINT('Ctrl Pts',(-20.0713994992223,52.2593710413567,122.394141575625)) ;
#85041 = CARTESIAN_POINT('Ctrl Pts',(-20.2838395622631,52.272844490112,122.581345054792)) ;
#85042 = CARTESIAN_POINT('Ctrl Pts',(-20.412650215348,52.2826774479178,122.743072361352)) ;
#85043 = CARTESIAN_POINT('Ctrl Pts',(-20.5134840114003,52.2926407213685,122.926645543791)) ;
#85044 = CARTESIAN_POINT('Ctrl Pts',(-20.5809847415257,52.3026777951864,123.126566369539)) ;
#85045 = CARTESIAN_POINT('Ctrl Pts',(-20.6126263091998,52.3125527981981,123.331769600244)) ;
#85046 = CARTESIAN_POINT('Ctrl Pts',(-20.6080629083535,52.3226204778243,123.543345637874)) ;
#85047 = CARTESIAN_POINT('Ctrl Pts',(-20.567868291895,52.332461328042,123.746312988223)) ;
#85048 = CARTESIAN_POINT('Ctrl Pts',(-20.4670269754835,52.345797526518,124.007905058879)) ;
#85049 = CARTESIAN_POINT('Ctrl Pts',(-20.3015604237131,52.3590150503324,124.235140155152)) ;
#85050 = CARTESIAN_POINT('Ctrl Pts',(-20.0837896410243,52.3723499768236,124.411582706571)) ;
#85051 = CARTESIAN_POINT('Ctrl Pts',(-19.900255890719,52.3823330774182,124.513471532459)) ;
#85052 = CARTESIAN_POINT('Ctrl Pts',(-19.7005525301672,52.3923778533179,124.582048554509)) ;
#85053 = CARTESIAN_POINT('Ctrl Pts',(-19.496714380431,52.4021957765038,124.614579095384)) ;
#85054 = CARTESIAN_POINT('Ctrl Pts',(-19.2854774970839,52.4122450904591,124.611577339329)) ;
#85055 = CARTESIAN_POINT('Ctrl Pts',(-19.0108629775907,52.4255488310817,124.558542159798)) ;
#85056 = CARTESIAN_POINT('Ctrl Pts',(-18.6949729851528,52.4420390265583,124.406311397953)) ;
#85057 = CARTESIAN_POINT('Ctrl Pts',(-18.446743481216,52.458758191483,124.151888766635)) ;
#85058 = CARTESIAN_POINT('Ctrl Pts',(-18.3113738894575,52.4719191851531,123.910570921189)) ;
#85059 = CARTESIAN_POINT('Ctrl Pts',(-18.2412220343529,52.4819154072584,123.712480369397)) ;
#85060 = CARTESIAN_POINT('Ctrl Pts',(-18.2069072499247,52.4919392467921,123.504562221584)) ;
#85061 = CARTESIAN_POINT('Ctrl Pts',(-18.2093339290395,52.5051325687854,123.227174035408)) ;
#85062 = CARTESIAN_POINT('Ctrl Pts',(-18.3035482233452,52.5217917405627,122.885761998308)) ;
#85063 = CARTESIAN_POINT('Ctrl Pts',(-18.5490022666075,52.5417019160484,122.540816632851)) ;
#85064 = CARTESIAN_POINT('Ctrl Pts',(-18.896602436041,52.5615919038928,122.299840270026)) ;
#85065 = CARTESIAN_POINT('Ctrl Pts',(-19.3079252000315,52.5815973519076,122.191722541258)) ;
#85066 = CARTESIAN_POINT('Ctrl Pts',(-19.7281008050595,52.6014337459349,122.229713440232)) ;
#85067 = CARTESIAN_POINT('Ctrl Pts',(-20.1132537389157,52.6214415398316,122.410106061638)) ;
#85068 = CARTESIAN_POINT('Ctrl Pts',(-20.4112472617472,52.6412681761255,122.708408581873)) ;
#85069 = CARTESIAN_POINT('Ctrl Pts',(-20.591586675119,52.6612471190794,123.093018079891)) ;
#85070 = CARTESIAN_POINT('Ctrl Pts',(-20.6290084966282,52.6811789209484,123.515109816037)) ;
#85071 = CARTESIAN_POINT('Ctrl Pts',(-20.5220590950608,52.701003221446,123.922971129483)) ;
#85072 = CARTESIAN_POINT('Ctrl Pts',(-20.2786176824893,52.7210992227858,124.273924750652)) ;
#85073 = CARTESIAN_POINT('Ctrl Pts',(-19.9358039298988,52.7408576388898,124.51720323267)) ;
#85074 = CARTESIAN_POINT('Ctrl Pts',(-19.5241772464082,52.7609513317739,124.630789979139)) ;
#85075 = CARTESIAN_POINT('Ctrl Pts',(-19.2461498794551,52.7740622976805,124.608685688099)) ;
#85076 = CARTESIAN_POINT('Ctrl Pts',(-19.1099523892177,52.7807756724684,124.573829556462)) ;
#85077 = CARTESIAN_POINT('Ctrl Pts',(-20.8283360085486,11.7999200508426,122.926058340311)) ;
#85078 = CARTESIAN_POINT('Ctrl Pts',(-20.8845464538574,11.8065469016607,123.090182099353)) ;
#85079 = CARTESIAN_POINT('Ctrl Pts',(-20.9394674069342,11.8197775281417,123.437524293028)) ;
#85080 = CARTESIAN_POINT('Ctrl Pts',(-20.8387914871724,11.8397531494004,123.958813977782)) ;
#85081 = CARTESIAN_POINT('Ctrl Pts',(-20.5666784354472,11.8596704843023,124.412866308854)) ;
#85082 = CARTESIAN_POINT('Ctrl Pts',(-20.1575619136445,11.8795437610183,124.747046208683)) ;
#85083 = CARTESIAN_POINT('Ctrl Pts',(-19.6551371496748,11.8995682511823,124.92249916066)) ;
#85084 = CARTESIAN_POINT('Ctrl Pts',(-19.1270451744641,11.919436092333,124.915907267661)) ;
#85085 = CARTESIAN_POINT('Ctrl Pts',(-18.6308008607008,11.9393817432125,124.729592278927)) ;
#85086 = CARTESIAN_POINT('Ctrl Pts',(-18.2288280457431,11.9592871438295,124.385624086374)) ;
#85087 = CARTESIAN_POINT('Ctrl Pts',(-17.9678591535732,11.9791613716459,123.926365470291)) ;
#85088 = CARTESIAN_POINT('Ctrl Pts',(-17.8787398474485,11.9991471625235,123.402691583813)) ;
#85089 = CARTESIAN_POINT('Ctrl Pts',(-17.9735233382965,12.0190414051832,122.882536434516)) ;
#85090 = CARTESIAN_POINT('Ctrl Pts',(-18.2387585289407,12.0389201212553,122.425519450945)) ;
#85091 = CARTESIAN_POINT('Ctrl Pts',(-18.6476197278655,12.0589595710999,122.084275218605)) ;
#85092 = CARTESIAN_POINT('Ctrl Pts',(-19.1441777499651,12.0788227326378,121.904537351317)) ;
#85093 = CARTESIAN_POINT('Ctrl Pts',(-19.6750288445506,12.098802100652,121.904738156225)) ;
#85094 = CARTESIAN_POINT('Ctrl Pts',(-20.1701856143784,12.1186126811748,122.084100255283)) ;
#85095 = CARTESIAN_POINT('Ctrl Pts',(-20.5782317220315,12.1385936094604,122.423828694064)) ;
#85096 = CARTESIAN_POINT('Ctrl Pts',(-20.8444525967082,12.1584862813298,122.880697423595)) ;
#85097 = CARTESIAN_POINT('Ctrl Pts',(-20.9398398136422,12.1784126116169,123.401645628938)) ;
#85098 = CARTESIAN_POINT('Ctrl Pts',(-20.851062860932,12.1983831657092,123.924943760388)) ;
#85099 = CARTESIAN_POINT('Ctrl Pts',(-20.6345502730467,12.2149150047968,124.307289073383)) ;
#85100 = CARTESIAN_POINT('Ctrl Pts',(-20.3891153931417,12.2282547436244,124.557618291671)) ;
#85101 = CARTESIAN_POINT('Ctrl Pts',(-20.1744356948872,12.238286985843,124.71063155409)) ;
#85102 = CARTESIAN_POINT('Ctrl Pts',(-19.9407461181023,12.2481446864865,124.82243808738)) ;
#85103 = CARTESIAN_POINT('Ctrl Pts',(-19.6879479903912,12.2581365511257,124.893369098924)) ;
#85104 = CARTESIAN_POINT('Ctrl Pts',(-19.4284766803744,12.2680591008858,124.919096784819)) ;
#85105 = CARTESIAN_POINT('Ctrl Pts',(-19.0804161519456,12.2813368743793,124.893600455121)) ;
#85106 = CARTESIAN_POINT('Ctrl Pts',(-18.7455915471493,12.2946842133199,124.776633305253)) ;
#85107 = CARTESIAN_POINT('Ctrl Pts',(-18.4584578761078,12.3078914451131,124.581565716411)) ;
#85108 = CARTESIAN_POINT('Ctrl Pts',(-18.2699644759195,12.3178785612028,124.39900581103)) ;
#85109 = CARTESIAN_POINT('Ctrl Pts',(-18.1163990348321,12.3278294667826,124.187285865335)) ;
#85110 = CARTESIAN_POINT('Ctrl Pts',(-18.0010402192528,12.33788456879,123.949600254045)) ;
#85111 = CARTESIAN_POINT('Ctrl Pts',(-17.9299289800127,12.3477062421111,123.701455973458)) ;
#85112 = CARTESIAN_POINT('Ctrl Pts',(-17.9019096964941,12.357764713186,123.438645136577)) ;
#85113 = CARTESIAN_POINT('Ctrl Pts',(-17.9200603909808,12.3676893243625,123.178453886709)) ;
#85114 = CARTESIAN_POINT('Ctrl Pts',(-18.0035385415921,12.3809666632629,122.839641054544)) ;
#85115 = CARTESIAN_POINT('Ctrl Pts',(-18.1740845283454,12.3942655425005,122.530112925337)) ;
#85116 = CARTESIAN_POINT('Ctrl Pts',(-18.4148347268114,12.4075044146712,122.278925757333)) ;
#85117 = CARTESIAN_POINT('Ctrl Pts',(-18.626729428275,12.4175110328078,122.123187062121)) ;
#85118 = CARTESIAN_POINT('Ctrl Pts',(-18.8632335737039,12.4275419778693,122.006787551109)) ;
#85119 = CARTESIAN_POINT('Ctrl Pts',(-19.1118364896857,12.4373981512211,121.934037501767)) ;
#85120 = CARTESIAN_POINT('Ctrl Pts',(-19.3729328187221,12.447397422184,121.904821743981)) ;
#85121 = CARTESIAN_POINT('Ctrl Pts',(-19.6324990778504,12.4572918739413,121.920913539679)) ;
#85122 = CARTESIAN_POINT('Ctrl Pts',(-19.8895297331301,12.4673551897507,121.982929816623)) ;
#85123 = CARTESIAN_POINT('Ctrl Pts',(-20.1266869407979,12.4771940464903,122.086036295395)) ;
#85124 = CARTESIAN_POINT('Ctrl Pts',(-20.3474074551281,12.4872601683079,122.231757371538)) ;
#85125 = CARTESIAN_POINT('Ctrl Pts',(-20.5359559653956,12.4971433960322,122.410425895404)) ;
#85126 = CARTESIAN_POINT('Ctrl Pts',(-20.6927050538892,12.5071328573109,122.620969850052)) ;
#85127 = CARTESIAN_POINT('Ctrl Pts',(-20.810144830431,12.5170965677374,122.855005173606)) ;
#85128 = CARTESIAN_POINT('Ctrl Pts',(-20.8856671720647,12.5270915704683,123.106592117066)) ;
#85129 = CARTESIAN_POINT('Ctrl Pts',(-20.916070552576,12.5371279014786,123.36856478643)) ;
#85130 = CARTESIAN_POINT('Ctrl Pts',(-20.9012433064245,12.5469741308209,123.62690469604)) ;
#85131 = CARTESIAN_POINT('Ctrl Pts',(-20.8414337010136,12.5569596290961,123.882363589347)) ;
#85132 = CARTESIAN_POINT('Ctrl Pts',(-20.7388385515527,12.5668945320791,124.122491967746)) ;
#85133 = CARTESIAN_POINT('Ctrl Pts',(-20.5941950356551,12.5769520351743,124.343654958997)) ;
#85134 = CARTESIAN_POINT('Ctrl Pts',(-20.4178326753157,12.5867736915449,124.532143914003)) ;
#85135 = CARTESIAN_POINT('Ctrl Pts',(-20.2068320884318,12.59682975421,124.691210472913)) ;
#85136 = CARTESIAN_POINT('Ctrl Pts',(-19.9738765529842,12.6067704189132,124.809442393321)) ;
#85137 = CARTESIAN_POINT('Ctrl Pts',(-19.7250875546676,12.6166748228617,124.885930317569)) ;
#85138 = CARTESIAN_POINT('Ctrl Pts',(-19.4630957051046,12.6267213078553,124.918354057249)) ;
#85139 = CARTESIAN_POINT('Ctrl Pts',(-19.2033273420661,12.636617535667,124.905216890975)) ;
#85140 = CARTESIAN_POINT('Ctrl Pts',(-18.9456557927353,12.6466771192305,124.846275394572)) ;
#85141 = CARTESIAN_POINT('Ctrl Pts',(-18.7071089141504,12.6565291288993,124.74562108305)) ;
#85142 = CARTESIAN_POINT('Ctrl Pts',(-18.4867674844916,12.6664916603389,124.604252671323)) ;
#85143 = CARTESIAN_POINT('Ctrl Pts',(-18.2932471898541,12.6765232085783,124.425230066221)) ;
#85144 = CARTESIAN_POINT('Ctrl Pts',(-18.1357855764971,12.6864146197913,124.218414587344)) ;
#85145 = CARTESIAN_POINT('Ctrl Pts',(-18.0146947587827,12.6964308734993,123.984694568915)) ;
#85146 = CARTESIAN_POINT('Ctrl Pts',(-17.9364655443542,12.706460976344,123.732995067848)) ;
#85147 = CARTESIAN_POINT('Ctrl Pts',(-17.9032103304628,12.7163174252977,123.476104767026)) ;
#85148 = CARTESIAN_POINT('Ctrl Pts',(-17.9149031126223,12.72631643607,123.213643474476)) ;
#85149 = CARTESIAN_POINT('Ctrl Pts',(-17.9711347927928,12.736211652988,122.959716591098)) ;
#85150 = CARTESIAN_POINT('Ctrl Pts',(-18.0722621730133,12.7462721683453,122.715478970838)) ;
#85151 = CARTESIAN_POINT('Ctrl Pts',(-18.2111849666589,12.7561214617324,122.497067612659)) ;
#85152 = CARTESIAN_POINT('Ctrl Pts',(-18.3885653163835,12.7661486374124,122.30221638746)) ;
#85153 = CARTESIAN_POINT('Ctrl Pts',(-18.5975514154094,12.7761772130396,122.141639073802)) ;
#85154 = CARTESIAN_POINT('Ctrl Pts',(-18.8267178958733,12.7860223065854,122.021590045095)) ;
#85155 = CARTESIAN_POINT('Ctrl Pts',(-19.0767118104658,12.7960135480172,121.94132806078)) ;
#85156 = CARTESIAN_POINT('Ctrl Pts',(-19.3380817266942,12.8060493291605,121.906076455516)) ;
#85157 = CARTESIAN_POINT('Ctrl Pts',(-19.596780887396,12.8159015348902,121.916202048577)) ;
#85158 = CARTESIAN_POINT('Ctrl Pts',(-19.8527792150898,12.8258636290072,121.970959750396)) ;
#85159 = CARTESIAN_POINT('Ctrl Pts',(-20.0967365608284,12.8358861898343,122.070232238452)) ;
#85160 = CARTESIAN_POINT('Ctrl Pts',(-20.3178000252107,12.8458139614859,122.208825541157)) ;
#85161 = CARTESIAN_POINT('Ctrl Pts',(-20.5136248486434,12.8558563456107,122.38570732732)) ;
#85162 = CARTESIAN_POINT('Ctrl Pts',(-20.67339581321,12.8657455696813,122.590690688902)) ;
#85163 = CARTESIAN_POINT('Ctrl Pts',(-20.7968031363708,12.8757348178486,122.822371490678)) ;
#85164 = CARTESIAN_POINT('Ctrl Pts',(-20.8776695418149,12.8856933948906,123.071257865387)) ;
#85165 = CARTESIAN_POINT('Ctrl Pts',(-20.9145160925794,12.8955929639819,123.328801889037)) ;
#85166 = CARTESIAN_POINT('Ctrl Pts',(-20.9058665992661,12.9056408760659,123.592681474373)) ;
#85167 = CARTESIAN_POINT('Ctrl Pts',(-20.8525411197741,12.9155362303731,123.847236588034)) ;
#85168 = CARTESIAN_POINT('Ctrl Pts',(-20.7542629977425,12.9255978808643,124.092671346512)) ;
#85169 = CARTESIAN_POINT('Ctrl Pts',(-20.6178824497922,12.9354424963268,124.312521389387)) ;
#85170 = CARTESIAN_POINT('Ctrl Pts',(-20.4440872979319,12.9454025752282,124.508228135365)) ;
#85171 = CARTESIAN_POINT('Ctrl Pts',(-20.2370284211193,12.9554407695865,124.671653791003)) ;
#85172 = CARTESIAN_POINT('Ctrl Pts',(-20.008735431722,12.9653144849861,124.795042874335)) ;
#85173 = CARTESIAN_POINT('Ctrl Pts',(-19.7576063109488,12.9753861945204,124.878511544747)) ;
#85174 = CARTESIAN_POINT('Ctrl Pts',(-19.5019831838198,12.9852186349729,124.916346652394)) ;
#85175 = CARTESIAN_POINT('Ctrl Pts',(-19.2384448043294,12.9952504558983,124.909813965164)) ;
#85176 = CARTESIAN_POINT('Ctrl Pts',(-18.9804789488314,13.0052708257839,124.856943439991)) ;
#85177 = CARTESIAN_POINT('Ctrl Pts',(-18.7391020985709,13.0151375969176,124.762195065093)) ;
#85178 = CARTESIAN_POINT('Ctrl Pts',(-18.5133119731303,13.025208368107,124.624195283185)) ;
#85179 = CARTESIAN_POINT('Ctrl Pts',(-18.3193460395093,13.0350515286286,124.453039947988)) ;
#85180 = CARTESIAN_POINT('Ctrl Pts',(-18.1551409871327,13.045031761815,124.248545739038)) ;
#85181 = CARTESIAN_POINT('Ctrl Pts',(-18.0288968334375,13.0550502818502,124.01751953666)) ;
#85182 = CARTESIAN_POINT('Ctrl Pts',(-17.9452843626105,13.0649335902339,123.771589310434)) ;
#85183 = CARTESIAN_POINT('Ctrl Pts',(-17.9050279627347,13.0750018744047,123.510130021932)) ;
#85184 = CARTESIAN_POINT('Ctrl Pts',(-17.9103427016909,13.0848320010723,123.251814495464)) ;
#85185 = CARTESIAN_POINT('Ctrl Pts',(-17.9612809092981,13.0948985732789,122.992269532793)) ;
#85186 = CARTESIAN_POINT('Ctrl Pts',(-18.0550171292814,13.1047887295196,122.749822905915)) ;
#85187 = CARTESIAN_POINT('Ctrl Pts',(-18.1903054658587,13.114781257096,122.524782428398)) ;
#85188 = CARTESIAN_POINT('Ctrl Pts',(-18.3622584156365,13.1247427469703,122.327401305476)) ;
#85189 = CARTESIAN_POINT('Ctrl Pts',(-18.5644359884156,13.1346519688575,122.163265725879)) ;
#85190 = CARTESIAN_POINT('Ctrl Pts',(-18.7952652342093,13.1447005486678,122.035044644749)) ;
#85191 = CARTESIAN_POINT('Ctrl Pts',(-19.0407361930169,13.1545835231379,121.950173803814)) ;
#85192 = CARTESIAN_POINT('Ctrl Pts',(-19.3000068336127,13.1645784342806,121.908192940554)) ;
#85193 = CARTESIAN_POINT('Ctrl Pts',(-19.5633186687248,13.1745988208542,121.912239958628)) ;
#85194 = CARTESIAN_POINT('Ctrl Pts',(-19.8190763964686,13.1845089247113,121.961246286646)) ;
#85195 = CARTESIAN_POINT('Ctrl Pts',(-20.0631402215822,13.1944366369212,122.053450497386)) ;
#85196 = CARTESIAN_POINT('Ctrl Pts',(-20.2899638294564,13.2044797466884,122.188360062557)) ;
#85197 = CARTESIAN_POINT('Ctrl Pts',(-20.4869257177344,13.214366167144,122.35780741445)) ;
#85198 = CARTESIAN_POINT('Ctrl Pts',(-20.6535775719235,13.2243593447496,122.560745126669)) ;
#85199 = CARTESIAN_POINT('Ctrl Pts',(-20.781768758078,13.2343050076535,122.788511159415)) ;
#85200 = CARTESIAN_POINT('Ctrl Pts',(-20.8689866491185,13.2442523038587,123.034949721076)) ;
#85201 = CARTESIAN_POINT('Ctrl Pts',(-20.9122331010744,13.2543000694366,123.295421612396)) ;
#85202 = CARTESIAN_POINT('Ctrl Pts',(-20.9098535935215,13.2641482826542,123.554208720169)) ;
#85203 = CARTESIAN_POINT('Ctrl Pts',(-20.862891829645,13.2741078554483,123.811687555265)) ;
#85204 = CARTESIAN_POINT('Ctrl Pts',(-20.7708019573289,13.2841444764808,124.058831482253)) ;
#85205 = CARTESIAN_POINT('Ctrl Pts',(-20.6396072016662,13.2940249912912,124.282931024446)) ;
#85206 = CARTESIAN_POINT('Ctrl Pts',(-20.4686846093292,13.3040776425982,124.484308739774)) ;
#85207 = CARTESIAN_POINT('Ctrl Pts',(-20.2685764087636,13.3139730408782,124.650446241866)) ;
#85208 = CARTESIAN_POINT('Ctrl Pts',(-20.0392572485433,13.3240231625843,124.781393384691)) ;
#85209 = CARTESIAN_POINT('Ctrl Pts',(-19.7947435724965,13.3339074421262,124.869123479395)) ;
#85210 = CARTESIAN_POINT('Ctrl Pts',(-19.5359835923959,13.3439022234181,124.914032922456)) ;
#85211 = CARTESIAN_POINT('Ctrl Pts',(-19.2745480154649,13.3538500686049,124.913233748315)) ;
#85212 = CARTESIAN_POINT('Ctrl Pts',(-19.0174771736584,13.3637870319923,124.867483970433)) ;
#85213 = CARTESIAN_POINT('Ctrl Pts',(-18.770953528208,13.3737699967295,124.777666914607)) ;
#85214 = CARTESIAN_POINT('Ctrl Pts',(-18.5426825818329,13.3838138481452,124.645222231553)) ;
#85215 = CARTESIAN_POINT('Ctrl Pts',(-18.3447626868737,13.3936420494799,124.479227338155)) ;
#85216 = CARTESIAN_POINT('Ctrl Pts',(-18.174439114941,13.403718622078,124.276543144147)) ;
#85217 = CARTESIAN_POINT('Ctrl Pts',(-18.0446799079283,13.4135707020855,124.052439270463)) ;
#85218 = CARTESIAN_POINT('Ctrl Pts',(-17.9536328215657,13.4236439870896,123.803921128187)) ;
#85219 = CARTESIAN_POINT('Ctrl Pts',(-17.908245672822,13.4334853388001,123.549293611183)) ;
#85220 = CARTESIAN_POINT('Ctrl Pts',(-17.9067874767793,13.4434468381966,123.287535568875)) ;
#85221 = CARTESIAN_POINT('Ctrl Pts',(-17.9515894545495,13.4534826143266,123.027629899913)) ;
#85222 = CARTESIAN_POINT('Ctrl Pts',(-18.0392686443259,13.4633710409642,122.783013986504)) ;
#85223 = CARTESIAN_POINT('Ctrl Pts',(-18.1693153244225,13.4733863630391,122.554183172307)) ;
#85224 = CARTESIAN_POINT('Ctrl Pts',(-18.3378376719635,13.4834167119393,122.35150318048)) ;
#85225 = CARTESIAN_POINT('Ctrl Pts',(-18.5349010784944,13.493260087546,122.183945153477)) ;
#85226 = CARTESIAN_POINT('Ctrl Pts',(-18.761992836842,13.5032895244431,122.050165209368)) ;
#85227 = CARTESIAN_POINT('Ctrl Pts',(-19.0091803607605,13.513321402376,121.958500067657)) ;
#85228 = CARTESIAN_POINT('Ctrl Pts',(-19.2631820189547,13.5231510254815,121.911588708017)) ;
#85229 = CARTESIAN_POINT('Ctrl Pts',(-19.5256857167379,13.5331404966346,121.908671418978)) ;
#85230 = CARTESIAN_POINT('Ctrl Pts',(-19.7859990638554,13.543184345397,121.952270006427)) ;
#85231 = CARTESIAN_POINT('Ctrl Pts',(-20.0294662569613,13.5530060509287,122.037953136693)) ;
#85232 = CARTESIAN_POINT('Ctrl Pts',(-20.2595578583272,13.5630410907565,122.166795368885)) ;
#85233 = CARTESIAN_POINT('Ctrl Pts',(-20.4631193550347,13.573065797648,122.334030527681)) ;
#85234 = CARTESIAN_POINT('Ctrl Pts',(-20.6320196881759,13.5829185019887,122.530273988873)) ;
#85235 = CARTESIAN_POINT('Ctrl Pts',(-20.7664821078402,13.5929066241964,122.755672189208)) ;
#85236 = CARTESIAN_POINT('Ctrl Pts',(-20.8592301070909,13.6028350943037,122.999547591303)) ;
#85237 = CARTESIAN_POINT('Ctrl Pts',(-20.9089521249442,13.6128240714709,123.257308236829)) ;
#85238 = CARTESIAN_POINT('Ctrl Pts',(-20.9127323662985,13.6228618787506,123.521057016566)) ;
#85239 = CARTESIAN_POINT('Ctrl Pts',(-20.8718783998989,13.6327081796139,123.776564736996)) ;
#85240 = CARTESIAN_POINT('Ctrl Pts',(-20.7862945910431,13.6427339229932,124.025746367502)) ;
#85241 = CARTESIAN_POINT('Ctrl Pts',(-20.6580767870656,13.6527647894322,124.256070820692)) ;
#85242 = CARTESIAN_POINT('Ctrl Pts',(-20.4954356848382,13.662602148231,124.457000727745)) ;
#85243 = CARTESIAN_POINT('Ctrl Pts',(-20.2977665459096,13.6725941091647,124.629841734287)) ;
#85244 = CARTESIAN_POINT('Ctrl Pts',(-20.0718975262772,13.6826264717213,124.765837185899)) ;
#85245 = CARTESIAN_POINT('Ctrl Pts',(-19.8300805604924,13.6924916322957,124.859254064222)) ;
#85246 = CARTESIAN_POINT('Ctrl Pts',(-19.5733470333744,13.7024535368734,124.910489003739)) ;
#85247 = CARTESIAN_POINT('Ctrl Pts',(-19.3097110945833,13.7124884669491,124.915979322584)) ;
#85248 = CARTESIAN_POINT('Ctrl Pts',(-19.052903569064,13.7223734138028,124.876639088694)) ;
#85249 = CARTESIAN_POINT('Ctrl Pts',(-18.802425491904,13.7324390901142,124.791752081939)) ;
#85250 = CARTESIAN_POINT('Ctrl Pts',(-18.5755121673576,13.7422780097491,124.667718382011)) ;
#85251 = CARTESIAN_POINT('Ctrl Pts',(-18.3688230223248,13.7523415194835,124.502800514481)) ;
#85252 = CARTESIAN_POINT('Ctrl Pts',(-18.1969779972077,13.7622351326453,124.307654410282)) ;
#85253 = CARTESIAN_POINT('Ctrl Pts',(-18.0603814063974,13.7721791394587,124.084921230377)) ;
#85254 = CARTESIAN_POINT('Ctrl Pts',(-17.9638424346081,13.782180093813,123.840436569305)) ;
#85255 = CARTESIAN_POINT('Ctrl Pts',(-17.9114952956979,13.7922188515053,123.581898288947)) ;
#85256 = CARTESIAN_POINT('Ctrl Pts',(-17.9044097597817,13.8020430356753,123.323804444879)) ;
#85257 = CARTESIAN_POINT('Ctrl Pts',(-17.942755586416,13.8121011012747,123.062308840123)) ;
#85258 = CARTESIAN_POINT('Ctrl Pts',(-18.0252033616295,13.8220311480494,122.814707785698)) ;
#85259 = CARTESIAN_POINT('Ctrl Pts',(-18.1490450109907,13.8319825903865,122.58437299172)) ;
#85260 = CARTESIAN_POINT('Ctrl Pts',(-18.312830616674,13.8420293875658,122.377301209051)) ;
#85261 = CARTESIAN_POINT('Ctrl Pts',(-18.5060204476613,13.8518773282459,122.20510405819)) ;
#85262 = CARTESIAN_POINT('Ctrl Pts',(-18.7282785603277,13.8618389595885,122.066811224224)) ;
#85263 = CARTESIAN_POINT('Ctrl Pts',(-18.9729559764164,13.8718676189644,121.968851551182)) ;
#85264 = CARTESIAN_POINT('Ctrl Pts',(-19.2278374256175,13.8817779218526,121.915423966121)) ;
#85265 = CARTESIAN_POINT('Ctrl Pts',(-19.4887668418426,13.8917128164148,121.906358743324)) ;
#85266 = CARTESIAN_POINT('Ctrl Pts',(-19.7500201068666,13.9017539150817,121.943366287556)) ;
#85267 = CARTESIAN_POINT('Ctrl Pts',(-19.997114009859,13.9116411975861,122.023756349265)) ;
#85268 = CARTESIAN_POINT('Ctrl Pts',(-20.229100640813,13.9216329380966,122.146710775795)) ;
#85269 = CARTESIAN_POINT('Ctrl Pts',(-20.435328819661,13.931583487332,122.307501482509)) ;
#85270 = CARTESIAN_POINT('Ctrl Pts',(-20.610513668173,13.9415191649668,122.501085313789)) ;
#85271 = CARTESIAN_POINT('Ctrl Pts',(-20.7503773911135,13.9515045827596,122.723134407814)) ;
#85272 = CARTESIAN_POINT('Ctrl Pts',(-20.8496809192691,13.9615333756301,122.967254089343)) ;
#85273 = CARTESIAN_POINT('Ctrl Pts',(-20.9045337829199,13.9714128868581,123.221012810142)) ;
#85274 = CARTESIAN_POINT('Ctrl Pts',(-20.9152110491903,13.981406423531,123.483425425094)) ;
#85275 = CARTESIAN_POINT('Ctrl Pts',(-20.8794859206276,13.9914386917948,123.744619970286)) ;
#85276 = CARTESIAN_POINT('Ctrl Pts',(-20.8008196116492,14.0013026538007,123.991638075795)) ;
#85277 = CARTESIAN_POINT('Ctrl Pts',(-20.6780078275285,14.0113727151456,124.226013909898)) ;
#85278 = CARTESIAN_POINT('Ctrl Pts',(-20.5199890005443,14.0212150794943,124.43079250126)) ;
#85279 = CARTESIAN_POINT('Ctrl Pts',(-20.3271803845075,14.0311757519968,124.607819487763)) ;
#85280 = CARTESIAN_POINT('Ctrl Pts',(-20.1045706887236,14.0412138230646,124.749326629548)) ;
#85281 = CARTESIAN_POINT('Ctrl Pts',(-19.8649107838462,14.051087438025,124.848860391817)) ;
#85282 = CARTESIAN_POINT('Ctrl Pts',(-19.6065853682649,14.0611596726063,124.906317466992)) ;
#85283 = CARTESIAN_POINT('Ctrl Pts',(-19.3486353561911,14.0709836910551,124.91805722916)) ;
#85284 = CARTESIAN_POINT('Ctrl Pts',(-19.0863513066081,14.0810486120311,124.884370279709)) ;
#85285 = CARTESIAN_POINT('Ctrl Pts',(-18.7548552994364,14.0942589103259,124.781024489845)) ;
#85286 = CARTESIAN_POINT('Ctrl Pts',(-18.4555139703643,14.1075743570578,124.592476583949)) ;
#85287 = CARTESIAN_POINT('Ctrl Pts',(-18.2182215362896,14.1208646023251,124.336059674344)) ;
#85288 = CARTESIAN_POINT('Ctrl Pts',(-18.0753754053462,14.1309153519322,124.113963002068)) ;
#85289 = CARTESIAN_POINT('Ctrl Pts',(-17.9751742641188,14.1407279589144,123.876319735043)) ;
#85290 = CARTESIAN_POINT('Ctrl Pts',(-17.9159189092107,14.1507990569087,123.618416063707)) ;
#85291 = CARTESIAN_POINT('Ctrl Pts',(-17.9028526558769,14.1606886296836,123.35883798821)) ;
#85292 = CARTESIAN_POINT('Ctrl Pts',(-17.9449956703198,14.1739587364869,123.012660958945)) ;
#85293 = CARTESIAN_POINT('Ctrl Pts',(-18.110043879932,14.1905754234094,122.603035428979)) ;
#85294 = CARTESIAN_POINT('Ctrl Pts',(-18.4039594470265,14.2071494667256,122.274938448092)) ;
#85295 = CARTESIAN_POINT('Ctrl Pts',(-18.6963137378166,14.2204460341574,122.08351795448)) ;
#85296 = CARTESIAN_POINT('Ctrl Pts',(-18.9385848307681,14.2304760977348,121.979689993019)) ;
#85297 = CARTESIAN_POINT('Ctrl Pts',(-19.1916875088085,14.240369989584,121.920298097705)) ;
#85298 = CARTESIAN_POINT('Ctrl Pts',(-19.5394066171243,14.2536227453696,121.899565963118)) ;
#85299 = CARTESIAN_POINT('Ctrl Pts',(-19.9747350131759,14.270350850362,121.989580778364)) ;
#85300 = CARTESIAN_POINT('Ctrl Pts',(-20.4235622970495,14.2901816868405,122.266085506153)) ;
#85301 = CARTESIAN_POINT('Ctrl Pts',(-20.7535383605483,14.3101070787307,122.680152104981)) ;
#85302 = CARTESIAN_POINT('Ctrl Pts',(-20.9224097639681,14.3300322920827,123.182173590077)) ;
#85303 = CARTESIAN_POINT('Ctrl Pts',(-20.909967365172,14.3499573055678,123.711540173755)) ;
#85304 = CARTESIAN_POINT('Ctrl Pts',(-20.7187416801209,14.3698337772678,124.204034514213)) ;
#85305 = CARTESIAN_POINT('Ctrl Pts',(-20.3693357021894,14.3898130951767,124.603894071184)) ;
#85306 = CARTESIAN_POINT('Ctrl Pts',(-19.9052962266747,14.4097460987527,124.85959923876)) ;
#85307 = CARTESIAN_POINT('Ctrl Pts',(-19.3830046122281,14.4296413687804,124.941993474064)) ;
#85308 = CARTESIAN_POINT('Ctrl Pts',(-18.863111653506,14.4495627066862,124.841603993362)) ;
#85309 = CARTESIAN_POINT('Ctrl Pts',(-18.4079099213766,14.4695203299524,124.569231338478)) ;
#85310 = CARTESIAN_POINT('Ctrl Pts',(-18.0742589102781,14.4894001619096,124.159636622647)) ;
#85311 = CARTESIAN_POINT('Ctrl Pts',(-17.8989537036202,14.5092820132065,123.661028976949)) ;
#85312 = CARTESIAN_POINT('Ctrl Pts',(-17.9053799742444,14.5293530303103,123.127680005003)) ;
#85313 = CARTESIAN_POINT('Ctrl Pts',(-18.090928041147,14.5491602540634,122.634917461125)) ;
#85314 = CARTESIAN_POINT('Ctrl Pts',(-18.4354593545979,14.5691413896322,122.230840604619)) ;
#85315 = CARTESIAN_POINT('Ctrl Pts',(-18.8964698224689,14.5890688829714,121.970192630458)) ;
#85316 = CARTESIAN_POINT('Ctrl Pts',(-19.4158400705055,14.6088895443292,121.881168125595)) ;
#85317 = CARTESIAN_POINT('Ctrl Pts',(-19.9411622969537,14.628986733551,121.976797339529)) ;
#85318 = CARTESIAN_POINT('Ctrl Pts',(-20.3952297063123,14.6487504125593,122.241401014461)) ;
#85319 = CARTESIAN_POINT('Ctrl Pts',(-20.7369043382646,14.6688076912324,122.650295252524)) ;
#85320 = CARTESIAN_POINT('Ctrl Pts',(-20.9160056364455,14.6886031149798,123.145152863214)) ;
#85321 = CARTESIAN_POINT('Ctrl Pts',(-20.9171281004685,14.7085667597074,123.675691935841)) ;
#85322 = CARTESIAN_POINT('Ctrl Pts',(-20.7357205067967,14.7285502509815,124.174887049982)) ;
#85323 = CARTESIAN_POINT('Ctrl Pts',(-20.398657784175,14.7483577461308,124.579349028364)) ;
#85324 = CARTESIAN_POINT('Ctrl Pts',(-19.9402292141674,14.7683403368509,124.847300212365)) ;
#85325 = CARTESIAN_POINT('Ctrl Pts',(-19.4202472432439,14.7882229908422,124.942207693304)) ;
#85326 = CARTESIAN_POINT('Ctrl Pts',(-18.8972710117422,14.8081812357052,124.854072619313)) ;
#85327 = CARTESIAN_POINT('Ctrl Pts',(-18.4373523571738,14.8280568227468,124.59403836842)) ;
#85328 = CARTESIAN_POINT('Ctrl Pts',(-18.0917464518894,14.8480377108821,124.190871761856)) ;
#85329 = CARTESIAN_POINT('Ctrl Pts',(-17.9052470733622,14.8679728519931,123.694860655022)) ;
#85330 = CARTESIAN_POINT('Ctrl Pts',(-17.8988327545552,14.8878848700041,123.165719308424)) ;
#85331 = CARTESIAN_POINT('Ctrl Pts',(-18.0726432682034,14.9077730882477,122.666502021473)) ;
#85332 = CARTESIAN_POINT('Ctrl Pts',(-18.3508412756587,14.9243713920946,122.324182529583)) ;
#85333 = CARTESIAN_POINT('Ctrl Pts',(-18.6332517724376,14.9376439819974,122.119434069299)) ;
#85334 = CARTESIAN_POINT('Ctrl Pts',(-18.8696162522265,14.9476513969483,122.004144120758)) ;
#85335 = CARTESIAN_POINT('Ctrl Pts',(-19.122481344444,14.9576587436809,121.931865885675)) ;
#85336 = CARTESIAN_POINT('Ctrl Pts',(-19.4692168268051,14.9709251034825,121.895493051636)) ;
#85337 = CARTESIAN_POINT('Ctrl Pts',(-19.9027943031777,14.9874397611055,121.963407923393)) ;
#85338 = CARTESIAN_POINT('Ctrl Pts',(-20.289623579524,15.0040371943481,122.175392008362)) ;
#85339 = CARTESIAN_POINT('Ctrl Pts',(-20.5428597744861,15.0173851914931,122.41816948796)) ;
#85340 = CARTESIAN_POINT('Ctrl Pts',(-20.6967684183011,15.0272809458447,122.627784026657)) ;
#85341 = CARTESIAN_POINT('Ctrl Pts',(-20.81329530157,15.0372688997761,122.862950598469)) ;
#85342 = CARTESIAN_POINT('Ctrl Pts',(-20.8871174069244,15.0472261234808,123.114018836122)) ;
#85343 = CARTESIAN_POINT('Ctrl Pts',(-20.9163251075997,15.0572616700375,123.376101669285)) ;
#85344 = CARTESIAN_POINT('Ctrl Pts',(-20.9000253490332,15.0671487813136,123.635429990405)) ;
#85345 = CARTESIAN_POINT('Ctrl Pts',(-20.8387149445651,15.0771401864144,123.890722088326)) ;
#85346 = CARTESIAN_POINT('Ctrl Pts',(-20.7344102203298,15.0870858076292,124.130366678656)) ;
#85347 = CARTESIAN_POINT('Ctrl Pts',(-20.5904612859192,15.0970350558975,124.348645357239)) ;
#85348 = CARTESIAN_POINT('Ctrl Pts',(-20.4088366867784,15.1070815510661,124.540239084563)) ;
#85349 = CARTESIAN_POINT('Ctrl Pts',(-20.2009583169496,15.1169328938577,124.694555578007)) ;
#85350 = CARTESIAN_POINT('Ctrl Pts',(-19.966949092894,15.126904673985,124.812422819299)) ;
#85351 = CARTESIAN_POINT('Ctrl Pts',(-19.7153621269984,15.1368998739627,124.888039277954)) ;
#85352 = CARTESIAN_POINT('Ctrl Pts',(-19.4534809990243,15.1469338656587,124.918615290549)) ;
#85353 = CARTESIAN_POINT('Ctrl Pts',(-19.1948823108826,15.1567892706313,124.903936975073)) ;
#85354 = CARTESIAN_POINT('Ctrl Pts',(-18.9390660225398,15.166788568477,124.844078851224)) ;
#85355 = CARTESIAN_POINT('Ctrl Pts',(-18.6998538262199,15.1766836810822,124.742011656425)) ;
#85356 = CARTESIAN_POINT('Ctrl Pts',(-18.4784349324494,15.1867443266172,124.59760214482)) ;
#85357 = CARTESIAN_POINT('Ctrl Pts',(-18.289374519982,15.1965932036064,124.420815614991)) ;
#85358 = CARTESIAN_POINT('Ctrl Pts',(-18.1305264432099,15.2066219147,124.210528253693)) ;
#85359 = CARTESIAN_POINT('Ctrl Pts',(-18.0112304288892,15.2166513159561,123.975504636893)) ;
#85360 = CARTESIAN_POINT('Ctrl Pts',(-17.9354501387818,15.2264915077521,123.728262940677)) ;
#85361 = CARTESIAN_POINT('Ctrl Pts',(-17.9027451697684,15.2364949369451,123.467452153963)) ;
#85362 = CARTESIAN_POINT('Ctrl Pts',(-17.9158870952322,15.2464804494113,123.205327859872)) ;
#85363 = CARTESIAN_POINT('Ctrl Pts',(-17.9749122216437,15.2565215457953,122.94817162508)) ;
#85364 = CARTESIAN_POINT('Ctrl Pts',(-18.075352673942,15.2663647417463,122.709774454952)) ;
#85365 = CARTESIAN_POINT('Ctrl Pts',(-18.2172239193815,15.2763510528007,122.489051700623)) ;
#85366 = CARTESIAN_POINT('Ctrl Pts',(-18.3942788891156,15.2862857380584,122.297122889139)) ;
#85367 = CARTESIAN_POINT('Ctrl Pts',(-18.6046088256348,15.2963432992754,122.137133343391)) ;
#85368 = CARTESIAN_POINT('Ctrl Pts',(-18.8338906873732,15.306164940884,122.018552182692)) ;
#85369 = CARTESIAN_POINT('Ctrl Pts',(-19.0859639637451,15.316221004475,121.939290081059)) ;
#85370 = CARTESIAN_POINT('Ctrl Pts',(-19.3450573076827,15.3261616802368,121.905856443279)) ;
#85371 = CARTESIAN_POINT('Ctrl Pts',(-19.6050966128801,15.3360660390251,121.917057614141)) ;
#85372 = CARTESIAN_POINT('Ctrl Pts',(-19.8628314894455,15.3461126936009,121.974204391667)) ;
#85373 = CARTESIAN_POINT('Ctrl Pts',(-20.1032054022461,15.3560082882438,122.073524957395)) ;
#85374 = CARTESIAN_POINT('Ctrl Pts',(-20.3263274818967,15.3660702349007,122.215360141734)) ;
#85375 = CARTESIAN_POINT('Ctrl Pts',(-20.5173806023937,15.3759198588328,122.390011089637)) ;
#85376 = CARTESIAN_POINT('Ctrl Pts',(-20.6776940933443,15.3858830978627,122.596996909064)) ;
#85377 = CARTESIAN_POINT('Ctrl Pts',(-20.8000760560513,15.3959076726385,122.830296872806)) ;
#85378 = CARTESIAN_POINT('Ctrl Pts',(-20.8793976462342,15.4058262353262,123.078576451367)) ;
#85379 = CARTESIAN_POINT('Ctrl Pts',(-20.9151255754094,15.4158184220502,123.338734291713)) ;
#85380 = CARTESIAN_POINT('Ctrl Pts',(-20.9046224904582,15.4258532206344,123.602218432797)) ;
#85381 = CARTESIAN_POINT('Ctrl Pts',(-20.8499613006373,15.4357084113081,123.855389436239)) ;
#85382 = CARTESIAN_POINT('Ctrl Pts',(-20.7510911952532,15.4457077594611,124.098804793932)) ;
#85383 = CARTESIAN_POINT('Ctrl Pts',(-20.6131053102038,15.4556028851362,124.319258702986)) ;
#85384 = CARTESIAN_POINT('Ctrl Pts',(-20.4360576038621,15.4656634280843,124.51555709839)) ;
#85385 = CARTESIAN_POINT('Ctrl Pts',(-20.2320397835465,15.4755127023512,124.674867184459)) ;
#85386 = CARTESIAN_POINT('Ctrl Pts',(-19.9996679689736,15.4855399269211,124.799102630686)) ;
#85387 = CARTESIAN_POINT('Ctrl Pts',(-19.7489910633449,15.4955683261089,124.880464971312)) ;
#85388 = CARTESIAN_POINT('Ctrl Pts',(-19.4928458279102,15.5054140765224,124.916870140584)) ;
#85389 = CARTESIAN_POINT('Ctrl Pts',(-19.2304605256444,15.5154028669231,124.908855957832)) ;
#85390 = CARTESIAN_POINT('Ctrl Pts',(-18.9721684140402,15.5254477953228,124.854455310312)) ;
#85391 = CARTESIAN_POINT('Ctrl Pts',(-18.7323714755152,15.5352722801118,124.7587411508)) ;
#85392 = CARTESIAN_POINT('Ctrl Pts',(-18.5074627778425,15.545329677653,124.619968276734)) ;
#85393 = CARTESIAN_POINT('Ctrl Pts',(-18.3128405903418,15.5552557692392,124.446263039187)) ;
#85394 = CARTESIAN_POINT('Ctrl Pts',(-18.150350868832,15.5652105543838,124.241248427742)) ;
#85395 = CARTESIAN_POINT('Ctrl Pts',(-18.0251521487945,15.5752479240414,124.009084692641)) ;
#85396 = CARTESIAN_POINT('Ctrl Pts',(-17.9432016162711,15.585136734163,123.762469410516)) ;
#85397 = CARTESIAN_POINT('Ctrl Pts',(-17.9044670409744,15.5951260932141,123.502838762861)) ;
#85398 = CARTESIAN_POINT('Ctrl Pts',(-17.9115749765126,15.6050846406702,123.24124293323)) ;
#85399 = CARTESIAN_POINT('Ctrl Pts',(-17.9630623576573,15.6149842172212,122.986221570105)) ;
#85400 = CARTESIAN_POINT('Ctrl Pts',(-18.0595417871603,15.6250321290519,122.740459685975)) ;
#85401 = CARTESIAN_POINT('Ctrl Pts',(-18.1949986414737,15.6349274769125,122.518438659765)) ;
#85402 = CARTESIAN_POINT('Ctrl Pts',(-18.3697629356532,15.6449891534437,122.320059129432)) ;
#85403 = CARTESIAN_POINT('Ctrl Pts',(-18.5718644577124,15.6548336711928,122.158541982419)) ;
#85404 = CARTESIAN_POINT('Ctrl Pts',(-18.8011526189207,15.6647941149076,122.032301199326)) ;
#85405 = CARTESIAN_POINT('Ctrl Pts',(-19.0509357609831,15.6748309477258,121.947606476504)) ;
#85406 = CARTESIAN_POINT('Ctrl Pts',(-19.3074921480599,15.6847097444726,121.907773626489)) ;
#85407 = CARTESIAN_POINT('Ctrl Pts',(-19.5717593834283,15.694769060601,121.913104494787)) ;
#85408 = CARTESIAN_POINT('Ctrl Pts',(-19.8262605890557,15.7046395073542,121.963283380412)) ;
#85409 = CARTESIAN_POINT('Ctrl Pts',(-20.0714198955884,15.7146321456122,122.057380334014)) ;
#85410 = CARTESIAN_POINT('Ctrl Pts',(-20.2971021415107,15.7246641611601,122.193630102715)) ;
#85411 = CARTESIAN_POINT('Ctrl Pts',(-20.4928065396954,15.7345300174667,122.363722707075)) ;
#85412 = CARTESIAN_POINT('Ctrl Pts',(-20.659353254304,15.7445993069358,122.569307538849)) ;
#85413 = CARTESIAN_POINT('Ctrl Pts',(-20.7848456281026,15.7544428644871,122.795525024093)) ;
#85414 = CARTESIAN_POINT('Ctrl Pts',(-20.8711257023825,15.764422991275,123.043184928911)) ;
#85415 = CARTESIAN_POINT('Ctrl Pts',(-20.9127559215498,15.7744415398749,123.303142599032)) ;
#85416 = CARTESIAN_POINT('Ctrl Pts',(-20.9092242705699,15.7843248403981,123.562873547571)) ;
#85417 = CARTESIAN_POINT('Ctrl Pts',(-20.8596396741269,15.7943931274462,123.822725252708)) ;
#85418 = CARTESIAN_POINT('Ctrl Pts',(-20.7681651750302,15.8042232504649,124.064360555124)) ;
#85419 = CARTESIAN_POINT('Ctrl Pts',(-20.6332871001612,15.8142898343902,124.291882100143)) ;
#85420 = CARTESIAN_POINT('Ctrl Pts',(-20.4638049151612,15.8241799474047,124.48896825144)) ;
#85421 = CARTESIAN_POINT('Ctrl Pts',(-20.2609877478758,15.8341726361673,124.655734358688)) ;
#85422 = CARTESIAN_POINT('Ctrl Pts',(-20.0329028474693,15.8441335245231,124.784198130911)) ;
#85423 = CARTESIAN_POINT('Ctrl Pts',(-19.7872175767508,15.8540514694031,124.871145968037)) ;
#85424 = CARTESIAN_POINT('Ctrl Pts',(-19.5278485703835,15.8640592224993,124.914811107078)) ;
#85425 = CARTESIAN_POINT('Ctrl Pts',(-19.2642689030462,15.8740903164583,124.91223920911)) ;
#85426 = CARTESIAN_POINT('Ctrl Pts',(-19.0097316360131,15.8839382844863,124.865387875955)) ;
#85427 = CARTESIAN_POINT('Ctrl Pts',(-18.761882854262,15.8940002406122,124.773318370912)) ;
#85428 = CARTESIAN_POINT('Ctrl Pts',(-18.5376157807696,15.9038974522133,124.641576258663)) ;
#85429 = CARTESIAN_POINT('Ctrl Pts',(-18.3384056514573,15.9138286188779,124.472982338498)) ;
#85430 = CARTESIAN_POINT('Ctrl Pts',(-18.1698491513015,15.9238708030821,124.269933564785)) ;
#85431 = CARTESIAN_POINT('Ctrl Pts',(-18.0409623377378,15.9337574713353,124.044330723478)) ;
#85432 = CARTESIAN_POINT('Ctrl Pts',(-17.9518555076836,15.9437505833135,123.79731633989)) ;
#85433 = CARTESIAN_POINT('Ctrl Pts',(-17.9072992563308,15.9536962609293,123.539779663906)) ;
#85434 = CARTESIAN_POINT('Ctrl Pts',(-17.9076038590327,15.9636435639143,123.278362513842)) ;
#85435 = CARTESIAN_POINT('Ctrl Pts',(-17.954039484633,15.9736912876611,123.018441119269)) ;
#85436 = CARTESIAN_POINT('Ctrl Pts',(-18.0429092629221,15.9835396614236,122.77537631077)) ;
#85437 = CARTESIAN_POINT('Ctrl Pts',(-18.1733362386872,15.9934986338693,122.548480377477)) ;
#85438 = CARTESIAN_POINT('Ctrl Pts',(-18.3428858266523,16.0035374957505,122.346380568049)) ;
#85439 = CARTESIAN_POINT('Ctrl Pts',(-18.5414869910732,16.0134160999223,122.179156901752)) ;
#85440 = CARTESIAN_POINT('Ctrl Pts',(-18.7699271953843,16.0234676411256,122.046612208989)) ;
#85441 = CARTESIAN_POINT('Ctrl Pts',(-19.0141072069317,16.0333630391059,121.957051725276)) ;
#85442 = CARTESIAN_POINT('Ctrl Pts',(-19.2740547380586,16.0434142716512,121.910401805192)) ;
#85443 = CARTESIAN_POINT('Ctrl Pts',(-19.5338803406111,16.0533004622755,121.909579455401)) ;
#85444 = CARTESIAN_POINT('Ctrl Pts',(-19.7926868268136,16.0632930015913,121.953875934243)) ;
#85445 = CARTESIAN_POINT('Ctrl Pts',(-20.0387894173471,16.073241447486,122.04213980991)) ;
#85446 = CARTESIAN_POINT('Ctrl Pts',(-20.265712566684,16.0831782500179,122.171300244256)) ;
#85447 = CARTESIAN_POINT('Ctrl Pts',(-20.4679516213838,16.0931612574692,122.338455368566)) ;
#85448 = CARTESIAN_POINT('Ctrl Pts',(-20.6387206153012,16.103205098884,122.539669360996)) ;
#85449 = CARTESIAN_POINT('Ctrl Pts',(-20.7696595815421,16.1130332975079,122.762338547933)) ;
#85450 = CARTESIAN_POINT('Ctrl Pts',(-20.8623125592493,16.1231098909501,123.010343765831)) ;
#85451 = CARTESIAN_POINT('Ctrl Pts',(-20.9095729442255,16.1329618902917,123.264952690282)) ;
#85452 = CARTESIAN_POINT('Ctrl Pts',(-20.9121762627497,16.1430354771156,123.529617389355)) ;
#85453 = CARTESIAN_POINT('Ctrl Pts',(-20.869730533684,16.152875702213,123.784725112839)) ;
#85454 = CARTESIAN_POINT('Ctrl Pts',(-20.7834213237411,16.1628414062417,124.031959888329)) ;
#85455 = CARTESIAN_POINT('Ctrl Pts',(-20.6543616553613,16.1728680395483,124.261695407877)) ;
#85456 = CARTESIAN_POINT('Ctrl Pts',(-20.4893937694131,16.1827823352601,124.463343826805)) ;
#85457 = CARTESIAN_POINT('Ctrl Pts',(-20.2907385375805,16.1927706239526,124.634927879414)) ;
#85458 = CARTESIAN_POINT('Ctrl Pts',(-20.063944204818,16.2028093571109,124.769667401044)) ;
#85459 = CARTESIAN_POINT('Ctrl Pts',(-19.8221495313365,16.2126526889385,124.861577146822)) ;
#85460 = CARTESIAN_POINT('Ctrl Pts',(-19.5634230879079,16.2226804148181,124.911613949581)) ;
#85461 = CARTESIAN_POINT('Ctrl Pts',(-19.2997995110888,16.2327127512066,124.915252649983)) ;
#85462 = CARTESIAN_POINT('Ctrl Pts',(-19.0447508850932,16.2425422515072,124.87443461805)) ;
#85463 = CARTESIAN_POINT('Ctrl Pts',(-18.7964127409365,16.252531755424,124.789315485236)) ;
#85464 = CARTESIAN_POINT('Ctrl Pts',(-18.5657100501157,16.2625755959364,124.661096709419)) ;
#85465 = CARTESIAN_POINT('Ctrl Pts',(-18.3649684583117,16.2723973017045,124.498860195946)) ;
#85466 = CARTESIAN_POINT('Ctrl Pts',(-18.1912776614032,16.2824323488368,124.30043121603)) ;
#85467 = CARTESIAN_POINT('Ctrl Pts',(-18.0554378922695,16.2924570262737,124.074705597496)) ;
#85468 = CARTESIAN_POINT('Ctrl Pts',(-17.9619696621494,16.3023098411282,123.833243322249)) ;
#85469 = CARTESIAN_POINT('Ctrl Pts',(-17.9107123152974,16.3122975507357,123.575850309162)) ;
#85470 = CARTESIAN_POINT('Ctrl Pts',(-17.9049458569947,16.3222275607298,123.314954275145)) ;
#85471 = CARTESIAN_POINT('Ctrl Pts',(-17.9444047205986,16.332217315949,123.055411337041)) ;
#85472 = CARTESIAN_POINT('Ctrl Pts',(-18.0289611024086,16.3422439246319,122.805854001657)) ;
#85473 = CARTESIAN_POINT('Ctrl Pts',(-18.1535398915879,16.3521278646537,122.577945287591)) ;
#85474 = CARTESIAN_POINT('Ctrl Pts',(-18.3170581793031,16.3621170921922,122.372577155451)) ;
#85475 = CARTESIAN_POINT('Ctrl Pts',(-18.5151613636324,16.3721599627159,122.198204531201)) ;
#85476 = CARTESIAN_POINT('Ctrl Pts',(-18.7355937159182,16.3819923494713,122.06340510794)) ;
#85477 = CARTESIAN_POINT('Ctrl Pts',(-18.9797379454661,16.3919856426429,121.966674506609)) ;
#85478 = CARTESIAN_POINT('Ctrl Pts',(-19.2380933202206,16.4020176482913,121.914136786792)) ;
#85479 = CARTESIAN_POINT('Ctrl Pts',(-19.4972319162803,16.4118829042603,121.907050750478)) ;
#85480 = CARTESIAN_POINT('Ctrl Pts',(-19.7563049005742,16.4218447841678,121.944708800064)) ;
#85481 = CARTESIAN_POINT('Ctrl Pts',(-20.0065704728934,16.4318797175297,122.027782317763)) ;
#85482 = CARTESIAN_POINT('Ctrl Pts',(-20.235395236987,16.441764675909,122.150815185132)) ;
#85483 = CARTESIAN_POINT('Ctrl Pts',(-20.4430095418267,16.4518303028317,122.314647056948)) ;
#85484 = CARTESIAN_POINT('Ctrl Pts',(-20.6153156253427,16.461669408496,122.507485556433)) ;
#85485 = CARTESIAN_POINT('Ctrl Pts',(-20.7548759132793,16.4717322235013,122.732057555602)) ;
#85486 = CARTESIAN_POINT('Ctrl Pts',(-20.8514951454901,16.48162842955,122.973534637153)) ;
#85487 = CARTESIAN_POINT('Ctrl Pts',(-20.9056579365925,16.4915692525753,123.229061857975)) ;
#85488 = CARTESIAN_POINT('Ctrl Pts',(-20.9147539350784,16.501573835554,123.491844043348)) ;
#85489 = CARTESIAN_POINT('Ctrl Pts',(-20.8777116944424,16.5115947299987,123.752558207369)) ;
#85490 = CARTESIAN_POINT('Ctrl Pts',(-20.7973193962089,16.5214866505881,123.9997713371)) ;
#85491 = CARTESIAN_POINT('Ctrl Pts',(-20.6743097948123,16.5314800829335,124.231787262463)) ;
#85492 = CARTESIAN_POINT('Ctrl Pts',(-20.5135843010475,16.5414256878334,124.437884102592)) ;
#85493 = CARTESIAN_POINT('Ctrl Pts',(-20.3198274952116,16.5513729613149,124.613376926942)) ;
#85494 = CARTESIAN_POINT('Ctrl Pts',(-20.0961655477988,16.5614208757913,124.753706244345)) ;
#85495 = CARTESIAN_POINT('Ctrl Pts',(-19.8564832755268,16.5712685161386,124.851295914385)) ;
#85496 = CARTESIAN_POINT('Ctrl Pts',(-19.6007546274818,16.5812302315152,124.907216087891)) ;
#85497 = CARTESIAN_POINT('Ctrl Pts',(-19.3374019357033,16.591258855088,124.917623305779)) ;
#85498 = CARTESIAN_POINT('Ctrl Pts',(-19.0793392609636,16.6011692171544,124.882650735253)) ;
#85499 = CARTESIAN_POINT('Ctrl Pts',(-18.8304294039593,16.6111039108068,124.803856446845)) ;
#85500 = CARTESIAN_POINT('Ctrl Pts',(-18.596627686363,16.6211457539347,124.681515843378)) ;
#85501 = CARTESIAN_POINT('Ctrl Pts',(-18.3907224983714,16.6310302595051,124.523120625139)) ;
#85502 = CARTESIAN_POINT('Ctrl Pts',(-18.213179611499,16.6410323632903,124.329353348425)) ;
#85503 = CARTESIAN_POINT('Ctrl Pts',(-18.0729347335421,16.6509507147053,124.109605240172)) ;
#85504 = CARTESIAN_POINT('Ctrl Pts',(-17.9717684511152,16.6609983707262,123.865757550208)) ;
#85505 = CARTESIAN_POINT('Ctrl Pts',(-17.9151801485084,16.6708695637544,123.612544609832)) ;
#85506 = CARTESIAN_POINT('Ctrl Pts',(-17.9031486210089,16.6809352768979,123.348363900477)) ;
#85507 = CARTESIAN_POINT('Ctrl Pts',(-17.9361680628292,16.6907877374706,123.091490849331)) ;
#85508 = CARTESIAN_POINT('Ctrl Pts',(-18.041350571431,16.7042162001931,122.754758769299)) ;
#85509 = CARTESIAN_POINT('Ctrl Pts',(-18.2267930848674,16.7172971477102,122.460500377085)) ;
#85510 = CARTESIAN_POINT('Ctrl Pts',(-18.4863600281543,16.7307716459448,122.219764136354)) ;
#85511 = CARTESIAN_POINT('Ctrl Pts',(-18.7036600720593,16.7406037495542,122.079903461464)) ;
#85512 = CARTESIAN_POINT('Ctrl Pts',(-18.9447043729808,16.7505696526809,121.977589420528)) ;
#85513 = CARTESIAN_POINT('Ctrl Pts',(-19.2015822289623,16.7605970619911,121.918702174221)) ;
#85514 = CARTESIAN_POINT('Ctrl Pts',(-19.4616612966653,16.7705080933577,121.90540119112)) ;
#85515 = CARTESIAN_POINT('Ctrl Pts',(-19.8072674417979,16.7837524009787,121.947145247852)) ;
#85516 = CARTESIAN_POINT('Ctrl Pts',(-20.2188607320283,16.8004528836499,122.113061781685)) ;
#85517 = CARTESIAN_POINT('Ctrl Pts',(-20.5455735820307,16.8169597128057,122.405977428994)) ;
#85518 = CARTESIAN_POINT('Ctrl Pts',(-20.7373318770542,16.8302703410433,122.698474315006)) ;
#85519 = CARTESIAN_POINT('Ctrl Pts',(-20.8410538416381,16.8402629045834,122.939759731386)) ;
#85520 = CARTESIAN_POINT('Ctrl Pts',(-20.9012068159582,16.8502929875849,123.196350988495)) ;
#85521 = CARTESIAN_POINT('Ctrl Pts',(-20.9212193192341,16.8634665915827,123.542025913649)) ;
#85522 = CARTESIAN_POINT('Ctrl Pts',(-20.832303368653,16.8801042968141,123.975028581527)) ;
#85523 = CARTESIAN_POINT('Ctrl Pts',(-20.5559527242748,16.8999860593815,124.425665773585)) ;
#85524 = CARTESIAN_POINT('Ctrl Pts',(-20.2087278908941,16.916682411598,124.701769095248)) ;
#85525 = CARTESIAN_POINT('Ctrl Pts',(-19.8917137009118,16.9298394393871,124.83996615317)) ;
#85526 = CARTESIAN_POINT('Ctrl Pts',(-19.5501593226237,16.9432167940307,124.923024211938)) ;
#85527 = CARTESIAN_POINT('Ctrl Pts',(-19.1108610444918,16.9597476282895,124.912764903616)) ;
#85528 = CARTESIAN_POINT('Ctrl Pts',(-18.6161741406845,16.9797123180326,124.720936570403)) ;
#85529 = CARTESIAN_POINT('Ctrl Pts',(-18.2178875673859,16.9996288114562,124.372240740112)) ;
#85530 = CARTESIAN_POINT('Ctrl Pts',(-17.9619000053034,17.0195185308058,123.909658769635)) ;
#85531 = CARTESIAN_POINT('Ctrl Pts',(-17.8790923718899,17.0395252604536,123.384478022634)) ;
#85532 = CARTESIAN_POINT('Ctrl Pts',(-17.9792607793457,17.0593633141005,122.866706624068)) ;
#85533 = CARTESIAN_POINT('Ctrl Pts',(-18.251654980879,17.0793566523141,122.410555995914)) ;
#85534 = CARTESIAN_POINT('Ctrl Pts',(-18.6614413308425,17.0992394517207,122.076728435462)) ;
#85535 = CARTESIAN_POINT('Ctrl Pts',(-19.1602498824996,17.1191316326394,121.901928665033)) ;
#85536 = CARTESIAN_POINT('Ctrl Pts',(-19.6893506726758,17.1390338111345,121.906954280708)) ;
#85537 = CARTESIAN_POINT('Ctrl Pts',(-20.1877372859541,17.1590711223382,122.094250728715)) ;
#85538 = CARTESIAN_POINT('Ctrl Pts',(-20.5885147516778,17.1788835638791,122.436171529998)) ;
#85539 = CARTESIAN_POINT('Ctrl Pts',(-20.8514859106502,17.198948804614,122.899836288904)) ;
#85540 = CARTESIAN_POINT('Ctrl Pts',(-20.9395751047835,17.2187060094698,123.417764524091)) ;
#85541 = CARTESIAN_POINT('Ctrl Pts',(-20.8451902721094,17.2387392821155,123.941511312625)) ;
#85542 = CARTESIAN_POINT('Ctrl Pts',(-20.5803738327966,17.2585521905694,124.396949460866)) ;
#85543 = CARTESIAN_POINT('Ctrl Pts',(-20.1731152784338,17.2785483366968,124.738041234505)) ;
#85544 = CARTESIAN_POINT('Ctrl Pts',(-19.6769118272769,17.2984100899193,124.918872799759)) ;
#85545 = CARTESIAN_POINT('Ctrl Pts',(-19.1436416860639,17.3184786070474,124.919193987262)) ;
#85546 = CARTESIAN_POINT('Ctrl Pts',(-18.648109623505,17.3383094800442,124.739265310968)) ;
#85547 = CARTESIAN_POINT('Ctrl Pts',(-18.2411319113203,17.3582313908609,124.40073894506)) ;
#85548 = CARTESIAN_POINT('Ctrl Pts',(-17.9740323769222,17.3781608342962,123.94322080473)) ;
#85549 = CARTESIAN_POINT('Ctrl Pts',(-17.8790250602224,17.3980705044126,123.422734778079)) ;
#85550 = CARTESIAN_POINT('Ctrl Pts',(-17.9662662127267,17.4179438616755,122.901724773555)) ;
#85551 = CARTESIAN_POINT('Ctrl Pts',(-18.2276294818176,17.4379353962934,122.439190238654)) ;
#85552 = CARTESIAN_POINT('Ctrl Pts',(-18.6285734387837,17.4578010137041,122.095521594485)) ;
#85553 = CARTESIAN_POINT('Ctrl Pts',(-19.1253152085356,17.4777819435324,121.907762643509)) ;
#85554 = CARTESIAN_POINT('Ctrl Pts',(-19.6552200286643,17.4977204056155,121.901390129916)) ;
#85555 = CARTESIAN_POINT('Ctrl Pts',(-20.1546489410619,17.5176125988372,122.075060293898)) ;
#85556 = CARTESIAN_POINT('Ctrl Pts',(-20.5661552710587,17.5375833138726,122.410136115304)) ;
#85557 = CARTESIAN_POINT('Ctrl Pts',(-20.837318013256,17.5573929855387,122.861593772204)) ;
#85558 = CARTESIAN_POINT('Ctrl Pts',(-20.9394053743083,17.5773862022299,123.382882566089)) ;
#85559 = CARTESIAN_POINT('Ctrl Pts',(-20.8584272459729,17.5972371144262,123.904456907226)) ;
#85560 = CARTESIAN_POINT('Ctrl Pts',(-20.6013722647494,17.6173117207453,124.371835879059)) ;
#85561 = CARTESIAN_POINT('Ctrl Pts',(-20.2709413387604,17.6338283526286,124.661087804809)) ;
#85562 = CARTESIAN_POINT('Ctrl Pts',(-19.9567456572262,17.6471670603227,124.816311506479)) ;
#85563 = CARTESIAN_POINT('Ctrl Pts',(-19.7085634180374,17.657009434631,124.889285728244)) ;
#85564 = CARTESIAN_POINT('Ctrl Pts',(-19.4460346302332,17.6670644546137,124.918920394545)) ;
#85565 = CARTESIAN_POINT('Ctrl Pts',(-19.0989340056819,17.6802966112713,124.897325675655)) ;
#85566 = CARTESIAN_POINT('Ctrl Pts',(-18.6800921880835,17.6969115786164,124.757498322391)) ;
#85567 = CARTESIAN_POINT('Ctrl Pts',(-18.3346383771164,17.7135061656276,124.483309875907)) ;
#85568 = CARTESIAN_POINT('Ctrl Pts',(-18.1268953740658,17.726739733983,124.204383339548)) ;
#85569 = CARTESIAN_POINT('Ctrl Pts',(-18.0083495823601,17.7367833517917,123.968592623646)) ;
#85570 = CARTESIAN_POINT('Ctrl Pts',(-17.9336310060421,17.7466702760265,123.71972753629)) ;
#85571 = CARTESIAN_POINT('Ctrl Pts',(-17.9024800444537,17.7566609304733,123.459055825321)) ;
#85572 = CARTESIAN_POINT('Ctrl Pts',(-17.91707504202,17.7666226889273,123.197677226246)) ;
#85573 = CARTESIAN_POINT('Ctrl Pts',(-17.9967448142101,17.7799625539945,122.856223951778)) ;
#85574 = CARTESIAN_POINT('Ctrl Pts',(-18.1639793074523,17.7932713369078,122.544584740488)) ;
#85575 = CARTESIAN_POINT('Ctrl Pts',(-18.4009261605596,17.8064670943519,122.291390427509)) ;
#85576 = CARTESIAN_POINT('Ctrl Pts',(-18.6098409160699,17.8164289780284,122.133625520298)) ;
#85577 = CARTESIAN_POINT('Ctrl Pts',(-18.8450658298774,17.826472087543,122.013949993326)) ;
#85578 = CARTESIAN_POINT('Ctrl Pts',(-19.092621766734,17.8363243375422,121.938100172443)) ;
#85579 = CARTESIAN_POINT('Ctrl Pts',(-19.3525817752957,17.8462958744927,121.905367673207)) ;
#85580 = CARTESIAN_POINT('Ctrl Pts',(-19.6149678521797,17.8562911399702,121.918326097359)) ;
#85581 = CARTESIAN_POINT('Ctrl Pts',(-19.8719764054818,17.8663251128439,121.977174194731)) ;
#85582 = CARTESIAN_POINT('Ctrl Pts',(-20.1107443124788,17.8761805276062,122.07756701248)) ;
#85583 = CARTESIAN_POINT('Ctrl Pts',(-20.3317665609879,17.886179805115,122.219601552815)) ;
#85584 = CARTESIAN_POINT('Ctrl Pts',(-20.5230159036683,17.896074989278,122.39585448978)) ;
#85585 = CARTESIAN_POINT('Ctrl Pts',(-20.6833174072794,17.9061353689188,122.60604307054)) ;
#85586 = CARTESIAN_POINT('Ctrl Pts',(-20.8023179831757,17.9159852379269,122.835939812967)) ;
#85587 = CARTESIAN_POINT('Ctrl Pts',(-20.8815806037002,17.9260167991348,123.08734301173)) ;
#85588 = CARTESIAN_POINT('Ctrl Pts',(-20.9153942834191,17.9360272480171,123.348249186297)) ;
#85589 = CARTESIAN_POINT('Ctrl Pts',(-20.9038056440646,17.9459339874341,123.608321329956)) ;
#85590 = CARTESIAN_POINT('Ctrl Pts',(-20.8475549821368,17.9558720035025,123.863336913945)) ;
#85591 = CARTESIAN_POINT('Ctrl Pts',(-20.7473491124227,17.9658772499537,124.106450718163)) ;
#85592 = CARTESIAN_POINT('Ctrl Pts',(-20.6056897092289,17.97591131101,124.328835897672)) ;
#85593 = CARTESIAN_POINT('Ctrl Pts',(-20.4312337067048,17.9857563920681,124.519908095883)) ;
#85594 = CARTESIAN_POINT('Ctrl Pts',(-20.2236664013566,17.9957421980216,124.680396433313)) ;
#85595 = CARTESIAN_POINT('Ctrl Pts',(-19.992579689612,18.0056770185758,124.801991034309)) ;
#85596 = CARTESIAN_POINT('Ctrl Pts',(-19.7408295621782,18.015734543708,124.882346278087)) ;
#85597 = CARTESIAN_POINT('Ctrl Pts',(-19.4850812770158,18.0255561943594,124.917339204616)) ;
#85598 = CARTESIAN_POINT('Ctrl Pts',(-19.2210175734843,18.0356122578641,124.907651917327)) ;
#85599 = CARTESIAN_POINT('Ctrl Pts',(-18.9656796380445,18.045552924928,124.85243013731)) ;
#85600 = CARTESIAN_POINT('Ctrl Pts',(-18.7243886052584,18.055457318594,124.754831562349)) ;
#85601 = CARTESIAN_POINT('Ctrl Pts',(-18.5006574893832,18.065503842357,124.61470975614)) ;
#85602 = CARTESIAN_POINT('Ctrl Pts',(-18.307369291185,18.0753999253734,124.440656203214)) ;
#85603 = CARTESIAN_POINT('Ctrl Pts',(-18.1445872821212,18.0854666246034,124.232186912263)) ;
#85604 = CARTESIAN_POINT('Ctrl Pts',(-18.0231672453592,18.0952902350045,124.004324151478)) ;
#85605 = CARTESIAN_POINT('Ctrl Pts',(-17.9408459619243,18.105346095182,123.753251808151)) ;
#85606 = CARTESIAN_POINT('Ctrl Pts',(-17.9041508391774,18.1152792414869,123.494778928388)) ;
#85607 = CARTESIAN_POINT('Ctrl Pts',(-17.9123669611964,18.1252244972575,123.233587463902)) ;
#85608 = CARTESIAN_POINT('Ctrl Pts',(-17.965820602866,18.135207795696,122.976706518041)) ;
#85609 = CARTESIAN_POINT('Ctrl Pts',(-18.063904304486,18.1452449758426,122.731876350353)) ;
#85610 = CARTESIAN_POINT('Ctrl Pts',(-18.2001593676184,18.1550995285521,122.511623169625)) ;
#85611 = CARTESIAN_POINT('Ctrl Pts',(-18.3748041349657,18.1650990469994,122.315340175389)) ;
#85612 = CARTESIAN_POINT('Ctrl Pts',(-18.5786232758408,18.1749941294615,122.153792991792)) ;
#85613 = CARTESIAN_POINT('Ctrl Pts',(-18.8111647901301,18.1850546749676,122.028081402506)) ;
#85614 = CARTESIAN_POINT('Ctrl Pts',(-19.0567404030301,18.1949039822156,121.94625334283)) ;
#85615 = CARTESIAN_POINT('Ctrl Pts',(-19.3172903973273,18.204931072303,121.906964506293)) ;
#85616 = CARTESIAN_POINT('Ctrl Pts',(-19.5807510422382,18.2149599764399,121.914213939927)) ;
#85617 = CARTESIAN_POINT('Ctrl Pts',(-19.8342692925352,18.2248038415392,121.965616328592)) ;
#85618 = CARTESIAN_POINT('Ctrl Pts',(-20.0789732695833,18.2347996682476,122.061118208397)) ;
#85619 = CARTESIAN_POINT('Ctrl Pts',(-20.3037898720174,18.2448248848966,122.198476327115)) ;
#85620 = CARTESIAN_POINT('Ctrl Pts',(-20.4989049499709,18.2547147170542,122.37016702887)) ;
#85621 = CARTESIAN_POINT('Ctrl Pts',(-20.6631753421901,18.2647055731389,122.574966335763)) ;
#85622 = CARTESIAN_POINT('Ctrl Pts',(-20.788773377905,18.2746506677318,122.804154170433)) ;
#85623 = CARTESIAN_POINT('Ctrl Pts',(-20.8731939482788,18.2846025714999,123.051690442556)) ;
#85624 = CARTESIAN_POINT('Ctrl Pts',(-20.9134619567521,18.2946389709693,123.312337432225)) ;
#85625 = CARTESIAN_POINT('Ctrl Pts',(-20.9081339354844,18.304528041058,123.572166354225)) ;
#85626 = CARTESIAN_POINT('Ctrl Pts',(-20.8577276976876,18.3145173304289,123.829783197126)) ;
#85627 = CARTESIAN_POINT('Ctrl Pts',(-20.7634652567705,18.3244758966386,124.073909818492)) ;
#85628 = CARTESIAN_POINT('Ctrl Pts',(-20.6295842577516,18.3343754678554,124.296985254271)) ;
#85629 = CARTESIAN_POINT('Ctrl Pts',(-20.4564060477001,18.3444233822697,124.496275231277)) ;
#85630 = CARTESIAN_POINT('Ctrl Pts',(-20.2544457726215,18.3543187251302,124.660147079943)) ;
#85631 = CARTESIAN_POINT('Ctrl Pts',(-20.0233589167788,18.3643804190777,124.788582887775)) ;
#85632 = CARTESIAN_POINT('Ctrl Pts',(-19.7788516309637,18.3742248721618,124.873135508736)) ;
#85633 = CARTESIAN_POINT('Ctrl Pts',(-19.5205311753707,18.3841855571203,124.915333903471)) ;
#85634 = CARTESIAN_POINT('Ctrl Pts',(-19.2568158507944,18.3942214896288,124.91156959599)) ;
#85635 = CARTESIAN_POINT('Ctrl Pts',(-19.0015267672572,18.4041101053169,124.863056912793)) ;
#85636 = CARTESIAN_POINT('Ctrl Pts',(-18.7552413200576,18.4141245144593,124.770264913515)) ;
#85637 = CARTESIAN_POINT('Ctrl Pts',(-18.5287491933341,18.4241583234171,124.635287434208)) ;
#85638 = CARTESIAN_POINT('Ctrl Pts',(-18.3326736838035,18.4339887776733,124.467040337069)) ;
#85639 = CARTESIAN_POINT('Ctrl Pts',(-18.1646552309895,18.4440664452515,124.262399712302)) ;
#85640 = CARTESIAN_POINT('Ctrl Pts',(-18.0374628156085,18.4539183133737,124.036835965427)) ;
#85641 = CARTESIAN_POINT('Ctrl Pts',(-17.9492624861745,18.4639913509391,123.787301761498)) ;
#85642 = CARTESIAN_POINT('Ctrl Pts',(-17.9067521481246,18.47383390429,123.532143869047)) ;
#85643 = CARTESIAN_POINT('Ctrl Pts',(-17.9083434021815,18.4838142997834,123.269885593791)) ;
#85644 = CARTESIAN_POINT('Ctrl Pts',(-17.9561323187471,18.4938327777612,123.010990190508)) ;
#85645 = CARTESIAN_POINT('Ctrl Pts',(-18.0463999219275,18.5037160920673,122.767424084949)) ;
#85646 = CARTESIAN_POINT('Ctrl Pts',(-18.1801054394556,18.513784394606,122.53915993018)) ;
#85647 = CARTESIAN_POINT('Ctrl Pts',(-18.3471840847822,18.5236144418794,122.342083268111)) ;
#85648 = CARTESIAN_POINT('Ctrl Pts',(-18.5504477114517,18.5336813132949,122.172834206145)) ;
#85649 = CARTESIAN_POINT('Ctrl Pts',(-18.7760961055222,18.543570352094,122.043850044035)) ;
#85650 = CARTESIAN_POINT('Ctrl Pts',(-19.0231397001699,18.5535670502281,121.954587201367)) ;
#85651 = CARTESIAN_POINT('Ctrl Pts',(-19.2808470530102,18.5635194759401,121.909875533707)) ;
#85652 = CARTESIAN_POINT('Ctrl Pts',(-19.5420744376569,18.573460778173,121.910226123319)) ;
#85653 = CARTESIAN_POINT('Ctrl Pts',(-19.8004561957054,18.5834440172569,121.955853427861)) ;
#85654 = CARTESIAN_POINT('Ctrl Pts',(-20.048172080969,18.5934828188255,122.046518326737)) ;
#85655 = CARTESIAN_POINT('Ctrl Pts',(-20.2723410125305,18.6033309249472,122.17589057555)) ;
#85656 = CARTESIAN_POINT('Ctrl Pts',(-20.4750350377161,18.6133911205225,122.345583287443)) ;
#85657 = CARTESIAN_POINT('Ctrl Pts',(-20.6422769769176,18.6232888038339,122.544802617581)) ;
#85658 = CARTESIAN_POINT('Ctrl Pts',(-20.7735588255307,18.6332198442079,122.770350862156)) ;
#85659 = CARTESIAN_POINT('Ctrl Pts',(-20.8644257386545,18.6432620618645,123.018108220622)) ;
#85660 = CARTESIAN_POINT('Ctrl Pts',(-20.9103608198524,18.6531487225985,123.2738391975)) ;
#85661 = CARTESIAN_POINT('Ctrl Pts',(-20.9116439914806,18.663141831201,123.536431039595)) ;
#85662 = CARTESIAN_POINT('Ctrl Pts',(-20.8674236850463,18.6730875298392,123.794025919388)) ;
#85663 = CARTESIAN_POINT('Ctrl Pts',(-20.7796339406571,18.6830347521103,124.040260003737)) ;
#85664 = CARTESIAN_POINT('Ctrl Pts',(-20.648865853499,18.6930827776904,124.269647102596)) ;
#85665 = CARTESIAN_POINT('Ctrl Pts',(-20.4837880164837,18.7029300248333,124.468930982032)) ;
#85666 = CARTESIAN_POINT('Ctrl Pts',(-20.2848353076597,18.712893201924,124.639124066068)) ;
#85667 = CARTESIAN_POINT('Ctrl Pts',(-20.057643225627,18.7229229229575,124.772734603442)) ;
#85668 = CARTESIAN_POINT('Ctrl Pts',(-19.8138733025437,18.7328273904903,124.864024891333)) ;
#85669 = CARTESIAN_POINT('Ctrl Pts',(-19.5549244555012,18.7428518763201,124.91225661059)) ;
#85670 = CARTESIAN_POINT('Ctrl Pts',(-19.2946394655604,18.752755711444,124.914979535986)) ;
#85671 = CARTESIAN_POINT('Ctrl Pts',(-19.0340712151648,18.762806902154,124.871903053952)) ;
#85672 = CARTESIAN_POINT('Ctrl Pts',(-18.7890046631621,18.7726913448123,124.785719653912)) ;
#85673 = CARTESIAN_POINT('Ctrl Pts',(-18.5599429927726,18.7826843526642,124.657344067074)) ;
#85674 = CARTESIAN_POINT('Ctrl Pts',(-18.3575852293697,18.7926326723805,124.491794444498)) ;
#85675 = CARTESIAN_POINT('Ctrl Pts',(-18.1869857767214,18.8025695110899,124.294126119609)) ;
#85676 = CARTESIAN_POINT('Ctrl Pts',(-18.0523654033191,18.8125525000095,124.068917991237)) ;
#85677 = CARTESIAN_POINT('Ctrl Pts',(-17.9588008233373,18.8225963793736,123.822148861517)) ;
#85678 = CARTESIAN_POINT('Ctrl Pts',(-17.9099472787027,18.832424444732,123.568497660891)) ;
#85679 = CARTESIAN_POINT('Ctrl Pts',(-17.9056636523394,18.8425015332869,123.303776150982)) ;
#85680 = CARTESIAN_POINT('Ctrl Pts',(-17.9463206545568,18.8523516854432,123.048068626949)) ;
#85681 = CARTESIAN_POINT('Ctrl Pts',(-18.0325884242925,18.8624321658956,122.797675319086)) ;
#85682 = CARTESIAN_POINT('Ctrl Pts',(-18.1574960786457,18.8722466636644,122.571957568326)) ;
#85683 = CARTESIAN_POINT('Ctrl Pts',(-18.3234918042426,18.8823149596845,122.366002659658)) ;
#85684 = CARTESIAN_POINT('Ctrl Pts',(-18.5195168321674,18.8922137921673,122.194898302409)) ;
#85685 = CARTESIAN_POINT('Ctrl Pts',(-18.7455899254507,18.9022666721818,122.058322027411)) ;
#85686 = CARTESIAN_POINT('Ctrl Pts',(-18.9874685791596,18.912136487678,121.96454261231)) ;
#85687 = CARTESIAN_POINT('Ctrl Pts',(-19.247074514884,18.9222091687608,121.913098195303)) ;
#85688 = CARTESIAN_POINT('Ctrl Pts',(-19.5054282253465,18.9320416473318,121.907540984529)) ;
#85689 = CARTESIAN_POINT('Ctrl Pts',(-19.7660476083419,18.9420722813179,121.946964015993)) ;
#85690 = CARTESIAN_POINT('Ctrl Pts',(-20.015663124333,18.952103838537,122.031786628564)) ;
#85691 = CARTESIAN_POINT('Ctrl Pts',(-20.242340733487,18.9619335474087,122.155620704585)) ;
#85692 = CARTESIAN_POINT('Ctrl Pts',(-20.4478596794803,18.9719229962108,122.318956902595)) ;
#85693 = CARTESIAN_POINT('Ctrl Pts',(-20.6223353947974,18.9819668486108,122.517002479713)) ;
#85694 = CARTESIAN_POINT('Ctrl Pts',(-20.7571909721581,18.9917885619429,122.737075061606)) ;
#85695 = CARTESIAN_POINT('Ctrl Pts',(-20.8544420213186,19.0018235669316,122.982196100149)) ;
#85696 = CARTESIAN_POINT('Ctrl Pts',(-20.9068867752531,19.0118484053792,123.24037432519)) ;
#85697 = CARTESIAN_POINT('Ctrl Pts',(-20.9141429657687,19.0217006183344,123.499179168148)) ;
#85698 = CARTESIAN_POINT('Ctrl Pts',(-20.8762673910892,19.0316905745282,123.758937854536)) ;
#85699 = CARTESIAN_POINT('Ctrl Pts',(-20.7943862514496,19.0416186848114,124.00666549439)) ;
#85700 = CARTESIAN_POINT('Ctrl Pts',(-20.6703510230735,19.051607284891,124.238008956621)) ;
#85701 = CARTESIAN_POINT('Ctrl Pts',(-20.5071291776537,19.0616338768185,124.444859269663)) ;
#85702 = CARTESIAN_POINT('Ctrl Pts',(-20.3134350002054,19.0715190048827,124.617949216475)) ;
#85703 = CARTESIAN_POINT('Ctrl Pts',(-20.0905630047009,19.0815101223562,124.756761630848)) ;
#85704 = CARTESIAN_POINT('Ctrl Pts',(-19.8455702342905,19.091550738208,124.854732580101)) ;
#85705 = CARTESIAN_POINT('Ctrl Pts',(-19.5927186533089,19.1013837290617,124.907978535889)) ;
#85706 = CARTESIAN_POINT('Ctrl Pts',(-19.3302830880624,19.111376860512,124.917403980521)) ;
#85707 = CARTESIAN_POINT('Ctrl Pts',(-19.0692443271857,19.1214089089474,124.880431822587)) ;
#85708 = CARTESIAN_POINT('Ctrl Pts',(-18.8226828953735,19.1312741554898,124.800366929372)) ;
#85709 = CARTESIAN_POINT('Ctrl Pts',(-18.5911601979227,19.1412360303166,124.678161518773)) ;
#85710 = CARTESIAN_POINT('Ctrl Pts',(-18.3831390570505,19.1512709934279,124.516107567008)) ;
#85711 = CARTESIAN_POINT('Ctrl Pts',(-18.2086970669107,19.1611558378903,124.323580061315)) ;
#85712 = CARTESIAN_POINT('Ctrl Pts',(-18.0679004045374,19.171221890731,124.099692955036)) ;
#85713 = CARTESIAN_POINT('Ctrl Pts',(-17.9700782692514,19.18105940664,123.860343413881)) ;
#85714 = CARTESIAN_POINT('Ctrl Pts',(-17.9137587529611,19.1911281547489,123.601857544703)) ;
#85715 = CARTESIAN_POINT('Ctrl Pts',(-17.9034670306657,19.2010086717799,123.342371871998)) ;
#85716 = CARTESIAN_POINT('Ctrl Pts',(-17.9382401306853,19.2109998587144,123.08216562488)) ;
#85717 = CARTESIAN_POINT('Ctrl Pts',(-18.017346517817,19.2209529249893,122.83281725219)) ;
#85718 = CARTESIAN_POINT('Ctrl Pts',(-18.1396020443988,19.2309887625219,122.599158531839)) ;
#85719 = CARTESIAN_POINT('Ctrl Pts',(-18.2981172600277,19.2408788887333,122.393170709056)) ;
#85720 = CARTESIAN_POINT('Ctrl Pts',(-18.4916634610177,19.2508710706413,122.215735660309)) ;
#85721 = CARTESIAN_POINT('Ctrl Pts',(-18.7121126054784,19.2608170105799,122.075322038536)) ;
#85722 = CARTESIAN_POINT('Ctrl Pts',(-18.9534330921312,19.270764194344,121.974810909958)) ;
#85723 = CARTESIAN_POINT('Ctrl Pts',(-19.2111660245585,19.2808121326514,121.917443070718)) ;
#85724 = CARTESIAN_POINT('Ctrl Pts',(-19.46968806927,19.2906597673917,121.905712436638)) ;
#85725 = CARTESIAN_POINT('Ctrl Pts',(-19.7293828802566,19.3006214813655,121.938618525281)) ;
#85726 = CARTESIAN_POINT('Ctrl Pts',(-19.9810273924312,19.3106501161564,122.01696448955)) ;
#85727 = CARTESIAN_POINT('Ctrl Pts',(-20.2124964374937,19.3205604347535,122.136300351223)) ;
#85728 = CARTESIAN_POINT('Ctrl Pts',(-20.4206742458988,19.330495291065,122.293871266416)) ;
#85729 = CARTESIAN_POINT('Ctrl Pts',(-20.6000312207341,19.3405365270257,122.487400631673)) ;
#85730 = CARTESIAN_POINT('Ctrl Pts',(-20.7410617512557,19.3504232986057,122.705636493677)) ;
#85731 = CARTESIAN_POINT('Ctrl Pts',(-20.8434829085783,19.3604234773119,122.947608430064)) ;
#85732 = CARTESIAN_POINT('Ctrl Pts',(-20.9020842657226,19.3703407555215,123.201594819178)) ;
#85733 = CARTESIAN_POINT('Ctrl Pts',(-20.9157885273105,19.3803880019352,123.465233400112)) ;
#85734 = CARTESIAN_POINT('Ctrl Pts',(-20.8843312394049,19.3902618909165,123.722835831488)) ;
#85735 = CARTESIAN_POINT('Ctrl Pts',(-20.8073413256974,19.400323908497,123.975764420132)) ;
#85736 = CARTESIAN_POINT('Ctrl Pts',(-20.6898211294301,19.4101949702313,124.207038033062)) ;
#85737 = CARTESIAN_POINT('Ctrl Pts',(-20.5325845494946,19.4201890335916,124.417401603479)) ;
#85738 = CARTESIAN_POINT('Ctrl Pts',(-20.3400856995338,19.430221191625,124.59752229965)) ;
#85739 = CARTESIAN_POINT('Ctrl Pts',(-20.1232221891283,19.4400850678652,124.739562342653)) ;
#85740 = CARTESIAN_POINT('Ctrl Pts',(-19.8800650899672,19.4501555825034,124.843936496975)) ;
#85741 = CARTESIAN_POINT('Ctrl Pts',(-19.6283151955898,19.4599962194444,124.903158307787)) ;
#85742 = CARTESIAN_POINT('Ctrl Pts',(-19.3668809125715,19.4699633482846,124.91881772904)) ;
#85743 = CARTESIAN_POINT('Ctrl Pts',(-19.1054682843621,19.4799773214091,124.888425374719)) ;
#85744 = CARTESIAN_POINT('Ctrl Pts',(-18.7709161948087,19.4932620552724,124.788603773578)) ;
#85745 = CARTESIAN_POINT('Ctrl Pts',(-18.4713172138264,19.5064873199872,124.604876555852)) ;
#85746 = CARTESIAN_POINT('Ctrl Pts',(-18.2302531727005,19.519797842542,124.351369013514)) ;
#85747 = CARTESIAN_POINT('Ctrl Pts',(-18.0847512811712,19.5298264874442,124.131644354945)) ;
#85748 = CARTESIAN_POINT('Ctrl Pts',(-17.9809400631191,19.5397075197981,123.89362910154)) ;
#85749 = CARTESIAN_POINT('Ctrl Pts',(-17.9188886192552,19.5496884924782,123.638788056693)) ;
#85750 = CARTESIAN_POINT('Ctrl Pts',(-17.902254691945,19.5596696200642,123.377037428699)) ;
#85751 = CARTESIAN_POINT('Ctrl Pts',(-17.9400916999754,19.5729128103256,123.031015386685)) ;
#85752 = CARTESIAN_POINT('Ctrl Pts',(-18.1006952198866,19.5895808056864,122.618253916938)) ;
#85753 = CARTESIAN_POINT('Ctrl Pts',(-18.3897868588537,19.6061013056984,122.287674714517)) ;
#85754 = CARTESIAN_POINT('Ctrl Pts',(-18.6800761568763,19.6194143220144,122.092482801336)) ;
#85755 = CARTESIAN_POINT('Ctrl Pts',(-18.9182029603172,19.6293308802474,121.986519910248)) ;
#85756 = CARTESIAN_POINT('Ctrl Pts',(-19.1738678812539,19.6393585485503,121.922922940547)) ;
#85757 = CARTESIAN_POINT('Ctrl Pts',(-19.5194780323658,19.652539138295,121.898097021449)) ;
#85758 = CARTESIAN_POINT('Ctrl Pts',(-19.9563288314783,19.6692872774143,121.982471851941)) ;
#85759 = CARTESIAN_POINT('Ctrl Pts',(-20.4082007931077,19.6890820199249,122.252403503244)) ;
#85760 = CARTESIAN_POINT('Ctrl Pts',(-20.7451774511471,19.7091264127337,122.664799510157)) ;
#85761 = CARTESIAN_POINT('Ctrl Pts',(-20.9190665009058,19.7289655950324,123.162745067453)) ;
#85762 = CARTESIAN_POINT('Ctrl Pts',(-20.9138754834601,19.7488909187253,123.692173591397)) ;
#85763 = CARTESIAN_POINT('Ctrl Pts',(-20.7282061366091,19.7688145567768,124.188186165143)) ;
#85764 = CARTESIAN_POINT('Ctrl Pts',(-20.384618994923,19.7887394302423,124.591086031158)) ;
#85765 = CARTESIAN_POINT('Ctrl Pts',(-19.9254980781481,19.8086180373213,124.852590538209)) ;
#85766 = CARTESIAN_POINT('Ctrl Pts',(-19.4021944235472,19.8285954801532,124.942415684017)) ;
#85767 = CARTESIAN_POINT('Ctrl Pts',(-18.8808504945977,19.8485273282379,124.848110950266)) ;
#85768 = CARTESIAN_POINT('Ctrl Pts',(-18.4236327836799,19.8684225965805,124.582537401173)) ;
#85769 = CARTESIAN_POINT('Ctrl Pts',(-18.0835396042065,19.8883450949926,124.176670177314)) ;
#85770 = CARTESIAN_POINT('Ctrl Pts',(-17.9021501379471,19.9083045768686,123.678122009356)) ;
#85771 = CARTESIAN_POINT('Ctrl Pts',(-17.9016826808945,19.928182329328,123.14988706624)) ;
#85772 = CARTESIAN_POINT('Ctrl Pts',(-18.0801848929392,19.9480641200625,122.652414260717)) ;
#85773 = CARTESIAN_POINT('Ctrl Pts',(-18.4216899540666,19.9681374589135,122.242615414334)) ;
#85774 = CARTESIAN_POINT('Ctrl Pts',(-18.8764503196767,19.9879419261493,121.977339845321)) ;
#85775 = CARTESIAN_POINT('Ctrl Pts',(-19.398725666126,20.0079252665571,121.881194515216)) ;
#85776 = CARTESIAN_POINT('Ctrl Pts',(-19.9205991086772,20.0278402311551,121.96959503457)) ;
#85777 = CARTESIAN_POINT('Ctrl Pts',(-20.3807214883969,20.0477087658715,122.228929102253)) ;
#85778 = CARTESIAN_POINT('Ctrl Pts',(-20.7270865861408,20.0677611500832,122.633789392997)) ;
#85779 = CARTESIAN_POINT('Ctrl Pts',(-20.9126916804623,20.0875351138724,123.125708607321)) ;
#85780 = CARTESIAN_POINT('Ctrl Pts',(-20.9197926939565,20.1075894928938,123.658461280195)) ;
#85781 = CARTESIAN_POINT('Ctrl Pts',(-20.7466018541178,20.127386230467,124.1554690317)) ;
#85782 = CARTESIAN_POINT('Ctrl Pts',(-20.4126503321151,20.1473540428185,124.567785296605)) ;
#85783 = CARTESIAN_POINT('Ctrl Pts',(-19.9576268829892,20.1673130188835,124.840673205932)) ;
#85784 = CARTESIAN_POINT('Ctrl Pts',(-19.4386508322908,20.1872079371609,124.94188751217)) ;
#85785 = CARTESIAN_POINT('Ctrl Pts',(-18.9161782831837,20.2071042496112,124.860571732585)) ;
#85786 = CARTESIAN_POINT('Ctrl Pts',(-18.4521872012561,20.2270121829853,124.606170401089)) ;
#85787 = CARTESIAN_POINT('Ctrl Pts',(-18.1022237455605,20.2469620732738,124.207890683089)) ;
#85788 = CARTESIAN_POINT('Ctrl Pts',(-17.9093454009066,20.2668393037751,123.715999312751)) ;
#85789 = CARTESIAN_POINT('Ctrl Pts',(-17.8955608540406,20.2868219726461,123.185097942073)) ;
#85790 = CARTESIAN_POINT('Ctrl Pts',(-18.0637245954641,20.3067548592265,122.682641570739)) ;
#85791 = CARTESIAN_POINT('Ctrl Pts',(-18.3925761888793,20.3266676052444,122.268015072213)) ;
#85792 = CARTESIAN_POINT('Ctrl Pts',(-18.7672875195584,20.3432373265862,122.036639218976)) ;
#85793 = CARTESIAN_POINT('Ctrl Pts',(-19.1020112523894,20.3565373378912,121.93602784581)) ;
#85794 = CARTESIAN_POINT('Ctrl Pts',(-19.4482933884682,20.3698075256411,121.894667854607)) ;
#85795 = CARTESIAN_POINT('Ctrl Pts',(-19.8857616860693,20.3864349080065,121.957330261882)) ;
#85796 = CARTESIAN_POINT('Ctrl Pts',(-20.2753843629908,20.4030571977517,122.165611719854)) ;
#85797 = CARTESIAN_POINT('Ctrl Pts',(-20.5295904307739,20.4163024121462,122.403368996714)) ;
#85798 = CARTESIAN_POINT('Ctrl Pts',(-20.6866680641732,20.4262143771069,122.61117509767)) ;
#85799 = CARTESIAN_POINT('Ctrl Pts',(-20.806737474672,20.4362730002714,122.846628519742)) ;
#85800 = CARTESIAN_POINT('Ctrl Pts',(-20.8828053848385,20.4461131143872,123.093815056759)) ;
#85801 = CARTESIAN_POINT('Ctrl Pts',(-20.9157850235484,20.4561788993448,123.356230024175)) ;
#85802 = CARTESIAN_POINT('Ctrl Pts',(-20.9028213821857,20.4660622171327,123.615663268066)) ;
#85803 = CARTESIAN_POINT('Ctrl Pts',(-20.8449589694743,20.4760516549913,123.871692434311)) ;
#85804 = CARTESIAN_POINT('Ctrl Pts',(-20.74368006627,20.486015369044,124.113161475895)) ;
#85805 = CARTESIAN_POINT('Ctrl Pts',(-20.6017961937113,20.4960103807032,124.334224144279)) ;
#85806 = CARTESIAN_POINT('Ctrl Pts',(-20.4226668968658,20.5060466723975,124.527786878245)) ;
#85807 = CARTESIAN_POINT('Ctrl Pts',(-20.2168574908497,20.5158930500909,124.684641027028)) ;
#85808 = CARTESIAN_POINT('Ctrl Pts',(-19.9839816914647,20.5258779942416,124.805469402538)) ;
#85809 = CARTESIAN_POINT('Ctrl Pts',(-19.7348364121739,20.5358149653716,124.883819573151)) ;
#85810 = CARTESIAN_POINT('Ctrl Pts',(-19.4729804417369,20.5458647500033,124.917956892684)) ;
#85811 = CARTESIAN_POINT('Ctrl Pts',(-19.2143536333705,20.5557152120808,124.906538794214)) ;
#85812 = CARTESIAN_POINT('Ctrl Pts',(-18.9584230841274,20.5656872256012,124.850373618486)) ;
#85813 = CARTESIAN_POINT('Ctrl Pts',(-18.7155134690777,20.5756823727206,124.75033150436)) ;
#85814 = CARTESIAN_POINT('Ctrl Pts',(-18.4930284866175,20.5857163424567,124.608850714625)) ;
#85815 = CARTESIAN_POINT('Ctrl Pts',(-18.301639069362,20.5955718881273,124.43432218421)) ;
#85816 = CARTESIAN_POINT('Ctrl Pts',(-18.1409105781554,20.6055706451405,124.22651165924)) ;
#85817 = CARTESIAN_POINT('Ctrl Pts',(-18.0196900933075,20.6154677803777,123.996357848347)) ;
#85818 = CARTESIAN_POINT('Ctrl Pts',(-17.9389969296105,20.6255208762173,123.744826815494)) ;
#85819 = CARTESIAN_POINT('Ctrl Pts',(-17.9037758541384,20.6354043849479,123.487479681158)) ;
#85820 = CARTESIAN_POINT('Ctrl Pts',(-17.9132711224096,20.645399257594,123.225004546721)) ;
#85821 = CARTESIAN_POINT('Ctrl Pts',(-17.9687399657228,20.6554192192297,122.96758422729)) ;
#85822 = CARTESIAN_POINT('Ctrl Pts',(-18.0667172219578,20.6653245830296,122.726428828135)) ;
#85823 = CARTESIAN_POINT('Ctrl Pts',(-18.2051112656729,20.6752651706371,122.504892851635)) ;
#85824 = CARTESIAN_POINT('Ctrl Pts',(-18.3808832318701,20.6852679887378,122.309400454705)) ;
#85825 = CARTESIAN_POINT('Ctrl Pts',(-18.5888185798447,20.6953027004619,122.147247116949)) ;
#85826 = CARTESIAN_POINT('Ctrl Pts',(-18.8171665168026,20.7051476071992,122.025597143536)) ;
#85827 = CARTESIAN_POINT('Ctrl Pts',(-19.0664811329135,20.7151334597682,121.943845159401)) ;
#85828 = CARTESIAN_POINT('Ctrl Pts',(-19.3249386776779,20.7250682681813,121.906617308344)) ;
#85829 = CARTESIAN_POINT('Ctrl Pts',(-19.5890636684313,20.7351257952623,121.915166166779)) ;
#85830 = CARTESIAN_POINT('Ctrl Pts',(-19.8417720817048,20.7449474502594,121.967799082809)) ;
#85831 = CARTESIAN_POINT('Ctrl Pts',(-20.0873597067846,20.7550034944324,122.065317687553)) ;
#85832 = CARTESIAN_POINT('Ctrl Pts',(-20.3094854721539,20.7649442344776,122.202825084637)) ;
#85833 = CARTESIAN_POINT('Ctrl Pts',(-20.5041808420828,20.7748483555505,122.375555985901)) ;
#85834 = CARTESIAN_POINT('Ctrl Pts',(-20.6681287825517,20.7848958967047,122.582504505087)) ;
#85835 = CARTESIAN_POINT('Ctrl Pts',(-20.7919881814226,20.7947946483051,122.811292280779)) ;
#85836 = CARTESIAN_POINT('Ctrl Pts',(-20.8755740195429,20.8048431272709,123.061746962003)) ;
#85837 = CARTESIAN_POINT('Ctrl Pts',(-20.9138090117843,20.8147306243546,123.318779270284)) ;
#85838 = CARTESIAN_POINT('Ctrl Pts',(-20.9072479453517,20.8247237146527,123.581282226704)) ;
#85839 = CARTESIAN_POINT('Ctrl Pts',(-20.8553241322653,20.834675884713,123.837624769112)) ;
#85840 = CARTESIAN_POINT('Ctrl Pts',(-20.7601574063262,20.8446143046275,124.080820832448)) ;
#85841 = CARTESIAN_POINT('Ctrl Pts',(-20.6237998714096,20.8545994347131,124.305038244249)) ;
#85842 = CARTESIAN_POINT('Ctrl Pts',(-20.4494221518513,20.8646361241272,124.502900480269)) ;
#85843 = CARTESIAN_POINT('Ctrl Pts',(-20.2473013388322,20.8744908081197,124.664842526609)) ;
#85844 = CARTESIAN_POINT('Ctrl Pts',(-20.0170290666669,20.8844902921675,124.7913425284)) ;
#85845 = CARTESIAN_POINT('Ctrl Pts',(-19.7708926225284,20.8943853809444,124.875346148885)) ;
#85846 = CARTESIAN_POINT('Ctrl Pts',(-19.5096857275806,20.9044459355906,124.915966548158)) ;
#85847 = CARTESIAN_POINT('Ctrl Pts',(-19.2508869429393,20.9142951999635,124.910873014686)) ;
#85848 = CARTESIAN_POINT('Ctrl Pts',(-18.9922127135504,20.9243224524113,124.860678227348)) ;
#85849 = CARTESIAN_POINT('Ctrl Pts',(-18.7463889477668,20.9343507499815,124.765668763576)) ;
#85850 = CARTESIAN_POINT('Ctrl Pts',(-18.5246560820803,20.9441968789875,124.632331993503)) ;
#85851 = CARTESIAN_POINT('Ctrl Pts',(-18.3260748632208,20.9541907843496,124.460462272426)) ;
#85852 = CARTESIAN_POINT('Ctrl Pts',(-18.1602131738219,20.9642148820326,124.255803821438)) ;
#85853 = CARTESIAN_POINT('Ctrl Pts',(-18.0338336778558,20.9741047098866,124.028700863845)) ;
#85854 = CARTESIAN_POINT('Ctrl Pts',(-17.9475715523185,20.9840966913171,123.780706945075)) ;
#85855 = CARTESIAN_POINT('Ctrl Pts',(-17.9059277190108,20.9940436960829,123.522648076826)) ;
#85856 = CARTESIAN_POINT('Ctrl Pts',(-17.9092446774268,21.0039933474727,123.26119173999)) ;
#85857 = CARTESIAN_POINT('Ctrl Pts',(-17.9585439446535,21.0140303504501,123.002085877506)) ;
#85858 = CARTESIAN_POINT('Ctrl Pts',(-18.0505382977171,21.0239192588851,122.759033267901)) ;
#85859 = CARTESIAN_POINT('Ctrl Pts',(-18.1842691504711,21.0339085913626,122.533148901569)) ;
#85860 = CARTESIAN_POINT('Ctrl Pts',(-18.3548109388882,21.0438671467997,122.334658060956)) ;
#85861 = CARTESIAN_POINT('Ctrl Pts',(-18.5556391649582,21.0537667180002,122.16926520889)) ;
#85862 = CARTESIAN_POINT('Ctrl Pts',(-18.7855363124599,21.0638146432522,122.039439979611)) ;
#85863 = CARTESIAN_POINT('Ctrl Pts',(-19.030698238794,21.0737099427782,121.952623471748)) ;
#85864 = CARTESIAN_POINT('Ctrl Pts',(-19.291450065471,21.0837717992262,121.908950298832)) ;
#85865 = CARTESIAN_POINT('Ctrl Pts',(-19.5501399989178,21.0936156456428,121.91111408291)) ;
#85866 = CARTESIAN_POINT('Ctrl Pts',(-19.807740031436,21.1035785947709,121.957838664783)) ;
#85867 = CARTESIAN_POINT('Ctrl Pts',(-20.0549347555783,21.1136126311989,122.049642784503)) ;
#85868 = CARTESIAN_POINT('Ctrl Pts',(-20.2792391844421,21.1235000581569,122.180784673848)) ;
#85869 = CARTESIAN_POINT('Ctrl Pts',(-20.4802501125778,21.1335144924933,122.350672310585)) ;
#85870 = CARTESIAN_POINT('Ctrl Pts',(-20.6485231786559,21.1435494371282,122.553690979311)) ;
#85871 = CARTESIAN_POINT('Ctrl Pts',(-20.776994667693,21.1533817871592,122.777909498819)) ;
#85872 = CARTESIAN_POINT('Ctrl Pts',(-20.8667919124949,21.1634572262764,123.026935129347)) ;
#85873 = CARTESIAN_POINT('Ctrl Pts',(-20.911151449371,21.173309691511,123.282075921991)) ;
#85874 = CARTESIAN_POINT('Ctrl Pts',(-20.9107346702923,21.1833825690879,123.546735142883)) ;
#85875 = CARTESIAN_POINT('Ctrl Pts',(-20.8653838187256,21.1932251652804,123.801404395061)) ;
#85876 = CARTESIAN_POINT('Ctrl Pts',(-20.776098005712,21.2032055493957,124.048000989328)) ;
#85877 = CARTESIAN_POINT('Ctrl Pts',(-20.6444053880161,21.2132240300445,124.275965170634)) ;
#85878 = CARTESIAN_POINT('Ctrl Pts',(-20.4778156031857,21.2231073450449,124.47526543333)) ;
#85879 = CARTESIAN_POINT('Ctrl Pts',(-20.2754160656576,21.2331756421353,124.645605897759)) ;
#85880 = CARTESIAN_POINT('Ctrl Pts',(-20.0520068570127,21.2430057105076,124.775388910782)) ;
#85881 = CARTESIAN_POINT('Ctrl Pts',(-19.8038192003743,21.253072502976,124.866829885988)) ;
#85882 = CARTESIAN_POINT('Ctrl Pts',(-19.5479997475856,21.2629618364645,124.912863623908)) ;
#85883 = CARTESIAN_POINT('Ctrl Pts',(-19.2852043849924,21.2729639678806,124.914202847899)) ;
#85884 = CARTESIAN_POINT('Ctrl Pts',(-19.0280750006297,21.2828878375016,124.870388521691)) ;
#85885 = CARTESIAN_POINT('Ctrl Pts',(-18.77960570535,21.2929313530188,124.781491000549)) ;
#85886 = CARTESIAN_POINT('Ctrl Pts',(-18.5538025555048,21.3028135659071,124.653119146439)) ;
#85887 = CARTESIAN_POINT('Ctrl Pts',(-18.3500349006823,21.3128816431265,124.484434278303)) ;
#85888 = CARTESIAN_POINT('Ctrl Pts',(-18.1823229673718,21.3227201478607,124.28760693878)) ;
#85889 = CARTESIAN_POINT('Ctrl Pts',(-18.0480641582105,21.3327829162901,124.059823359472)) ;
#85890 = CARTESIAN_POINT('Ctrl Pts',(-17.9571706997418,21.3426799095728,123.816123607726)) ;
#85891 = CARTESIAN_POINT('Ctrl Pts',(-17.9089560570351,21.3526111372076,123.559639960323)) ;
#85892 = CARTESIAN_POINT('Ctrl Pts',(-17.9062641201702,21.3626532958498,123.295759494904)) ;
#85893 = CARTESIAN_POINT('Ctrl Pts',(-17.9485807750656,21.3725400053808,123.039404443611)) ;
#85894 = CARTESIAN_POINT('Ctrl Pts',(-18.0352662045675,21.3825329778094,122.791531975748)) ;
#85895 = CARTESIAN_POINT('Ctrl Pts',(-18.1631733074527,21.392479172346,122.56359572005)) ;
#85896 = CARTESIAN_POINT('Ctrl Pts',(-18.3282744150043,21.4024245471975,122.360963544721)) ;
#85897 = CARTESIAN_POINT('Ctrl Pts',(-18.5284565572223,21.4124794665574,122.188538399723)) ;
#85898 = CARTESIAN_POINT('Ctrl Pts',(-18.7500672200615,21.4223009860009,122.056167239099)) ;
#85899 = CARTESIAN_POINT('Ctrl Pts',(-18.9971032250605,21.4323667547678,121.961729368594)) ;
#85900 = CARTESIAN_POINT('Ctrl Pts',(-19.252665844166,21.4422686764229,121.912504687733)) ;
#85901 = CARTESIAN_POINT('Ctrl Pts',(-19.516526510854,21.4523117352439,121.908111222315)) ;
#85902 = CARTESIAN_POINT('Ctrl Pts',(-19.7735943063744,21.4622177292866,121.949174521215)) ;
#85903 = CARTESIAN_POINT('Ctrl Pts',(-20.0206585177756,21.4721555023684,122.033793699405)) ;
#85904 = CARTESIAN_POINT('Ctrl Pts',(-20.2514967965682,21.4821958661007,122.161575037695)) ;
#85905 = CARTESIAN_POINT('Ctrl Pts',(-20.4536528904977,21.4920832098242,122.324826619752)) ;
#85906 = CARTESIAN_POINT('Ctrl Pts',(-20.6265093028174,21.5020754403929,122.522468692439)) ;
#85907 = CARTESIAN_POINT('Ctrl Pts',(-20.7617843910413,21.5120239681765,122.746204499775)) ;
#85908 = CARTESIAN_POINT('Ctrl Pts',(-20.8563752029685,21.5219607518998,122.989574942634)) ;
#85909 = CARTESIAN_POINT('Ctrl Pts',(-20.9078459005937,21.5319437526968,123.246853300404)) ;
#85910 = CARTESIAN_POINT('Ctrl Pts',(-20.9134112422956,21.5419876395375,123.510706398789)) ;
#85911 = CARTESIAN_POINT('Ctrl Pts',(-20.8745423295287,21.5518156631121,123.766077419227)) ;
#85912 = CARTESIAN_POINT('Ctrl Pts',(-20.7899649656379,21.5618929113257,124.016964720075)) ;
#85913 = CARTESIAN_POINT('Ctrl Pts',(-20.6660716447633,21.571742466631,124.244301696396)) ;
#85914 = CARTESIAN_POINT('Ctrl Pts',(-20.5009218271621,21.5818251748287,124.451413147156)) ;
#85915 = CARTESIAN_POINT('Ctrl Pts',(-20.3077024679785,21.5916377677552,124.622265315751)) ;
#85916 = CARTESIAN_POINT('Ctrl Pts',(-20.082372609264,21.6017049600131,124.76077174282)) ;
#85917 = CARTESIAN_POINT('Ctrl Pts',(-19.8403774418101,21.6116037894757,124.856379349723)) ;
#85918 = CARTESIAN_POINT('Ctrl Pts',(-19.5816048957035,21.6216577806659,124.909420890267)) ;
#85919 = CARTESIAN_POINT('Ctrl Pts',(-19.3222374612088,21.6315295054491,124.916826891635)) ;
#85920 = CARTESIAN_POINT('Ctrl Pts',(-19.0604462619463,21.6415999475793,124.878403745685)) ;
#85921 = CARTESIAN_POINT('Ctrl Pts',(-18.8151200955136,21.6514330260096,124.797161576374)) ;
#85922 = CARTESIAN_POINT('Ctrl Pts',(-18.5827353405762,21.661463499511,124.672775000186)) ;
#85923 = CARTESIAN_POINT('Ctrl Pts',(-18.3759109672851,21.6714950988097,124.509291299171)) ;
#85924 = CARTESIAN_POINT('Ctrl Pts',(-18.2037611889679,21.6813247998478,124.316724488468)) ;
#85925 = CARTESIAN_POINT('Ctrl Pts',(-18.0647714451557,21.6913142379043,124.094017139833)) ;
#85926 = CARTESIAN_POINT('Ctrl Pts',(-17.9666536761754,21.7013581411204,123.848992514289)) ;
#85927 = CARTESIAN_POINT('Ctrl Pts',(-17.9132395630017,21.7111796619339,123.596478590155)) ;
#85928 = CARTESIAN_POINT('Ctrl Pts',(-17.9036603191974,21.721215386181,123.332930237762)) ;
#85929 = CARTESIAN_POINT('Ctrl Pts',(-17.9406169716176,21.7312375401135,123.072144554952)) ;
#85930 = CARTESIAN_POINT('Ctrl Pts',(-18.0205753951748,21.7410997718708,122.825638668101)) ;
#85931 = CARTESIAN_POINT('Ctrl Pts',(-18.1426765255731,21.7510588423287,122.5941443993)) ;
#85932 = CARTESIAN_POINT('Ctrl Pts',(-18.3046553200881,21.7610940147049,122.386052860544)) ;
#85933 = CARTESIAN_POINT('Ctrl Pts',(-18.4970548092859,21.7709743998631,122.211659235178)) ;
#85934 = CARTESIAN_POINT('Ctrl Pts',(-18.7206332905695,21.7810311144571,122.070794791818)) ;
#85935 = CARTESIAN_POINT('Ctrl Pts',(-18.9610017685015,21.7909103830291,121.972655816629)) ;
#85936 = CARTESIAN_POINT('Ctrl Pts',(-19.2174642405481,21.8009013405148,121.916435631599)) ;
#85937 = CARTESIAN_POINT('Ctrl Pts',(-19.4811229674523,21.81094199915,121.906127926293)) ;
#85938 = CARTESIAN_POINT('Ctrl Pts',(-19.7372102471354,21.820774978858,121.940589760359)) ;
#85939 = CARTESIAN_POINT('Ctrl Pts',(-19.987662151828,21.8307681121077,122.019553890229)) ;
#85940 = CARTESIAN_POINT('Ctrl Pts',(-20.221266587985,21.8408001644911,122.141771264833)) ;
#85941 = CARTESIAN_POINT('Ctrl Pts',(-20.4268046448549,21.8506653934424,122.299749040127)) ;
#85942 = CARTESIAN_POINT('Ctrl Pts',(-20.6040649592092,21.8606273346856,122.492404487236)) ;
#85943 = CARTESIAN_POINT('Ctrl Pts',(-20.7458436231991,21.8706620497224,122.714735308757)) ;
#85944 = CARTESIAN_POINT('Ctrl Pts',(-20.8457694698757,21.8805478200664,122.954570602703)) ;
#85945 = CARTESIAN_POINT('Ctrl Pts',(-20.903532112246,21.8906104174552,123.212586648096)) ;
#85946 = CARTESIAN_POINT('Ctrl Pts',(-20.9154805876386,21.9004608292904,123.471189998348)) ;
#85947 = CARTESIAN_POINT('Ctrl Pts',(-20.882426858183,21.9104879985763,123.73260477288)) ;
#85948 = CARTESIAN_POINT('Ctrl Pts',(-20.8038186859197,21.9205154792905,123.984131914222)) ;
#85949 = CARTESIAN_POINT('Ctrl Pts',(-20.6854109255077,21.9303585318698,124.214093694813)) ;
#85950 = CARTESIAN_POINT('Ctrl Pts',(-20.5270023291853,21.9403524353084,124.423570385325)) ;
#85951 = CARTESIAN_POINT('Ctrl Pts',(-20.3336537691034,21.9503795580848,124.602604087814)) ;
#85952 = CARTESIAN_POINT('Ctrl Pts',(-20.1153478377517,21.9602702629769,124.743677527019)) ;
#85953 = CARTESIAN_POINT('Ctrl Pts',(-19.8735692667385,21.9702622898272,124.846083256019)) ;
#85954 = CARTESIAN_POINT('Ctrl Pts',(-19.6188372985755,21.9802082713157,124.904607587831)) ;
#85955 = CARTESIAN_POINT('Ctrl Pts',(-19.3577931878943,21.9901554439376,124.918542373026)) ;
#85956 = CARTESIAN_POINT('Ctrl Pts',(-19.0957252140819,22.0002033852638,124.886329581241)) ;
#85957 = CARTESIAN_POINT('Ctrl Pts',(-18.8481898209292,22.0100510190716,124.810847917876)) ;
#85958 = CARTESIAN_POINT('Ctrl Pts',(-18.6144904935636,22.0200127337566,124.692911935522)) ;
#85959 = CARTESIAN_POINT('Ctrl Pts',(-18.4035879139127,22.0300413666351,124.534852114603)) ;
#85960 = CARTESIAN_POINT('Ctrl Pts',(-18.2254150484394,22.0399516921703,124.344920009527)) ;
#85961 = CARTESIAN_POINT('Ctrl Pts',(-18.0819977432726,22.049886522642,124.126756044865)) ;
#85962 = CARTESIAN_POINT('Ctrl Pts',(-17.9777399583878,22.059927855024,123.884350623129)) ;
#85963 = CARTESIAN_POINT('Ctrl Pts',(-17.9179599830939,22.0698207284628,123.631344850412)) ;
#85964 = CARTESIAN_POINT('Ctrl Pts',(-17.9022371535386,22.0797898942807,123.369827155738)) ;
#85965 = CARTESIAN_POINT('Ctrl Pts',(-17.9327716986324,22.0898186279972,123.108078060828)) ;
#85966 = CARTESIAN_POINT('Ctrl Pts',(-18.0314269334723,22.1030111467684,122.775654275456)) ;
#85967 = CARTESIAN_POINT('Ctrl Pts',(-18.2167874151558,22.1163710148111,122.472935258562)) ;
#85968 = CARTESIAN_POINT('Ctrl Pts',(-18.4689775945887,22.1295963519599,122.233681798304)) ;
#85969 = CARTESIAN_POINT('Ctrl Pts',(-18.6872947818254,22.1395775778005,122.088312201797)) ;
#85970 = CARTESIAN_POINT('Ctrl Pts',(-18.9290513962181,22.1496131447834,121.982956255966)) ;
#85971 = CARTESIAN_POINT('Ctrl Pts',(-19.1809335406282,22.1594762227455,121.921719585)) ;
#85972 = CARTESIAN_POINT('Ctrl Pts',(-19.4449971797,22.1695465215466,121.904746363636)) ;
#85973 = CARTESIAN_POINT('Ctrl Pts',(-19.7020801434068,22.1793888201144,121.933241045844)) ;
#85974 = CARTESIAN_POINT('Ctrl Pts',(-19.9535498675344,22.1893495182842,122.005881902579)) ;
#85975 = CARTESIAN_POINT('Ctrl Pts',(-20.1901770423832,22.1993875524637,122.122446448014)) ;
#85976 = CARTESIAN_POINT('Ctrl Pts',(-20.3998103087612,22.2092612893102,122.275407092462)) ;
#85977 = CARTESIAN_POINT('Ctrl Pts',(-20.5832357329711,22.2193330732354,122.466165386452)) ;
#85978 = CARTESIAN_POINT('Ctrl Pts',(-20.7274078859713,22.2291651944366,122.680609736101)) ;
#85979 = CARTESIAN_POINT('Ctrl Pts',(-20.8349279101504,22.239198218462,122.921333612289)) ;
#85980 = CARTESIAN_POINT('Ctrl Pts',(-20.8982607406429,22.2492140986587,123.176824810715)) ;
#85981 = CARTESIAN_POINT('Ctrl Pts',(-20.9165125593692,22.2590976177529,123.43591069118)) ;
#85982 = CARTESIAN_POINT('Ctrl Pts',(-20.8895476418826,22.2690880301166,123.697042256073)) ;
#85983 = CARTESIAN_POINT('Ctrl Pts',(-20.794199097017,22.28235119332,124.032313731486)) ;
#85984 = CARTESIAN_POINT('Ctrl Pts',(-20.6136506128505,22.2956287635712,124.335485744995)) ;
#85985 = CARTESIAN_POINT('Ctrl Pts',(-20.3624307998912,22.3089590660778,124.579675665852)) ;
#85986 = CARTESIAN_POINT('Ctrl Pts',(-20.1474734503822,22.3188577478942,124.726159691664)) ;
#85987 = CARTESIAN_POINT('Ctrl Pts',(-19.9083044716856,22.3288472629417,124.8343602261)) ;
#85988 = CARTESIAN_POINT('Ctrl Pts',(-19.6550143972876,22.3387953147168,124.89911320866)) ;
#85989 = CARTESIAN_POINT('Ctrl Pts',(-19.3945571768419,22.3487367179953,124.919216158149)) ;
#85990 = CARTESIAN_POINT('Ctrl Pts',(-19.0469801715719,22.3620233827762,124.885646801854)) ;
#85991 = CARTESIAN_POINT('Ctrl Pts',(-18.6334919756593,22.378633804431,124.731055814575)) ;
#85992 = CARTESIAN_POINT('Ctrl Pts',(-18.2305162797271,22.3985450666818,124.387992218144)) ;
#85993 = CARTESIAN_POINT('Ctrl Pts',(-17.9681847100688,22.4184891958467,123.927340765981)) ;
#85994 = CARTESIAN_POINT('Ctrl Pts',(-17.8789700282879,22.4384123584518,123.405435456902)) ;
#85995 = CARTESIAN_POINT('Ctrl Pts',(-17.9722068017202,22.4583024808584,122.88499296031)) ;
#85996 = CARTESIAN_POINT('Ctrl Pts',(-18.2392469664603,22.4783074344585,122.425313505132)) ;
#85997 = CARTESIAN_POINT('Ctrl Pts',(-18.6435932599694,22.4981456914741,122.086755742294)) ;
#85998 = CARTESIAN_POINT('Ctrl Pts',(-19.1427570950757,22.5181399922607,121.904630400796)) ;
#85999 = CARTESIAN_POINT('Ctrl Pts',(-19.6712866823868,22.5380252343051,121.904256042346)) ;
#86000 = CARTESIAN_POINT('Ctrl Pts',(-20.1684531083155,22.557900180781,122.082765057008)) ;
#86001 = CARTESIAN_POINT('Ctrl Pts',(-20.5778666143493,22.5779332507221,122.423256582873)) ;
#86002 = CARTESIAN_POINT('Ctrl Pts',(-20.8439539041053,22.5978217576225,122.879952432642)) ;
#86003 = CARTESIAN_POINT('Ctrl Pts',(-20.9398901568453,22.6176766174038,123.398949134001)) ;
#86004 = CARTESIAN_POINT('Ctrl Pts',(-20.8512776370932,22.6377274511915,123.92432167666)) ;
#86005 = CARTESIAN_POINT('Ctrl Pts',(-20.5928105483306,22.6574933930808,124.381851942389)) ;
#86006 = CARTESIAN_POINT('Ctrl Pts',(-20.1896636816174,22.6775061245401,124.728595251841)) ;
#86007 = CARTESIAN_POINT('Ctrl Pts',(-19.6948416932879,22.6973989594837,124.915260290639)) ;
#86008 = CARTESIAN_POINT('Ctrl Pts',(-19.1659292643134,22.7173059828232,124.922744509421)) ;
#86009 = CARTESIAN_POINT('Ctrl Pts',(-18.6655675605648,22.7372212477239,124.749699013636)) ;
#86010 = CARTESIAN_POINT('Ctrl Pts',(-18.2524453398778,22.7572529398836,124.413924653691)) ;
#86011 = CARTESIAN_POINT('Ctrl Pts',(-17.9812029359813,22.7770959864566,123.961563010291)) ;
#86012 = CARTESIAN_POINT('Ctrl Pts',(-17.8790677895418,22.7970125343564,123.442240253503)) ;
#86013 = CARTESIAN_POINT('Ctrl Pts',(-17.9604555657489,22.8169447773477,122.918716094646)) ;
#86014 = CARTESIAN_POINT('Ctrl Pts',(-18.2149597212616,22.836848612157,122.454982006216)) ;
#86015 = CARTESIAN_POINT('Ctrl Pts',(-18.6119455544731,22.8567490123445,122.105477724641)) ;
#86016 = CARTESIAN_POINT('Ctrl Pts',(-19.1055301645696,22.8766986887238,121.911730698857)) ;
#86017 = CARTESIAN_POINT('Ctrl Pts',(-19.6351375624815,22.8966312129442,121.898173547559)) ;
#86018 = CARTESIAN_POINT('Ctrl Pts',(-20.1374387737837,22.9165512219304,122.065632357375)) ;
#86019 = CARTESIAN_POINT('Ctrl Pts',(-20.5530897144561,22.9365081281066,122.395063821693)) ;
#86020 = CARTESIAN_POINT('Ctrl Pts',(-20.8308724977881,22.9563939676081,122.844830062582)) ;
#86021 = CARTESIAN_POINT('Ctrl Pts',(-20.9388539512202,22.9763651397439,123.364411422884)) ;
#86022 = CARTESIAN_POINT('Ctrl Pts',(-20.8643389626638,22.9961793367283,123.885825621413)) ;
#86023 = CARTESIAN_POINT('Ctrl Pts',(-20.6149971103256,23.0161605226965,124.354606393768)) ;
#86024 = CARTESIAN_POINT('Ctrl Pts',(-20.2875827610197,23.0327360280858,124.64946647421)) ;
#86025 = CARTESIAN_POINT('Ctrl Pts',(-19.9761963329815,23.0460454759494,124.808750590775)) ;
#86026 = CARTESIAN_POINT('Ctrl Pts',(-19.6403478940357,23.059413173726,124.911784399414)) ;
#86027 = CARTESIAN_POINT('Ctrl Pts',(-19.2023596389031,23.0759037453919,124.927929061235)) ;
#86028 = CARTESIAN_POINT('Ctrl Pts',(-18.6980186540393,23.0958240177247,124.767071885537)) ;
#86029 = CARTESIAN_POINT('Ctrl Pts',(-18.3484072158521,23.1124410534457,124.497150544743)) ;
#86030 = CARTESIAN_POINT('Ctrl Pts',(-18.1364154882604,23.1257319037268,124.219541419118)) ;
#86031 = CARTESIAN_POINT('Ctrl Pts',(-18.0158927766921,23.1357009488813,123.986966551078)) ;
#86032 = CARTESIAN_POINT('Ctrl Pts',(-17.937590459842,23.1456043395148,123.738742873997)) ;
#86033 = CARTESIAN_POINT('Ctrl Pts',(-17.9031973751966,23.1556621256276,123.476711455943)) ;
#86034 = CARTESIAN_POINT('Ctrl Pts',(-17.9143593563858,23.1655141622773,123.218025990263)) ;
#86035 = CARTESIAN_POINT('Ctrl Pts',(-17.9896268659552,23.1788792864205,122.874973437508)) ;
#86036 = CARTESIAN_POINT('Ctrl Pts',(-18.151401302181,23.1921053493835,122.562854577334)) ;
#86037 = CARTESIAN_POINT('Ctrl Pts',(-18.3866165742264,23.2054089976658,122.304238650459)) ;
#86038 = CARTESIAN_POINT('Ctrl Pts',(-18.5942744744476,23.2154005288288,122.143499851417)) ;
#86039 = CARTESIAN_POINT('Ctrl Pts',(-18.8279217544426,23.2254399766281,122.02101181735)) ;
#86040 = CARTESIAN_POINT('Ctrl Pts',(-19.0743059149406,23.235283752142,121.942132253362)) ;
#86041 = CARTESIAN_POINT('Ctrl Pts',(-19.3342082548891,23.2452693935296,121.906215557607)) ;
#86042 = CARTESIAN_POINT('Ctrl Pts',(-19.595203409344,23.2552061778914,121.915784532965)) ;
#86043 = CARTESIAN_POINT('Ctrl Pts',(-19.8533817478491,23.2652560123588,121.971267328799)) ;
#86044 = CARTESIAN_POINT('Ctrl Pts',(-20.0932669657549,23.2751064618619,122.068597590794)) ;
#86045 = CARTESIAN_POINT('Ctrl Pts',(-20.3156335651349,23.285078475844,122.207190765456)) ;
#86046 = CARTESIAN_POINT('Ctrl Pts',(-20.5110432440586,23.2950736336911,122.382771699199)) ;
#86047 = CARTESIAN_POINT('Ctrl Pts',(-20.6733357401702,23.3051075600548,122.590562603099)) ;
#86048 = CARTESIAN_POINT('Ctrl Pts',(-20.7952641776477,23.3149632684872,122.81909160789)) ;
#86049 = CARTESIAN_POINT('Ctrl Pts',(-20.8771604366914,23.3249614178259,123.068699179642)) ;
#86050 = CARTESIAN_POINT('Ctrl Pts',(-20.9143466504709,23.3348608209994,123.326212352676)) ;
#86051 = CARTESIAN_POINT('Ctrl Pts',(-20.9061903378289,23.3449120178879,123.590193277281)) ;
#86052 = CARTESIAN_POINT('Ctrl Pts',(-20.8532554613795,23.3547943417008,123.844458307403)) ;
#86053 = CARTESIAN_POINT('Ctrl Pts',(-20.7564386685029,23.3647892373574,124.088610236154)) ;
#86054 = CARTESIAN_POINT('Ctrl Pts',(-20.6179988147476,23.3748103367399,124.312644230857)) ;
#86055 = CARTESIAN_POINT('Ctrl Pts',(-20.4449168413211,23.384717604602,124.507129660358)) ;
#86056 = CARTESIAN_POINT('Ctrl Pts',(-20.240390604112,23.3946559484272,124.669516991948)) ;
#86057 = CARTESIAN_POINT('Ctrl Pts',(-20.0093102113973,23.4046593677277,124.794907442227)) ;
#86058 = CARTESIAN_POINT('Ctrl Pts',(-19.7590948886003,23.4146939184348,124.878100956568)) ;
#86059 = CARTESIAN_POINT('Ctrl Pts',(-19.5031986835257,23.4245388680404,124.916298887153)) ;
#86060 = CARTESIAN_POINT('Ctrl Pts',(-19.240901379397,23.4345247101533,124.909881080696)) ;
#86061 = CARTESIAN_POINT('Ctrl Pts',(-18.9848919832439,23.4444595175224,124.858447576063)) ;
#86062 = CARTESIAN_POINT('Ctrl Pts',(-18.7388649759424,23.4545170592357,124.761980421742)) ;
#86063 = CARTESIAN_POINT('Ctrl Pts',(-18.5183526283299,23.4643386567478,124.627795609594)) ;
#86064 = CARTESIAN_POINT('Ctrl Pts',(-18.3195736794291,23.4743949162283,124.453691135326)) ;
#86065 = CARTESIAN_POINT('Ctrl Pts',(-18.1562934925279,23.4843348525287,124.249783586925)) ;
#86066 = CARTESIAN_POINT('Ctrl Pts',(-18.0306337931109,23.4942419732731,124.021771235105)) ;
#86067 = CARTESIAN_POINT('Ctrl Pts',(-17.9454129427096,23.5042848791984,123.771998892176)) ;
#86068 = CARTESIAN_POINT('Ctrl Pts',(-17.9053473190908,23.5141926602976,123.514723390938)) ;
#86069 = CARTESIAN_POINT('Ctrl Pts',(-17.9101532963783,23.5242030293,123.251696708579)) ;
#86070 = CARTESIAN_POINT('Ctrl Pts',(-17.961184062847,23.5342338678688,122.993085702516)) ;
#86071 = CARTESIAN_POINT('Ctrl Pts',(-18.0542237398046,23.5440867075085,122.751450868495)) ;
#86072 = CARTESIAN_POINT('Ctrl Pts',(-18.1892126976711,23.5540747086735,122.526373711805)) ;
#86073 = CARTESIAN_POINT('Ctrl Pts',(-18.3602268731788,23.5640035276526,122.329304006708)) ;
#86074 = CARTESIAN_POINT('Ctrl Pts',(-18.5637893871461,23.5739912303749,122.163599331592)) ;
#86075 = CARTESIAN_POINT('Ctrl Pts',(-18.7943337470643,23.5840272301776,122.035538227318)) ;
#86076 = CARTESIAN_POINT('Ctrl Pts',(-19.0390033894445,23.593882099979,121.95058970854)) ;
#86077 = CARTESIAN_POINT('Ctrl Pts',(-19.2983352169612,23.6038815304026,121.908467679911)) ;
#86078 = CARTESIAN_POINT('Ctrl Pts',(-19.5583918752554,23.6137766478679,121.911699650908)) ;
#86079 = CARTESIAN_POINT('Ctrl Pts',(-19.8181268029097,23.6238371413848,121.960855606037)) ;
#86080 = CARTESIAN_POINT('Ctrl Pts',(-20.0602942162802,23.633686621586,122.052288166794)) ;
#86081 = CARTESIAN_POINT('Ctrl Pts',(-20.2872341468449,23.6437130718498,122.186156421621)) ;
#86082 = CARTESIAN_POINT('Ctrl Pts',(-20.4871135693957,23.6537443623279,122.358035384557)) ;
#86083 = CARTESIAN_POINT('Ctrl Pts',(-20.6513848025357,23.6635857499797,122.55778850806)) ;
#86084 = CARTESIAN_POINT('Ctrl Pts',(-20.7809994490433,23.6735891508709,122.786461903559)) ;
#86085 = CARTESIAN_POINT('Ctrl Pts',(-20.8686943861811,23.6835735336621,123.033800795154)) ;
#86086 = CARTESIAN_POINT('Ctrl Pts',(-20.9120896033788,23.6936126236755,123.2939975435)) ;
#86087 = CARTESIAN_POINT('Ctrl Pts',(-20.9100555677439,23.7034584325847,123.552746650312)) ;
#86088 = CARTESIAN_POINT('Ctrl Pts',(-20.8629995601481,23.7134428554037,123.810834394173)) ;
#86089 = CARTESIAN_POINT('Ctrl Pts',(-20.7723339495502,23.7233824806449,124.055836429127)) ;
#86090 = CARTESIAN_POINT('Ctrl Pts',(-20.6391535588763,23.7334221701635,124.283563391533)) ;
#86091 = CARTESIAN_POINT('Ctrl Pts',(-20.4711070029557,23.7433103585821,124.481782915492)) ;
#86092 = CARTESIAN_POINT('Ctrl Pts',(-20.2694803443746,23.7532998845842,124.649877833456)) ;
#86093 = CARTESIAN_POINT('Ctrl Pts',(-20.042335267145,23.7632583859393,124.7798313255)) ;
#86094 = CARTESIAN_POINT('Ctrl Pts',(-19.7977296828341,23.773157979943,124.868459892283)) ;
#86095 = CARTESIAN_POINT('Ctrl Pts',(-19.5376387109747,23.7832058680643,124.913842306988)) ;
#86096 = CARTESIAN_POINT('Ctrl Pts',(-19.2775559394141,23.7931012933098,124.913585868621)) ;
#86097 = CARTESIAN_POINT('Ctrl Pts',(-19.0172389437925,23.8031626840104,124.867462659727)) ;
#86098 = CARTESIAN_POINT('Ctrl Pts',(-18.774152370709,23.8130082676971,124.778813564933)) ;
#86099 = CARTESIAN_POINT('Ctrl Pts',(-18.5470679864683,23.8229712410063,124.648540906934)) ;
#86100 = CARTESIAN_POINT('Ctrl Pts',(-18.3449854684297,23.8329969078321,124.479471088792)) ;
#86101 = CARTESIAN_POINT('Ctrl Pts',(-18.1771183031737,23.8429113856984,124.280226434427)) ;
#86102 = CARTESIAN_POINT('Ctrl Pts',(-18.0449530498413,23.8528999003734,124.053415180834)) ;
#86103 = CARTESIAN_POINT('Ctrl Pts',(-17.9542174865925,23.8629440112888,123.805578221622)) ;
#86104 = CARTESIAN_POINT('Ctrl Pts',(-17.9082598864059,23.8727721488834,123.551388438519)) ;
#86105 = CARTESIAN_POINT('Ctrl Pts',(-17.9069862290974,23.8828487169423,123.286644032258)) ;
#86106 = CARTESIAN_POINT('Ctrl Pts',(-17.9505929400621,23.8927008788465,123.031379907163)) ;
#86107 = CARTESIAN_POINT('Ctrl Pts',(-18.0395746759122,23.9027738408033,122.782125620061)) ;
#86108 = CARTESIAN_POINT('Ctrl Pts',(-18.1675552431538,23.9126164028062,122.557328161597)) ;
#86109 = CARTESIAN_POINT('Ctrl Pts',(-18.3342353084014,23.9225968393,122.35484385985)) ;
#86110 = CARTESIAN_POINT('Ctrl Pts',(-18.5346335209383,23.9326151446244,122.184110750498)) ;
#86111 = CARTESIAN_POINT('Ctrl Pts',(-18.7583418735152,23.9424991085438,122.052074633009)) ;
#86112 = CARTESIAN_POINT('Ctrl Pts',(-19.0060227711856,23.9525649852824,121.959294062984)) ;
#86113 = CARTESIAN_POINT('Ctrl Pts',(-19.2602154899171,23.9624040861433,121.911839822886)) ;
#86114 = CARTESIAN_POINT('Ctrl Pts',(-19.5238406827779,23.972437169009,121.90852668778)) ;
#86115 = CARTESIAN_POINT('Ctrl Pts',(-19.7836670395102,23.9824588542845,121.951641266166)) ;
#86116 = CARTESIAN_POINT('Ctrl Pts',(-20.0283217952903,23.992325549383,122.037454405699)) ;
#86117 = CARTESIAN_POINT('Ctrl Pts',(-20.256860421925,24.0022854391175,122.165053725248)) ;
#86118 = CARTESIAN_POINT('Ctrl Pts',(-20.4610242017121,24.012320426943,122.331938946934)) ;
#86119 = CARTESIAN_POINT('Ctrl Pts',(-20.6309297767146,24.0222071310173,122.528544653014)) ;
#86120 = CARTESIAN_POINT('Ctrl Pts',(-20.7664224941324,24.0322722752502,122.755656874661)) ;
#86121 = CARTESIAN_POINT('Ctrl Pts',(-20.858590344017,24.0421115659788,122.997281659938)) ;
#86122 = CARTESIAN_POINT('Ctrl Pts',(-20.9088537868088,24.0521741234172,123.256862342196)) ;
#86123 = CARTESIAN_POINT('Ctrl Pts',(-20.9129308819633,24.0620711746693,123.516929777868)) ;
#86124 = CARTESIAN_POINT('Ctrl Pts',(-20.8725108015801,24.0720023814176,123.77475646931)) ;
#86125 = CARTESIAN_POINT('Ctrl Pts',(-20.7867177695425,24.0820445656364,124.024315773816)) ;
#86126 = CARTESIAN_POINT('Ctrl Pts',(-20.661034087862,24.0919311937473,124.251717624557)) ;
#86127 = CARTESIAN_POINT('Ctrl Pts',(-20.4963706306924,24.1019244662797,124.456275571947)) ;
#86128 = CARTESIAN_POINT('Ctrl Pts',(-20.2995736659004,24.1118695418212,124.628245533589)) ;
#86129 = CARTESIAN_POINT('Ctrl Pts',(-20.0760604743478,24.1218190925494,124.763934584824)) ;
#86130 = CARTESIAN_POINT('Ctrl Pts',(-19.8301158593886,24.1318584273974,124.859366095419)) ;
#86131 = CARTESIAN_POINT('Ctrl Pts',(-19.5752990612999,24.1417445663413,124.910102290642)) ;
#86132 = CARTESIAN_POINT('Ctrl Pts',(-19.3126616551709,24.151742679315,124.916221608112)) ;
#86133 = CARTESIAN_POINT('Ctrl Pts',(-19.0549019437606,24.1616624416675,124.877102085613)) ;
#86134 = CARTESIAN_POINT('Ctrl Pts',(-18.8048861129423,24.1717018372801,124.792908728752)) ;
#86135 = CARTESIAN_POINT('Ctrl Pts',(-18.5763150218767,24.1816110230684,124.668144211837)) ;
#86136 = CARTESIAN_POINT('Ctrl Pts',(-18.3718886839389,24.1915462072259,124.50573368631)) ;
#86137 = CARTESIAN_POINT('Ctrl Pts',(-18.1971228535137,24.2015872646118,124.308047316945)) ;
#86138 = CARTESIAN_POINT('Ctrl Pts',(-18.0612783306157,24.2114744226451,124.086547050275)) ;
#86139 = CARTESIAN_POINT('Ctrl Pts',(-17.9645493227509,24.221466702321,123.842445202394)) ;
#86140 = CARTESIAN_POINT('Ctrl Pts',(-17.9119696693637,24.2314152193661,123.586335183678)) ;
#86141 = CARTESIAN_POINT('Ctrl Pts',(-17.9042989976674,24.2413519969365,123.325341447214)) ;
#86142 = CARTESIAN_POINT('Ctrl Pts',(-17.9419176299516,24.2513350330834,123.06567537359)) ;
#86143 = CARTESIAN_POINT('Ctrl Pts',(-18.0249900888699,24.2613787846771,122.815181470846)) ;
#86144 = CARTESIAN_POINT('Ctrl Pts',(-18.1471098273281,24.2712073138897,122.587547692865)) ;
#86145 = CARTESIAN_POINT('Ctrl Pts',(-18.3107425634225,24.2812826747984,122.379462252064)) ;
#86146 = CARTESIAN_POINT('Ctrl Pts',(-18.5037560854593,24.2911392736856,122.206642338797)) ;
#86147 = CARTESIAN_POINT('Ctrl Pts',(-18.7282169843324,24.3012022677035,122.066922869341)) ;
#86148 = CARTESIAN_POINT('Ctrl Pts',(-18.9691137819942,24.311080201993,121.970094344382)) ;
#86149 = CARTESIAN_POINT('Ctrl Pts',(-19.2261436370484,24.321080849551,121.915522158594)) ;
#86150 = CARTESIAN_POINT('Ctrl Pts',(-19.4866572465794,24.3309986959891,121.906283510334)) ;
#86151 = CARTESIAN_POINT('Ctrl Pts',(-19.7481874126353,24.3410498129947,121.942965407598)) ;
#86152 = CARTESIAN_POINT('Ctrl Pts',(-19.995044655726,24.3509205483053,122.022786909086)) ;
#86153 = CARTESIAN_POINT('Ctrl Pts',(-20.2288798534327,24.3609912555483,122.146628302463)) ;
#86154 = CARTESIAN_POINT('Ctrl Pts',(-20.4328576975085,24.3708242630002,122.305301061164)) ;
#86155 = CARTESIAN_POINT('Ctrl Pts',(-20.6102013492879,24.3808547553025,122.500299127757)) ;
#86156 = CARTESIAN_POINT('Ctrl Pts',(-20.7503713756113,24.3908863503759,122.723582642861)) ;
#86157 = CARTESIAN_POINT('Ctrl Pts',(-20.8481322685785,24.4007160495141,122.962664906748)) ;
#86158 = CARTESIAN_POINT('Ctrl Pts',(-20.9045567151015,24.4107054993957,123.219049565126)) ;
#86159 = CARTESIAN_POINT('Ctrl Pts',(-20.9149976124652,24.4207493572114,123.482781782384)) ;
#86160 = CARTESIAN_POINT('Ctrl Pts',(-20.8808031916903,24.4305710478016,123.738611883266)) ;
#86161 = CARTESIAN_POINT('Ctrl Pts',(-20.8016222714478,24.440606138342,123.990150687533)) ;
#86162 = CARTESIAN_POINT('Ctrl Pts',(-20.6794652177334,24.4506306573247,124.223569827565)) ;
#86163 = CARTESIAN_POINT('Ctrl Pts',(-20.5216485278088,24.4604905027349,124.429046599541)) ;
#86164 = CARTESIAN_POINT('Ctrl Pts',(-20.3290856748974,24.4704502790506,124.60632034406)) ;
#86165 = CARTESIAN_POINT('Ctrl Pts',(-20.1069640189552,24.4804784763652,124.748123595379)) ;
#86166 = CARTESIAN_POINT('Ctrl Pts',(-19.8666180274097,24.4903860186555,124.848283735091)) ;
#86167 = CARTESIAN_POINT('Ctrl Pts',(-19.6093832914182,24.5004186692194,124.905987754454)) ;
#86168 = CARTESIAN_POINT('Ctrl Pts',(-19.3499154760575,24.510302625646,124.918048718704)) ;
#86169 = CARTESIAN_POINT('Ctrl Pts',(-19.0894596086663,24.5202923270079,124.885168267668)) ;
#86170 = CARTESIAN_POINT('Ctrl Pts',(-18.8375518685682,24.5303333222839,124.806629416254)) ;
#86171 = CARTESIAN_POINT('Ctrl Pts',(-18.607775073596,24.5401662115523,124.688434190657)) ;
#86172 = CARTESIAN_POINT('Ctrl Pts',(-18.3982021069512,24.5501593699197,124.530191196066)) ;
#86173 = CARTESIAN_POINT('Ctrl Pts',(-18.2189836852721,24.5601914122718,124.336829304906)) ;
#86174 = CARTESIAN_POINT('Ctrl Pts',(-18.0781826899015,24.5700566562302,124.119164288488)) ;
#86175 = CARTESIAN_POINT('Ctrl Pts',(-17.9756353809418,24.5800185474762,123.878288988731)) ;
#86176 = CARTESIAN_POINT('Ctrl Pts',(-17.9164583703033,24.5900534474947,123.621321390185)) ;
#86177 = CARTESIAN_POINT('Ctrl Pts',(-17.9025709875067,24.5999385279093,123.361889607157)) ;
#86178 = CARTESIAN_POINT('Ctrl Pts',(-17.9345306575501,24.6100037000341,123.0993606842)) ;
#86179 = CARTESIAN_POINT('Ctrl Pts',(-18.009793838017,24.6198509347576,122.851745183802)) ;
#86180 = CARTESIAN_POINT('Ctrl Pts',(-18.1285188816227,24.6298817460754,122.616416570995)) ;
#86181 = CARTESIAN_POINT('Ctrl Pts',(-18.2864282941797,24.6398913619889,122.406008126817)) ;
#86182 = CARTESIAN_POINT('Ctrl Pts',(-18.4763620674248,24.6498021413926,122.227839272266)) ;
#86183 = CARTESIAN_POINT('Ctrl Pts',(-18.6944258490363,24.6597314071816,122.084521998851)) ;
#86184 = CARTESIAN_POINT('Ctrl Pts',(-18.9368657879906,24.6697741004942,121.980279706775)) ;
#86185 = CARTESIAN_POINT('Ctrl Pts',(-19.1897153085028,24.679660633189,121.92048694765)) ;
#86186 = CARTESIAN_POINT('Ctrl Pts',(-19.4518476983688,24.6896537782922,121.904901247144)) ;
#86187 = CARTESIAN_POINT('Ctrl Pts',(-19.7114689211226,24.6995994589663,121.935024786244)) ;
#86188 = CARTESIAN_POINT('Ctrl Pts',(-19.9621203216531,24.709546716593,122.009272431099)) ;
#86189 = CARTESIAN_POINT('Ctrl Pts',(-20.1982874731001,24.7195946187145,122.127349372162)) ;
#86190 = CARTESIAN_POINT('Ctrl Pts',(-20.4062771468984,24.7294423243362,122.281336350192)) ;
#86191 = CARTESIAN_POINT('Ctrl Pts',(-20.5870191315301,24.7394037909703,122.470689270979)) ;
#86192 = CARTESIAN_POINT('Ctrl Pts',(-20.7328443334499,24.7494333442385,122.690250749449)) ;
#86193 = CARTESIAN_POINT('Ctrl Pts',(-20.8371756815299,24.7593402362659,122.928777696645)) ;
#86194 = CARTESIAN_POINT('Ctrl Pts',(-20.8992448149416,24.7692878803789,123.182694125672)) ;
#86195 = CARTESIAN_POINT('Ctrl Pts',(-20.9165397755815,24.7792879234078,123.444949438803)) ;
#86196 = CARTESIAN_POINT('Ctrl Pts',(-20.8874649816599,24.7893266894018,123.707130191398)) ;
#86197 = CARTESIAN_POINT('Ctrl Pts',(-20.8154023193973,24.7991517514241,123.955080646736)) ;
#86198 = CARTESIAN_POINT('Ctrl Pts',(-20.6991263352566,24.8092062987504,124.192325406435)) ;
#86199 = CARTESIAN_POINT('Ctrl Pts',(-20.5447671392046,24.8191495421996,124.403167472963)) ;
#86200 = CARTESIAN_POINT('Ctrl Pts',(-20.3574869860895,24.8290517138075,124.58383784483)) ;
#86201 = CARTESIAN_POINT('Ctrl Pts',(-20.1383185841272,24.8391045494177,124.731315017245)) ;
#86202 = CARTESIAN_POINT('Ctrl Pts',(-19.901213310372,24.8489776071032,124.836683877999)) ;
#86203 = CARTESIAN_POINT('Ctrl Pts',(-19.646468082972,24.8589728686289,124.900684701347)) ;
#86204 = CARTESIAN_POINT('Ctrl Pts',(-19.3836496123046,24.8689982380494,124.919067997293)) ;
#86205 = CARTESIAN_POINT('Ctrl Pts',(-19.1251299071319,24.878888070576,124.892249885578)) ;
#86206 = CARTESIAN_POINT('Ctrl Pts',(-18.7890091715742,24.8921860413854,124.796799294934)) ;
#86207 = CARTESIAN_POINT('Ctrl Pts',(-18.4874128569439,24.9053844364946,124.617566260999)) ;
#86208 = CARTESIAN_POINT('Ctrl Pts',(-18.2417575404836,24.918779878774,124.365456812483)) ;
#86209 = CARTESIAN_POINT('Ctrl Pts',(-18.0954573193109,24.928655717013,124.151048711038)) ;
#86210 = CARTESIAN_POINT('Ctrl Pts',(-17.9865203150819,24.9387171196107,123.910175250881)) ;
#86211 = CARTESIAN_POINT('Ctrl Pts',(-17.9222460999715,24.9485821765459,123.658987057165)) ;
#86212 = CARTESIAN_POINT('Ctrl Pts',(-17.9018079283208,24.9585942724947,123.396707820689)) ;
#86213 = CARTESIAN_POINT('Ctrl Pts',(-17.9355686586318,24.9718715816401,123.049393446101)) ;
#86214 = CARTESIAN_POINT('Ctrl Pts',(-18.0899475407356,24.9884706071474,122.636126991343)) ;
#86215 = CARTESIAN_POINT('Ctrl Pts',(-18.3760314708444,25.0050696551804,122.300327989926)) ;
#86216 = CARTESIAN_POINT('Ctrl Pts',(-18.6623187112641,25.0183130672114,122.102384463216)) ;
#86217 = CARTESIAN_POINT('Ctrl Pts',(-18.9019733035102,25.0283504948998,121.992225850964)) ;
#86218 = CARTESIAN_POINT('Ctrl Pts',(-19.1537567559459,25.0382547968554,121.926273908146)) ;
#86219 = CARTESIAN_POINT('Ctrl Pts',(-19.5011724762164,25.0515216368306,121.896923152544)) ;
#86220 = CARTESIAN_POINT('Ctrl Pts',(-19.9361209211562,25.0681478349205,121.974892242463)) ;
#86221 = CARTESIAN_POINT('Ctrl Pts',(-20.3941483506745,25.0880669503039,122.240432926128)) ;
#86222 = CARTESIAN_POINT('Ctrl Pts',(-20.6778013141646,25.1046733734382,122.578575786354)) ;
#86223 = CARTESIAN_POINT('Ctrl Pts',(-20.8254198064288,25.1179695939339,122.895276836921)) ;
#86224 = CARTESIAN_POINT('Ctrl Pts',(-20.9163896664301,25.1312384262753,123.231970672834)) ;
#86225 = CARTESIAN_POINT('Ctrl Pts',(-20.9167689419944,25.1479296743084,123.675492638632)) ;
#86226 = CARTESIAN_POINT('Ctrl Pts',(-20.7380584204792,25.1677394059812,124.170815449789)) ;
#86227 = CARTESIAN_POINT('Ctrl Pts',(-20.3990544179289,25.1877170133098,124.579453442232)) ;
#86228 = CARTESIAN_POINT('Ctrl Pts',(-19.9416756734989,25.2076433223676,124.846325842365)) ;
#86229 = CARTESIAN_POINT('Ctrl Pts',(-19.4236779184025,25.2274601825323,124.942437107342)) ;
#86230 = CARTESIAN_POINT('Ctrl Pts',(-18.8970108487145,25.2475599981263,124.854014090052)) ;
#86231 = CARTESIAN_POINT('Ctrl Pts',(-18.4395915110761,25.2673169620089,124.595686505518)) ;
#86232 = CARTESIAN_POINT('Ctrl Pts',(-18.0924071157132,25.2873538880783,124.192105333411)) ;
#86233 = CARTESIAN_POINT('Ctrl Pts',(-17.9060265000467,25.3072234704598,123.697842908581)) ;
#86234 = CARTESIAN_POINT('Ctrl Pts',(-17.8981566895004,25.327128042213,123.168973851605)) ;
#86235 = CARTESIAN_POINT('Ctrl Pts',(-18.0717642136479,25.3470806444115,122.667793933237)) ;
#86236 = CARTESIAN_POINT('Ctrl Pts',(-18.4052645219479,25.3669901353818,122.257095727428)) ;
#86237 = CARTESIAN_POINT('Ctrl Pts',(-18.8570067132281,25.3868415040812,121.984255857802)) ;
#86238 = CARTESIAN_POINT('Ctrl Pts',(-19.3806239056403,25.4069217002172,121.881586989434)) ;
#86239 = CARTESIAN_POINT('Ctrl Pts',(-19.9007576230194,25.4267226437926,121.962652492736)) ;
#86240 = CARTESIAN_POINT('Ctrl Pts',(-20.3666506513675,25.4467066203021,122.217535832542)) ;
#86241 = CARTESIAN_POINT('Ctrl Pts',(-20.7158407306792,25.4666225832777,122.615352102572)) ;
#86242 = CARTESIAN_POINT('Ctrl Pts',(-20.9092753913654,25.4864930180996,123.10688621769)) ;
#86243 = CARTESIAN_POINT('Ctrl Pts',(-20.9225933282135,25.5065433033327,123.63946964645)) ;
#86244 = CARTESIAN_POINT('Ctrl Pts',(-20.7563011574428,25.526317272092,124.138248789555)) ;
#86245 = CARTESIAN_POINT('Ctrl Pts',(-20.4256737839772,25.5463737302116,124.55612392467)) ;
#86246 = CARTESIAN_POINT('Ctrl Pts',(-19.9778044990182,25.5661686132026,124.832472781124)) ;
#86247 = CARTESIAN_POINT('Ctrl Pts',(-19.4586089000129,25.5861352685049,124.941740459474)) ;
#86248 = CARTESIAN_POINT('Ctrl Pts',(-18.933405433002,25.6060942385814,124.866405585267)) ;
#86249 = CARTESIAN_POINT('Ctrl Pts',(-18.4668441914665,25.6259903261715,124.617555781116)) ;
#86250 = CARTESIAN_POINT('Ctrl Pts',(-18.1127144201242,25.6458884960831,124.224823959823)) ;
#86251 = CARTESIAN_POINT('Ctrl Pts',(-17.9132301741929,25.6657943314502,123.734766837906)) ;
#86252 = CARTESIAN_POINT('Ctrl Pts',(-17.8929228695584,25.6857442563881,123.204966867725)) ;
#86253 = CARTESIAN_POINT('Ctrl Pts',(-18.0536111401075,25.7056234462985,122.701580140501)) ;
#86254 = CARTESIAN_POINT('Ctrl Pts',(-18.377808589848,25.7256047705791,122.281003832198)) ;
#86255 = CARTESIAN_POINT('Ctrl Pts',(-18.8251899843192,25.7455345547874,121.99718762822)) ;
#86256 = CARTESIAN_POINT('Ctrl Pts',(-19.3420583616094,25.7654545441782,121.883074058097)) ;
#86257 = CARTESIAN_POINT('Ctrl Pts',(-19.8655398108464,25.7853097395322,121.95081448643)) ;
#86258 = CARTESIAN_POINT('Ctrl Pts',(-20.3385236962934,25.8053557411916,122.195787304325)) ;
#86259 = CARTESIAN_POINT('Ctrl Pts',(-20.6359551620709,25.8218554884014,122.518224212841)) ;
#86260 = CARTESIAN_POINT('Ctrl Pts',(-20.7997772299296,25.8352440928495,122.829543405343)) ;
#86261 = CARTESIAN_POINT('Ctrl Pts',(-20.878806089281,25.8451059211844,123.076370301885)) ;
#86262 = CARTESIAN_POINT('Ctrl Pts',(-20.9149660822381,25.855072063942,123.335767898469)) ;
#86263 = CARTESIAN_POINT('Ctrl Pts',(-20.901681357157,25.8684338100669,123.686592876107)) ;
#86264 = CARTESIAN_POINT('Ctrl Pts',(-20.7738066717889,25.884888139022,124.104963749759)) ;
#86265 = CARTESIAN_POINT('Ctrl Pts',(-20.5060796437535,25.9016553840703,124.461005538212)) ;
#86266 = CARTESIAN_POINT('Ctrl Pts',(-20.2328324341928,25.9148419493443,124.674328351222)) ;
#86267 = CARTESIAN_POINT('Ctrl Pts',(-20.0014412245227,25.9248314080889,124.798165745444)) ;
#86268 = CARTESIAN_POINT('Ctrl Pts',(-19.7528536304337,25.93478518057,124.879736163845)) ;
#86269 = CARTESIAN_POINT('Ctrl Pts',(-19.4914876961368,25.9448329971027,124.917038232705)) ;
#86270 = CARTESIAN_POINT('Ctrl Pts',(-19.2329656958291,25.9546745302252,124.908870993837)) ;
#86271 = CARTESIAN_POINT('Ctrl Pts',(-18.9760196741983,25.9646607724449,124.85572458636)) ;
#86272 = CARTESIAN_POINT('Ctrl Pts',(-18.7332872577401,25.9745973958698,124.759342505799)) ;
#86273 = CARTESIAN_POINT('Ctrl Pts',(-18.5085731788918,25.9846472732528,124.620640269178)) ;
#86274 = CARTESIAN_POINT('Ctrl Pts',(-18.3151059732975,25.9944977120304,124.448627307497)) ;
#86275 = CARTESIAN_POINT('Ctrl Pts',(-18.1519582512238,26.0044697259991,124.243595958302)) ;
#86276 = CARTESIAN_POINT('Ctrl Pts',(-18.0265942662714,26.0144648946252,124.012733796054)) ;
#86277 = CARTESIAN_POINT('Ctrl Pts',(-17.94321575523,26.0244987778864,123.762605317723)) ;
#86278 = CARTESIAN_POINT('Ctrl Pts',(-17.9048256332287,26.0343546479497,123.506445495096)) ;
#86279 = CARTESIAN_POINT('Ctrl Pts',(-17.9111726656182,26.0443521938669,123.243825664362)) ;
#86280 = CARTESIAN_POINT('Ctrl Pts',(-17.9624847437566,26.0542603207662,122.988545851874)) ;
#86281 = CARTESIAN_POINT('Ctrl Pts',(-18.0578964910856,26.0642706922883,122.743382417585)) ;
#86282 = CARTESIAN_POINT('Ctrl Pts',(-18.195192673543,26.0743011350357,122.518384012855)) ;
#86283 = CARTESIAN_POINT('Ctrl Pts',(-18.3658649539483,26.084149087589,122.323819765035)) ;
#86284 = CARTESIAN_POINT('Ctrl Pts',(-18.5719645952938,26.09421175661,122.158181340976)) ;
#86285 = CARTESIAN_POINT('Ctrl Pts',(-18.7999511759967,26.1041061320739,122.033112687758)) ;
#86286 = CARTESIAN_POINT('Ctrl Pts',(-19.0470918391407,26.1140479303921,121.948484295276)) ;
#86287 = CARTESIAN_POINT('Ctrl Pts',(-19.3067989983835,26.1240504241194,121.907695937297)) ;
#86288 = CARTESIAN_POINT('Ctrl Pts',(-19.5704318398782,26.1340852226263,121.913051573615)) ;
#86289 = CARTESIAN_POINT('Ctrl Pts',(-19.824351246944,26.1439301066057,121.9627151315)) ;
#86290 = CARTESIAN_POINT('Ctrl Pts',(-20.0693695516345,26.1539159634237,122.056561537333)) ;
#86291 = CARTESIAN_POINT('Ctrl Pts',(-20.2933941815534,26.1638507775985,122.19072291664)) ;
#86292 = CARTESIAN_POINT('Ctrl Pts',(-20.4929379375906,26.1739082773838,122.36397713695)) ;
#86293 = CARTESIAN_POINT('Ctrl Pts',(-20.6558144439717,26.1837300358021,122.564237995494)) ;
#86294 = CARTESIAN_POINT('Ctrl Pts',(-20.7848455998996,26.1937856935861,122.79482096552)) ;
#86295 = CARTESIAN_POINT('Ctrl Pts',(-20.8704620781849,26.2037278757661,123.041679298249)) ;
#86296 = CARTESIAN_POINT('Ctrl Pts',(-20.9125411179837,26.2136330844608,123.298550407497)) ;
#86297 = CARTESIAN_POINT('Ctrl Pts',(-20.9092518862155,26.2236748754233,123.56241297677)) ;
#86298 = CARTESIAN_POINT('Ctrl Pts',(-20.8608770737848,26.2335826498955,123.81825615933)) ;
#86299 = CARTESIAN_POINT('Ctrl Pts',(-20.7683065805399,26.2435941501231,124.064531536108)) ;
#86300 = CARTESIAN_POINT('Ctrl Pts',(-20.6336276204181,26.2536269105158,124.291186385178)) ;
#86301 = CARTESIAN_POINT('Ctrl Pts',(-20.4651029134243,26.2634774796507,124.487687379059)) ;
#86302 = CARTESIAN_POINT('Ctrl Pts',(-20.2625522855935,26.2734660891806,124.654609276642)) ;
#86303 = CARTESIAN_POINT('Ctrl Pts',(-20.0354400287525,26.2833947452047,124.783063120699)) ;
#86304 = CARTESIAN_POINT('Ctrl Pts',(-19.7881531187985,26.2933824913825,124.871070996956)) ;
#86305 = CARTESIAN_POINT('Ctrl Pts',(-19.5280420904567,26.3034184803182,124.914573869556)) ;
#86306 = CARTESIAN_POINT('Ctrl Pts',(-19.2690516259357,26.3132733501318,124.912723418728)) ;
#86307 = CARTESIAN_POINT('Ctrl Pts',(-19.0105800370941,26.3232727913736,124.86560866309)) ;
#86308 = CARTESIAN_POINT('Ctrl Pts',(-18.7666075707734,26.3331678655537,124.775514885921)) ;
#86309 = CARTESIAN_POINT('Ctrl Pts',(-18.5383077888514,26.3432285213934,124.642249303302)) ;
#86310 = CARTESIAN_POINT('Ctrl Pts',(-18.3407235540066,26.353077395589,124.475043878373)) ;
#86311 = CARTESIAN_POINT('Ctrl Pts',(-18.1716552019844,26.3631061075523,124.272882308973)) ;
#86312 = CARTESIAN_POINT('Ctrl Pts',(-18.040865209082,26.3731355081354,124.044055902173)) ;
#86313 = CARTESIAN_POINT('Ctrl Pts',(-17.9529323432651,26.3829757017522,123.800871133778)) ;
#86314 = CARTESIAN_POINT('Ctrl Pts',(-17.907349688925,26.3929791243274,123.542000520602)) ;
#86315 = CARTESIAN_POINT('Ctrl Pts',(-17.9074933099312,26.4029646614205,123.279546917314)) ;
#86316 = CARTESIAN_POINT('Ctrl Pts',(-17.9537071122485,26.4130056659073,123.019784028195)) ;
#86317 = CARTESIAN_POINT('Ctrl Pts',(-18.0422247319121,26.4228492048485,122.776701044052)) ;
#86318 = CARTESIAN_POINT('Ctrl Pts',(-18.172959280111,26.4328342358393,122.549236855608)) ;
#86319 = CARTESIAN_POINT('Ctrl Pts',(-18.3404039267093,26.4427736983613,122.348721052526)) ;
#86320 = CARTESIAN_POINT('Ctrl Pts',(-18.5421292540438,26.4528134305851,122.17870944488)) ;
#86321 = CARTESIAN_POINT('Ctrl Pts',(-18.7668321702435,26.4627016109023,122.048175439295)) ;
#86322 = CARTESIAN_POINT('Ctrl Pts',(-19.0130942013059,26.4726911266048,121.957267850095)) ;
#86323 = CARTESIAN_POINT('Ctrl Pts',(-19.270636423452,26.4826496772595,121.910844672131)) ;
#86324 = CARTESIAN_POINT('Ctrl Pts',(-19.5307953770956,26.4925490843645,121.909202223713)) ;
#86325 = CARTESIAN_POINT('Ctrl Pts',(-19.7910846414141,26.5025976707808,121.953512811704)) ;
#86326 = CARTESIAN_POINT('Ctrl Pts',(-20.0360368235489,26.5124904897453,122.040759031323)) ;
#86327 = CARTESIAN_POINT('Ctrl Pts',(-20.2660528706653,26.5225616072751,122.171557281645)) ;
#86328 = CARTESIAN_POINT('Ctrl Pts',(-20.4649953247139,26.5323773012411,122.335824675937)) ;
#86329 = CARTESIAN_POINT('Ctrl Pts',(-20.6368891208767,26.5424436787384,122.536824123293)) ;
#86330 = CARTESIAN_POINT('Ctrl Pts',(-20.7690314537872,26.5523426648203,122.760972791709)) ;
#86331 = CARTESIAN_POINT('Ctrl Pts',(-20.8617289021231,26.5623968448138,123.008329329804)) ;
#86332 = CARTESIAN_POINT('Ctrl Pts',(-20.9094601027412,26.5722676577465,123.263357508459)) ;
#86333 = CARTESIAN_POINT('Ctrl Pts',(-20.9122321988059,26.5823415586003,123.528012047214)) ;
#86334 = CARTESIAN_POINT('Ctrl Pts',(-20.8703917027367,26.592161713987,123.782723049251)) ;
#86335 = CARTESIAN_POINT('Ctrl Pts',(-20.7829899901851,26.6022404209392,124.032674888992)) ;
#86336 = CARTESIAN_POINT('Ctrl Pts',(-20.6564493553006,26.612092009478,124.25860286663)) ;
#86337 = CARTESIAN_POINT('Ctrl Pts',(-20.4891684822601,26.622165126003,124.463697321808)) ;
#86338 = CARTESIAN_POINT('Ctrl Pts',(-20.293323576881,26.6320076430988,124.632686826274)) ;
#86339 = CARTESIAN_POINT('Ctrl Pts',(-20.0684805251643,26.6419881046528,124.76769750117)) ;
#86340 = CARTESIAN_POINT('Ctrl Pts',(-19.8224939925488,26.6520063546435,124.861502416363)) ;
#86341 = CARTESIAN_POINT('Ctrl Pts',(-19.5674893463834,26.6618905148373,124.91103746618)) ;
#86342 = CARTESIAN_POINT('Ctrl Pts',(-19.3030567708649,26.6719556618123,124.915566855908)) ;
#86343 = CARTESIAN_POINT('Ctrl Pts',(-19.0475793987206,26.6817974854531,124.875168472208)) ;
#86344 = CARTESIAN_POINT('Ctrl Pts',(-18.7981276860572,26.6918269579139,124.79009847604)) ;
#86345 = CARTESIAN_POINT('Ctrl Pts',(-18.5676426643981,26.701853813176,124.662390118096)) ;
#86346 = CARTESIAN_POINT('Ctrl Pts',(-18.3661950342201,26.7116970632865,124.500120225689)) ;
#86347 = CARTESIAN_POINT('Ctrl Pts',(-18.1921722448789,26.7217455028697,124.301522698417)) ;
#86348 = CARTESIAN_POINT('Ctrl Pts',(-18.0569733160775,26.7316949971176,124.077726969622)) ;
#86349 = CARTESIAN_POINT('Ctrl Pts',(-17.9623479206744,26.7416028528436,123.835146450497)) ;
#86350 = CARTESIAN_POINT('Ctrl Pts',(-17.9107817759331,26.7516623294935,123.57590066682)) ;
#86351 = CARTESIAN_POINT('Ctrl Pts',(-17.9047865023787,26.7615031389022,123.317331030199)) ;
#86352 = CARTESIAN_POINT('Ctrl Pts',(-17.9443188755689,26.771565289203,123.055908426171)) ;
#86353 = CARTESIAN_POINT('Ctrl Pts',(-18.0275281430875,26.7814624503255,122.809476370172)) ;
#86354 = CARTESIAN_POINT('Ctrl Pts',(-18.1519197086005,26.7913936247296,122.580053321706)) ;
#86355 = CARTESIAN_POINT('Ctrl Pts',(-18.3162992678989,26.8014358284546,122.373607725889)) ;
#86356 = CARTESIAN_POINT('Ctrl Pts',(-18.5108502149347,26.8113224108851,122.201394321902)) ;
#86357 = CARTESIAN_POINT('Ctrl Pts',(-18.7344911406208,26.8213158466334,122.063754577682)) ;
#86358 = CARTESIAN_POINT('Ctrl Pts',(-18.9774833859817,26.8312603149915,121.96757970157)) ;
#86359 = CARTESIAN_POINT('Ctrl Pts',(-19.2335820350933,26.8412121312371,121.91453316318)) ;
#86360 = CARTESIAN_POINT('Ctrl Pts',(-19.4972322377189,26.8512495673516,121.906934424089)) ;
#86361 = CARTESIAN_POINT('Ctrl Pts',(-19.754305398308,26.8611345265279,121.944403815041)) ;
#86362 = CARTESIAN_POINT('Ctrl Pts',(-20.0038371906887,26.8711326447399,122.026561032475)) ;
#86363 = CARTESIAN_POINT('Ctrl Pts',(-20.2336644999362,26.8810535772519,122.149706995992)) ;
#86364 = CARTESIAN_POINT('Ctrl Pts',(-20.4411151613036,26.8910948774739,122.312763749208)) ;
#86365 = CARTESIAN_POINT('Ctrl Pts',(-20.6146912031061,26.9010017958639,122.506803957199)) ;
#86366 = CARTESIAN_POINT('Ctrl Pts',(-20.7529734778652,26.910937587573,122.728283521879)) ;
#86367 = CARTESIAN_POINT('Ctrl Pts',(-20.8514823737436,26.9209784821509,122.973063068783)) ;
#86368 = CARTESIAN_POINT('Ctrl Pts',(-20.9053481968387,26.9308656838647,123.227257943129)) ;
#86369 = CARTESIAN_POINT('Ctrl Pts',(-20.9147883410893,26.9408579516263,123.489656489309)) ;
#86370 = CARTESIAN_POINT('Ctrl Pts',(-20.8786067103794,26.9508064726481,123.74859249786)) ;
#86371 = CARTESIAN_POINT('Ctrl Pts',(-20.7984720557952,26.9607432462258,123.997098137103)) ;
#86372 = CARTESIAN_POINT('Ctrl Pts',(-20.676104628499,26.9707262943668,124.229192313943)) ;
#86373 = CARTESIAN_POINT('Ctrl Pts',(-20.5139774785616,26.9807700019769,124.437430943901)) ;
#86374 = CARTESIAN_POINT('Ctrl Pts',(-20.3227007873807,26.9905986951302,124.61104899263)) ;
#86375 = CARTESIAN_POINT('Ctrl Pts',(-20.0988745919875,27.0006734442596,124.75238354413)) ;
#86376 = CARTESIAN_POINT('Ctrl Pts',(-19.8589158285045,27.0105387700552,124.850593645606)) ;
#86377 = CARTESIAN_POINT('Ctrl Pts',(-19.6017027315997,27.0205609444121,124.907173107382)) ;
#86378 = CARTESIAN_POINT('Ctrl Pts',(-19.3384167298905,27.030586997619,124.917590734457)) ;
#86379 = CARTESIAN_POINT('Ctrl Pts',(-19.0817902884042,27.0404406944653,124.883165473566)) ;
#86380 = CARTESIAN_POINT('Ctrl Pts',(-18.8321269948554,27.0504000992183,124.804605397786)) ;
#86381 = CARTESIAN_POINT('Ctrl Pts',(-18.5982965329107,27.0604383449232,124.682527849518)) ;
#86382 = CARTESIAN_POINT('Ctrl Pts',(-18.3923088563404,27.0703125290852,124.524671749467)) ;
#86383 = CARTESIAN_POINT('Ctrl Pts',(-18.213440473293,27.0803823122231,124.329704461917)) ;
#86384 = CARTESIAN_POINT('Ctrl Pts',(-18.074335807759,27.0902155672439,124.111906520483)) ;
#86385 = CARTESIAN_POINT('Ctrl Pts',(-17.9724962914812,27.1002459933756,123.868794804679)) ;
#86386 = CARTESIAN_POINT('Ctrl Pts',(-17.9151518381184,27.1102776055626,123.61147237248)) ;
#86387 = CARTESIAN_POINT('Ctrl Pts',(-17.9030590057314,27.1201073024172,123.353458137196)) ;
#86388 = CARTESIAN_POINT('Ctrl Pts',(-17.9357095844985,27.1300967443197,123.092976875081)) ;
#86389 = CARTESIAN_POINT('Ctrl Pts',(-18.0141505189305,27.1401406363354,122.840961680301)) ;
#86390 = CARTESIAN_POINT('Ctrl Pts',(-18.1320070501894,27.1499621981046,122.611342543819)) ;
#86391 = CARTESIAN_POINT('Ctrl Pts',(-18.2908176421164,27.1599977697288,122.400792255072)) ;
#86392 = CARTESIAN_POINT('Ctrl Pts',(-18.4841896216697,27.1700270440106,122.221709205105)) ;
#86393 = CARTESIAN_POINT('Ctrl Pts',(-18.7010325739723,27.1798608811293,122.08111845669)) ;
#86394 = CARTESIAN_POINT('Ctrl Pts',(-18.9441365822861,27.1899132772174,121.97778844473)) ;
#86395 = CARTESIAN_POINT('Ctrl Pts',(-19.1986307271689,27.1998500441679,121.919247113411)) ;
#86396 = CARTESIAN_POINT('Ctrl Pts',(-19.4593067664465,27.2097842791472,121.905113637741)) ;
#86397 = CARTESIAN_POINT('Ctrl Pts',(-19.7207933748905,27.219808042474,121.936899749053)) ;
#86398 = CARTESIAN_POINT('Ctrl Pts',(-19.9693907811413,27.2296943838587,122.012371578883)) ;
#86399 = CARTESIAN_POINT('Ctrl Pts',(-20.2037993675098,27.2396834326256,122.130541837784)) ;
#86400 = CARTESIAN_POINT('Ctrl Pts',(-20.4148911017479,27.249724653323,122.288871926613)) ;
#86401 = CARTESIAN_POINT('Ctrl Pts',(-20.5918449134471,27.2595572935009,122.477157471636)) ;
#86402 = CARTESIAN_POINT('Ctrl Pts',(-20.7363711758217,27.2695512228089,122.696442446085)) ;
#86403 = CARTESIAN_POINT('Ctrl Pts',(-20.8404837011343,27.2795804304894,122.938566164147)) ;
#86404 = CARTESIAN_POINT('Ctrl Pts',(-20.9004632009322,27.2894562421935,123.191081286783)) ;
#86405 = CARTESIAN_POINT('Ctrl Pts',(-20.9161620820543,27.2994554691649,123.453345856358)) ;
#86406 = CARTESIAN_POINT('Ctrl Pts',(-20.8865937388302,27.3093649503206,123.712111167712)) ;
#86407 = CARTESIAN_POINT('Ctrl Pts',(-20.8114565304405,27.3194181806215,123.9653601692)) ;
#86408 = CARTESIAN_POINT('Ctrl Pts',(-20.695723180066,27.3292887971726,124.197519423031)) ;
#86409 = CARTESIAN_POINT('Ctrl Pts',(-20.5395590565441,27.3393104589046,124.409577578881)) ;
#86410 = CARTESIAN_POINT('Ctrl Pts',(-20.3484964827814,27.3493332720857,124.590894769313)) ;
#86411 = CARTESIAN_POINT('Ctrl Pts',(-20.1325252181775,27.3592004365456,124.734373686293)) ;
#86412 = CARTESIAN_POINT('Ctrl Pts',(-19.8921052555751,27.3691938787656,124.840061281651)) ;
#86413 = CARTESIAN_POINT('Ctrl Pts',(-19.6358971489778,27.3792255523659,124.902135847813)) ;
#86414 = CARTESIAN_POINT('Ctrl Pts',(-19.3771491513025,27.3890919874789,124.918905570282)) ;
#86415 = CARTESIAN_POINT('Ctrl Pts',(-19.1162550336676,27.399079438012,124.890574288521)) ;
#86416 = CARTESIAN_POINT('Ctrl Pts',(-18.8652095381394,27.4090243678399,124.817799802531)) ;
#86417 = CARTESIAN_POINT('Ctrl Pts',(-18.6283777604426,27.4190692628951,124.701277213198)) ;
#86418 = CARTESIAN_POINT('Ctrl Pts',(-18.4190826873744,27.4289313245809,124.548398528838)) ;
#86419 = CARTESIAN_POINT('Ctrl Pts',(-18.23679990877,27.4389230473678,124.35943784464)) ;
#86420 = CARTESIAN_POINT('Ctrl Pts',(-18.0910351330655,27.4488552616077,124.142920914045)) ;
#86421 = CARTESIAN_POINT('Ctrl Pts',(-17.9844514742124,27.4587945801734,123.90445397346)) ;
#86422 = CARTESIAN_POINT('Ctrl Pts',(-17.9204596210356,27.4688387549493,123.648382078966)) ;
#86423 = CARTESIAN_POINT('Ctrl Pts',(-17.902082443692,27.4787093090143,123.389646586281)) ;
#86424 = CARTESIAN_POINT('Ctrl Pts',(-17.9284117059881,27.4886742913685,123.129103791897)) ;
#86425 = CARTESIAN_POINT('Ctrl Pts',(-18.0004358375775,27.4987049942583,122.875545886623)) ;
#86426 = CARTESIAN_POINT('Ctrl Pts',(-18.1134828367361,27.5085973342835,122.641417708606)) ;
#86427 = CARTESIAN_POINT('Ctrl Pts',(-18.2678736241984,27.5186505674435,122.427083046342)) ;
#86428 = CARTESIAN_POINT('Ctrl Pts',(-18.4538449647151,27.5285318119202,122.245793517395)) ;
#86429 = CARTESIAN_POINT('Ctrl Pts',(-18.6715808971833,27.5385649327912,122.097192547089)) ;
#86430 = CARTESIAN_POINT('Ctrl Pts',(-18.9081664411668,27.5484461430663,121.990047207349)) ;
#86431 = CARTESIAN_POINT('Ctrl Pts',(-19.1642609051452,27.5585082188356,121.924381854683)) ;
#86432 = CARTESIAN_POINT('Ctrl Pts',(-19.4225664239136,27.5683652772174,121.904494754885)) ;
#86433 = CARTESIAN_POINT('Ctrl Pts',(-19.6839699262157,27.5783598325064,121.929577621368)) ;
#86434 = CARTESIAN_POINT('Ctrl Pts',(-19.9354082337427,27.5882857200419,121.999117799901)) ;
#86435 = CARTESIAN_POINT('Ctrl Pts',(-20.1732877832902,27.5983107400372,122.112287014641)) ;
#86436 = CARTESIAN_POINT('Ctrl Pts',(-20.3852469318587,27.6082081171408,122.263036295737)) ;
#86437 = CARTESIAN_POINT('Ctrl Pts',(-20.5699322318413,27.6181983542217,122.44963382705)) ;
#86438 = CARTESIAN_POINT('Ctrl Pts',(-20.7196829783269,27.6282349670305,122.666746029416)) ;
#86439 = CARTESIAN_POINT('Ctrl Pts',(-20.8278068728803,27.6380848504485,122.901936609501)) ;
#86440 = CARTESIAN_POINT('Ctrl Pts',(-20.8949783481644,27.648088467351,123.156067646929)) ;
#86441 = CARTESIAN_POINT('Ctrl Pts',(-20.9168353812002,27.6580778791161,123.417709468201)) ;
#86442 = CARTESIAN_POINT('Ctrl Pts',(-20.8927038903756,27.6680966404609,123.679858425827)) ;
#86443 = CARTESIAN_POINT('Ctrl Pts',(-20.8017637690144,27.681315315842,124.015169943229)) ;
#86444 = CARTESIAN_POINT('Ctrl Pts',(-20.624397640746,27.6946256230867,124.321149899939)) ;
#86445 = CARTESIAN_POINT('Ctrl Pts',(-20.3779433771167,27.7078632893127,124.566721861766)) ;
#86446 = CARTESIAN_POINT('Ctrl Pts',(-20.1646154796001,27.7177829847234,124.716537787326)) ;
#86447 = CARTESIAN_POINT('Ctrl Pts',(-19.9252314219541,27.727835851722,124.828242513711)) ;
#86448 = CARTESIAN_POINT('Ctrl Pts',(-19.6751407014436,27.7376912600512,124.895632476655)) ;
#86449 = CARTESIAN_POINT('Ctrl Pts',(-19.412428193496,27.7477298917278,124.919430792106)) ;
#86450 = CARTESIAN_POINT('Ctrl Pts',(-19.0641209038591,27.7610320739948,124.889619359484)) ;
#86451 = CARTESIAN_POINT('Ctrl Pts',(-18.6502903905597,27.7775770870777,124.740836279188)) ;
#86452 = CARTESIAN_POINT('Ctrl Pts',(-18.3098859245536,27.7942291031539,124.458090863763)) ;
#86453 = CARTESIAN_POINT('Ctrl Pts',(-18.1090493187269,27.8074521940591,124.17447204272)) ;
#86454 = CARTESIAN_POINT('Ctrl Pts',(-17.9965232918457,27.8174131536185,123.938133979673)) ;
#86455 = CARTESIAN_POINT('Ctrl Pts',(-17.9266087730233,27.8274379503696,123.684145144491)) ;
#86456 = CARTESIAN_POINT('Ctrl Pts',(-17.8934656932994,27.8406623977654,123.338168391895)) ;
#86457 = CARTESIAN_POINT('Ctrl Pts',(-17.9661155358838,27.8572961824645,122.902139051415)) ;
#86458 = CARTESIAN_POINT('Ctrl Pts',(-18.2260073081097,27.8771988491894,122.441354547989)) ;
#86459 = CARTESIAN_POINT('Ctrl Pts',(-18.6269746119238,27.8970990769713,122.096481259438)) ;
#86460 = CARTESIAN_POINT('Ctrl Pts',(-19.1218890723207,27.9170165645028,121.908622605301)) ;
#86461 = CARTESIAN_POINT('Ctrl Pts',(-19.6515477387723,27.9369460903197,121.90059571952)) ;
#86462 = CARTESIAN_POINT('Ctrl Pts',(-20.1529442502027,27.956908358206,122.07417484712)) ;
#86463 = CARTESIAN_POINT('Ctrl Pts',(-20.5634708106491,27.9767985531582,122.407134552226)) ;
#86464 = CARTESIAN_POINT('Ctrl Pts',(-20.8369751729256,27.9966887979044,122.859670241796)) ;
#86465 = CARTESIAN_POINT('Ctrl Pts',(-20.9394668766951,28.0167631704669,123.383205991598)) ;
#86466 = CARTESIAN_POINT('Ctrl Pts',(-20.8584842588624,28.0365485478272,123.902864524186)) ;
#86467 = CARTESIAN_POINT('Ctrl Pts',(-20.6042776799615,28.0565104218943,124.368499119697)) ;
#86468 = CARTESIAN_POINT('Ctrl Pts',(-20.2051858780569,28.0764903973848,124.718841264619)) ;
#86469 = CARTESIAN_POINT('Ctrl Pts',(-19.7150043467851,28.0963028272628,124.911309469325)) ;
#86470 = CARTESIAN_POINT('Ctrl Pts',(-19.1842604378428,28.1162829353531,124.925752106115)) ;
#86471 = CARTESIAN_POINT('Ctrl Pts',(-18.6824773897549,28.1361773189503,124.758643613806)) ;
#86472 = CARTESIAN_POINT('Ctrl Pts',(-18.2670496367191,28.1561042469275,124.430319759425)) ;
#86473 = CARTESIAN_POINT('Ctrl Pts',(-17.9883198062167,28.1759991042288,123.980833693048)) ;
#86474 = CARTESIAN_POINT('Ctrl Pts',(-17.8794805614305,28.1960382978324,123.459516608282)) ;
#86475 = CARTESIAN_POINT('Ctrl Pts',(-17.9544486755063,28.2158782657432,122.937505697659)) ;
#86476 = CARTESIAN_POINT('Ctrl Pts',(-18.2027332815713,28.2357930827073,122.470098177361)) ;
#86477 = CARTESIAN_POINT('Ctrl Pts',(-18.5964066329864,28.2557353281035,122.115256848635)) ;
#86478 = CARTESIAN_POINT('Ctrl Pts',(-19.0856168086369,28.275607376218,121.915866271612)) ;
#86479 = CARTESIAN_POINT('Ctrl Pts',(-19.6169218061426,28.2956184411721,121.895642781133)) ;
#86480 = CARTESIAN_POINT('Ctrl Pts',(-20.1188292935515,28.3154299654757,122.055652903489)) ;
#86481 = CARTESIAN_POINT('Ctrl Pts',(-20.5414244265229,28.3355251774391,122.381920562138)) ;
#86482 = CARTESIAN_POINT('Ctrl Pts',(-20.8229842740963,28.3553059013589,122.826156087312)) ;
#86483 = CARTESIAN_POINT('Ctrl Pts',(-20.9383586766976,28.3752969770017,123.344606135062)) ;
#86484 = CARTESIAN_POINT('Ctrl Pts',(-20.8698588440805,28.3951789160447,123.868727080192)) ;
#86485 = CARTESIAN_POINT('Ctrl Pts',(-20.6263861212141,28.415131520548,124.33974290189)) ;
#86486 = CARTESIAN_POINT('Ctrl Pts',(-20.2377379988083,28.4350303892786,124.69852394791)) ;
#86487 = CARTESIAN_POINT('Ctrl Pts',(-19.7505120225895,28.4549237890882,124.903632562329)) ;
#86488 = CARTESIAN_POINT('Ctrl Pts',(-19.2219604499456,28.4748329199282,124.931009679036)) ;
#86489 = CARTESIAN_POINT('Ctrl Pts',(-18.7130412720916,28.4948650196918,124.774779736929)) ;
#86490 = CARTESIAN_POINT('Ctrl Pts',(-18.3620584933981,28.5113970928613,124.510284590691)) ;
#86491 = CARTESIAN_POINT('Ctrl Pts',(-18.1460674126106,28.5247324334672,124.234383966013)) ;
#86492 = CARTESIAN_POINT('Ctrl Pts',(-18.0239856925731,28.5345749920069,124.006320082283)) ;
#86493 = CARTESIAN_POINT('Ctrl Pts',(-17.9414030192515,28.5446268988568,123.755444503094)) ;
#86494 = CARTESIAN_POINT('Ctrl Pts',(-17.8916917870985,28.5578754132477,123.410803822859)) ;
#86495 = CARTESIAN_POINT('Ctrl Pts',(-17.9431871506201,28.5744745881955,122.972697293955)) ;
#86496 = CARTESIAN_POINT('Ctrl Pts',(-18.1408539621108,28.5910633739905,122.578582469759)) ;
#86497 = CARTESIAN_POINT('Ctrl Pts',(-18.3723983221645,28.6043391903325,122.317615113724)) ;
#86498 = CARTESIAN_POINT('Ctrl Pts',(-18.577527292145,28.6143130411263,122.154436808147)) ;
#86499 = CARTESIAN_POINT('Ctrl Pts',(-18.8092646056395,28.6243420732187,122.028922034954)) ;
#86500 = CARTESIAN_POINT('Ctrl Pts',(-19.0557478273817,28.6342321987206,121.946437772454)) ;
#86501 = CARTESIAN_POINT('Ctrl Pts',(-19.3153706733146,28.6442246769921,121.907264160908)) ;
#86502 = CARTESIAN_POINT('Ctrl Pts',(-19.5768427425273,28.6541758920895,121.913598624698)) ;
#86503 = CARTESIAN_POINT('Ctrl Pts',(-19.8356388835886,28.6642243938445,121.9659387871)) ;
#86504 = CARTESIAN_POINT('Ctrl Pts',(-20.0765080850792,28.6740657434613,122.060169659542)) ;
#86505 = CARTESIAN_POINT('Ctrl Pts',(-20.300843510358,28.6840520344815,122.196258449548)) ;
#86506 = CARTESIAN_POINT('Ctrl Pts',(-20.4973109441294,28.6939886462101,122.368330827901)) ;
#86507 = CARTESIAN_POINT('Ctrl Pts',(-20.6626341566035,28.7040385215777,122.57425065372)) ;
#86508 = CARTESIAN_POINT('Ctrl Pts',(-20.7873624065296,28.7138889801131,122.801100887893)) ;
#86509 = CARTESIAN_POINT('Ctrl Pts',(-20.8724691047688,28.7238609170659,123.048913631883)) ;
#86510 = CARTESIAN_POINT('Ctrl Pts',(-20.9133208956479,28.733856373998,123.308428140769)) ;
#86511 = CARTESIAN_POINT('Ctrl Pts',(-20.9081765057666,28.7438891810511,123.572012092005)) ;
#86512 = CARTESIAN_POINT('Ctrl Pts',(-20.8585590805843,28.7537490676411,123.826338311456)) ;
#86513 = CARTESIAN_POINT('Ctrl Pts',(-20.764789229398,28.7637381482063,124.071497059533)) ;
#86514 = CARTESIAN_POINT('Ctrl Pts',(-20.6306361728563,28.7736696274155,124.295376547867)) ;
#86515 = CARTESIAN_POINT('Ctrl Pts',(-20.4590320836787,28.7836554868614,124.493932716745)) ;
#86516 = CARTESIAN_POINT('Ctrl Pts',(-20.2542272972785,28.7936936375086,124.660161314307)) ;
#86517 = CARTESIAN_POINT('Ctrl Pts',(-20.0282560662824,28.803541728013,124.78635916123)) ;
#86518 = CARTESIAN_POINT('Ctrl Pts',(-19.7786454124,28.813602636531,124.873435806326)) ;
#86519 = CARTESIAN_POINT('Ctrl Pts',(-19.5219342752848,28.8234974836889,124.914980277803)) ;
#86520 = CARTESIAN_POINT('Ctrl Pts',(-19.26072567087,28.833439155734,124.911999560869)) ;
#86521 = CARTESIAN_POINT('Ctrl Pts',(-19.0023461124135,28.8434416828595,124.863503088264)) ;
#86522 = CARTESIAN_POINT('Ctrl Pts',(-18.7557142855735,28.8534764740469,124.770209950683)) ;
#86523 = CARTESIAN_POINT('Ctrl Pts',(-18.5330665031705,28.863321353906,124.638416591467)) ;
#86524 = CARTESIAN_POINT('Ctrl Pts',(-18.3335959771311,28.8733072345245,124.467967806184)) ;
#86525 = CARTESIAN_POINT('Ctrl Pts',(-18.1674022200289,28.8832419576177,124.266559871745)) ;
#86526 = CARTESIAN_POINT('Ctrl Pts',(-18.0373647499672,28.8932997979289,124.036497815317)) ;
#86527 = CARTESIAN_POINT('Ctrl Pts',(-17.950911814326,28.9031202853254,123.793301563566)) ;
#86528 = CARTESIAN_POINT('Ctrl Pts',(-17.9065295280347,28.9131806866705,123.532709133583)) ;
#86529 = CARTESIAN_POINT('Ctrl Pts',(-17.9084022908856,28.9231116522234,123.271710634104)) ;
#86530 = CARTESIAN_POINT('Ctrl Pts',(-17.9550199869084,28.9330505145599,123.014749249068)) ;
#86531 = CARTESIAN_POINT('Ctrl Pts',(-18.0458283672377,28.9430362454861,122.768516340365)) ;
#86532 = CARTESIAN_POINT('Ctrl Pts',(-18.1787394441072,28.9530606309135,122.541096570347)) ;
#86533 = CARTESIAN_POINT('Ctrl Pts',(-18.3467919785273,28.9629639152668,122.342338042519)) ;
#86534 = CARTESIAN_POINT('Ctrl Pts',(-18.5499731696622,28.9730239198448,122.173252013428)) ;
#86535 = CARTESIAN_POINT('Ctrl Pts',(-18.7744434743641,28.9828671889139,122.044654486055)) ;
#86536 = CARTESIAN_POINT('Ctrl Pts',(-19.0212126462486,28.9928577545216,121.955119711378)) ;
#86537 = CARTESIAN_POINT('Ctrl Pts',(-19.2782134163419,29.0027858863004,121.910108935023)) ;
#86538 = CARTESIAN_POINT('Ctrl Pts',(-19.5406963148018,29.0127737733813,121.909949720142)) ;
#86539 = CARTESIAN_POINT('Ctrl Pts',(-19.8003636387641,29.02280972295,121.956024596532)) ;
#86540 = CARTESIAN_POINT('Ctrl Pts',(-20.0437946869578,29.0326646093288,122.0444605937)) ;
#86541 = CARTESIAN_POINT('Ctrl Pts',(-20.2715846639012,29.0426640236767,122.175375625611)) ;
#86542 = CARTESIAN_POINT('Ctrl Pts',(-20.4713275194905,29.0525591888672,122.34193965665)) ;
#86543 = CARTESIAN_POINT('Ctrl Pts',(-20.6418433631902,29.0626195075592,122.543928922245)) ;
#86544 = CARTESIAN_POINT('Ctrl Pts',(-20.7720825546946,29.0724696393352,122.767656038512)) ;
#86545 = CARTESIAN_POINT('Ctrl Pts',(-20.8637061447357,29.0825002097855,123.014799627036)) ;
#86546 = CARTESIAN_POINT('Ctrl Pts',(-20.9103762630913,29.0925143604583,123.273804452751)) ;
#86547 = CARTESIAN_POINT('Ctrl Pts',(-20.9117741336975,29.1024072940037,123.53378141723)) ;
#86548 = CARTESIAN_POINT('Ctrl Pts',(-20.867883240844,29.112396807994,123.792574654758)) ;
#86549 = CARTESIAN_POINT('Ctrl Pts',(-20.7801810778798,29.1223505786464,124.039048417847)) ;
#86550 = CARTESIAN_POINT('Ctrl Pts',(-20.6496213778519,29.132398347307,124.268526107138)) ;
#86551 = CARTESIAN_POINT('Ctrl Pts',(-20.4848587379141,29.1422400737468,124.46791155322)) ;
#86552 = CARTESIAN_POINT('Ctrl Pts',(-20.2855219341304,29.1522255905695,124.638505213354)) ;
#86553 = CARTESIAN_POINT('Ctrl Pts',(-20.0606187506956,29.1621649222651,124.771401656305)) ;
#86554 = CARTESIAN_POINT('Ctrl Pts',(-19.8136216179253,29.1722046919626,124.864082795799)) ;
#86555 = CARTESIAN_POINT('Ctrl Pts',(-19.558187368143,29.1820928532114,124.911871502229)) ;
#86556 = CARTESIAN_POINT('Ctrl Pts',(-19.2957011783519,29.1920824077138,124.915102448404)) ;
#86557 = CARTESIAN_POINT('Ctrl Pts',(-19.0374781818425,29.2020408222374,124.872643060304)) ;
#86558 = CARTESIAN_POINT('Ctrl Pts',(-18.7917703837319,29.2119407350668,124.787095968834)) ;
#86559 = CARTESIAN_POINT('Ctrl Pts',(-18.5613536456222,29.2219874347167,124.65825660223)) ;
#86560 = CARTESIAN_POINT('Ctrl Pts',(-18.3596420924881,29.2318872950223,124.493892512925)) ;
#86561 = CARTESIAN_POINT('Ctrl Pts',(-18.1869148909575,29.2419386992278,124.294103199834)) ;
#86562 = CARTESIAN_POINT('Ctrl Pts',(-18.0536769669931,29.2518197361489,124.071184737114)) ;
#86563 = CARTESIAN_POINT('Ctrl Pts',(-17.9597521892141,29.2618195683264,123.825804732125)) ;
#86564 = CARTESIAN_POINT('Ctrl Pts',(-17.9100403484687,29.2717375713113,123.569907928987)) ;
#86565 = CARTESIAN_POINT('Ctrl Pts',(-17.9055429199268,29.2817888771858,123.305853384214)) ;
#86566 = CARTESIAN_POINT('Ctrl Pts',(-17.9459174143974,29.2916587005774,123.049589465829)) ;
#86567 = CARTESIAN_POINT('Ctrl Pts',(-18.0318972364498,29.3017328666277,122.799266072468)) ;
#86568 = CARTESIAN_POINT('Ctrl Pts',(-18.1565829873438,29.3115529507693,122.573255953319)) ;
#86569 = CARTESIAN_POINT('Ctrl Pts',(-18.3226099186623,29.3216316775052,122.36697855623)) ;
#86570 = CARTESIAN_POINT('Ctrl Pts',(-18.5174760158988,29.3314832581547,122.196440883835)) ;
#86571 = CARTESIAN_POINT('Ctrl Pts',(-18.7437589213341,29.3415563864531,122.059171973647)) ;
#86572 = CARTESIAN_POINT('Ctrl Pts',(-18.9848715208291,29.3513988643445,121.965485865843)) ;
#86573 = CARTESIAN_POINT('Ctrl Pts',(-19.2419396876553,29.3613794709426,121.913527744618)) ;
#86574 = CARTESIAN_POINT('Ctrl Pts',(-19.5051237744955,29.3713971799614,121.907465724619)) ;
#86575 = CARTESIAN_POINT('Ctrl Pts',(-19.7620431375332,29.3812833589988,121.946175909808)) ;
#86576 = CARTESIAN_POINT('Ctrl Pts',(-20.0125730392579,29.3913409715712,122.030311528781)) ;
#86577 = CARTESIAN_POINT('Ctrl Pts',(-20.2405533557099,29.4012173649433,122.154388504609)) ;
#86578 = CARTESIAN_POINT('Ctrl Pts',(-20.4463541851592,29.4112123930937,122.317580930784)) ;
#86579 = CARTESIAN_POINT('Ctrl Pts',(-20.6208172138511,29.4212331399397,122.514846934847)) ;
#86580 = CARTESIAN_POINT('Ctrl Pts',(-20.7570016708868,29.4311352086061,122.736578720449)) ;
#86581 = CARTESIAN_POINT('Ctrl Pts',(-20.8538352390123,29.4411259484258,122.980616710616)) ;
#86582 = CARTESIAN_POINT('Ctrl Pts',(-20.9064868502557,29.4510891446361,123.23707769916)) ;
#86583 = CARTESIAN_POINT('Ctrl Pts',(-20.914410419633,29.4609933289362,123.497253000178)) ;
#86584 = CARTESIAN_POINT('Ctrl Pts',(-20.8762358005154,29.4710537893271,123.758827580412)) ;
#86585 = CARTESIAN_POINT('Ctrl Pts',(-20.7953305897781,29.4808943351979,124.004481871684)) ;
#86586 = CARTESIAN_POINT('Ctrl Pts',(-20.6705730749621,29.4909565559097,124.237592816873)) ;
#86587 = CARTESIAN_POINT('Ctrl Pts',(-20.5096749757579,29.5008536989262,124.441955772106)) ;
#86588 = CARTESIAN_POINT('Ctrl Pts',(-20.3156640114165,29.5107848753434,124.616506656617)) ;
#86589 = CARTESIAN_POINT('Ctrl Pts',(-20.0916629418475,29.520827089122,124.756019382219)) ;
#86590 = CARTESIAN_POINT('Ctrl Pts',(-19.8506899321232,29.5307136293248,124.853178323577)) ;
#86591 = CARTESIAN_POINT('Ctrl Pts',(-19.5938766834909,29.5407072239302,124.908009663912)) ;
#86592 = CARTESIAN_POINT('Ctrl Pts',(-19.332712747215,29.5506510990877,124.917331744836)) ;
#86593 = CARTESIAN_POINT('Ctrl Pts',(-19.0734479879124,29.5606116352025,124.881449299093)) ;
#86594 = CARTESIAN_POINT('Ctrl Pts',(-18.8233593876915,29.5706082385252,124.800941689882)) ;
#86595 = CARTESIAN_POINT('Ctrl Pts',(-18.5904051560722,29.5806413214798,124.677470404879)) ;
#86596 = CARTESIAN_POINT('Ctrl Pts',(-18.3859961074744,29.5904924901813,124.518621309858)) ;
#86597 = CARTESIAN_POINT('Ctrl Pts',(-18.2097416401463,29.6004549808802,124.325047682833)) ;
#86598 = CARTESIAN_POINT('Ctrl Pts',(-18.0691118335263,29.6104834092979,124.102151585275)) ;
#86599 = CARTESIAN_POINT('Ctrl Pts',(-17.9704269675126,29.6203937766625,123.861151262509)) ;
#86600 = CARTESIAN_POINT('Ctrl Pts',(-17.9142776230811,29.6303286442776,123.606174600459)) ;
#86601 = CARTESIAN_POINT('Ctrl Pts',(-17.9033816131702,29.6403697862566,123.342537736076)) ;
#86602 = CARTESIAN_POINT('Ctrl Pts',(-17.9377116774726,29.6502569224598,123.084976886491)) ;
#86603 = CARTESIAN_POINT('Ctrl Pts',(-18.0166487960382,29.6602492048632,122.834555046718)) ;
#86604 = CARTESIAN_POINT('Ctrl Pts',(-18.1374177643865,29.6701977328284,122.60266731771)) ;
#86605 = CARTESIAN_POINT('Ctrl Pts',(-18.2961113277449,29.6801344639905,122.395320977446)) ;
#86606 = CARTESIAN_POINT('Ctrl Pts',(-18.4891133100422,29.6901176748505,122.217574840443)) ;
#86607 = CARTESIAN_POINT('Ctrl Pts',(-18.7115763555757,29.7001607740004,122.075621485712)) ;
#86608 = CARTESIAN_POINT('Ctrl Pts',(-18.949992826985,29.7099917382753,121.976031903192)) ;
#86609 = CARTESIAN_POINT('Ctrl Pts',(-19.2081671628499,29.7200645906612,121.917784053486)) ;
#86610 = CARTESIAN_POINT('Ctrl Pts',(-19.467127300379,29.729928718373,121.905550210389)) ;
#86611 = CARTESIAN_POINT('Ctrl Pts',(-19.7284409010787,29.7399509205079,121.938343116302)) ;
#86612 = CARTESIAN_POINT('Ctrl Pts',(-19.9800566224885,29.7499781134763,122.016652854863)) ;
#86613 = CARTESIAN_POINT('Ctrl Pts',(-20.210400702207,29.7598337074433,122.135017062282)) ;
#86614 = CARTESIAN_POINT('Ctrl Pts',(-20.4193129127433,29.7697908793086,122.292588450327)) ;
#86615 = CARTESIAN_POINT('Ctrl Pts',(-20.5988052662756,29.779829723307,122.485901523046)) ;
#86616 = CARTESIAN_POINT('Ctrl Pts',(-20.740066998357,29.7897037471826,122.703600137925)) ;
#86617 = CARTESIAN_POINT('Ctrl Pts',(-20.8433563231969,29.799773573173,122.947193893449)) ;
#86618 = CARTESIAN_POINT('Ctrl Pts',(-20.9015323318944,29.8096068170702,123.198990450446)) ;
#86619 = CARTESIAN_POINT('Ctrl Pts',(-20.9161199372986,29.8196372448433,123.462166811631)) ;
#86620 = CARTESIAN_POINT('Ctrl Pts',(-20.8840222579638,29.8296688615884,123.723840344967)) ;
#86621 = CARTESIAN_POINT('Ctrl Pts',(-20.8090522677205,29.8394985385691,123.971017934646)) ;
#86622 = CARTESIAN_POINT('Ctrl Pts',(-20.6910925085159,29.8494880554091,124.205545773944)) ;
#86623 = CARTESIAN_POINT('Ctrl Pts',(-20.5328239158274,29.8595316675488,124.416758785664)) ;
#86624 = CARTESIAN_POINT('Ctrl Pts',(-20.3448871273158,29.8693542738841,124.593710045622)) ;
#86625 = CARTESIAN_POINT('Ctrl Pts',(-20.1246838233644,29.8793925037834,124.738944315077)) ;
#86626 = CARTESIAN_POINT('Ctrl Pts',(-19.8829956359094,29.8894035385753,124.842903601253)) ;
#86627 = CARTESIAN_POINT('Ctrl Pts',(-19.629944134694,29.8993012695424,124.903033941421)) ;
#86628 = CARTESIAN_POINT('Ctrl Pts',(-19.3679037961103,29.9092908973929,124.918797744218)) ;
#86629 = CARTESIAN_POINT('Ctrl Pts',(-19.1080010949963,29.9192466878389,124.88883390131)) ;
#86630 = CARTESIAN_POINT('Ctrl Pts',(-18.857809354991,29.929174086401,124.814884890953)) ;
#86631 = CARTESIAN_POINT('Ctrl Pts',(-18.6219992187214,29.9391996815108,124.697407355649)) ;
#86632 = CARTESIAN_POINT('Ctrl Pts',(-18.4130181328675,29.9490855321804,124.543075003642)) ;
#86633 = CARTESIAN_POINT('Ctrl Pts',(-18.2316836984906,29.9590747120246,124.353257774373)) ;
#86634 = CARTESIAN_POINT('Ctrl Pts',(-18.0857681933595,29.9691158991282,124.133401993258)) ;
#86635 = CARTESIAN_POINT('Ctrl Pts',(-17.9820470555373,29.9789485426041,123.896746050801)) ;
#86636 = CARTESIAN_POINT('Ctrl Pts',(-17.9192601596466,29.9889424923136,123.641732893525)) ;
#86637 = CARTESIAN_POINT('Ctrl Pts',(-17.9021985043466,29.9989716150901,123.378728309774)) ;
#86638 = CARTESIAN_POINT('Ctrl Pts',(-17.9302095800825,30.0088477460088,123.120696813041)) ;
#86639 = CARTESIAN_POINT('Ctrl Pts',(-18.0031833304748,30.0188457810258,122.868329081507)) ;
#86640 = CARTESIAN_POINT('Ctrl Pts',(-18.1177424147025,30.0287597107845,122.634304146691)) ;
#86641 = CARTESIAN_POINT('Ctrl Pts',(-18.2731207173211,30.0388028985223,122.420990591887)) ;
#86642 = CARTESIAN_POINT('Ctrl Pts',(-18.460477880612,30.0487027406627,122.240473905107)) ;
#86643 = CARTESIAN_POINT('Ctrl Pts',(-18.6780038327348,30.0586940074707,122.093431755788)) ;
#86644 = CARTESIAN_POINT('Ctrl Pts',(-18.9189236827015,30.0687261096027,121.986371546732)) ;
#86645 = CARTESIAN_POINT('Ctrl Pts',(-19.170468246111,30.0785929905574,121.92348620404)) ;
#86646 = CARTESIAN_POINT('Ctrl Pts',(-19.4323508510835,30.0885847818456,121.904376081853)) ;
#86647 = CARTESIAN_POINT('Ctrl Pts',(-19.6945696776365,30.0986168977571,121.931642192667)) ;
#86648 = CARTESIAN_POINT('Ctrl Pts',(-19.9440014901615,30.1084832145571,122.002451382793)) ;
#86649 = CARTESIAN_POINT('Ctrl Pts',(-20.1803630188248,30.1184706960307,122.116477795654)) ;
#86650 = CARTESIAN_POINT('Ctrl Pts',(-20.392566350984,30.1284156204096,122.269087188915)) ;
#86651 = CARTESIAN_POINT('Ctrl Pts',(-20.5767324875527,30.1384605063203,122.458162856591)) ;
#86652 = CARTESIAN_POINT('Ctrl Pts',(-20.7227801654869,30.1483226100329,122.67228121434)) ;
#86653 = CARTESIAN_POINT('Ctrl Pts',(-20.8312983726913,30.1583141738574,122.911353552395)) ;
#86654 = CARTESIAN_POINT('Ctrl Pts',(-20.8961724450446,30.1682469819203,123.164186294995)) ;
#86655 = CARTESIAN_POINT('Ctrl Pts',(-20.916810994507,30.1781840841566,123.424522266059)) ;
#86656 = CARTESIAN_POINT('Ctrl Pts',(-20.8912996042722,30.188236530427,123.687434835979)) ;
#86657 = CARTESIAN_POINT('Ctrl Pts',(-20.8223241947769,30.1980826460086,123.936840767883)) ;
#86658 = CARTESIAN_POINT('Ctrl Pts',(-20.7091987850365,30.2081306657235,124.17541152145)) ;
#86659 = CARTESIAN_POINT('Ctrl Pts',(-20.5576650602483,30.2180726173524,124.388259700238)) ;
#86660 = CARTESIAN_POINT('Ctrl Pts',(-20.3719976932811,30.2280113983515,124.57195695698)) ;
#86661 = CARTESIAN_POINT('Ctrl Pts',(-20.1552718930415,30.2380374470776,124.721755575099)) ;
#86662 = CARTESIAN_POINT('Ctrl Pts',(-19.9192454996909,30.2479243074858,124.830442864662)) ;
#86663 = CARTESIAN_POINT('Ctrl Pts',(-19.6643659591417,30.2579555826176,124.897557475444)) ;
#86664 = CARTESIAN_POINT('Ctrl Pts',(-19.4055132729224,30.267838559918,124.919346689653)) ;
#86665 = CARTESIAN_POINT('Ctrl Pts',(-19.1423742851105,30.2778954133252,124.895462225033)) ;
#86666 = CARTESIAN_POINT('Ctrl Pts',(-18.8081585492134,30.2910636544011,124.805348478367)) ;
#86667 = CARTESIAN_POINT('Ctrl Pts',(-18.4999606060616,30.3044646836276,124.627109350704)) ;
#86668 = CARTESIAN_POINT('Ctrl Pts',(-18.2548402508357,30.3176776003585,124.381034742561)) ;
#86669 = CARTESIAN_POINT('Ctrl Pts',(-18.1049154570646,30.3276059948117,124.167570645998)) ;
#86670 = CARTESIAN_POINT('Ctrl Pts',(-17.9935223888196,30.3375874949398,123.930052646589)) ;
#86671 = CARTESIAN_POINT('Ctrl Pts',(-17.9250251231697,30.3476280382099,123.675258459608)) ;
#86672 = CARTESIAN_POINT('Ctrl Pts',(-17.9019089621538,30.357477369993,123.417459308466)) ;
#86673 = CARTESIAN_POINT('Ctrl Pts',(-17.9235593814897,30.3674727744647,123.155687344675)) ;
#86674 = CARTESIAN_POINT('Ctrl Pts',(-17.9909293206155,30.3774891019133,122.901233828562)) ;
#86675 = CARTESIAN_POINT('Ctrl Pts',(-18.1363619700471,30.3907127590798,122.585590307536)) ;
#86676 = CARTESIAN_POINT('Ctrl Pts',(-18.3617445260575,30.4040070504692,122.313580619713)) ;
#86677 = CARTESIAN_POINT('Ctrl Pts',(-18.6465310373536,30.4172914014007,122.111548083525)) ;
#86678 = CARTESIAN_POINT('Ctrl Pts',(-18.8832363601411,30.4272637824625,121.999174549586)) ;
#86679 = CARTESIAN_POINT('Ctrl Pts',(-19.1341844428468,30.4371721620881,121.929596295639)) ;
#86680 = CARTESIAN_POINT('Ctrl Pts',(-19.3971607833827,30.4472261608362,121.904405542938)) ;
#86681 = CARTESIAN_POINT('Ctrl Pts',(-19.6555624151399,30.4570883579525,121.924666180462)) ;
#86682 = CARTESIAN_POINT('Ctrl Pts',(-19.9952854684949,30.4704354843266,122.01183022792)) ;
#86683 = CARTESIAN_POINT('Ctrl Pts',(-20.3783427936636,30.486972449968,122.227450317524)) ;
#86684 = CARTESIAN_POINT('Ctrl Pts',(-20.6669629084573,30.5036070541419,122.562246315872)) ;
#86685 = CARTESIAN_POINT('Ctrl Pts',(-20.8186251415275,30.5168968473846,122.876913691283)) ;
#86686 = CARTESIAN_POINT('Ctrl Pts',(-20.8898702450345,30.526849478644,123.128536989928)) ;
#86687 = CARTESIAN_POINT('Ctrl Pts',(-20.9166526278365,30.5368014459487,123.388718812429)) ;
#86688 = CARTESIAN_POINT('Ctrl Pts',(-20.8911983771875,30.5501687044125,123.739033428064)) ;
#86689 = CARTESIAN_POINT('Ctrl Pts',(-20.7477475189037,30.5666855163617,124.154053346653)) ;
#86690 = CARTESIAN_POINT('Ctrl Pts',(-20.4126988443248,30.586711411368,124.567435413989)) ;
#86691 = CARTESIAN_POINT('Ctrl Pts',(-19.9614671654052,30.6065221414982,124.838987072851)) ;
#86692 = CARTESIAN_POINT('Ctrl Pts',(-19.4406806653169,30.626499357628,124.942199667842)) ;
#86693 = CARTESIAN_POINT('Ctrl Pts',(-18.9173904837054,30.6464262330233,124.86074682562)) ;
#86694 = CARTESIAN_POINT('Ctrl Pts',(-18.4548551754709,30.6662476944996,124.608403042469)) ;
#86695 = CARTESIAN_POINT('Ctrl Pts',(-18.1021138578036,30.6863220123089,124.208208372338)) ;
#86696 = CARTESIAN_POINT('Ctrl Pts',(-17.9097086793361,30.7061699813168,123.716866447982)) ;
#86697 = CARTESIAN_POINT('Ctrl Pts',(-17.8953715490996,30.72611701538,123.187016557676)) ;
#86698 = CARTESIAN_POINT('Ctrl Pts',(-18.0624519723751,30.7460129663522,122.685261153681)) ;
#86699 = CARTESIAN_POINT('Ctrl Pts',(-18.3899873246686,30.7659084459704,122.270164037835)) ;
#86700 = CARTESIAN_POINT('Ctrl Pts',(-18.8408813750857,30.7858645569352,121.990764998331)) ;
#86701 = CARTESIAN_POINT('Ctrl Pts',(-19.3586318139167,30.8057691049752,121.882458783378)) ;
#86702 = CARTESIAN_POINT('Ctrl Pts',(-19.8818185744041,30.8256432292943,121.955925643777)) ;
#86703 = CARTESIAN_POINT('Ctrl Pts',(-20.3522474723433,30.8456977592933,122.206355579186)) ;
#86704 = CARTESIAN_POINT('Ctrl Pts',(-20.7048311303731,30.8655052730533,122.59744630561)) ;
#86705 = CARTESIAN_POINT('Ctrl Pts',(-20.9055172328141,30.885488628821,123.089116826482)) ;
#86706 = CARTESIAN_POINT('Ctrl Pts',(-20.9255113800788,30.905406931405,123.618128166974)) ;
#86707 = CARTESIAN_POINT('Ctrl Pts',(-20.7655078140649,30.9252751468507,124.121480433858)) ;
#86708 = CARTESIAN_POINT('Ctrl Pts',(-20.4398813109932,30.945325463647,124.543131309097)) ;
#86709 = CARTESIAN_POINT('Ctrl Pts',(-19.9961416301673,30.9651015255295,124.825243045067)) ;
#86710 = CARTESIAN_POINT('Ctrl Pts',(-19.4760428857146,30.9851561312219,124.940890724397)) ;
#86711 = CARTESIAN_POINT('Ctrl Pts',(-18.9542245242808,31.0049498203778,124.872803577724)) ;
#86712 = CARTESIAN_POINT('Ctrl Pts',(-18.4824553574321,31.0249165119722,124.630033633571)) ;
#86713 = CARTESIAN_POINT('Ctrl Pts',(-18.1224338999949,31.0448765577232,124.240259071478)) ;
#86714 = CARTESIAN_POINT('Ctrl Pts',(-17.9173964213131,31.0647748178734,123.752794316431)) ;
#86715 = CARTESIAN_POINT('Ctrl Pts',(-17.8903757638579,31.0846697334226,123.22473469265)) ;
#86716 = CARTESIAN_POINT('Ctrl Pts',(-18.0448284170245,31.1045799138362,122.718600932171)) ;
#86717 = CARTESIAN_POINT('Ctrl Pts',(-18.3629565328079,31.1245157129505,122.29484956572)) ;
#86718 = CARTESIAN_POINT('Ctrl Pts',(-18.8066023023989,31.1444535746046,122.005048043472)) ;
#86719 = CARTESIAN_POINT('Ctrl Pts',(-19.3219837707938,31.1643726212422,121.883821949317)) ;
#86720 = CARTESIAN_POINT('Ctrl Pts',(-19.8485586474663,31.1843215192964,121.945761987751)) ;
#86721 = CARTESIAN_POINT('Ctrl Pts',(-20.3214530576657,31.2042273467395,122.183047702527)) ;
#86722 = CARTESIAN_POINT('Ctrl Pts',(-20.62457405632,31.2208100421048,122.502904725448)) ;
#86723 = CARTESIAN_POINT('Ctrl Pts',(-20.7912398187945,31.2340842558284,122.809407390215)) ;
#86724 = CARTESIAN_POINT('Ctrl Pts',(-20.8750277230681,31.2441309750277,123.059747682737)) ;
#86725 = CARTESIAN_POINT('Ctrl Pts',(-20.9135794146644,31.2539750096734,123.315566077138)) ;
#86726 = CARTESIAN_POINT('Ctrl Pts',(-20.9056166911276,31.267309394578,123.665879105346)) ;
#86727 = CARTESIAN_POINT('Ctrl Pts',(-20.7817240069621,31.2838966118777,124.089024590941)) ;
#86728 = CARTESIAN_POINT('Ctrl Pts',(-20.5204927418564,31.3005298239156,124.44560763796)) ;
#86729 = CARTESIAN_POINT('Ctrl Pts',(-20.2482842473179,31.3138122661878,124.664159228814)) ;
#86730 = CARTESIAN_POINT('Ctrl Pts',(-20.0203552489676,31.323718154102,124.789870365395)) ;
#86731 = CARTESIAN_POINT('Ctrl Pts',(-19.7720861356419,31.3337065722071,124.875118114952)) ;
#86732 = CARTESIAN_POINT('Ctrl Pts',(-19.5118369240493,31.3437299994459,124.915827009597)) ;
#86733 = CARTESIAN_POINT('Ctrl Pts',(-19.2516219194721,31.3536344305629,124.910938614496)) ;
#86734 = CARTESIAN_POINT('Ctrl Pts',(-18.9093544512018,31.3668975831733,124.844874070695)) ;
#86735 = CARTESIAN_POINT('Ctrl Pts',(-18.5909341743351,31.3802224810772,124.689988959161)) ;
#86736 = CARTESIAN_POINT('Ctrl Pts',(-18.3276472878309,31.3934782246928,124.461818204276)) ;
#86737 = CARTESIAN_POINT('Ctrl Pts',(-18.1623509832731,31.4034375981401,124.258944934311)) ;
#86738 = CARTESIAN_POINT('Ctrl Pts',(-18.0346692467731,31.4133814220671,124.030912426066)) ;
#86739 = CARTESIAN_POINT('Ctrl Pts',(-17.9478499345261,31.4234293662144,123.781565182109)) ;
#86740 = CARTESIAN_POINT('Ctrl Pts',(-17.9062405916385,31.4332803374325,123.526042263013)) ;
#86741 = CARTESIAN_POINT('Ctrl Pts',(-17.9089961332649,31.4432521548746,123.264037869211)) ;
#86742 = CARTESIAN_POINT('Ctrl Pts',(-17.9573713255669,31.4532475771667,123.0058246328)) ;
#86743 = CARTESIAN_POINT('Ctrl Pts',(-18.0504365475839,31.4632806422904,122.759146467247)) ;
#86744 = CARTESIAN_POINT('Ctrl Pts',(-18.182455819894,31.4731459749556,122.53603494168)) ;
#86745 = CARTESIAN_POINT('Ctrl Pts',(-18.3522600986835,31.4831065175532,122.336826203529)) ;
#86746 = CARTESIAN_POINT('Ctrl Pts',(-18.555825302581,31.4931402030549,122.169258613365)) ;
#86747 = CARTESIAN_POINT('Ctrl Pts',(-18.7818081775691,31.5030250350452,122.04108939127)) ;
#86748 = CARTESIAN_POINT('Ctrl Pts',(-19.0310789742768,31.513092461805,121.952582039014)) ;
#86749 = CARTESIAN_POINT('Ctrl Pts',(-19.2860425398375,31.5229309509638,121.909432534115)) ;
#86750 = CARTESIAN_POINT('Ctrl Pts',(-19.5504588373335,31.532994432154,121.910897207184)) ;
#86751 = CARTESIAN_POINT('Ctrl Pts',(-19.806252038689,31.5428885899691,121.957687925717)) ;
#86752 = CARTESIAN_POINT('Ctrl Pts',(-20.0513987980626,31.5528304467134,122.047929059202)) ;
#86753 = CARTESIAN_POINT('Ctrl Pts',(-20.2786389120805,31.5628329243848,122.180116472421)) ;
#86754 = CARTESIAN_POINT('Ctrl Pts',(-20.4798154738035,31.5728677286891,122.350583181619)) ;
#86755 = CARTESIAN_POINT('Ctrl Pts',(-20.6455040679005,31.5827126055348,122.549301249805)) ;
#86756 = CARTESIAN_POINT('Ctrl Pts',(-20.7764127766709,31.5926984850903,122.776686313643)) ;
#86757 = CARTESIAN_POINT('Ctrl Pts',(-20.8656033287989,31.6026332154488,123.022106958682)) ;
#86758 = CARTESIAN_POINT('Ctrl Pts',(-20.9111243111444,31.6126910277617,123.282421856098)) ;
#86759 = CARTESIAN_POINT('Ctrl Pts',(-20.9112068367647,31.6225116198861,123.540539997943)) ;
#86760 = CARTESIAN_POINT('Ctrl Pts',(-20.865687331279,31.6325782054958,123.801079440899)) ;
#86761 = CARTESIAN_POINT('Ctrl Pts',(-20.7770317266897,31.6424777860777,124.045722854565)) ;
#86762 = CARTESIAN_POINT('Ctrl Pts',(-20.6453936142839,31.6525293857559,124.274672946805)) ;
#86763 = CARTESIAN_POINT('Ctrl Pts',(-20.4790792984421,31.6624035721729,124.473913961419)) ;
#86764 = CARTESIAN_POINT('Ctrl Pts',(-20.2772197656373,31.6724600480538,124.644405849723)) ;
#86765 = CARTESIAN_POINT('Ctrl Pts',(-20.0524976022664,31.6823529793564,124.775234014397)) ;
#86766 = CARTESIAN_POINT('Ctrl Pts',(-19.8043940631741,31.692415758069,124.866611670972)) ;
#86767 = CARTESIAN_POINT('Ctrl Pts',(-19.5498389701363,31.7022582836502,124.912638260607)) ;
#86768 = CARTESIAN_POINT('Ctrl Pts',(-19.287331714963,31.7122490490751,124.914410642322)) ;
#86769 = CARTESIAN_POINT('Ctrl Pts',(-19.0300907670381,31.7221771250731,124.870797527224)) ;
#86770 = CARTESIAN_POINT('Ctrl Pts',(-18.7826960536114,31.7321650354601,124.783086226261)) ;
#86771 = CARTESIAN_POINT('Ctrl Pts',(-18.5534309522588,31.7422009475851,124.652751134591)) ;
#86772 = CARTESIAN_POINT('Ctrl Pts',(-18.353644514985,31.7520559604328,124.487929296874)) ;
#86773 = CARTESIAN_POINT('Ctrl Pts',(-18.1828179715406,31.762054906349,124.288330075696)) ;
#86774 = CARTESIAN_POINT('Ctrl Pts',(-18.0503460097519,31.771951818797,124.064468215422)) ;
#86775 = CARTESIAN_POINT('Ctrl Pts',(-17.9573008027146,31.7820056168905,123.817225770989)) ;
#86776 = CARTESIAN_POINT('Ctrl Pts',(-17.9093501306192,31.7918865377172,123.562001493347)) ;
#86777 = CARTESIAN_POINT('Ctrl Pts',(-17.9059334517401,31.8018910637149,123.299145753374)) ;
#86778 = CARTESIAN_POINT('Ctrl Pts',(-17.9482120491376,31.8118750273324,123.040161685246)) ;
#86779 = CARTESIAN_POINT('Ctrl Pts',(-18.0355138245975,31.8219146678837,122.791213968382)) ;
#86780 = CARTESIAN_POINT('Ctrl Pts',(-18.1619308507885,31.8317586934984,122.565514127231)) ;
#86781 = CARTESIAN_POINT('Ctrl Pts',(-18.3274742184349,31.8417496993158,122.361724868883)) ;
#86782 = CARTESIAN_POINT('Ctrl Pts',(-18.5272092718872,31.8517874908479,122.189426042634)) ;
#86783 = CARTESIAN_POINT('Ctrl Pts',(-18.7492365418585,31.8616318906363,122.05662983357)) ;
#86784 = CARTESIAN_POINT('Ctrl Pts',(-18.9941697641335,31.8716166911931,121.962618647792)) ;
#86785 = CARTESIAN_POINT('Ctrl Pts',(-19.2505857843533,31.8815562146042,121.912666206365)) ;
#86786 = CARTESIAN_POINT('Ctrl Pts',(-19.5143572467387,31.8915959337052,121.908010594915)) ;
#86787 = CARTESIAN_POINT('Ctrl Pts',(-19.771053035124,31.9014841056245,121.94848018403)) ;
#86788 = CARTESIAN_POINT('Ctrl Pts',(-20.0194783206586,31.9114736680415,122.033298650539)) ;
#86789 = CARTESIAN_POINT('Ctrl Pts',(-20.2485944427228,31.9214320402362,122.159742447755)) ;
#86790 = CARTESIAN_POINT('Ctrl Pts',(-20.4514867933735,31.9313321144669,122.322607169725)) ;
#86791 = CARTESIAN_POINT('Ctrl Pts',(-20.6255075792033,31.9413782108405,122.521118480551)) ;
#86792 = CARTESIAN_POINT('Ctrl Pts',(-20.7605689119132,31.9512867948376,122.743753647204)) ;
#86793 = CARTESIAN_POINT('Ctrl Pts',(-20.8563432165643,31.9612973734285,122.988771599216)) ;
#86794 = CARTESIAN_POINT('Ctrl Pts',(-20.9076937965973,31.9713265315413,123.247285998441)) ;
#86795 = CARTESIAN_POINT('Ctrl Pts',(-20.9136494977614,31.9811794133794,123.506125048581)) ;
#86796 = CARTESIAN_POINT('Ctrl Pts',(-20.8749431252904,31.9911389745304,123.764982177503)) ;
#86797 = CARTESIAN_POINT('Ctrl Pts',(-20.7907719543159,32.0011774091195,124.014974716044)) ;
#86798 = CARTESIAN_POINT('Ctrl Pts',(-20.66695264249,32.0110506813466,124.243030789615)) ;
#86799 = CARTESIAN_POINT('Ctrl Pts',(-20.5021399302121,32.0211239233402,124.450109642599)) ;
#86800 = CARTESIAN_POINT('Ctrl Pts',(-20.3089945095504,32.0309442548732,124.621352168166)) ;
#86801 = CARTESIAN_POINT('Ctrl Pts',(-20.0834973590324,32.0410229161,124.760153885266)) ;
#86802 = CARTESIAN_POINT('Ctrl Pts',(-19.8427881240408,32.0508745113942,124.855626446842)) ;
#86803 = CARTESIAN_POINT('Ctrl Pts',(-19.5836101770202,32.060947646623,124.909232373603)) ;
#86804 = CARTESIAN_POINT('Ctrl Pts',(-19.3250477235278,32.0707900821481,124.91680672433)) ;
#86805 = CARTESIAN_POINT('Ctrl Pts',(-19.0654135129984,32.0807708512815,124.879716005305)) ;
#86806 = CARTESIAN_POINT('Ctrl Pts',(-18.8153951069858,32.0907879525253,124.797342091289)) ;
#86807 = CARTESIAN_POINT('Ctrl Pts',(-18.5862068913827,32.1006764001272,124.674829079308)) ;
#86808 = CARTESIAN_POINT('Ctrl Pts',(-18.3783323865825,32.110732114308,124.511717380021)) ;
#86809 = CARTESIAN_POINT('Ctrl Pts',(-18.20504643639,32.1206073207219,124.318515886017)) ;
#86810 = CARTESIAN_POINT('Ctrl Pts',(-18.0657523054065,32.1306023731946,124.095843008576)) ;
#86811 = CARTESIAN_POINT('Ctrl Pts',(-17.9673624393521,32.1406242571567,123.851536926118)) ;
#86812 = CARTESIAN_POINT('Ctrl Pts',(-17.9132447511668,32.150528229686,123.596960929366)) ;
#86813 = CARTESIAN_POINT('Ctrl Pts',(-17.9036966014167,32.1605167263469,123.334645288358)) ;
#86814 = CARTESIAN_POINT('Ctrl Pts',(-17.939924691972,32.1704805235949,123.07533896734)) ;
#86815 = CARTESIAN_POINT('Ctrl Pts',(-18.0195480393415,32.1803845469029,122.827524176256)) ;
#86816 = CARTESIAN_POINT('Ctrl Pts',(-18.1430776002173,32.1904450502245,122.593816083373)) ;
#86817 = CARTESIAN_POINT('Ctrl Pts',(-18.3015440658301,32.2002855853644,122.389414603507)) ;
#86818 = CARTESIAN_POINT('Ctrl Pts',(-18.4971343102704,32.210347806069,122.211511240556)) ;
#86819 = CARTESIAN_POINT('Ctrl Pts',(-18.7171578358292,32.2202449598452,122.072795116102)) ;
#86820 = CARTESIAN_POINT('Ctrl Pts',(-18.9584036223106,32.2301760932307,121.973254778566)) ;
#86821 = CARTESIAN_POINT('Ctrl Pts',(-19.2161862551315,32.2402184683764,121.916771627792)) ;
#86822 = CARTESIAN_POINT('Ctrl Pts',(-19.4757653790532,32.2501044061426,121.905874060276)) ;
#86823 = CARTESIAN_POINT('Ctrl Pts',(-19.7361743618916,32.2601002491274,121.940186996512)) ;
#86824 = CARTESIAN_POINT('Ctrl Pts',(-19.9853445011283,32.270042227006,122.01880797192)) ;
#86825 = CARTESIAN_POINT('Ctrl Pts',(-20.2176224237473,32.280001601487,122.139380240724)) ;
#86826 = CARTESIAN_POINT('Ctrl Pts',(-20.4263292540062,32.2899982173208,122.298965348353)) ;
#86827 = CARTESIAN_POINT('Ctrl Pts',(-20.6045437074103,32.3000324358943,122.49330330733)) ;
#86828 = CARTESIAN_POINT('Ctrl Pts',(-20.7440160089712,32.3098855031049,122.711454247693)) ;
#86829 = CARTESIAN_POINT('Ctrl Pts',(-20.8452761241106,32.3198457609825,122.952809541801)) ;
#86830 = CARTESIAN_POINT('Ctrl Pts',(-20.9031915155856,32.3298747876881,123.209934123648)) ;
#86831 = CARTESIAN_POINT('Ctrl Pts',(-20.9155108381836,32.3397849947225,123.470061362045)) ;
#86832 = CARTESIAN_POINT('Ctrl Pts',(-20.8830729146311,32.3497199053701,123.729125220497)) ;
#86833 = CARTESIAN_POINT('Ctrl Pts',(-20.8050925575432,32.3597610355494,123.98120077394)) ;
#86834 = CARTESIAN_POINT('Ctrl Pts',(-20.6865290803088,32.3696481759193,124.212412477173)) ;
#86835 = CARTESIAN_POINT('Ctrl Pts',(-20.5283214706852,32.3796404534553,124.421965720278)) ;
#86836 = CARTESIAN_POINT('Ctrl Pts',(-20.3368987653535,32.3895889967236,124.600050795474)) ;
#86837 = CARTESIAN_POINT('Ctrl Pts',(-20.1179553075885,32.3995256715408,124.742318590014)) ;
#86838 = CARTESIAN_POINT('Ctrl Pts',(-19.8765857645309,32.4095090924772,124.845198491733)) ;
#86839 = CARTESIAN_POINT('Ctrl Pts',(-19.6194540624684,32.4195514076664,124.904530262006)) ;
#86840 = CARTESIAN_POINT('Ctrl Pts',(-19.3612323588906,32.4293917251056,124.918456384701)) ;
#86841 = CARTESIAN_POINT('Ctrl Pts',(-19.0995012622624,32.4394214291631,124.887349726659)) ;
#86842 = CARTESIAN_POINT('Ctrl Pts',(-18.8475761386304,32.4494423858856,124.81065894568)) ;
#86843 = CARTESIAN_POINT('Ctrl Pts',(-18.6160938856141,32.4593089281892,124.693811732837)) ;
#86844 = CARTESIAN_POINT('Ctrl Pts',(-18.4041445829569,32.4693800281344,124.535355939284)) ;
#86845 = CARTESIAN_POINT('Ctrl Pts',(-18.2270297897121,32.4792221023119,124.346861724585)) ;
#86846 = CARTESIAN_POINT('Ctrl Pts',(-18.0828270949522,32.489182896899,124.128411540511)) ;
#86847 = CARTESIAN_POINT('Ctrl Pts',(-17.978420138532,32.4992207697998,123.88617867698)) ;
#86848 = CARTESIAN_POINT('Ctrl Pts',(-17.918171831887,32.5090950553439,123.633750736518)) ;
#86849 = CARTESIAN_POINT('Ctrl Pts',(-17.9023810135821,32.5191648057578,123.369635645094)) ;
#86850 = CARTESIAN_POINT('Ctrl Pts',(-17.9318454096663,32.5289980902925,123.112890613939)) ;
#86851 = CARTESIAN_POINT('Ctrl Pts',(-18.0061909068655,32.5390284310925,122.860013828916)) ;
#86852 = CARTESIAN_POINT('Ctrl Pts',(-18.1240350153628,32.5490603550921,122.624176778822)) ;
#86853 = CARTESIAN_POINT('Ctrl Pts',(-18.2773901023668,32.558888890028,122.416362824848)) ;
#86854 = CARTESIAN_POINT('Ctrl Pts',(-18.4671549519202,32.5688826677927,122.234811814169)) ;
#86855 = CARTESIAN_POINT('Ctrl Pts',(-18.6865982599419,32.5789103782782,122.088899208413)) ;
#86856 = CARTESIAN_POINT('Ctrl Pts',(-18.9245545564035,32.5887987891122,121.984478210373)) ;
#86857 = CARTESIAN_POINT('Ctrl Pts',(-19.179155033595,32.5987756396477,121.921970498854)) ;
#86858 = CARTESIAN_POINT('Ctrl Pts',(-19.4411893341139,32.6087674361982,121.904567510373)) ;
#86859 = CARTESIAN_POINT('Ctrl Pts',(-19.703326580114,32.6188034422919,121.933365758691)) ;
#86860 = CARTESIAN_POINT('Ctrl Pts',(-19.9519587960283,32.6286541765547,122.005505794216)) ;
#86861 = CARTESIAN_POINT('Ctrl Pts',(-20.1877508005523,32.6386454350829,122.120918680607)) ;
#86862 = CARTESIAN_POINT('Ctrl Pts',(-20.3985123625034,32.6485633299861,122.274300781478)) ;
#86863 = CARTESIAN_POINT('Ctrl Pts',(-20.5814614274393,32.6585914716491,122.463947516891)) ;
#86864 = CARTESIAN_POINT('Ctrl Pts',(-20.7267096138185,32.668476639765,122.679326125919)) ;
#86865 = CARTESIAN_POINT('Ctrl Pts',(-20.8340502982722,32.678466003271,122.918892802554)) ;
#86866 = CARTESIAN_POINT('Ctrl Pts',(-20.8979545030379,32.6885071382811,123.174908117759)) ;
#86867 = CARTESIAN_POINT('Ctrl Pts',(-20.9164761609195,32.6983398064691,123.432631238316)) ;
#86868 = CARTESIAN_POINT('Ctrl Pts',(-20.8902807920564,32.7083337094236,123.693949516132)) ;
#86869 = CARTESIAN_POINT('Ctrl Pts',(-20.8183191956796,32.7183629945081,123.947496333409)) ;
#86870 = CARTESIAN_POINT('Ctrl Pts',(-20.7055639452945,32.72823852295,124.181255541168)) ;
#86871 = CARTESIAN_POINT('Ctrl Pts',(-20.5522820009705,32.7382388055661,124.394679958423)) ;
#86872 = CARTESIAN_POINT('Ctrl Pts',(-20.366031988061,32.7481508216231,124.57682210646)) ;
#86873 = CARTESIAN_POINT('Ctrl Pts',(-20.1482437968875,32.7581928969621,124.725815001188)) ;
#86874 = CARTESIAN_POINT('Ctrl Pts',(-19.9112655719754,32.7680927296182,124.8331936985)) ;
#86875 = CARTESIAN_POINT('Ctrl Pts',(-19.65704415951,32.7780851301962,124.898959513189)) ;
#86876 = CARTESIAN_POINT('Ctrl Pts',(-19.3941345542646,32.7881191519556,124.919203661167)) ;
#86877 = CARTESIAN_POINT('Ctrl Pts',(-19.1361107148346,32.7979837627968,124.894256925511)) ;
#86878 = CARTESIAN_POINT('Ctrl Pts',(-18.8829224544705,32.807976162258,124.824605397838)) ;
#86879 = CARTESIAN_POINT('Ctrl Pts',(-18.6449612635533,32.8180081155909,124.711138853319)) ;
#86880 = CARTESIAN_POINT('Ctrl Pts',(-18.4336192368535,32.8278744745325,124.560921747617)) ;
#86881 = CARTESIAN_POINT('Ctrl Pts',(-18.2490612673754,32.8378619500183,124.374355254994)) ;
#86882 = CARTESIAN_POINT('Ctrl Pts',(-18.1001820205622,32.8478068562068,124.159518606616)) ;
#86883 = CARTESIAN_POINT('Ctrl Pts',(-17.9899307415803,32.857851820867,123.919702152225)) ;
#86884 = CARTESIAN_POINT('Ctrl Pts',(-17.9239755325999,32.8677136277719,123.669054864759)) ;
#86885 = CARTESIAN_POINT('Ctrl Pts',(-17.9017602263012,32.8777063000777,123.407426433999)) ;
#86886 = CARTESIAN_POINT('Ctrl Pts',(-17.9251935246742,32.887634971023,123.147548631717)) ;
#86887 = CARTESIAN_POINT('Ctrl Pts',(-17.9931352135227,32.8975875132483,122.895003816011)) ;
#86888 = CARTESIAN_POINT('Ctrl Pts',(-18.1043312287972,32.9075888692442,122.656829799846)) ;
#86889 = CARTESIAN_POINT('Ctrl Pts',(-18.2558767004374,32.9176174815189,122.441233493131)) ;
#86890 = CARTESIAN_POINT('Ctrl Pts',(-18.4392492938704,32.9274818160684,122.257982555295)) ;
#86891 = CARTESIAN_POINT('Ctrl Pts',(-18.6541333399341,32.937474140145,122.107122522269)) ;
#86892 = CARTESIAN_POINT('Ctrl Pts',(-18.8904036310431,32.9474016325109,121.996414241407)) ;
#86893 = CARTESIAN_POINT('Ctrl Pts',(-19.144776160248,32.9574289910617,121.927756331862)) ;
#86894 = CARTESIAN_POINT('Ctrl Pts',(-19.4035634233285,32.9673154091128,121.904356292453)) ;
#86895 = CARTESIAN_POINT('Ctrl Pts',(-19.6662173972518,32.9773471438482,121.926427682475)) ;
#86896 = CARTESIAN_POINT('Ctrl Pts',(-19.9173873207107,32.9872287250915,121.992537401162)) ;
#86897 = CARTESIAN_POINT('Ctrl Pts',(-20.1575155915266,32.9972907031238,122.103143972169)) ;
#86898 = CARTESIAN_POINT('Ctrl Pts',(-20.370483550717,33.0071477814855,122.250663584042)) ;
#86899 = CARTESIAN_POINT('Ctrl Pts',(-20.5574852732715,33.0171423545915,122.435031329392)) ;
#86900 = CARTESIAN_POINT('Ctrl Pts',(-20.7087098909113,33.0270681508791,122.647604267584)) ;
#86901 = CARTESIAN_POINT('Ctrl Pts',(-20.8218893770371,33.0370935180488,122.885487342572)) ;
#86902 = CARTESIAN_POINT('Ctrl Pts',(-20.8912556584646,33.0469895977027,123.136134795138)) ;
#86903 = CARTESIAN_POINT('Ctrl Pts',(-20.9168234356785,33.0569846774083,123.397550614612)) ;
#86904 = CARTESIAN_POINT('Ctrl Pts',(-20.8961029605947,33.0670097652241,123.660183142044)) ;
#86905 = CARTESIAN_POINT('Ctrl Pts',(-20.8098991145045,33.0801935875914,123.99574300305)) ;
#86906 = CARTESIAN_POINT('Ctrl Pts',(-20.6369446858756,33.0935157057373,124.304678709047)) ;
#86907 = CARTESIAN_POINT('Ctrl Pts',(-20.3908204960889,33.1068949153649,124.555834602614)) ;
#86908 = CARTESIAN_POINT('Ctrl Pts',(-20.1809494793358,33.1167331526091,124.706837071298)) ;
#86909 = CARTESIAN_POINT('Ctrl Pts',(-19.942577781835,33.1268060758678,124.821869252031)) ;
#86910 = CARTESIAN_POINT('Ctrl Pts',(-19.693263181732,33.1366627173229,124.892205355517)) ;
#86911 = CARTESIAN_POINT('Ctrl Pts',(-19.4322613230798,33.146648092829,124.919218109963)) ;
#86912 = CARTESIAN_POINT('Ctrl Pts',(-19.0841401970618,33.1599321242894,124.89401589364)) ;
#86913 = CARTESIAN_POINT('Ctrl Pts',(-18.6686887473864,33.1764509161598,124.751538820693)) ;
#86914 = CARTESIAN_POINT('Ctrl Pts',(-18.322123263724,33.1932366331664,124.470796884464)) ;
#86915 = CARTESIAN_POINT('Ctrl Pts',(-18.1195228019478,33.2063497816754,124.191941939277)) ;
#86916 = CARTESIAN_POINT('Ctrl Pts',(-18.0029823657326,33.2163853307556,123.955407109914)) ;
#86917 = CARTESIAN_POINT('Ctrl Pts',(-17.9301367991554,33.226401386935,123.70244375215)) ;
#86918 = CARTESIAN_POINT('Ctrl Pts',(-17.8928038233433,33.239579422801,123.358205398184)) ;
#86919 = CARTESIAN_POINT('Ctrl Pts',(-17.9589484139631,33.2561812999881,122.921862723111)) ;
#86920 = CARTESIAN_POINT('Ctrl Pts',(-18.2153509315473,33.276244444604,122.454328572859)) ;
#86921 = CARTESIAN_POINT('Ctrl Pts',(-18.610517617413,33.2960453346877,122.106659477122)) ;
#86922 = CARTESIAN_POINT('Ctrl Pts',(-19.1034981315604,33.3159884599664,121.912149478104)) ;
#86923 = CARTESIAN_POINT('Ctrl Pts',(-19.6321521720369,33.335886505086,121.897927841427)) ;
#86924 = CARTESIAN_POINT('Ctrl Pts',(-20.1341123261989,33.3557722647127,122.063632571961)) ;
#86925 = CARTESIAN_POINT('Ctrl Pts',(-20.5525339489159,33.3758374398926,122.394216721666)) ;
#86926 = CARTESIAN_POINT('Ctrl Pts',(-20.8296056794486,33.3956640829954,122.842560084467)) ;
#86927 = CARTESIAN_POINT('Ctrl Pts',(-20.9388743874097,33.4155727924438,123.360152546638)) ;
#86928 = CARTESIAN_POINT('Ctrl Pts',(-20.8648847574417,33.4355246294756,123.885402002908)) ;
#86929 = CARTESIAN_POINT('Ctrl Pts',(-20.6147318866576,33.4555331041787,124.35462141048)) ;
#86930 = CARTESIAN_POINT('Ctrl Pts',(-20.2239322170856,33.4753345629402,124.707141469447)) ;
#86931 = CARTESIAN_POINT('Ctrl Pts',(-19.7330000970732,33.4952914511762,124.907967316448)) ;
#86932 = CARTESIAN_POINT('Ctrl Pts',(-19.2022616264228,33.5152752885903,124.92803419319)) ;
#86933 = CARTESIAN_POINT('Ctrl Pts',(-18.7005637331334,33.5350837278112,124.768198422526)) ;
#86934 = CARTESIAN_POINT('Ctrl Pts',(-18.2796383911774,33.5550694371914,124.44444941678)) ;
#86935 = CARTESIAN_POINT('Ctrl Pts',(-17.9957682334727,33.5749389602067,123.998878153294)) ;
#86936 = CARTESIAN_POINT('Ctrl Pts',(-17.8804168309484,33.5949596993239,123.479617978128)) ;
#86937 = CARTESIAN_POINT('Ctrl Pts',(-17.9478193704265,33.6147637643009,122.957391827928)) ;
#86938 = CARTESIAN_POINT('Ctrl Pts',(-18.1922075876265,33.6348257280316,122.483648094758)) ;
#86939 = CARTESIAN_POINT('Ctrl Pts',(-18.5796761414085,33.6546589083201,122.126063706925)) ;
#86940 = CARTESIAN_POINT('Ctrl Pts',(-19.0672471785734,33.6745781056462,121.919993572332)) ;
#86941 = CARTESIAN_POINT('Ctrl Pts',(-19.5964794361335,33.6945161307595,121.892984850209)) ;
#86942 = CARTESIAN_POINT('Ctrl Pts',(-20.1019033803434,33.7143941768156,122.047027331049)) ;
#86943 = CARTESIAN_POINT('Ctrl Pts',(-20.5266212368,33.7343789111036,122.365892503823)) ;
#86944 = CARTESIAN_POINT('Ctrl Pts',(-20.8161596894946,33.7542897277821,122.809038474966)) ;
#86945 = CARTESIAN_POINT('Ctrl Pts',(-20.9372320691971,33.7742887033008,123.326476372936)) ;
#86946 = CARTESIAN_POINT('Ctrl Pts',(-20.8757063920879,33.794093623946,123.849357303765)) ;
#86947 = CARTESIAN_POINT('Ctrl Pts',(-20.6381117871144,33.8140775842373,124.324253054695)) ;
#86948 = CARTESIAN_POINT('Ctrl Pts',(-20.2542831223755,33.8339637879612,124.68776744017)) ;
#86949 = CARTESIAN_POINT('Ctrl Pts',(-19.7682875774795,33.8539129662844,124.899638859617)) ;
#86950 = CARTESIAN_POINT('Ctrl Pts',(-19.2403826918121,33.8738147655239,124.932749323291)) ;
#86951 = CARTESIAN_POINT('Ctrl Pts',(-18.7331049966278,33.8936933705763,124.784958195481)) ;
#86952 = CARTESIAN_POINT('Ctrl Pts',(-18.3035554846274,33.913725730302,124.470321163056)) ;
#86953 = CARTESIAN_POINT('Ctrl Pts',(-18.0587986989934,33.9303074562581,124.103799046386)) ;
#86954 = CARTESIAN_POINT('Ctrl Pts',(-17.9464440989299,33.943501626556,123.775801865132)) ;
#86955 = CARTESIAN_POINT('Ctrl Pts',(-17.891701854277,33.9568138046492,123.430280794334)) ;
#86956 = CARTESIAN_POINT('Ctrl Pts',(-17.937495113229,33.9733799842425,122.992341681738)) ;
#86957 = CARTESIAN_POINT('Ctrl Pts',(-18.1302774467429,33.9900081791027,122.594720028889)) ;
#86958 = CARTESIAN_POINT('Ctrl Pts',(-18.3588197435753,34.0032967608125,122.330608010279)) ;
#86959 = CARTESIAN_POINT('Ctrl Pts',(-18.5618595656554,34.0132650089161,122.165129183368)) ;
#86960 = CARTESIAN_POINT('Ctrl Pts',(-18.7891847096601,34.0231797651722,122.037806845521)) ;
#86961 = CARTESIAN_POINT('Ctrl Pts',(-19.0375192291355,34.0331929158234,121.950759748817)) ;
#86962 = CARTESIAN_POINT('Ctrl Pts',(-19.2972286630396,34.0432056230254,121.908570343025)) ;
#86963 = CARTESIAN_POINT('Ctrl Pts',(-19.6446460039,34.0564249117167,121.912596021897)) ;
#86964 = CARTESIAN_POINT('Ctrl Pts',(-20.0699254705713,34.0730435927147,122.03142792988)) ;
#86965 = CARTESIAN_POINT('Ctrl Pts',(-20.4284671618756,34.0896085004882,122.287092857787)) ;
#86966 = CARTESIAN_POINT('Ctrl Pts',(-20.6522378081821,34.103006972099,122.558923682417)) ;
#86967 = CARTESIAN_POINT('Ctrl Pts',(-20.779673548747,34.112848227586,122.78398886291)) ;
#86968 = CARTESIAN_POINT('Ctrl Pts',(-20.8678897526762,34.1228345431742,123.031102300472)) ;
#86969 = CARTESIAN_POINT('Ctrl Pts',(-20.9117788511624,34.1327711507606,123.288555336312)) ;
#86970 = CARTESIAN_POINT('Ctrl Pts',(-20.9101514532125,34.1428210181289,123.552623293535)) ;
#86971 = CARTESIAN_POINT('Ctrl Pts',(-20.863821952132,34.1526715128037,123.807324091934)) ;
#86972 = CARTESIAN_POINT('Ctrl Pts',(-20.7735256213535,34.1626433131982,124.053287870522)) ;
#86973 = CARTESIAN_POINT('Ctrl Pts',(-20.6415098394546,34.172639280224,124.280439245738)) ;
#86974 = CARTESIAN_POINT('Ctrl Pts',(-20.4711254085416,34.1826767396052,124.481765931649)) ;
#86975 = CARTESIAN_POINT('Ctrl Pts',(-20.2726263760509,34.1925174405059,124.647547741897)) ;
#86976 = CARTESIAN_POINT('Ctrl Pts',(-20.0438538007464,34.2025654617733,124.779381747442)) ;
#86977 = CARTESIAN_POINT('Ctrl Pts',(-19.7979948387222,34.212512854856,124.868199817644)) ;
#86978 = CARTESIAN_POINT('Ctrl Pts',(-19.5415398597008,34.2224230009024,124.913598266864)) ;
#86979 = CARTESIAN_POINT('Ctrl Pts',(-19.2772295562355,34.232481914752,124.913481740672)) ;
#86980 = CARTESIAN_POINT('Ctrl Pts',(-19.0224749494035,34.2423226850413,124.868818922004)) ;
#86981 = CARTESIAN_POINT('Ctrl Pts',(-18.7738170634932,34.2523855546199,124.778924498811)) ;
#86982 = CARTESIAN_POINT('Ctrl Pts',(-18.5484380725391,34.2622798777504,124.649212333765)) ;
#86983 = CARTESIAN_POINT('Ctrl Pts',(-18.3476405758638,34.2722216848449,124.482118201079)) ;
#86984 = CARTESIAN_POINT('Ctrl Pts',(-18.1777564580938,34.2822241958002,124.281491322928)) ;
#86985 = CARTESIAN_POINT('Ctrl Pts',(-18.0452449011872,34.2922589166186,124.053519923631)) ;
#86986 = CARTESIAN_POINT('Ctrl Pts',(-17.9556349074693,34.3021040941243,123.810796881849)) ;
#86987 = CARTESIAN_POINT('Ctrl Pts',(-17.9083784162444,34.3120888545254,123.552736052031)) ;
#86988 = CARTESIAN_POINT('Ctrl Pts',(-17.9065296697451,34.3220277608418,123.291519123483)) ;
#86989 = CARTESIAN_POINT('Ctrl Pts',(-17.9505964036269,34.3320699884775,123.031352463089)) ;
#86990 = CARTESIAN_POINT('Ctrl Pts',(-18.037624931531,34.3419552000619,122.786560063066)) ;
#86991 = CARTESIAN_POINT('Ctrl Pts',(-18.1669823934787,34.3519541302638,122.557890019545)) ;
#86992 = CARTESIAN_POINT('Ctrl Pts',(-18.3326161325234,34.3618715531743,122.356617211244)) ;
#86993 = CARTESIAN_POINT('Ctrl Pts',(-18.5332582552476,34.371919485253,122.185024436481)) ;
#86994 = CARTESIAN_POINT('Ctrl Pts',(-18.7567288565943,34.3817968610624,122.052891702144)) ;
#86995 = CARTESIAN_POINT('Ctrl Pts',(-19.0039582074564,34.3918507542303,121.959841830907)) ;
#86996 = CARTESIAN_POINT('Ctrl Pts',(-19.2595239194454,34.4017443774836,121.911772148145)) ;
#86997 = CARTESIAN_POINT('Ctrl Pts',(-19.5238983005659,34.4118069711066,121.908716657906)) ;
#86998 = CARTESIAN_POINT('Ctrl Pts',(-19.7791766052678,34.4216495450957,121.950552116811)) ;
#86999 = CARTESIAN_POINT('Ctrl Pts',(-20.0271336820024,34.4316403019786,122.036751836133)) ;
#87000 = CARTESIAN_POINT('Ctrl Pts',(-20.254936747224,34.4415683637365,122.163955290834)) ;
#87001 = CARTESIAN_POINT('Ctrl Pts',(-20.4586999823896,34.4515563396257,122.329419432095)) ;
#87002 = CARTESIAN_POINT('Ctrl Pts',(-20.6311135230344,34.4615920039821,122.528971921844)) ;
#87003 = CARTESIAN_POINT('Ctrl Pts',(-20.7641991432005,34.4714479424018,122.751184316972)) ;
#87004 = CARTESIAN_POINT('Ctrl Pts',(-20.8583766148853,34.4814434337987,122.996362053338)) ;
#87005 = CARTESIAN_POINT('Ctrl Pts',(-20.9082075537525,34.4913532387521,123.251982490847)) ;
#87006 = CARTESIAN_POINT('Ctrl Pts',(-20.9133731041675,34.5013654610189,123.515048494353)) ;
#87007 = CARTESIAN_POINT('Ctrl Pts',(-20.8722117287927,34.5113933417117,123.775338285339)) ;
#87008 = CARTESIAN_POINT('Ctrl Pts',(-20.7883656546394,34.5212497376943,124.020406248148)) ;
#87009 = CARTESIAN_POINT('Ctrl Pts',(-20.6615835386418,34.5312745348743,124.251337874107)) ;
#87010 = CARTESIAN_POINT('Ctrl Pts',(-20.4960213753757,34.5413054648581,124.456471359235)) ;
#87011 = CARTESIAN_POINT('Ctrl Pts',(-20.3013678063014,34.5511500673668,124.626861391942)) ;
#87012 = CARTESIAN_POINT('Ctrl Pts',(-20.0771540029309,34.5611409185909,124.763475181664)) ;
#87013 = CARTESIAN_POINT('Ctrl Pts',(-19.8312684979688,34.5711787516021,124.858978848205)) ;
#87014 = CARTESIAN_POINT('Ctrl Pts',(-19.577597721108,34.5810231400675,124.909794407279)) ;
#87015 = CARTESIAN_POINT('Ctrl Pts',(-19.3153254135936,34.5910079444371,124.916395570921)) ;
#87016 = CARTESIAN_POINT('Ctrl Pts',(-19.0569804860377,34.6009474639199,124.87763585839)) ;
#87017 = CARTESIAN_POINT('Ctrl Pts',(-18.806866607614,34.6109871949213,124.793729916711)) ;
#87018 = CARTESIAN_POINT('Ctrl Pts',(-18.5785256075441,34.6208753231676,124.669671687923)) ;
#87019 = CARTESIAN_POINT('Ctrl Pts',(-18.3728209709373,34.6308650483761,124.506586268412)) ;
#87020 = CARTESIAN_POINT('Ctrl Pts',(-18.1992525056931,34.6408228130776,124.31075898755)) ;
#87021 = CARTESIAN_POINT('Ctrl Pts',(-18.0625580666762,34.6507251544896,124.089319343284)) ;
#87022 = CARTESIAN_POINT('Ctrl Pts',(-17.9650433992383,34.660769350196,123.844056094203)) ;
#87023 = CARTESIAN_POINT('Ctrl Pts',(-17.9122901221407,34.6706767509553,123.589085907757)) ;
#87024 = CARTESIAN_POINT('Ctrl Pts',(-17.9040671219944,34.6806873508296,123.326142620746)) ;
#87025 = CARTESIAN_POINT('Ctrl Pts',(-17.942203265216,34.6907176467418,123.065322697016)) ;
#87026 = CARTESIAN_POINT('Ctrl Pts',(-18.0232493114111,34.7005724263915,122.819373677744)) ;
#87027 = CARTESIAN_POINT('Ctrl Pts',(-18.1463519672124,34.710529754609,122.588461269854)) ;
#87028 = CARTESIAN_POINT('Ctrl Pts',(-18.309353042108,34.7205687875159,122.381049743484)) ;
#87029 = CARTESIAN_POINT('Ctrl Pts',(-18.5023659383517,34.7304418994052,122.207599723295)) ;
#87030 = CARTESIAN_POINT('Ctrl Pts',(-18.7269874138073,34.7405151844323,122.06763353317)) ;
#87031 = CARTESIAN_POINT('Ctrl Pts',(-18.966311174259,34.7503355041691,121.970921603636)) ;
#87032 = CARTESIAN_POINT('Ctrl Pts',(-19.2252615250139,34.7604141695475,121.915607928114)) ;
#87033 = CARTESIAN_POINT('Ctrl Pts',(-19.4840428530472,34.7702657600313,121.906215757302)) ;
#87034 = CARTESIAN_POINT('Ctrl Pts',(-19.7462130095486,34.7803389103502,121.942457891797)) ;
#87035 = CARTESIAN_POINT('Ctrl Pts',(-19.9923964312408,34.7901812903253,122.021867293698)) ;
#87036 = CARTESIAN_POINT('Ctrl Pts',(-20.224633402004,34.8001622665683,122.143734711503)) ;
#87037 = CARTESIAN_POINT('Ctrl Pts',(-20.4326722972678,34.8101785949236,122.305014175264)) ;
#87038 = CARTESIAN_POINT('Ctrl Pts',(-20.6076836467507,34.8200763919147,122.497420427446)) ;
#87039 = CARTESIAN_POINT('Ctrl Pts',(-20.7486352078836,34.8300889486468,122.719624524635)) ;
#87040 = CARTESIAN_POINT('Ctrl Pts',(-20.8484693509522,34.8401209834933,122.963608083388)) ;
#87041 = CARTESIAN_POINT('Ctrl Pts',(-20.9039852822509,34.8499603843087,123.216169118791)) ;
#87042 = CARTESIAN_POINT('Ctrl Pts',(-20.915252015336,34.8600261699603,123.480416453755)) ;
#87043 = CARTESIAN_POINT('Ctrl Pts',(-20.8809428954112,34.8699166250749,123.738080890662)) ;
#87044 = CARTESIAN_POINT('Ctrl Pts',(-20.8021590268459,34.8799087437107,123.988551842107)) ;
#87045 = CARTESIAN_POINT('Ctrl Pts',(-20.6812162451853,34.8898715704737,124.220748500845)) ;
#87046 = CARTESIAN_POINT('Ctrl Pts',(-20.5232363311893,34.8997758537466,124.427621791333)) ;
#87047 = CARTESIAN_POINT('Ctrl Pts',(-20.328602748606,34.9098362876937,124.606497029424)) ;
#87048 = CARTESIAN_POINT('Ctrl Pts',(-20.1108581510111,34.9196768403669,124.746063981003)) ;
#87049 = CARTESIAN_POINT('Ctrl Pts',(-19.8670007279919,34.9297390603126,124.848234310547)) ;
#87050 = CARTESIAN_POINT('Ctrl Pts',(-19.6132374871759,34.9396361995912,124.9052994767)) ;
#87051 = CARTESIAN_POINT('Ctrl Pts',(-19.352586866818,34.9495673917262,124.918345206172)) ;
#87052 = CARTESIAN_POINT('Ctrl Pts',(-19.0907761598874,34.9596095463713,124.885281266899)) ;
#87053 = CARTESIAN_POINT('Ctrl Pts',(-18.8424935087745,34.9694963073906,124.808663455936)) ;
#87054 = CARTESIAN_POINT('Ctrl Pts',(-18.6085514013706,34.9794956091078,124.689074670539)) ;
#87055 = CARTESIAN_POINT('Ctrl Pts',(-18.4004100503073,34.9894164072746,124.532024155764)) ;
#87056 = CARTESIAN_POINT('Ctrl Pts',(-18.220695374879,34.9994504608713,124.339108184459)) ;
#87057 = CARTESIAN_POINT('Ctrl Pts',(-18.0786234259347,35.0093735784377,124.120391230864)) ;
#87058 = CARTESIAN_POINT('Ctrl Pts',(-17.9753990929057,35.0194297019368,123.877150159267)) ;
#87059 = CARTESIAN_POINT('Ctrl Pts',(-17.917104068257,35.0292751435917,123.62506345845)) ;
#87060 = CARTESIAN_POINT('Ctrl Pts',(-17.9024452588224,35.0392374447158,123.36369174523)) ;
#87061 = CARTESIAN_POINT('Ctrl Pts',(-17.933946461117,35.0492659239909,123.102025569632)) ;
#87062 = CARTESIAN_POINT('Ctrl Pts',(-18.0094085575674,35.0591762775006,122.852777323591)) ;
#87063 = CARTESIAN_POINT('Ctrl Pts',(-18.1266927602278,35.0691111496778,122.619516835167)) ;
#87064 = CARTESIAN_POINT('Ctrl Pts',(-18.2845521812503,35.0791522872635,122.408084929037)) ;
#87065 = CARTESIAN_POINT('Ctrl Pts',(-18.4736704054688,35.0890394364781,122.22989810543)) ;
#87066 = CARTESIAN_POINT('Ctrl Pts',(-18.6928945527343,35.0990316712291,122.085390254205)) ;
#87067 = CARTESIAN_POINT('Ctrl Pts',(-18.932889746988,35.1089803767921,121.9816540539)) ;
#87068 = CARTESIAN_POINT('Ctrl Pts',(-19.1868087710443,35.1189164452158,121.92087877605)) ;
#87069 = CARTESIAN_POINT('Ctrl Pts',(-19.4487510389459,35.1289021294316,121.904734357307)) ;
#87070 = CARTESIAN_POINT('Ctrl Pts',(-19.7108597155161,35.1389425560002,121.934890399688)) ;
#87071 = CARTESIAN_POINT('Ctrl Pts',(-19.9588218803458,35.148781669464,122.008182230702)) ;
#87072 = CARTESIAN_POINT('Ctrl Pts',(-20.195037968623,35.1588114036398,122.125114451366)) ;
#87073 = CARTESIAN_POINT('Ctrl Pts',(-20.4067898564085,35.1688335031457,122.281715086655)) ;
#87074 = CARTESIAN_POINT('Ctrl Pts',(-20.5858406931206,35.1787019430391,122.46934344386)) ;
#87075 = CARTESIAN_POINT('Ctrl Pts',(-20.7324825930465,35.1887708077248,122.689561854867)) ;
#87076 = CARTESIAN_POINT('Ctrl Pts',(-20.8362960938539,35.1986134808234,122.926479912635)) ;
#87077 = CARTESIAN_POINT('Ctrl Pts',(-20.899055079425,35.2085741149858,123.180594616481)) ;
#87078 = CARTESIAN_POINT('Ctrl Pts',(-20.9163568869125,35.2186120306639,123.44380305098)) ;
#87079 = CARTESIAN_POINT('Ctrl Pts',(-20.8886337721967,35.2284863055234,123.701836099716)) ;
#87080 = CARTESIAN_POINT('Ctrl Pts',(-20.815106074293,35.2385560558985,123.956001024207)) ;
#87081 = CARTESIAN_POINT('Ctrl Pts',(-20.701400325098,35.248389351273,124.188072701268)) ;
#87082 = CARTESIAN_POINT('Ctrl Pts',(-20.5466987675831,35.2584196487526,124.401475805769)) ;
#87083 = CARTESIAN_POINT('Ctrl Pts',(-20.3567063540923,35.2684517351941,124.584263100217)) ;
#87084 = CARTESIAN_POINT('Ctrl Pts',(-20.1426513521819,35.278279663683,124.72875221101)) ;
#87085 = CARTESIAN_POINT('Ctrl Pts',(-19.9030046171071,35.2882757047938,124.836324512499)) ;
#87086 = CARTESIAN_POINT('Ctrl Pts',(-19.6474276615906,35.298301516895,124.900352262788)) ;
#87087 = CARTESIAN_POINT('Ctrl Pts',(-19.3882751938659,35.3081887517898,124.919108279541)) ;
#87088 = CARTESIAN_POINT('Ctrl Pts',(-19.1274391236298,35.3181656180008,124.892776277121)) ;
#87089 = CARTESIAN_POINT('Ctrl Pts',(-18.8746646646945,35.3281585618726,124.821468377364)) ;
#87090 = CARTESIAN_POINT('Ctrl Pts',(-18.6372430900327,35.338196484544,124.706562893995)) ;
#87091 = CARTESIAN_POINT('Ctrl Pts',(-18.4271550056594,35.3480449488057,124.555385469111)) ;
#87092 = CARTESIAN_POINT('Ctrl Pts',(-18.2435829818069,35.3580368155497,124.367696236912)) ;
#87093 = CARTESIAN_POINT('Ctrl Pts',(-18.0963252747795,35.3679545475909,124.152615497661)) ;
#87094 = CARTESIAN_POINT('Ctrl Pts',(-17.9874096726993,35.3779827324862,123.912669454081)) ;
#87095 = CARTESIAN_POINT('Ctrl Pts',(-17.9226347534564,35.387867890535,123.66109622289)) ;
#87096 = CARTESIAN_POINT('Ctrl Pts',(-17.9016765666423,35.3978572510767,123.39941901094)) ;
#87097 = CARTESIAN_POINT('Ctrl Pts',(-17.9271558083283,35.4078984080111,123.136781335397)) ;
#87098 = CARTESIAN_POINT('Ctrl Pts',(-17.9959687525466,35.4177309914662,122.88772650032)) ;
#87099 = CARTESIAN_POINT('Ctrl Pts',(-18.1081319471754,35.4277252114282,122.650247800051)) ;
#87100 = CARTESIAN_POINT('Ctrl Pts',(-18.2607849253877,35.4377533132155,122.435427774985)) ;
#87101 = CARTESIAN_POINT('Ctrl Pts',(-18.4453853520115,35.4476332578386,122.252848690864)) ;
#87102 = CARTESIAN_POINT('Ctrl Pts',(-18.6610214269731,35.4576235843956,122.103123520847)) ;
#87103 = CARTESIAN_POINT('Ctrl Pts',(-18.8982196683709,35.4675645160499,121.993647605999)) ;
#87104 = CARTESIAN_POINT('Ctrl Pts',(-19.1519136468404,35.4775516345528,121.926344805637)) ;
#87105 = CARTESIAN_POINT('Ctrl Pts',(-19.4146479680384,35.48758496745,121.904428438846)) ;
#87106 = CARTESIAN_POINT('Ctrl Pts',(-19.6729148068661,35.4974510718947,121.927562236653)) ;
#87107 = CARTESIAN_POINT('Ctrl Pts',(-19.9282737618614,35.5075171857751,121.996483449793)) ;
#87108 = CARTESIAN_POINT('Ctrl Pts',(-20.1628377208178,35.5173731975435,122.106361679407)) ;
#87109 = CARTESIAN_POINT('Ctrl Pts',(-20.3781660934209,35.5273679011748,122.256744946492)) ;
#87110 = CARTESIAN_POINT('Ctrl Pts',(-20.5644031071723,35.5373992368997,122.443319308297)) ;
#87111 = CARTESIAN_POINT('Ctrl Pts',(-20.7132753997824,35.5472657621033,122.655613795221)) ;
#87112 = CARTESIAN_POINT('Ctrl Pts',(-20.824735991116,35.5572531901491,122.893195278124)) ;
#87113 = CARTESIAN_POINT('Ctrl Pts',(-20.8931143715501,35.5671981198355,123.145473611636)) ;
#87114 = CARTESIAN_POINT('Ctrl Pts',(-20.916731989703,35.5772430379441,123.408359549251)) ;
#87115 = CARTESIAN_POINT('Ctrl Pts',(-20.8949804435051,35.587105007558,123.66662867698)) ;
#87116 = CARTESIAN_POINT('Ctrl Pts',(-20.8283478671713,35.5970970755792,123.920587710675)) ;
#87117 = CARTESIAN_POINT('Ctrl Pts',(-20.719243324381,35.6070280009538,124.157679141684)) ;
#87118 = CARTESIAN_POINT('Ctrl Pts',(-20.5707147508326,35.6169786291772,124.372871095378)) ;
#87119 = CARTESIAN_POINT('Ctrl Pts',(-20.3862369565019,35.6269788682363,124.560073078809)) ;
#87120 = CARTESIAN_POINT('Ctrl Pts',(-20.1712640574126,35.6370073236055,124.712497104667)) ;
#87121 = CARTESIAN_POINT('Ctrl Pts',(-19.9370958263856,35.6468733581888,124.823815964018)) ;
#87122 = CARTESIAN_POINT('Ctrl Pts',(-19.6841078343026,35.6568656799362,124.894073754451)) ;
#87123 = CARTESIAN_POINT('Ctrl Pts',(-19.4242931282444,35.6667979696132,124.919232541197)) ;
#87124 = CARTESIAN_POINT('Ctrl Pts',(-19.1622457507477,35.676799614584,124.89901214049)) ;
#87125 = CARTESIAN_POINT('Ctrl Pts',(-18.8234350299955,35.690112248,124.811793581749)) ;
#87126 = CARTESIAN_POINT('Ctrl Pts',(-18.5168964604078,35.7033439973816,124.639445590766)) ;
#87127 = CARTESIAN_POINT('Ctrl Pts',(-18.2664225908945,35.7166672621986,124.394805388771)) ;
#87128 = CARTESIAN_POINT('Ctrl Pts',(-18.1147450135693,35.7265429684163,124.184207203932)) ;
#87129 = CARTESIAN_POINT('Ctrl Pts',(-18.0003454842561,35.7365325595163,123.947960343234)) ;
#87130 = CARTESIAN_POINT('Ctrl Pts',(-17.9289701667244,35.7464596559717,123.697008534527)) ;
#87131 = CARTESIAN_POINT('Ctrl Pts',(-17.9019627690378,35.7564848044763,123.434969684401)) ;
#87132 = CARTESIAN_POINT('Ctrl Pts',(-17.9204625057985,35.766380458623,123.175558526549)) ;
#87133 = CARTESIAN_POINT('Ctrl Pts',(-17.9840399510721,35.7763839930012,122.920505986074)) ;
#87134 = CARTESIAN_POINT('Ctrl Pts',(-18.0907912526402,35.7863691314413,122.680759611974)) ;
#87135 = CARTESIAN_POINT('Ctrl Pts',(-18.2384845563749,35.7964050560366,122.462276828214)) ;
#87136 = CARTESIAN_POINT('Ctrl Pts',(-18.4182832581623,35.8062563314643,122.276022071899)) ;
#87137 = CARTESIAN_POINT('Ctrl Pts',(-18.6302545916797,35.8162485926257,122.121024656498)) ;
#87138 = CARTESIAN_POINT('Ctrl Pts',(-18.8673155093982,35.8262884766433,122.005244450248)) ;
#87139 = CARTESIAN_POINT('Ctrl Pts',(-19.1155599860478,35.8361232511457,121.93323039927)) ;
#87140 = CARTESIAN_POINT('Ctrl Pts',(-19.3787662820051,35.846199632166,121.90464170685)) ;
#87141 = CARTESIAN_POINT('Ctrl Pts',(-19.6369856027935,35.8560459053166,121.921721200336)) ;
#87142 = CARTESIAN_POINT('Ctrl Pts',(-19.9782318745606,35.8694104266019,122.004755386422)) ;
#87143 = CARTESIAN_POINT('Ctrl Pts',(-20.2860781894191,35.8826166710363,122.173358222392)) ;
#87144 = CARTESIAN_POINT('Ctrl Pts',(-20.5388194305417,35.8958816257135,122.413415383819)) ;
#87145 = CARTESIAN_POINT('Ctrl Pts',(-20.6954518663001,35.9059139062652,122.625487616004)) ;
#87146 = CARTESIAN_POINT('Ctrl Pts',(-20.8114494728934,35.9158226397831,122.858608403369)) ;
#87147 = CARTESIAN_POINT('Ctrl Pts',(-20.8860782708486,35.9257601906506,123.108875396054)) ;
#87148 = CARTESIAN_POINT('Ctrl Pts',(-20.9161752733181,35.9357900382445,123.370700554843)) ;
#87149 = CARTESIAN_POINT('Ctrl Pts',(-20.8957731929268,35.949025178165,123.717991080168)) ;
#87150 = CARTESIAN_POINT('Ctrl Pts',(-20.7562782646861,35.9656936425361,124.138331425498)) ;
#87151 = CARTESIAN_POINT('Ctrl Pts',(-20.4290918169683,35.98556465441,124.553143935095)) ;
#87152 = CARTESIAN_POINT('Ctrl Pts',(-20.0516669376428,36.002271738793,124.786848654509)) ;
#87153 = CARTESIAN_POINT('Ctrl Pts',(-19.7200488034031,36.0154490201036,124.886772678737)) ;
#87154 = CARTESIAN_POINT('Ctrl Pts',(-19.3739896601812,36.0287164806177,124.929104605177)) ;
#87155 = CARTESIAN_POINT('Ctrl Pts',(-18.9367256618785,36.0453303713049,124.867571649377)) ;
#87156 = CARTESIAN_POINT('Ctrl Pts',(-18.4683585867537,36.0652791707323,124.618963683723)) ;
#87157 = CARTESIAN_POINT('Ctrl Pts',(-18.1135879764182,36.0852002822632,124.2260271695)) ;
#87158 = CARTESIAN_POINT('Ctrl Pts',(-17.9136719684102,36.1050667304361,123.737230065052)) ;
#87159 = CARTESIAN_POINT('Ctrl Pts',(-17.8927126209991,36.1250930770532,123.205433374261)) ;
#87160 = CARTESIAN_POINT('Ctrl Pts',(-18.0533007215964,36.1449551214427,122.702455916173)) ;
#87161 = CARTESIAN_POINT('Ctrl Pts',(-18.3764776353452,36.1649004241238,122.282339628229)) ;
#87162 = CARTESIAN_POINT('Ctrl Pts',(-18.8226158877263,36.1847957311827,121.998462474444)) ;
#87163 = CARTESIAN_POINT('Ctrl Pts',(-19.3385842783177,36.2046890013503,121.882951679264)) ;
#87164 = CARTESIAN_POINT('Ctrl Pts',(-19.8648495105545,36.2246545940308,121.950798037064)) ;
#87165 = CARTESIAN_POINT('Ctrl Pts',(-20.334465653922,36.2445299177156,122.192756268591)) ;
#87166 = CARTESIAN_POINT('Ctrl Pts',(-20.6955169132806,36.2645049802905,122.582020760569)) ;
#87167 = CARTESIAN_POINT('Ctrl Pts',(-20.9010738348726,36.2844573899217,123.070861900805)) ;
#87168 = CARTESIAN_POINT('Ctrl Pts',(-20.9283436001929,36.3042934441578,123.597363126459)) ;
#87169 = CARTESIAN_POINT('Ctrl Pts',(-20.7737705212242,36.3242713555753,124.10534582472)) ;
#87170 = CARTESIAN_POINT('Ctrl Pts',(-20.4556033727974,36.3441894050788,124.528410951894)) ;
#87171 = CARTESIAN_POINT('Ctrl Pts',(-20.0139153720363,36.3640575488469,124.818025234808)) ;
#87172 = CARTESIAN_POINT('Ctrl Pts',(-19.4952301669597,36.3841084054342,124.939796977761)) ;
#87173 = CARTESIAN_POINT('Ctrl Pts',(-18.9729215440468,36.4038888418901,124.878628473693)) ;
#87174 = CARTESIAN_POINT('Ctrl Pts',(-18.4967651240595,36.4239188975679,124.640802577976)) ;
#87175 = CARTESIAN_POINT('Ctrl Pts',(-18.1335848516454,36.4438000027427,124.25686352696)) ;
#87176 = CARTESIAN_POINT('Ctrl Pts',(-17.9219195474901,36.4636804651105,123.77277946085)) ;
#87177 = CARTESIAN_POINT('Ctrl Pts',(-17.8881151233781,36.4836656122549,123.242666380459)) ;
#87178 = CARTESIAN_POINT('Ctrl Pts',(-18.0366553794252,36.5035561907912,122.73529278596)) ;
#87179 = CARTESIAN_POINT('Ctrl Pts',(-18.3487072158258,36.5234502106656,122.308453160384)) ;
#87180 = CARTESIAN_POINT('Ctrl Pts',(-18.7881486981132,36.543371655392,122.013243316393)) ;
#87181 = CARTESIAN_POINT('Ctrl Pts',(-19.3013483876729,36.5632697934474,121.884892286894)) ;
#87182 = CARTESIAN_POINT('Ctrl Pts',(-19.8317595038524,36.5833405486635,121.940839429391)) ;
#87183 = CARTESIAN_POINT('Ctrl Pts',(-20.3047244450388,36.6031260987147,122.170976388332)) ;
#87184 = CARTESIAN_POINT('Ctrl Pts',(-20.6751961018729,36.6231091735921,122.551414789717)) ;
#87185 = CARTESIAN_POINT('Ctrl Pts',(-20.8920876251874,36.643018256238,123.034079238211)) ;
#87186 = CARTESIAN_POINT('Ctrl Pts',(-20.9326736949197,36.6628768153608,123.560393777446)) ;
#87187 = CARTESIAN_POINT('Ctrl Pts',(-20.7893507745121,36.6829202591995,124.073361851782)) ;
#87188 = CARTESIAN_POINT('Ctrl Pts',(-20.5344135959182,36.6994203239287,124.430349947457)) ;
#87189 = CARTESIAN_POINT('Ctrl Pts',(-20.2630412458369,36.7128100637776,124.654248532504)) ;
#87190 = CARTESIAN_POINT('Ctrl Pts',(-20.0376657911243,36.722666964986,124.781998493706)) ;
#87191 = CARTESIAN_POINT('Ctrl Pts',(-19.790451891043,36.7326584908325,124.870339079412)) ;
#87192 = CARTESIAN_POINT('Ctrl Pts',(-19.5333205208731,36.7425831712835,124.914226210988)) ;
#87193 = CARTESIAN_POINT('Ctrl Pts',(-19.2702961550599,36.7525937613279,124.912889798325)) ;
#87194 = CARTESIAN_POINT('Ctrl Pts',(-18.9272992756477,36.7658530220315,124.851022900053)) ;
#87195 = CARTESIAN_POINT('Ctrl Pts',(-18.6064416437255,36.7792040971818,124.699737523157)) ;
#87196 = CARTESIAN_POINT('Ctrl Pts',(-18.3413179144251,36.7924104064166,124.475682143339)) ;
#87197 = CARTESIAN_POINT('Ctrl Pts',(-18.1729500479038,36.8023972400069,124.274423037726)) ;
#87198 = CARTESIAN_POINT('Ctrl Pts',(-18.0423739740692,36.812349967503,124.047750299169)) ;
#87199 = CARTESIAN_POINT('Ctrl Pts',(-17.952518013425,36.8223980643446,123.799486638763)) ;
#87200 = CARTESIAN_POINT('Ctrl Pts',(-17.907757267272,36.8322395212164,123.544740945739)) ;
#87201 = CARTESIAN_POINT('Ctrl Pts',(-17.9073502062391,36.8422257881299,123.282355578864)) ;
#87202 = CARTESIAN_POINT('Ctrl Pts',(-17.9521694205823,36.8521623890303,123.025063136411)) ;
#87203 = CARTESIAN_POINT('Ctrl Pts',(-18.0420963058471,36.8622123318174,122.776771029239)) ;
#87204 = CARTESIAN_POINT('Ctrl Pts',(-18.1710052785227,36.8720625315031,122.552279193621)) ;
#87205 = CARTESIAN_POINT('Ctrl Pts',(-18.3384408575299,36.8820354364352,122.350698607091)) ;
#87206 = CARTESIAN_POINT('Ctrl Pts',(-18.5389463808558,36.8920338109148,122.18084427361)) ;
#87207 = CARTESIAN_POINT('Ctrl Pts',(-18.7664541058527,36.9020539847848,122.048279786072)) ;
#87208 = CARTESIAN_POINT('Ctrl Pts',(-19.0105222002321,36.9119550287268,121.95809778858)) ;
#87209 = CARTESIAN_POINT('Ctrl Pts',(-19.268728383313,36.9219438324511,121.910847088745)) ;
#87210 = CARTESIAN_POINT('Ctrl Pts',(-19.5305939085291,36.9319092992829,121.909337770446)) ;
#87211 = CARTESIAN_POINT('Ctrl Pts',(-19.7872824216961,36.9418128615559,121.95243202349)) ;
#87212 = CARTESIAN_POINT('Ctrl Pts',(-20.0363517848326,36.9518735394339,122.041006819332)) ;
#87213 = CARTESIAN_POINT('Ctrl Pts',(-20.2614482794892,36.9617138373834,122.1683698474)) ;
#87214 = CARTESIAN_POINT('Ctrl Pts',(-20.4656746860891,36.9717768322928,122.336311677907)) ;
#87215 = CARTESIAN_POINT('Ctrl Pts',(-20.6346325844978,36.9816711264399,122.533982970242)) ;
#87216 = CARTESIAN_POINT('Ctrl Pts',(-20.7679155889213,36.9916129241368,122.758650934849)) ;
#87217 = CARTESIAN_POINT('Ctrl Pts',(-20.8608421966797,37.0016155016659,123.004571300072)) ;
#87218 = CARTESIAN_POINT('Ctrl Pts',(-20.9094048501918,37.011649965587,123.26374268831)) ;
#87219 = CARTESIAN_POINT('Ctrl Pts',(-20.9125815920894,37.0214961041081,123.522477689503)) ;
#87220 = CARTESIAN_POINT('Ctrl Pts',(-20.8707936127288,37.0314772773451,123.781401079755)) ;
#87221 = CARTESIAN_POINT('Ctrl Pts',(-20.7848638119868,37.0414295713023,124.028425816195)) ;
#87222 = CARTESIAN_POINT('Ctrl Pts',(-20.6570438981956,37.0514283664369,124.258022088148)) ;
#87223 = CARTESIAN_POINT('Ctrl Pts',(-20.4902612991329,37.0614674746977,124.462411340172)) ;
#87224 = CARTESIAN_POINT('Ctrl Pts',(-20.2951235539568,37.0712924161369,124.631500866346)) ;
#87225 = CARTESIAN_POINT('Ctrl Pts',(-20.0686616200432,37.0813471032113,124.767597084672)) ;
#87226 = CARTESIAN_POINT('Ctrl Pts',(-19.8245710827869,37.0912899081514,124.860842297865)) ;
#87227 = CARTESIAN_POINT('Ctrl Pts',(-19.5691588004271,37.1011936941479,124.910878499083)) ;
#87228 = CARTESIAN_POINT('Ctrl Pts',(-19.3052063233042,37.1112405107127,124.915717087351)) ;
#87229 = CARTESIAN_POINT('Ctrl Pts',(-19.0482495106725,37.1211360301914,124.875491392646)) ;
#87230 = CARTESIAN_POINT('Ctrl Pts',(-18.7981148297119,37.1311981155158,124.789869782215)) ;
#87231 = CARTESIAN_POINT('Ctrl Pts',(-18.5715632075335,37.1410408264737,124.664999559399)) ;
#87232 = CARTESIAN_POINT('Ctrl Pts',(-18.3667645398744,37.1510315437798,124.500772902301)) ;
#87233 = CARTESIAN_POINT('Ctrl Pts',(-18.1946815226206,37.1609596268764,124.304654257152)) ;
#87234 = CARTESIAN_POINT('Ctrl Pts',(-18.0580587042926,37.1709475569881,124.080530224495)) ;
#87235 = CARTESIAN_POINT('Ctrl Pts',(-17.9623882859192,37.1809833831154,123.834772735687)) ;
#87236 = CARTESIAN_POINT('Ctrl Pts',(-17.9113591892937,37.190838720229,123.580846703996)) ;
#87237 = CARTESIAN_POINT('Ctrl Pts',(-17.9046918793828,37.2008364550792,123.318229679078)) ;
#87238 = CARTESIAN_POINT('Ctrl Pts',(-17.9432929783789,37.2107443590637,123.060725439739)) ;
#87239 = CARTESIAN_POINT('Ctrl Pts',(-18.0264609446868,37.2207554336121,122.811128639324)) ;
#87240 = CARTESIAN_POINT('Ctrl Pts',(-18.1523845768401,37.2307832891477,122.579637946315)) ;
#87241 = CARTESIAN_POINT('Ctrl Pts',(-18.313434602913,37.240640883053,122.376742009224)) ;
#87242 = CARTESIAN_POINT('Ctrl Pts',(-18.510241481172,37.2506675698911,122.201537057415)) ;
#87243 = CARTESIAN_POINT('Ctrl Pts',(-18.7348729634303,37.2606962390448,122.063695449204)) ;
#87244 = CARTESIAN_POINT('Ctrl Pts',(-18.9753445770678,37.2705414473262,121.96828080011)) ;
#87245 = CARTESIAN_POINT('Ctrl Pts',(-19.2323500330995,37.2805321362893,121.914602131553)) ;
#87246 = CARTESIAN_POINT('Ctrl Pts',(-19.4960202224024,37.2905700125716,121.9069126897)) ;
#87247 = CARTESIAN_POINT('Ctrl Pts',(-19.7520669609929,37.3004143902138,121.943940420464)) ;
#87248 = CARTESIAN_POINT('Ctrl Pts',(-20.0014193408441,37.3103991946052,122.025510816322)) ;
#87249 = CARTESIAN_POINT('Ctrl Pts',(-20.2318871717339,37.3203387248238,122.148511202845)) ;
#87250 = CARTESIAN_POINT('Ctrl Pts',(-20.4394866075736,37.3303784128607,122.311296862849)) ;
#87251 = CARTESIAN_POINT('Ctrl Pts',(-20.6131300585679,37.340266702229,122.504635758308)) ;
#87252 = CARTESIAN_POINT('Ctrl Pts',(-20.7523750420527,37.3502558259138,122.727153728378)) ;
#87253 = CARTESIAN_POINT('Ctrl Pts',(-20.8503938939143,37.3602158355884,122.969841158144)) ;
#87254 = CARTESIAN_POINT('Ctrl Pts',(-20.9050687368293,37.3701162652927,123.224212899945)) ;
#87255 = CARTESIAN_POINT('Ctrl Pts',(-20.9148721088486,37.3801593466994,123.487941036205)) ;
#87256 = CARTESIAN_POINT('Ctrl Pts',(-20.8792246033343,37.390066740607,123.745859387518)) ;
#87257 = CARTESIAN_POINT('Ctrl Pts',(-20.7989609173973,37.4000784715962,123.996417274373)) ;
#87258 = CARTESIAN_POINT('Ctrl Pts',(-20.6756955451906,37.410110689311,124.22947112403)) ;
#87259 = CARTESIAN_POINT('Ctrl Pts',(-20.51702591384,37.4199631985572,124.434050623572)) ;
#87260 = CARTESIAN_POINT('Ctrl Pts',(-20.3237233572184,37.4299211351002,124.610450271903)) ;
#87261 = CARTESIAN_POINT('Ctrl Pts',(-20.1007000293467,37.4399600051085,124.751331487019)) ;
#87262 = CARTESIAN_POINT('Ctrl Pts',(-19.8607616035958,37.4498331602667,124.850169231509)) ;
#87263 = CARTESIAN_POINT('Ctrl Pts',(-19.602246757542,37.4599064351164,124.906872980276)) ;
#87264 = CARTESIAN_POINT('Ctrl Pts',(-19.3443562287078,37.4697267522938,124.917896850224)) ;
#87265 = CARTESIAN_POINT('Ctrl Pts',(-19.0818283552624,37.4798054380873,124.883340221226)) ;
#87266 = CARTESIAN_POINT('Ctrl Pts',(-18.8348322832029,37.4896569494704,124.805570098911)) ;
#87267 = CARTESIAN_POINT('Ctrl Pts',(-18.599913832951,37.499730395777,124.683655014206)) ;
#87268 = CARTESIAN_POINT('Ctrl Pts',(-18.3945253990698,37.5095716709017,124.526446904205)) ;
#87269 = CARTESIAN_POINT('Ctrl Pts',(-18.2164310699433,37.5195567705585,124.333775949038)) ;
#87270 = CARTESIAN_POINT('Ctrl Pts',(-18.0744621012236,37.5295642466928,124.11237858257)) ;
#87271 = CARTESIAN_POINT('Ctrl Pts',(-17.9737434063258,37.5394868344017,123.871874033015)) ;
#87272 = CARTESIAN_POINT('Ctrl Pts',(-17.9155198712875,37.5494734386751,123.615951736417)) ;
#87273 = CARTESIAN_POINT('Ctrl Pts',(-17.9030442398782,37.5595135670092,123.352424180443)) ;
#87274 = CARTESIAN_POINT('Ctrl Pts',(-17.9352929472443,37.5693530015426,123.095845830502)) ;
#87275 = CARTESIAN_POINT('Ctrl Pts',(-18.0131166461626,37.5794170560336,122.843116592569)) ;
#87276 = CARTESIAN_POINT('Ctrl Pts',(-18.1316981730949,37.5893079752708,122.611787994209)) ;
#87277 = CARTESIAN_POINT('Ctrl Pts',(-18.2897770295622,37.5992999685768,122.402140602484)) ;
#87278 = CARTESIAN_POINT('Ctrl Pts',(-18.4814669497025,37.6092628325361,122.223821161659)) ;
#87279 = CARTESIAN_POINT('Ctrl Pts',(-18.6995802858491,37.6191670923539,122.081762570876)) ;
#87280 = CARTESIAN_POINT('Ctrl Pts',(-18.9428624159537,37.6292275829253,121.978356993375)) ;
#87281 = CARTESIAN_POINT('Ctrl Pts',(-19.1947597030667,37.6390679325563,121.919723653256)) ;
#87282 = CARTESIAN_POINT('Ctrl Pts',(-19.4587639337918,37.6491309080463,121.905087450184)) ;
#87283 = CARTESIAN_POINT('Ctrl Pts',(-19.7169360685854,37.6590252281897,121.936206707452)) ;
#87284 = CARTESIAN_POINT('Ctrl Pts',(-19.9671186320429,37.6689669413213,122.011348625595)) ;
#87285 = CARTESIAN_POINT('Ctrl Pts',(-20.2020080675906,37.6789698311154,122.129443636696)) ;
#87286 = CARTESIAN_POINT('Ctrl Pts',(-20.4132615576,37.6890096882759,122.287457794107)) ;
#87287 = CARTESIAN_POINT('Ctrl Pts',(-20.5904502427968,37.6988338691135,122.475251891521)) ;
#87288 = CARTESIAN_POINT('Ctrl Pts',(-20.735982916264,37.7088908426167,122.69583339334)) ;
#87289 = CARTESIAN_POINT('Ctrl Pts',(-20.8393694687883,37.7188189668038,122.93539179218)) ;
#87290 = CARTESIAN_POINT('Ctrl Pts',(-20.9004226762574,37.7287726618772,123.18974167518)) ;
#87291 = CARTESIAN_POINT('Ctrl Pts',(-20.9161571182402,37.7388188554525,123.453273135493)) ;
#87292 = CARTESIAN_POINT('Ctrl Pts',(-20.8867385875313,37.7486669578124,123.710392738064)) ;
#87293 = CARTESIAN_POINT('Ctrl Pts',(-20.8130541065125,37.75862854604,123.96157704454)) ;
#87294 = CARTESIAN_POINT('Ctrl Pts',(-20.6957843077402,37.7686572161963,124.197608569847)) ;
#87295 = CARTESIAN_POINT('Ctrl Pts',(-20.5412434271641,37.778567519078,124.407217781717)) ;
#87296 = CARTESIAN_POINT('Ctrl Pts',(-20.352645450369,37.7885024028859,124.58776383537)) ;
#87297 = CARTESIAN_POINT('Ctrl Pts',(-20.133119143806,37.7985435445765,124.734158279139)) ;
#87298 = CARTESIAN_POINT('Ctrl Pts',(-19.895266526059,37.8084306657405,124.838762309883)) ;
#87299 = CARTESIAN_POINT('Ctrl Pts',(-19.6403142341081,37.818423008589,124.901552440905)) ;
#87300 = CARTESIAN_POINT('Ctrl Pts',(-19.3794511200074,37.828371309813,124.918971337681)) ;
#87301 = CARTESIAN_POINT('Ctrl Pts',(-19.1197938910939,37.8383088874951,124.891242488897)) ;
#87302 = CARTESIAN_POINT('Ctrl Pts',(-18.8675519902502,37.8482954619457,124.818740589761)) ;
#87303 = CARTESIAN_POINT('Ctrl Pts',(-18.6308845594972,37.8583242718541,124.702791487369)) ;
#87304 = CARTESIAN_POINT('Ctrl Pts',(-18.4209911500482,37.8682025931609,124.550044711612)) ;
#87305 = CARTESIAN_POINT('Ctrl Pts',(-18.2382893834789,37.8781942405083,124.361450555223)) ;
#87306 = CARTESIAN_POINT('Ctrl Pts',(-18.0909361216224,37.8882287639461,124.142780458619)) ;
#87307 = CARTESIAN_POINT('Ctrl Pts',(-17.9851082426078,37.8980921208247,123.90613973582)) ;
#87308 = CARTESIAN_POINT('Ctrl Pts',(-17.9206158973704,37.908162347505,123.649512993499)) ;
#87309 = CARTESIAN_POINT('Ctrl Pts',(-17.9021014477694,37.9180046556397,123.391519278401)) ;
#87310 = CARTESIAN_POINT('Ctrl Pts',(-17.9280213893312,37.9279653876631,123.131054268142)) ;
#87311 = CARTESIAN_POINT('Ctrl Pts',(-17.9998223639555,37.9380032768612,122.877238454483)) ;
#87312 = CARTESIAN_POINT('Ctrl Pts',(-18.1123180047447,37.94787755978,122.643370168163)) ;
#87313 = CARTESIAN_POINT('Ctrl Pts',(-18.2666811956989,37.9579473043975,122.428479079685)) ;
#87314 = CARTESIAN_POINT('Ctrl Pts',(-18.4515097019627,37.9677806147431,122.247856374346)) ;
#87315 = CARTESIAN_POINT('Ctrl Pts',(-18.6687188341038,37.9778108580958,122.098544975013)) ;
#87316 = CARTESIAN_POINT('Ctrl Pts',(-18.9089398495734,37.9878431460742,121.989907265577)) ;
#87317 = CARTESIAN_POINT('Ctrl Pts',(-19.1589973603507,37.9976703225423,121.925371796745)) ;
#87318 = CARTESIAN_POINT('Ctrl Pts',(-19.4210528476622,38.0076757054092,121.904329796489)) ;
#87319 = CARTESIAN_POINT('Ctrl Pts',(-19.6822603276462,38.0176583444019,121.929146579502)) ;
#87320 = CARTESIAN_POINT('Ctrl Pts',(-19.9365866650456,38.0277024115385,121.999661380241)) ;
#87321 = CARTESIAN_POINT('Ctrl Pts',(-20.1697455284941,38.0375236303425,122.110354265076)) ;
#87322 = CARTESIAN_POINT('Ctrl Pts',(-20.3851407356152,38.0475604692805,122.262573522578)) ;
#87323 = CARTESIAN_POINT('Ctrl Pts',(-20.5700791380799,38.0575848813783,122.450185779491)) ;
#87324 = CARTESIAN_POINT('Ctrl Pts',(-20.7175310391498,38.0674369657836,122.663002255422)) ;
#87325 = CARTESIAN_POINT('Ctrl Pts',(-20.8276645507075,38.0774278625268,122.901301885871)) ;
#87326 = CARTESIAN_POINT('Ctrl Pts',(-20.8944393360025,38.0873458544277,123.153269837169)) ;
#87327 = CARTESIAN_POINT('Ctrl Pts',(-20.916752709306,38.0973739698847,123.415831037644)) ;
#87328 = CARTESIAN_POINT('Ctrl Pts',(-20.89358187262,38.1072591458268,123.674574253975)) ;
#87329 = CARTESIAN_POINT('Ctrl Pts',(-20.8257391871181,38.1172485042337,123.928171654191)) ;
#87330 = CARTESIAN_POINT('Ctrl Pts',(-20.7138167717013,38.127289651814,124.167129479311)) ;
#87331 = CARTESIAN_POINT('Ctrl Pts',(-20.5656061454427,38.1371222748204,124.378785103182)) ;
#87332 = CARTESIAN_POINT('Ctrl Pts',(-20.3804240799344,38.1471163459312,124.565013167833)) ;
#87333 = CARTESIAN_POINT('Ctrl Pts',(-20.1646606886898,38.1571450035721,124.716368185705)) ;
#87334 = CARTESIAN_POINT('Ctrl Pts',(-19.9294754177371,38.1670293297649,124.826601817947)) ;
#87335 = CARTESIAN_POINT('Ctrl Pts',(-19.6768051124309,38.1769950732555,124.89551183432)) ;
#87336 = CARTESIAN_POINT('Ctrl Pts',(-19.4143545698229,38.1870234523867,124.919272831667)) ;
#87337 = CARTESIAN_POINT('Ctrl Pts',(-19.155026247405,38.1969242985936,124.897774472843)) ;
#87338 = CARTESIAN_POINT('Ctrl Pts',(-18.899449911136,38.2069829560107,124.830469885562)) ;
#87339 = CARTESIAN_POINT('Ctrl Pts',(-18.6640472589483,38.2168405187926,124.72223521876)) ;
#87340 = CARTESIAN_POINT('Ctrl Pts',(-18.4464297173287,38.2269089213458,124.571809104608)) ;
#87341 = CARTESIAN_POINT('Ctrl Pts',(-18.262192640318,38.2367643200854,124.389754401548)) ;
#87342 = CARTESIAN_POINT('Ctrl Pts',(-18.1096196037123,38.2467591871593,124.175968694404)) ;
#87343 = CARTESIAN_POINT('Ctrl Pts',(-17.9965795627306,38.2567904821428,123.937817735641)) ;
#87344 = CARTESIAN_POINT('Ctrl Pts',(-17.9273563602029,38.2666570068693,123.687937654047)) ;
#87345 = CARTESIAN_POINT('Ctrl Pts',(-17.9018527032758,38.276644477565,123.426751350671)) ;
#87346 = CARTESIAN_POINT('Ctrl Pts',(-17.9218607437343,38.2865892371289,123.166140198543)) ;
#87347 = CARTESIAN_POINT('Ctrl Pts',(-17.9876155290226,38.2966347930777,122.910504235427)) ;
#87348 = CARTESIAN_POINT('Ctrl Pts',(-18.0945121468168,38.3064943814529,122.674449960714)) ;
#87349 = CARTESIAN_POINT('Ctrl Pts',(-18.2424996480843,38.3164953365889,122.457313423853)) ;
#87350 = CARTESIAN_POINT('Ctrl Pts',(-18.4240798301571,38.3263995638665,122.270788969546)) ;
#87351 = CARTESIAN_POINT('Ctrl Pts',(-18.6381236155899,38.3364416407616,122.116493175448)) ;
#87352 = CARTESIAN_POINT('Ctrl Pts',(-18.8725441547087,38.3463492534478,122.003091772094)) ;
#87353 = CARTESIAN_POINT('Ctrl Pts',(-19.1267212481479,38.3564037840635,121.931068647469)) ;
#87354 = CARTESIAN_POINT('Ctrl Pts',(-19.3845339848272,38.3662645706124,121.904631230091)) ;
#87355 = CARTESIAN_POINT('Ctrl Pts',(-19.6464652984615,38.3762583256834,121.92312229318)) ;
#87356 = CARTESIAN_POINT('Ctrl Pts',(-19.8995750129763,38.3861836859234,121.986273003471)) ;
#87357 = CARTESIAN_POINT('Ctrl Pts',(-20.140272020409,38.3962116153187,122.093470120755)) ;
#87358 = CARTESIAN_POINT('Ctrl Pts',(-20.3558252995868,38.406097882118,122.238568442777)) ;
#87359 = CARTESIAN_POINT('Ctrl Pts',(-20.5456984409777,38.4161296510163,122.42138753169)) ;
#87360 = CARTESIAN_POINT('Ctrl Pts',(-20.698877922451,38.4260112468599,122.631132419724)) ;
#87361 = CARTESIAN_POINT('Ctrl Pts',(-20.8154213762224,38.4360731323278,122.8684346522)) ;
#87362 = CARTESIAN_POINT('Ctrl Pts',(-20.8875986677405,38.4459305663467,123.117253823727)) ;
#87363 = CARTESIAN_POINT('Ctrl Pts',(-20.9164045121782,38.4559238093887,123.378246907377)) ;
#87364 = CARTESIAN_POINT('Ctrl Pts',(-20.8995775457113,38.465854570275,123.638690081529)) ;
#87365 = CARTESIAN_POINT('Ctrl Pts',(-20.816850334482,38.4792035624722,123.979625573362)) ;
#87366 = CARTESIAN_POINT('Ctrl Pts',(-20.6476612787041,38.4924719352886,124.289010646964)) ;
#87367 = CARTESIAN_POINT('Ctrl Pts',(-20.4070708455003,38.505754876673,124.541958141041)) ;
#87368 = CARTESIAN_POINT('Ctrl Pts',(-20.1946437063502,38.5157976625152,124.698532719528)) ;
#87369 = CARTESIAN_POINT('Ctrl Pts',(-19.9628978193437,38.5256476050673,124.813858968729)) ;
#87370 = CARTESIAN_POINT('Ctrl Pts',(-19.7111423066587,38.5356448379863,124.888916493239)) ;
#87371 = CARTESIAN_POINT('Ctrl Pts',(-19.4496444734046,38.5456597333208,124.918770576671)) ;
#87372 = CARTESIAN_POINT('Ctrl Pts',(-19.102347554309,38.558899409959,124.897958325602)) ;
#87373 = CARTESIAN_POINT('Ctrl Pts',(-18.6847987628518,38.5754466343643,124.759928991449)) ;
#87374 = CARTESIAN_POINT('Ctrl Pts',(-18.3371659709119,38.5920940714954,124.486215378783)) ;
#87375 = CARTESIAN_POINT('Ctrl Pts',(-18.1282833266673,38.6053835689736,124.206304846633)) ;
#87376 = CARTESIAN_POINT('Ctrl Pts',(-18.0108766480719,38.615256976796,123.974924396754)) ;
#87377 = CARTESIAN_POINT('Ctrl Pts',(-17.9340194463027,38.6253093543887,123.722198205263)) ;
#87378 = CARTESIAN_POINT('Ctrl Pts',(-17.9027887073884,38.6352130079296,123.463801752552)) ;
#87379 = CARTESIAN_POINT('Ctrl Pts',(-17.9163242119673,38.6451572769249,123.202860594878)) ;
#87380 = CARTESIAN_POINT('Ctrl Pts',(-17.9947872688244,38.6584882852576,122.861360560677)) ;
#87381 = CARTESIAN_POINT('Ctrl Pts',(-18.2021257874539,38.6751098657819,122.471340515978)) ;
#87382 = CARTESIAN_POINT('Ctrl Pts',(-18.5280196716949,38.6916525364803,122.176175599121)) ;
#87383 = CARTESIAN_POINT('Ctrl Pts',(-18.84008875281,38.7050016960432,122.015952826464)) ;
#87384 = CARTESIAN_POINT('Ctrl Pts',(-19.1721179105993,38.7182298462027,121.912874830925)) ;
#87385 = CARTESIAN_POINT('Ctrl Pts',(-19.6137093351474,38.7348605233402,121.89504706836)) ;
#87386 = CARTESIAN_POINT('Ctrl Pts',(-20.1178745686584,38.7547634626283,122.055405875493)) ;
#87387 = CARTESIAN_POINT('Ctrl Pts',(-20.5372564996866,38.7746663292316,122.377645054216)) ;
#87388 = CARTESIAN_POINT('Ctrl Pts',(-20.8224486031123,38.7945794943364,122.823633412691)) ;
#87389 = CARTESIAN_POINT('Ctrl Pts',(-20.9381893408,38.8146153234777,123.343346667635)) ;
#87390 = CARTESIAN_POINT('Ctrl Pts',(-20.8706660685584,38.8344338983558,123.865874261203)) ;
#87391 = CARTESIAN_POINT('Ctrl Pts',(-20.627922443163,38.8544041993978,124.337692899044)) ;
#87392 = CARTESIAN_POINT('Ctrl Pts',(-20.2401234229137,38.8742957317623,124.69730681963)) ;
#87393 = CARTESIAN_POINT('Ctrl Pts',(-19.7497967047093,38.8943188295789,124.903871868757)) ;
#87394 = CARTESIAN_POINT('Ctrl Pts',(-19.2242573161077,38.9141155824988,124.930795625851)) ;
#87395 = CARTESIAN_POINT('Ctrl Pts',(-18.7165907441389,38.9340766709876,124.776879006077)) ;
#87396 = CARTESIAN_POINT('Ctrl Pts',(-18.2921488184441,38.9540549399198,124.457746589565)) ;
#87397 = CARTESIAN_POINT('Ctrl Pts',(-18.0037947360342,38.9738749547108,124.016952429214)) ;
#87398 = CARTESIAN_POINT('Ctrl Pts',(-17.8810979198861,38.9938133639626,123.501394794737)) ;
#87399 = CARTESIAN_POINT('Ctrl Pts',(-17.9432262389664,39.013860481355,122.972141220867)) ;
#87400 = CARTESIAN_POINT('Ctrl Pts',(-18.179999474083,39.0337067271889,122.500852961374)) ;
#87401 = CARTESIAN_POINT('Ctrl Pts',(-18.5620692319856,39.0535556957009,122.137036795423)) ;
#87402 = CARTESIAN_POINT('Ctrl Pts',(-19.0504584844477,39.0736059980122,121.923948334636)) ;
#87403 = CARTESIAN_POINT('Ctrl Pts',(-19.5767211389698,39.0934409204434,121.8907738155)) ;
#87404 = CARTESIAN_POINT('Ctrl Pts',(-20.0851205819504,39.1133713216693,122.038805273945)) ;
#87405 = CARTESIAN_POINT('Ctrl Pts',(-20.5122385328754,39.1332562670282,122.350424357377)) ;
#87406 = CARTESIAN_POINT('Ctrl Pts',(-20.8092718181263,39.1533288751795,122.793463019832)) ;
#87407 = CARTESIAN_POINT('Ctrl Pts',(-20.9356236783323,39.1731201915077,123.304163853874)) ;
#87408 = CARTESIAN_POINT('Ctrl Pts',(-20.8812715084831,39.1930849812749,123.831959781897)) ;
#87409 = CARTESIAN_POINT('Ctrl Pts',(-20.6486431634336,39.2130679370252,124.309427208045)) ;
#87410 = CARTESIAN_POINT('Ctrl Pts',(-20.2711039549004,39.2328764590014,124.676430038506)) ;
#87411 = CARTESIAN_POINT('Ctrl Pts',(-19.7870902404589,39.2528620337372,124.894984520865)) ;
#87412 = CARTESIAN_POINT('Ctrl Pts',(-19.2600307895484,39.2727446738056,124.934952427669)) ;
#87413 = CARTESIAN_POINT('Ctrl Pts',(-18.7492190934437,39.2926999859375,124.792610565746)) ;
#87414 = CARTESIAN_POINT('Ctrl Pts',(-18.3190388924115,39.3125743425453,124.485911249285)) ;
#87415 = CARTESIAN_POINT('Ctrl Pts',(-18.0175162438669,39.3325565494064,124.048781584885)) ;
#87416 = CARTESIAN_POINT('Ctrl Pts',(-17.8838364996547,39.3524876273563,123.536075517646)) ;
#87417 = CARTESIAN_POINT('Ctrl Pts',(-17.9330377132969,39.3724146022113,123.008847051512)) ;
#87418 = CARTESIAN_POINT('Ctrl Pts',(-18.1572602607085,39.3922470611602,122.531726093143)) ;
#87419 = CARTESIAN_POINT('Ctrl Pts',(-18.4706715836701,39.4089047453354,122.219175253551)) ;
#87420 = CARTESIAN_POINT('Ctrl Pts',(-18.7724853140679,39.4221539692425,122.045409139846)) ;
#87421 = CARTESIAN_POINT('Ctrl Pts',(-19.0206746467771,39.4322029906937,121.95528639923)) ;
#87422 = CARTESIAN_POINT('Ctrl Pts',(-19.2758714027625,39.4420629989242,121.910414373671)) ;
#87423 = CARTESIAN_POINT('Ctrl Pts',(-19.6249850662901,39.4553465121488,121.909430053781)) ;
#87424 = CARTESIAN_POINT('Ctrl Pts',(-20.0524695157253,39.4719924311496,122.023204765113)) ;
#87425 = CARTESIAN_POINT('Ctrl Pts',(-20.4138864148045,39.4885464089657,122.274186137911)) ;
#87426 = CARTESIAN_POINT('Ctrl Pts',(-20.6406300091737,39.5019061379373,122.542218010001)) ;
#87427 = CARTESIAN_POINT('Ctrl Pts',(-20.7717096169385,39.511799189734,122.766754046185)) ;
#87428 = CARTESIAN_POINT('Ctrl Pts',(-20.8630087660866,39.521789155015,123.012860662966)) ;
#87429 = CARTESIAN_POINT('Ctrl Pts',(-20.9101748143691,39.5317410358759,123.270138684946)) ;
#87430 = CARTESIAN_POINT('Ctrl Pts',(-20.9117456673708,39.5417893875677,123.534165997582)) ;
#87431 = CARTESIAN_POINT('Ctrl Pts',(-20.8686552536552,39.5516306716739,123.789195920828)) ;
#87432 = CARTESIAN_POINT('Ctrl Pts',(-20.7812002337361,39.5616173747996,124.036586790097)) ;
#87433 = CARTESIAN_POINT('Ctrl Pts',(-20.6528795142412,39.571552403617,124.264016264375)) ;
#87434 = CARTESIAN_POINT('Ctrl Pts',(-20.4848907700779,39.5816081985239,124.46795141361)) ;
#87435 = CARTESIAN_POINT('Ctrl Pts',(-20.2887891671277,39.5914365618132,124.636091146284)) ;
#87436 = CARTESIAN_POINT('Ctrl Pts',(-20.0614641234576,39.6014975317111,124.771025787529)) ;
#87437 = CARTESIAN_POINT('Ctrl Pts',(-19.8176332037188,39.6114118106009,124.862898597772)) ;
#87438 = CARTESIAN_POINT('Ctrl Pts',(-19.5592282819904,39.6214208050691,124.912002571716)) ;
#87439 = CARTESIAN_POINT('Ctrl Pts',(-19.2956754516133,39.6314506396329,124.914961194742)) ;
#87440 = CARTESIAN_POINT('Ctrl Pts',(-19.0399610301937,39.6413088697051,124.873328894269)) ;
#87441 = CARTESIAN_POINT('Ctrl Pts',(-18.7918272427075,39.6513075754475,124.787030713098)) ;
#87442 = CARTESIAN_POINT('Ctrl Pts',(-18.5646041239284,39.6612022313663,124.660518202869)) ;
#87443 = CARTESIAN_POINT('Ctrl Pts',(-18.3594891226658,39.6712652957503,124.493676816178)) ;
#87444 = CARTESIAN_POINT('Ctrl Pts',(-18.1900268540481,39.6811049540302,124.298315227073)) ;
#87445 = CARTESIAN_POINT('Ctrl Pts',(-18.053792583236,39.691168121112,124.071699946612)) ;
#87446 = CARTESIAN_POINT('Ctrl Pts',(-17.960749315,39.7010623662391,123.828876199066)) ;
#87447 = CARTESIAN_POINT('Ctrl Pts',(-17.9103583441189,39.7110041878437,123.572554229599)) ;
#87448 = CARTESIAN_POINT('Ctrl Pts',(-17.9051091078073,39.7210067187618,123.309715572966)) ;
#87449 = CARTESIAN_POINT('Ctrl Pts',(-17.9461034213345,39.7310413452193,123.049236091637)) ;
#87450 = CARTESIAN_POINT('Ctrl Pts',(-18.0297068679523,39.7408868802057,122.804375715976)) ;
#87451 = CARTESIAN_POINT('Ctrl Pts',(-18.1557911659349,39.7508703050448,122.574330051635)) ;
#87452 = CARTESIAN_POINT('Ctrl Pts',(-18.3194197366641,39.7608206954098,122.370358879002)) ;
#87453 = CARTESIAN_POINT('Ctrl Pts',(-18.5166895154144,39.7708183357069,122.1968019572)) ;
#87454 = CARTESIAN_POINT('Ctrl Pts',(-18.7422717110751,39.7808574162701,122.06004045278)) ;
#87455 = CARTESIAN_POINT('Ctrl Pts',(-18.9827757053251,39.7906835670392,121.966001404595)) ;
#87456 = CARTESIAN_POINT('Ctrl Pts',(-19.241779151991,39.8007401419683,121.913550884301)) ;
#87457 = CARTESIAN_POINT('Ctrl Pts',(-19.5029424763994,39.8106806813486,121.907401203059)) ;
#87458 = CARTESIAN_POINT('Ctrl Pts',(-19.7603853137432,39.820585074325,121.945742920367)) ;
#87459 = CARTESIAN_POINT('Ctrl Pts',(-20.0107266937267,39.8306317285299,122.029537599121)) ;
#87460 = CARTESIAN_POINT('Ctrl Pts',(-20.2393968682051,39.8405272904683,122.153454191526)) ;
#87461 = CARTESIAN_POINT('Ctrl Pts',(-20.4464414983218,39.8505893683139,122.317864784386)) ;
#87462 = CARTESIAN_POINT('Ctrl Pts',(-20.6181263774124,39.8604320667276,122.511365345899)) ;
#87463 = CARTESIAN_POINT('Ctrl Pts',(-20.7561382322086,39.8704228416891,122.734672291079)) ;
#87464 = CARTESIAN_POINT('Ctrl Pts',(-20.8526500680807,39.8803507067082,122.97707426249)) ;
#87465 = CARTESIAN_POINT('Ctrl Pts',(-20.9063594910296,39.8903394514744,123.234019741878)) ;
#87466 = CARTESIAN_POINT('Ctrl Pts',(-20.9142878541207,39.9003722370613,123.497555642552)) ;
#87467 = CARTESIAN_POINT('Ctrl Pts',(-20.8772279525817,39.910238921682,123.754170693425)) ;
#87468 = CARTESIAN_POINT('Ctrl Pts',(-20.7961043668712,39.9202008138451,124.003076881027)) ;
#87469 = CARTESIAN_POINT('Ctrl Pts',(-20.6717493071348,39.9302342907577,124.2355665129)) ;
#87470 = CARTESIAN_POINT('Ctrl Pts',(-20.5116325782537,39.940118632006,124.440138606861)) ;
#87471 = CARTESIAN_POINT('Ctrl Pts',(-20.3149883606172,39.9501815741271,124.61689780952)) ;
#87472 = CARTESIAN_POINT('Ctrl Pts',(-20.0953995131372,39.9600319757467,124.754007658767)) ;
#87473 = CARTESIAN_POINT('Ctrl Pts',(-19.8513143447031,39.9700588645364,124.853250471539)) ;
#87474 = CARTESIAN_POINT('Ctrl Pts',(-19.5934970141475,39.9800874794926,124.907943166141)) ;
#87475 = CARTESIAN_POINT('Ctrl Pts',(-19.3349601607156,39.9899327026126,124.917361759063)) ;
#87476 = CARTESIAN_POINT('Ctrl Pts',(-19.0748122096571,39.9999233864186,124.881915578707)) ;
#87477 = CARTESIAN_POINT('Ctrl Pts',(-18.8237784515497,40.009961268491,124.800902625927)) ;
#87478 = CARTESIAN_POINT('Ctrl Pts',(-18.5948964274932,40.0198056281299,124.68030432098)) ;
#87479 = CARTESIAN_POINT('Ctrl Pts',(-18.3872328665451,40.0297904987446,124.519971576075)) ;
#87480 = CARTESIAN_POINT('Ctrl Pts',(-18.2112308942488,40.0397297820733,124.326928042325)) ;
#87481 = CARTESIAN_POINT('Ctrl Pts',(-18.0701011370966,40.0497703914464,124.10401924585)) ;
#87482 = CARTESIAN_POINT('Ctrl Pts',(-17.9711747293191,40.0596552423596,123.863797270785)) ;
#87483 = CARTESIAN_POINT('Ctrl Pts',(-17.914507891847,40.0696571985284,123.607177988291)) ;
#87484 = CARTESIAN_POINT('Ctrl Pts',(-17.9031408318448,40.0795757952489,123.346733888948)) ;
#87485 = CARTESIAN_POINT('Ctrl Pts',(-17.9376487606401,40.0896226173247,123.085016388873)) ;
#87486 = CARTESIAN_POINT('Ctrl Pts',(-18.0155031495141,40.0994968984374,122.837438413162)) ;
#87487 = CARTESIAN_POINT('Ctrl Pts',(-18.1371591486748,40.109551098482,122.602950598639)) ;
#87488 = CARTESIAN_POINT('Ctrl Pts',(-18.2951196454476,40.1194465281173,122.396320882415)) ;
#87489 = CARTESIAN_POINT('Ctrl Pts',(-18.4896702718675,40.1295081564346,122.217309891194)) ;
#87490 = CARTESIAN_POINT('Ctrl Pts',(-18.7075627861497,40.1393527852645,122.077821066016)) ;
#87491 = CARTESIAN_POINT('Ctrl Pts',(-18.9487886325186,40.1493128328701,121.976254285154)) ;
#87492 = CARTESIAN_POINT('Ctrl Pts',(-19.2060965362213,40.1593511390442,121.918165822933)) ;
#87493 = CARTESIAN_POINT('Ctrl Pts',(-19.4652798129029,40.1692244384768,121.905341126692)) ;
#87494 = CARTESIAN_POINT('Ctrl Pts',(-19.7278620306309,40.1792977000631,121.938443177458)) ;
#87495 = CARTESIAN_POINT('Ctrl Pts',(-19.9745652121543,40.1891179260198,122.014376604329)) ;
#87496 = CARTESIAN_POINT('Ctrl Pts',(-20.210384152523,40.1991969899593,122.134825848413)) ;
#87497 = CARTESIAN_POINT('Ctrl Pts',(-20.4170898719692,40.2090470799791,122.290751429487)) ;
#87498 = CARTESIAN_POINT('Ctrl Pts',(-20.5976846428322,40.2191258335929,122.484401518764)) ;
#87499 = CARTESIAN_POINT('Ctrl Pts',(-20.7384649199968,40.2289473008524,122.700793862279)) ;
#87500 = CARTESIAN_POINT('Ctrl Pts',(-20.8423732928383,40.23901289921,122.943977873275)) ;
#87501 = CARTESIAN_POINT('Ctrl Pts',(-20.9014655130511,40.2489155549847,123.197477874162)) ;
#87502 = CARTESIAN_POINT('Ctrl Pts',(-20.9159315140315,40.2589663808143,123.461152741984)) ;
#87503 = CARTESIAN_POINT('Ctrl Pts',(-20.8851862687562,40.2688405851532,123.718866407652)) ;
#87504 = CARTESIAN_POINT('Ctrl Pts',(-20.8087033848994,40.2789130351923,123.972210529531)) ;
#87505 = CARTESIAN_POINT('Ctrl Pts',(-20.6924508708633,40.2887420519658,124.202923123241)) ;
#87506 = CARTESIAN_POINT('Ctrl Pts',(-20.534514449587,40.2988088978806,124.415095541138)) ;
#87507 = CARTESIAN_POINT('Ctrl Pts',(-20.3453419288887,40.3086990691824,124.593367187674)) ;
#87508 = CARTESIAN_POINT('Ctrl Pts',(-20.126206043176,40.3186912628062,124.738011905012)) ;
#87509 = CARTESIAN_POINT('Ctrl Pts',(-19.8858849575961,40.3286540734297,124.841878589706)) ;
#87510 = CARTESIAN_POINT('Ctrl Pts',(-19.6328023115127,40.3385583462731,124.902733214097)) ;
#87511 = CARTESIAN_POINT('Ctrl Pts',(-19.368941004048,40.3486188380777,124.918739240953)) ;
#87512 = CARTESIAN_POINT('Ctrl Pts',(-19.111948949925,40.3584591697501,124.889672424697)) ;
#87513 = CARTESIAN_POINT('Ctrl Pts',(-18.8582728174585,40.3685222158418,124.815092864794)) ;
#87514 = CARTESIAN_POINT('Ctrl Pts',(-18.6254185641157,40.3784162715369,124.699353388829)) ;
#87515 = CARTESIAN_POINT('Ctrl Pts',(-18.414789936686,40.3883589718599,124.544790683395)) ;
#87516 = CARTESIAN_POINT('Ctrl Pts',(-18.2329762001901,40.3983647127875,124.354801620633)) ;
#87517 = CARTESIAN_POINT('Ctrl Pts',(-18.0869571139645,40.408385623303,124.135661151696)) ;
#87518 = CARTESIAN_POINT('Ctrl Pts',(-17.982299068752,40.418276358753,123.897735676412)) ;
#87519 = CARTESIAN_POINT('Ctrl Pts',(-17.9195403076832,40.4282678994818,123.64278976609)) ;
#87520 = CARTESIAN_POINT('Ctrl Pts',(-17.9021523398952,40.4382157599035,123.381951195381)) ;
#87521 = CARTESIAN_POINT('Ctrl Pts',(-17.9298041725074,40.4481624290898,123.122015017719)) ;
#87522 = CARTESIAN_POINT('Ctrl Pts',(-18.0031779584756,40.4582105052254,122.868371382531)) ;
#87523 = CARTESIAN_POINT('Ctrl Pts',(-18.1169687224454,40.468058103231,122.635944200235)) ;
#87524 = CARTESIAN_POINT('Ctrl Pts',(-18.2704811318407,40.4780198263155,122.423910978732)) ;
#87525 = CARTESIAN_POINT('Ctrl Pts',(-18.4599935581485,40.4880484613985,122.240750173216)) ;
#87526 = CARTESIAN_POINT('Ctrl Pts',(-18.6757822343563,40.4979587697165,122.094962047602)) ;
#87527 = CARTESIAN_POINT('Ctrl Pts',(-18.9139355025239,40.5078936668524,121.987961124184)) ;
#87528 = CARTESIAN_POINT('Ctrl Pts',(-19.1697997287511,40.517934749795,121.923493244547)) ;
#87529 = CARTESIAN_POINT('Ctrl Pts',(-19.428950366049,40.5278220926232,121.904543523959)) ;
#87530 = CARTESIAN_POINT('Ctrl Pts',(-19.6901959445774,40.5378136075626,121.930704214457)) ;
#87531 = CARTESIAN_POINT('Ctrl Pts',(-19.9419057770973,40.5477649987591,122.001654050665)) ;
#87532 = CARTESIAN_POINT('Ctrl Pts',(-20.1772160470658,40.5576975320917,122.114605806638)) ;
#87533 = CARTESIAN_POINT('Ctrl Pts',(-20.390773351119,40.5676946899911,122.267599496389)) ;
#87534 = CARTESIAN_POINT('Ctrl Pts',(-20.5744051539528,40.5776797001546,122.455089020715)) ;
#87535 = CARTESIAN_POINT('Ctrl Pts',(-20.723188468568,40.5877225267244,122.673023900318)) ;
#87536 = CARTESIAN_POINT('Ctrl Pts',(-20.8301426365293,40.5975527610294,122.908217068064)) ;
#87537 = CARTESIAN_POINT('Ctrl Pts',(-20.8963379142863,40.607628786264,123.164540306248)) ;
#87538 = CARTESIAN_POINT('Ctrl Pts',(-20.9167055563444,40.6174810227549,123.422701150021)) ;
#87539 = CARTESIAN_POINT('Ctrl Pts',(-20.891615051151,40.627554229189,123.686179366379)) ;
#87540 = CARTESIAN_POINT('Ctrl Pts',(-20.8226924038434,40.6373957386962,123.935469529968)) ;
#87541 = CARTESIAN_POINT('Ctrl Pts',(-20.7110845119955,40.647356685476,124.172237837628)) ;
#87542 = CARTESIAN_POINT('Ctrl Pts',(-20.5584645897465,40.657394514276,124.387376516039)) ;
#87543 = CARTESIAN_POINT('Ctrl Pts',(-20.3741751702042,40.6672688240305,124.570098190474)) ;
#87544 = CARTESIAN_POINT('Ctrl Pts',(-20.1567868434197,40.6773385217037,124.720922673687)) ;
#87545 = CARTESIAN_POINT('Ctrl Pts',(-19.9221561017423,40.6871719929911,124.829257549577)) ;
#87546 = CARTESIAN_POINT('Ctrl Pts',(-19.6675134133936,40.697201639521,124.897250208865)) ;
#87547 = CARTESIAN_POINT('Ctrl Pts',(-19.404726915787,40.7072361538484,124.919206335434)) ;
#87548 = CARTESIAN_POINT('Ctrl Pts',(-19.1475426653616,40.7170614393193,124.896320551621)) ;
#87549 = CARTESIAN_POINT('Ctrl Pts',(-18.8935848410147,40.7270656808678,124.828449926807)) ;
#87550 = CARTESIAN_POINT('Ctrl Pts',(-18.6557571219536,40.7370483259469,124.717619979883)) ;
#87551 = CARTESIAN_POINT('Ctrl Pts',(-18.4396753878514,40.7470935230384,124.566036174496)) ;
#87552 = CARTESIAN_POINT('Ctrl Pts',(-18.2569837011254,40.7569166387985,124.383646814928)) ;
#87553 = CARTESIAN_POINT('Ctrl Pts',(-18.1050079926846,40.7669512505988,124.168150561838)) ;
#87554 = CARTESIAN_POINT('Ctrl Pts',(-17.9935267427077,40.776976259372,123.929445084339)) ;
#87555 = CARTESIAN_POINT('Ctrl Pts',(-17.9258202753636,40.7868281842135,123.679551402899)) ;
#87556 = CARTESIAN_POINT('Ctrl Pts',(-17.9018056354857,40.7968191225363,123.418132469691)) ;
#87557 = CARTESIAN_POINT('Ctrl Pts',(-17.9232248951131,40.8067371076827,123.158348244679)) ;
#87558 = CARTESIAN_POINT('Ctrl Pts',(-17.9900857838276,40.8167652085782,122.903464281987)) ;
#87559 = CARTESIAN_POINT('Ctrl Pts',(-18.0985313024471,40.8266504495208,122.667402977687)) ;
#87560 = CARTESIAN_POINT('Ctrl Pts',(-18.2473410925538,40.8366395624874,122.451144336104)) ;
#87561 = CARTESIAN_POINT('Ctrl Pts',(-18.4328177933568,40.8466816268282,122.263433343905)) ;
#87562 = CARTESIAN_POINT('Ctrl Pts',(-18.6432373021323,40.8565108282327,122.113605035665)) ;
#87563 = CARTESIAN_POINT('Ctrl Pts',(-18.8804063338663,40.8665176689909,122.000080751744)) ;
#87564 = CARTESIAN_POINT('Ctrl Pts',(-19.1333087574883,40.8765051931828,121.929728664348)) ;
#87565 = CARTESIAN_POINT('Ctrl Pts',(-19.3956374933461,40.8865348389914,121.904438993338)) ;
#87566 = CARTESIAN_POINT('Ctrl Pts',(-19.6543707145139,40.8964088697302,121.924454848222)) ;
#87567 = CARTESIAN_POINT('Ctrl Pts',(-19.9089008937694,40.9064081925943,121.989579416378)) ;
#87568 = CARTESIAN_POINT('Ctrl Pts',(-20.1463240582721,40.9163190281699,122.096753063302)) ;
#87569 = CARTESIAN_POINT('Ctrl Pts',(-20.3645193729387,40.9263732761439,122.245676406375)) ;
#87570 = CARTESIAN_POINT('Ctrl Pts',(-20.5501419901856,40.9362320204066,122.42647707007)) ;
#87571 = CARTESIAN_POINT('Ctrl Pts',(-20.7048457015326,40.9463001064796,122.641065679255)) ;
#87572 = CARTESIAN_POINT('Ctrl Pts',(-20.8175173641889,40.9561555896591,122.874289210237)) ;
#87573 = CARTESIAN_POINT('Ctrl Pts',(-20.8897275055665,40.9661504354533,123.126813177261)) ;
#87574 = CARTESIAN_POINT('Ctrl Pts',(-20.9165302141604,40.9761817311159,123.389064120819)) ;
#87575 = CARTESIAN_POINT('Ctrl Pts',(-20.898116848103,40.9860482744057,123.647700931821)) ;
#87576 = CARTESIAN_POINT('Ctrl Pts',(-20.8347236238339,40.9960356701691,123.902356200774)) ;
#87577 = CARTESIAN_POINT('Ctrl Pts',(-20.7286285702455,41.0059807108991,124.141239921477)) ;
#87578 = CARTESIAN_POINT('Ctrl Pts',(-20.5811211598771,41.0160252171158,124.360105227099)) ;
#87579 = CARTESIAN_POINT('Ctrl Pts',(-20.4012876880261,41.0258887232531,124.546811663943)) ;
#87580 = CARTESIAN_POINT('Ctrl Pts',(-20.1893463018213,41.0358815840892,124.701796997942)) ;
#87581 = CARTESIAN_POINT('Ctrl Pts',(-19.9552720707621,41.0458077778081,124.816998522553)) ;
#87582 = CARTESIAN_POINT('Ctrl Pts',(-19.7024899327944,41.0558267038407,124.890516309692)) ;
#87583 = CARTESIAN_POINT('Ctrl Pts',(-19.4434540809893,41.0657417032083,124.918982353563)) ;
#87584 = CARTESIAN_POINT('Ctrl Pts',(-19.179821038914,41.0757964747656,124.901749795245)) ;
#87585 = CARTESIAN_POINT('Ctrl Pts',(-18.9280800412219,41.0856554370632,124.840372296681)) ;
#87586 = CARTESIAN_POINT('Ctrl Pts',(-18.6874351062413,41.095649680901,124.735268941808)) ;
#87587 = CARTESIAN_POINT('Ctrl Pts',(-18.4700684891871,41.1055749103252,124.591037888929)) ;
#87588 = CARTESIAN_POINT('Ctrl Pts',(-18.2791378076578,41.1156028742167,124.409455504001)) ;
#87589 = CARTESIAN_POINT('Ctrl Pts',(-18.1245883806122,41.1254891338471,124.20057485489)) ;
#87590 = CARTESIAN_POINT('Ctrl Pts',(-18.0068635292268,41.1355208969249,123.964745548738)) ;
#87591 = CARTESIAN_POINT('Ctrl Pts',(-17.9327293076382,41.1454025232191,123.715825423128)) ;
#87592 = CARTESIAN_POINT('Ctrl Pts',(-17.9023394171472,41.1554642927052,123.453203976772)) ;
#87593 = CARTESIAN_POINT('Ctrl Pts',(-17.9176211064176,41.1653221602007,123.194569188612)) ;
#87594 = CARTESIAN_POINT('Ctrl Pts',(-17.9778112462982,41.1753137853181,122.939023648064)) ;
#87595 = CARTESIAN_POINT('Ctrl Pts',(-18.0809522301768,41.1852505844263,122.699110258918)) ;
#87596 = CARTESIAN_POINT('Ctrl Pts',(-18.2246372961258,41.1952414139836,122.479365383899)) ;
#87597 = CARTESIAN_POINT('Ctrl Pts',(-18.4051031632681,41.2052646496968,122.287492545493)) ;
#87598 = CARTESIAN_POINT('Ctrl Pts',(-18.6133310445568,41.215160997726,122.131695698258)) ;
#87599 = CARTESIAN_POINT('Ctrl Pts',(-18.8473975521708,41.2251505602285,122.012807543813)) ;
#87600 = CARTESIAN_POINT('Ctrl Pts',(-19.0999569107167,41.235190867913,121.936495551711)) ;
#87601 = CARTESIAN_POINT('Ctrl Pts',(-19.35673862267,41.2450331712602,121.905316610654)) ;
#87602 = CARTESIAN_POINT('Ctrl Pts',(-19.619750139844,41.2550568795393,121.919098001981)) ;
#87603 = CARTESIAN_POINT('Ctrl Pts',(-19.9583979422888,41.268279057007,121.997129854709)) ;
#87604 = CARTESIAN_POINT('Ctrl Pts',(-20.2706317559911,41.2815716420663,122.162222495001)) ;
#87605 = CARTESIAN_POINT('Ctrl Pts',(-20.5265422578919,41.2948564979879,122.399798532575)) ;
#87606 = CARTESIAN_POINT('Ctrl Pts',(-20.6848531440753,41.3048287251607,122.608586988607)) ;
#87607 = CARTESIAN_POINT('Ctrl Pts',(-20.8041778753836,41.3147373415997,122.840061396327)) ;
#87608 = CARTESIAN_POINT('Ctrl Pts',(-20.8825078353512,41.3247905469834,123.092342498857)) ;
#87609 = CARTESIAN_POINT('Ctrl Pts',(-20.9153911019207,41.3346556807437,123.349517175633)) ;
#87610 = CARTESIAN_POINT('Ctrl Pts',(-20.8994532016943,41.34799473837,123.699671410169)) ;
#87611 = CARTESIAN_POINT('Ctrl Pts',(-20.7662682588357,41.3645639257032,124.119498420051)) ;
#87612 = CARTESIAN_POINT('Ctrl Pts',(-20.4969289351474,41.3812090655542,124.470369460942)) ;
#87613 = CARTESIAN_POINT('Ctrl Pts',(-20.2201112015402,41.3944813680276,124.682651973969)) ;
#87614 = CARTESIAN_POINT('Ctrl Pts',(-19.9875982884763,41.4044623314752,124.803972762843)) ;
#87615 = CARTESIAN_POINT('Ctrl Pts',(-19.738528944689,41.4144041635445,124.882935891262)) ;
#87616 = CARTESIAN_POINT('Ctrl Pts',(-19.3916330563447,41.42772373276,124.929305565793)) ;
#87617 = CARTESIAN_POINT('Ctrl Pts',(-18.9557211738586,41.4442538876927,124.873625074331)) ;
#87618 = CARTESIAN_POINT('Ctrl Pts',(-18.4827898293542,41.4642756131848,124.629964635199)) ;
#87619 = CARTESIAN_POINT('Ctrl Pts',(-18.1247913754587,41.4840870097916,124.243659355812)) ;
#87620 = CARTESIAN_POINT('Ctrl Pts',(-17.9175945300158,41.5040722585005,123.754695417451)) ;
#87621 = CARTESIAN_POINT('Ctrl Pts',(-17.8901702572938,41.5239663211364,123.226570828249)) ;
#87622 = CARTESIAN_POINT('Ctrl Pts',(-18.0441233573117,41.54389800031,122.719693569398)) ;
#87623 = CARTESIAN_POINT('Ctrl Pts',(-18.3626064665209,41.563862054782,122.295289089254)) ;
#87624 = CARTESIAN_POINT('Ctrl Pts',(-18.8047488016914,41.5837429565449,122.005904879941)) ;
#87625 = CARTESIAN_POINT('Ctrl Pts',(-19.320432669292,41.6036816181533,121.883949466073)) ;
#87626 = CARTESIAN_POINT('Ctrl Pts',(-19.845694207807,41.6235781434086,121.945081447372)) ;
#87627 = CARTESIAN_POINT('Ctrl Pts',(-20.3189427672172,41.6434731818629,122.181005425179)) ;
#87628 = CARTESIAN_POINT('Ctrl Pts',(-20.6844409401465,41.663437005169,122.565598444425)) ;
#87629 = CARTESIAN_POINT('Ctrl Pts',(-20.8961948389639,41.6833111292981,123.049559754929)) ;
#87630 = CARTESIAN_POINT('Ctrl Pts',(-20.930750337764,41.7032862050253,123.5793623284)) ;
#87631 = CARTESIAN_POINT('Ctrl Pts',(-20.7818779747331,41.7232397743819,124.088362609543)) ;
#87632 = CARTESIAN_POINT('Ctrl Pts',(-20.4708653827436,41.7430776845698,124.514126207426)) ;
#87633 = CARTESIAN_POINT('Ctrl Pts',(-20.0305044149458,41.7630535131407,124.810712363069)) ;
#87634 = CARTESIAN_POINT('Ctrl Pts',(-19.5167523633582,41.782971557851,124.938278605792)) ;
#87635 = CARTESIAN_POINT('Ctrl Pts',(-18.9912886178478,41.8028418036386,124.884326486846)) ;
#87636 = CARTESIAN_POINT('Ctrl Pts',(-18.5120647055615,41.8228908067382,124.651624297318)) ;
#87637 = CARTESIAN_POINT('Ctrl Pts',(-18.1453880278503,41.842670047979,124.274702004828)) ;
#87638 = CARTESIAN_POINT('Ctrl Pts',(-17.9259851440591,41.8627001116879,123.789780611659)) ;
#87639 = CARTESIAN_POINT('Ctrl Pts',(-17.8863697134436,41.8825823965899,123.262746959437)) ;
#87640 = CARTESIAN_POINT('Ctrl Pts',(-18.0275326386484,41.9024646974829,122.753560552606)) ;
#87641 = CARTESIAN_POINT('Ctrl Pts',(-18.3357088896958,41.9224478071012,122.320980688982)) ;
#87642 = CARTESIAN_POINT('Ctrl Pts',(-18.7710306130654,41.9423382024791,122.02096992026)) ;
#87643 = CARTESIAN_POINT('Ctrl Pts',(-19.2824613005974,41.9622349925134,121.886735352838)) ;
#87644 = CARTESIAN_POINT('Ctrl Pts',(-19.8096884308124,41.982152046455,121.934563073507)) ;
#87645 = CARTESIAN_POINT('Ctrl Pts',(-20.2909909356095,42.0021555946585,122.16058890975)) ;
#87646 = CARTESIAN_POINT('Ctrl Pts',(-20.6644231854792,42.0220938883111,122.53654694601)) ;
#87647 = CARTESIAN_POINT('Ctrl Pts',(-20.8870221312374,42.041915375744,123.014039318309)) ;
#87648 = CARTESIAN_POINT('Ctrl Pts',(-20.9342135131919,42.0618937687349,123.542870872687)) ;
#87649 = CARTESIAN_POINT('Ctrl Pts',(-20.7983116521925,42.0817921503486,124.05406099751)) ;
#87650 = CARTESIAN_POINT('Ctrl Pts',(-20.5470876259133,42.0983750810785,124.416078628644)) ;
#87651 = CARTESIAN_POINT('Ctrl Pts',(-20.2810340791425,42.1116493166673,124.641785333089)) ;
#87652 = CARTESIAN_POINT('Ctrl Pts',(-20.0530711216127,42.1216957341235,124.774894284612)) ;
#87653 = CARTESIAN_POINT('Ctrl Pts',(-19.8104700418555,42.1315409593428,124.864850290018)) ;
#87654 = CARTESIAN_POINT('Ctrl Pts',(-19.4658985569829,42.1448759303822,124.928521275722)) ;
#87655 = CARTESIAN_POINT('Ctrl Pts',(-19.0264447066916,42.1614587871748,124.893669283051)) ;
#87656 = CARTESIAN_POINT('Ctrl Pts',(-18.6239261419113,42.1781017895242,124.710472536037)) ;
#87657 = CARTESIAN_POINT('Ctrl Pts',(-18.3550087789404,42.1913455205559,124.489421557899)) ;
#87658 = CARTESIAN_POINT('Ctrl Pts',(-18.1831612885463,42.2013999152305,124.288789628079)) ;
#87659 = CARTESIAN_POINT('Ctrl Pts',(-18.0512749568523,42.2112409766191,124.066279127092)) ;
#87660 = CARTESIAN_POINT('Ctrl Pts',(-17.9577303156056,42.2213072009756,123.818889092396)) ;
#87661 = CARTESIAN_POINT('Ctrl Pts',(-17.9095286836072,42.2311878138952,123.563707583519)) ;
#87662 = CARTESIAN_POINT('Ctrl Pts',(-17.9058337757334,42.2411811070548,123.301162738247)) ;
#87663 = CARTESIAN_POINT('Ctrl Pts',(-17.9475195177784,42.2511321152785,123.042958068114)) ;
#87664 = CARTESIAN_POINT('Ctrl Pts',(-18.0344126776209,42.2611806296404,122.793630948039)) ;
#87665 = CARTESIAN_POINT('Ctrl Pts',(-18.1603920215042,42.2710221357031,122.56773601956)) ;
#87666 = CARTESIAN_POINT('Ctrl Pts',(-18.3255845008848,42.2810077883328,122.363897258987)) ;
#87667 = CARTESIAN_POINT('Ctrl Pts',(-18.5227313519484,42.2909467971777,122.192513006054)) ;
#87668 = CARTESIAN_POINT('Ctrl Pts',(-18.7489176532003,42.3009877224707,122.056676120919)) ;
#87669 = CARTESIAN_POINT('Ctrl Pts',(-18.9915477533087,42.3108780442256,121.96343274295)) ;
#87670 = CARTESIAN_POINT('Ctrl Pts',(-19.2492897392915,42.320874017559,121.912831427002)) ;
#87671 = CARTESIAN_POINT('Ctrl Pts',(-19.510238542724,42.3308054171411,121.90776329539)) ;
#87672 = CARTESIAN_POINT('Ctrl Pts',(-19.7700878324599,42.3408109576181,121.948013744856)) ;
#87673 = CARTESIAN_POINT('Ctrl Pts',(-20.0195067969403,42.3508439415494,122.033453514433)) ;
#87674 = CARTESIAN_POINT('Ctrl Pts',(-20.2464693982846,42.3606995723763,122.158262805078)) ;
#87675 = CARTESIAN_POINT('Ctrl Pts',(-20.4514198298294,42.3706989745694,122.322645616245)) ;
#87676 = CARTESIAN_POINT('Ctrl Pts',(-20.6231827987995,42.3805934439305,122.517917638285)) ;
#87677 = CARTESIAN_POINT('Ctrl Pts',(-20.7606195436203,42.3906565580947,122.743793366782)) ;
#87678 = CARTESIAN_POINT('Ctrl Pts',(-20.8549120164977,42.4004962038111,122.984609559958)) ;
#87679 = CARTESIAN_POINT('Ctrl Pts',(-20.9074321966083,42.4105593713669,123.243754099235)) ;
#87680 = CARTESIAN_POINT('Ctrl Pts',(-20.9138270218801,42.4204536271617,123.503714919927)) ;
#87681 = CARTESIAN_POINT('Ctrl Pts',(-20.8755128410189,42.4303954056214,123.762117252756)) ;
#87682 = CARTESIAN_POINT('Ctrl Pts',(-20.7924756140901,42.4403980984516,124.011553585451)) ;
#87683 = CARTESIAN_POINT('Ctrl Pts',(-20.6666672130897,42.4504321204054,124.243274149404)) ;
#87684 = CARTESIAN_POINT('Ctrl Pts',(-20.5058796969663,42.4602799114944,124.446064360107)) ;
#87685 = CARTESIAN_POINT('Ctrl Pts',(-20.3101026092512,42.4702614360435,124.62060077918)) ;
#87686 = CARTESIAN_POINT('Ctrl Pts',(-20.0876687178098,42.4802106595344,124.758029297087)) ;
#87687 = CARTESIAN_POINT('Ctrl Pts',(-19.8436792195384,42.490208315751,124.855531589647)) ;
#87688 = CARTESIAN_POINT('Ctrl Pts',(-19.5853068270162,42.500248528806,124.908912389975)) ;
#87689 = CARTESIAN_POINT('Ctrl Pts',(-19.3271481560831,42.5100765760823,124.917023207503)) ;
#87690 = CARTESIAN_POINT('Ctrl Pts',(-19.065587620381,42.5201309231147,124.879749670527)) ;
#87691 = CARTESIAN_POINT('Ctrl Pts',(-18.8174156782774,42.5300720594432,124.798125360101)) ;
#87692 = CARTESIAN_POINT('Ctrl Pts',(-18.5876622498009,42.5399762925229,124.675821006536)) ;
#87693 = CARTESIAN_POINT('Ctrl Pts',(-18.3798098223478,42.5500229893665,124.513062959193)) ;
#87694 = CARTESIAN_POINT('Ctrl Pts',(-18.205809991047,42.5599185406468,124.319751471792)) ;
#87695 = CARTESIAN_POINT('Ctrl Pts',(-18.0657424005529,42.5699806184863,124.095520805029)) ;
#87696 = CARTESIAN_POINT('Ctrl Pts',(-17.9687323982393,42.5798233275824,123.855713961264)) ;
#87697 = CARTESIAN_POINT('Ctrl Pts',(-17.9134293922222,42.5898140598208,123.599092869816)) ;
#87698 = CARTESIAN_POINT('Ctrl Pts',(-17.9036266135817,42.5997420850496,123.338364905447)) ;
#87699 = CARTESIAN_POINT('Ctrl Pts',(-17.9390160350888,42.6097302317001,123.078277461847)) ;
#87700 = CARTESIAN_POINT('Ctrl Pts',(-18.0197861525379,42.6197652495401,122.827237976155)) ;
#87701 = CARTESIAN_POINT('Ctrl Pts',(-18.140582591483,42.6296300466453,122.597876275323)) ;
#87702 = CARTESIAN_POINT('Ctrl Pts',(-18.3003156640756,42.6395907790014,122.390498248251)) ;
#87703 = CARTESIAN_POINT('Ctrl Pts',(-18.4953259743341,42.6496242413984,122.213054154998)) ;
#87704 = CARTESIAN_POINT('Ctrl Pts',(-18.7147012146566,42.6595097756098,122.073852925735)) ;
#87705 = CARTESIAN_POINT('Ctrl Pts',(-18.9592157983849,42.6695746162898,121.973094770652)) ;
#87706 = CARTESIAN_POINT('Ctrl Pts',(-19.211976927808,42.6794227480187,121.917420334612)) ;
#87707 = CARTESIAN_POINT('Ctrl Pts',(-19.4752162394926,42.6894502450088,121.905599515675)) ;
#87708 = CARTESIAN_POINT('Ctrl Pts',(-19.7364643783176,42.6994786970539,121.940363154748)) ;
#87709 = CARTESIAN_POINT('Ctrl Pts',(-19.983240895575,42.709323963618,122.018027966902)) ;
#87710 = CARTESIAN_POINT('Ctrl Pts',(-20.2165165477863,42.7193146365589,122.138509322655)) ;
#87711 = CARTESIAN_POINT('Ctrl Pts',(-20.42595149829,42.7293525186474,122.298877797518)) ;
#87712 = CARTESIAN_POINT('Ctrl Pts',(-20.6012619502332,42.739196889087,122.489133616188)) ;
#87713 = CARTESIAN_POINT('Ctrl Pts',(-20.7432777778674,42.7491817164824,122.709727782596)) ;
#87714 = CARTESIAN_POINT('Ctrl Pts',(-20.8445084625415,42.7591211618877,122.950553007713)) ;
#87715 = CARTESIAN_POINT('Ctrl Pts',(-20.902884175201,42.7691611661736,123.207827740318)) ;
#87716 = CARTESIAN_POINT('Ctrl Pts',(-20.9156867364475,42.7790482753592,123.467365079687)) ;
#87717 = CARTESIAN_POINT('Ctrl Pts',(-20.8831915581267,42.7890483352617,123.728098704159)) ;
#87718 = CARTESIAN_POINT('Ctrl Pts',(-20.8067445599132,42.7989657511764,123.977299323762)) ;
#87719 = CARTESIAN_POINT('Ctrl Pts',(-20.686612406926,42.8090125659172,124.212363180922)) ;
#87720 = CARTESIAN_POINT('Ctrl Pts',(-20.5303690658562,42.8188880431139,124.419630089936)) ;
#87721 = CARTESIAN_POINT('Ctrl Pts',(-20.337202917031,42.8289441388351,124.599902985176)) ;
#87722 = CARTESIAN_POINT('Ctrl Pts',(-20.1192329290402,42.8388373008502,124.741697871364)) ;
#87723 = CARTESIAN_POINT('Ctrl Pts',(-19.8759728300273,42.8488995368728,124.845270931614)) ;
#87724 = CARTESIAN_POINT('Ctrl Pts',(-19.6239615863206,42.8587440025017,124.903774649878)) ;
#87725 = CARTESIAN_POINT('Ctrl Pts',(-19.3626527477167,42.8687040952058,124.91873716026)) ;
#87726 = CARTESIAN_POINT('Ctrl Pts',(-19.1007442432168,42.8787423841869,124.887345479684)) ;
#87727 = CARTESIAN_POINT('Ctrl Pts',(-18.852219395114,42.8886157072931,124.812672988231)) ;
#87728 = CARTESIAN_POINT('Ctrl Pts',(-18.6158652448163,42.8986888913782,124.693587821864)) ;
#87729 = CARTESIAN_POINT('Ctrl Pts',(-18.408809846254,42.9085094036661,124.539447907291)) ;
#87730 = CARTESIAN_POINT('Ctrl Pts',(-18.2269164681603,42.9185873997819,124.347038540938)) ;
#87731 = CARTESIAN_POINT('Ctrl Pts',(-18.0843140642102,42.9284414747652,124.130813462835)) ;
#87732 = CARTESIAN_POINT('Ctrl Pts',(-17.9790106190544,42.9385053563489,123.888269164773)) ;
#87733 = CARTESIAN_POINT('Ctrl Pts',(-17.9185491680014,42.9483887823227,123.635632007947)) ;
#87734 = CARTESIAN_POINT('Ctrl Pts',(-17.9022737750403,42.9583893862437,123.373377146627)) ;
#87735 = CARTESIAN_POINT('Ctrl Pts',(-17.9313895259165,42.9683091705816,123.114278441424)) ;
#87736 = CARTESIAN_POINT('Ctrl Pts',(-18.0060320164047,42.9783565209384,122.861060709944)) ;
#87737 = CARTESIAN_POINT('Ctrl Pts',(-18.1212870190588,42.9882338631727,122.628427841327)) ;
#87738 = CARTESIAN_POINT('Ctrl Pts',(-18.2781351229889,42.9983037442474,122.415360927794)) ;
#87739 = CARTESIAN_POINT('Ctrl Pts',(-18.4649150055318,43.008133449449,122.2368543242)) ;
#87740 = CARTESIAN_POINT('Ctrl Pts',(-18.6847596765535,43.0182001106154,122.089792158768)) ;
#87741 = CARTESIAN_POINT('Ctrl Pts',(-18.9226931773935,43.0280903324827,121.985125306975)) ;
#87742 = CARTESIAN_POINT('Ctrl Pts',(-19.1776048761138,43.0380825085929,121.922176627254)) ;
#87743 = CARTESIAN_POINT('Ctrl Pts',(-19.4388303799402,43.0480453387055,121.904745061404)) ;
#87744 = CARTESIAN_POINT('Ctrl Pts',(-19.697682792419,43.0579495511058,121.932114404861)) ;
#87745 = CARTESIAN_POINT('Ctrl Pts',(-19.951683312586,43.0680102651937,122.005359612903)) ;
#87746 = CARTESIAN_POINT('Ctrl Pts',(-20.1841105631504,43.0778497681765,122.118753970002)) ;
#87747 = CARTESIAN_POINT('Ctrl Pts',(-20.3982269814349,43.0879159067429,122.274016136349)) ;
#87748 = CARTESIAN_POINT('Ctrl Pts',(-20.5787646114016,43.0977984212289,122.460756397599)) ;
#87749 = CARTESIAN_POINT('Ctrl Pts',(-20.7261333194938,43.1077907205845,122.678042925821)) ;
#87750 = CARTESIAN_POINT('Ctrl Pts',(-20.833206366185,43.1177437875379,122.916721805344)) ;
#87751 = CARTESIAN_POINT('Ctrl Pts',(-20.897614117175,43.1277784957431,123.172416207021)) ;
#87752 = CARTESIAN_POINT('Ctrl Pts',(-20.9165610195701,43.1376667166473,123.43159275742)) ;
#87753 = CARTESIAN_POINT('Ctrl Pts',(-20.8903677843384,43.1476611396777,123.692911928234)) ;
#87754 = CARTESIAN_POINT('Ctrl Pts',(-20.8194444690435,43.1576064791239,123.944458675462)) ;
#87755 = CARTESIAN_POINT('Ctrl Pts',(-20.7063781227187,43.1675538237352,124.180161559428)) ;
#87756 = CARTESIAN_POINT('Ctrl Pts',(-20.5523346077461,43.1776017191462,124.394608128497)) ;
#87757 = CARTESIAN_POINT('Ctrl Pts',(-20.3673072274807,43.1874493646256,124.575539263631)) ;
#87758 = CARTESIAN_POINT('Ctrl Pts',(-20.1516760965307,43.1974110785396,124.723955111939)) ;
#87759 = CARTESIAN_POINT('Ctrl Pts',(-19.9117864879595,43.2074397028305,124.833114513842)) ;
#87760 = CARTESIAN_POINT('Ctrl Pts',(-19.6596450451628,43.2173500634872,124.898260239512)) ;
#87761 = CARTESIAN_POINT('Ctrl Pts',(-19.3994169455173,43.2272847620605,124.919374953537)) ;
#87762 = CARTESIAN_POINT('Ctrl Pts',(-19.1367199893783,43.2373265869147,124.894463864514)) ;
#87763 = CARTESIAN_POINT('Ctrl Pts',(-18.886225085537,43.2472111606591,124.825627198555)) ;
#87764 = CARTESIAN_POINT('Ctrl Pts',(-18.6486227140851,43.2572130100223,124.713331619215)) ;
#87765 = CARTESIAN_POINT('Ctrl Pts',(-18.4357298701924,43.2671323115963,124.562855492148)) ;
#87766 = CARTESIAN_POINT('Ctrl Pts',(-18.2499252216547,43.2771764199416,124.375414816484)) ;
#87767 = CARTESIAN_POINT('Ctrl Pts',(-18.1017967666107,43.2870608433839,124.162024125329)) ;
#87768 = CARTESIAN_POINT('Ctrl Pts',(-17.9909876140739,43.2970772052933,123.923254596581)) ;
#87769 = CARTESIAN_POINT('Ctrl Pts',(-17.923859840719,43.3071138607987,123.668202194077)) ;
#87770 = CARTESIAN_POINT('Ctrl Pts',(-17.9017809512743,43.316943990988,123.410789908408)) ;
#87771 = CARTESIAN_POINT('Ctrl Pts',(-17.9252094807461,43.3270200440779,123.14709156434)) ;
#87772 = CARTESIAN_POINT('Ctrl Pts',(-17.9924299188192,43.3368722732637,122.897006470178)) ;
#87773 = CARTESIAN_POINT('Ctrl Pts',(-18.1042679823455,43.346945481063,122.657125718903)) ;
#87774 = CARTESIAN_POINT('Ctrl Pts',(-18.2526600247285,43.3567869924144,122.445286955059)) ;
#87775 = CARTESIAN_POINT('Ctrl Pts',(-18.4370833480714,43.3667479304519,122.259535607649)) ;
#87776 = CARTESIAN_POINT('Ctrl Pts',(-18.6529137116503,43.3767857923769,122.107894632329)) ;
#87777 = CARTESIAN_POINT('Ctrl Pts',(-18.8877318802292,43.386659978374,121.997399835187)) ;
#87778 = CARTESIAN_POINT('Ctrl Pts',(-19.1430767424442,43.3967301379519,121.928047356041)) ;
#87779 = CARTESIAN_POINT('Ctrl Pts',(-19.4003939023348,43.4065618853777,121.904482946936)) ;
#87780 = CARTESIAN_POINT('Ctrl Pts',(-19.6632619536359,43.416597965449,121.925714449018)) ;
#87781 = CARTESIAN_POINT('Ctrl Pts',(-19.9178244791952,43.4266150123015,121.992789588399)) ;
#87782 = CARTESIAN_POINT('Ctrl Pts',(-20.1538536760543,43.4364972704681,122.101114447307)) ;
#87783 = CARTESIAN_POINT('Ctrl Pts',(-20.3699131764678,43.4464849532645,122.250085365114)) ;
#87784 = CARTESIAN_POINT('Ctrl Pts',(-20.5562534234135,43.4564316099812,122.433448480984)) ;
#87785 = CARTESIAN_POINT('Ctrl Pts',(-20.7093464656126,43.4664886680613,122.648845014339)) ;
#87786 = CARTESIAN_POINT('Ctrl Pts',(-20.8203630654668,43.4763068476108,122.881767028925)) ;
#87787 = CARTESIAN_POINT('Ctrl Pts',(-20.8914610512173,43.4863427820498,123.135729585425)) ;
#87788 = CARTESIAN_POINT('Ctrl Pts',(-20.9166029199042,43.4963674364788,123.397974203455)) ;
#87789 = CARTESIAN_POINT('Ctrl Pts',(-20.8967578932332,43.5062194560583,123.656117782256)) ;
#87790 = CARTESIAN_POINT('Ctrl Pts',(-20.831881508292,43.5162103697732,123.910494310723)) ;
#87791 = CARTESIAN_POINT('Ctrl Pts',(-20.7247399963963,43.5261283586128,124.148122891889)) ;
#87792 = CARTESIAN_POINT('Ctrl Pts',(-20.5764179652717,43.5361564693436,124.365922998669)) ;
#87793 = CARTESIAN_POINT('Ctrl Pts',(-20.3952122093275,43.546041667252,124.552066450949)) ;
#87794 = CARTESIAN_POINT('Ctrl Pts',(-20.1825938294097,43.55603094252,124.706038954203)) ;
#87795 = CARTESIAN_POINT('Ctrl Pts',(-19.9449996926765,43.5660724006895,124.820834858962)) ;
#87796 = CARTESIAN_POINT('Ctrl Pts',(-19.6965069343808,43.5759038644778,124.89159240592)) ;
#87797 = CARTESIAN_POINT('Ctrl Pts',(-19.4350698137697,43.5859087967817,124.919173839307)) ;
#87798 = CARTESIAN_POINT('Ctrl Pts',(-19.1732351295058,43.5958951606764,124.900827612683)) ;
#87799 = CARTESIAN_POINT('Ctrl Pts',(-18.9175770787377,43.6059247895623,124.836838031948)) ;
#87800 = CARTESIAN_POINT('Ctrl Pts',(-18.6804371598066,43.6158000116707,124.731369996855)) ;
#87801 = CARTESIAN_POINT('Ctrl Pts',(-18.4623477415022,43.6258012240678,124.584774106996)) ;
#87802 = CARTESIAN_POINT('Ctrl Pts',(-18.2745444168899,43.6357098033033,124.404343207406)) ;
#87803 = CARTESIAN_POINT('Ctrl Pts',(-18.1187722259552,43.6457646558593,124.190964881095)) ;
#87804 = CARTESIAN_POINT('Ctrl Pts',(-18.004380821327,43.6556232381341,123.958462580893)) ;
#87805 = CARTESIAN_POINT('Ctrl Pts',(-17.9304301319305,43.6656913675768,123.704467954817)) ;
#87806 = CARTESIAN_POINT('Ctrl Pts',(-17.9023257120292,43.6755468392659,123.446983659363)) ;
#87807 = CARTESIAN_POINT('Ctrl Pts',(-17.9188088681527,43.6855416876521,123.18485588981)) ;
#87808 = CARTESIAN_POINT('Ctrl Pts',(-17.9813360998204,43.6955729844366,122.928761468334)) ;
#87809 = CARTESIAN_POINT('Ctrl Pts',(-18.0852611565216,43.7054395206467,122.691208548975)) ;
#87810 = CARTESIAN_POINT('Ctrl Pts',(-18.2302389701534,43.7154269436075,122.472461402679)) ;
#87811 = CARTESIAN_POINT('Ctrl Pts',(-18.4101746479847,43.7253718826273,122.282878179321)) ;
#87812 = CARTESIAN_POINT('Ctrl Pts',(-18.6224381752842,43.7354167684873,122.125988815331)) ;
#87813 = CARTESIAN_POINT('Ctrl Pts',(-18.8545304610227,43.7452853035735,122.010266829846)) ;
#87814 = CARTESIAN_POINT('Ctrl Pts',(-19.1054170228572,43.7552511715802,121.935180988231)) ;
#87815 = CARTESIAN_POINT('Ctrl Pts',(-19.3670753403128,43.7652738190327,121.904915997745)) ;
#87816 = CARTESIAN_POINT('Ctrl Pts',(-19.6273895696262,43.7751974580403,121.920314786866)) ;
#87817 = CARTESIAN_POINT('Ctrl Pts',(-19.8817360875412,43.785140183046,121.980191368914)) ;
#87818 = CARTESIAN_POINT('Ctrl Pts',(-20.1241540955357,43.7951857890979,122.084667591629)) ;
#87819 = CARTESIAN_POINT('Ctrl Pts',(-20.3408919295591,43.805047211619,122.226772581987)) ;
#87820 = CARTESIAN_POINT('Ctrl Pts',(-20.5324564346371,43.8150407800682,122.406363357882)) ;
#87821 = CARTESIAN_POINT('Ctrl Pts',(-20.6890092975618,43.8249662508235,122.615035530979)) ;
#87822 = CARTESIAN_POINT('Ctrl Pts',(-20.8081450016785,43.8349939247794,122.850047539463)) ;
#87823 = CARTESIAN_POINT('Ctrl Pts',(-20.8838536120231,43.8448811028211,123.098633773252)) ;
#87824 = CARTESIAN_POINT('Ctrl Pts',(-20.9158727010176,43.8549094821892,123.360180929265)) ;
#87825 = CARTESIAN_POINT('Ctrl Pts',(-20.9023154130468,43.8648037249107,123.61987110098)) ;
#87826 = CARTESIAN_POINT('Ctrl Pts',(-20.8237526627658,43.8781566415616,123.961832644244)) ;
#87827 = CARTESIAN_POINT('Ctrl Pts',(-20.659605419344,43.8913591593083,124.272026060151)) ;
#87828 = CARTESIAN_POINT('Ctrl Pts',(-20.4209894341323,43.9047150645893,124.529371523142)) ;
#87829 = CARTESIAN_POINT('Ctrl Pts',(-20.2138465893309,43.9146117132271,124.686685290461)) ;
#87830 = CARTESIAN_POINT('Ctrl Pts',(-19.9790841361338,43.9246598512796,124.807515218539)) ;
#87831 = CARTESIAN_POINT('Ctrl Pts',(-19.7308190710791,43.9345508114574,124.884524562432)) ;
#87832 = CARTESIAN_POINT('Ctrl Pts',(-19.4703839376697,43.9445436473341,124.918248825918)) ;
#87833 = CARTESIAN_POINT('Ctrl Pts',(-19.2068845324014,43.9545827423357,124.905579235426)) ;
#87834 = CARTESIAN_POINT('Ctrl Pts',(-18.9545857300593,43.9644200981869,124.849099649171)) ;
#87835 = CARTESIAN_POINT('Ctrl Pts',(-18.6296690897415,43.9778130461176,124.713956490856)) ;
#87836 = CARTESIAN_POINT('Ctrl Pts',(-18.3520981743961,43.9909797225445,124.500694921199)) ;
#87837 = CARTESIAN_POINT('Ctrl Pts',(-18.1378620138643,44.0043645039513,124.221797775786)) ;
#87838 = CARTESIAN_POINT('Ctrl Pts',(-18.0179672616378,44.0142262865952,123.991995123024)) ;
#87839 = CARTESIAN_POINT('Ctrl Pts',(-17.9383259095293,44.0242254345482,123.741642443432)) ;
#87840 = CARTESIAN_POINT('Ctrl Pts',(-17.9034476011342,44.0341282271653,123.483699776961)) ;
#87841 = CARTESIAN_POINT('Ctrl Pts',(-17.9141092543276,44.0441778070562,123.219886940427)) ;
#87842 = CARTESIAN_POINT('Ctrl Pts',(-17.987359893705,44.0573648808657,122.881047522662)) ;
#87843 = CARTESIAN_POINT('Ctrl Pts',(-18.1910325351083,44.0741176708369,122.485294726917)) ;
#87844 = CARTESIAN_POINT('Ctrl Pts',(-18.5127079665964,44.0906063229316,122.187409946864)) ;
#87845 = CARTESIAN_POINT('Ctrl Pts',(-18.8227881728284,44.103963149115,122.02310778574)) ;
#87846 = CARTESIAN_POINT('Ctrl Pts',(-19.0702563997621,44.1138595339929,121.942965399191)) ;
#87847 = CARTESIAN_POINT('Ctrl Pts',(-19.3306048043616,44.1238660485134,121.906491121348)) ;
#87848 = CARTESIAN_POINT('Ctrl Pts',(-19.6771635039031,44.1370561720298,121.917876124668)) ;
#87849 = CARTESIAN_POINT('Ctrl Pts',(-20.1033013954012,44.1538227331793,122.047686667172)) ;
#87850 = CARTESIAN_POINT('Ctrl Pts',(-20.5238929989773,44.1736072218874,122.363542810504)) ;
#87851 = CARTESIAN_POINT('Ctrl Pts',(-20.815011621917,44.1935526694839,122.806412748844)) ;
#87852 = CARTESIAN_POINT('Ctrl Pts',(-20.9368621718498,44.2134643316398,123.321424916447)) ;
#87853 = CARTESIAN_POINT('Ctrl Pts',(-20.8768657552607,44.2333565236587,123.846793390736)) ;
#87854 = CARTESIAN_POINT('Ctrl Pts',(-20.6387805843268,44.2533976542133,124.323200523711)) ;
#87855 = CARTESIAN_POINT('Ctrl Pts',(-20.2567572002547,44.2732159888289,124.686031568202)) ;
#87856 = CARTESIAN_POINT('Ctrl Pts',(-19.7707167595738,44.2931885540485,124.899018477373)) ;
#87857 = CARTESIAN_POINT('Ctrl Pts',(-19.243012073421,44.3130777702201,124.933377526462)) ;
#87858 = CARTESIAN_POINT('Ctrl Pts',(-18.7322499924567,44.3331013445428,124.784342715249)) ;
#87859 = CARTESIAN_POINT('Ctrl Pts',(-18.3074523247711,44.352898507631,124.473689351128)) ;
#87860 = CARTESIAN_POINT('Ctrl Pts',(-18.0107208479656,44.3728640014548,124.033892370887)) ;
#87861 = CARTESIAN_POINT('Ctrl Pts',(-17.8825301084476,44.3928177091962,123.519135613177)) ;
#87862 = CARTESIAN_POINT('Ctrl Pts',(-17.9375131053142,44.4127250859228,122.993014954846)) ;
#87863 = CARTESIAN_POINT('Ctrl Pts',(-18.1669119070672,44.4325772974714,122.517754743088)) ;
#87864 = CARTESIAN_POINT('Ctrl Pts',(-18.5491999521954,44.4526496844171,122.145668046979)) ;
#87865 = CARTESIAN_POINT('Ctrl Pts',(-19.0301389700753,44.4724875540574,121.9295612266)) ;
#87866 = CARTESIAN_POINT('Ctrl Pts',(-19.556112431027,44.4923382086105,121.888236492257)) ;
#87867 = CARTESIAN_POINT('Ctrl Pts',(-20.0695268056747,44.512390142951,122.031046366895)) ;
#87868 = CARTESIAN_POINT('Ctrl Pts',(-20.4987446170897,44.532223330517,122.337261350157)) ;
#87869 = CARTESIAN_POINT('Ctrl Pts',(-20.7998380093603,44.5521525427477,122.772809047979)) ;
#87870 = CARTESIAN_POINT('Ctrl Pts',(-20.9346380609838,44.5720375079621,123.284047944812)) ;
#87871 = CARTESIAN_POINT('Ctrl Pts',(-20.8856425940297,44.5921112491067,123.815212598448)) ;
#87872 = CARTESIAN_POINT('Ctrl Pts',(-20.6614851629729,44.6119044308871,124.291227274791)) ;
#87873 = CARTESIAN_POINT('Ctrl Pts',(-20.2863772074548,44.6318671388898,124.666405427892)) ;
#87874 = CARTESIAN_POINT('Ctrl Pts',(-19.8046798286043,44.6518500906322,124.8901432235)) ;
#87875 = CARTESIAN_POINT('Ctrl Pts',(-19.2801648941078,44.6716607104044,124.936716143029)) ;
#87876 = CARTESIAN_POINT('Ctrl Pts',(-18.7667918531497,44.6916444264373,124.800971420717)) ;
#87877 = CARTESIAN_POINT('Ctrl Pts',(-18.332633623527,44.7115258903346,124.499523849295)) ;
#87878 = CARTESIAN_POINT('Ctrl Pts',(-18.0261041134591,44.731481220179,124.066823654643)) ;
#87879 = CARTESIAN_POINT('Ctrl Pts',(-17.8857718639008,44.7513566809845,123.557460531844)) ;
#87880 = CARTESIAN_POINT('Ctrl Pts',(-17.9275871464799,44.771341001036,123.028016369146)) ;
#87881 = CARTESIAN_POINT('Ctrl Pts',(-18.1472823916272,44.7912690338256,122.54594681577)) ;
#87882 = CARTESIAN_POINT('Ctrl Pts',(-18.4563072638141,44.8078777957654,122.230852995871)) ;
#87883 = CARTESIAN_POINT('Ctrl Pts',(-18.7544344166136,44.8210654344555,122.054104346629)) ;
#87884 = CARTESIAN_POINT('Ctrl Pts',(-18.9997577413404,44.8310518688156,121.960933276629)) ;
#87885 = CARTESIAN_POINT('Ctrl Pts',(-19.2582000487417,44.841061242775,121.911919172374)) ;
#87886 = CARTESIAN_POINT('Ctrl Pts',(-19.6074259157018,44.8543512763403,121.90718231146)) ;
#87887 = CARTESIAN_POINT('Ctrl Pts',(-20.0350744145889,44.8709452640027,122.015110092288)) ;
#87888 = CARTESIAN_POINT('Ctrl Pts',(-20.4010334172279,44.8875775192782,122.263044894367)) ;
#87889 = CARTESIAN_POINT('Ctrl Pts',(-20.6289076195677,44.9008199029461,122.52606867887)) ;
#87890 = CARTESIAN_POINT('Ctrl Pts',(-20.7634193394176,44.9107341111735,122.749205301052)) ;
#87891 = CARTESIAN_POINT('Ctrl Pts',(-20.8581992855926,44.9207907504452,122.995881649194)) ;
#87892 = CARTESIAN_POINT('Ctrl Pts',(-20.9079626866539,44.9306365568653,123.249811042525)) ;
#87893 = CARTESIAN_POINT('Ctrl Pts',(-20.9134321153544,44.9406815564985,123.513714183674)) ;
#87894 = CARTESIAN_POINT('Ctrl Pts',(-20.8594529735354,44.9539625788713,123.85851431483)) ;
#87895 = CARTESIAN_POINT('Ctrl Pts',(-20.7185138341195,44.9671600253959,124.179729076087)) ;
#87896 = CARTESIAN_POINT('Ctrl Pts',(-20.4978542341181,44.9805743232029,124.454653630732)) ;
#87897 = CARTESIAN_POINT('Ctrl Pts',(-20.3035482186063,44.9904133886056,124.625258093541)) ;
#87898 = CARTESIAN_POINT('Ctrl Pts',(-20.0797292255048,45.0003965948833,124.762068121514)) ;
#87899 = CARTESIAN_POINT('Ctrl Pts',(-19.8362653995539,45.0103478297961,124.857563683997)) ;
#87900 = CARTESIAN_POINT('Ctrl Pts',(-19.5787021577369,45.0203488294977,124.90990497468)) ;
#87901 = CARTESIAN_POINT('Ctrl Pts',(-19.3151704808666,45.0303801752851,124.916336383632)) ;
#87902 = CARTESIAN_POINT('Ctrl Pts',(-19.059076565559,45.0402339399901,124.877961736359)) ;
#87903 = CARTESIAN_POINT('Ctrl Pts',(-18.8104579041759,45.0502045936584,124.795331193507)) ;
#87904 = CARTESIAN_POINT('Ctrl Pts',(-18.5792936637788,45.0602018373156,124.670414452979)) ;
#87905 = CARTESIAN_POINT('Ctrl Pts',(-18.372843216216,45.0702352932598,124.506439042019)) ;
#87906 = CARTESIAN_POINT('Ctrl Pts',(-18.2007560512662,45.0800907975602,124.312851502277)) ;
#87907 = CARTESIAN_POINT('Ctrl Pts',(-18.0626513107753,45.0900902338463,124.08934966355)) ;
#87908 = CARTESIAN_POINT('Ctrl Pts',(-17.966160872868,45.0999846933622,123.847847223486)) ;
#87909 = CARTESIAN_POINT('Ctrl Pts',(-17.9122601551696,45.1100478128138,123.588997131048)) ;
#87910 = CARTESIAN_POINT('Ctrl Pts',(-17.9040157128179,45.1198874472258,123.330510182851)) ;
#87911 = CARTESIAN_POINT('Ctrl Pts',(-17.9412701233928,45.1299506547116,123.068734224408)) ;
#87912 = CARTESIAN_POINT('Ctrl Pts',(-18.0222577929814,45.1398447620908,122.821630638561)) ;
#87913 = CARTESIAN_POINT('Ctrl Pts',(-18.1448705736183,45.1497870942832,122.590953885684)) ;
#87914 = CARTESIAN_POINT('Ctrl Pts',(-18.3065622324811,45.1597877205982,122.383723321206)) ;
#87915 = CARTESIAN_POINT('Ctrl Pts',(-18.502862990913,45.1698294548801,122.207402005079)) ;
#87916 = CARTESIAN_POINT('Ctrl Pts',(-18.7217059912546,45.1796548808292,122.070339801105)) ;
#87917 = CARTESIAN_POINT('Ctrl Pts',(-18.966474765151,45.1897117073569,121.970725354272)) ;
#87918 = CARTESIAN_POINT('Ctrl Pts',(-19.2216074988033,45.1996391404784,121.916190939513)) ;
#87919 = CARTESIAN_POINT('Ctrl Pts',(-19.4828944941186,45.2095891328847,121.906015436364)) ;
#87920 = CARTESIAN_POINT('Ctrl Pts',(-19.7446272926651,45.2196443339587,121.942195083293)) ;
#87921 = CARTESIAN_POINT('Ctrl Pts',(-19.9904565700812,45.229466608011,122.020960921677)) ;
#87922 = CARTESIAN_POINT('Ctrl Pts',(-20.2244926759389,45.2395225019702,122.143638300963)) ;
#87923 = CARTESIAN_POINT('Ctrl Pts',(-20.4310152546762,45.2494632238153,122.303624668569)) ;
#87924 = CARTESIAN_POINT('Ctrl Pts',(-20.6065787562621,45.2593675679019,122.495779589979)) ;
#87925 = CARTESIAN_POINT('Ctrl Pts',(-20.7479598031112,45.2694142352014,122.718723494218)) ;
#87926 = CARTESIAN_POINT('Ctrl Pts',(-20.847214873449,45.2793097936513,122.959126759267)) ;
#87927 = CARTESIAN_POINT('Ctrl Pts',(-20.9041452558885,45.289371872356,123.217307547921)) ;
#87928 = CARTESIAN_POINT('Ctrl Pts',(-20.9152880545128,45.2992145708218,123.475752573775)) ;
#87929 = CARTESIAN_POINT('Ctrl Pts',(-20.8815017658848,45.3092053447163,123.736083691839)) ;
#87930 = CARTESIAN_POINT('Ctrl Pts',(-20.803464341165,45.3191332139512,123.985045208885)) ;
#87931 = CARTESIAN_POINT('Ctrl Pts',(-20.6830597025419,45.329121942921,124.218310172985)) ;
#87932 = CARTESIAN_POINT('Ctrl Pts',(-20.5228027489551,45.3391613449048,124.427867674991)) ;
#87933 = CARTESIAN_POINT('Ctrl Pts',(-20.3327730605954,45.3490015126416,124.603267061586)) ;
#87934 = CARTESIAN_POINT('Ctrl Pts',(-20.1108060666027,45.3590497230161,124.746272176201)) ;
#87935 = CARTESIAN_POINT('Ctrl Pts',(-19.8696532867426,45.3689968933038,124.847160076547)) ;
#87936 = CARTESIAN_POINT('Ctrl Pts',(-19.6157459454995,45.3789077415589,124.90519559881)) ;
#87937 = CARTESIAN_POINT('Ctrl Pts',(-19.3518125734357,45.3889640692367,124.918205064877)) ;
#87938 = CARTESIAN_POINT('Ctrl Pts',(-19.0949419766038,45.3988144820052,124.886084607511)) ;
#87939 = CARTESIAN_POINT('Ctrl Pts',(-18.8429458077784,45.4088413678389,124.809102515911)) ;
#87940 = CARTESIAN_POINT('Ctrl Pts',(-18.6084007715185,45.4188699834697,124.688897924885)) ;
#87941 = CARTESIAN_POINT('Ctrl Pts',(-18.4018578835291,45.4287152068472,124.533108889477)) ;
#87942 = CARTESIAN_POINT('Ctrl Pts',(-18.2223677576914,45.4387058889488,124.341493091567)) ;
#87943 = CARTESIAN_POINT('Ctrl Pts',(-18.0786949591788,45.4487437775813,124.120270887316)) ;
#87944 = CARTESIAN_POINT('Ctrl Pts',(-17.9771820255855,45.4585881126844,123.882309246234)) ;
#87945 = CARTESIAN_POINT('Ctrl Pts',(-17.9171992662685,45.4685730748819,123.62689961788)) ;
#87946 = CARTESIAN_POINT('Ctrl Pts',(-17.9024172623288,45.4785120164153,123.366094931073)) ;
#87947 = CARTESIAN_POINT('Ctrl Pts',(-17.9335377045302,45.4885539013867,123.104071689988)) ;
#87948 = CARTESIAN_POINT('Ctrl Pts',(-18.0083583615695,45.498440449295,122.855243316233)) ;
#87949 = CARTESIAN_POINT('Ctrl Pts',(-18.1261441567159,45.508434374795,122.620545045069)) ;
#87950 = CARTESIAN_POINT('Ctrl Pts',(-18.2819302055561,45.5183704659215,122.410950315548)) ;
#87951 = CARTESIAN_POINT('Ctrl Pts',(-18.4735027254418,45.5283997349014,122.229995789476)) ;
#87952 = CARTESIAN_POINT('Ctrl Pts',(-18.690241481066,45.5382821174607,122.086859617476)) ;
#87953 = CARTESIAN_POINT('Ctrl Pts',(-18.9325349471609,45.5483346345486,121.981703543276)) ;
#87954 = CARTESIAN_POINT('Ctrl Pts',(-19.185413729496,45.5582287553725,121.921034104185)) ;
#87955 = CARTESIAN_POINT('Ctrl Pts',(-19.4493049697019,45.5682907347929,121.904866941073)) ;
#87956 = CARTESIAN_POINT('Ctrl Pts',(-19.7063630081236,45.5781352680218,121.934093132553)) ;
#87957 = CARTESIAN_POINT('Ctrl Pts',(-19.9576058706028,45.5880953469281,122.007462571973)) ;
#87958 = CARTESIAN_POINT('Ctrl Pts',(-20.1938981415272,45.5981336235007,122.124711964626)) ;
#87959 = CARTESIAN_POINT('Ctrl Pts',(-20.4030909048024,45.6080070100386,122.278267729606)) ;
#87960 = CARTESIAN_POINT('Ctrl Pts',(-20.5859499300167,45.6180799528056,122.469592306891)) ;
#87961 = CARTESIAN_POINT('Ctrl Pts',(-20.7294620067179,45.6279013669339,122.684171707813)) ;
#87962 = CARTESIAN_POINT('Ctrl Pts',(-20.836469961144,45.6379759970062,122.92628036698)) ;
#87963 = CARTESIAN_POINT('Ctrl Pts',(-20.8984204591589,45.6478426343231,123.178089581566)) ;
#87964 = CARTESIAN_POINT('Ctrl Pts',(-20.9166539511471,45.6578661796949,123.440853736035)) ;
#87965 = CARTESIAN_POINT('Ctrl Pts',(-20.8883451902421,45.6678919312121,123.702810647261)) ;
#87966 = CARTESIAN_POINT('Ctrl Pts',(-20.8166655858108,45.6777455182215,123.951620064222)) ;
#87967 = CARTESIAN_POINT('Ctrl Pts',(-20.7020665615135,45.6877224784494,124.187438612339)) ;
#87968 = CARTESIAN_POINT('Ctrl Pts',(-20.5472320226334,45.6977436214779,124.400440473039)) ;
#87969 = CARTESIAN_POINT('Ctrl Pts',(-20.3607129644231,45.7076262274978,124.581203675269)) ;
#87970 = CARTESIAN_POINT('Ctrl Pts',(-20.1416041543845,45.7176946981305,124.729442692636)) ;
#87971 = CARTESIAN_POINT('Ctrl Pts',(-19.9058440233542,45.7275247813142,124.835139992)) ;
#87972 = CARTESIAN_POINT('Ctrl Pts',(-19.6494558792354,45.7375913409946,124.900127141566)) ;
#87973 = CARTESIAN_POINT('Ctrl Pts',(-19.3902123872049,45.7474815908238,124.919112847795)) ;
#87974 = CARTESIAN_POINT('Ctrl Pts',(-19.1289348372093,45.7574737565726,124.893103063459)) ;
#87975 = CARTESIAN_POINT('Ctrl Pts',(-18.8769434953996,45.7674366001687,124.822088336448)) ;
#87976 = CARTESIAN_POINT('Ctrl Pts',(-18.6421852615433,45.7773407689965,124.709652708434)) ;
#87977 = CARTESIAN_POINT('Ctrl Pts',(-18.4273528974957,45.7874016438908,124.555606852268)) ;
#87978 = CARTESIAN_POINT('Ctrl Pts',(-18.2462968796542,45.7972405472202,124.370967398921)) ;
#87979 = CARTESIAN_POINT('Ctrl Pts',(-18.0964786782735,45.8073089235941,124.152936536302)) ;
#87980 = CARTESIAN_POINT('Ctrl Pts',(-17.9888851621427,45.8171895402267,123.916582846629)) ;
#87981 = CARTESIAN_POINT('Ctrl Pts',(-17.9227453188288,45.8271807004557,123.662532284139)) ;
#87982 = CARTESIAN_POINT('Ctrl Pts',(-17.9017535244661,45.8371337738878,123.401780145108)) ;
#87983 = CARTESIAN_POINT('Ctrl Pts',(-17.9266404178476,45.8471696095005,123.139247618234)) ;
#87984 = CARTESIAN_POINT('Ctrl Pts',(-17.9955552265189,45.8570597362306,122.888631027566)) ;
#87985 = CARTESIAN_POINT('Ctrl Pts',(-18.1076934818933,45.8670519179999,122.651211136144)) ;
#87986 = CARTESIAN_POINT('Ctrl Pts',(-18.2587304245374,45.8769978579744,122.437900289644)) ;
#87987 = CARTESIAN_POINT('Ctrl Pts',(-18.4441704878577,45.8869450417339,122.253645296691)) ;
#87988 = CARTESIAN_POINT('Ctrl Pts',(-18.6611101574099,45.8969929800242,122.103131587065)) ;
#87989 = CARTESIAN_POINT('Ctrl Pts',(-18.8960272898149,45.9068406148377,121.994572618097)) ;
#87990 = CARTESIAN_POINT('Ctrl Pts',(-19.148898873225,45.9168023285357,121.926896838604)) ;
#87991 = CARTESIAN_POINT('Ctrl Pts',(-19.4114894160667,45.9268309643569,121.904333417555)) ;
#87992 = CARTESIAN_POINT('Ctrl Pts',(-19.6708912056313,45.9367412791087,121.92734461787)) ;
#87993 = CARTESIAN_POINT('Ctrl Pts',(-19.9231784918885,45.9466761497713,121.994557839022)) ;
#87994 = CARTESIAN_POINT('Ctrl Pts',(-20.1623713001247,45.9567173321731,122.10595274913)) ;
#87995 = CARTESIAN_POINT('Ctrl Pts',(-20.3754171966407,45.9666043036378,122.254712550326)) ;
#87996 = CARTESIAN_POINT('Ctrl Pts',(-20.5616853384859,45.9766037359004,122.440014625736)) ;
#87997 = CARTESIAN_POINT('Ctrl Pts',(-20.7119304588546,45.986523801157,122.65309125952)) ;
#87998 = CARTESIAN_POINT('Ctrl Pts',(-20.8242304858689,45.9965606537412,122.891731631287)) ;
#87999 = CARTESIAN_POINT('Ctrl Pts',(-20.8925312466949,46.0064733130812,123.143117767075)) ;
#88000 = CARTESIAN_POINT('Ctrl Pts',(-20.9169022735991,46.0164645249961,123.404558617935)) ;
#88001 = CARTESIAN_POINT('Ctrl Pts',(-20.8948119575861,46.0265061663992,123.667495012575)) ;
#88002 = CARTESIAN_POINT('Ctrl Pts',(-20.8294454785966,46.0363349606062,123.917414465479)) ;
#88003 = CARTESIAN_POINT('Ctrl Pts',(-20.7191022663443,46.0464113717275,124.158067817818)) ;
#88004 = CARTESIAN_POINT('Ctrl Pts',(-20.5720475565284,46.05626350477,124.371223090758)) ;
#88005 = CARTESIAN_POINT('Ctrl Pts',(-20.3863654461432,46.0663367391113,124.559830827429)) ;
#88006 = CARTESIAN_POINT('Ctrl Pts',(-20.1756244871386,46.0761782404379,124.709777652691)) ;
#88007 = CARTESIAN_POINT('Ctrl Pts',(-19.9396627498854,46.0861391920327,124.823081201135)) ;
#88008 = CARTESIAN_POINT('Ctrl Pts',(-19.6855248863959,46.0961770097533,124.893729687363)) ;
#88009 = CARTESIAN_POINT('Ctrl Pts',(-19.427262518452,46.1060513590104,124.919247547046)) ;
#88010 = CARTESIAN_POINT('Ctrl Pts',(-19.1634478041723,46.1161209097526,124.899133803632)) ;
#88011 = CARTESIAN_POINT('Ctrl Pts',(-18.9130319171502,46.1259549292612,124.835182189416)) ;
#88012 = CARTESIAN_POINT('Ctrl Pts',(-18.6724817634697,46.1359890838408,124.727205773932)) ;
#88013 = CARTESIAN_POINT('Ctrl Pts',(-18.4550722737311,46.1460050096632,124.57881549919)) ;
#88014 = CARTESIAN_POINT('Ctrl Pts',(-18.2689263313037,46.1558872648575,124.397725200321)) ;
#88015 = CARTESIAN_POINT('Ctrl Pts',(-18.1151695920916,46.1658760713684,124.185010592068)) ;
#88016 = CARTESIAN_POINT('Ctrl Pts',(-18.0009343743277,46.1758246386311,123.949804922474)) ;
#88017 = CARTESIAN_POINT('Ctrl Pts',(-17.9287986502812,46.1858794439331,123.695642276881)) ;
#88018 = CARTESIAN_POINT('Ctrl Pts',(-17.9021457183122,46.1956982271967,123.438981604419)) ;
#88019 = CARTESIAN_POINT('Ctrl Pts',(-17.920160334372,46.2057339995573,123.175874359375)) ;
#88020 = CARTESIAN_POINT('Ctrl Pts',(-17.984249977082,46.2157586985859,122.920340925666)) ;
#88021 = CARTESIAN_POINT('Ctrl Pts',(-18.0893591005861,46.225610701845,122.683731790801)) ;
#88022 = CARTESIAN_POINT('Ctrl Pts',(-18.2356413391738,46.2356016362422,122.465745544367)) ;
#88023 = CARTESIAN_POINT('Ctrl Pts',(-18.4161423749505,46.2455195586733,122.277688444646)) ;
#88024 = CARTESIAN_POINT('Ctrl Pts',(-18.6288192425981,46.2555479143556,122.122101309996)) ;
#88025 = CARTESIAN_POINT('Ctrl Pts',(-18.8618561314838,46.2654321988662,122.007348465011)) ;
#88026 = CARTESIAN_POINT('Ctrl Pts',(-19.1138378721338,46.2754248827741,121.933438370644)) ;
#88027 = CARTESIAN_POINT('Ctrl Pts',(-19.3758193880109,46.2854536197818,121.904757212364)) ;
#88028 = CARTESIAN_POINT('Ctrl Pts',(-19.6350724012937,46.2953390164107,121.921411675567)) ;
#88029 = CARTESIAN_POINT('Ctrl Pts',(-19.8901659266548,46.3053269018246,121.983092596544)) ;
#88030 = CARTESIAN_POINT('Ctrl Pts',(-20.1298859961201,46.3152776044852,122.087654097686)) ;
#88031 = CARTESIAN_POINT('Ctrl Pts',(-20.3496387002322,46.3253179225826,122.233636338155)) ;
#88032 = CARTESIAN_POINT('Ctrl Pts',(-20.5377696612843,46.3351924879158,122.412406684327)) ;
#88033 = CARTESIAN_POINT('Ctrl Pts',(-20.6941818778816,46.3451921479769,122.623513973067)) ;
#88034 = CARTESIAN_POINT('Ctrl Pts',(-20.8107624841862,46.3551011431446,122.856409152193)) ;
#88035 = CARTESIAN_POINT('Ctrl Pts',(-20.8861223158461,46.3651558843079,123.109617925359)) ;
#88036 = CARTESIAN_POINT('Ctrl Pts',(-20.9160894530664,46.3750144962217,123.366999052458)) ;
#88037 = CARTESIAN_POINT('Ctrl Pts',(-20.90075393306,46.385082618501,123.631095083211)) ;
#88038 = CARTESIAN_POINT('Ctrl Pts',(-20.8410490247791,46.3949380892042,123.883133457476)) ;
#88039 = CARTESIAN_POINT('Ctrl Pts',(-20.7377739074065,46.4049329486976,124.124622613945)) ;
#88040 = CARTESIAN_POINT('Ctrl Pts',(-20.5931317991477,46.4149642020395,124.345013634199)) ;
#88041 = CARTESIAN_POINT('Ctrl Pts',(-20.4156811920431,46.4248309009126,124.534077171764)) ;
#88042 = CARTESIAN_POINT('Ctrl Pts',(-20.2058603225502,46.4348177166638,124.691672146936)) ;
#88043 = CARTESIAN_POINT('Ctrl Pts',(-19.9727878453625,46.4447649218593,124.810106319578)) ;
#88044 = CARTESIAN_POINT('Ctrl Pts',(-19.7203014995016,46.4548079099855,124.886878521839)) ;
#88045 = CARTESIAN_POINT('Ctrl Pts',(-19.462892547754,46.464675264607,124.918244909157)) ;
#88046 = CARTESIAN_POINT('Ctrl Pts',(-19.2013450743715,46.4746411579051,124.905008550705)) ;
#88047 = CARTESIAN_POINT('Ctrl Pts',(-18.9446202495613,46.4846649352812,124.845948246086)) ;
#88048 = CARTESIAN_POINT('Ctrl Pts',(-18.7044304082566,46.4945904832129,124.744281867912)) ;
#88049 = CARTESIAN_POINT('Ctrl Pts',(-18.4848534110883,46.5045309596339,124.60274474947)) ;
#88050 = CARTESIAN_POINT('Ctrl Pts',(-18.2913765899753,46.5145771692968,124.423144114639)) ;
#88051 = CARTESIAN_POINT('Ctrl Pts',(-18.1347125364933,46.5244384259586,124.216689383634)) ;
#88052 = CARTESIAN_POINT('Ctrl Pts',(-18.0143126829843,46.5344320542339,123.983335039586)) ;
#88053 = CARTESIAN_POINT('Ctrl Pts',(-17.9366394008495,46.5443574515441,123.734298668841)) ;
#88054 = CARTESIAN_POINT('Ctrl Pts',(-17.9030455996264,46.5543853594543,123.472960192196)) ;
#88055 = CARTESIAN_POINT('Ctrl Pts',(-17.9149012642186,46.5642716751235,123.213390481439)) ;
#88056 = CARTESIAN_POINT('Ctrl Pts',(-17.972325349276,46.5743032700273,122.956144198347)) ;
#88057 = CARTESIAN_POINT('Ctrl Pts',(-18.0718482092479,46.584185512979,122.716230515682)) ;
#88058 = CARTESIAN_POINT('Ctrl Pts',(-18.2138880944537,46.5942449840088,122.493315287928)) ;
#88059 = CARTESIAN_POINT('Ctrl Pts',(-18.3891039122629,46.604111428672,122.302179808622)) ;
#88060 = CARTESIAN_POINT('Ctrl Pts',(-18.596403594826,46.6140775531207,122.142134294108)) ;
#88061 = CARTESIAN_POINT('Ctrl Pts',(-18.8300357306055,46.6241077965118,122.020104455616)) ;
#88062 = CARTESIAN_POINT('Ctrl Pts',(-19.0777840409719,46.6340008314649,121.941221742418)) ;
#88063 = CARTESIAN_POINT('Ctrl Pts',(-19.3395213808909,46.6440517457017,121.905936560177)) ;
#88064 = CARTESIAN_POINT('Ctrl Pts',(-19.5992144386022,46.6539415719263,121.916434213114)) ;
#88065 = CARTESIAN_POINT('Ctrl Pts',(-19.9417614873954,46.6672763869732,121.990497581648)) ;
#88066 = CARTESIAN_POINT('Ctrl Pts',(-20.2554096954557,46.6805534781447,122.152105027392)) ;
#88067 = CARTESIAN_POINT('Ctrl Pts',(-20.5136667534488,46.693801766743,122.385643139726)) ;
#88068 = CARTESIAN_POINT('Ctrl Pts',(-20.6757363842069,46.7038566082371,122.594281387087)) ;
#88069 = CARTESIAN_POINT('Ctrl Pts',(-20.7967988624566,46.7136875975446,122.822559708019)) ;
#88070 = CARTESIAN_POINT('Ctrl Pts',(-20.8785312557402,46.7237641618679,123.074384834974)) ;
#88071 = CARTESIAN_POINT('Ctrl Pts',(-20.9144702982914,46.7336134870018,123.33073485832)) ;
#88072 = CARTESIAN_POINT('Ctrl Pts',(-20.9029684187357,46.7469614866391,123.681333495441)) ;
#88073 = CARTESIAN_POINT('Ctrl Pts',(-20.7745139330427,46.7635462461757,124.102969724517)) ;
#88074 = CARTESIAN_POINT('Ctrl Pts',(-20.5110315388571,46.7801147975237,124.4557847313)) ;
#88075 = CARTESIAN_POINT('Ctrl Pts',(-20.23514044175,46.7934746223427,124.672959741583)) ;
#88076 = CARTESIAN_POINT('Ctrl Pts',(-20.0058449666823,46.8033800311734,124.796184304861)) ;
#88077 = CARTESIAN_POINT('Ctrl Pts',(-19.7574240387125,46.8133400577574,124.878527441293)) ;
#88078 = CARTESIAN_POINT('Ctrl Pts',(-19.4127438329402,46.8265976419427,124.929510558515)) ;
#88079 = CARTESIAN_POINT('Ctrl Pts',(-18.9730785233433,46.8432488534374,124.87894995727)) ;
#88080 = CARTESIAN_POINT('Ctrl Pts',(-18.4995437565153,46.8631670675477,124.642323373345)) ;
#88081 = CARTESIAN_POINT('Ctrl Pts',(-18.1350267198472,46.8830448307685,124.259795228635)) ;
#88082 = CARTESIAN_POINT('Ctrl Pts',(-17.9219959153182,46.9030574985557,123.772520415574)) ;
#88083 = CARTESIAN_POINT('Ctrl Pts',(-17.8878670522062,46.9228700212223,123.246943798671)) ;
#88084 = CARTESIAN_POINT('Ctrl Pts',(-18.035546506357,46.9428533212222,122.736872230293)) ;
#88085 = CARTESIAN_POINT('Ctrl Pts',(-18.3474461325361,46.9627475983235,122.309804698334)) ;
#88086 = CARTESIAN_POINT('Ctrl Pts',(-18.7866677876835,46.9826803600813,122.013601770197)) ;
#88087 = CARTESIAN_POINT('Ctrl Pts',(-19.3015657425341,47.002646365846,121.885203552185)) ;
#88088 = CARTESIAN_POINT('Ctrl Pts',(-19.8271303436553,47.0225248980109,121.939603120483)) ;
#88089 = CARTESIAN_POINT('Ctrl Pts',(-20.3041868868379,47.0424645646712,122.170298147785)) ;
#88090 = CARTESIAN_POINT('Ctrl Pts',(-20.6732403950815,47.0623594393166,122.549057326393)) ;
#88091 = CARTESIAN_POINT('Ctrl Pts',(-20.8914282381446,47.0822665786099,123.030940138027)) ;
#88092 = CARTESIAN_POINT('Ctrl Pts',(-20.9330126326835,47.1021771266884,123.558665033763)) ;
#88093 = CARTESIAN_POINT('Ctrl Pts',(-20.7897985089648,47.1222457120455,124.072348596256)) ;
#88094 = CARTESIAN_POINT('Ctrl Pts',(-20.4845832960142,47.1420275093603,124.500664842063)) ;
#88095 = CARTESIAN_POINT('Ctrl Pts',(-20.0473415775769,47.1620350563049,124.802948543256)) ;
#88096 = CARTESIAN_POINT('Ctrl Pts',(-19.5376373388019,47.1818567946077,124.936737621714)) ;
#88097 = CARTESIAN_POINT('Ctrl Pts',(-19.0088143994453,47.2018368145119,124.889159509882)) ;
#88098 = CARTESIAN_POINT('Ctrl Pts',(-18.5296831814101,47.2217542657741,124.664016484713)) ;
#88099 = CARTESIAN_POINT('Ctrl Pts',(-18.156054658413,47.2416291869468,124.290549692997)) ;
#88100 = CARTESIAN_POINT('Ctrl Pts',(-17.9309560929439,47.2616535554976,123.808318679437)) ;
#88101 = CARTESIAN_POINT('Ctrl Pts',(-17.8844429064027,47.2815202398711,123.282262426708)) ;
#88102 = CARTESIAN_POINT('Ctrl Pts',(-18.0199062073946,47.3014640617173,122.769851703785)) ;
#88103 = CARTESIAN_POINT('Ctrl Pts',(-18.321723185349,47.3213714309688,122.335270498965)) ;
#88104 = CARTESIAN_POINT('Ctrl Pts',(-18.7524373240201,47.3412461287155,122.029471467672)) ;
#88105 = CARTESIAN_POINT('Ctrl Pts',(-19.2643995478987,47.3612280712373,121.888115658735)) ;
#88106 = CARTESIAN_POINT('Ctrl Pts',(-19.7916438055128,47.3811307381481,121.930221264192)) ;
#88107 = CARTESIAN_POINT('Ctrl Pts',(-20.2724952367668,47.4009860956868,122.147830932133)) ;
#88108 = CARTESIAN_POINT('Ctrl Pts',(-20.6536636578321,47.4210501344028,122.52065673183)) ;
#88109 = CARTESIAN_POINT('Ctrl Pts',(-20.8822481029672,47.4409053141279,122.996516067802)) ;
#88110 = CARTESIAN_POINT('Ctrl Pts',(-20.935436165233,47.4608854187923,123.524678358585)) ;
#88111 = CARTESIAN_POINT('Ctrl Pts',(-20.8068403946321,47.4806945239621,124.035381850163)) ;
#88112 = CARTESIAN_POINT('Ctrl Pts',(-20.5095795524021,47.5006871443028,124.475622450521)) ;
#88113 = CARTESIAN_POINT('Ctrl Pts',(-20.1539694207839,47.5172266268069,124.734264236863)) ;
#88114 = CARTESIAN_POINT('Ctrl Pts',(-19.8262823346885,47.5305909448711,124.860472249389)) ;
#88115 = CARTESIAN_POINT('Ctrl Pts',(-19.485405542771,47.5438085473726,124.927559945783)) ;
#88116 = CARTESIAN_POINT('Ctrl Pts',(-19.0437703200357,47.5604661416504,124.898016262381)) ;
#88117 = CARTESIAN_POINT('Ctrl Pts',(-18.5604499932118,47.5803318436921,124.685212590745)) ;
#88118 = CARTESIAN_POINT('Ctrl Pts',(-18.2406362283115,47.5969615703822,124.380257695188)) ;
#88119 = CARTESIAN_POINT('Ctrl Pts',(-18.0589404833083,47.61025068552,124.081950760843)) ;
#88120 = CARTESIAN_POINT('Ctrl Pts',(-17.9633474747988,47.6202150324971,123.838187618009)) ;
#88121 = CARTESIAN_POINT('Ctrl Pts',(-17.9115445460179,47.6301434004986,123.582486569596)) ;
#88122 = CARTESIAN_POINT('Ctrl Pts',(-17.9020103793018,47.6434268335873,123.233497874318)) ;
#88123 = CARTESIAN_POINT('Ctrl Pts',(-18.005095080809,47.6600789113277,122.803114333347)) ;
#88124 = CARTESIAN_POINT('Ctrl Pts',(-18.247209882945,47.6766302806285,122.435837759358)) ;
#88125 = CARTESIAN_POINT('Ctrl Pts',(-18.50783847541,47.6899177087775,122.203427580766)) ;
#88126 = CARTESIAN_POINT('Ctrl Pts',(-18.7324805385707,47.6999622484776,122.064856373526)) ;
#88127 = CARTESIAN_POINT('Ctrl Pts',(-18.9727568592771,47.7098050903014,121.969045673601)) ;
#88128 = CARTESIAN_POINT('Ctrl Pts',(-19.2294948681427,47.7197893745484,121.915068774287)) ;
#88129 = CARTESIAN_POINT('Ctrl Pts',(-19.4908350255121,47.7297390199475,121.906573088993)) ;
#88130 = CARTESIAN_POINT('Ctrl Pts',(-19.7510324518848,47.7397387816359,121.943450958025)) ;
#88131 = CARTESIAN_POINT('Ctrl Pts',(-20.001511154546,47.7497701275948,122.025612884837)) ;
#88132 = CARTESIAN_POINT('Ctrl Pts',(-20.2300186287295,47.7596250820719,122.147499644092)) ;
#88133 = CARTESIAN_POINT('Ctrl Pts',(-20.4366754769559,47.7695976200724,122.308615609026)) ;
#88134 = CARTESIAN_POINT('Ctrl Pts',(-20.612644360831,47.7795926138074,122.503667729469)) ;
#88135 = CARTESIAN_POINT('Ctrl Pts',(-20.7523101013191,47.7896266726015,122.727299317315)) ;
#88136 = CARTESIAN_POINT('Ctrl Pts',(-20.8496668786128,47.7994820154245,122.967319880366)) ;
#88137 = CARTESIAN_POINT('Ctrl Pts',(-20.904992548046,47.8094814947701,123.224157421193)) ;
#88138 = CARTESIAN_POINT('Ctrl Pts',(-20.9150779626639,47.8193759435254,123.484026654786)) ;
#88139 = CARTESIAN_POINT('Ctrl Pts',(-20.879224101965,47.8294390629599,123.745986877431)) ;
#88140 = CARTESIAN_POINT('Ctrl Pts',(-20.8004688342771,47.8392787082011,123.992322380341)) ;
#88141 = CARTESIAN_POINT('Ctrl Pts',(-20.6777398160996,47.8493418723872,124.226526704695)) ;
#88142 = CARTESIAN_POINT('Ctrl Pts',(-20.5187066498922,47.859236142136,124.432268221858)) ;
#88143 = CARTESIAN_POINT('Ctrl Pts',(-20.3259668872383,47.8691778681498,124.608589479913)) ;
#88144 = CARTESIAN_POINT('Ctrl Pts',(-20.1041808999464,47.8791807568092,124.749765186793)) ;
#88145 = CARTESIAN_POINT('Ctrl Pts',(-19.8602299792522,47.8892206056032,124.850187093091)) ;
#88146 = CARTESIAN_POINT('Ctrl Pts',(-19.6081642424219,47.8990448210641,124.906094643254)) ;
#88147 = CARTESIAN_POINT('Ctrl Pts',(-19.3441702977261,47.9091016645576,124.918019813108)) ;
#88148 = CARTESIAN_POINT('Ctrl Pts',(-19.0854703555384,47.9190302739536,124.884016066394)) ;
#88149 = CARTESIAN_POINT('Ctrl Pts',(-18.835802023627,47.9289821579915,124.806127703608)) ;
#88150 = CARTESIAN_POINT('Ctrl Pts',(-18.6013347301841,47.9390351107991,124.684442693465)) ;
#88151 = CARTESIAN_POINT('Ctrl Pts',(-18.3960367832778,47.9488579872653,124.527928911458)) ;
#88152 = CARTESIAN_POINT('Ctrl Pts',(-18.2165695066782,47.9589137198354,124.333990312506)) ;
#88153 = CARTESIAN_POINT('Ctrl Pts',(-18.0755119524271,47.9688544848231,124.114102984926)) ;
#88154 = CARTESIAN_POINT('Ctrl Pts',(-17.97439677815,47.9787588177287,123.874266207495)) ;
#88155 = CARTESIAN_POINT('Ctrl Pts',(-17.9157978478123,47.9888054866094,123.616858452994)) ;
#88156 = CARTESIAN_POINT('Ctrl Pts',(-17.9027391893822,47.9987010499152,123.357099240434)) ;
#88157 = CARTESIAN_POINT('Ctrl Pts',(-17.9355139727328,48.0087631076155,123.094756208375)) ;
#88158 = CARTESIAN_POINT('Ctrl Pts',(-18.0115247975341,48.018605885243,122.847487885336)) ;
#88159 = CARTESIAN_POINT('Ctrl Pts',(-18.130499270546,48.0285963634949,122.613492148444)) ;
#88160 = CARTESIAN_POINT('Ctrl Pts',(-18.2873849531134,48.0385253361384,122.404982545336)) ;
#88161 = CARTESIAN_POINT('Ctrl Pts',(-18.4789956662502,48.048516473018,122.225477178445)) ;
#88162 = CARTESIAN_POINT('Ctrl Pts',(-18.6997215251481,48.0585385905069,122.081788244482)) ;
#88163 = CARTESIAN_POINT('Ctrl Pts',(-18.9390060894404,48.0684391009091,121.979633386977)) ;
#88164 = CARTESIAN_POINT('Ctrl Pts',(-19.1945602868354,48.0784280936552,121.9196516612)) ;
#88165 = CARTESIAN_POINT('Ctrl Pts',(-19.4560251777434,48.0883933377058,121.905170872972)) ;
#88166 = CARTESIAN_POINT('Ctrl Pts',(-19.714544749918,48.098297602219,121.935512588317)) ;
#88167 = CARTESIAN_POINT('Ctrl Pts',(-19.9676521572524,48.1083556939172,122.01159018475)) ;
#88168 = CARTESIAN_POINT('Ctrl Pts',(-20.1989410280847,48.1182056343456,122.127843264376)) ;
#88169 = CARTESIAN_POINT('Ctrl Pts',(-20.4106352779193,48.1282326455192,122.284734900046)) ;
#88170 = CARTESIAN_POINT('Ctrl Pts',(-20.5914129661359,48.1382612321312,122.476515291714)) ;
#88171 = CARTESIAN_POINT('Ctrl Pts',(-20.7338940826546,48.1481064462439,122.692453451488)) ;
#88172 = CARTESIAN_POINT('Ctrl Pts',(-20.8388889355934,48.1580971944235,122.933098046713)) ;
#88173 = CARTESIAN_POINT('Ctrl Pts',(-20.9002278538488,48.168134828009,123.189645406397)) ;
#88174 = CARTESIAN_POINT('Ctrl Pts',(-20.9162157833847,48.1779801172218,123.447878692139)) ;
#88175 = CARTESIAN_POINT('Ctrl Pts',(-20.8873032918651,48.1879615180277,123.708561008633)) ;
#88176 = CARTESIAN_POINT('Ctrl Pts',(-20.8137139164343,48.1979137510176,123.959536527466)) ;
#88177 = CARTESIAN_POINT('Ctrl Pts',(-20.6974226162219,48.2079125624742,124.195182186014)) ;
#88178 = CARTESIAN_POINT('Ctrl Pts',(-20.5409679874558,48.2179516664049,124.40758088976)) ;
#88179 = CARTESIAN_POINT('Ctrl Pts',(-20.3544447338278,48.2277766088242,124.58612785741)) ;
#88180 = CARTESIAN_POINT('Ctrl Pts',(-20.1350015577314,48.2378312963002,124.733273340073)) ;
#88181 = CARTESIAN_POINT('Ctrl Pts',(-19.8958290741237,48.247774098657,124.838493759771)) ;
#88182 = CARTESIAN_POINT('Ctrl Pts',(-19.6432087007226,48.2576778945968,124.901118420341)) ;
#88183 = CARTESIAN_POINT('Ctrl Pts',(-19.3798197798372,48.2677246739718,124.919026044654)) ;
#88184 = CARTESIAN_POINT('Ctrl Pts',(-19.1211868057863,48.2776203322664,124.891570258685)) ;
#88185 = CARTESIAN_POINT('Ctrl Pts',(-18.8671159689922,48.287681899517,124.818466322481)) ;
#88186 = CARTESIAN_POINT('Ctrl Pts',(-18.6346672337003,48.2975265439543,124.704882074842)) ;
#88187 = CARTESIAN_POINT('Ctrl Pts',(-18.4224774448849,48.307486590197,124.551645752143)) ;
#88188 = CARTESIAN_POINT('Ctrl Pts',(-18.2390630273348,48.3175248862154,124.362065332604)) ;
#88189 = CARTESIAN_POINT('Ctrl Pts',(-18.0933378214402,48.3273982276337,124.147345292635)) ;
#88190 = CARTESIAN_POINT('Ctrl Pts',(-17.9850701345174,48.337471331433,123.905844629381)) ;
#88191 = CARTESIAN_POINT('Ctrl Pts',(-17.9216618145417,48.3472921465519,123.655621239189)) ;
#88192 = CARTESIAN_POINT('Ctrl Pts',(-17.9018739629238,48.3573690116299,123.391601343181)) ;
#88193 = CARTESIAN_POINT('Ctrl Pts',(-17.9277813877702,48.3672337512852,123.133631857944)) ;
#88194 = CARTESIAN_POINT('Ctrl Pts',(-17.9985353622652,48.3772561545265,122.879946100013)) ;
#88195 = CARTESIAN_POINT('Ctrl Pts',(-18.1129061323741,48.387281878815,122.642581869023)) ;
#88196 = CARTESIAN_POINT('Ctrl Pts',(-18.2637423254893,48.3971366618363,122.432087433426)) ;
#88197 = CARTESIAN_POINT('Ctrl Pts',(-18.4507029295602,48.4071155055596,122.248197667358)) ;
#88198 = CARTESIAN_POINT('Ctrl Pts',(-18.6678616263483,48.4171343977962,122.099352690164)) ;
#88199 = CARTESIAN_POINT('Ctrl Pts',(-18.9041396211026,48.4270176068372,121.991439850928)) ;
#88200 = CARTESIAN_POINT('Ctrl Pts',(-19.1602260657838,48.4370859161774,121.925097919403)) ;
#88201 = CARTESIAN_POINT('Ctrl Pts',(-19.4177670696848,48.4469160415101,121.904413532861)) ;
#88202 = CARTESIAN_POINT('Ctrl Pts',(-19.6811181172093,48.4569825938871,121.928996874006)) ;
#88203 = CARTESIAN_POINT('Ctrl Pts',(-19.9317618895005,48.4668728307808,121.997882966823)) ;
#88204 = CARTESIAN_POINT('Ctrl Pts',(-20.1692610222621,48.4768650555748,122.109851831293)) ;
#88205 = CARTESIAN_POINT('Ctrl Pts',(-20.3829445510021,48.4868276759257,122.261113657658)) ;
#88206 = CARTESIAN_POINT('Ctrl Pts',(-20.5665261218062,48.4967326786889,122.445666071956)) ;
#88207 = CARTESIAN_POINT('Ctrl Pts',(-20.7173958030492,48.506790441087,122.662655601088)) ;
#88208 = CARTESIAN_POINT('Ctrl Pts',(-20.8262238273378,48.5166409604658,122.897552034887)) ;
#88209 = CARTESIAN_POINT('Ctrl Pts',(-20.8943829996658,48.526672537464,123.152189944527)) ;
#88210 = CARTESIAN_POINT('Ctrl Pts',(-20.9167426169127,48.5366822725689,123.414312273892)) ;
#88211 = CARTESIAN_POINT('Ctrl Pts',(-20.8937179531658,48.5465918491952,123.673683390135)) ;
#88212 = CARTESIAN_POINT('Ctrl Pts',(-20.8265228052753,48.5565192350519,123.925774756106)) ;
#88213 = CARTESIAN_POINT('Ctrl Pts',(-20.7150907300863,48.5665641695422,124.165059353475)) ;
#88214 = CARTESIAN_POINT('Ctrl Pts',(-20.5663090616085,48.5764501017301,124.378048058078)) ;
#88215 = CARTESIAN_POINT('Ctrl Pts',(-20.3811550715041,48.5864434076831,124.564263272707)) ;
#88216 = CARTESIAN_POINT('Ctrl Pts',(-20.1674323885774,48.596389045465,124.714704721664)) ;
#88217 = CARTESIAN_POINT('Ctrl Pts',(-19.9310127579831,48.6063363138109,124.826259865705)) ;
#88218 = CARTESIAN_POINT('Ctrl Pts',(-19.6762062907194,48.616384215948,124.895474138505)) ;
#88219 = CARTESIAN_POINT('Ctrl Pts',(-19.4185018206962,48.6262319107882,124.919135372387)) ;
#88220 = CARTESIAN_POINT('Ctrl Pts',(-19.157566898572,48.6361934205326,124.898267563706)) ;
#88221 = CARTESIAN_POINT('Ctrl Pts',(-18.9025619508575,48.6462228121415,124.831614773843)) ;
#88222 = CARTESIAN_POINT('Ctrl Pts',(-18.6658627752509,48.6561303076962,124.723165141493)) ;
#88223 = CARTESIAN_POINT('Ctrl Pts',(-18.4504930203598,48.6660756993592,124.575141126783)) ;
#88224 = CARTESIAN_POINT('Ctrl Pts',(-18.2628876791554,48.6760776169566,124.391000597497)) ;
#88225 = CARTESIAN_POINT('Ctrl Pts',(-18.1099535759632,48.6861176845088,124.176032718824)) ;
#88226 = CARTESIAN_POINT('Ctrl Pts',(-17.9985528130765,48.6959419959486,123.943106599342)) ;
#88227 = CARTESIAN_POINT('Ctrl Pts',(-17.9273154063796,48.7059982371047,123.688649150822)) ;
#88228 = CARTESIAN_POINT('Ctrl Pts',(-17.9019656863292,48.7159291588403,123.428879136997)) ;
#88229 = CARTESIAN_POINT('Ctrl Pts',(-17.9215938866681,48.7258723949166,123.168352780034)) ;
#88230 = CARTESIAN_POINT('Ctrl Pts',(-17.9861802002328,48.735853678929,122.914090093812)) ;
#88231 = CARTESIAN_POINT('Ctrl Pts',(-18.0949989715361,48.7458979805547,122.673647794656)) ;
#88232 = CARTESIAN_POINT('Ctrl Pts',(-18.2402534708388,48.7557260617741,122.460043836669)) ;
#88233 = CARTESIAN_POINT('Ctrl Pts',(-18.4247849710024,48.7658026646233,122.270203460101)) ;
#88234 = CARTESIAN_POINT('Ctrl Pts',(-18.6347065996334,48.7756547437418,122.118569547531)) ;
#88235 = CARTESIAN_POINT('Ctrl Pts',(-18.8728105251633,48.7857280020508,122.002995475702)) ;
#88236 = CARTESIAN_POINT('Ctrl Pts',(-19.1215857423761,48.7955694614311,121.932239761547)) ;
#88237 = CARTESIAN_POINT('Ctrl Pts',(-19.3818649812545,48.8055305568434,121.904458482012)) ;
#88238 = CARTESIAN_POINT('Ctrl Pts',(-19.6449795161499,48.8155678412401,121.922944960723)) ;
#88239 = CARTESIAN_POINT('Ctrl Pts',(-19.8969273677844,48.8254441799754,121.985379683799)) ;
#88240 = CARTESIAN_POINT('Ctrl Pts',(-20.1386336262622,48.8355063061287,122.092521249283)) ;
#88241 = CARTESIAN_POINT('Ctrl Pts',(-20.3539244509202,48.8453744801052,122.237144739534)) ;
#88242 = CARTESIAN_POINT('Ctrl Pts',(-20.543755011927,48.855380028609,122.419026520356)) ;
#88243 = CARTESIAN_POINT('Ctrl Pts',(-20.6987419364052,48.8653626605046,122.630740739498)) ;
#88244 = CARTESIAN_POINT('Ctrl Pts',(-20.8150482287937,48.8754066029264,122.867653599729)) ;
#88245 = CARTESIAN_POINT('Ctrl Pts',(-20.8872135170498,48.8852347509536,123.115640682786)) ;
#88246 = CARTESIAN_POINT('Ctrl Pts',(-20.9165222913364,48.8952246183279,123.376523659417)) ;
#88247 = CARTESIAN_POINT('Ctrl Pts',(-20.8993147872527,48.9052683572834,123.639900737698)) ;
#88248 = CARTESIAN_POINT('Ctrl Pts',(-20.8385460028974,48.9150901058214,123.890749443944)) ;
#88249 = CARTESIAN_POINT('Ctrl Pts',(-20.7334926344583,48.9251250834311,124.132629488794)) ;
#88250 = CARTESIAN_POINT('Ctrl Pts',(-20.5875669348054,48.9351499961888,124.351974416172)) ;
#88251 = CARTESIAN_POINT('Ctrl Pts',(-20.4093201184437,48.9450019392826,124.539749635484)) ;
#88252 = CARTESIAN_POINT('Ctrl Pts',(-20.1985093079883,48.9549929006117,124.696195980077)) ;
#88253 = CARTESIAN_POINT('Ctrl Pts',(-19.9654731355136,48.9649107754802,124.812985422573)) ;
#88254 = CARTESIAN_POINT('Ctrl Pts',(-19.7129807407904,48.9749392944814,124.888406605347)) ;
#88255 = CARTESIAN_POINT('Ctrl Pts',(-19.4549910732823,48.9848229732793,124.918538485184)) ;
#88256 = CARTESIAN_POINT('Ctrl Pts',(-19.1927471785049,48.994817916719,124.903825171715)) ;
#88257 = CARTESIAN_POINT('Ctrl Pts',(-18.9363271652186,49.0048447705414,124.84316892203)) ;
#88258 = CARTESIAN_POINT('Ctrl Pts',(-18.6976274329194,49.0147289348803,124.740719075366)) ;
#88259 = CARTESIAN_POINT('Ctrl Pts',(-18.4778974629818,49.0247170329227,124.597194644998)) ;
#88260 = CARTESIAN_POINT('Ctrl Pts',(-18.2869925249069,49.0346681393798,124.418428962904)) ;
#88261 = CARTESIAN_POINT('Ctrl Pts',(-18.1286921061756,49.0447131905479,124.207206823015)) ;
#88262 = CARTESIAN_POINT('Ctrl Pts',(-18.0115110053641,49.0545749509062,123.976053919716)) ;
#88263 = CARTESIAN_POINT('Ctrl Pts',(-17.9347018565793,49.0645377677367,123.725760547945)) ;
#88264 = CARTESIAN_POINT('Ctrl Pts',(-17.9027372037974,49.0745724490174,123.464015962194)) ;
#88265 = CARTESIAN_POINT('Ctrl Pts',(-17.9160561245772,49.0844574787982,123.204553334292)) ;
#88266 = CARTESIAN_POINT('Ctrl Pts',(-17.9753271704611,49.0945230721962,122.946810192394)) ;
#88267 = CARTESIAN_POINT('Ctrl Pts',(-18.0759231780919,49.1043622405577,122.708574067968)) ;
#88268 = CARTESIAN_POINT('Ctrl Pts',(-18.2192006262921,49.1144248382992,122.486356375471)) ;
#88269 = CARTESIAN_POINT('Ctrl Pts',(-18.3961652533745,49.1243218507061,122.2957392912)) ;
#88270 = CARTESIAN_POINT('Ctrl Pts',(-18.6037154643153,49.1342531725317,122.137521228201)) ;
#88271 = CARTESIAN_POINT('Ctrl Pts',(-18.8382964268997,49.1442949352862,122.016665264985)) ;
#88272 = CARTESIAN_POINT('Ctrl Pts',(-19.0864079744247,49.1541831341769,121.939390497466)) ;
#88273 = CARTESIAN_POINT('Ctrl Pts',(-19.3468353464452,49.1641770727768,121.905608425672)) ;
#88274 = CARTESIAN_POINT('Ctrl Pts',(-19.6078151277302,49.1741178938136,121.91751361713)) ;
#88275 = CARTESIAN_POINT('Ctrl Pts',(-19.8632816579453,49.1840772761019,121.974327396906)) ;
#88276 = CARTESIAN_POINT('Ctrl Pts',(-20.1060322896982,49.1940750357542,122.074891251936)) ;
#88277 = CARTESIAN_POINT('Ctrl Pts',(-20.3282620364892,49.2041111719565,122.21690786839)) ;
#88278 = CARTESIAN_POINT('Ctrl Pts',(-20.5190808378173,49.2139619694474,122.391836817215)) ;
#88279 = CARTESIAN_POINT('Ctrl Pts',(-20.6790012985683,49.2239228345237,122.599055308519)) ;
#88280 = CARTESIAN_POINT('Ctrl Pts',(-20.8010708002223,49.2339517021541,122.832645696346)) ;
#88281 = CARTESIAN_POINT('Ctrl Pts',(-20.879853818226,49.2438619382905,123.080862806442)) ;
#88282 = CARTESIAN_POINT('Ctrl Pts',(-20.9151078932877,49.253796891605,123.339559285952)) ;
#88283 = CARTESIAN_POINT('Ctrl Pts',(-20.9045592317714,49.2638378220146,123.603207119489)) ;
#88284 = CARTESIAN_POINT('Ctrl Pts',(-20.8494077535675,49.2737257187962,123.857140794924)) ;
#88285 = CARTESIAN_POINT('Ctrl Pts',(-20.7504505562724,49.2837151704549,124.100280633098)) ;
#88286 = CARTESIAN_POINT('Ctrl Pts',(-20.6110277047872,49.2936742608203,124.321756486501)) ;
#88287 = CARTESIAN_POINT('Ctrl Pts',(-20.4368338343713,49.3035715731266,124.514921157602)) ;
#88288 = CARTESIAN_POINT('Ctrl Pts',(-20.2284024122809,49.3136279990268,124.677354927092)) ;
#88289 = CARTESIAN_POINT('Ctrl Pts',(-19.9992830178138,49.3234980016166,124.798974471006)) ;
#88290 = CARTESIAN_POINT('Ctrl Pts',(-19.7493901780766,49.3335019347938,124.880531822233)) ;
#88291 = CARTESIAN_POINT('Ctrl Pts',(-19.4894780018953,49.3434891952577,124.917271202357)) ;
#88292 = CARTESIAN_POINT('Ctrl Pts',(-19.2261559513639,49.3535162468434,124.908135759446)) ;
#88293 = CARTESIAN_POINT('Ctrl Pts',(-18.9718205949569,49.3634073366695,124.854401512994)) ;
#88294 = CARTESIAN_POINT('Ctrl Pts',(-18.6475387787366,49.3767050914506,124.724316756299)) ;
#88295 = CARTESIAN_POINT('Ctrl Pts',(-18.3663439177842,49.3899031510587,124.514527900887)) ;
#88296 = CARTESIAN_POINT('Ctrl Pts',(-18.1484048267078,49.4032998916279,124.238071111464)) ;
#88297 = CARTESIAN_POINT('Ctrl Pts',(-18.0253527815644,49.4131708037013,124.009661322498)) ;
#88298 = CARTESIAN_POINT('Ctrl Pts',(-17.9421985890326,49.4232443654695,123.758399347314)) ;
#88299 = CARTESIAN_POINT('Ctrl Pts',(-17.9045673262481,49.4330657780578,123.502999840485)) ;
#88300 = CARTESIAN_POINT('Ctrl Pts',(-17.9117874809025,49.4431397952888,123.238428805641)) ;
#88301 = CARTESIAN_POINT('Ctrl Pts',(-17.9808625993538,49.4562985822534,122.899526034126)) ;
#88302 = CARTESIAN_POINT('Ctrl Pts',(-18.1386493012278,49.4696646853476,122.58136729471)) ;
#88303 = CARTESIAN_POINT('Ctrl Pts',(-18.3706579537025,49.4829786202367,122.319337160576)) ;
#88304 = CARTESIAN_POINT('Ctrl Pts',(-18.5739338777232,49.4928786596841,122.157029405636)) ;
#88305 = CARTESIAN_POINT('Ctrl Pts',(-18.8036238095851,49.5028430628186,122.031257984843)) ;
#88306 = CARTESIAN_POINT('Ctrl Pts',(-19.05335921375,49.5128730299398,121.946955300818)) ;
#88307 = CARTESIAN_POINT('Ctrl Pts',(-19.3105895258516,49.5227753065488,121.907692131419)) ;
#88308 = CARTESIAN_POINT('Ctrl Pts',(-19.6591707264257,49.536041235718,121.91483615231)) ;
#88309 = CARTESIAN_POINT('Ctrl Pts',(-20.0833606626239,49.5526627668244,122.037946979199)) ;
#88310 = CARTESIAN_POINT('Ctrl Pts',(-20.5104593674055,49.5725375954691,122.348915166531)) ;
#88311 = CARTESIAN_POINT('Ctrl Pts',(-20.7582535736872,49.5892108035709,122.716248365857)) ;
#88312 = CARTESIAN_POINT('Ctrl Pts',(-20.8714352247518,49.6024619285522,123.045592382337)) ;
#88313 = CARTESIAN_POINT('Ctrl Pts',(-20.9269354813126,49.615704247373,123.389194785708)) ;
#88314 = CARTESIAN_POINT('Ctrl Pts',(-20.8811511581855,49.6324374877125,123.831492590155)) ;
#88315 = CARTESIAN_POINT('Ctrl Pts',(-20.6511878464973,49.6522666359005,124.305812689138)) ;
#88316 = CARTESIAN_POINT('Ctrl Pts',(-20.2723991280832,49.6721913310011,124.675727471051)) ;
#88317 = CARTESIAN_POINT('Ctrl Pts',(-19.7899488954886,49.6921145595845,124.894193343067)) ;
#88318 = CARTESIAN_POINT('Ctrl Pts',(-19.2619611266706,49.7120416987106,124.935069014905)) ;
#88319 = CARTESIAN_POINT('Ctrl Pts',(-18.7527411075181,49.7319181613263,124.794310345686)) ;
#88320 = CARTESIAN_POINT('Ctrl Pts',(-18.3198072271694,49.7518953899316,124.486931020539)) ;
#88321 = CARTESIAN_POINT('Ctrl Pts',(-18.018710731692,49.7718302479053,124.050908756306)) ;
#88322 = CARTESIAN_POINT('Ctrl Pts',(-17.8842375144528,49.7917266968361,123.539519466163)) ;
#88323 = CARTESIAN_POINT('Ctrl Pts',(-17.9318221676816,49.8116479809027,123.012164589738)) ;
#88324 = CARTESIAN_POINT('Ctrl Pts',(-18.1570615290371,49.8316046305737,122.531918504927)) ;
#88325 = CARTESIAN_POINT('Ctrl Pts',(-18.5309830443767,49.8514819236853,122.158801133981)) ;
#88326 = CARTESIAN_POINT('Ctrl Pts',(-19.0095255521828,49.8713683959137,121.934252429302)) ;
#88327 = CARTESIAN_POINT('Ctrl Pts',(-19.5406391317515,49.8914299618377,121.886868078949)) ;
#88328 = CARTESIAN_POINT('Ctrl Pts',(-20.0501878146875,49.9112703693785,122.022537685724)) ;
#88329 = CARTESIAN_POINT('Ctrl Pts',(-20.4843856180674,49.9311216933514,122.322319927731)) ;
#88330 = CARTESIAN_POINT('Ctrl Pts',(-20.7926218042951,49.9511749633028,122.757047288943)) ;
#88331 = CARTESIAN_POINT('Ctrl Pts',(-20.9325314728205,49.9709956206862,123.265078314232)) ;
#88332 = CARTESIAN_POINT('Ctrl Pts',(-20.8912422361684,49.9909670420167,123.794102750068)) ;
#88333 = CARTESIAN_POINT('Ctrl Pts',(-20.672728228111,50.0108605343804,124.275780483601)) ;
#88334 = CARTESIAN_POINT('Ctrl Pts',(-20.3004875803372,50.0308846206214,124.65599343755)) ;
#88335 = CARTESIAN_POINT('Ctrl Pts',(-19.8260699488102,50.0506894997343,124.884165170859)) ;
#88336 = CARTESIAN_POINT('Ctrl Pts',(-19.2984073272745,50.0706485154322,124.938579634073)) ;
#88337 = CARTESIAN_POINT('Ctrl Pts',(-18.7834458131184,50.0906345390612,124.808287005669)) ;
#88338 = CARTESIAN_POINT('Ctrl Pts',(-18.3471380862029,50.1104430348217,124.513561025804)) ;
#88339 = CARTESIAN_POINT('Ctrl Pts',(-18.034433731144,50.1304256739273,124.08441134622)) ;
#88340 = CARTESIAN_POINT('Ctrl Pts',(-17.8877548058213,50.1503071217213,123.576622519046)) ;
#88341 = CARTESIAN_POINT('Ctrl Pts',(-17.9228590595857,50.1702635884589,123.047489138174)) ;
#88342 = CARTESIAN_POINT('Ctrl Pts',(-18.135325664709,50.1901409854144,122.563692670579)) ;
#88343 = CARTESIAN_POINT('Ctrl Pts',(-18.5017404753757,50.2101229315897,122.179326787256)) ;
#88344 = CARTESIAN_POINT('Ctrl Pts',(-18.9763311717451,50.2300520306265,121.94386229144)) ;
#88345 = CARTESIAN_POINT('Ctrl Pts',(-19.5025542136779,50.2499806538391,121.884425032197)) ;
#88346 = CARTESIAN_POINT('Ctrl Pts',(-20.0154098113017,50.2698149779455,122.006618943828)) ;
#88347 = CARTESIAN_POINT('Ctrl Pts',(-20.3852796718983,50.2864672653289,122.249530478733)) ;
#88348 = CARTESIAN_POINT('Ctrl Pts',(-20.6170613698565,50.2997277663511,122.509825199118)) ;
#88349 = CARTESIAN_POINT('Ctrl Pts',(-20.7555282047836,50.3097292435524,122.733215342447)) ;
#88350 = CARTESIAN_POINT('Ctrl Pts',(-20.8529948357394,50.3197612644119,122.978175098663)) ;
#88351 = CARTESIAN_POINT('Ctrl Pts',(-20.9058575761444,50.3296248081375,123.231923138614)) ;
#88352 = CARTESIAN_POINT('Ctrl Pts',(-20.9146380480463,50.3395935218076,123.493747759478)) ;
#88353 = CARTESIAN_POINT('Ctrl Pts',(-20.8648603610188,50.3529392692113,123.840886646443)) ;
#88354 = CARTESIAN_POINT('Ctrl Pts',(-20.7281950716831,50.366089824284,124.162613928907)) ;
#88355 = CARTESIAN_POINT('Ctrl Pts',(-20.5118305427497,50.3794752048338,124.439920066173)) ;
#88356 = CARTESIAN_POINT('Ctrl Pts',(-20.3188172284818,50.3893631408267,124.613934022329)) ;
#88357 = CARTESIAN_POINT('Ctrl Pts',(-20.0965116250302,50.3993543306393,124.753570663319)) ;
#88358 = CARTESIAN_POINT('Ctrl Pts',(-19.8542622927966,50.4093064291776,124.852232186328)) ;
#88359 = CARTESIAN_POINT('Ctrl Pts',(-19.5961633789181,50.4193526856281,124.907673196293)) ;
#88360 = CARTESIAN_POINT('Ctrl Pts',(-19.3375104748675,50.4292021330222,124.917455726656)) ;
#88361 = CARTESIAN_POINT('Ctrl Pts',(-19.0780426601325,50.4391647855174,124.882591527256)) ;
#88362 = CARTESIAN_POINT('Ctrl Pts',(-18.8271559377994,50.4491878711595,124.802384290233)) ;
#88363 = CARTESIAN_POINT('Ctrl Pts',(-18.5961209801117,50.4591129869164,124.681281420803)) ;
#88364 = CARTESIAN_POINT('Ctrl Pts',(-18.3870807334424,50.4691654653163,124.519806842714)) ;
#88365 = CARTESIAN_POINT('Ctrl Pts',(-18.2126501072753,50.479016964019,124.32847873655)) ;
#88366 = CARTESIAN_POINT('Ctrl Pts',(-18.0718501454337,50.4889887032215,124.107511530402)) ;
#88367 = CARTESIAN_POINT('Ctrl Pts',(-17.9713211447881,50.4989839109872,123.864801095388)) ;
#88368 = CARTESIAN_POINT('Ctrl Pts',(-17.9145692121074,50.5090179124563,123.607321569366)) ;
#88369 = CARTESIAN_POINT('Ctrl Pts',(-17.9031710447773,50.5188732705486,123.348557997671)) ;
#88370 = CARTESIAN_POINT('Ctrl Pts',(-17.9370086645265,50.5288727461419,123.088017414384)) ;
#88371 = CARTESIAN_POINT('Ctrl Pts',(-18.0144915110239,50.538767194637,122.839763225874)) ;
#88372 = CARTESIAN_POINT('Ctrl Pts',(-18.1359636490848,50.5488303188647,122.604915926376)) ;
#88373 = CARTESIAN_POINT('Ctrl Pts',(-18.2926316435237,50.5586699451933,122.399152962944)) ;
#88374 = CARTESIAN_POINT('Ctrl Pts',(-18.486678321847,50.5687331802363,122.219538927624)) ;
#88375 = CARTESIAN_POINT('Ctrl Pts',(-18.7053988201739,50.5786271854703,122.078904883828)) ;
#88376 = CARTESIAN_POINT('Ctrl Pts',(-18.9460659097001,50.5885698986861,121.977250669726)) ;
#88377 = CARTESIAN_POINT('Ctrl Pts',(-19.2023861460661,50.5985756384843,121.918495735838)) ;
#88378 = CARTESIAN_POINT('Ctrl Pts',(-19.4653940518091,50.6085965406307,121.9054168295)) ;
#88379 = CARTESIAN_POINT('Ctrl Pts',(-19.7233358092848,50.6184873106796,121.937482828107)) ;
#88380 = CARTESIAN_POINT('Ctrl Pts',(-19.9744185614306,50.6284787214593,122.014246082198)) ;
#88381 = CARTESIAN_POINT('Ctrl Pts',(-20.2073144805598,50.6384270671238,122.133004263277)) ;
#88382 = CARTESIAN_POINT('Ctrl Pts',(-20.4163335012571,50.648371925185,122.289918302436)) ;
#88383 = CARTESIAN_POINT('Ctrl Pts',(-20.5965902441456,50.6584267605779,122.483081634732)) ;
#88384 = CARTESIAN_POINT('Ctrl Pts',(-20.7376425347096,50.6682491326794,122.69928261909)) ;
#88385 = CARTESIAN_POINT('Ctrl Pts',(-20.8418429067607,50.6783050001231,122.942107997445)) ;
#88386 = CARTESIAN_POINT('Ctrl Pts',(-20.9011591134657,50.688245729981,123.196526972203)) ;
#88387 = CARTESIAN_POINT('Ctrl Pts',(-20.9161606255222,50.6981500685321,123.456374885143)) ;
#88388 = CARTESIAN_POINT('Ctrl Pts',(-20.8852161971234,50.7081967499607,123.718548743211)) ;
#88389 = CARTESIAN_POINT('Ctrl Pts',(-20.8105731784495,50.7180922574299,123.967693866746)) ;
#88390 = CARTESIAN_POINT('Ctrl Pts',(-20.6918696445542,50.7281545259285,124.203934788214)) ;
#88391 = CARTESIAN_POINT('Ctrl Pts',(-20.5374931111289,50.7379965161991,124.411487122097)) ;
#88392 = CARTESIAN_POINT('Ctrl Pts',(-20.3469886042085,50.7479899330801,124.592192301977)) ;
#88393 = CARTESIAN_POINT('Ctrl Pts',(-20.129467915059,50.7579144209322,124.736132155614)) ;
#88394 = CARTESIAN_POINT('Ctrl Pts',(-19.8886030526091,50.7679140548407,124.841138181418)) ;
#88395 = CARTESIAN_POINT('Ctrl Pts',(-19.6334526076263,50.7779001650975,124.902666745097)) ;
#88396 = CARTESIAN_POINT('Ctrl Pts',(-19.370234794874,50.7879361162846,124.9187595243)) ;
#88397 = CARTESIAN_POINT('Ctrl Pts',(-19.1128081761444,50.7977927546194,124.889819939285)) ;
#88398 = CARTESIAN_POINT('Ctrl Pts',(-18.8606967834269,50.8077917146974,124.815928138923)) ;
#88399 = CARTESIAN_POINT('Ctrl Pts',(-18.6274830798784,50.8176869450112,124.700806449973)) ;
#88400 = CARTESIAN_POINT('Ctrl Pts',(-18.4143788196718,50.8277474574798,124.544393204072)) ;
#88401 = CARTESIAN_POINT('Ctrl Pts',(-18.2353627908807,50.837596749026,124.357426939128)) ;
#88402 = CARTESIAN_POINT('Ctrl Pts',(-18.0883925533693,50.8476239349582,124.138724931857)) ;
#88403 = CARTESIAN_POINT('Ctrl Pts',(-17.9822394761601,50.8576524714175,123.897495737677)) ;
#88404 = CARTESIAN_POINT('Ctrl Pts',(-17.9202588837812,50.8674977113825,123.646321073152)) ;
#88405 = CARTESIAN_POINT('Ctrl Pts',(-17.9018714931078,50.8774884063057,123.384414305504)) ;
#88406 = CARTESIAN_POINT('Ctrl Pts',(-17.9299486548859,50.8875262270643,123.122130520275)) ;
#88407 = CARTESIAN_POINT('Ctrl Pts',(-18.0013103641566,50.8973708208412,122.873455872908)) ;
#88408 = CARTESIAN_POINT('Ctrl Pts',(-18.1158568183376,50.9073548162173,122.637438180659)) ;
#88409 = CARTESIAN_POINT('Ctrl Pts',(-18.2691496553917,50.9173038647787,122.425625938668)) ;
#88410 = CARTESIAN_POINT('Ctrl Pts',(-18.4576995104374,50.9273063037532,122.242469851909)) ;
#88411 = CARTESIAN_POINT('Ctrl Pts',(-18.675790127976,50.9373275450496,122.094857283506)) ;
#88412 = CARTESIAN_POINT('Ctrl Pts',(-18.9129857115445,50.9472202234891,121.988448302435)) ;
#88413 = CARTESIAN_POINT('Ctrl Pts',(-19.1674288630117,50.9572102774367,121.923807401294)) ;
#88414 = CARTESIAN_POINT('Ctrl Pts',(-19.42840760001,50.9671686385852,121.904576356759)) ;
#88415 = CARTESIAN_POINT('Ctrl Pts',(-19.6873151025459,50.97706826547,121.930161648276)) ;
#88416 = CARTESIAN_POINT('Ctrl Pts',(-19.9415317404535,50.9871161622734,122.001441737826)) ;
#88417 = CARTESIAN_POINT('Ctrl Pts',(-20.1760473918664,50.9970115199094,122.11388903272)) ;
#88418 = CARTESIAN_POINT('Ctrl Pts',(-20.3909934475873,51.0070731723661,122.267820853643)) ;
#88419 = CARTESIAN_POINT('Ctrl Pts',(-20.5720124432176,51.016917776638,122.452660571482)) ;
#88420 = CARTESIAN_POINT('Ctrl Pts',(-20.7206679475832,51.026877898336,122.668085454437)) ;
#88421 = CARTESIAN_POINT('Ctrl Pts',(-20.8300463265181,51.0369159326985,122.908118283207)) ;
#88422 = CARTESIAN_POINT('Ctrl Pts',(-20.8954797450795,51.046790245285,123.159253141407)) ;
#88423 = CARTESIAN_POINT('Ctrl Pts',(-20.9167078074931,51.0568597260677,123.422979437591)) ;
#88424 = CARTESIAN_POINT('Ctrl Pts',(-20.8925366127019,51.0666940620848,123.68030532245)) ;
#88425 = CARTESIAN_POINT('Ctrl Pts',(-20.8233738618489,51.076727019813,123.934719313341)) ;
#88426 = CARTESIAN_POINT('Ctrl Pts',(-20.7105654023123,51.0867474183882,124.172661102908)) ;
#88427 = CARTESIAN_POINT('Ctrl Pts',(-20.5610356799522,51.0966129921594,124.384475866047)) ;
#88428 = CARTESIAN_POINT('Ctrl Pts',(-20.3732440668846,51.1066818668155,124.570842766502)) ;
#88429 = CARTESIAN_POINT('Ctrl Pts',(-20.1607562670967,51.116527297721,124.718478795522)) ;
#88430 = CARTESIAN_POINT('Ctrl Pts',(-19.9230357260641,51.1265069225917,124.829213605734)) ;
#88431 = CARTESIAN_POINT('Ctrl Pts',(-19.6685786829973,51.1365256055058,124.896772999361)) ;
#88432 = CARTESIAN_POINT('Ctrl Pts',(-19.4098095174621,51.1464088706896,124.919373434)) ;
#88433 = CARTESIAN_POINT('Ctrl Pts',(-19.1462888986317,51.156477164781,124.896167375007)) ;
#88434 = CARTESIAN_POINT('Ctrl Pts',(-18.8966808735186,51.1663072949663,124.829451529774)) ;
#88435 = CARTESIAN_POINT('Ctrl Pts',(-18.6567504696124,51.1763738431815,124.718134366409)) ;
#88436 = CARTESIAN_POINT('Ctrl Pts',(-18.4436238223543,51.1862640918701,124.569323332905)) ;
#88437 = CARTESIAN_POINT('Ctrl Pts',(-18.2573048544974,51.1962562736461,124.384316168399)) ;
#88438 = CARTESIAN_POINT('Ctrl Pts',(-18.1065797448196,51.2062190542739,124.170249228209)) ;
#88439 = CARTESIAN_POINT('Ctrl Pts',(-17.9953654455778,51.2161234589477,123.934908116965)) ;
#88440 = CARTESIAN_POINT('Ctrl Pts',(-17.925826600637,51.2261834534267,123.679876469333)) ;
#88441 = CARTESIAN_POINT('Ctrl Pts',(-17.9019091868143,51.2360320753965,123.422152612981)) ;
#88442 = CARTESIAN_POINT('Ctrl Pts',(-17.9229023529744,51.2460625148083,123.15941586086)) ;
#88443 = CARTESIAN_POINT('Ctrl Pts',(-17.9895839704234,51.2560722304431,122.904933300777)) ;
#88444 = CARTESIAN_POINT('Ctrl Pts',(-18.0981009034146,51.2659829831357,122.668199754966)) ;
#88445 = CARTESIAN_POINT('Ctrl Pts',(-18.2458319639415,51.2759122560821,122.453101902059)) ;
#88446 = CARTESIAN_POINT('Ctrl Pts',(-18.4308984169478,51.2859549474748,122.264969338689)) ;
#88447 = CARTESIAN_POINT('Ctrl Pts',(-18.6424005039535,51.2958414806923,122.114056148567)) ;
#88448 = CARTESIAN_POINT('Ctrl Pts',(-18.8792033416488,51.3058346256243,122.000563484601)) ;
#88449 = CARTESIAN_POINT('Ctrl Pts',(-19.1309552845419,51.3157803064608,121.930339339444)) ;
#88450 = CARTESIAN_POINT('Ctrl Pts',(-19.3910775718894,51.3257275636094,121.904356869132)) ;
#88451 = CARTESIAN_POINT('Ctrl Pts',(-19.6543533589848,51.3357754674813,121.924427076619)) ;
#88452 = CARTESIAN_POINT('Ctrl Pts',(-19.9051120288232,51.3456231665793,121.988392795178)) ;
#88453 = CARTESIAN_POINT('Ctrl Pts',(-20.144008897239,51.355584657558,122.095399647996)) ;
#88454 = CARTESIAN_POINT('Ctrl Pts',(-20.3619945141337,51.3656141199719,122.24356719647)) ;
#88455 = CARTESIAN_POINT('Ctrl Pts',(-20.5487308944332,51.3755213510718,122.424986082512)) ;
#88456 = CARTESIAN_POINT('Ctrl Pts',(-20.7021540436023,51.3854677297493,122.636582411564)) ;
#88457 = CARTESIAN_POINT('Ctrl Pts',(-20.8172786899295,51.3954724985581,122.872977021104)) ;
#88458 = CARTESIAN_POINT('Ctrl Pts',(-20.889429832364,51.4054936195783,123.126239425325)) ;
#88459 = CARTESIAN_POINT('Ctrl Pts',(-20.9164566681768,51.4153844854309,123.384761481474)) ;
#88460 = CARTESIAN_POINT('Ctrl Pts',(-20.8983887932973,51.4253752941902,123.646672004827)) ;
#88461 = CARTESIAN_POINT('Ctrl Pts',(-20.835318400747,51.4353259523705,123.900458111221)) ;
#88462 = CARTESIAN_POINT('Ctrl Pts',(-20.7296282507546,51.4452621620126,124.139202828454)) ;
#88463 = CARTESIAN_POINT('Ctrl Pts',(-20.5836546019347,51.4552453287375,124.357227797165)) ;
#88464 = CARTESIAN_POINT('Ctrl Pts',(-20.4006303942084,51.4652891259478,124.547361584233)) ;
#88465 = CARTESIAN_POINT('Ctrl Pts',(-20.192254850081,51.4751173421161,124.700025669877)) ;
#88466 = CARTESIAN_POINT('Ctrl Pts',(-19.9548227665226,51.4851939095853,124.81714527759)) ;
#88467 = CARTESIAN_POINT('Ctrl Pts',(-19.7062541409025,51.4950459952747,124.889764801909)) ;
#88468 = CARTESIAN_POINT('Ctrl Pts',(-19.4431990726262,51.5051192626801,124.918970553885)) ;
#88469 = CARTESIAN_POINT('Ctrl Pts',(-19.1850914917787,51.5149606791037,124.902372431121)) ;
#88470 = CARTESIAN_POINT('Ctrl Pts',(-18.9305244646705,51.5249219372464,124.841424401148)) ;
#88471 = CARTESIAN_POINT('Ctrl Pts',(-18.6887877930121,51.5349586136784,124.735942523709)) ;
#88472 = CARTESIAN_POINT('Ctrl Pts',(-18.4722292764915,51.5448372215422,124.592733444186)) ;
#88473 = CARTESIAN_POINT('Ctrl Pts',(-18.2803671864941,51.554897450181,124.410900084706)) ;
#88474 = CARTESIAN_POINT('Ctrl Pts',(-18.1259134655434,51.5647644343418,124.202585813997)) ;
#88475 = CARTESIAN_POINT('Ctrl Pts',(-18.0079247984675,51.5747700005945,123.96764851309)) ;
#88476 = CARTESIAN_POINT('Ctrl Pts',(-17.9327258735387,51.5847537890091,123.716244471843)) ;
#88477 = CARTESIAN_POINT('Ctrl Pts',(-17.9024259130523,51.5947996458117,123.454016015245)) ;
#88478 = CARTESIAN_POINT('Ctrl Pts',(-17.917439480721,51.6046255230277,123.196237952779)) ;
#88479 = CARTESIAN_POINT('Ctrl Pts',(-17.9771454730441,51.614615998869,122.940577894991)) ;
#88480 = CARTESIAN_POINT('Ctrl Pts',(-18.0815215144472,51.6246595747678,122.698158310666)) ;
#88481 = CARTESIAN_POINT('Ctrl Pts',(-18.2227516785276,51.6344813670658,122.482120314041)) ;
#88482 = CARTESIAN_POINT('Ctrl Pts',(-18.40270986864,51.6445163326917,122.289358503398)) ;
#88483 = CARTESIAN_POINT('Ctrl Pts',(-18.6136393360001,51.6545412496248,122.13151278075)) ;
#88484 = CARTESIAN_POINT('Ctrl Pts',(-18.8444580637235,51.6643931880009,122.014234397312)) ;
#88485 = CARTESIAN_POINT('Ctrl Pts',(-19.0954754548516,51.6743841640256,121.9373786769)) ;
#88486 = CARTESIAN_POINT('Ctrl Pts',(-19.3541618616858,51.6843019848293,121.905328500858)) ;
#88487 = CARTESIAN_POINT('Ctrl Pts',(-19.617334158459,51.6943307053939,121.918784864329)) ;
#88488 = CARTESIAN_POINT('Ctrl Pts',(-19.8705294306841,51.7042136320031,121.976713058442)) ;
#88489 = CARTESIAN_POINT('Ctrl Pts',(-20.1128710137296,51.7142179171226,122.078557970596)) ;
#88490 = CARTESIAN_POINT('Ctrl Pts',(-20.3334390737872,51.7242015983304,122.220706430317)) ;
#88491 = CARTESIAN_POINT('Ctrl Pts',(-20.526827334217,51.7342425970603,122.400195572372)) ;
#88492 = CARTESIAN_POINT('Ctrl Pts',(-20.6831082514724,51.7440750419275,122.60596620502)) ;
#88493 = CARTESIAN_POINT('Ctrl Pts',(-20.8039234261917,51.7540700403578,122.839180993671)) ;
#88494 = CARTESIAN_POINT('Ctrl Pts',(-20.8821642141018,51.7641015891074,123.090935669259)) ;
#88495 = CARTESIAN_POINT('Ctrl Pts',(-20.915271599229,51.7739669674129,123.348051007155)) ;
#88496 = CARTESIAN_POINT('Ctrl Pts',(-20.9038525681082,51.7839288148732,123.609596824492)) ;
#88497 = CARTESIAN_POINT('Ctrl Pts',(-20.8463633745007,51.7939637556874,123.866947061797)) ;
#88498 = CARTESIAN_POINT('Ctrl Pts',(-20.7469611887257,51.8038487167046,124.106982513468)) ;
#88499 = CARTESIAN_POINT('Ctrl Pts',(-20.6048348390858,51.8139143256234,124.330017808425)) ;
#88500 = CARTESIAN_POINT('Ctrl Pts',(-20.4302962655908,51.8237535006651,124.520838097593)) ;
#88501 = CARTESIAN_POINT('Ctrl Pts',(-20.2209018146829,51.833816056165,124.682277389154)) ;
#88502 = CARTESIAN_POINT('Ctrl Pts',(-19.9903358407335,51.843713230858,124.802662438006)) ;
#88503 = CARTESIAN_POINT('Ctrl Pts',(-19.7418135968401,51.8536439457813,124.882280836008)) ;
#88504 = CARTESIAN_POINT('Ctrl Pts',(-19.4802517626863,51.8636879738589,124.917639362177)) ;
#88505 = CARTESIAN_POINT('Ctrl Pts',(-19.2206361067492,51.8735741757122,124.907413635339)) ;
#88506 = CARTESIAN_POINT('Ctrl Pts',(-18.9639533078119,51.8835673421791,124.852066742979)) ;
#88507 = CARTESIAN_POINT('Ctrl Pts',(-18.7220007871068,51.8935068131662,124.753573074232)) ;
#88508 = CARTESIAN_POINT('Ctrl Pts',(-18.4991343218233,51.9035233275204,124.613563016952)) ;
#88509 = CARTESIAN_POINT('Ctrl Pts',(-18.3054534957154,51.9134533539972,124.438628708333)) ;
#88510 = CARTESIAN_POINT('Ctrl Pts',(-18.1432387360808,51.9235058895067,124.230157322887)) ;
#88511 = CARTESIAN_POINT('Ctrl Pts',(-18.02207359166,51.9333522927264,124.001515921378)) ;
#88512 = CARTESIAN_POINT('Ctrl Pts',(-17.9407164669733,51.9433143355804,123.752702026381)) ;
#88513 = CARTESIAN_POINT('Ctrl Pts',(-17.9038854280585,51.9533428863711,123.491731120395)) ;
#88514 = CARTESIAN_POINT('Ctrl Pts',(-17.912731672611,51.9632532120887,123.231460267867)) ;
#88515 = CARTESIAN_POINT('Ctrl Pts',(-17.966105221735,51.9731881239183,122.975886847945)) ;
#88516 = CARTESIAN_POINT('Ctrl Pts',(-18.0642983867156,51.9832291306864,122.730978652853)) ;
#88517 = CARTESIAN_POINT('Ctrl Pts',(-18.2012613019034,51.9931167635186,122.510155194213)) ;
#88518 = CARTESIAN_POINT('Ctrl Pts',(-18.3759219646091,52.0031071946166,122.314162879866)) ;
#88519 = CARTESIAN_POINT('Ctrl Pts',(-18.5813424888858,52.0130626311739,122.152141812982)) ;
#88520 = CARTESIAN_POINT('Ctrl Pts',(-18.8104988520299,52.0229735792732,122.028393562061)) ;
#88521 = CARTESIAN_POINT('Ctrl Pts',(-19.0601248152919,52.0329856553709,121.945174289692)) ;
#88522 = CARTESIAN_POINT('Ctrl Pts',(-19.3208342889526,52.0430129774459,121.907035972771)) ;
#88523 = CARTESIAN_POINT('Ctrl Pts',(-19.5798702658014,52.0528717524,121.913965038983)) ;
#88524 = CARTESIAN_POINT('Ctrl Pts',(-19.9254189752122,52.0662979452124,121.984776021455)) ;
#88525 = CARTESIAN_POINT('Ctrl Pts',(-20.2369069489131,52.0793819609939,122.139699278538)) ;
#88526 = CARTESIAN_POINT('Ctrl Pts',(-20.5025007000134,52.0928554097491,122.373739586692)) ;
#88527 = CARTESIAN_POINT('Ctrl Pts',(-20.663502478955,52.1026883675549,122.575893701772)) ;
#88528 = CARTESIAN_POINT('Ctrl Pts',(-20.7895447714591,52.1126516410056,122.80536324698)) ;
#88529 = CARTESIAN_POINT('Ctrl Pts',(-20.8739174433946,52.1226887148236,123.055264793137)) ;
#88530 = CARTESIAN_POINT('Ctrl Pts',(-20.913466812998,52.1325637178352,123.311769299998)) ;
#88531 = CARTESIAN_POINT('Ctrl Pts',(-20.907759863983,52.1426313974614,123.576238886036)) ;
#88532 = CARTESIAN_POINT('Ctrl Pts',(-20.8575136474615,52.1524722476791,123.829949405008)) ;
#88533 = CARTESIAN_POINT('Ctrl Pts',(-20.7314604670083,52.1658084461551,124.156927153833)) ;
#88534 = CARTESIAN_POINT('Ctrl Pts',(-20.5246587062285,52.1790259699695,124.440942087782)) ;
#88535 = CARTESIAN_POINT('Ctrl Pts',(-20.2524006445835,52.1923608964608,124.661535277277)) ;
#88536 = CARTESIAN_POINT('Ctrl Pts',(-20.0229908221438,52.2023439970554,124.788885516254)) ;
#88537 = CARTESIAN_POINT('Ctrl Pts',(-19.7733578676333,52.212388772955,124.874606471109)) ;
#88538 = CARTESIAN_POINT('Ctrl Pts',(-19.5185625305117,52.2222066961409,124.91526712013)) ;
#88539 = CARTESIAN_POINT('Ctrl Pts',(-19.2545108614186,52.2322560100963,124.911509845062)) ;
#88540 = CARTESIAN_POINT('Ctrl Pts',(-18.9112692834644,52.2455597507188,124.845226243308)) ;
#88541 = CARTESIAN_POINT('Ctrl Pts',(-18.5163692561841,52.2620499461955,124.6549048869)) ;
#88542 = CARTESIAN_POINT('Ctrl Pts',(-18.2061367720864,52.2787691111201,124.336934261931)) ;
#88543 = CARTESIAN_POINT('Ctrl Pts',(-18.0368883651409,52.2919301047903,124.035235554106)) ;
#88544 = CARTESIAN_POINT('Ctrl Pts',(-17.9492083451138,52.3019263268955,123.78763251036)) ;
#88545 = CARTESIAN_POINT('Ctrl Pts',(-17.9063157112242,52.3119501664292,123.527728946304)) ;
#88546 = CARTESIAN_POINT('Ctrl Pts',(-17.9093488352234,52.3251434884225,123.181008469196)) ;
#88547 = CARTESIAN_POINT('Ctrl Pts',(-18.0271239216375,52.3418026601998,122.754229453944)) ;
#88548 = CARTESIAN_POINT('Ctrl Pts',(-18.3339431995994,52.3617128356855,122.323055504623)) ;
#88549 = CARTESIAN_POINT('Ctrl Pts',(-18.7684450300349,52.3816028235299,122.021837292416)) ;
#88550 = CARTESIAN_POINT('Ctrl Pts',(-19.2825994094008,52.4016082715447,121.886694009092)) ;
#88551 = CARTESIAN_POINT('Ctrl Pts',(-19.8078170341868,52.421444665572,121.934185674863)) ;
#88552 = CARTESIAN_POINT('Ctrl Pts',(-20.289256959109,52.4414524594687,122.159679285256)) ;
#88553 = CARTESIAN_POINT('Ctrl Pts',(-20.6617455226346,52.4612790957627,122.532558034168)) ;
#88554 = CARTESIAN_POINT('Ctrl Pts',(-20.8871676648136,52.4812580387165,123.013320567925)) ;
#88555 = CARTESIAN_POINT('Ctrl Pts',(-20.9339425757462,52.5011898405856,123.540934620001)) ;
#88556 = CARTESIAN_POINT('Ctrl Pts',(-20.8002546271562,52.5210141410831,124.050758632293)) ;
#88557 = CARTESIAN_POINT('Ctrl Pts',(-20.495952731629,52.5411101424229,124.489450915891)) ;
#88558 = CARTESIAN_POINT('Ctrl Pts',(-20.0674306833606,52.5608685585269,124.793545669361)) ;
#88559 = CARTESIAN_POINT('Ctrl Pts',(-19.5529252626636,52.580962251411,124.935529369241)) ;
#88560 = CARTESIAN_POINT('Ctrl Pts',(-19.2053368719646,52.5940732173177,124.907896808842)) ;
#88561 = CARTESIAN_POINT('Ctrl Pts',(-19.0351230767564,52.6007865921055,124.864328531831)) ;
#88562 = CARTESIAN_POINT('',(-20.0093941796458,13.5522956097346,122.037202589381)) ;
#88563 = CARTESIAN_POINT('Ctrl Pts',(-20.8811762570041,12.5498512937297,123.700066866625)) ;
#88564 = CARTESIAN_POINT('Ctrl Pts',(-20.8692620836651,12.5522145745311,123.760777799691)) ;
#88565 = CARTESIAN_POINT('Ctrl Pts',(-20.8316080708744,12.5579111037291,123.905360901057)) ;
#88566 = CARTESIAN_POINT('Ctrl Pts',(-20.7388385515527,12.5668945320791,124.122491967746)) ;
#88567 = CARTESIAN_POINT('Ctrl Pts',(-20.5941950356551,12.5769520351743,124.343654958997)) ;
#88568 = CARTESIAN_POINT('Ctrl Pts',(-20.4178326753157,12.5867736915449,124.532143914003)) ;
#88569 = CARTESIAN_POINT('Ctrl Pts',(-20.2068320884318,12.59682975421,124.691210472913)) ;
#88570 = CARTESIAN_POINT('Ctrl Pts',(-19.9738765529842,12.6067704189132,124.809442393321)) ;
#88571 = CARTESIAN_POINT('Ctrl Pts',(-19.7250875546676,12.6166748228617,124.885930317569)) ;
#88572 = CARTESIAN_POINT('Ctrl Pts',(-19.4630957051046,12.6267213078553,124.918354057249)) ;
#88573 = CARTESIAN_POINT('Ctrl Pts',(-19.2033273420661,12.636617535667,124.905216890975)) ;
#88574 = CARTESIAN_POINT('Ctrl Pts',(-18.9456557927353,12.6466771192305,124.846275394572)) ;
#88575 = CARTESIAN_POINT('Ctrl Pts',(-18.7071089141504,12.6565291288993,124.74562108305)) ;
#88576 = CARTESIAN_POINT('Ctrl Pts',(-18.4867674844916,12.6664916603389,124.604252671323)) ;
#88577 = CARTESIAN_POINT('Ctrl Pts',(-18.2932471898541,12.6765232085783,124.425230066221)) ;
#88578 = CARTESIAN_POINT('Ctrl Pts',(-18.1357855764971,12.6864146197913,124.218414587344)) ;
#88579 = CARTESIAN_POINT('Ctrl Pts',(-18.0146947587827,12.6964308734993,123.984694568915)) ;
#88580 = CARTESIAN_POINT('Ctrl Pts',(-17.9364655443542,12.706460976344,123.732995067848)) ;
#88581 = CARTESIAN_POINT('Ctrl Pts',(-17.9032103304628,12.7163174252977,123.476104767026)) ;
#88582 = CARTESIAN_POINT('Ctrl Pts',(-17.9149031126223,12.72631643607,123.213643474476)) ;
#88583 = CARTESIAN_POINT('Ctrl Pts',(-17.9711347927928,12.736211652988,122.959716591098)) ;
#88584 = CARTESIAN_POINT('Ctrl Pts',(-18.0722621730133,12.7462721683453,122.715478970838)) ;
#88585 = CARTESIAN_POINT('Ctrl Pts',(-18.2111849666589,12.7561214617324,122.497067612659)) ;
#88586 = CARTESIAN_POINT('Ctrl Pts',(-18.3885653163835,12.7661486374124,122.30221638746)) ;
#88587 = CARTESIAN_POINT('Ctrl Pts',(-18.5975514154094,12.7761772130396,122.141639073802)) ;
#88588 = CARTESIAN_POINT('Ctrl Pts',(-18.8267178958733,12.7860223065854,122.021590045095)) ;
#88589 = CARTESIAN_POINT('Ctrl Pts',(-19.0767118104658,12.7960135480172,121.94132806078)) ;
#88590 = CARTESIAN_POINT('Ctrl Pts',(-19.3380817266942,12.8060493291605,121.906076455516)) ;
#88591 = CARTESIAN_POINT('Ctrl Pts',(-19.596780887396,12.8159015348902,121.916202048577)) ;
#88592 = CARTESIAN_POINT('Ctrl Pts',(-19.8527792150898,12.8258636290072,121.970959750396)) ;
#88593 = CARTESIAN_POINT('Ctrl Pts',(-20.0967365608284,12.8358861898343,122.070232238452)) ;
#88594 = CARTESIAN_POINT('Ctrl Pts',(-20.3178000252107,12.8458139614859,122.208825541157)) ;
#88595 = CARTESIAN_POINT('Ctrl Pts',(-20.5136248486434,12.8558563456107,122.38570732732)) ;
#88596 = CARTESIAN_POINT('Ctrl Pts',(-20.6733958132101,12.8657455696813,122.590690688902)) ;
#88597 = CARTESIAN_POINT('Ctrl Pts',(-20.7968031363708,12.8757348178486,122.822371490678)) ;
#88598 = CARTESIAN_POINT('Ctrl Pts',(-20.8776695418149,12.8856933948906,123.071257865387)) ;
#88599 = CARTESIAN_POINT('Ctrl Pts',(-20.9145160925794,12.8955929639819,123.328801889037)) ;
#88600 = CARTESIAN_POINT('Ctrl Pts',(-20.9058665992661,12.9056408760659,123.592681474373)) ;
#88601 = CARTESIAN_POINT('Ctrl Pts',(-20.8525411197741,12.9155362303731,123.847236588034)) ;
#88602 = CARTESIAN_POINT('Ctrl Pts',(-20.7542629977426,12.9255978808643,124.092671346512)) ;
#88603 = CARTESIAN_POINT('Ctrl Pts',(-20.6178824497922,12.9354424963268,124.312521389387)) ;
#88604 = CARTESIAN_POINT('Ctrl Pts',(-20.4440872979319,12.9454025752282,124.508228135365)) ;
#88605 = CARTESIAN_POINT('Ctrl Pts',(-20.2370284211193,12.9554407695865,124.671653791003)) ;
#88606 = CARTESIAN_POINT('Ctrl Pts',(-20.008735431722,12.9653144849861,124.795042874335)) ;
#88607 = CARTESIAN_POINT('Ctrl Pts',(-19.7576063109488,12.9753861945204,124.878511544747)) ;
#88608 = CARTESIAN_POINT('Ctrl Pts',(-19.5019831838198,12.9852186349729,124.916346652394)) ;
#88609 = CARTESIAN_POINT('Ctrl Pts',(-19.2384448043294,12.9952504558983,124.909813965164)) ;
#88610 = CARTESIAN_POINT('Ctrl Pts',(-18.9804789488314,13.0052708257839,124.856943439991)) ;
#88611 = CARTESIAN_POINT('Ctrl Pts',(-18.7391020985709,13.0151375969176,124.762195065093)) ;
#88612 = CARTESIAN_POINT('Ctrl Pts',(-18.5133119731303,13.025208368107,124.624195283185)) ;
#88613 = CARTESIAN_POINT('Ctrl Pts',(-18.3193460395093,13.0350515286286,124.453039947988)) ;
#88614 = CARTESIAN_POINT('Ctrl Pts',(-18.1551409871327,13.045031761815,124.248545739038)) ;
#88615 = CARTESIAN_POINT('Ctrl Pts',(-18.0288968334375,13.0550502818502,124.01751953666)) ;
#88616 = CARTESIAN_POINT('Ctrl Pts',(-17.9452843626105,13.0649335902339,123.771589310434)) ;
#88617 = CARTESIAN_POINT('Ctrl Pts',(-17.9050279627347,13.0750018744047,123.510130021932)) ;
#88618 = CARTESIAN_POINT('Ctrl Pts',(-17.9103427016909,13.0848320010723,123.251814495464)) ;
#88619 = CARTESIAN_POINT('Ctrl Pts',(-17.9612809092981,13.0948985732789,122.992269532793)) ;
#88620 = CARTESIAN_POINT('Ctrl Pts',(-18.0550171292814,13.1047887295196,122.749822905915)) ;
#88621 = CARTESIAN_POINT('Ctrl Pts',(-18.1903054658587,13.114781257096,122.524782428398)) ;
#88622 = CARTESIAN_POINT('Ctrl Pts',(-18.3622584156365,13.1247427469703,122.327401305476)) ;
#88623 = CARTESIAN_POINT('Ctrl Pts',(-18.5644359884156,13.1346519688575,122.163265725879)) ;
#88624 = CARTESIAN_POINT('Ctrl Pts',(-18.7952652342093,13.1447005486678,122.035044644749)) ;
#88625 = CARTESIAN_POINT('Ctrl Pts',(-19.0407361930169,13.1545835231379,121.950173803814)) ;
#88626 = CARTESIAN_POINT('Ctrl Pts',(-19.3000068336127,13.1645784342806,121.908192940554)) ;
#88627 = CARTESIAN_POINT('Ctrl Pts',(-19.5633186687248,13.1745988208542,121.912239958628)) ;
#88628 = CARTESIAN_POINT('Ctrl Pts',(-19.8190763964686,13.1845089247113,121.961246286646)) ;
#88629 = CARTESIAN_POINT('Ctrl Pts',(-20.0631402215822,13.1944366369212,122.053450497386)) ;
#88630 = CARTESIAN_POINT('Ctrl Pts',(-20.2899638294564,13.2044797466884,122.188360062557)) ;
#88631 = CARTESIAN_POINT('Ctrl Pts',(-20.4869257177344,13.214366167144,122.35780741445)) ;
#88632 = CARTESIAN_POINT('Ctrl Pts',(-20.6535775719235,13.2243593447496,122.560745126669)) ;
#88633 = CARTESIAN_POINT('Ctrl Pts',(-20.781768758078,13.2343050076535,122.788511159415)) ;
#88634 = CARTESIAN_POINT('Ctrl Pts',(-20.8689866491185,13.2442523038587,123.034949721076)) ;
#88635 = CARTESIAN_POINT('Ctrl Pts',(-20.9122331010744,13.2543000694366,123.295421612396)) ;
#88636 = CARTESIAN_POINT('Ctrl Pts',(-20.9098535935215,13.2641482826542,123.554208720169)) ;
#88637 = CARTESIAN_POINT('Ctrl Pts',(-20.862891829645,13.2741078554483,123.811687555265)) ;
#88638 = CARTESIAN_POINT('Ctrl Pts',(-20.7708019573289,13.2841444764808,124.058831482253)) ;
#88639 = CARTESIAN_POINT('Ctrl Pts',(-20.6396072016662,13.2940249912912,124.282931024446)) ;
#88640 = CARTESIAN_POINT('Ctrl Pts',(-20.4686846093292,13.3040776425982,124.484308739774)) ;
#88641 = CARTESIAN_POINT('Ctrl Pts',(-20.2685764087636,13.3139730408782,124.650446241866)) ;
#88642 = CARTESIAN_POINT('Ctrl Pts',(-20.0392572485433,13.3240231625843,124.781393384691)) ;
#88643 = CARTESIAN_POINT('Ctrl Pts',(-19.7947435724965,13.3339074421262,124.869123479395)) ;
#88644 = CARTESIAN_POINT('Ctrl Pts',(-19.5359835923959,13.3439022234181,124.914032922456)) ;
#88645 = CARTESIAN_POINT('Ctrl Pts',(-19.2745480154649,13.3538500686049,124.913233748315)) ;
#88646 = CARTESIAN_POINT('Ctrl Pts',(-19.0174771736584,13.3637870319923,124.867483970433)) ;
#88647 = CARTESIAN_POINT('Ctrl Pts',(-18.770953528208,13.3737699967295,124.777666914607)) ;
#88648 = CARTESIAN_POINT('Ctrl Pts',(-18.5426825818329,13.3838138481452,124.645222231553)) ;
#88649 = CARTESIAN_POINT('Ctrl Pts',(-18.3447626868737,13.3936420494799,124.479227338155)) ;
#88650 = CARTESIAN_POINT('Ctrl Pts',(-18.174439114941,13.403718622078,124.276543144147)) ;
#88651 = CARTESIAN_POINT('Ctrl Pts',(-18.0446799079283,13.4135707020855,124.052439270463)) ;
#88652 = CARTESIAN_POINT('Ctrl Pts',(-17.9536328215657,13.4236439870896,123.803921128187)) ;
#88653 = CARTESIAN_POINT('Ctrl Pts',(-17.908245672822,13.4334853388001,123.549293611183)) ;
#88654 = CARTESIAN_POINT('Ctrl Pts',(-17.9067874767793,13.4434468381966,123.287535568875)) ;
#88655 = CARTESIAN_POINT('Ctrl Pts',(-17.9515894545495,13.4534826143266,123.027629899913)) ;
#88656 = CARTESIAN_POINT('Ctrl Pts',(-18.0392686443259,13.4633710409642,122.783013986504)) ;
#88657 = CARTESIAN_POINT('Ctrl Pts',(-18.1693153244225,13.4733863630391,122.554183172307)) ;
#88658 = CARTESIAN_POINT('Ctrl Pts',(-18.3378376719635,13.4834167119393,122.35150318048)) ;
#88659 = CARTESIAN_POINT('Ctrl Pts',(-18.5349010784944,13.493260087546,122.183945153477)) ;
#88660 = CARTESIAN_POINT('Ctrl Pts',(-18.761992836842,13.5032895244431,122.050165209368)) ;
#88661 = CARTESIAN_POINT('Ctrl Pts',(-19.0091803607605,13.513321402376,121.958500067657)) ;
#88662 = CARTESIAN_POINT('Ctrl Pts',(-19.2631820189547,13.5231510254815,121.911588708017)) ;
#88663 = CARTESIAN_POINT('Ctrl Pts',(-19.5256857167379,13.5331404966346,121.908671418978)) ;
#88664 = CARTESIAN_POINT('Ctrl Pts',(-19.7794742643537,13.5429325945739,121.95117720022)) ;
#88665 = CARTESIAN_POINT('Ctrl Pts',(-19.9360895547681,13.5492395742091,122.005136428262)) ;
#88666 = CARTESIAN_POINT('Ctrl Pts',(-20.0093941796458,13.5522956097346,122.037202589381)) ;
#88667 = CARTESIAN_POINT('Ctrl Pts',(-19.3053878987309,13.6947924674762,122.201356690921)) ;
#88668 = CARTESIAN_POINT('Ctrl Pts',(-19.356349637348,13.6822848109803,122.171875951815)) ;
#88669 = CARTESIAN_POINT('Ctrl Pts',(-19.4101184737497,13.6698676303486,122.14590971193)) ;
#88670 = CARTESIAN_POINT('Ctrl Pts',(-19.5160286269017,13.6467016771096,122.104119584246)) ;
#88671 = CARTESIAN_POINT('Ctrl Pts',(-19.5746444702855,13.6345804393052,122.08517512299)) ;
#88672 = CARTESIAN_POINT('Ctrl Pts',(-19.7010870355378,13.6094612987591,122.056219247648)) ;
#88673 = CARTESIAN_POINT('Ctrl Pts',(-19.7611384259661,13.5978109265327,122.046461245458)) ;
#88674 = CARTESIAN_POINT('Ctrl Pts',(-19.8838264753735,13.5747381235504,122.035109517786)) ;
#88675 = CARTESIAN_POINT('Ctrl Pts',(-19.9460097293868,13.5635055402564,122.033994044163)) ;
#88676 = CARTESIAN_POINT('Ctrl Pts',(-20.0093941796457,13.5522956097346,122.037202589381)) ;
#88677 = CARTESIAN_POINT('Ctrl Pts',(-20.8283360085486,11.7999200508426,122.926058340311)) ;
#88678 = CARTESIAN_POINT('Ctrl Pts',(-20.8845464538574,11.8065469016607,123.090182099353)) ;
#88679 = CARTESIAN_POINT('Ctrl Pts',(-20.9394674069342,11.8197775281417,123.437524293028)) ;
#88680 = CARTESIAN_POINT('Ctrl Pts',(-20.8387914871724,11.8397531494004,123.958813977782)) ;
#88681 = CARTESIAN_POINT('Ctrl Pts',(-20.5666784354472,11.8596704843023,124.412866308854)) ;
#88682 = CARTESIAN_POINT('Ctrl Pts',(-20.1575619136445,11.8795437610183,124.747046208683)) ;
#88683 = CARTESIAN_POINT('Ctrl Pts',(-19.6551371496748,11.8995682511823,124.92249916066)) ;
#88684 = CARTESIAN_POINT('Ctrl Pts',(-19.1270451744641,11.919436092333,124.915907267661)) ;
#88685 = CARTESIAN_POINT('Ctrl Pts',(-18.6308008607008,11.9393817432125,124.729592278927)) ;
#88686 = CARTESIAN_POINT('Ctrl Pts',(-18.2288280457431,11.9592871438295,124.385624086374)) ;
#88687 = CARTESIAN_POINT('Ctrl Pts',(-17.9678591535732,11.9791613716459,123.926365470291)) ;
#88688 = CARTESIAN_POINT('Ctrl Pts',(-17.8787398474485,11.9991471625235,123.402691583813)) ;
#88689 = CARTESIAN_POINT('Ctrl Pts',(-17.9735233382965,12.0190414051832,122.882536434516)) ;
#88690 = CARTESIAN_POINT('Ctrl Pts',(-18.2387585289407,12.0389201212553,122.425519450945)) ;
#88691 = CARTESIAN_POINT('Ctrl Pts',(-18.6476197278655,12.0589595710999,122.084275218605)) ;
#88692 = CARTESIAN_POINT('Ctrl Pts',(-19.1441777499651,12.0788227326378,121.904537351317)) ;
#88693 = CARTESIAN_POINT('Ctrl Pts',(-19.6750288445506,12.098802100652,121.904738156225)) ;
#88694 = CARTESIAN_POINT('Ctrl Pts',(-20.1701856143784,12.1186126811748,122.084100255283)) ;
#88695 = CARTESIAN_POINT('Ctrl Pts',(-20.5782317220315,12.1385936094604,122.423828694064)) ;
#88696 = CARTESIAN_POINT('Ctrl Pts',(-20.8444525967082,12.1584862813298,122.880697423595)) ;
#88697 = CARTESIAN_POINT('Ctrl Pts',(-20.9398398136422,12.1784126116169,123.401645628938)) ;
#88698 = CARTESIAN_POINT('Ctrl Pts',(-20.851062860932,12.1983831657092,123.924943760388)) ;
#88699 = CARTESIAN_POINT('Ctrl Pts',(-20.6345502730467,12.2149150047968,124.307289073383)) ;
#88700 = CARTESIAN_POINT('Ctrl Pts',(-20.3891153931417,12.2282547436244,124.557618291671)) ;
#88701 = CARTESIAN_POINT('Ctrl Pts',(-20.1744356948872,12.238286985843,124.71063155409)) ;
#88702 = CARTESIAN_POINT('Ctrl Pts',(-19.9407461181023,12.2481446864865,124.82243808738)) ;
#88703 = CARTESIAN_POINT('Ctrl Pts',(-19.6879479903912,12.2581365511257,124.893369098924)) ;
#88704 = CARTESIAN_POINT('Ctrl Pts',(-19.4284766803744,12.2680591008858,124.919096784819)) ;
#88705 = CARTESIAN_POINT('Ctrl Pts',(-19.0804161519456,12.2813368743793,124.893600455121)) ;
#88706 = CARTESIAN_POINT('Ctrl Pts',(-18.7455915471493,12.2946842133199,124.776633305253)) ;
#88707 = CARTESIAN_POINT('Ctrl Pts',(-18.4584578761078,12.3078914451131,124.581565716411)) ;
#88708 = CARTESIAN_POINT('Ctrl Pts',(-18.2699644759195,12.3178785612028,124.39900581103)) ;
#88709 = CARTESIAN_POINT('Ctrl Pts',(-18.1163990348321,12.3278294667826,124.187285865335)) ;
#88710 = CARTESIAN_POINT('Ctrl Pts',(-18.0010402192528,12.33788456879,123.949600254045)) ;
#88711 = CARTESIAN_POINT('Ctrl Pts',(-17.9299289800127,12.3477062421111,123.701455973458)) ;
#88712 = CARTESIAN_POINT('Ctrl Pts',(-17.9019096964941,12.357764713186,123.438645136577)) ;
#88713 = CARTESIAN_POINT('Ctrl Pts',(-17.9200603909808,12.3676893243625,123.178453886709)) ;
#88714 = CARTESIAN_POINT('Ctrl Pts',(-18.0035385415921,12.3809666632629,122.839641054544)) ;
#88715 = CARTESIAN_POINT('Ctrl Pts',(-18.1740845283454,12.3942655425005,122.530112925337)) ;
#88716 = CARTESIAN_POINT('Ctrl Pts',(-18.4148347268114,12.4075044146712,122.278925757333)) ;
#88717 = CARTESIAN_POINT('Ctrl Pts',(-18.626729428275,12.4175110328078,122.123187062121)) ;
#88718 = CARTESIAN_POINT('Ctrl Pts',(-18.8632335737039,12.4275419778693,122.006787551109)) ;
#88719 = CARTESIAN_POINT('Ctrl Pts',(-19.1118364896857,12.4373981512211,121.934037501767)) ;
#88720 = CARTESIAN_POINT('Ctrl Pts',(-19.3729328187221,12.447397422184,121.904821743981)) ;
#88721 = CARTESIAN_POINT('Ctrl Pts',(-19.6324990778504,12.4572918739413,121.920913539679)) ;
#88722 = CARTESIAN_POINT('Ctrl Pts',(-19.8895297331301,12.4673551897507,121.982929816623)) ;
#88723 = CARTESIAN_POINT('Ctrl Pts',(-20.1266869407979,12.4771940464903,122.086036295395)) ;
#88724 = CARTESIAN_POINT('Ctrl Pts',(-20.3474074551281,12.4872601683079,122.231757371538)) ;
#88725 = CARTESIAN_POINT('Ctrl Pts',(-20.5359559653956,12.4971433960322,122.410425895404)) ;
#88726 = CARTESIAN_POINT('Ctrl Pts',(-20.6927050538892,12.5071328573109,122.620969850052)) ;
#88727 = CARTESIAN_POINT('Ctrl Pts',(-20.810144830431,12.5170965677374,122.855005173606)) ;
#88728 = CARTESIAN_POINT('Ctrl Pts',(-20.8856671720647,12.5270915704683,123.106592117066)) ;
#88729 = CARTESIAN_POINT('Ctrl Pts',(-20.916070552576,12.5371279014786,123.36856478643)) ;
#88730 = CARTESIAN_POINT('Ctrl Pts',(-20.9012433064245,12.5469741308209,123.62690469604)) ;
#88731 = CARTESIAN_POINT('Ctrl Pts',(-20.8414337010136,12.5569596290961,123.882363589347)) ;
#88732 = CARTESIAN_POINT('Ctrl Pts',(-20.7388385515527,12.5668945320791,124.122491967746)) ;
#88733 = CARTESIAN_POINT('Ctrl Pts',(-20.5941950356551,12.5769520351743,124.343654958997)) ;
#88734 = CARTESIAN_POINT('Ctrl Pts',(-20.4178326753157,12.5867736915449,124.532143914003)) ;
#88735 = CARTESIAN_POINT('Ctrl Pts',(-20.2068320884318,12.59682975421,124.691210472913)) ;
#88736 = CARTESIAN_POINT('Ctrl Pts',(-19.9738765529842,12.6067704189132,124.809442393321)) ;
#88737 = CARTESIAN_POINT('Ctrl Pts',(-19.7250875546676,12.6166748228617,124.885930317569)) ;
#88738 = CARTESIAN_POINT('Ctrl Pts',(-19.4630957051046,12.6267213078553,124.918354057249)) ;
#88739 = CARTESIAN_POINT('Ctrl Pts',(-19.2033273420661,12.636617535667,124.905216890975)) ;
#88740 = CARTESIAN_POINT('Ctrl Pts',(-18.9456557927353,12.6466771192305,124.846275394572)) ;
#88741 = CARTESIAN_POINT('Ctrl Pts',(-18.7071089141504,12.6565291288993,124.74562108305)) ;
#88742 = CARTESIAN_POINT('Ctrl Pts',(-18.4867674844916,12.6664916603389,124.604252671323)) ;
#88743 = CARTESIAN_POINT('Ctrl Pts',(-18.2932471898541,12.6765232085783,124.425230066221)) ;
#88744 = CARTESIAN_POINT('Ctrl Pts',(-18.1357855764971,12.6864146197913,124.218414587344)) ;
#88745 = CARTESIAN_POINT('Ctrl Pts',(-18.0146947587827,12.6964308734993,123.984694568915)) ;
#88746 = CARTESIAN_POINT('Ctrl Pts',(-17.9364655443542,12.706460976344,123.732995067848)) ;
#88747 = CARTESIAN_POINT('Ctrl Pts',(-17.9032103304628,12.7163174252977,123.476104767026)) ;
#88748 = CARTESIAN_POINT('Ctrl Pts',(-17.9149031126223,12.72631643607,123.213643474476)) ;
#88749 = CARTESIAN_POINT('Ctrl Pts',(-17.9711347927928,12.736211652988,122.959716591098)) ;
#88750 = CARTESIAN_POINT('Ctrl Pts',(-18.0722621730133,12.7462721683453,122.715478970838)) ;
#88751 = CARTESIAN_POINT('Ctrl Pts',(-18.2111849666589,12.7561214617324,122.497067612659)) ;
#88752 = CARTESIAN_POINT('Ctrl Pts',(-18.3885653163835,12.7661486374124,122.30221638746)) ;
#88753 = CARTESIAN_POINT('Ctrl Pts',(-18.5975514154094,12.7761772130396,122.141639073802)) ;
#88754 = CARTESIAN_POINT('Ctrl Pts',(-18.8267178958733,12.7860223065854,122.021590045095)) ;
#88755 = CARTESIAN_POINT('Ctrl Pts',(-19.0767118104658,12.7960135480172,121.94132806078)) ;
#88756 = CARTESIAN_POINT('Ctrl Pts',(-19.3380817266942,12.8060493291605,121.906076455516)) ;
#88757 = CARTESIAN_POINT('Ctrl Pts',(-19.596780887396,12.8159015348902,121.916202048577)) ;
#88758 = CARTESIAN_POINT('Ctrl Pts',(-19.8527792150898,12.8258636290072,121.970959750396)) ;
#88759 = CARTESIAN_POINT('Ctrl Pts',(-20.0967365608284,12.8358861898343,122.070232238452)) ;
#88760 = CARTESIAN_POINT('Ctrl Pts',(-20.3178000252107,12.8458139614859,122.208825541157)) ;
#88761 = CARTESIAN_POINT('Ctrl Pts',(-20.5136248486434,12.8558563456107,122.38570732732)) ;
#88762 = CARTESIAN_POINT('Ctrl Pts',(-20.67339581321,12.8657455696813,122.590690688902)) ;
#88763 = CARTESIAN_POINT('Ctrl Pts',(-20.7968031363708,12.8757348178486,122.822371490678)) ;
#88764 = CARTESIAN_POINT('Ctrl Pts',(-20.8776695418149,12.8856933948906,123.071257865387)) ;
#88765 = CARTESIAN_POINT('Ctrl Pts',(-20.9145160925794,12.8955929639819,123.328801889037)) ;
#88766 = CARTESIAN_POINT('Ctrl Pts',(-20.9058665992661,12.9056408760659,123.592681474373)) ;
#88767 = CARTESIAN_POINT('Ctrl Pts',(-20.8525411197741,12.9155362303731,123.847236588034)) ;
#88768 = CARTESIAN_POINT('Ctrl Pts',(-20.7542629977425,12.9255978808643,124.092671346512)) ;
#88769 = CARTESIAN_POINT('Ctrl Pts',(-20.6178824497922,12.9354424963268,124.312521389387)) ;
#88770 = CARTESIAN_POINT('Ctrl Pts',(-20.4440872979319,12.9454025752282,124.508228135365)) ;
#88771 = CARTESIAN_POINT('Ctrl Pts',(-20.2370284211193,12.9554407695865,124.671653791003)) ;
#88772 = CARTESIAN_POINT('Ctrl Pts',(-20.008735431722,12.9653144849861,124.795042874335)) ;
#88773 = CARTESIAN_POINT('Ctrl Pts',(-19.7576063109488,12.9753861945204,124.878511544747)) ;
#88774 = CARTESIAN_POINT('Ctrl Pts',(-19.5019831838198,12.9852186349729,124.916346652394)) ;
#88775 = CARTESIAN_POINT('Ctrl Pts',(-19.2384448043294,12.9952504558983,124.909813965164)) ;
#88776 = CARTESIAN_POINT('Ctrl Pts',(-18.9804789488314,13.0052708257839,124.856943439991)) ;
#88777 = CARTESIAN_POINT('Ctrl Pts',(-18.7391020985709,13.0151375969176,124.762195065093)) ;
#88778 = CARTESIAN_POINT('Ctrl Pts',(-18.5133119731303,13.025208368107,124.624195283185)) ;
#88779 = CARTESIAN_POINT('Ctrl Pts',(-18.3193460395093,13.0350515286286,124.453039947988)) ;
#88780 = CARTESIAN_POINT('Ctrl Pts',(-18.1551409871327,13.045031761815,124.248545739038)) ;
#88781 = CARTESIAN_POINT('Ctrl Pts',(-18.0288968334375,13.0550502818502,124.01751953666)) ;
#88782 = CARTESIAN_POINT('Ctrl Pts',(-17.9452843626105,13.0649335902339,123.771589310434)) ;
#88783 = CARTESIAN_POINT('Ctrl Pts',(-17.9050279627347,13.0750018744047,123.510130021932)) ;
#88784 = CARTESIAN_POINT('Ctrl Pts',(-17.9103427016909,13.0848320010723,123.251814495464)) ;
#88785 = CARTESIAN_POINT('Ctrl Pts',(-17.9612809092981,13.0948985732789,122.992269532793)) ;
#88786 = CARTESIAN_POINT('Ctrl Pts',(-18.0550171292814,13.1047887295196,122.749822905915)) ;
#88787 = CARTESIAN_POINT('Ctrl Pts',(-18.1903054658587,13.114781257096,122.524782428398)) ;
#88788 = CARTESIAN_POINT('Ctrl Pts',(-18.3622584156365,13.1247427469703,122.327401305476)) ;
#88789 = CARTESIAN_POINT('Ctrl Pts',(-18.5644359884156,13.1346519688575,122.163265725879)) ;
#88790 = CARTESIAN_POINT('Ctrl Pts',(-18.7952652342093,13.1447005486678,122.035044644749)) ;
#88791 = CARTESIAN_POINT('Ctrl Pts',(-19.0407361930169,13.1545835231379,121.950173803814)) ;
#88792 = CARTESIAN_POINT('Ctrl Pts',(-19.3000068336127,13.1645784342806,121.908192940554)) ;
#88793 = CARTESIAN_POINT('Ctrl Pts',(-19.5633186687248,13.1745988208542,121.912239958628)) ;
#88794 = CARTESIAN_POINT('Ctrl Pts',(-19.8190763964686,13.1845089247113,121.961246286646)) ;
#88795 = CARTESIAN_POINT('Ctrl Pts',(-20.0631402215822,13.1944366369212,122.053450497386)) ;
#88796 = CARTESIAN_POINT('Ctrl Pts',(-20.2899638294564,13.2044797466884,122.188360062557)) ;
#88797 = CARTESIAN_POINT('Ctrl Pts',(-20.4869257177344,13.214366167144,122.35780741445)) ;
#88798 = CARTESIAN_POINT('Ctrl Pts',(-20.6535775719235,13.2243593447496,122.560745126669)) ;
#88799 = CARTESIAN_POINT('Ctrl Pts',(-20.781768758078,13.2343050076535,122.788511159415)) ;
#88800 = CARTESIAN_POINT('Ctrl Pts',(-20.8689866491185,13.2442523038587,123.034949721076)) ;
#88801 = CARTESIAN_POINT('Ctrl Pts',(-20.9122331010744,13.2543000694366,123.295421612396)) ;
#88802 = CARTESIAN_POINT('Ctrl Pts',(-20.9098535935215,13.2641482826542,123.554208720169)) ;
#88803 = CARTESIAN_POINT('Ctrl Pts',(-20.862891829645,13.2741078554483,123.811687555265)) ;
#88804 = CARTESIAN_POINT('Ctrl Pts',(-20.7708019573289,13.2841444764808,124.058831482253)) ;
#88805 = CARTESIAN_POINT('Ctrl Pts',(-20.6396072016662,13.2940249912912,124.282931024446)) ;
#88806 = CARTESIAN_POINT('Ctrl Pts',(-20.4686846093292,13.3040776425982,124.484308739774)) ;
#88807 = CARTESIAN_POINT('Ctrl Pts',(-20.2685764087636,13.3139730408782,124.650446241866)) ;
#88808 = CARTESIAN_POINT('Ctrl Pts',(-20.0392572485433,13.3240231625843,124.781393384691)) ;
#88809 = CARTESIAN_POINT('Ctrl Pts',(-19.7947435724965,13.3339074421262,124.869123479395)) ;
#88810 = CARTESIAN_POINT('Ctrl Pts',(-19.5359835923959,13.3439022234181,124.914032922456)) ;
#88811 = CARTESIAN_POINT('Ctrl Pts',(-19.2745480154649,13.3538500686049,124.913233748315)) ;
#88812 = CARTESIAN_POINT('Ctrl Pts',(-19.0174771736584,13.3637870319923,124.867483970433)) ;
#88813 = CARTESIAN_POINT('Ctrl Pts',(-18.770953528208,13.3737699967295,124.777666914607)) ;
#88814 = CARTESIAN_POINT('Ctrl Pts',(-18.5426825818329,13.3838138481452,124.645222231553)) ;
#88815 = CARTESIAN_POINT('Ctrl Pts',(-18.3447626868737,13.3936420494799,124.479227338155)) ;
#88816 = CARTESIAN_POINT('Ctrl Pts',(-18.174439114941,13.403718622078,124.276543144147)) ;
#88817 = CARTESIAN_POINT('Ctrl Pts',(-18.0446799079283,13.4135707020855,124.052439270463)) ;
#88818 = CARTESIAN_POINT('Ctrl Pts',(-17.9536328215657,13.4236439870896,123.803921128187)) ;
#88819 = CARTESIAN_POINT('Ctrl Pts',(-17.908245672822,13.4334853388001,123.549293611183)) ;
#88820 = CARTESIAN_POINT('Ctrl Pts',(-17.9067874767793,13.4434468381966,123.287535568875)) ;
#88821 = CARTESIAN_POINT('Ctrl Pts',(-17.9515894545495,13.4534826143266,123.027629899913)) ;
#88822 = CARTESIAN_POINT('Ctrl Pts',(-18.0392686443259,13.4633710409642,122.783013986504)) ;
#88823 = CARTESIAN_POINT('Ctrl Pts',(-18.1693153244225,13.4733863630391,122.554183172307)) ;
#88824 = CARTESIAN_POINT('Ctrl Pts',(-18.3378376719635,13.4834167119393,122.35150318048)) ;
#88825 = CARTESIAN_POINT('Ctrl Pts',(-18.5349010784944,13.493260087546,122.183945153477)) ;
#88826 = CARTESIAN_POINT('Ctrl Pts',(-18.761992836842,13.5032895244431,122.050165209368)) ;
#88827 = CARTESIAN_POINT('Ctrl Pts',(-19.0091803607605,13.513321402376,121.958500067657)) ;
#88828 = CARTESIAN_POINT('Ctrl Pts',(-19.2631820189547,13.5231510254815,121.911588708017)) ;
#88829 = CARTESIAN_POINT('Ctrl Pts',(-19.5256857167379,13.5331404966346,121.908671418978)) ;
#88830 = CARTESIAN_POINT('Ctrl Pts',(-19.7859990638554,13.543184345397,121.952270006427)) ;
#88831 = CARTESIAN_POINT('Ctrl Pts',(-20.0294662569613,13.5530060509287,122.037953136693)) ;
#88832 = CARTESIAN_POINT('Ctrl Pts',(-20.2595578583272,13.5630410907565,122.166795368885)) ;
#88833 = CARTESIAN_POINT('Ctrl Pts',(-20.4631193550347,13.573065797648,122.334030527681)) ;
#88834 = CARTESIAN_POINT('Ctrl Pts',(-20.6320196881759,13.5829185019887,122.530273988873)) ;
#88835 = CARTESIAN_POINT('Ctrl Pts',(-20.7664821078402,13.5929066241964,122.755672189208)) ;
#88836 = CARTESIAN_POINT('Ctrl Pts',(-20.8592301070909,13.6028350943037,122.999547591303)) ;
#88837 = CARTESIAN_POINT('Ctrl Pts',(-20.9089521249442,13.6128240714709,123.257308236829)) ;
#88838 = CARTESIAN_POINT('Ctrl Pts',(-20.9127323662985,13.6228618787506,123.521057016566)) ;
#88839 = CARTESIAN_POINT('Ctrl Pts',(-20.8718783998989,13.6327081796139,123.776564736996)) ;
#88840 = CARTESIAN_POINT('Ctrl Pts',(-20.7862945910431,13.6427339229932,124.025746367502)) ;
#88841 = CARTESIAN_POINT('Ctrl Pts',(-20.6580767870656,13.6527647894322,124.256070820692)) ;
#88842 = CARTESIAN_POINT('Ctrl Pts',(-20.4954356848382,13.662602148231,124.457000727745)) ;
#88843 = CARTESIAN_POINT('Ctrl Pts',(-20.2977665459096,13.6725941091647,124.629841734287)) ;
#88844 = CARTESIAN_POINT('Ctrl Pts',(-20.0718975262772,13.6826264717213,124.765837185899)) ;
#88845 = CARTESIAN_POINT('Ctrl Pts',(-19.8300805604924,13.6924916322957,124.859254064222)) ;
#88846 = CARTESIAN_POINT('Ctrl Pts',(-19.5733470333744,13.7024535368734,124.910489003739)) ;
#88847 = CARTESIAN_POINT('Ctrl Pts',(-19.3097110945833,13.7124884669491,124.915979322584)) ;
#88848 = CARTESIAN_POINT('Ctrl Pts',(-19.052903569064,13.7223734138028,124.876639088694)) ;
#88849 = CARTESIAN_POINT('Ctrl Pts',(-18.802425491904,13.7324390901142,124.791752081939)) ;
#88850 = CARTESIAN_POINT('Ctrl Pts',(-18.5755121673576,13.7422780097491,124.667718382011)) ;
#88851 = CARTESIAN_POINT('Ctrl Pts',(-18.3688230223248,13.7523415194835,124.502800514481)) ;
#88852 = CARTESIAN_POINT('Ctrl Pts',(-18.1969779972077,13.7622351326453,124.307654410282)) ;
#88853 = CARTESIAN_POINT('Ctrl Pts',(-18.0603814063974,13.7721791394587,124.084921230377)) ;
#88854 = CARTESIAN_POINT('Ctrl Pts',(-17.9638424346081,13.782180093813,123.840436569305)) ;
#88855 = CARTESIAN_POINT('Ctrl Pts',(-17.9114952956979,13.7922188515053,123.581898288947)) ;
#88856 = CARTESIAN_POINT('Ctrl Pts',(-17.9044097597817,13.8020430356753,123.323804444879)) ;
#88857 = CARTESIAN_POINT('Ctrl Pts',(-17.942755586416,13.8121011012747,123.062308840123)) ;
#88858 = CARTESIAN_POINT('Ctrl Pts',(-18.0252033616295,13.8220311480494,122.814707785698)) ;
#88859 = CARTESIAN_POINT('Ctrl Pts',(-18.1490450109907,13.8319825903865,122.58437299172)) ;
#88860 = CARTESIAN_POINT('Ctrl Pts',(-18.312830616674,13.8420293875658,122.377301209051)) ;
#88861 = CARTESIAN_POINT('Ctrl Pts',(-18.5060204476613,13.8518773282459,122.20510405819)) ;
#88862 = CARTESIAN_POINT('Ctrl Pts',(-18.7282785603277,13.8618389595885,122.066811224224)) ;
#88863 = CARTESIAN_POINT('Ctrl Pts',(-18.9729559764164,13.8718676189644,121.968851551182)) ;
#88864 = CARTESIAN_POINT('Ctrl Pts',(-19.2278374256175,13.8817779218526,121.915423966121)) ;
#88865 = CARTESIAN_POINT('Ctrl Pts',(-19.4887668418426,13.8917128164148,121.906358743324)) ;
#88866 = CARTESIAN_POINT('Ctrl Pts',(-19.7500201068666,13.9017539150817,121.943366287556)) ;
#88867 = CARTESIAN_POINT('Ctrl Pts',(-19.997114009859,13.9116411975861,122.023756349265)) ;
#88868 = CARTESIAN_POINT('Ctrl Pts',(-20.229100640813,13.9216329380966,122.146710775795)) ;
#88869 = CARTESIAN_POINT('Ctrl Pts',(-20.435328819661,13.931583487332,122.307501482509)) ;
#88870 = CARTESIAN_POINT('Ctrl Pts',(-20.610513668173,13.9415191649668,122.501085313789)) ;
#88871 = CARTESIAN_POINT('Ctrl Pts',(-20.7503773911135,13.9515045827596,122.723134407814)) ;
#88872 = CARTESIAN_POINT('Ctrl Pts',(-20.8496809192691,13.9615333756301,122.967254089343)) ;
#88873 = CARTESIAN_POINT('Ctrl Pts',(-20.9045337829199,13.9714128868581,123.221012810142)) ;
#88874 = CARTESIAN_POINT('Ctrl Pts',(-20.9152110491903,13.981406423531,123.483425425094)) ;
#88875 = CARTESIAN_POINT('Ctrl Pts',(-20.8794859206276,13.9914386917948,123.744619970286)) ;
#88876 = CARTESIAN_POINT('Ctrl Pts',(-20.8008196116492,14.0013026538007,123.991638075795)) ;
#88877 = CARTESIAN_POINT('Ctrl Pts',(-20.6780078275285,14.0113727151456,124.226013909898)) ;
#88878 = CARTESIAN_POINT('Ctrl Pts',(-20.5199890005443,14.0212150794943,124.43079250126)) ;
#88879 = CARTESIAN_POINT('Ctrl Pts',(-20.3271803845075,14.0311757519968,124.607819487763)) ;
#88880 = CARTESIAN_POINT('Ctrl Pts',(-20.1045706887236,14.0412138230646,124.749326629548)) ;
#88881 = CARTESIAN_POINT('Ctrl Pts',(-19.8649107838462,14.051087438025,124.848860391817)) ;
#88882 = CARTESIAN_POINT('Ctrl Pts',(-19.6065853682649,14.0611596726063,124.906317466992)) ;
#88883 = CARTESIAN_POINT('Ctrl Pts',(-19.3486353561911,14.0709836910551,124.91805722916)) ;
#88884 = CARTESIAN_POINT('Ctrl Pts',(-19.0863513066081,14.0810486120311,124.884370279709)) ;
#88885 = CARTESIAN_POINT('Ctrl Pts',(-18.7548552994364,14.0942589103259,124.781024489845)) ;
#88886 = CARTESIAN_POINT('Ctrl Pts',(-18.4555139703643,14.1075743570578,124.592476583949)) ;
#88887 = CARTESIAN_POINT('Ctrl Pts',(-18.2182215362896,14.1208646023251,124.336059674344)) ;
#88888 = CARTESIAN_POINT('Ctrl Pts',(-18.0753754053462,14.1309153519322,124.113963002068)) ;
#88889 = CARTESIAN_POINT('Ctrl Pts',(-17.9751742641188,14.1407279589144,123.876319735043)) ;
#88890 = CARTESIAN_POINT('Ctrl Pts',(-17.9159189092107,14.1507990569087,123.618416063707)) ;
#88891 = CARTESIAN_POINT('Ctrl Pts',(-17.9028526558769,14.1606886296836,123.35883798821)) ;
#88892 = CARTESIAN_POINT('Ctrl Pts',(-17.9449956703198,14.1739587364869,123.012660958945)) ;
#88893 = CARTESIAN_POINT('Ctrl Pts',(-18.110043879932,14.1905754234094,122.603035428979)) ;
#88894 = CARTESIAN_POINT('Ctrl Pts',(-18.4039594470265,14.2071494667256,122.274938448092)) ;
#88895 = CARTESIAN_POINT('Ctrl Pts',(-18.6963137378166,14.2204460341574,122.08351795448)) ;
#88896 = CARTESIAN_POINT('Ctrl Pts',(-18.9385848307681,14.2304760977348,121.979689993019)) ;
#88897 = CARTESIAN_POINT('Ctrl Pts',(-19.1916875088085,14.240369989584,121.920298097705)) ;
#88898 = CARTESIAN_POINT('Ctrl Pts',(-19.5394066171243,14.2536227453696,121.899565963118)) ;
#88899 = CARTESIAN_POINT('Ctrl Pts',(-19.9747350131759,14.270350850362,121.989580778364)) ;
#88900 = CARTESIAN_POINT('Ctrl Pts',(-20.4235622970495,14.2901816868405,122.266085506153)) ;
#88901 = CARTESIAN_POINT('Ctrl Pts',(-20.7535383605483,14.3101070787307,122.680152104981)) ;
#88902 = CARTESIAN_POINT('Ctrl Pts',(-20.9224097639681,14.3300322920827,123.182173590077)) ;
#88903 = CARTESIAN_POINT('Ctrl Pts',(-20.909967365172,14.3499573055678,123.711540173755)) ;
#88904 = CARTESIAN_POINT('Ctrl Pts',(-20.7187416801209,14.3698337772678,124.204034514213)) ;
#88905 = CARTESIAN_POINT('Ctrl Pts',(-20.3693357021894,14.3898130951767,124.603894071184)) ;
#88906 = CARTESIAN_POINT('Ctrl Pts',(-19.9052962266747,14.4097460987527,124.85959923876)) ;
#88907 = CARTESIAN_POINT('Ctrl Pts',(-19.3830046122281,14.4296413687804,124.941993474064)) ;
#88908 = CARTESIAN_POINT('Ctrl Pts',(-18.863111653506,14.4495627066862,124.841603993362)) ;
#88909 = CARTESIAN_POINT('Ctrl Pts',(-18.4079099213766,14.4695203299524,124.569231338478)) ;
#88910 = CARTESIAN_POINT('Ctrl Pts',(-18.0742589102781,14.4894001619096,124.159636622647)) ;
#88911 = CARTESIAN_POINT('Ctrl Pts',(-17.8989537036202,14.5092820132065,123.661028976949)) ;
#88912 = CARTESIAN_POINT('Ctrl Pts',(-17.9053799742444,14.5293530303103,123.127680005003)) ;
#88913 = CARTESIAN_POINT('Ctrl Pts',(-18.090928041147,14.5491602540634,122.634917461125)) ;
#88914 = CARTESIAN_POINT('Ctrl Pts',(-18.4354593545979,14.5691413896322,122.230840604619)) ;
#88915 = CARTESIAN_POINT('Ctrl Pts',(-18.8964698224689,14.5890688829714,121.970192630458)) ;
#88916 = CARTESIAN_POINT('Ctrl Pts',(-19.4158400705055,14.6088895443292,121.881168125595)) ;
#88917 = CARTESIAN_POINT('Ctrl Pts',(-19.9411622969537,14.628986733551,121.976797339529)) ;
#88918 = CARTESIAN_POINT('Ctrl Pts',(-20.3952297063123,14.6487504125593,122.241401014461)) ;
#88919 = CARTESIAN_POINT('Ctrl Pts',(-20.7369043382646,14.6688076912324,122.650295252524)) ;
#88920 = CARTESIAN_POINT('Ctrl Pts',(-20.9160056364455,14.6886031149798,123.145152863214)) ;
#88921 = CARTESIAN_POINT('Ctrl Pts',(-20.9171281004685,14.7085667597074,123.675691935841)) ;
#88922 = CARTESIAN_POINT('Ctrl Pts',(-20.7357205067967,14.7285502509815,124.174887049982)) ;
#88923 = CARTESIAN_POINT('Ctrl Pts',(-20.398657784175,14.7483577461308,124.579349028364)) ;
#88924 = CARTESIAN_POINT('Ctrl Pts',(-19.9402292141674,14.7683403368509,124.847300212365)) ;
#88925 = CARTESIAN_POINT('Ctrl Pts',(-19.4202472432439,14.7882229908422,124.942207693304)) ;
#88926 = CARTESIAN_POINT('Ctrl Pts',(-18.8972710117422,14.8081812357052,124.854072619313)) ;
#88927 = CARTESIAN_POINT('Ctrl Pts',(-18.4373523571738,14.8280568227468,124.59403836842)) ;
#88928 = CARTESIAN_POINT('Ctrl Pts',(-18.0917464518894,14.8480377108821,124.190871761856)) ;
#88929 = CARTESIAN_POINT('Ctrl Pts',(-17.9052470733622,14.8679728519931,123.694860655022)) ;
#88930 = CARTESIAN_POINT('Ctrl Pts',(-17.8988327545552,14.8878848700041,123.165719308424)) ;
#88931 = CARTESIAN_POINT('Ctrl Pts',(-18.0726432682034,14.9077730882477,122.666502021473)) ;
#88932 = CARTESIAN_POINT('Ctrl Pts',(-18.3508412756587,14.9243713920946,122.324182529583)) ;
#88933 = CARTESIAN_POINT('Ctrl Pts',(-18.6332517724376,14.9376439819974,122.119434069299)) ;
#88934 = CARTESIAN_POINT('Ctrl Pts',(-18.8696162522265,14.9476513969483,122.004144120758)) ;
#88935 = CARTESIAN_POINT('Ctrl Pts',(-19.122481344444,14.9576587436809,121.931865885675)) ;
#88936 = CARTESIAN_POINT('Ctrl Pts',(-19.4692168268051,14.9709251034825,121.895493051636)) ;
#88937 = CARTESIAN_POINT('Ctrl Pts',(-19.9027943031777,14.9874397611055,121.963407923393)) ;
#88938 = CARTESIAN_POINT('Ctrl Pts',(-20.289623579524,15.0040371943481,122.175392008362)) ;
#88939 = CARTESIAN_POINT('Ctrl Pts',(-20.5428597744861,15.0173851914931,122.41816948796)) ;
#88940 = CARTESIAN_POINT('Ctrl Pts',(-20.6967684183011,15.0272809458447,122.627784026657)) ;
#88941 = CARTESIAN_POINT('Ctrl Pts',(-20.81329530157,15.0372688997761,122.862950598469)) ;
#88942 = CARTESIAN_POINT('Ctrl Pts',(-20.8871174069244,15.0472261234808,123.114018836122)) ;
#88943 = CARTESIAN_POINT('Ctrl Pts',(-20.9163251075997,15.0572616700375,123.376101669285)) ;
#88944 = CARTESIAN_POINT('Ctrl Pts',(-20.9000253490332,15.0671487813136,123.635429990405)) ;
#88945 = CARTESIAN_POINT('Ctrl Pts',(-20.8387149445651,15.0771401864144,123.890722088326)) ;
#88946 = CARTESIAN_POINT('Ctrl Pts',(-20.7344102203298,15.0870858076292,124.130366678656)) ;
#88947 = CARTESIAN_POINT('Ctrl Pts',(-20.5904612859192,15.0970350558975,124.348645357239)) ;
#88948 = CARTESIAN_POINT('Ctrl Pts',(-20.4088366867784,15.1070815510661,124.540239084563)) ;
#88949 = CARTESIAN_POINT('Ctrl Pts',(-20.2009583169496,15.1169328938577,124.694555578007)) ;
#88950 = CARTESIAN_POINT('Ctrl Pts',(-19.966949092894,15.126904673985,124.812422819299)) ;
#88951 = CARTESIAN_POINT('Ctrl Pts',(-19.7153621269984,15.1368998739627,124.888039277954)) ;
#88952 = CARTESIAN_POINT('Ctrl Pts',(-19.4534809990243,15.1469338656587,124.918615290549)) ;
#88953 = CARTESIAN_POINT('Ctrl Pts',(-19.1948823108826,15.1567892706313,124.903936975073)) ;
#88954 = CARTESIAN_POINT('Ctrl Pts',(-18.9390660225398,15.166788568477,124.844078851224)) ;
#88955 = CARTESIAN_POINT('Ctrl Pts',(-18.6998538262199,15.1766836810822,124.742011656425)) ;
#88956 = CARTESIAN_POINT('Ctrl Pts',(-18.4784349324494,15.1867443266172,124.59760214482)) ;
#88957 = CARTESIAN_POINT('Ctrl Pts',(-18.289374519982,15.1965932036064,124.420815614991)) ;
#88958 = CARTESIAN_POINT('Ctrl Pts',(-18.1305264432099,15.2066219147,124.210528253693)) ;
#88959 = CARTESIAN_POINT('Ctrl Pts',(-18.0112304288892,15.2166513159561,123.975504636893)) ;
#88960 = CARTESIAN_POINT('Ctrl Pts',(-17.9354501387818,15.2264915077521,123.728262940677)) ;
#88961 = CARTESIAN_POINT('Ctrl Pts',(-17.9027451697684,15.2364949369451,123.467452153963)) ;
#88962 = CARTESIAN_POINT('Ctrl Pts',(-17.9158870952322,15.2464804494113,123.205327859872)) ;
#88963 = CARTESIAN_POINT('Ctrl Pts',(-17.9749122216437,15.2565215457953,122.94817162508)) ;
#88964 = CARTESIAN_POINT('Ctrl Pts',(-18.075352673942,15.2663647417463,122.709774454952)) ;
#88965 = CARTESIAN_POINT('Ctrl Pts',(-18.2172239193815,15.2763510528007,122.489051700623)) ;
#88966 = CARTESIAN_POINT('Ctrl Pts',(-18.3942788891156,15.2862857380584,122.297122889139)) ;
#88967 = CARTESIAN_POINT('Ctrl Pts',(-18.6046088256348,15.2963432992754,122.137133343391)) ;
#88968 = CARTESIAN_POINT('Ctrl Pts',(-18.8338906873732,15.306164940884,122.018552182692)) ;
#88969 = CARTESIAN_POINT('Ctrl Pts',(-19.0859639637451,15.316221004475,121.939290081059)) ;
#88970 = CARTESIAN_POINT('Ctrl Pts',(-19.3450573076827,15.3261616802368,121.905856443279)) ;
#88971 = CARTESIAN_POINT('Ctrl Pts',(-19.6050966128801,15.3360660390251,121.917057614141)) ;
#88972 = CARTESIAN_POINT('Ctrl Pts',(-19.8628314894455,15.3461126936009,121.974204391667)) ;
#88973 = CARTESIAN_POINT('Ctrl Pts',(-20.1032054022461,15.3560082882438,122.073524957395)) ;
#88974 = CARTESIAN_POINT('Ctrl Pts',(-20.3263274818967,15.3660702349007,122.215360141734)) ;
#88975 = CARTESIAN_POINT('Ctrl Pts',(-20.5173806023937,15.3759198588328,122.390011089637)) ;
#88976 = CARTESIAN_POINT('Ctrl Pts',(-20.6776940933443,15.3858830978627,122.596996909064)) ;
#88977 = CARTESIAN_POINT('Ctrl Pts',(-20.8000760560513,15.3959076726385,122.830296872806)) ;
#88978 = CARTESIAN_POINT('Ctrl Pts',(-20.8793976462342,15.4058262353262,123.078576451367)) ;
#88979 = CARTESIAN_POINT('Ctrl Pts',(-20.9151255754094,15.4158184220502,123.338734291713)) ;
#88980 = CARTESIAN_POINT('Ctrl Pts',(-20.9046224904582,15.4258532206344,123.602218432797)) ;
#88981 = CARTESIAN_POINT('Ctrl Pts',(-20.8499613006373,15.4357084113081,123.855389436239)) ;
#88982 = CARTESIAN_POINT('Ctrl Pts',(-20.7510911952532,15.4457077594611,124.098804793932)) ;
#88983 = CARTESIAN_POINT('Ctrl Pts',(-20.6131053102038,15.4556028851362,124.319258702986)) ;
#88984 = CARTESIAN_POINT('Ctrl Pts',(-20.4360576038621,15.4656634280843,124.51555709839)) ;
#88985 = CARTESIAN_POINT('Ctrl Pts',(-20.2320397835465,15.4755127023512,124.674867184459)) ;
#88986 = CARTESIAN_POINT('Ctrl Pts',(-19.9996679689736,15.4855399269211,124.799102630686)) ;
#88987 = CARTESIAN_POINT('Ctrl Pts',(-19.7489910633449,15.4955683261089,124.880464971312)) ;
#88988 = CARTESIAN_POINT('Ctrl Pts',(-19.4928458279102,15.5054140765224,124.916870140584)) ;
#88989 = CARTESIAN_POINT('Ctrl Pts',(-19.2304605256444,15.5154028669231,124.908855957832)) ;
#88990 = CARTESIAN_POINT('Ctrl Pts',(-18.9721684140402,15.5254477953228,124.854455310312)) ;
#88991 = CARTESIAN_POINT('Ctrl Pts',(-18.7323714755152,15.5352722801118,124.7587411508)) ;
#88992 = CARTESIAN_POINT('Ctrl Pts',(-18.5074627778425,15.545329677653,124.619968276734)) ;
#88993 = CARTESIAN_POINT('Ctrl Pts',(-18.3128405903418,15.5552557692392,124.446263039187)) ;
#88994 = CARTESIAN_POINT('Ctrl Pts',(-18.150350868832,15.5652105543838,124.241248427742)) ;
#88995 = CARTESIAN_POINT('Ctrl Pts',(-18.0251521487945,15.5752479240414,124.009084692641)) ;
#88996 = CARTESIAN_POINT('Ctrl Pts',(-17.9432016162711,15.585136734163,123.762469410516)) ;
#88997 = CARTESIAN_POINT('Ctrl Pts',(-17.9044670409744,15.5951260932141,123.502838762861)) ;
#88998 = CARTESIAN_POINT('Ctrl Pts',(-17.9115749765126,15.6050846406702,123.24124293323)) ;
#88999 = CARTESIAN_POINT('Ctrl Pts',(-17.9630623576573,15.6149842172212,122.986221570105)) ;
#89000 = CARTESIAN_POINT('Ctrl Pts',(-18.0595417871603,15.6250321290519,122.740459685975)) ;
#89001 = CARTESIAN_POINT('Ctrl Pts',(-18.1949986414737,15.6349274769125,122.518438659765)) ;
#89002 = CARTESIAN_POINT('Ctrl Pts',(-18.3697629356532,15.6449891534437,122.320059129432)) ;
#89003 = CARTESIAN_POINT('Ctrl Pts',(-18.5718644577124,15.6548336711928,122.158541982419)) ;
#89004 = CARTESIAN_POINT('Ctrl Pts',(-18.8011526189207,15.6647941149076,122.032301199326)) ;
#89005 = CARTESIAN_POINT('Ctrl Pts',(-19.0509357609831,15.6748309477258,121.947606476504)) ;
#89006 = CARTESIAN_POINT('Ctrl Pts',(-19.3074921480599,15.6847097444726,121.907773626489)) ;
#89007 = CARTESIAN_POINT('Ctrl Pts',(-19.5717593834283,15.694769060601,121.913104494787)) ;
#89008 = CARTESIAN_POINT('Ctrl Pts',(-19.8262605890557,15.7046395073542,121.963283380412)) ;
#89009 = CARTESIAN_POINT('Ctrl Pts',(-20.0714198955884,15.7146321456122,122.057380334014)) ;
#89010 = CARTESIAN_POINT('Ctrl Pts',(-20.2971021415107,15.7246641611601,122.193630102715)) ;
#89011 = CARTESIAN_POINT('Ctrl Pts',(-20.4928065396954,15.7345300174667,122.363722707075)) ;
#89012 = CARTESIAN_POINT('Ctrl Pts',(-20.659353254304,15.7445993069358,122.569307538849)) ;
#89013 = CARTESIAN_POINT('Ctrl Pts',(-20.7848456281026,15.7544428644871,122.795525024093)) ;
#89014 = CARTESIAN_POINT('Ctrl Pts',(-20.8711257023825,15.764422991275,123.043184928911)) ;
#89015 = CARTESIAN_POINT('Ctrl Pts',(-20.9127559215498,15.7744415398749,123.303142599032)) ;
#89016 = CARTESIAN_POINT('Ctrl Pts',(-20.9092242705699,15.7843248403981,123.562873547571)) ;
#89017 = CARTESIAN_POINT('Ctrl Pts',(-20.8596396741269,15.7943931274462,123.822725252708)) ;
#89018 = CARTESIAN_POINT('Ctrl Pts',(-20.7681651750302,15.8042232504649,124.064360555124)) ;
#89019 = CARTESIAN_POINT('Ctrl Pts',(-20.6332871001612,15.8142898343902,124.291882100143)) ;
#89020 = CARTESIAN_POINT('Ctrl Pts',(-20.4638049151612,15.8241799474047,124.48896825144)) ;
#89021 = CARTESIAN_POINT('Ctrl Pts',(-20.2609877478758,15.8341726361673,124.655734358688)) ;
#89022 = CARTESIAN_POINT('Ctrl Pts',(-20.0329028474693,15.8441335245231,124.784198130911)) ;
#89023 = CARTESIAN_POINT('Ctrl Pts',(-19.7872175767508,15.8540514694031,124.871145968037)) ;
#89024 = CARTESIAN_POINT('Ctrl Pts',(-19.5278485703835,15.8640592224993,124.914811107078)) ;
#89025 = CARTESIAN_POINT('Ctrl Pts',(-19.2642689030462,15.8740903164583,124.91223920911)) ;
#89026 = CARTESIAN_POINT('Ctrl Pts',(-19.0097316360131,15.8839382844863,124.865387875955)) ;
#89027 = CARTESIAN_POINT('Ctrl Pts',(-18.761882854262,15.8940002406122,124.773318370912)) ;
#89028 = CARTESIAN_POINT('Ctrl Pts',(-18.5376157807696,15.9038974522133,124.641576258663)) ;
#89029 = CARTESIAN_POINT('Ctrl Pts',(-18.3384056514573,15.9138286188779,124.472982338498)) ;
#89030 = CARTESIAN_POINT('Ctrl Pts',(-18.1698491513015,15.9238708030821,124.269933564785)) ;
#89031 = CARTESIAN_POINT('Ctrl Pts',(-18.0409623377378,15.9337574713353,124.044330723478)) ;
#89032 = CARTESIAN_POINT('Ctrl Pts',(-17.9518555076836,15.9437505833135,123.79731633989)) ;
#89033 = CARTESIAN_POINT('Ctrl Pts',(-17.9072992563308,15.9536962609293,123.539779663906)) ;
#89034 = CARTESIAN_POINT('Ctrl Pts',(-17.9076038590327,15.9636435639143,123.278362513842)) ;
#89035 = CARTESIAN_POINT('Ctrl Pts',(-17.954039484633,15.9736912876611,123.018441119269)) ;
#89036 = CARTESIAN_POINT('Ctrl Pts',(-18.0429092629221,15.9835396614236,122.77537631077)) ;
#89037 = CARTESIAN_POINT('Ctrl Pts',(-18.1733362386872,15.9934986338693,122.548480377477)) ;
#89038 = CARTESIAN_POINT('Ctrl Pts',(-18.3428858266523,16.0035374957505,122.346380568049)) ;
#89039 = CARTESIAN_POINT('Ctrl Pts',(-18.5414869910732,16.0134160999223,122.179156901752)) ;
#89040 = CARTESIAN_POINT('Ctrl Pts',(-18.7699271953843,16.0234676411256,122.046612208989)) ;
#89041 = CARTESIAN_POINT('Ctrl Pts',(-19.0141072069317,16.0333630391059,121.957051725276)) ;
#89042 = CARTESIAN_POINT('Ctrl Pts',(-19.2740547380586,16.0434142716512,121.910401805192)) ;
#89043 = CARTESIAN_POINT('Ctrl Pts',(-19.5338803406111,16.0533004622755,121.909579455401)) ;
#89044 = CARTESIAN_POINT('Ctrl Pts',(-19.7926868268136,16.0632930015913,121.953875934243)) ;
#89045 = CARTESIAN_POINT('Ctrl Pts',(-20.0387894173471,16.073241447486,122.04213980991)) ;
#89046 = CARTESIAN_POINT('Ctrl Pts',(-20.265712566684,16.0831782500179,122.171300244256)) ;
#89047 = CARTESIAN_POINT('Ctrl Pts',(-20.4679516213838,16.0931612574692,122.338455368566)) ;
#89048 = CARTESIAN_POINT('Ctrl Pts',(-20.6387206153012,16.103205098884,122.539669360996)) ;
#89049 = CARTESIAN_POINT('Ctrl Pts',(-20.7696595815421,16.1130332975079,122.762338547933)) ;
#89050 = CARTESIAN_POINT('Ctrl Pts',(-20.8623125592493,16.1231098909501,123.010343765831)) ;
#89051 = CARTESIAN_POINT('Ctrl Pts',(-20.9095729442255,16.1329618902917,123.264952690282)) ;
#89052 = CARTESIAN_POINT('Ctrl Pts',(-20.9121762627497,16.1430354771156,123.529617389355)) ;
#89053 = CARTESIAN_POINT('Ctrl Pts',(-20.869730533684,16.152875702213,123.784725112839)) ;
#89054 = CARTESIAN_POINT('Ctrl Pts',(-20.7834213237411,16.1628414062417,124.031959888329)) ;
#89055 = CARTESIAN_POINT('Ctrl Pts',(-20.6543616553613,16.1728680395483,124.261695407877)) ;
#89056 = CARTESIAN_POINT('Ctrl Pts',(-20.4893937694131,16.1827823352601,124.463343826805)) ;
#89057 = CARTESIAN_POINT('Ctrl Pts',(-20.2907385375805,16.1927706239526,124.634927879414)) ;
#89058 = CARTESIAN_POINT('Ctrl Pts',(-20.063944204818,16.2028093571109,124.769667401044)) ;
#89059 = CARTESIAN_POINT('Ctrl Pts',(-19.8221495313365,16.2126526889385,124.861577146822)) ;
#89060 = CARTESIAN_POINT('Ctrl Pts',(-19.5634230879079,16.2226804148181,124.911613949581)) ;
#89061 = CARTESIAN_POINT('Ctrl Pts',(-19.2997995110888,16.2327127512066,124.915252649983)) ;
#89062 = CARTESIAN_POINT('Ctrl Pts',(-19.0447508850932,16.2425422515072,124.87443461805)) ;
#89063 = CARTESIAN_POINT('Ctrl Pts',(-18.7964127409365,16.252531755424,124.789315485236)) ;
#89064 = CARTESIAN_POINT('Ctrl Pts',(-18.5657100501157,16.2625755959364,124.661096709419)) ;
#89065 = CARTESIAN_POINT('Ctrl Pts',(-18.3649684583117,16.2723973017045,124.498860195946)) ;
#89066 = CARTESIAN_POINT('Ctrl Pts',(-18.1912776614032,16.2824323488368,124.30043121603)) ;
#89067 = CARTESIAN_POINT('Ctrl Pts',(-18.0554378922695,16.2924570262737,124.074705597496)) ;
#89068 = CARTESIAN_POINT('Ctrl Pts',(-17.9619696621494,16.3023098411282,123.833243322249)) ;
#89069 = CARTESIAN_POINT('Ctrl Pts',(-17.9107123152974,16.3122975507357,123.575850309162)) ;
#89070 = CARTESIAN_POINT('Ctrl Pts',(-17.9049458569947,16.3222275607298,123.314954275145)) ;
#89071 = CARTESIAN_POINT('Ctrl Pts',(-17.9444047205986,16.332217315949,123.055411337041)) ;
#89072 = CARTESIAN_POINT('Ctrl Pts',(-18.0289611024086,16.3422439246319,122.805854001657)) ;
#89073 = CARTESIAN_POINT('Ctrl Pts',(-18.1535398915879,16.3521278646537,122.577945287591)) ;
#89074 = CARTESIAN_POINT('Ctrl Pts',(-18.3170581793031,16.3621170921922,122.372577155451)) ;
#89075 = CARTESIAN_POINT('Ctrl Pts',(-18.5151613636324,16.3721599627159,122.198204531201)) ;
#89076 = CARTESIAN_POINT('Ctrl Pts',(-18.7355937159182,16.3819923494713,122.06340510794)) ;
#89077 = CARTESIAN_POINT('Ctrl Pts',(-18.9797379454661,16.3919856426429,121.966674506609)) ;
#89078 = CARTESIAN_POINT('Ctrl Pts',(-19.2380933202206,16.4020176482913,121.914136786792)) ;
#89079 = CARTESIAN_POINT('Ctrl Pts',(-19.4972319162803,16.4118829042603,121.907050750478)) ;
#89080 = CARTESIAN_POINT('Ctrl Pts',(-19.7563049005742,16.4218447841678,121.944708800064)) ;
#89081 = CARTESIAN_POINT('Ctrl Pts',(-20.0065704728934,16.4318797175297,122.027782317763)) ;
#89082 = CARTESIAN_POINT('Ctrl Pts',(-20.235395236987,16.441764675909,122.150815185132)) ;
#89083 = CARTESIAN_POINT('Ctrl Pts',(-20.4430095418267,16.4518303028317,122.314647056948)) ;
#89084 = CARTESIAN_POINT('Ctrl Pts',(-20.6153156253427,16.461669408496,122.507485556433)) ;
#89085 = CARTESIAN_POINT('Ctrl Pts',(-20.7548759132793,16.4717322235013,122.732057555602)) ;
#89086 = CARTESIAN_POINT('Ctrl Pts',(-20.8514951454901,16.48162842955,122.973534637153)) ;
#89087 = CARTESIAN_POINT('Ctrl Pts',(-20.9056579365925,16.4915692525753,123.229061857975)) ;
#89088 = CARTESIAN_POINT('Ctrl Pts',(-20.9147539350784,16.501573835554,123.491844043348)) ;
#89089 = CARTESIAN_POINT('Ctrl Pts',(-20.8777116944424,16.5115947299987,123.752558207369)) ;
#89090 = CARTESIAN_POINT('Ctrl Pts',(-20.7973193962089,16.5214866505881,123.9997713371)) ;
#89091 = CARTESIAN_POINT('Ctrl Pts',(-20.6743097948123,16.5314800829335,124.231787262463)) ;
#89092 = CARTESIAN_POINT('Ctrl Pts',(-20.5135843010475,16.5414256878334,124.437884102592)) ;
#89093 = CARTESIAN_POINT('Ctrl Pts',(-20.3198274952116,16.5513729613149,124.613376926942)) ;
#89094 = CARTESIAN_POINT('Ctrl Pts',(-20.0961655477988,16.5614208757913,124.753706244345)) ;
#89095 = CARTESIAN_POINT('Ctrl Pts',(-19.8564832755268,16.5712685161386,124.851295914385)) ;
#89096 = CARTESIAN_POINT('Ctrl Pts',(-19.6007546274818,16.5812302315152,124.907216087891)) ;
#89097 = CARTESIAN_POINT('Ctrl Pts',(-19.3374019357033,16.591258855088,124.917623305779)) ;
#89098 = CARTESIAN_POINT('Ctrl Pts',(-19.0793392609636,16.6011692171544,124.882650735253)) ;
#89099 = CARTESIAN_POINT('Ctrl Pts',(-18.8304294039593,16.6111039108068,124.803856446845)) ;
#89100 = CARTESIAN_POINT('Ctrl Pts',(-18.596627686363,16.6211457539347,124.681515843378)) ;
#89101 = CARTESIAN_POINT('Ctrl Pts',(-18.3907224983714,16.6310302595051,124.523120625139)) ;
#89102 = CARTESIAN_POINT('Ctrl Pts',(-18.213179611499,16.6410323632903,124.329353348425)) ;
#89103 = CARTESIAN_POINT('Ctrl Pts',(-18.0729347335421,16.6509507147053,124.109605240172)) ;
#89104 = CARTESIAN_POINT('Ctrl Pts',(-17.9717684511152,16.6609983707262,123.865757550208)) ;
#89105 = CARTESIAN_POINT('Ctrl Pts',(-17.9151801485084,16.6708695637544,123.612544609832)) ;
#89106 = CARTESIAN_POINT('Ctrl Pts',(-17.9031486210089,16.6809352768979,123.348363900477)) ;
#89107 = CARTESIAN_POINT('Ctrl Pts',(-17.9361680628292,16.6907877374706,123.091490849331)) ;
#89108 = CARTESIAN_POINT('Ctrl Pts',(-18.041350571431,16.7042162001931,122.754758769299)) ;
#89109 = CARTESIAN_POINT('Ctrl Pts',(-18.2267930848674,16.7172971477102,122.460500377085)) ;
#89110 = CARTESIAN_POINT('Ctrl Pts',(-18.4863600281543,16.7307716459448,122.219764136354)) ;
#89111 = CARTESIAN_POINT('Ctrl Pts',(-18.7036600720593,16.7406037495542,122.079903461464)) ;
#89112 = CARTESIAN_POINT('Ctrl Pts',(-18.9447043729808,16.7505696526809,121.977589420528)) ;
#89113 = CARTESIAN_POINT('Ctrl Pts',(-19.2015822289623,16.7605970619911,121.918702174221)) ;
#89114 = CARTESIAN_POINT('Ctrl Pts',(-19.4616612966653,16.7705080933577,121.90540119112)) ;
#89115 = CARTESIAN_POINT('Ctrl Pts',(-19.8072674417979,16.7837524009787,121.947145247852)) ;
#89116 = CARTESIAN_POINT('Ctrl Pts',(-20.2188607320283,16.8004528836499,122.113061781685)) ;
#89117 = CARTESIAN_POINT('Ctrl Pts',(-20.5455735820307,16.8169597128057,122.405977428994)) ;
#89118 = CARTESIAN_POINT('Ctrl Pts',(-20.7373318770542,16.8302703410433,122.698474315006)) ;
#89119 = CARTESIAN_POINT('Ctrl Pts',(-20.8410538416381,16.8402629045834,122.939759731386)) ;
#89120 = CARTESIAN_POINT('Ctrl Pts',(-20.9012068159582,16.8502929875849,123.196350988495)) ;
#89121 = CARTESIAN_POINT('Ctrl Pts',(-20.9212193192341,16.8634665915827,123.542025913649)) ;
#89122 = CARTESIAN_POINT('Ctrl Pts',(-20.832303368653,16.8801042968141,123.975028581527)) ;
#89123 = CARTESIAN_POINT('Ctrl Pts',(-20.5559527242748,16.8999860593815,124.425665773585)) ;
#89124 = CARTESIAN_POINT('Ctrl Pts',(-20.2087278908941,16.916682411598,124.701769095248)) ;
#89125 = CARTESIAN_POINT('Ctrl Pts',(-19.8917137009118,16.9298394393871,124.83996615317)) ;
#89126 = CARTESIAN_POINT('Ctrl Pts',(-19.5501593226237,16.9432167940307,124.923024211938)) ;
#89127 = CARTESIAN_POINT('Ctrl Pts',(-19.1108610444918,16.9597476282895,124.912764903616)) ;
#89128 = CARTESIAN_POINT('Ctrl Pts',(-18.6161741406845,16.9797123180326,124.720936570403)) ;
#89129 = CARTESIAN_POINT('Ctrl Pts',(-18.2178875673859,16.9996288114562,124.372240740112)) ;
#89130 = CARTESIAN_POINT('Ctrl Pts',(-17.9619000053034,17.0195185308058,123.909658769635)) ;
#89131 = CARTESIAN_POINT('Ctrl Pts',(-17.8790923718899,17.0395252604536,123.384478022634)) ;
#89132 = CARTESIAN_POINT('Ctrl Pts',(-17.9792607793457,17.0593633141005,122.866706624068)) ;
#89133 = CARTESIAN_POINT('Ctrl Pts',(-18.251654980879,17.0793566523141,122.410555995914)) ;
#89134 = CARTESIAN_POINT('Ctrl Pts',(-18.6614413308425,17.0992394517207,122.076728435462)) ;
#89135 = CARTESIAN_POINT('Ctrl Pts',(-19.1602498824996,17.1191316326394,121.901928665033)) ;
#89136 = CARTESIAN_POINT('Ctrl Pts',(-19.6893506726758,17.1390338111345,121.906954280708)) ;
#89137 = CARTESIAN_POINT('Ctrl Pts',(-20.1877372859541,17.1590711223382,122.094250728715)) ;
#89138 = CARTESIAN_POINT('Ctrl Pts',(-20.5885147516778,17.1788835638791,122.436171529998)) ;
#89139 = CARTESIAN_POINT('Ctrl Pts',(-20.8514859106502,17.198948804614,122.899836288904)) ;
#89140 = CARTESIAN_POINT('Ctrl Pts',(-20.9395751047835,17.2187060094698,123.417764524091)) ;
#89141 = CARTESIAN_POINT('Ctrl Pts',(-20.8451902721094,17.2387392821155,123.941511312625)) ;
#89142 = CARTESIAN_POINT('Ctrl Pts',(-20.5803738327966,17.2585521905694,124.396949460866)) ;
#89143 = CARTESIAN_POINT('Ctrl Pts',(-20.1731152784338,17.2785483366968,124.738041234505)) ;
#89144 = CARTESIAN_POINT('Ctrl Pts',(-19.6769118272769,17.2984100899193,124.918872799759)) ;
#89145 = CARTESIAN_POINT('Ctrl Pts',(-19.1436416860639,17.3184786070474,124.919193987262)) ;
#89146 = CARTESIAN_POINT('Ctrl Pts',(-18.648109623505,17.3383094800442,124.739265310968)) ;
#89147 = CARTESIAN_POINT('Ctrl Pts',(-18.2411319113203,17.3582313908609,124.40073894506)) ;
#89148 = CARTESIAN_POINT('Ctrl Pts',(-17.9740323769222,17.3781608342962,123.94322080473)) ;
#89149 = CARTESIAN_POINT('Ctrl Pts',(-17.8790250602224,17.3980705044126,123.422734778079)) ;
#89150 = CARTESIAN_POINT('Ctrl Pts',(-17.9662662127267,17.4179438616755,122.901724773555)) ;
#89151 = CARTESIAN_POINT('Ctrl Pts',(-18.2276294818176,17.4379353962934,122.439190238654)) ;
#89152 = CARTESIAN_POINT('Ctrl Pts',(-18.6285734387837,17.4578010137041,122.095521594485)) ;
#89153 = CARTESIAN_POINT('Ctrl Pts',(-19.1253152085356,17.4777819435324,121.907762643509)) ;
#89154 = CARTESIAN_POINT('Ctrl Pts',(-19.6552200286643,17.4977204056155,121.901390129916)) ;
#89155 = CARTESIAN_POINT('Ctrl Pts',(-20.1546489410619,17.5176125988372,122.075060293898)) ;
#89156 = CARTESIAN_POINT('Ctrl Pts',(-20.5661552710587,17.5375833138726,122.410136115304)) ;
#89157 = CARTESIAN_POINT('Ctrl Pts',(-20.837318013256,17.5573929855387,122.861593772204)) ;
#89158 = CARTESIAN_POINT('Ctrl Pts',(-20.9394053743083,17.5773862022299,123.382882566089)) ;
#89159 = CARTESIAN_POINT('Ctrl Pts',(-20.8584272459729,17.5972371144262,123.904456907226)) ;
#89160 = CARTESIAN_POINT('Ctrl Pts',(-20.6013722647494,17.6173117207453,124.371835879059)) ;
#89161 = CARTESIAN_POINT('Ctrl Pts',(-20.2709413387604,17.6338283526286,124.661087804809)) ;
#89162 = CARTESIAN_POINT('Ctrl Pts',(-19.9567456572262,17.6471670603227,124.816311506479)) ;
#89163 = CARTESIAN_POINT('Ctrl Pts',(-19.7085634180374,17.657009434631,124.889285728244)) ;
#89164 = CARTESIAN_POINT('Ctrl Pts',(-19.4460346302332,17.6670644546137,124.918920394545)) ;
#89165 = CARTESIAN_POINT('Ctrl Pts',(-19.0989340056819,17.6802966112713,124.897325675655)) ;
#89166 = CARTESIAN_POINT('Ctrl Pts',(-18.6800921880835,17.6969115786164,124.757498322391)) ;
#89167 = CARTESIAN_POINT('Ctrl Pts',(-18.3346383771164,17.7135061656276,124.483309875907)) ;
#89168 = CARTESIAN_POINT('Ctrl Pts',(-18.1268953740658,17.726739733983,124.204383339548)) ;
#89169 = CARTESIAN_POINT('Ctrl Pts',(-18.0083495823601,17.7367833517917,123.968592623646)) ;
#89170 = CARTESIAN_POINT('Ctrl Pts',(-17.9336310060421,17.7466702760265,123.71972753629)) ;
#89171 = CARTESIAN_POINT('Ctrl Pts',(-17.9024800444537,17.7566609304733,123.459055825321)) ;
#89172 = CARTESIAN_POINT('Ctrl Pts',(-17.91707504202,17.7666226889273,123.197677226246)) ;
#89173 = CARTESIAN_POINT('Ctrl Pts',(-17.9967448142101,17.7799625539945,122.856223951778)) ;
#89174 = CARTESIAN_POINT('Ctrl Pts',(-18.1639793074523,17.7932713369078,122.544584740488)) ;
#89175 = CARTESIAN_POINT('Ctrl Pts',(-18.4009261605596,17.8064670943519,122.291390427509)) ;
#89176 = CARTESIAN_POINT('Ctrl Pts',(-18.6098409160699,17.8164289780284,122.133625520298)) ;
#89177 = CARTESIAN_POINT('Ctrl Pts',(-18.8450658298774,17.826472087543,122.013949993326)) ;
#89178 = CARTESIAN_POINT('Ctrl Pts',(-19.092621766734,17.8363243375422,121.938100172443)) ;
#89179 = CARTESIAN_POINT('Ctrl Pts',(-19.3525817752957,17.8462958744927,121.905367673207)) ;
#89180 = CARTESIAN_POINT('Ctrl Pts',(-19.6149678521797,17.8562911399702,121.918326097359)) ;
#89181 = CARTESIAN_POINT('Ctrl Pts',(-19.8719764054818,17.8663251128439,121.977174194731)) ;
#89182 = CARTESIAN_POINT('Ctrl Pts',(-20.1107443124788,17.8761805276062,122.07756701248)) ;
#89183 = CARTESIAN_POINT('Ctrl Pts',(-20.3317665609879,17.886179805115,122.219601552815)) ;
#89184 = CARTESIAN_POINT('Ctrl Pts',(-20.5230159036683,17.896074989278,122.39585448978)) ;
#89185 = CARTESIAN_POINT('Ctrl Pts',(-20.6833174072794,17.9061353689188,122.60604307054)) ;
#89186 = CARTESIAN_POINT('Ctrl Pts',(-20.8023179831757,17.9159852379269,122.835939812967)) ;
#89187 = CARTESIAN_POINT('Ctrl Pts',(-20.8815806037002,17.9260167991348,123.08734301173)) ;
#89188 = CARTESIAN_POINT('Ctrl Pts',(-20.9153942834191,17.9360272480171,123.348249186297)) ;
#89189 = CARTESIAN_POINT('Ctrl Pts',(-20.9038056440646,17.9459339874341,123.608321329956)) ;
#89190 = CARTESIAN_POINT('Ctrl Pts',(-20.8475549821368,17.9558720035025,123.863336913945)) ;
#89191 = CARTESIAN_POINT('Ctrl Pts',(-20.7473491124227,17.9658772499537,124.106450718163)) ;
#89192 = CARTESIAN_POINT('Ctrl Pts',(-20.6056897092289,17.97591131101,124.328835897672)) ;
#89193 = CARTESIAN_POINT('Ctrl Pts',(-20.4312337067048,17.9857563920681,124.519908095883)) ;
#89194 = CARTESIAN_POINT('Ctrl Pts',(-20.2236664013566,17.9957421980216,124.680396433313)) ;
#89195 = CARTESIAN_POINT('Ctrl Pts',(-19.992579689612,18.0056770185758,124.801991034309)) ;
#89196 = CARTESIAN_POINT('Ctrl Pts',(-19.7408295621782,18.015734543708,124.882346278087)) ;
#89197 = CARTESIAN_POINT('Ctrl Pts',(-19.4850812770158,18.0255561943594,124.917339204616)) ;
#89198 = CARTESIAN_POINT('Ctrl Pts',(-19.2210175734843,18.0356122578641,124.907651917327)) ;
#89199 = CARTESIAN_POINT('Ctrl Pts',(-18.9656796380445,18.045552924928,124.85243013731)) ;
#89200 = CARTESIAN_POINT('Ctrl Pts',(-18.7243886052584,18.055457318594,124.754831562349)) ;
#89201 = CARTESIAN_POINT('Ctrl Pts',(-18.5006574893832,18.065503842357,124.61470975614)) ;
#89202 = CARTESIAN_POINT('Ctrl Pts',(-18.307369291185,18.0753999253734,124.440656203214)) ;
#89203 = CARTESIAN_POINT('Ctrl Pts',(-18.1445872821212,18.0854666246034,124.232186912263)) ;
#89204 = CARTESIAN_POINT('Ctrl Pts',(-18.0231672453592,18.0952902350045,124.004324151478)) ;
#89205 = CARTESIAN_POINT('Ctrl Pts',(-17.9408459619243,18.105346095182,123.753251808151)) ;
#89206 = CARTESIAN_POINT('Ctrl Pts',(-17.9041508391774,18.1152792414869,123.494778928388)) ;
#89207 = CARTESIAN_POINT('Ctrl Pts',(-17.9123669611964,18.1252244972575,123.233587463902)) ;
#89208 = CARTESIAN_POINT('Ctrl Pts',(-17.965820602866,18.135207795696,122.976706518041)) ;
#89209 = CARTESIAN_POINT('Ctrl Pts',(-18.063904304486,18.1452449758426,122.731876350353)) ;
#89210 = CARTESIAN_POINT('Ctrl Pts',(-18.2001593676184,18.1550995285521,122.511623169625)) ;
#89211 = CARTESIAN_POINT('Ctrl Pts',(-18.3748041349657,18.1650990469994,122.315340175389)) ;
#89212 = CARTESIAN_POINT('Ctrl Pts',(-18.5786232758408,18.1749941294615,122.153792991792)) ;
#89213 = CARTESIAN_POINT('Ctrl Pts',(-18.8111647901301,18.1850546749676,122.028081402506)) ;
#89214 = CARTESIAN_POINT('Ctrl Pts',(-19.0567404030301,18.1949039822156,121.94625334283)) ;
#89215 = CARTESIAN_POINT('Ctrl Pts',(-19.3172903973273,18.204931072303,121.906964506293)) ;
#89216 = CARTESIAN_POINT('Ctrl Pts',(-19.5807510422382,18.2149599764399,121.914213939927)) ;
#89217 = CARTESIAN_POINT('Ctrl Pts',(-19.8342692925352,18.2248038415392,121.965616328592)) ;
#89218 = CARTESIAN_POINT('Ctrl Pts',(-20.0789732695833,18.2347996682476,122.061118208397)) ;
#89219 = CARTESIAN_POINT('Ctrl Pts',(-20.3037898720174,18.2448248848966,122.198476327115)) ;
#89220 = CARTESIAN_POINT('Ctrl Pts',(-20.4989049499709,18.2547147170542,122.37016702887)) ;
#89221 = CARTESIAN_POINT('Ctrl Pts',(-20.6631753421901,18.2647055731389,122.574966335763)) ;
#89222 = CARTESIAN_POINT('Ctrl Pts',(-20.788773377905,18.2746506677318,122.804154170433)) ;
#89223 = CARTESIAN_POINT('Ctrl Pts',(-20.8731939482788,18.2846025714999,123.051690442556)) ;
#89224 = CARTESIAN_POINT('Ctrl Pts',(-20.9134619567521,18.2946389709693,123.312337432225)) ;
#89225 = CARTESIAN_POINT('Ctrl Pts',(-20.9081339354844,18.304528041058,123.572166354225)) ;
#89226 = CARTESIAN_POINT('Ctrl Pts',(-20.8577276976876,18.3145173304289,123.829783197126)) ;
#89227 = CARTESIAN_POINT('Ctrl Pts',(-20.7634652567705,18.3244758966386,124.073909818492)) ;
#89228 = CARTESIAN_POINT('Ctrl Pts',(-20.6295842577516,18.3343754678554,124.296985254271)) ;
#89229 = CARTESIAN_POINT('Ctrl Pts',(-20.4564060477001,18.3444233822697,124.496275231277)) ;
#89230 = CARTESIAN_POINT('Ctrl Pts',(-20.2544457726215,18.3543187251302,124.660147079943)) ;
#89231 = CARTESIAN_POINT('Ctrl Pts',(-20.0233589167788,18.3643804190777,124.788582887775)) ;
#89232 = CARTESIAN_POINT('Ctrl Pts',(-19.7788516309637,18.3742248721618,124.873135508736)) ;
#89233 = CARTESIAN_POINT('Ctrl Pts',(-19.5205311753707,18.3841855571203,124.915333903471)) ;
#89234 = CARTESIAN_POINT('Ctrl Pts',(-19.2568158507944,18.3942214896288,124.91156959599)) ;
#89235 = CARTESIAN_POINT('Ctrl Pts',(-19.0015267672572,18.4041101053169,124.863056912793)) ;
#89236 = CARTESIAN_POINT('Ctrl Pts',(-18.7552413200576,18.4141245144593,124.770264913515)) ;
#89237 = CARTESIAN_POINT('Ctrl Pts',(-18.5287491933341,18.4241583234171,124.635287434208)) ;
#89238 = CARTESIAN_POINT('Ctrl Pts',(-18.3326736838035,18.4339887776733,124.467040337069)) ;
#89239 = CARTESIAN_POINT('Ctrl Pts',(-18.1646552309895,18.4440664452515,124.262399712302)) ;
#89240 = CARTESIAN_POINT('Ctrl Pts',(-18.0374628156085,18.4539183133737,124.036835965427)) ;
#89241 = CARTESIAN_POINT('Ctrl Pts',(-17.9492624861745,18.4639913509391,123.787301761498)) ;
#89242 = CARTESIAN_POINT('Ctrl Pts',(-17.9067521481246,18.47383390429,123.532143869047)) ;
#89243 = CARTESIAN_POINT('Ctrl Pts',(-17.9083434021815,18.4838142997834,123.269885593791)) ;
#89244 = CARTESIAN_POINT('Ctrl Pts',(-17.9561323187471,18.4938327777612,123.010990190508)) ;
#89245 = CARTESIAN_POINT('Ctrl Pts',(-18.0463999219275,18.5037160920673,122.767424084949)) ;
#89246 = CARTESIAN_POINT('Ctrl Pts',(-18.1801054394556,18.513784394606,122.53915993018)) ;
#89247 = CARTESIAN_POINT('Ctrl Pts',(-18.3471840847822,18.5236144418794,122.342083268111)) ;
#89248 = CARTESIAN_POINT('Ctrl Pts',(-18.5504477114517,18.5336813132949,122.172834206145)) ;
#89249 = CARTESIAN_POINT('Ctrl Pts',(-18.7760961055222,18.543570352094,122.043850044035)) ;
#89250 = CARTESIAN_POINT('Ctrl Pts',(-19.0231397001699,18.5535670502281,121.954587201367)) ;
#89251 = CARTESIAN_POINT('Ctrl Pts',(-19.2808470530102,18.5635194759401,121.909875533707)) ;
#89252 = CARTESIAN_POINT('Ctrl Pts',(-19.5420744376569,18.573460778173,121.910226123319)) ;
#89253 = CARTESIAN_POINT('Ctrl Pts',(-19.8004561957054,18.5834440172569,121.955853427861)) ;
#89254 = CARTESIAN_POINT('Ctrl Pts',(-20.048172080969,18.5934828188255,122.046518326737)) ;
#89255 = CARTESIAN_POINT('Ctrl Pts',(-20.2723410125305,18.6033309249472,122.17589057555)) ;
#89256 = CARTESIAN_POINT('Ctrl Pts',(-20.4750350377161,18.6133911205225,122.345583287443)) ;
#89257 = CARTESIAN_POINT('Ctrl Pts',(-20.6422769769176,18.6232888038339,122.544802617581)) ;
#89258 = CARTESIAN_POINT('Ctrl Pts',(-20.7735588255307,18.6332198442079,122.770350862156)) ;
#89259 = CARTESIAN_POINT('Ctrl Pts',(-20.8644257386545,18.6432620618645,123.018108220622)) ;
#89260 = CARTESIAN_POINT('Ctrl Pts',(-20.9103608198524,18.6531487225985,123.2738391975)) ;
#89261 = CARTESIAN_POINT('Ctrl Pts',(-20.9116439914806,18.663141831201,123.536431039595)) ;
#89262 = CARTESIAN_POINT('Ctrl Pts',(-20.8674236850463,18.6730875298392,123.794025919388)) ;
#89263 = CARTESIAN_POINT('Ctrl Pts',(-20.7796339406571,18.6830347521103,124.040260003737)) ;
#89264 = CARTESIAN_POINT('Ctrl Pts',(-20.648865853499,18.6930827776904,124.269647102596)) ;
#89265 = CARTESIAN_POINT('Ctrl Pts',(-20.4837880164837,18.7029300248333,124.468930982032)) ;
#89266 = CARTESIAN_POINT('Ctrl Pts',(-20.2848353076597,18.712893201924,124.639124066068)) ;
#89267 = CARTESIAN_POINT('Ctrl Pts',(-20.057643225627,18.7229229229575,124.772734603442)) ;
#89268 = CARTESIAN_POINT('Ctrl Pts',(-19.8138733025437,18.7328273904903,124.864024891333)) ;
#89269 = CARTESIAN_POINT('Ctrl Pts',(-19.5549244555012,18.7428518763201,124.91225661059)) ;
#89270 = CARTESIAN_POINT('Ctrl Pts',(-19.2946394655604,18.752755711444,124.914979535986)) ;
#89271 = CARTESIAN_POINT('Ctrl Pts',(-19.0340712151648,18.762806902154,124.871903053952)) ;
#89272 = CARTESIAN_POINT('Ctrl Pts',(-18.7890046631621,18.7726913448123,124.785719653912)) ;
#89273 = CARTESIAN_POINT('Ctrl Pts',(-18.5599429927726,18.7826843526642,124.657344067074)) ;
#89274 = CARTESIAN_POINT('Ctrl Pts',(-18.3575852293697,18.7926326723805,124.491794444498)) ;
#89275 = CARTESIAN_POINT('Ctrl Pts',(-18.1869857767214,18.8025695110899,124.294126119609)) ;
#89276 = CARTESIAN_POINT('Ctrl Pts',(-18.0523654033191,18.8125525000095,124.068917991237)) ;
#89277 = CARTESIAN_POINT('Ctrl Pts',(-17.9588008233373,18.8225963793736,123.822148861517)) ;
#89278 = CARTESIAN_POINT('Ctrl Pts',(-17.9099472787027,18.832424444732,123.568497660891)) ;
#89279 = CARTESIAN_POINT('Ctrl Pts',(-17.9056636523394,18.8425015332869,123.303776150982)) ;
#89280 = CARTESIAN_POINT('Ctrl Pts',(-17.9463206545568,18.8523516854432,123.048068626949)) ;
#89281 = CARTESIAN_POINT('Ctrl Pts',(-18.0325884242925,18.8624321658956,122.797675319086)) ;
#89282 = CARTESIAN_POINT('Ctrl Pts',(-18.1574960786457,18.8722466636644,122.571957568326)) ;
#89283 = CARTESIAN_POINT('Ctrl Pts',(-18.3234918042426,18.8823149596845,122.366002659658)) ;
#89284 = CARTESIAN_POINT('Ctrl Pts',(-18.5195168321674,18.8922137921673,122.194898302409)) ;
#89285 = CARTESIAN_POINT('Ctrl Pts',(-18.7455899254507,18.9022666721818,122.058322027411)) ;
#89286 = CARTESIAN_POINT('Ctrl Pts',(-18.9874685791596,18.912136487678,121.96454261231)) ;
#89287 = CARTESIAN_POINT('Ctrl Pts',(-19.247074514884,18.9222091687608,121.913098195303)) ;
#89288 = CARTESIAN_POINT('Ctrl Pts',(-19.5054282253465,18.9320416473318,121.907540984529)) ;
#89289 = CARTESIAN_POINT('Ctrl Pts',(-19.7660476083419,18.9420722813179,121.946964015993)) ;
#89290 = CARTESIAN_POINT('Ctrl Pts',(-20.015663124333,18.952103838537,122.031786628564)) ;
#89291 = CARTESIAN_POINT('Ctrl Pts',(-20.242340733487,18.9619335474087,122.155620704585)) ;
#89292 = CARTESIAN_POINT('Ctrl Pts',(-20.4478596794803,18.9719229962108,122.318956902595)) ;
#89293 = CARTESIAN_POINT('Ctrl Pts',(-20.6223353947974,18.9819668486108,122.517002479713)) ;
#89294 = CARTESIAN_POINT('Ctrl Pts',(-20.7571909721581,18.9917885619429,122.737075061606)) ;
#89295 = CARTESIAN_POINT('Ctrl Pts',(-20.8544420213186,19.0018235669316,122.982196100149)) ;
#89296 = CARTESIAN_POINT('Ctrl Pts',(-20.9068867752531,19.0118484053792,123.24037432519)) ;
#89297 = CARTESIAN_POINT('Ctrl Pts',(-20.9141429657687,19.0217006183344,123.499179168148)) ;
#89298 = CARTESIAN_POINT('Ctrl Pts',(-20.8762673910892,19.0316905745282,123.758937854536)) ;
#89299 = CARTESIAN_POINT('Ctrl Pts',(-20.7943862514496,19.0416186848114,124.00666549439)) ;
#89300 = CARTESIAN_POINT('Ctrl Pts',(-20.6703510230735,19.051607284891,124.238008956621)) ;
#89301 = CARTESIAN_POINT('Ctrl Pts',(-20.5071291776537,19.0616338768185,124.444859269663)) ;
#89302 = CARTESIAN_POINT('Ctrl Pts',(-20.3134350002054,19.0715190048827,124.617949216475)) ;
#89303 = CARTESIAN_POINT('Ctrl Pts',(-20.0905630047009,19.0815101223562,124.756761630848)) ;
#89304 = CARTESIAN_POINT('Ctrl Pts',(-19.8455702342905,19.091550738208,124.854732580101)) ;
#89305 = CARTESIAN_POINT('Ctrl Pts',(-19.5927186533089,19.1013837290617,124.907978535889)) ;
#89306 = CARTESIAN_POINT('Ctrl Pts',(-19.3302830880624,19.111376860512,124.917403980521)) ;
#89307 = CARTESIAN_POINT('Ctrl Pts',(-19.0692443271857,19.1214089089474,124.880431822587)) ;
#89308 = CARTESIAN_POINT('Ctrl Pts',(-18.8226828953735,19.1312741554898,124.800366929372)) ;
#89309 = CARTESIAN_POINT('Ctrl Pts',(-18.5911601979227,19.1412360303166,124.678161518773)) ;
#89310 = CARTESIAN_POINT('Ctrl Pts',(-18.3831390570505,19.1512709934279,124.516107567008)) ;
#89311 = CARTESIAN_POINT('Ctrl Pts',(-18.2086970669107,19.1611558378903,124.323580061315)) ;
#89312 = CARTESIAN_POINT('Ctrl Pts',(-18.0679004045374,19.171221890731,124.099692955036)) ;
#89313 = CARTESIAN_POINT('Ctrl Pts',(-17.9700782692514,19.18105940664,123.860343413881)) ;
#89314 = CARTESIAN_POINT('Ctrl Pts',(-17.9137587529611,19.1911281547489,123.601857544703)) ;
#89315 = CARTESIAN_POINT('Ctrl Pts',(-17.9034670306657,19.2010086717799,123.342371871998)) ;
#89316 = CARTESIAN_POINT('Ctrl Pts',(-17.9382401306853,19.2109998587144,123.08216562488)) ;
#89317 = CARTESIAN_POINT('Ctrl Pts',(-18.017346517817,19.2209529249893,122.83281725219)) ;
#89318 = CARTESIAN_POINT('Ctrl Pts',(-18.1396020443988,19.2309887625219,122.599158531839)) ;
#89319 = CARTESIAN_POINT('Ctrl Pts',(-18.2981172600277,19.2408788887333,122.393170709056)) ;
#89320 = CARTESIAN_POINT('Ctrl Pts',(-18.4916634610177,19.2508710706413,122.215735660309)) ;
#89321 = CARTESIAN_POINT('Ctrl Pts',(-18.7121126054784,19.2608170105799,122.075322038536)) ;
#89322 = CARTESIAN_POINT('Ctrl Pts',(-18.9534330921312,19.270764194344,121.974810909958)) ;
#89323 = CARTESIAN_POINT('Ctrl Pts',(-19.2111660245585,19.2808121326514,121.917443070718)) ;
#89324 = CARTESIAN_POINT('Ctrl Pts',(-19.46968806927,19.2906597673917,121.905712436638)) ;
#89325 = CARTESIAN_POINT('Ctrl Pts',(-19.7293828802566,19.3006214813655,121.938618525281)) ;
#89326 = CARTESIAN_POINT('Ctrl Pts',(-19.9810273924312,19.3106501161564,122.01696448955)) ;
#89327 = CARTESIAN_POINT('Ctrl Pts',(-20.2124964374937,19.3205604347535,122.136300351223)) ;
#89328 = CARTESIAN_POINT('Ctrl Pts',(-20.4206742458988,19.330495291065,122.293871266416)) ;
#89329 = CARTESIAN_POINT('Ctrl Pts',(-20.6000312207341,19.3405365270257,122.487400631673)) ;
#89330 = CARTESIAN_POINT('Ctrl Pts',(-20.7410617512557,19.3504232986057,122.705636493677)) ;
#89331 = CARTESIAN_POINT('Ctrl Pts',(-20.8434829085783,19.3604234773119,122.947608430064)) ;
#89332 = CARTESIAN_POINT('Ctrl Pts',(-20.9020842657226,19.3703407555215,123.201594819178)) ;
#89333 = CARTESIAN_POINT('Ctrl Pts',(-20.9157885273105,19.3803880019352,123.465233400112)) ;
#89334 = CARTESIAN_POINT('Ctrl Pts',(-20.8843312394049,19.3902618909165,123.722835831488)) ;
#89335 = CARTESIAN_POINT('Ctrl Pts',(-20.8073413256974,19.400323908497,123.975764420132)) ;
#89336 = CARTESIAN_POINT('Ctrl Pts',(-20.6898211294301,19.4101949702313,124.207038033062)) ;
#89337 = CARTESIAN_POINT('Ctrl Pts',(-20.5325845494946,19.4201890335916,124.417401603479)) ;
#89338 = CARTESIAN_POINT('Ctrl Pts',(-20.3400856995338,19.430221191625,124.59752229965)) ;
#89339 = CARTESIAN_POINT('Ctrl Pts',(-20.1232221891283,19.4400850678652,124.739562342653)) ;
#89340 = CARTESIAN_POINT('Ctrl Pts',(-19.8800650899672,19.4501555825034,124.843936496975)) ;
#89341 = CARTESIAN_POINT('Ctrl Pts',(-19.6283151955898,19.4599962194444,124.903158307787)) ;
#89342 = CARTESIAN_POINT('Ctrl Pts',(-19.3668809125715,19.4699633482846,124.91881772904)) ;
#89343 = CARTESIAN_POINT('Ctrl Pts',(-19.1054682843621,19.4799773214091,124.888425374719)) ;
#89344 = CARTESIAN_POINT('Ctrl Pts',(-18.7709161948087,19.4932620552724,124.788603773578)) ;
#89345 = CARTESIAN_POINT('Ctrl Pts',(-18.4713172138264,19.5064873199872,124.604876555852)) ;
#89346 = CARTESIAN_POINT('Ctrl Pts',(-18.2302531727005,19.519797842542,124.351369013514)) ;
#89347 = CARTESIAN_POINT('Ctrl Pts',(-18.0847512811712,19.5298264874442,124.131644354945)) ;
#89348 = CARTESIAN_POINT('Ctrl Pts',(-17.9809400631191,19.5397075197981,123.89362910154)) ;
#89349 = CARTESIAN_POINT('Ctrl Pts',(-17.9188886192552,19.5496884924782,123.638788056693)) ;
#89350 = CARTESIAN_POINT('Ctrl Pts',(-17.902254691945,19.5596696200642,123.377037428699)) ;
#89351 = CARTESIAN_POINT('Ctrl Pts',(-17.9400916999754,19.5729128103256,123.031015386685)) ;
#89352 = CARTESIAN_POINT('Ctrl Pts',(-18.1006952198866,19.5895808056864,122.618253916938)) ;
#89353 = CARTESIAN_POINT('Ctrl Pts',(-18.3897868588537,19.6061013056984,122.287674714517)) ;
#89354 = CARTESIAN_POINT('Ctrl Pts',(-18.6800761568763,19.6194143220144,122.092482801336)) ;
#89355 = CARTESIAN_POINT('Ctrl Pts',(-18.9182029603172,19.6293308802474,121.986519910248)) ;
#89356 = CARTESIAN_POINT('Ctrl Pts',(-19.1738678812539,19.6393585485503,121.922922940547)) ;
#89357 = CARTESIAN_POINT('Ctrl Pts',(-19.5194780323658,19.652539138295,121.898097021449)) ;
#89358 = CARTESIAN_POINT('Ctrl Pts',(-19.9563288314783,19.6692872774143,121.982471851941)) ;
#89359 = CARTESIAN_POINT('Ctrl Pts',(-20.4082007931077,19.6890820199249,122.252403503244)) ;
#89360 = CARTESIAN_POINT('Ctrl Pts',(-20.7451774511471,19.7091264127337,122.664799510157)) ;
#89361 = CARTESIAN_POINT('Ctrl Pts',(-20.9190665009058,19.7289655950324,123.162745067453)) ;
#89362 = CARTESIAN_POINT('Ctrl Pts',(-20.9138754834601,19.7488909187253,123.692173591397)) ;
#89363 = CARTESIAN_POINT('Ctrl Pts',(-20.7282061366091,19.7688145567768,124.188186165143)) ;
#89364 = CARTESIAN_POINT('Ctrl Pts',(-20.384618994923,19.7887394302423,124.591086031158)) ;
#89365 = CARTESIAN_POINT('Ctrl Pts',(-19.9254980781481,19.8086180373213,124.852590538209)) ;
#89366 = CARTESIAN_POINT('Ctrl Pts',(-19.4021944235472,19.8285954801532,124.942415684017)) ;
#89367 = CARTESIAN_POINT('Ctrl Pts',(-18.8808504945977,19.8485273282379,124.848110950266)) ;
#89368 = CARTESIAN_POINT('Ctrl Pts',(-18.4236327836799,19.8684225965805,124.582537401173)) ;
#89369 = CARTESIAN_POINT('Ctrl Pts',(-18.0835396042065,19.8883450949926,124.176670177314)) ;
#89370 = CARTESIAN_POINT('Ctrl Pts',(-17.9021501379471,19.9083045768686,123.678122009356)) ;
#89371 = CARTESIAN_POINT('Ctrl Pts',(-17.9016826808945,19.928182329328,123.14988706624)) ;
#89372 = CARTESIAN_POINT('Ctrl Pts',(-18.0801848929392,19.9480641200625,122.652414260717)) ;
#89373 = CARTESIAN_POINT('Ctrl Pts',(-18.4216899540666,19.9681374589135,122.242615414334)) ;
#89374 = CARTESIAN_POINT('Ctrl Pts',(-18.8764503196767,19.9879419261493,121.977339845321)) ;
#89375 = CARTESIAN_POINT('Ctrl Pts',(-19.398725666126,20.0079252665571,121.881194515216)) ;
#89376 = CARTESIAN_POINT('Ctrl Pts',(-19.9205991086772,20.0278402311551,121.96959503457)) ;
#89377 = CARTESIAN_POINT('Ctrl Pts',(-20.3807214883969,20.0477087658715,122.228929102253)) ;
#89378 = CARTESIAN_POINT('Ctrl Pts',(-20.7270865861408,20.0677611500832,122.633789392997)) ;
#89379 = CARTESIAN_POINT('Ctrl Pts',(-20.9126916804623,20.0875351138724,123.125708607321)) ;
#89380 = CARTESIAN_POINT('Ctrl Pts',(-20.9197926939565,20.1075894928938,123.658461280195)) ;
#89381 = CARTESIAN_POINT('Ctrl Pts',(-20.7466018541178,20.127386230467,124.1554690317)) ;
#89382 = CARTESIAN_POINT('Ctrl Pts',(-20.4126503321151,20.1473540428185,124.567785296605)) ;
#89383 = CARTESIAN_POINT('Ctrl Pts',(-19.9576268829892,20.1673130188835,124.840673205932)) ;
#89384 = CARTESIAN_POINT('Ctrl Pts',(-19.4386508322908,20.1872079371609,124.94188751217)) ;
#89385 = CARTESIAN_POINT('Ctrl Pts',(-18.9161782831837,20.2071042496112,124.860571732585)) ;
#89386 = CARTESIAN_POINT('Ctrl Pts',(-18.4521872012561,20.2270121829853,124.606170401089)) ;
#89387 = CARTESIAN_POINT('Ctrl Pts',(-18.1022237455605,20.2469620732738,124.207890683089)) ;
#89388 = CARTESIAN_POINT('Ctrl Pts',(-17.9093454009066,20.2668393037751,123.715999312751)) ;
#89389 = CARTESIAN_POINT('Ctrl Pts',(-17.8955608540406,20.2868219726461,123.185097942073)) ;
#89390 = CARTESIAN_POINT('Ctrl Pts',(-18.0637245954641,20.3067548592265,122.682641570739)) ;
#89391 = CARTESIAN_POINT('Ctrl Pts',(-18.3925761888793,20.3266676052444,122.268015072213)) ;
#89392 = CARTESIAN_POINT('Ctrl Pts',(-18.7672875195584,20.3432373265862,122.036639218976)) ;
#89393 = CARTESIAN_POINT('Ctrl Pts',(-19.1020112523894,20.3565373378912,121.93602784581)) ;
#89394 = CARTESIAN_POINT('Ctrl Pts',(-19.4482933884682,20.3698075256411,121.894667854607)) ;
#89395 = CARTESIAN_POINT('Ctrl Pts',(-19.8857616860693,20.3864349080065,121.957330261882)) ;
#89396 = CARTESIAN_POINT('Ctrl Pts',(-20.2753843629908,20.4030571977517,122.165611719854)) ;
#89397 = CARTESIAN_POINT('Ctrl Pts',(-20.5295904307739,20.4163024121462,122.403368996714)) ;
#89398 = CARTESIAN_POINT('Ctrl Pts',(-20.6866680641732,20.4262143771069,122.61117509767)) ;
#89399 = CARTESIAN_POINT('Ctrl Pts',(-20.806737474672,20.4362730002714,122.846628519742)) ;
#89400 = CARTESIAN_POINT('Ctrl Pts',(-20.8828053848385,20.4461131143872,123.093815056759)) ;
#89401 = CARTESIAN_POINT('Ctrl Pts',(-20.9157850235484,20.4561788993448,123.356230024175)) ;
#89402 = CARTESIAN_POINT('Ctrl Pts',(-20.9028213821857,20.4660622171327,123.615663268066)) ;
#89403 = CARTESIAN_POINT('Ctrl Pts',(-20.8449589694743,20.4760516549913,123.871692434311)) ;
#89404 = CARTESIAN_POINT('Ctrl Pts',(-20.74368006627,20.486015369044,124.113161475895)) ;
#89405 = CARTESIAN_POINT('Ctrl Pts',(-20.6017961937113,20.4960103807032,124.334224144279)) ;
#89406 = CARTESIAN_POINT('Ctrl Pts',(-20.4226668968658,20.5060466723975,124.527786878245)) ;
#89407 = CARTESIAN_POINT('Ctrl Pts',(-20.2168574908497,20.5158930500909,124.684641027028)) ;
#89408 = CARTESIAN_POINT('Ctrl Pts',(-19.9839816914647,20.5258779942416,124.805469402538)) ;
#89409 = CARTESIAN_POINT('Ctrl Pts',(-19.7348364121739,20.5358149653716,124.883819573151)) ;
#89410 = CARTESIAN_POINT('Ctrl Pts',(-19.4729804417369,20.5458647500033,124.917956892684)) ;
#89411 = CARTESIAN_POINT('Ctrl Pts',(-19.2143536333705,20.5557152120808,124.906538794214)) ;
#89412 = CARTESIAN_POINT('Ctrl Pts',(-18.9584230841274,20.5656872256012,124.850373618486)) ;
#89413 = CARTESIAN_POINT('Ctrl Pts',(-18.7155134690777,20.5756823727206,124.75033150436)) ;
#89414 = CARTESIAN_POINT('Ctrl Pts',(-18.4930284866175,20.5857163424567,124.608850714625)) ;
#89415 = CARTESIAN_POINT('Ctrl Pts',(-18.301639069362,20.5955718881273,124.43432218421)) ;
#89416 = CARTESIAN_POINT('Ctrl Pts',(-18.1409105781554,20.6055706451405,124.22651165924)) ;
#89417 = CARTESIAN_POINT('Ctrl Pts',(-18.0196900933075,20.6154677803777,123.996357848347)) ;
#89418 = CARTESIAN_POINT('Ctrl Pts',(-17.9389969296105,20.6255208762173,123.744826815494)) ;
#89419 = CARTESIAN_POINT('Ctrl Pts',(-17.9037758541384,20.6354043849479,123.487479681158)) ;
#89420 = CARTESIAN_POINT('Ctrl Pts',(-17.9132711224096,20.645399257594,123.225004546721)) ;
#89421 = CARTESIAN_POINT('Ctrl Pts',(-17.9687399657228,20.6554192192297,122.96758422729)) ;
#89422 = CARTESIAN_POINT('Ctrl Pts',(-18.0667172219578,20.6653245830296,122.726428828135)) ;
#89423 = CARTESIAN_POINT('Ctrl Pts',(-18.2051112656729,20.6752651706371,122.504892851635)) ;
#89424 = CARTESIAN_POINT('Ctrl Pts',(-18.3808832318701,20.6852679887378,122.309400454705)) ;
#89425 = CARTESIAN_POINT('Ctrl Pts',(-18.5888185798447,20.6953027004619,122.147247116949)) ;
#89426 = CARTESIAN_POINT('Ctrl Pts',(-18.8171665168026,20.7051476071992,122.025597143536)) ;
#89427 = CARTESIAN_POINT('Ctrl Pts',(-19.0664811329135,20.7151334597682,121.943845159401)) ;
#89428 = CARTESIAN_POINT('Ctrl Pts',(-19.3249386776779,20.7250682681813,121.906617308344)) ;
#89429 = CARTESIAN_POINT('Ctrl Pts',(-19.5890636684313,20.7351257952623,121.915166166779)) ;
#89430 = CARTESIAN_POINT('Ctrl Pts',(-19.8417720817048,20.7449474502594,121.967799082809)) ;
#89431 = CARTESIAN_POINT('Ctrl Pts',(-20.0873597067846,20.7550034944324,122.065317687553)) ;
#89432 = CARTESIAN_POINT('Ctrl Pts',(-20.3094854721539,20.7649442344776,122.202825084637)) ;
#89433 = CARTESIAN_POINT('Ctrl Pts',(-20.5041808420828,20.7748483555505,122.375555985901)) ;
#89434 = CARTESIAN_POINT('Ctrl Pts',(-20.6681287825517,20.7848958967047,122.582504505087)) ;
#89435 = CARTESIAN_POINT('Ctrl Pts',(-20.7919881814226,20.7947946483051,122.811292280779)) ;
#89436 = CARTESIAN_POINT('Ctrl Pts',(-20.8755740195429,20.8048431272709,123.061746962003)) ;
#89437 = CARTESIAN_POINT('Ctrl Pts',(-20.9138090117843,20.8147306243546,123.318779270284)) ;
#89438 = CARTESIAN_POINT('Ctrl Pts',(-20.9072479453517,20.8247237146527,123.581282226704)) ;
#89439 = CARTESIAN_POINT('Ctrl Pts',(-20.8553241322653,20.834675884713,123.837624769112)) ;
#89440 = CARTESIAN_POINT('Ctrl Pts',(-20.7601574063262,20.8446143046275,124.080820832448)) ;
#89441 = CARTESIAN_POINT('Ctrl Pts',(-20.6237998714096,20.8545994347131,124.305038244249)) ;
#89442 = CARTESIAN_POINT('Ctrl Pts',(-20.4494221518513,20.8646361241272,124.502900480269)) ;
#89443 = CARTESIAN_POINT('Ctrl Pts',(-20.2473013388322,20.8744908081197,124.664842526609)) ;
#89444 = CARTESIAN_POINT('Ctrl Pts',(-20.0170290666669,20.8844902921675,124.7913425284)) ;
#89445 = CARTESIAN_POINT('Ctrl Pts',(-19.7708926225284,20.8943853809444,124.875346148885)) ;
#89446 = CARTESIAN_POINT('Ctrl Pts',(-19.5096857275806,20.9044459355906,124.915966548158)) ;
#89447 = CARTESIAN_POINT('Ctrl Pts',(-19.2508869429393,20.9142951999635,124.910873014686)) ;
#89448 = CARTESIAN_POINT('Ctrl Pts',(-18.9922127135504,20.9243224524113,124.860678227348)) ;
#89449 = CARTESIAN_POINT('Ctrl Pts',(-18.7463889477668,20.9343507499815,124.765668763576)) ;
#89450 = CARTESIAN_POINT('Ctrl Pts',(-18.5246560820803,20.9441968789875,124.632331993503)) ;
#89451 = CARTESIAN_POINT('Ctrl Pts',(-18.3260748632208,20.9541907843496,124.460462272426)) ;
#89452 = CARTESIAN_POINT('Ctrl Pts',(-18.1602131738219,20.9642148820326,124.255803821438)) ;
#89453 = CARTESIAN_POINT('Ctrl Pts',(-18.0338336778558,20.9741047098866,124.028700863845)) ;
#89454 = CARTESIAN_POINT('Ctrl Pts',(-17.9475715523185,20.9840966913171,123.780706945075)) ;
#89455 = CARTESIAN_POINT('Ctrl Pts',(-17.9059277190108,20.9940436960829,123.522648076826)) ;
#89456 = CARTESIAN_POINT('Ctrl Pts',(-17.9092446774268,21.0039933474727,123.26119173999)) ;
#89457 = CARTESIAN_POINT('Ctrl Pts',(-17.9585439446535,21.0140303504501,123.002085877506)) ;
#89458 = CARTESIAN_POINT('Ctrl Pts',(-18.0505382977171,21.0239192588851,122.759033267901)) ;
#89459 = CARTESIAN_POINT('Ctrl Pts',(-18.1842691504711,21.0339085913626,122.533148901569)) ;
#89460 = CARTESIAN_POINT('Ctrl Pts',(-18.3548109388882,21.0438671467997,122.334658060956)) ;
#89461 = CARTESIAN_POINT('Ctrl Pts',(-18.5556391649582,21.0537667180002,122.16926520889)) ;
#89462 = CARTESIAN_POINT('Ctrl Pts',(-18.7855363124599,21.0638146432522,122.039439979611)) ;
#89463 = CARTESIAN_POINT('Ctrl Pts',(-19.030698238794,21.0737099427782,121.952623471748)) ;
#89464 = CARTESIAN_POINT('Ctrl Pts',(-19.291450065471,21.0837717992262,121.908950298832)) ;
#89465 = CARTESIAN_POINT('Ctrl Pts',(-19.5501399989178,21.0936156456428,121.91111408291)) ;
#89466 = CARTESIAN_POINT('Ctrl Pts',(-19.807740031436,21.1035785947709,121.957838664783)) ;
#89467 = CARTESIAN_POINT('Ctrl Pts',(-20.0549347555783,21.1136126311989,122.049642784503)) ;
#89468 = CARTESIAN_POINT('Ctrl Pts',(-20.2792391844421,21.1235000581569,122.180784673848)) ;
#89469 = CARTESIAN_POINT('Ctrl Pts',(-20.4802501125778,21.1335144924933,122.350672310585)) ;
#89470 = CARTESIAN_POINT('Ctrl Pts',(-20.6485231786559,21.1435494371282,122.553690979311)) ;
#89471 = CARTESIAN_POINT('Ctrl Pts',(-20.776994667693,21.1533817871592,122.777909498819)) ;
#89472 = CARTESIAN_POINT('Ctrl Pts',(-20.8667919124949,21.1634572262764,123.026935129347)) ;
#89473 = CARTESIAN_POINT('Ctrl Pts',(-20.911151449371,21.173309691511,123.282075921991)) ;
#89474 = CARTESIAN_POINT('Ctrl Pts',(-20.9107346702923,21.1833825690879,123.546735142883)) ;
#89475 = CARTESIAN_POINT('Ctrl Pts',(-20.8653838187256,21.1932251652804,123.801404395061)) ;
#89476 = CARTESIAN_POINT('Ctrl Pts',(-20.776098005712,21.2032055493957,124.048000989328)) ;
#89477 = CARTESIAN_POINT('Ctrl Pts',(-20.6444053880161,21.2132240300445,124.275965170634)) ;
#89478 = CARTESIAN_POINT('Ctrl Pts',(-20.4778156031857,21.2231073450449,124.47526543333)) ;
#89479 = CARTESIAN_POINT('Ctrl Pts',(-20.2754160656576,21.2331756421353,124.645605897759)) ;
#89480 = CARTESIAN_POINT('Ctrl Pts',(-20.0520068570127,21.2430057105076,124.775388910782)) ;
#89481 = CARTESIAN_POINT('Ctrl Pts',(-19.8038192003743,21.253072502976,124.866829885988)) ;
#89482 = CARTESIAN_POINT('Ctrl Pts',(-19.5479997475856,21.2629618364645,124.912863623908)) ;
#89483 = CARTESIAN_POINT('Ctrl Pts',(-19.2852043849924,21.2729639678806,124.914202847899)) ;
#89484 = CARTESIAN_POINT('Ctrl Pts',(-19.0280750006297,21.2828878375016,124.870388521691)) ;
#89485 = CARTESIAN_POINT('Ctrl Pts',(-18.77960570535,21.2929313530188,124.781491000549)) ;
#89486 = CARTESIAN_POINT('Ctrl Pts',(-18.5538025555048,21.3028135659071,124.653119146439)) ;
#89487 = CARTESIAN_POINT('Ctrl Pts',(-18.3500349006823,21.3128816431265,124.484434278303)) ;
#89488 = CARTESIAN_POINT('Ctrl Pts',(-18.1823229673718,21.3227201478607,124.28760693878)) ;
#89489 = CARTESIAN_POINT('Ctrl Pts',(-18.0480641582105,21.3327829162901,124.059823359472)) ;
#89490 = CARTESIAN_POINT('Ctrl Pts',(-17.9571706997418,21.3426799095728,123.816123607726)) ;
#89491 = CARTESIAN_POINT('Ctrl Pts',(-17.9089560570351,21.3526111372076,123.559639960323)) ;
#89492 = CARTESIAN_POINT('Ctrl Pts',(-17.9062641201702,21.3626532958498,123.295759494904)) ;
#89493 = CARTESIAN_POINT('Ctrl Pts',(-17.9485807750656,21.3725400053808,123.039404443611)) ;
#89494 = CARTESIAN_POINT('Ctrl Pts',(-18.0352662045675,21.3825329778094,122.791531975748)) ;
#89495 = CARTESIAN_POINT('Ctrl Pts',(-18.1631733074527,21.392479172346,122.56359572005)) ;
#89496 = CARTESIAN_POINT('Ctrl Pts',(-18.3282744150043,21.4024245471975,122.360963544721)) ;
#89497 = CARTESIAN_POINT('Ctrl Pts',(-18.5284565572223,21.4124794665574,122.188538399723)) ;
#89498 = CARTESIAN_POINT('Ctrl Pts',(-18.7500672200615,21.4223009860009,122.056167239099)) ;
#89499 = CARTESIAN_POINT('Ctrl Pts',(-18.9971032250605,21.4323667547678,121.961729368594)) ;
#89500 = CARTESIAN_POINT('Ctrl Pts',(-19.252665844166,21.4422686764229,121.912504687733)) ;
#89501 = CARTESIAN_POINT('Ctrl Pts',(-19.516526510854,21.4523117352439,121.908111222315)) ;
#89502 = CARTESIAN_POINT('Ctrl Pts',(-19.7735943063744,21.4622177292866,121.949174521215)) ;
#89503 = CARTESIAN_POINT('Ctrl Pts',(-20.0206585177756,21.4721555023684,122.033793699405)) ;
#89504 = CARTESIAN_POINT('Ctrl Pts',(-20.2514967965682,21.4821958661007,122.161575037695)) ;
#89505 = CARTESIAN_POINT('Ctrl Pts',(-20.4536528904977,21.4920832098242,122.324826619752)) ;
#89506 = CARTESIAN_POINT('Ctrl Pts',(-20.6265093028174,21.5020754403929,122.522468692439)) ;
#89507 = CARTESIAN_POINT('Ctrl Pts',(-20.7617843910413,21.5120239681765,122.746204499775)) ;
#89508 = CARTESIAN_POINT('Ctrl Pts',(-20.8563752029685,21.5219607518998,122.989574942634)) ;
#89509 = CARTESIAN_POINT('Ctrl Pts',(-20.9078459005937,21.5319437526968,123.246853300404)) ;
#89510 = CARTESIAN_POINT('Ctrl Pts',(-20.9134112422956,21.5419876395375,123.510706398789)) ;
#89511 = CARTESIAN_POINT('Ctrl Pts',(-20.8745423295287,21.5518156631121,123.766077419227)) ;
#89512 = CARTESIAN_POINT('Ctrl Pts',(-20.7899649656379,21.5618929113257,124.016964720075)) ;
#89513 = CARTESIAN_POINT('Ctrl Pts',(-20.6660716447633,21.571742466631,124.244301696396)) ;
#89514 = CARTESIAN_POINT('Ctrl Pts',(-20.5009218271621,21.5818251748287,124.451413147156)) ;
#89515 = CARTESIAN_POINT('Ctrl Pts',(-20.3077024679785,21.5916377677552,124.622265315751)) ;
#89516 = CARTESIAN_POINT('Ctrl Pts',(-20.082372609264,21.6017049600131,124.76077174282)) ;
#89517 = CARTESIAN_POINT('Ctrl Pts',(-19.8403774418101,21.6116037894757,124.856379349723)) ;
#89518 = CARTESIAN_POINT('Ctrl Pts',(-19.5816048957035,21.6216577806659,124.909420890267)) ;
#89519 = CARTESIAN_POINT('Ctrl Pts',(-19.3222374612088,21.6315295054491,124.916826891635)) ;
#89520 = CARTESIAN_POINT('Ctrl Pts',(-19.0604462619463,21.6415999475793,124.878403745685)) ;
#89521 = CARTESIAN_POINT('Ctrl Pts',(-18.8151200955136,21.6514330260096,124.797161576374)) ;
#89522 = CARTESIAN_POINT('Ctrl Pts',(-18.5827353405762,21.661463499511,124.672775000186)) ;
#89523 = CARTESIAN_POINT('Ctrl Pts',(-18.3759109672851,21.6714950988097,124.509291299171)) ;
#89524 = CARTESIAN_POINT('Ctrl Pts',(-18.2037611889679,21.6813247998478,124.316724488468)) ;
#89525 = CARTESIAN_POINT('Ctrl Pts',(-18.0647714451557,21.6913142379043,124.094017139833)) ;
#89526 = CARTESIAN_POINT('Ctrl Pts',(-17.9666536761754,21.7013581411204,123.848992514289)) ;
#89527 = CARTESIAN_POINT('Ctrl Pts',(-17.9132395630017,21.7111796619339,123.596478590155)) ;
#89528 = CARTESIAN_POINT('Ctrl Pts',(-17.9036603191974,21.721215386181,123.332930237762)) ;
#89529 = CARTESIAN_POINT('Ctrl Pts',(-17.9406169716176,21.7312375401135,123.072144554952)) ;
#89530 = CARTESIAN_POINT('Ctrl Pts',(-18.0205753951748,21.7410997718708,122.825638668101)) ;
#89531 = CARTESIAN_POINT('Ctrl Pts',(-18.1426765255731,21.7510588423287,122.5941443993)) ;
#89532 = CARTESIAN_POINT('Ctrl Pts',(-18.3046553200881,21.7610940147049,122.386052860544)) ;
#89533 = CARTESIAN_POINT('Ctrl Pts',(-18.4970548092859,21.7709743998631,122.211659235178)) ;
#89534 = CARTESIAN_POINT('Ctrl Pts',(-18.7206332905695,21.7810311144571,122.070794791818)) ;
#89535 = CARTESIAN_POINT('Ctrl Pts',(-18.9610017685015,21.7909103830291,121.972655816629)) ;
#89536 = CARTESIAN_POINT('Ctrl Pts',(-19.2174642405481,21.8009013405148,121.916435631599)) ;
#89537 = CARTESIAN_POINT('Ctrl Pts',(-19.4811229674523,21.81094199915,121.906127926293)) ;
#89538 = CARTESIAN_POINT('Ctrl Pts',(-19.7372102471354,21.820774978858,121.940589760359)) ;
#89539 = CARTESIAN_POINT('Ctrl Pts',(-19.987662151828,21.8307681121077,122.019553890229)) ;
#89540 = CARTESIAN_POINT('Ctrl Pts',(-20.221266587985,21.8408001644911,122.141771264833)) ;
#89541 = CARTESIAN_POINT('Ctrl Pts',(-20.4268046448549,21.8506653934424,122.299749040127)) ;
#89542 = CARTESIAN_POINT('Ctrl Pts',(-20.6040649592092,21.8606273346856,122.492404487236)) ;
#89543 = CARTESIAN_POINT('Ctrl Pts',(-20.7458436231991,21.8706620497224,122.714735308757)) ;
#89544 = CARTESIAN_POINT('Ctrl Pts',(-20.8457694698757,21.8805478200664,122.954570602703)) ;
#89545 = CARTESIAN_POINT('Ctrl Pts',(-20.903532112246,21.8906104174552,123.212586648096)) ;
#89546 = CARTESIAN_POINT('Ctrl Pts',(-20.9154805876386,21.9004608292904,123.471189998348)) ;
#89547 = CARTESIAN_POINT('Ctrl Pts',(-20.882426858183,21.9104879985763,123.73260477288)) ;
#89548 = CARTESIAN_POINT('Ctrl Pts',(-20.8038186859197,21.9205154792905,123.984131914222)) ;
#89549 = CARTESIAN_POINT('Ctrl Pts',(-20.6854109255077,21.9303585318698,124.214093694813)) ;
#89550 = CARTESIAN_POINT('Ctrl Pts',(-20.5270023291853,21.9403524353084,124.423570385325)) ;
#89551 = CARTESIAN_POINT('Ctrl Pts',(-20.3336537691034,21.9503795580848,124.602604087814)) ;
#89552 = CARTESIAN_POINT('Ctrl Pts',(-20.1153478377517,21.9602702629769,124.743677527019)) ;
#89553 = CARTESIAN_POINT('Ctrl Pts',(-19.8735692667385,21.9702622898272,124.846083256019)) ;
#89554 = CARTESIAN_POINT('Ctrl Pts',(-19.6188372985755,21.9802082713157,124.904607587831)) ;
#89555 = CARTESIAN_POINT('Ctrl Pts',(-19.3577931878943,21.9901554439376,124.918542373026)) ;
#89556 = CARTESIAN_POINT('Ctrl Pts',(-19.0957252140819,22.0002033852638,124.886329581241)) ;
#89557 = CARTESIAN_POINT('Ctrl Pts',(-18.8481898209292,22.0100510190716,124.810847917876)) ;
#89558 = CARTESIAN_POINT('Ctrl Pts',(-18.6144904935636,22.0200127337566,124.692911935522)) ;
#89559 = CARTESIAN_POINT('Ctrl Pts',(-18.4035879139127,22.0300413666351,124.534852114603)) ;
#89560 = CARTESIAN_POINT('Ctrl Pts',(-18.2254150484394,22.0399516921703,124.344920009527)) ;
#89561 = CARTESIAN_POINT('Ctrl Pts',(-18.0819977432726,22.049886522642,124.126756044865)) ;
#89562 = CARTESIAN_POINT('Ctrl Pts',(-17.9777399583878,22.059927855024,123.884350623129)) ;
#89563 = CARTESIAN_POINT('Ctrl Pts',(-17.9179599830939,22.0698207284628,123.631344850412)) ;
#89564 = CARTESIAN_POINT('Ctrl Pts',(-17.9022371535386,22.0797898942807,123.369827155738)) ;
#89565 = CARTESIAN_POINT('Ctrl Pts',(-17.9327716986324,22.0898186279972,123.108078060828)) ;
#89566 = CARTESIAN_POINT('Ctrl Pts',(-18.0314269334723,22.1030111467684,122.775654275456)) ;
#89567 = CARTESIAN_POINT('Ctrl Pts',(-18.2167874151558,22.1163710148111,122.472935258562)) ;
#89568 = CARTESIAN_POINT('Ctrl Pts',(-18.4689775945887,22.1295963519599,122.233681798304)) ;
#89569 = CARTESIAN_POINT('Ctrl Pts',(-18.6872947818254,22.1395775778005,122.088312201797)) ;
#89570 = CARTESIAN_POINT('Ctrl Pts',(-18.9290513962181,22.1496131447834,121.982956255966)) ;
#89571 = CARTESIAN_POINT('Ctrl Pts',(-19.1809335406282,22.1594762227455,121.921719585)) ;
#89572 = CARTESIAN_POINT('Ctrl Pts',(-19.4449971797,22.1695465215466,121.904746363636)) ;
#89573 = CARTESIAN_POINT('Ctrl Pts',(-19.7020801434068,22.1793888201144,121.933241045844)) ;
#89574 = CARTESIAN_POINT('Ctrl Pts',(-19.9535498675344,22.1893495182842,122.005881902579)) ;
#89575 = CARTESIAN_POINT('Ctrl Pts',(-20.1901770423832,22.1993875524637,122.122446448014)) ;
#89576 = CARTESIAN_POINT('Ctrl Pts',(-20.3998103087612,22.2092612893102,122.275407092462)) ;
#89577 = CARTESIAN_POINT('Ctrl Pts',(-20.5832357329711,22.2193330732354,122.466165386452)) ;
#89578 = CARTESIAN_POINT('Ctrl Pts',(-20.7274078859713,22.2291651944366,122.680609736101)) ;
#89579 = CARTESIAN_POINT('Ctrl Pts',(-20.8349279101504,22.239198218462,122.921333612289)) ;
#89580 = CARTESIAN_POINT('Ctrl Pts',(-20.8982607406429,22.2492140986587,123.176824810715)) ;
#89581 = CARTESIAN_POINT('Ctrl Pts',(-20.9165125593692,22.2590976177529,123.43591069118)) ;
#89582 = CARTESIAN_POINT('Ctrl Pts',(-20.8895476418826,22.2690880301166,123.697042256073)) ;
#89583 = CARTESIAN_POINT('Ctrl Pts',(-20.794199097017,22.28235119332,124.032313731486)) ;
#89584 = CARTESIAN_POINT('Ctrl Pts',(-20.6136506128505,22.2956287635712,124.335485744995)) ;
#89585 = CARTESIAN_POINT('Ctrl Pts',(-20.3624307998912,22.3089590660778,124.579675665852)) ;
#89586 = CARTESIAN_POINT('Ctrl Pts',(-20.1474734503822,22.3188577478942,124.726159691664)) ;
#89587 = CARTESIAN_POINT('Ctrl Pts',(-19.9083044716856,22.3288472629417,124.8343602261)) ;
#89588 = CARTESIAN_POINT('Ctrl Pts',(-19.6550143972876,22.3387953147168,124.89911320866)) ;
#89589 = CARTESIAN_POINT('Ctrl Pts',(-19.3945571768419,22.3487367179953,124.919216158149)) ;
#89590 = CARTESIAN_POINT('Ctrl Pts',(-19.0469801715719,22.3620233827762,124.885646801854)) ;
#89591 = CARTESIAN_POINT('Ctrl Pts',(-18.6334919756593,22.378633804431,124.731055814575)) ;
#89592 = CARTESIAN_POINT('Ctrl Pts',(-18.2305162797271,22.3985450666818,124.387992218144)) ;
#89593 = CARTESIAN_POINT('Ctrl Pts',(-17.9681847100688,22.4184891958467,123.927340765981)) ;
#89594 = CARTESIAN_POINT('Ctrl Pts',(-17.8789700282879,22.4384123584518,123.405435456902)) ;
#89595 = CARTESIAN_POINT('Ctrl Pts',(-17.9722068017202,22.4583024808584,122.88499296031)) ;
#89596 = CARTESIAN_POINT('Ctrl Pts',(-18.2392469664603,22.4783074344585,122.425313505132)) ;
#89597 = CARTESIAN_POINT('Ctrl Pts',(-18.6435932599694,22.4981456914741,122.086755742294)) ;
#89598 = CARTESIAN_POINT('Ctrl Pts',(-19.1427570950757,22.5181399922607,121.904630400796)) ;
#89599 = CARTESIAN_POINT('Ctrl Pts',(-19.6712866823868,22.5380252343051,121.904256042346)) ;
#89600 = CARTESIAN_POINT('Ctrl Pts',(-20.1684531083155,22.557900180781,122.082765057008)) ;
#89601 = CARTESIAN_POINT('Ctrl Pts',(-20.5778666143493,22.5779332507221,122.423256582873)) ;
#89602 = CARTESIAN_POINT('Ctrl Pts',(-20.8439539041053,22.5978217576225,122.879952432642)) ;
#89603 = CARTESIAN_POINT('Ctrl Pts',(-20.9398901568453,22.6176766174038,123.398949134001)) ;
#89604 = CARTESIAN_POINT('Ctrl Pts',(-20.8512776370932,22.6377274511915,123.92432167666)) ;
#89605 = CARTESIAN_POINT('Ctrl Pts',(-20.5928105483306,22.6574933930808,124.381851942389)) ;
#89606 = CARTESIAN_POINT('Ctrl Pts',(-20.1896636816174,22.6775061245401,124.728595251841)) ;
#89607 = CARTESIAN_POINT('Ctrl Pts',(-19.6948416932879,22.6973989594837,124.915260290639)) ;
#89608 = CARTESIAN_POINT('Ctrl Pts',(-19.1659292643134,22.7173059828232,124.922744509421)) ;
#89609 = CARTESIAN_POINT('Ctrl Pts',(-18.6655675605648,22.7372212477239,124.749699013636)) ;
#89610 = CARTESIAN_POINT('Ctrl Pts',(-18.2524453398778,22.7572529398836,124.413924653691)) ;
#89611 = CARTESIAN_POINT('Ctrl Pts',(-17.9812029359813,22.7770959864566,123.961563010291)) ;
#89612 = CARTESIAN_POINT('Ctrl Pts',(-17.8790677895418,22.7970125343564,123.442240253503)) ;
#89613 = CARTESIAN_POINT('Ctrl Pts',(-17.9604555657489,22.8169447773477,122.918716094646)) ;
#89614 = CARTESIAN_POINT('Ctrl Pts',(-18.2149597212616,22.836848612157,122.454982006216)) ;
#89615 = CARTESIAN_POINT('Ctrl Pts',(-18.6119455544731,22.8567490123445,122.105477724641)) ;
#89616 = CARTESIAN_POINT('Ctrl Pts',(-19.1055301645696,22.8766986887238,121.911730698857)) ;
#89617 = CARTESIAN_POINT('Ctrl Pts',(-19.6351375624815,22.8966312129442,121.898173547559)) ;
#89618 = CARTESIAN_POINT('Ctrl Pts',(-20.1374387737837,22.9165512219304,122.065632357375)) ;
#89619 = CARTESIAN_POINT('Ctrl Pts',(-20.5530897144561,22.9365081281066,122.395063821693)) ;
#89620 = CARTESIAN_POINT('Ctrl Pts',(-20.8308724977881,22.9563939676081,122.844830062582)) ;
#89621 = CARTESIAN_POINT('Ctrl Pts',(-20.9388539512202,22.9763651397439,123.364411422884)) ;
#89622 = CARTESIAN_POINT('Ctrl Pts',(-20.8643389626638,22.9961793367283,123.885825621413)) ;
#89623 = CARTESIAN_POINT('Ctrl Pts',(-20.6149971103256,23.0161605226965,124.354606393768)) ;
#89624 = CARTESIAN_POINT('Ctrl Pts',(-20.2875827610197,23.0327360280858,124.64946647421)) ;
#89625 = CARTESIAN_POINT('Ctrl Pts',(-19.9761963329815,23.0460454759494,124.808750590775)) ;
#89626 = CARTESIAN_POINT('Ctrl Pts',(-19.6403478940357,23.059413173726,124.911784399414)) ;
#89627 = CARTESIAN_POINT('Ctrl Pts',(-19.2023596389031,23.0759037453919,124.927929061235)) ;
#89628 = CARTESIAN_POINT('Ctrl Pts',(-18.6980186540393,23.0958240177247,124.767071885537)) ;
#89629 = CARTESIAN_POINT('Ctrl Pts',(-18.3484072158521,23.1124410534457,124.497150544743)) ;
#89630 = CARTESIAN_POINT('Ctrl Pts',(-18.1364154882604,23.1257319037268,124.219541419118)) ;
#89631 = CARTESIAN_POINT('Ctrl Pts',(-18.0158927766921,23.1357009488813,123.986966551078)) ;
#89632 = CARTESIAN_POINT('Ctrl Pts',(-17.937590459842,23.1456043395148,123.738742873997)) ;
#89633 = CARTESIAN_POINT('Ctrl Pts',(-17.9031973751966,23.1556621256276,123.476711455943)) ;
#89634 = CARTESIAN_POINT('Ctrl Pts',(-17.9143593563858,23.1655141622773,123.218025990263)) ;
#89635 = CARTESIAN_POINT('Ctrl Pts',(-17.9896268659552,23.1788792864205,122.874973437508)) ;
#89636 = CARTESIAN_POINT('Ctrl Pts',(-18.151401302181,23.1921053493835,122.562854577334)) ;
#89637 = CARTESIAN_POINT('Ctrl Pts',(-18.3866165742264,23.2054089976658,122.304238650459)) ;
#89638 = CARTESIAN_POINT('Ctrl Pts',(-18.5942744744476,23.2154005288288,122.143499851417)) ;
#89639 = CARTESIAN_POINT('Ctrl Pts',(-18.8279217544426,23.2254399766281,122.02101181735)) ;
#89640 = CARTESIAN_POINT('Ctrl Pts',(-19.0743059149406,23.235283752142,121.942132253362)) ;
#89641 = CARTESIAN_POINT('Ctrl Pts',(-19.3342082548891,23.2452693935296,121.906215557607)) ;
#89642 = CARTESIAN_POINT('Ctrl Pts',(-19.595203409344,23.2552061778914,121.915784532965)) ;
#89643 = CARTESIAN_POINT('Ctrl Pts',(-19.8533817478491,23.2652560123588,121.971267328799)) ;
#89644 = CARTESIAN_POINT('Ctrl Pts',(-20.0932669657549,23.2751064618619,122.068597590794)) ;
#89645 = CARTESIAN_POINT('Ctrl Pts',(-20.3156335651349,23.285078475844,122.207190765456)) ;
#89646 = CARTESIAN_POINT('Ctrl Pts',(-20.5110432440586,23.2950736336911,122.382771699199)) ;
#89647 = CARTESIAN_POINT('Ctrl Pts',(-20.6733357401702,23.3051075600548,122.590562603099)) ;
#89648 = CARTESIAN_POINT('Ctrl Pts',(-20.7952641776477,23.3149632684872,122.81909160789)) ;
#89649 = CARTESIAN_POINT('Ctrl Pts',(-20.8771604366914,23.3249614178259,123.068699179642)) ;
#89650 = CARTESIAN_POINT('Ctrl Pts',(-20.9143466504709,23.3348608209994,123.326212352676)) ;
#89651 = CARTESIAN_POINT('Ctrl Pts',(-20.9061903378289,23.3449120178879,123.590193277281)) ;
#89652 = CARTESIAN_POINT('Ctrl Pts',(-20.8532554613795,23.3547943417008,123.844458307403)) ;
#89653 = CARTESIAN_POINT('Ctrl Pts',(-20.7564386685029,23.3647892373574,124.088610236154)) ;
#89654 = CARTESIAN_POINT('Ctrl Pts',(-20.6179988147476,23.3748103367399,124.312644230857)) ;
#89655 = CARTESIAN_POINT('Ctrl Pts',(-20.4449168413211,23.384717604602,124.507129660358)) ;
#89656 = CARTESIAN_POINT('Ctrl Pts',(-20.240390604112,23.3946559484272,124.669516991948)) ;
#89657 = CARTESIAN_POINT('Ctrl Pts',(-20.0093102113973,23.4046593677277,124.794907442227)) ;
#89658 = CARTESIAN_POINT('Ctrl Pts',(-19.7590948886003,23.4146939184348,124.878100956568)) ;
#89659 = CARTESIAN_POINT('Ctrl Pts',(-19.5031986835257,23.4245388680404,124.916298887153)) ;
#89660 = CARTESIAN_POINT('Ctrl Pts',(-19.240901379397,23.4345247101533,124.909881080696)) ;
#89661 = CARTESIAN_POINT('Ctrl Pts',(-18.9848919832439,23.4444595175224,124.858447576063)) ;
#89662 = CARTESIAN_POINT('Ctrl Pts',(-18.7388649759424,23.4545170592357,124.761980421742)) ;
#89663 = CARTESIAN_POINT('Ctrl Pts',(-18.5183526283299,23.4643386567478,124.627795609594)) ;
#89664 = CARTESIAN_POINT('Ctrl Pts',(-18.3195736794291,23.4743949162283,124.453691135326)) ;
#89665 = CARTESIAN_POINT('Ctrl Pts',(-18.1562934925279,23.4843348525287,124.249783586925)) ;
#89666 = CARTESIAN_POINT('Ctrl Pts',(-18.0306337931109,23.4942419732731,124.021771235105)) ;
#89667 = CARTESIAN_POINT('Ctrl Pts',(-17.9454129427096,23.5042848791984,123.771998892176)) ;
#89668 = CARTESIAN_POINT('Ctrl Pts',(-17.9053473190908,23.5141926602976,123.514723390938)) ;
#89669 = CARTESIAN_POINT('Ctrl Pts',(-17.9101532963783,23.5242030293,123.251696708579)) ;
#89670 = CARTESIAN_POINT('Ctrl Pts',(-17.961184062847,23.5342338678688,122.993085702516)) ;
#89671 = CARTESIAN_POINT('Ctrl Pts',(-18.0542237398046,23.5440867075085,122.751450868495)) ;
#89672 = CARTESIAN_POINT('Ctrl Pts',(-18.1892126976711,23.5540747086735,122.526373711805)) ;
#89673 = CARTESIAN_POINT('Ctrl Pts',(-18.3602268731788,23.5640035276526,122.329304006708)) ;
#89674 = CARTESIAN_POINT('Ctrl Pts',(-18.5637893871461,23.5739912303749,122.163599331592)) ;
#89675 = CARTESIAN_POINT('Ctrl Pts',(-18.7943337470643,23.5840272301776,122.035538227318)) ;
#89676 = CARTESIAN_POINT('Ctrl Pts',(-19.0390033894445,23.593882099979,121.95058970854)) ;
#89677 = CARTESIAN_POINT('Ctrl Pts',(-19.2983352169612,23.6038815304026,121.908467679911)) ;
#89678 = CARTESIAN_POINT('Ctrl Pts',(-19.5583918752554,23.6137766478679,121.911699650908)) ;
#89679 = CARTESIAN_POINT('Ctrl Pts',(-19.8181268029097,23.6238371413848,121.960855606037)) ;
#89680 = CARTESIAN_POINT('Ctrl Pts',(-20.0602942162802,23.633686621586,122.052288166794)) ;
#89681 = CARTESIAN_POINT('Ctrl Pts',(-20.2872341468449,23.6437130718498,122.186156421621)) ;
#89682 = CARTESIAN_POINT('Ctrl Pts',(-20.4871135693957,23.6537443623279,122.358035384557)) ;
#89683 = CARTESIAN_POINT('Ctrl Pts',(-20.6513848025357,23.6635857499797,122.55778850806)) ;
#89684 = CARTESIAN_POINT('Ctrl Pts',(-20.7809994490433,23.6735891508709,122.786461903559)) ;
#89685 = CARTESIAN_POINT('Ctrl Pts',(-20.8686943861811,23.6835735336621,123.033800795154)) ;
#89686 = CARTESIAN_POINT('Ctrl Pts',(-20.9120896033788,23.6936126236755,123.2939975435)) ;
#89687 = CARTESIAN_POINT('Ctrl Pts',(-20.9100555677439,23.7034584325847,123.552746650312)) ;
#89688 = CARTESIAN_POINT('Ctrl Pts',(-20.8629995601481,23.7134428554037,123.810834394173)) ;
#89689 = CARTESIAN_POINT('Ctrl Pts',(-20.7723339495502,23.7233824806449,124.055836429127)) ;
#89690 = CARTESIAN_POINT('Ctrl Pts',(-20.6391535588763,23.7334221701635,124.283563391533)) ;
#89691 = CARTESIAN_POINT('Ctrl Pts',(-20.4711070029557,23.7433103585821,124.481782915492)) ;
#89692 = CARTESIAN_POINT('Ctrl Pts',(-20.2694803443746,23.7532998845842,124.649877833456)) ;
#89693 = CARTESIAN_POINT('Ctrl Pts',(-20.042335267145,23.7632583859393,124.7798313255)) ;
#89694 = CARTESIAN_POINT('Ctrl Pts',(-19.7977296828341,23.773157979943,124.868459892283)) ;
#89695 = CARTESIAN_POINT('Ctrl Pts',(-19.5376387109747,23.7832058680643,124.913842306988)) ;
#89696 = CARTESIAN_POINT('Ctrl Pts',(-19.2775559394141,23.7931012933098,124.913585868621)) ;
#89697 = CARTESIAN_POINT('Ctrl Pts',(-19.0172389437925,23.8031626840104,124.867462659727)) ;
#89698 = CARTESIAN_POINT('Ctrl Pts',(-18.774152370709,23.8130082676971,124.778813564933)) ;
#89699 = CARTESIAN_POINT('Ctrl Pts',(-18.5470679864683,23.8229712410063,124.648540906934)) ;
#89700 = CARTESIAN_POINT('Ctrl Pts',(-18.3449854684297,23.8329969078321,124.479471088792)) ;
#89701 = CARTESIAN_POINT('Ctrl Pts',(-18.1771183031737,23.8429113856984,124.280226434427)) ;
#89702 = CARTESIAN_POINT('Ctrl Pts',(-18.0449530498413,23.8528999003734,124.053415180834)) ;
#89703 = CARTESIAN_POINT('Ctrl Pts',(-17.9542174865925,23.8629440112888,123.805578221622)) ;
#89704 = CARTESIAN_POINT('Ctrl Pts',(-17.9082598864059,23.8727721488834,123.551388438519)) ;
#89705 = CARTESIAN_POINT('Ctrl Pts',(-17.9069862290974,23.8828487169423,123.286644032258)) ;
#89706 = CARTESIAN_POINT('Ctrl Pts',(-17.9505929400621,23.8927008788465,123.031379907163)) ;
#89707 = CARTESIAN_POINT('Ctrl Pts',(-18.0395746759122,23.9027738408033,122.782125620061)) ;
#89708 = CARTESIAN_POINT('Ctrl Pts',(-18.1675552431538,23.9126164028062,122.557328161597)) ;
#89709 = CARTESIAN_POINT('Ctrl Pts',(-18.3342353084014,23.9225968393,122.35484385985)) ;
#89710 = CARTESIAN_POINT('Ctrl Pts',(-18.5346335209383,23.9326151446244,122.184110750498)) ;
#89711 = CARTESIAN_POINT('Ctrl Pts',(-18.7583418735152,23.9424991085438,122.052074633009)) ;
#89712 = CARTESIAN_POINT('Ctrl Pts',(-19.0060227711856,23.9525649852824,121.959294062984)) ;
#89713 = CARTESIAN_POINT('Ctrl Pts',(-19.2602154899171,23.9624040861433,121.911839822886)) ;
#89714 = CARTESIAN_POINT('Ctrl Pts',(-19.5238406827779,23.972437169009,121.90852668778)) ;
#89715 = CARTESIAN_POINT('Ctrl Pts',(-19.7836670395102,23.9824588542845,121.951641266166)) ;
#89716 = CARTESIAN_POINT('Ctrl Pts',(-20.0283217952903,23.992325549383,122.037454405699)) ;
#89717 = CARTESIAN_POINT('Ctrl Pts',(-20.256860421925,24.0022854391175,122.165053725248)) ;
#89718 = CARTESIAN_POINT('Ctrl Pts',(-20.4610242017121,24.012320426943,122.331938946934)) ;
#89719 = CARTESIAN_POINT('Ctrl Pts',(-20.6309297767146,24.0222071310173,122.528544653014)) ;
#89720 = CARTESIAN_POINT('Ctrl Pts',(-20.7664224941324,24.0322722752502,122.755656874661)) ;
#89721 = CARTESIAN_POINT('Ctrl Pts',(-20.858590344017,24.0421115659788,122.997281659938)) ;
#89722 = CARTESIAN_POINT('Ctrl Pts',(-20.9088537868088,24.0521741234172,123.256862342196)) ;
#89723 = CARTESIAN_POINT('Ctrl Pts',(-20.9129308819633,24.0620711746693,123.516929777868)) ;
#89724 = CARTESIAN_POINT('Ctrl Pts',(-20.8725108015801,24.0720023814176,123.77475646931)) ;
#89725 = CARTESIAN_POINT('Ctrl Pts',(-20.7867177695425,24.0820445656364,124.024315773816)) ;
#89726 = CARTESIAN_POINT('Ctrl Pts',(-20.661034087862,24.0919311937473,124.251717624557)) ;
#89727 = CARTESIAN_POINT('Ctrl Pts',(-20.4963706306924,24.1019244662797,124.456275571947)) ;
#89728 = CARTESIAN_POINT('Ctrl Pts',(-20.2995736659004,24.1118695418212,124.628245533589)) ;
#89729 = CARTESIAN_POINT('Ctrl Pts',(-20.0760604743478,24.1218190925494,124.763934584824)) ;
#89730 = CARTESIAN_POINT('Ctrl Pts',(-19.8301158593886,24.1318584273974,124.859366095419)) ;
#89731 = CARTESIAN_POINT('Ctrl Pts',(-19.5752990612999,24.1417445663413,124.910102290642)) ;
#89732 = CARTESIAN_POINT('Ctrl Pts',(-19.3126616551709,24.151742679315,124.916221608112)) ;
#89733 = CARTESIAN_POINT('Ctrl Pts',(-19.0549019437606,24.1616624416675,124.877102085613)) ;
#89734 = CARTESIAN_POINT('Ctrl Pts',(-18.8048861129423,24.1717018372801,124.792908728752)) ;
#89735 = CARTESIAN_POINT('Ctrl Pts',(-18.5763150218767,24.1816110230684,124.668144211837)) ;
#89736 = CARTESIAN_POINT('Ctrl Pts',(-18.3718886839389,24.1915462072259,124.50573368631)) ;
#89737 = CARTESIAN_POINT('Ctrl Pts',(-18.1971228535137,24.2015872646118,124.308047316945)) ;
#89738 = CARTESIAN_POINT('Ctrl Pts',(-18.0612783306157,24.2114744226451,124.086547050275)) ;
#89739 = CARTESIAN_POINT('Ctrl Pts',(-17.9645493227509,24.221466702321,123.842445202394)) ;
#89740 = CARTESIAN_POINT('Ctrl Pts',(-17.9119696693637,24.2314152193661,123.586335183678)) ;
#89741 = CARTESIAN_POINT('Ctrl Pts',(-17.9042989976674,24.2413519969365,123.325341447214)) ;
#89742 = CARTESIAN_POINT('Ctrl Pts',(-17.9419176299516,24.2513350330834,123.06567537359)) ;
#89743 = CARTESIAN_POINT('Ctrl Pts',(-18.0249900888699,24.2613787846771,122.815181470846)) ;
#89744 = CARTESIAN_POINT('Ctrl Pts',(-18.1471098273281,24.2712073138897,122.587547692865)) ;
#89745 = CARTESIAN_POINT('Ctrl Pts',(-18.3107425634225,24.2812826747984,122.379462252064)) ;
#89746 = CARTESIAN_POINT('Ctrl Pts',(-18.5037560854593,24.2911392736856,122.206642338797)) ;
#89747 = CARTESIAN_POINT('Ctrl Pts',(-18.7282169843324,24.3012022677035,122.066922869341)) ;
#89748 = CARTESIAN_POINT('Ctrl Pts',(-18.9691137819942,24.311080201993,121.970094344382)) ;
#89749 = CARTESIAN_POINT('Ctrl Pts',(-19.2261436370484,24.321080849551,121.915522158594)) ;
#89750 = CARTESIAN_POINT('Ctrl Pts',(-19.4866572465794,24.3309986959891,121.906283510334)) ;
#89751 = CARTESIAN_POINT('Ctrl Pts',(-19.7481874126353,24.3410498129947,121.942965407598)) ;
#89752 = CARTESIAN_POINT('Ctrl Pts',(-19.995044655726,24.3509205483053,122.022786909086)) ;
#89753 = CARTESIAN_POINT('Ctrl Pts',(-20.2288798534327,24.3609912555483,122.146628302463)) ;
#89754 = CARTESIAN_POINT('Ctrl Pts',(-20.4328576975085,24.3708242630002,122.305301061164)) ;
#89755 = CARTESIAN_POINT('Ctrl Pts',(-20.6102013492879,24.3808547553025,122.500299127757)) ;
#89756 = CARTESIAN_POINT('Ctrl Pts',(-20.7503713756113,24.3908863503759,122.723582642861)) ;
#89757 = CARTESIAN_POINT('Ctrl Pts',(-20.8481322685785,24.4007160495141,122.962664906748)) ;
#89758 = CARTESIAN_POINT('Ctrl Pts',(-20.9045567151015,24.4107054993957,123.219049565126)) ;
#89759 = CARTESIAN_POINT('Ctrl Pts',(-20.9149976124652,24.4207493572114,123.482781782384)) ;
#89760 = CARTESIAN_POINT('Ctrl Pts',(-20.8808031916903,24.4305710478016,123.738611883266)) ;
#89761 = CARTESIAN_POINT('Ctrl Pts',(-20.8016222714478,24.440606138342,123.990150687533)) ;
#89762 = CARTESIAN_POINT('Ctrl Pts',(-20.6794652177334,24.4506306573247,124.223569827565)) ;
#89763 = CARTESIAN_POINT('Ctrl Pts',(-20.5216485278088,24.4604905027349,124.429046599541)) ;
#89764 = CARTESIAN_POINT('Ctrl Pts',(-20.3290856748974,24.4704502790506,124.60632034406)) ;
#89765 = CARTESIAN_POINT('Ctrl Pts',(-20.1069640189552,24.4804784763652,124.748123595379)) ;
#89766 = CARTESIAN_POINT('Ctrl Pts',(-19.8666180274097,24.4903860186555,124.848283735091)) ;
#89767 = CARTESIAN_POINT('Ctrl Pts',(-19.6093832914182,24.5004186692194,124.905987754454)) ;
#89768 = CARTESIAN_POINT('Ctrl Pts',(-19.3499154760575,24.510302625646,124.918048718704)) ;
#89769 = CARTESIAN_POINT('Ctrl Pts',(-19.0894596086663,24.5202923270079,124.885168267668)) ;
#89770 = CARTESIAN_POINT('Ctrl Pts',(-18.8375518685682,24.5303333222839,124.806629416254)) ;
#89771 = CARTESIAN_POINT('Ctrl Pts',(-18.607775073596,24.5401662115523,124.688434190657)) ;
#89772 = CARTESIAN_POINT('Ctrl Pts',(-18.3982021069512,24.5501593699197,124.530191196066)) ;
#89773 = CARTESIAN_POINT('Ctrl Pts',(-18.2189836852721,24.5601914122718,124.336829304906)) ;
#89774 = CARTESIAN_POINT('Ctrl Pts',(-18.0781826899015,24.5700566562302,124.119164288488)) ;
#89775 = CARTESIAN_POINT('Ctrl Pts',(-17.9756353809418,24.5800185474762,123.878288988731)) ;
#89776 = CARTESIAN_POINT('Ctrl Pts',(-17.9164583703033,24.5900534474947,123.621321390185)) ;
#89777 = CARTESIAN_POINT('Ctrl Pts',(-17.9025709875067,24.5999385279093,123.361889607157)) ;
#89778 = CARTESIAN_POINT('Ctrl Pts',(-17.9345306575501,24.6100037000341,123.0993606842)) ;
#89779 = CARTESIAN_POINT('Ctrl Pts',(-18.009793838017,24.6198509347576,122.851745183802)) ;
#89780 = CARTESIAN_POINT('Ctrl Pts',(-18.1285188816227,24.6298817460754,122.616416570995)) ;
#89781 = CARTESIAN_POINT('Ctrl Pts',(-18.2864282941797,24.6398913619889,122.406008126817)) ;
#89782 = CARTESIAN_POINT('Ctrl Pts',(-18.4763620674248,24.6498021413926,122.227839272266)) ;
#89783 = CARTESIAN_POINT('Ctrl Pts',(-18.6944258490363,24.6597314071816,122.084521998851)) ;
#89784 = CARTESIAN_POINT('Ctrl Pts',(-18.9368657879906,24.6697741004942,121.980279706775)) ;
#89785 = CARTESIAN_POINT('Ctrl Pts',(-19.1897153085028,24.679660633189,121.92048694765)) ;
#89786 = CARTESIAN_POINT('Ctrl Pts',(-19.4518476983688,24.6896537782922,121.904901247144)) ;
#89787 = CARTESIAN_POINT('Ctrl Pts',(-19.7114689211226,24.6995994589663,121.935024786244)) ;
#89788 = CARTESIAN_POINT('Ctrl Pts',(-19.9621203216531,24.709546716593,122.009272431099)) ;
#89789 = CARTESIAN_POINT('Ctrl Pts',(-20.1982874731001,24.7195946187145,122.127349372162)) ;
#89790 = CARTESIAN_POINT('Ctrl Pts',(-20.4062771468984,24.7294423243362,122.281336350192)) ;
#89791 = CARTESIAN_POINT('Ctrl Pts',(-20.5870191315301,24.7394037909703,122.470689270979)) ;
#89792 = CARTESIAN_POINT('Ctrl Pts',(-20.7328443334499,24.7494333442385,122.690250749449)) ;
#89793 = CARTESIAN_POINT('Ctrl Pts',(-20.8371756815299,24.7593402362659,122.928777696645)) ;
#89794 = CARTESIAN_POINT('Ctrl Pts',(-20.8992448149416,24.7692878803789,123.182694125672)) ;
#89795 = CARTESIAN_POINT('Ctrl Pts',(-20.9165397755815,24.7792879234078,123.444949438803)) ;
#89796 = CARTESIAN_POINT('Ctrl Pts',(-20.8874649816599,24.7893266894018,123.707130191398)) ;
#89797 = CARTESIAN_POINT('Ctrl Pts',(-20.8154023193973,24.7991517514241,123.955080646736)) ;
#89798 = CARTESIAN_POINT('Ctrl Pts',(-20.6991263352566,24.8092062987504,124.192325406435)) ;
#89799 = CARTESIAN_POINT('Ctrl Pts',(-20.5447671392046,24.8191495421996,124.403167472963)) ;
#89800 = CARTESIAN_POINT('Ctrl Pts',(-20.3574869860895,24.8290517138075,124.58383784483)) ;
#89801 = CARTESIAN_POINT('Ctrl Pts',(-20.1383185841272,24.8391045494177,124.731315017245)) ;
#89802 = CARTESIAN_POINT('Ctrl Pts',(-19.901213310372,24.8489776071032,124.836683877999)) ;
#89803 = CARTESIAN_POINT('Ctrl Pts',(-19.646468082972,24.8589728686289,124.900684701347)) ;
#89804 = CARTESIAN_POINT('Ctrl Pts',(-19.3836496123046,24.8689982380494,124.919067997293)) ;
#89805 = CARTESIAN_POINT('Ctrl Pts',(-19.1251299071319,24.878888070576,124.892249885578)) ;
#89806 = CARTESIAN_POINT('Ctrl Pts',(-18.7890091715742,24.8921860413854,124.796799294934)) ;
#89807 = CARTESIAN_POINT('Ctrl Pts',(-18.4874128569439,24.9053844364946,124.617566260999)) ;
#89808 = CARTESIAN_POINT('Ctrl Pts',(-18.2417575404836,24.918779878774,124.365456812483)) ;
#89809 = CARTESIAN_POINT('Ctrl Pts',(-18.0954573193109,24.928655717013,124.151048711038)) ;
#89810 = CARTESIAN_POINT('Ctrl Pts',(-17.9865203150819,24.9387171196107,123.910175250881)) ;
#89811 = CARTESIAN_POINT('Ctrl Pts',(-17.9222460999715,24.9485821765459,123.658987057165)) ;
#89812 = CARTESIAN_POINT('Ctrl Pts',(-17.9018079283208,24.9585942724947,123.396707820689)) ;
#89813 = CARTESIAN_POINT('Ctrl Pts',(-17.9355686586318,24.9718715816401,123.049393446101)) ;
#89814 = CARTESIAN_POINT('Ctrl Pts',(-18.0899475407356,24.9884706071474,122.636126991343)) ;
#89815 = CARTESIAN_POINT('Ctrl Pts',(-18.3760314708444,25.0050696551804,122.300327989926)) ;
#89816 = CARTESIAN_POINT('Ctrl Pts',(-18.6623187112641,25.0183130672114,122.102384463216)) ;
#89817 = CARTESIAN_POINT('Ctrl Pts',(-18.9019733035102,25.0283504948998,121.992225850964)) ;
#89818 = CARTESIAN_POINT('Ctrl Pts',(-19.1537567559459,25.0382547968554,121.926273908146)) ;
#89819 = CARTESIAN_POINT('Ctrl Pts',(-19.5011724762164,25.0515216368306,121.896923152544)) ;
#89820 = CARTESIAN_POINT('Ctrl Pts',(-19.9361209211562,25.0681478349205,121.974892242463)) ;
#89821 = CARTESIAN_POINT('Ctrl Pts',(-20.3941483506745,25.0880669503039,122.240432926128)) ;
#89822 = CARTESIAN_POINT('Ctrl Pts',(-20.6778013141646,25.1046733734382,122.578575786354)) ;
#89823 = CARTESIAN_POINT('Ctrl Pts',(-20.8254198064288,25.1179695939339,122.895276836921)) ;
#89824 = CARTESIAN_POINT('Ctrl Pts',(-20.9163896664301,25.1312384262753,123.231970672834)) ;
#89825 = CARTESIAN_POINT('Ctrl Pts',(-20.9167689419944,25.1479296743084,123.675492638632)) ;
#89826 = CARTESIAN_POINT('Ctrl Pts',(-20.7380584204792,25.1677394059812,124.170815449789)) ;
#89827 = CARTESIAN_POINT('Ctrl Pts',(-20.3990544179289,25.1877170133098,124.579453442232)) ;
#89828 = CARTESIAN_POINT('Ctrl Pts',(-19.9416756734989,25.2076433223676,124.846325842365)) ;
#89829 = CARTESIAN_POINT('Ctrl Pts',(-19.4236779184025,25.2274601825323,124.942437107342)) ;
#89830 = CARTESIAN_POINT('Ctrl Pts',(-18.8970108487145,25.2475599981263,124.854014090052)) ;
#89831 = CARTESIAN_POINT('Ctrl Pts',(-18.4395915110761,25.2673169620089,124.595686505518)) ;
#89832 = CARTESIAN_POINT('Ctrl Pts',(-18.0924071157132,25.2873538880783,124.192105333411)) ;
#89833 = CARTESIAN_POINT('Ctrl Pts',(-17.9060265000467,25.3072234704598,123.697842908581)) ;
#89834 = CARTESIAN_POINT('Ctrl Pts',(-17.8981566895004,25.327128042213,123.168973851605)) ;
#89835 = CARTESIAN_POINT('Ctrl Pts',(-18.0717642136479,25.3470806444115,122.667793933237)) ;
#89836 = CARTESIAN_POINT('Ctrl Pts',(-18.4052645219479,25.3669901353818,122.257095727428)) ;
#89837 = CARTESIAN_POINT('Ctrl Pts',(-18.8570067132281,25.3868415040812,121.984255857802)) ;
#89838 = CARTESIAN_POINT('Ctrl Pts',(-19.3806239056403,25.4069217002172,121.881586989434)) ;
#89839 = CARTESIAN_POINT('Ctrl Pts',(-19.9007576230194,25.4267226437926,121.962652492736)) ;
#89840 = CARTESIAN_POINT('Ctrl Pts',(-20.3666506513675,25.4467066203021,122.217535832542)) ;
#89841 = CARTESIAN_POINT('Ctrl Pts',(-20.7158407306792,25.4666225832777,122.615352102572)) ;
#89842 = CARTESIAN_POINT('Ctrl Pts',(-20.9092753913654,25.4864930180996,123.10688621769)) ;
#89843 = CARTESIAN_POINT('Ctrl Pts',(-20.9225933282135,25.5065433033327,123.63946964645)) ;
#89844 = CARTESIAN_POINT('Ctrl Pts',(-20.7563011574428,25.526317272092,124.138248789555)) ;
#89845 = CARTESIAN_POINT('Ctrl Pts',(-20.4256737839772,25.5463737302116,124.55612392467)) ;
#89846 = CARTESIAN_POINT('Ctrl Pts',(-19.9778044990182,25.5661686132026,124.832472781124)) ;
#89847 = CARTESIAN_POINT('Ctrl Pts',(-19.4586089000129,25.5861352685049,124.941740459474)) ;
#89848 = CARTESIAN_POINT('Ctrl Pts',(-18.933405433002,25.6060942385814,124.866405585267)) ;
#89849 = CARTESIAN_POINT('Ctrl Pts',(-18.4668441914665,25.6259903261715,124.617555781116)) ;
#89850 = CARTESIAN_POINT('Ctrl Pts',(-18.1127144201242,25.6458884960831,124.224823959823)) ;
#89851 = CARTESIAN_POINT('Ctrl Pts',(-17.9132301741929,25.6657943314502,123.734766837906)) ;
#89852 = CARTESIAN_POINT('Ctrl Pts',(-17.8929228695584,25.6857442563881,123.204966867725)) ;
#89853 = CARTESIAN_POINT('Ctrl Pts',(-18.0536111401075,25.7056234462985,122.701580140501)) ;
#89854 = CARTESIAN_POINT('Ctrl Pts',(-18.377808589848,25.7256047705791,122.281003832198)) ;
#89855 = CARTESIAN_POINT('Ctrl Pts',(-18.8251899843192,25.7455345547874,121.99718762822)) ;
#89856 = CARTESIAN_POINT('Ctrl Pts',(-19.3420583616094,25.7654545441782,121.883074058097)) ;
#89857 = CARTESIAN_POINT('Ctrl Pts',(-19.8655398108464,25.7853097395322,121.95081448643)) ;
#89858 = CARTESIAN_POINT('Ctrl Pts',(-20.3385236962934,25.8053557411916,122.195787304325)) ;
#89859 = CARTESIAN_POINT('Ctrl Pts',(-20.6359551620709,25.8218554884014,122.518224212841)) ;
#89860 = CARTESIAN_POINT('Ctrl Pts',(-20.7997772299296,25.8352440928495,122.829543405343)) ;
#89861 = CARTESIAN_POINT('Ctrl Pts',(-20.878806089281,25.8451059211844,123.076370301885)) ;
#89862 = CARTESIAN_POINT('Ctrl Pts',(-20.9149660822381,25.855072063942,123.335767898469)) ;
#89863 = CARTESIAN_POINT('Ctrl Pts',(-20.901681357157,25.8684338100669,123.686592876107)) ;
#89864 = CARTESIAN_POINT('Ctrl Pts',(-20.7738066717889,25.884888139022,124.104963749759)) ;
#89865 = CARTESIAN_POINT('Ctrl Pts',(-20.5060796437535,25.9016553840703,124.461005538212)) ;
#89866 = CARTESIAN_POINT('Ctrl Pts',(-20.2328324341928,25.9148419493443,124.674328351222)) ;
#89867 = CARTESIAN_POINT('Ctrl Pts',(-20.0014412245227,25.9248314080889,124.798165745444)) ;
#89868 = CARTESIAN_POINT('Ctrl Pts',(-19.7528536304337,25.93478518057,124.879736163845)) ;
#89869 = CARTESIAN_POINT('Ctrl Pts',(-19.4914876961368,25.9448329971027,124.917038232705)) ;
#89870 = CARTESIAN_POINT('Ctrl Pts',(-19.2329656958291,25.9546745302252,124.908870993837)) ;
#89871 = CARTESIAN_POINT('Ctrl Pts',(-18.9760196741983,25.9646607724449,124.85572458636)) ;
#89872 = CARTESIAN_POINT('Ctrl Pts',(-18.7332872577401,25.9745973958698,124.759342505799)) ;
#89873 = CARTESIAN_POINT('Ctrl Pts',(-18.5085731788918,25.9846472732528,124.620640269178)) ;
#89874 = CARTESIAN_POINT('Ctrl Pts',(-18.3151059732975,25.9944977120304,124.448627307497)) ;
#89875 = CARTESIAN_POINT('Ctrl Pts',(-18.1519582512238,26.0044697259991,124.243595958302)) ;
#89876 = CARTESIAN_POINT('Ctrl Pts',(-18.0265942662714,26.0144648946252,124.012733796054)) ;
#89877 = CARTESIAN_POINT('Ctrl Pts',(-17.94321575523,26.0244987778864,123.762605317723)) ;
#89878 = CARTESIAN_POINT('Ctrl Pts',(-17.9048256332287,26.0343546479497,123.506445495096)) ;
#89879 = CARTESIAN_POINT('Ctrl Pts',(-17.9111726656182,26.0443521938669,123.243825664362)) ;
#89880 = CARTESIAN_POINT('Ctrl Pts',(-17.9624847437566,26.0542603207662,122.988545851874)) ;
#89881 = CARTESIAN_POINT('Ctrl Pts',(-18.0578964910856,26.0642706922883,122.743382417585)) ;
#89882 = CARTESIAN_POINT('Ctrl Pts',(-18.195192673543,26.0743011350357,122.518384012855)) ;
#89883 = CARTESIAN_POINT('Ctrl Pts',(-18.3658649539483,26.084149087589,122.323819765035)) ;
#89884 = CARTESIAN_POINT('Ctrl Pts',(-18.5719645952938,26.09421175661,122.158181340976)) ;
#89885 = CARTESIAN_POINT('Ctrl Pts',(-18.7999511759967,26.1041061320739,122.033112687758)) ;
#89886 = CARTESIAN_POINT('Ctrl Pts',(-19.0470918391407,26.1140479303921,121.948484295276)) ;
#89887 = CARTESIAN_POINT('Ctrl Pts',(-19.3067989983835,26.1240504241194,121.907695937297)) ;
#89888 = CARTESIAN_POINT('Ctrl Pts',(-19.5704318398782,26.1340852226263,121.913051573615)) ;
#89889 = CARTESIAN_POINT('Ctrl Pts',(-19.824351246944,26.1439301066057,121.9627151315)) ;
#89890 = CARTESIAN_POINT('Ctrl Pts',(-20.0693695516345,26.1539159634237,122.056561537333)) ;
#89891 = CARTESIAN_POINT('Ctrl Pts',(-20.2933941815534,26.1638507775985,122.19072291664)) ;
#89892 = CARTESIAN_POINT('Ctrl Pts',(-20.4929379375906,26.1739082773838,122.36397713695)) ;
#89893 = CARTESIAN_POINT('Ctrl Pts',(-20.6558144439717,26.1837300358021,122.564237995494)) ;
#89894 = CARTESIAN_POINT('Ctrl Pts',(-20.7848455998996,26.1937856935861,122.79482096552)) ;
#89895 = CARTESIAN_POINT('Ctrl Pts',(-20.8704620781849,26.2037278757661,123.041679298249)) ;
#89896 = CARTESIAN_POINT('Ctrl Pts',(-20.9125411179837,26.2136330844608,123.298550407497)) ;
#89897 = CARTESIAN_POINT('Ctrl Pts',(-20.9092518862155,26.2236748754233,123.56241297677)) ;
#89898 = CARTESIAN_POINT('Ctrl Pts',(-20.8608770737848,26.2335826498955,123.81825615933)) ;
#89899 = CARTESIAN_POINT('Ctrl Pts',(-20.7683065805399,26.2435941501231,124.064531536108)) ;
#89900 = CARTESIAN_POINT('Ctrl Pts',(-20.6336276204181,26.2536269105158,124.291186385178)) ;
#89901 = CARTESIAN_POINT('Ctrl Pts',(-20.4651029134243,26.2634774796507,124.487687379059)) ;
#89902 = CARTESIAN_POINT('Ctrl Pts',(-20.2625522855935,26.2734660891806,124.654609276642)) ;
#89903 = CARTESIAN_POINT('Ctrl Pts',(-20.0354400287525,26.2833947452047,124.783063120699)) ;
#89904 = CARTESIAN_POINT('Ctrl Pts',(-19.7881531187985,26.2933824913825,124.871070996956)) ;
#89905 = CARTESIAN_POINT('Ctrl Pts',(-19.5280420904567,26.3034184803182,124.914573869556)) ;
#89906 = CARTESIAN_POINT('Ctrl Pts',(-19.2690516259357,26.3132733501318,124.912723418728)) ;
#89907 = CARTESIAN_POINT('Ctrl Pts',(-19.0105800370941,26.3232727913736,124.86560866309)) ;
#89908 = CARTESIAN_POINT('Ctrl Pts',(-18.7666075707734,26.3331678655537,124.775514885921)) ;
#89909 = CARTESIAN_POINT('Ctrl Pts',(-18.5383077888514,26.3432285213934,124.642249303302)) ;
#89910 = CARTESIAN_POINT('Ctrl Pts',(-18.3407235540066,26.353077395589,124.475043878373)) ;
#89911 = CARTESIAN_POINT('Ctrl Pts',(-18.1716552019844,26.3631061075523,124.272882308973)) ;
#89912 = CARTESIAN_POINT('Ctrl Pts',(-18.040865209082,26.3731355081354,124.044055902173)) ;
#89913 = CARTESIAN_POINT('Ctrl Pts',(-17.9529323432651,26.3829757017522,123.800871133778)) ;
#89914 = CARTESIAN_POINT('Ctrl Pts',(-17.907349688925,26.3929791243274,123.542000520602)) ;
#89915 = CARTESIAN_POINT('Ctrl Pts',(-17.9074933099312,26.4029646614205,123.279546917314)) ;
#89916 = CARTESIAN_POINT('Ctrl Pts',(-17.9537071122485,26.4130056659073,123.019784028195)) ;
#89917 = CARTESIAN_POINT('Ctrl Pts',(-18.0422247319121,26.4228492048485,122.776701044052)) ;
#89918 = CARTESIAN_POINT('Ctrl Pts',(-18.172959280111,26.4328342358393,122.549236855608)) ;
#89919 = CARTESIAN_POINT('Ctrl Pts',(-18.3404039267093,26.4427736983613,122.348721052526)) ;
#89920 = CARTESIAN_POINT('Ctrl Pts',(-18.5421292540438,26.4528134305851,122.17870944488)) ;
#89921 = CARTESIAN_POINT('Ctrl Pts',(-18.7668321702435,26.4627016109023,122.048175439295)) ;
#89922 = CARTESIAN_POINT('Ctrl Pts',(-19.0130942013059,26.4726911266048,121.957267850095)) ;
#89923 = CARTESIAN_POINT('Ctrl Pts',(-19.270636423452,26.4826496772595,121.910844672131)) ;
#89924 = CARTESIAN_POINT('Ctrl Pts',(-19.5307953770956,26.4925490843645,121.909202223713)) ;
#89925 = CARTESIAN_POINT('Ctrl Pts',(-19.7910846414141,26.5025976707808,121.953512811704)) ;
#89926 = CARTESIAN_POINT('Ctrl Pts',(-20.0360368235489,26.5124904897453,122.040759031323)) ;
#89927 = CARTESIAN_POINT('Ctrl Pts',(-20.2660528706653,26.5225616072751,122.171557281645)) ;
#89928 = CARTESIAN_POINT('Ctrl Pts',(-20.4649953247139,26.5323773012411,122.335824675937)) ;
#89929 = CARTESIAN_POINT('Ctrl Pts',(-20.6368891208767,26.5424436787384,122.536824123293)) ;
#89930 = CARTESIAN_POINT('Ctrl Pts',(-20.7690314537872,26.5523426648203,122.760972791709)) ;
#89931 = CARTESIAN_POINT('Ctrl Pts',(-20.8617289021231,26.5623968448138,123.008329329804)) ;
#89932 = CARTESIAN_POINT('Ctrl Pts',(-20.9094601027412,26.5722676577465,123.263357508459)) ;
#89933 = CARTESIAN_POINT('Ctrl Pts',(-20.9122321988059,26.5823415586003,123.528012047214)) ;
#89934 = CARTESIAN_POINT('Ctrl Pts',(-20.8703917027367,26.592161713987,123.782723049251)) ;
#89935 = CARTESIAN_POINT('Ctrl Pts',(-20.7829899901851,26.6022404209392,124.032674888992)) ;
#89936 = CARTESIAN_POINT('Ctrl Pts',(-20.6564493553006,26.612092009478,124.25860286663)) ;
#89937 = CARTESIAN_POINT('Ctrl Pts',(-20.4891684822601,26.622165126003,124.463697321808)) ;
#89938 = CARTESIAN_POINT('Ctrl Pts',(-20.293323576881,26.6320076430988,124.632686826274)) ;
#89939 = CARTESIAN_POINT('Ctrl Pts',(-20.0684805251643,26.6419881046528,124.76769750117)) ;
#89940 = CARTESIAN_POINT('Ctrl Pts',(-19.8224939925488,26.6520063546435,124.861502416363)) ;
#89941 = CARTESIAN_POINT('Ctrl Pts',(-19.5674893463834,26.6618905148373,124.91103746618)) ;
#89942 = CARTESIAN_POINT('Ctrl Pts',(-19.3030567708649,26.6719556618123,124.915566855908)) ;
#89943 = CARTESIAN_POINT('Ctrl Pts',(-19.0475793987206,26.6817974854531,124.875168472208)) ;
#89944 = CARTESIAN_POINT('Ctrl Pts',(-18.7981276860572,26.6918269579139,124.79009847604)) ;
#89945 = CARTESIAN_POINT('Ctrl Pts',(-18.5676426643981,26.701853813176,124.662390118096)) ;
#89946 = CARTESIAN_POINT('Ctrl Pts',(-18.3661950342201,26.7116970632865,124.500120225689)) ;
#89947 = CARTESIAN_POINT('Ctrl Pts',(-18.1921722448789,26.7217455028697,124.301522698417)) ;
#89948 = CARTESIAN_POINT('Ctrl Pts',(-18.0569733160775,26.7316949971176,124.077726969622)) ;
#89949 = CARTESIAN_POINT('Ctrl Pts',(-17.9623479206744,26.7416028528436,123.835146450497)) ;
#89950 = CARTESIAN_POINT('Ctrl Pts',(-17.9107817759331,26.7516623294935,123.57590066682)) ;
#89951 = CARTESIAN_POINT('Ctrl Pts',(-17.9047865023787,26.7615031389022,123.317331030199)) ;
#89952 = CARTESIAN_POINT('Ctrl Pts',(-17.9443188755689,26.771565289203,123.055908426171)) ;
#89953 = CARTESIAN_POINT('Ctrl Pts',(-18.0275281430875,26.7814624503255,122.809476370172)) ;
#89954 = CARTESIAN_POINT('Ctrl Pts',(-18.1519197086005,26.7913936247296,122.580053321706)) ;
#89955 = CARTESIAN_POINT('Ctrl Pts',(-18.3162992678989,26.8014358284546,122.373607725889)) ;
#89956 = CARTESIAN_POINT('Ctrl Pts',(-18.5108502149347,26.8113224108851,122.201394321902)) ;
#89957 = CARTESIAN_POINT('Ctrl Pts',(-18.7344911406208,26.8213158466334,122.063754577682)) ;
#89958 = CARTESIAN_POINT('Ctrl Pts',(-18.9774833859817,26.8312603149915,121.96757970157)) ;
#89959 = CARTESIAN_POINT('Ctrl Pts',(-19.2335820350933,26.8412121312371,121.91453316318)) ;
#89960 = CARTESIAN_POINT('Ctrl Pts',(-19.4972322377189,26.8512495673516,121.906934424089)) ;
#89961 = CARTESIAN_POINT('Ctrl Pts',(-19.754305398308,26.8611345265279,121.944403815041)) ;
#89962 = CARTESIAN_POINT('Ctrl Pts',(-20.0038371906887,26.8711326447399,122.026561032475)) ;
#89963 = CARTESIAN_POINT('Ctrl Pts',(-20.2336644999362,26.8810535772519,122.149706995992)) ;
#89964 = CARTESIAN_POINT('Ctrl Pts',(-20.4411151613036,26.8910948774739,122.312763749208)) ;
#89965 = CARTESIAN_POINT('Ctrl Pts',(-20.6146912031061,26.9010017958639,122.506803957199)) ;
#89966 = CARTESIAN_POINT('Ctrl Pts',(-20.7529734778652,26.910937587573,122.728283521879)) ;
#89967 = CARTESIAN_POINT('Ctrl Pts',(-20.8514823737436,26.9209784821509,122.973063068783)) ;
#89968 = CARTESIAN_POINT('Ctrl Pts',(-20.9053481968387,26.9308656838647,123.227257943129)) ;
#89969 = CARTESIAN_POINT('Ctrl Pts',(-20.9147883410893,26.9408579516263,123.489656489309)) ;
#89970 = CARTESIAN_POINT('Ctrl Pts',(-20.8786067103794,26.9508064726481,123.74859249786)) ;
#89971 = CARTESIAN_POINT('Ctrl Pts',(-20.7984720557952,26.9607432462258,123.997098137103)) ;
#89972 = CARTESIAN_POINT('Ctrl Pts',(-20.676104628499,26.9707262943668,124.229192313943)) ;
#89973 = CARTESIAN_POINT('Ctrl Pts',(-20.5139774785616,26.9807700019769,124.437430943901)) ;
#89974 = CARTESIAN_POINT('Ctrl Pts',(-20.3227007873807,26.9905986951302,124.61104899263)) ;
#89975 = CARTESIAN_POINT('Ctrl Pts',(-20.0988745919875,27.0006734442596,124.75238354413)) ;
#89976 = CARTESIAN_POINT('Ctrl Pts',(-19.8589158285045,27.0105387700552,124.850593645606)) ;
#89977 = CARTESIAN_POINT('Ctrl Pts',(-19.6017027315997,27.0205609444121,124.907173107382)) ;
#89978 = CARTESIAN_POINT('Ctrl Pts',(-19.3384167298905,27.030586997619,124.917590734457)) ;
#89979 = CARTESIAN_POINT('Ctrl Pts',(-19.0817902884042,27.0404406944653,124.883165473566)) ;
#89980 = CARTESIAN_POINT('Ctrl Pts',(-18.8321269948554,27.0504000992183,124.804605397786)) ;
#89981 = CARTESIAN_POINT('Ctrl Pts',(-18.5982965329107,27.0604383449232,124.682527849518)) ;
#89982 = CARTESIAN_POINT('Ctrl Pts',(-18.3923088563404,27.0703125290852,124.524671749467)) ;
#89983 = CARTESIAN_POINT('Ctrl Pts',(-18.213440473293,27.0803823122231,124.329704461917)) ;
#89984 = CARTESIAN_POINT('Ctrl Pts',(-18.074335807759,27.0902155672439,124.111906520483)) ;
#89985 = CARTESIAN_POINT('Ctrl Pts',(-17.9724962914812,27.1002459933756,123.868794804679)) ;
#89986 = CARTESIAN_POINT('Ctrl Pts',(-17.9151518381184,27.1102776055626,123.61147237248)) ;
#89987 = CARTESIAN_POINT('Ctrl Pts',(-17.9030590057314,27.1201073024172,123.353458137196)) ;
#89988 = CARTESIAN_POINT('Ctrl Pts',(-17.9357095844985,27.1300967443197,123.092976875081)) ;
#89989 = CARTESIAN_POINT('Ctrl Pts',(-18.0141505189305,27.1401406363354,122.840961680301)) ;
#89990 = CARTESIAN_POINT('Ctrl Pts',(-18.1320070501894,27.1499621981046,122.611342543819)) ;
#89991 = CARTESIAN_POINT('Ctrl Pts',(-18.2908176421164,27.1599977697288,122.400792255072)) ;
#89992 = CARTESIAN_POINT('Ctrl Pts',(-18.4841896216697,27.1700270440106,122.221709205105)) ;
#89993 = CARTESIAN_POINT('Ctrl Pts',(-18.7010325739723,27.1798608811293,122.08111845669)) ;
#89994 = CARTESIAN_POINT('Ctrl Pts',(-18.9441365822861,27.1899132772174,121.97778844473)) ;
#89995 = CARTESIAN_POINT('Ctrl Pts',(-19.1986307271689,27.1998500441679,121.919247113411)) ;
#89996 = CARTESIAN_POINT('Ctrl Pts',(-19.4593067664465,27.2097842791472,121.905113637741)) ;
#89997 = CARTESIAN_POINT('Ctrl Pts',(-19.7207933748905,27.219808042474,121.936899749053)) ;
#89998 = CARTESIAN_POINT('Ctrl Pts',(-19.9693907811413,27.2296943838587,122.012371578883)) ;
#89999 = CARTESIAN_POINT('Ctrl Pts',(-20.2037993675098,27.2396834326256,122.130541837784)) ;
#90000 = CARTESIAN_POINT('Ctrl Pts',(-20.4148911017479,27.249724653323,122.288871926613)) ;
#90001 = CARTESIAN_POINT('Ctrl Pts',(-20.5918449134471,27.2595572935009,122.477157471636)) ;
#90002 = CARTESIAN_POINT('Ctrl Pts',(-20.7363711758217,27.2695512228089,122.696442446085)) ;
#90003 = CARTESIAN_POINT('Ctrl Pts',(-20.8404837011343,27.2795804304894,122.938566164147)) ;
#90004 = CARTESIAN_POINT('Ctrl Pts',(-20.9004632009322,27.2894562421935,123.191081286783)) ;
#90005 = CARTESIAN_POINT('Ctrl Pts',(-20.9161620820543,27.2994554691649,123.453345856358)) ;
#90006 = CARTESIAN_POINT('Ctrl Pts',(-20.8865937388302,27.3093649503206,123.712111167712)) ;
#90007 = CARTESIAN_POINT('Ctrl Pts',(-20.8114565304405,27.3194181806215,123.9653601692)) ;
#90008 = CARTESIAN_POINT('Ctrl Pts',(-20.695723180066,27.3292887971726,124.197519423031)) ;
#90009 = CARTESIAN_POINT('Ctrl Pts',(-20.5395590565441,27.3393104589046,124.409577578881)) ;
#90010 = CARTESIAN_POINT('Ctrl Pts',(-20.3484964827814,27.3493332720857,124.590894769313)) ;
#90011 = CARTESIAN_POINT('Ctrl Pts',(-20.1325252181775,27.3592004365456,124.734373686293)) ;
#90012 = CARTESIAN_POINT('Ctrl Pts',(-19.8921052555751,27.3691938787656,124.840061281651)) ;
#90013 = CARTESIAN_POINT('Ctrl Pts',(-19.6358971489778,27.3792255523659,124.902135847813)) ;
#90014 = CARTESIAN_POINT('Ctrl Pts',(-19.3771491513025,27.3890919874789,124.918905570282)) ;
#90015 = CARTESIAN_POINT('Ctrl Pts',(-19.1162550336676,27.399079438012,124.890574288521)) ;
#90016 = CARTESIAN_POINT('Ctrl Pts',(-18.8652095381394,27.4090243678399,124.817799802531)) ;
#90017 = CARTESIAN_POINT('Ctrl Pts',(-18.6283777604426,27.4190692628951,124.701277213198)) ;
#90018 = CARTESIAN_POINT('Ctrl Pts',(-18.4190826873744,27.4289313245809,124.548398528838)) ;
#90019 = CARTESIAN_POINT('Ctrl Pts',(-18.23679990877,27.4389230473678,124.35943784464)) ;
#90020 = CARTESIAN_POINT('Ctrl Pts',(-18.0910351330655,27.4488552616077,124.142920914045)) ;
#90021 = CARTESIAN_POINT('Ctrl Pts',(-17.9844514742124,27.4587945801734,123.90445397346)) ;
#90022 = CARTESIAN_POINT('Ctrl Pts',(-17.9204596210356,27.4688387549493,123.648382078966)) ;
#90023 = CARTESIAN_POINT('Ctrl Pts',(-17.902082443692,27.4787093090143,123.389646586281)) ;
#90024 = CARTESIAN_POINT('Ctrl Pts',(-17.9284117059881,27.4886742913685,123.129103791897)) ;
#90025 = CARTESIAN_POINT('Ctrl Pts',(-18.0004358375775,27.4987049942583,122.875545886623)) ;
#90026 = CARTESIAN_POINT('Ctrl Pts',(-18.1134828367361,27.5085973342835,122.641417708606)) ;
#90027 = CARTESIAN_POINT('Ctrl Pts',(-18.2678736241984,27.5186505674435,122.427083046342)) ;
#90028 = CARTESIAN_POINT('Ctrl Pts',(-18.4538449647151,27.5285318119202,122.245793517395)) ;
#90029 = CARTESIAN_POINT('Ctrl Pts',(-18.6715808971833,27.5385649327912,122.097192547089)) ;
#90030 = CARTESIAN_POINT('Ctrl Pts',(-18.9081664411668,27.5484461430663,121.990047207349)) ;
#90031 = CARTESIAN_POINT('Ctrl Pts',(-19.1642609051452,27.5585082188356,121.924381854683)) ;
#90032 = CARTESIAN_POINT('Ctrl Pts',(-19.4225664239136,27.5683652772174,121.904494754885)) ;
#90033 = CARTESIAN_POINT('Ctrl Pts',(-19.6839699262157,27.5783598325064,121.929577621368)) ;
#90034 = CARTESIAN_POINT('Ctrl Pts',(-19.9354082337427,27.5882857200419,121.999117799901)) ;
#90035 = CARTESIAN_POINT('Ctrl Pts',(-20.1732877832902,27.5983107400372,122.112287014641)) ;
#90036 = CARTESIAN_POINT('Ctrl Pts',(-20.3852469318587,27.6082081171408,122.263036295737)) ;
#90037 = CARTESIAN_POINT('Ctrl Pts',(-20.5699322318413,27.6181983542217,122.44963382705)) ;
#90038 = CARTESIAN_POINT('Ctrl Pts',(-20.7196829783269,27.6282349670305,122.666746029416)) ;
#90039 = CARTESIAN_POINT('Ctrl Pts',(-20.8278068728803,27.6380848504485,122.901936609501)) ;
#90040 = CARTESIAN_POINT('Ctrl Pts',(-20.8949783481644,27.648088467351,123.156067646929)) ;
#90041 = CARTESIAN_POINT('Ctrl Pts',(-20.9168353812002,27.6580778791161,123.417709468201)) ;
#90042 = CARTESIAN_POINT('Ctrl Pts',(-20.8927038903756,27.6680966404609,123.679858425827)) ;
#90043 = CARTESIAN_POINT('Ctrl Pts',(-20.8017637690144,27.681315315842,124.015169943229)) ;
#90044 = CARTESIAN_POINT('Ctrl Pts',(-20.624397640746,27.6946256230867,124.321149899939)) ;
#90045 = CARTESIAN_POINT('Ctrl Pts',(-20.3779433771167,27.7078632893127,124.566721861766)) ;
#90046 = CARTESIAN_POINT('Ctrl Pts',(-20.1646154796001,27.7177829847234,124.716537787326)) ;
#90047 = CARTESIAN_POINT('Ctrl Pts',(-19.9252314219541,27.727835851722,124.828242513711)) ;
#90048 = CARTESIAN_POINT('Ctrl Pts',(-19.6751407014436,27.7376912600512,124.895632476655)) ;
#90049 = CARTESIAN_POINT('Ctrl Pts',(-19.412428193496,27.7477298917278,124.919430792106)) ;
#90050 = CARTESIAN_POINT('Ctrl Pts',(-19.0641209038591,27.7610320739948,124.889619359484)) ;
#90051 = CARTESIAN_POINT('Ctrl Pts',(-18.6502903905597,27.7775770870777,124.740836279188)) ;
#90052 = CARTESIAN_POINT('Ctrl Pts',(-18.3098859245536,27.7942291031539,124.458090863763)) ;
#90053 = CARTESIAN_POINT('Ctrl Pts',(-18.1090493187269,27.8074521940591,124.17447204272)) ;
#90054 = CARTESIAN_POINT('Ctrl Pts',(-17.9965232918457,27.8174131536185,123.938133979673)) ;
#90055 = CARTESIAN_POINT('Ctrl Pts',(-17.9266087730233,27.8274379503696,123.684145144491)) ;
#90056 = CARTESIAN_POINT('Ctrl Pts',(-17.8934656932994,27.8406623977654,123.338168391895)) ;
#90057 = CARTESIAN_POINT('Ctrl Pts',(-17.9661155358838,27.8572961824645,122.902139051415)) ;
#90058 = CARTESIAN_POINT('Ctrl Pts',(-18.2260073081097,27.8771988491894,122.441354547989)) ;
#90059 = CARTESIAN_POINT('Ctrl Pts',(-18.6269746119238,27.8970990769713,122.096481259438)) ;
#90060 = CARTESIAN_POINT('Ctrl Pts',(-19.1218890723207,27.9170165645028,121.908622605301)) ;
#90061 = CARTESIAN_POINT('Ctrl Pts',(-19.6515477387723,27.9369460903197,121.90059571952)) ;
#90062 = CARTESIAN_POINT('Ctrl Pts',(-20.1529442502027,27.956908358206,122.07417484712)) ;
#90063 = CARTESIAN_POINT('Ctrl Pts',(-20.5634708106491,27.9767985531582,122.407134552226)) ;
#90064 = CARTESIAN_POINT('Ctrl Pts',(-20.8369751729256,27.9966887979044,122.859670241796)) ;
#90065 = CARTESIAN_POINT('Ctrl Pts',(-20.9394668766951,28.0167631704669,123.383205991598)) ;
#90066 = CARTESIAN_POINT('Ctrl Pts',(-20.8584842588624,28.0365485478272,123.902864524186)) ;
#90067 = CARTESIAN_POINT('Ctrl Pts',(-20.6042776799615,28.0565104218943,124.368499119697)) ;
#90068 = CARTESIAN_POINT('Ctrl Pts',(-20.2051858780569,28.0764903973848,124.718841264619)) ;
#90069 = CARTESIAN_POINT('Ctrl Pts',(-19.7150043467851,28.0963028272628,124.911309469325)) ;
#90070 = CARTESIAN_POINT('Ctrl Pts',(-19.1842604378428,28.1162829353531,124.925752106115)) ;
#90071 = CARTESIAN_POINT('Ctrl Pts',(-18.6824773897549,28.1361773189503,124.758643613806)) ;
#90072 = CARTESIAN_POINT('Ctrl Pts',(-18.2670496367191,28.1561042469275,124.430319759425)) ;
#90073 = CARTESIAN_POINT('Ctrl Pts',(-17.9883198062167,28.1759991042288,123.980833693048)) ;
#90074 = CARTESIAN_POINT('Ctrl Pts',(-17.8794805614305,28.1960382978324,123.459516608282)) ;
#90075 = CARTESIAN_POINT('Ctrl Pts',(-17.9544486755063,28.2158782657432,122.937505697659)) ;
#90076 = CARTESIAN_POINT('Ctrl Pts',(-18.2027332815713,28.2357930827073,122.470098177361)) ;
#90077 = CARTESIAN_POINT('Ctrl Pts',(-18.5964066329864,28.2557353281035,122.115256848635)) ;
#90078 = CARTESIAN_POINT('Ctrl Pts',(-19.0856168086369,28.275607376218,121.915866271612)) ;
#90079 = CARTESIAN_POINT('Ctrl Pts',(-19.6169218061426,28.2956184411721,121.895642781133)) ;
#90080 = CARTESIAN_POINT('Ctrl Pts',(-20.1188292935515,28.3154299654757,122.055652903489)) ;
#90081 = CARTESIAN_POINT('Ctrl Pts',(-20.5414244265229,28.3355251774391,122.381920562138)) ;
#90082 = CARTESIAN_POINT('Ctrl Pts',(-20.8229842740963,28.3553059013589,122.826156087312)) ;
#90083 = CARTESIAN_POINT('Ctrl Pts',(-20.9383586766976,28.3752969770017,123.344606135062)) ;
#90084 = CARTESIAN_POINT('Ctrl Pts',(-20.8698588440805,28.3951789160447,123.868727080192)) ;
#90085 = CARTESIAN_POINT('Ctrl Pts',(-20.6263861212141,28.415131520548,124.33974290189)) ;
#90086 = CARTESIAN_POINT('Ctrl Pts',(-20.2377379988083,28.4350303892786,124.69852394791)) ;
#90087 = CARTESIAN_POINT('Ctrl Pts',(-19.7505120225895,28.4549237890882,124.903632562329)) ;
#90088 = CARTESIAN_POINT('Ctrl Pts',(-19.2219604499456,28.4748329199282,124.931009679036)) ;
#90089 = CARTESIAN_POINT('Ctrl Pts',(-18.7130412720916,28.4948650196918,124.774779736929)) ;
#90090 = CARTESIAN_POINT('Ctrl Pts',(-18.3620584933981,28.5113970928613,124.510284590691)) ;
#90091 = CARTESIAN_POINT('Ctrl Pts',(-18.1460674126106,28.5247324334672,124.234383966013)) ;
#90092 = CARTESIAN_POINT('Ctrl Pts',(-18.0239856925731,28.5345749920069,124.006320082283)) ;
#90093 = CARTESIAN_POINT('Ctrl Pts',(-17.9414030192515,28.5446268988568,123.755444503094)) ;
#90094 = CARTESIAN_POINT('Ctrl Pts',(-17.8916917870985,28.5578754132477,123.410803822859)) ;
#90095 = CARTESIAN_POINT('Ctrl Pts',(-17.9431871506201,28.5744745881955,122.972697293955)) ;
#90096 = CARTESIAN_POINT('Ctrl Pts',(-18.1408539621108,28.5910633739905,122.578582469759)) ;
#90097 = CARTESIAN_POINT('Ctrl Pts',(-18.3723983221645,28.6043391903325,122.317615113724)) ;
#90098 = CARTESIAN_POINT('Ctrl Pts',(-18.577527292145,28.6143130411263,122.154436808147)) ;
#90099 = CARTESIAN_POINT('Ctrl Pts',(-18.8092646056395,28.6243420732187,122.028922034954)) ;
#90100 = CARTESIAN_POINT('Ctrl Pts',(-19.0557478273817,28.6342321987206,121.946437772454)) ;
#90101 = CARTESIAN_POINT('Ctrl Pts',(-19.3153706733146,28.6442246769921,121.907264160908)) ;
#90102 = CARTESIAN_POINT('Ctrl Pts',(-19.5768427425273,28.6541758920895,121.913598624698)) ;
#90103 = CARTESIAN_POINT('Ctrl Pts',(-19.8356388835886,28.6642243938445,121.9659387871)) ;
#90104 = CARTESIAN_POINT('Ctrl Pts',(-20.0765080850792,28.6740657434613,122.060169659542)) ;
#90105 = CARTESIAN_POINT('Ctrl Pts',(-20.300843510358,28.6840520344815,122.196258449548)) ;
#90106 = CARTESIAN_POINT('Ctrl Pts',(-20.4973109441294,28.6939886462101,122.368330827901)) ;
#90107 = CARTESIAN_POINT('Ctrl Pts',(-20.6626341566035,28.7040385215777,122.57425065372)) ;
#90108 = CARTESIAN_POINT('Ctrl Pts',(-20.7873624065296,28.7138889801131,122.801100887893)) ;
#90109 = CARTESIAN_POINT('Ctrl Pts',(-20.8724691047688,28.7238609170659,123.048913631883)) ;
#90110 = CARTESIAN_POINT('Ctrl Pts',(-20.9133208956479,28.733856373998,123.308428140769)) ;
#90111 = CARTESIAN_POINT('Ctrl Pts',(-20.9081765057666,28.7438891810511,123.572012092005)) ;
#90112 = CARTESIAN_POINT('Ctrl Pts',(-20.8585590805843,28.7537490676411,123.826338311456)) ;
#90113 = CARTESIAN_POINT('Ctrl Pts',(-20.764789229398,28.7637381482063,124.071497059533)) ;
#90114 = CARTESIAN_POINT('Ctrl Pts',(-20.6306361728563,28.7736696274155,124.295376547867)) ;
#90115 = CARTESIAN_POINT('Ctrl Pts',(-20.4590320836787,28.7836554868614,124.493932716745)) ;
#90116 = CARTESIAN_POINT('Ctrl Pts',(-20.2542272972785,28.7936936375086,124.660161314307)) ;
#90117 = CARTESIAN_POINT('Ctrl Pts',(-20.0282560662824,28.803541728013,124.78635916123)) ;
#90118 = CARTESIAN_POINT('Ctrl Pts',(-19.7786454124,28.813602636531,124.873435806326)) ;
#90119 = CARTESIAN_POINT('Ctrl Pts',(-19.5219342752848,28.8234974836889,124.914980277803)) ;
#90120 = CARTESIAN_POINT('Ctrl Pts',(-19.26072567087,28.833439155734,124.911999560869)) ;
#90121 = CARTESIAN_POINT('Ctrl Pts',(-19.0023461124135,28.8434416828595,124.863503088264)) ;
#90122 = CARTESIAN_POINT('Ctrl Pts',(-18.7557142855735,28.8534764740469,124.770209950683)) ;
#90123 = CARTESIAN_POINT('Ctrl Pts',(-18.5330665031705,28.863321353906,124.638416591467)) ;
#90124 = CARTESIAN_POINT('Ctrl Pts',(-18.3335959771311,28.8733072345245,124.467967806184)) ;
#90125 = CARTESIAN_POINT('Ctrl Pts',(-18.1674022200289,28.8832419576177,124.266559871745)) ;
#90126 = CARTESIAN_POINT('Ctrl Pts',(-18.0373647499672,28.8932997979289,124.036497815317)) ;
#90127 = CARTESIAN_POINT('Ctrl Pts',(-17.950911814326,28.9031202853254,123.793301563566)) ;
#90128 = CARTESIAN_POINT('Ctrl Pts',(-17.9065295280347,28.9131806866705,123.532709133583)) ;
#90129 = CARTESIAN_POINT('Ctrl Pts',(-17.9084022908856,28.9231116522234,123.271710634104)) ;
#90130 = CARTESIAN_POINT('Ctrl Pts',(-17.9550199869084,28.9330505145599,123.014749249068)) ;
#90131 = CARTESIAN_POINT('Ctrl Pts',(-18.0458283672377,28.9430362454861,122.768516340365)) ;
#90132 = CARTESIAN_POINT('Ctrl Pts',(-18.1787394441072,28.9530606309135,122.541096570347)) ;
#90133 = CARTESIAN_POINT('Ctrl Pts',(-18.3467919785273,28.9629639152668,122.342338042519)) ;
#90134 = CARTESIAN_POINT('Ctrl Pts',(-18.5499731696622,28.9730239198448,122.173252013428)) ;
#90135 = CARTESIAN_POINT('Ctrl Pts',(-18.7744434743641,28.9828671889139,122.044654486055)) ;
#90136 = CARTESIAN_POINT('Ctrl Pts',(-19.0212126462486,28.9928577545216,121.955119711378)) ;
#90137 = CARTESIAN_POINT('Ctrl Pts',(-19.2782134163419,29.0027858863004,121.910108935023)) ;
#90138 = CARTESIAN_POINT('Ctrl Pts',(-19.5406963148018,29.0127737733813,121.909949720142)) ;
#90139 = CARTESIAN_POINT('Ctrl Pts',(-19.8003636387641,29.02280972295,121.956024596532)) ;
#90140 = CARTESIAN_POINT('Ctrl Pts',(-20.0437946869578,29.0326646093288,122.0444605937)) ;
#90141 = CARTESIAN_POINT('Ctrl Pts',(-20.2715846639012,29.0426640236767,122.175375625611)) ;
#90142 = CARTESIAN_POINT('Ctrl Pts',(-20.4713275194905,29.0525591888672,122.34193965665)) ;
#90143 = CARTESIAN_POINT('Ctrl Pts',(-20.6418433631902,29.0626195075592,122.543928922245)) ;
#90144 = CARTESIAN_POINT('Ctrl Pts',(-20.7720825546946,29.0724696393352,122.767656038512)) ;
#90145 = CARTESIAN_POINT('Ctrl Pts',(-20.8637061447357,29.0825002097855,123.014799627036)) ;
#90146 = CARTESIAN_POINT('Ctrl Pts',(-20.9103762630913,29.0925143604583,123.273804452751)) ;
#90147 = CARTESIAN_POINT('Ctrl Pts',(-20.9117741336975,29.1024072940037,123.53378141723)) ;
#90148 = CARTESIAN_POINT('Ctrl Pts',(-20.867883240844,29.112396807994,123.792574654758)) ;
#90149 = CARTESIAN_POINT('Ctrl Pts',(-20.7801810778798,29.1223505786464,124.039048417847)) ;
#90150 = CARTESIAN_POINT('Ctrl Pts',(-20.6496213778519,29.132398347307,124.268526107138)) ;
#90151 = CARTESIAN_POINT('Ctrl Pts',(-20.4848587379141,29.1422400737468,124.46791155322)) ;
#90152 = CARTESIAN_POINT('Ctrl Pts',(-20.2855219341304,29.1522255905695,124.638505213354)) ;
#90153 = CARTESIAN_POINT('Ctrl Pts',(-20.0606187506956,29.1621649222651,124.771401656305)) ;
#90154 = CARTESIAN_POINT('Ctrl Pts',(-19.8136216179253,29.1722046919626,124.864082795799)) ;
#90155 = CARTESIAN_POINT('Ctrl Pts',(-19.558187368143,29.1820928532114,124.911871502229)) ;
#90156 = CARTESIAN_POINT('Ctrl Pts',(-19.2957011783519,29.1920824077138,124.915102448404)) ;
#90157 = CARTESIAN_POINT('Ctrl Pts',(-19.0374781818425,29.2020408222374,124.872643060304)) ;
#90158 = CARTESIAN_POINT('Ctrl Pts',(-18.7917703837319,29.2119407350668,124.787095968834)) ;
#90159 = CARTESIAN_POINT('Ctrl Pts',(-18.5613536456222,29.2219874347167,124.65825660223)) ;
#90160 = CARTESIAN_POINT('Ctrl Pts',(-18.3596420924881,29.2318872950223,124.493892512925)) ;
#90161 = CARTESIAN_POINT('Ctrl Pts',(-18.1869148909575,29.2419386992278,124.294103199834)) ;
#90162 = CARTESIAN_POINT('Ctrl Pts',(-18.0536769669931,29.2518197361489,124.071184737114)) ;
#90163 = CARTESIAN_POINT('Ctrl Pts',(-17.9597521892141,29.2618195683264,123.825804732125)) ;
#90164 = CARTESIAN_POINT('Ctrl Pts',(-17.9100403484687,29.2717375713113,123.569907928987)) ;
#90165 = CARTESIAN_POINT('Ctrl Pts',(-17.9055429199268,29.2817888771858,123.305853384214)) ;
#90166 = CARTESIAN_POINT('Ctrl Pts',(-17.9459174143974,29.2916587005774,123.049589465829)) ;
#90167 = CARTESIAN_POINT('Ctrl Pts',(-18.0318972364498,29.3017328666277,122.799266072468)) ;
#90168 = CARTESIAN_POINT('Ctrl Pts',(-18.1565829873438,29.3115529507693,122.573255953319)) ;
#90169 = CARTESIAN_POINT('Ctrl Pts',(-18.3226099186623,29.3216316775052,122.36697855623)) ;
#90170 = CARTESIAN_POINT('Ctrl Pts',(-18.5174760158988,29.3314832581547,122.196440883835)) ;
#90171 = CARTESIAN_POINT('Ctrl Pts',(-18.7437589213341,29.3415563864531,122.059171973647)) ;
#90172 = CARTESIAN_POINT('Ctrl Pts',(-18.9848715208291,29.3513988643445,121.965485865843)) ;
#90173 = CARTESIAN_POINT('Ctrl Pts',(-19.2419396876553,29.3613794709426,121.913527744618)) ;
#90174 = CARTESIAN_POINT('Ctrl Pts',(-19.5051237744955,29.3713971799614,121.907465724619)) ;
#90175 = CARTESIAN_POINT('Ctrl Pts',(-19.7620431375332,29.3812833589988,121.946175909808)) ;
#90176 = CARTESIAN_POINT('Ctrl Pts',(-20.0125730392579,29.3913409715712,122.030311528781)) ;
#90177 = CARTESIAN_POINT('Ctrl Pts',(-20.2405533557099,29.4012173649433,122.154388504609)) ;
#90178 = CARTESIAN_POINT('Ctrl Pts',(-20.4463541851592,29.4112123930937,122.317580930784)) ;
#90179 = CARTESIAN_POINT('Ctrl Pts',(-20.6208172138511,29.4212331399397,122.514846934847)) ;
#90180 = CARTESIAN_POINT('Ctrl Pts',(-20.7570016708868,29.4311352086061,122.736578720449)) ;
#90181 = CARTESIAN_POINT('Ctrl Pts',(-20.8538352390123,29.4411259484258,122.980616710616)) ;
#90182 = CARTESIAN_POINT('Ctrl Pts',(-20.9064868502557,29.4510891446361,123.23707769916)) ;
#90183 = CARTESIAN_POINT('Ctrl Pts',(-20.914410419633,29.4609933289362,123.497253000178)) ;
#90184 = CARTESIAN_POINT('Ctrl Pts',(-20.8762358005154,29.4710537893271,123.758827580412)) ;
#90185 = CARTESIAN_POINT('Ctrl Pts',(-20.7953305897781,29.4808943351979,124.004481871684)) ;
#90186 = CARTESIAN_POINT('Ctrl Pts',(-20.6705730749621,29.4909565559097,124.237592816873)) ;
#90187 = CARTESIAN_POINT('Ctrl Pts',(-20.5096749757579,29.5008536989262,124.441955772106)) ;
#90188 = CARTESIAN_POINT('Ctrl Pts',(-20.3156640114165,29.5107848753434,124.616506656617)) ;
#90189 = CARTESIAN_POINT('Ctrl Pts',(-20.0916629418475,29.520827089122,124.756019382219)) ;
#90190 = CARTESIAN_POINT('Ctrl Pts',(-19.8506899321232,29.5307136293248,124.853178323577)) ;
#90191 = CARTESIAN_POINT('Ctrl Pts',(-19.5938766834909,29.5407072239302,124.908009663912)) ;
#90192 = CARTESIAN_POINT('Ctrl Pts',(-19.332712747215,29.5506510990877,124.917331744836)) ;
#90193 = CARTESIAN_POINT('Ctrl Pts',(-19.0734479879124,29.5606116352025,124.881449299093)) ;
#90194 = CARTESIAN_POINT('Ctrl Pts',(-18.8233593876915,29.5706082385252,124.800941689882)) ;
#90195 = CARTESIAN_POINT('Ctrl Pts',(-18.5904051560722,29.5806413214798,124.677470404879)) ;
#90196 = CARTESIAN_POINT('Ctrl Pts',(-18.3859961074744,29.5904924901813,124.518621309858)) ;
#90197 = CARTESIAN_POINT('Ctrl Pts',(-18.2097416401463,29.6004549808802,124.325047682833)) ;
#90198 = CARTESIAN_POINT('Ctrl Pts',(-18.0691118335263,29.6104834092979,124.102151585275)) ;
#90199 = CARTESIAN_POINT('Ctrl Pts',(-17.9704269675126,29.6203937766625,123.861151262509)) ;
#90200 = CARTESIAN_POINT('Ctrl Pts',(-17.9142776230811,29.6303286442776,123.606174600459)) ;
#90201 = CARTESIAN_POINT('Ctrl Pts',(-17.9033816131702,29.6403697862566,123.342537736076)) ;
#90202 = CARTESIAN_POINT('Ctrl Pts',(-17.9377116774726,29.6502569224598,123.084976886491)) ;
#90203 = CARTESIAN_POINT('Ctrl Pts',(-18.0166487960382,29.6602492048632,122.834555046718)) ;
#90204 = CARTESIAN_POINT('Ctrl Pts',(-18.1374177643865,29.6701977328284,122.60266731771)) ;
#90205 = CARTESIAN_POINT('Ctrl Pts',(-18.2961113277449,29.6801344639905,122.395320977446)) ;
#90206 = CARTESIAN_POINT('Ctrl Pts',(-18.4891133100422,29.6901176748505,122.217574840443)) ;
#90207 = CARTESIAN_POINT('Ctrl Pts',(-18.7115763555757,29.7001607740004,122.075621485712)) ;
#90208 = CARTESIAN_POINT('Ctrl Pts',(-18.949992826985,29.7099917382753,121.976031903192)) ;
#90209 = CARTESIAN_POINT('Ctrl Pts',(-19.2081671628499,29.7200645906612,121.917784053486)) ;
#90210 = CARTESIAN_POINT('Ctrl Pts',(-19.467127300379,29.729928718373,121.905550210389)) ;
#90211 = CARTESIAN_POINT('Ctrl Pts',(-19.7284409010787,29.7399509205079,121.938343116302)) ;
#90212 = CARTESIAN_POINT('Ctrl Pts',(-19.9800566224885,29.7499781134763,122.016652854863)) ;
#90213 = CARTESIAN_POINT('Ctrl Pts',(-20.210400702207,29.7598337074433,122.135017062282)) ;
#90214 = CARTESIAN_POINT('Ctrl Pts',(-20.4193129127433,29.7697908793086,122.292588450327)) ;
#90215 = CARTESIAN_POINT('Ctrl Pts',(-20.5988052662756,29.779829723307,122.485901523046)) ;
#90216 = CARTESIAN_POINT('Ctrl Pts',(-20.740066998357,29.7897037471826,122.703600137925)) ;
#90217 = CARTESIAN_POINT('Ctrl Pts',(-20.8433563231969,29.799773573173,122.947193893449)) ;
#90218 = CARTESIAN_POINT('Ctrl Pts',(-20.9015323318944,29.8096068170702,123.198990450446)) ;
#90219 = CARTESIAN_POINT('Ctrl Pts',(-20.9161199372986,29.8196372448433,123.462166811631)) ;
#90220 = CARTESIAN_POINT('Ctrl Pts',(-20.8840222579638,29.8296688615884,123.723840344967)) ;
#90221 = CARTESIAN_POINT('Ctrl Pts',(-20.8090522677205,29.8394985385691,123.971017934646)) ;
#90222 = CARTESIAN_POINT('Ctrl Pts',(-20.6910925085159,29.8494880554091,124.205545773944)) ;
#90223 = CARTESIAN_POINT('Ctrl Pts',(-20.5328239158274,29.8595316675488,124.416758785664)) ;
#90224 = CARTESIAN_POINT('Ctrl Pts',(-20.3448871273158,29.8693542738841,124.593710045622)) ;
#90225 = CARTESIAN_POINT('Ctrl Pts',(-20.1246838233644,29.8793925037834,124.738944315077)) ;
#90226 = CARTESIAN_POINT('Ctrl Pts',(-19.8829956359094,29.8894035385753,124.842903601253)) ;
#90227 = CARTESIAN_POINT('Ctrl Pts',(-19.629944134694,29.8993012695424,124.903033941421)) ;
#90228 = CARTESIAN_POINT('Ctrl Pts',(-19.3679037961103,29.9092908973929,124.918797744218)) ;
#90229 = CARTESIAN_POINT('Ctrl Pts',(-19.1080010949963,29.9192466878389,124.88883390131)) ;
#90230 = CARTESIAN_POINT('Ctrl Pts',(-18.857809354991,29.929174086401,124.814884890953)) ;
#90231 = CARTESIAN_POINT('Ctrl Pts',(-18.6219992187214,29.9391996815108,124.697407355649)) ;
#90232 = CARTESIAN_POINT('Ctrl Pts',(-18.4130181328675,29.9490855321804,124.543075003642)) ;
#90233 = CARTESIAN_POINT('Ctrl Pts',(-18.2316836984906,29.9590747120246,124.353257774373)) ;
#90234 = CARTESIAN_POINT('Ctrl Pts',(-18.0857681933595,29.9691158991282,124.133401993258)) ;
#90235 = CARTESIAN_POINT('Ctrl Pts',(-17.9820470555373,29.9789485426041,123.896746050801)) ;
#90236 = CARTESIAN_POINT('Ctrl Pts',(-17.9192601596466,29.9889424923136,123.641732893525)) ;
#90237 = CARTESIAN_POINT('Ctrl Pts',(-17.9021985043466,29.9989716150901,123.378728309774)) ;
#90238 = CARTESIAN_POINT('Ctrl Pts',(-17.9302095800825,30.0088477460088,123.120696813041)) ;
#90239 = CARTESIAN_POINT('Ctrl Pts',(-18.0031833304748,30.0188457810258,122.868329081507)) ;
#90240 = CARTESIAN_POINT('Ctrl Pts',(-18.1177424147025,30.0287597107845,122.634304146691)) ;
#90241 = CARTESIAN_POINT('Ctrl Pts',(-18.2731207173211,30.0388028985223,122.420990591887)) ;
#90242 = CARTESIAN_POINT('Ctrl Pts',(-18.460477880612,30.0487027406627,122.240473905107)) ;
#90243 = CARTESIAN_POINT('Ctrl Pts',(-18.6780038327348,30.0586940074707,122.093431755788)) ;
#90244 = CARTESIAN_POINT('Ctrl Pts',(-18.9189236827015,30.0687261096027,121.986371546732)) ;
#90245 = CARTESIAN_POINT('Ctrl Pts',(-19.170468246111,30.0785929905574,121.92348620404)) ;
#90246 = CARTESIAN_POINT('Ctrl Pts',(-19.4323508510835,30.0885847818456,121.904376081853)) ;
#90247 = CARTESIAN_POINT('Ctrl Pts',(-19.6945696776365,30.0986168977571,121.931642192667)) ;
#90248 = CARTESIAN_POINT('Ctrl Pts',(-19.9440014901615,30.1084832145571,122.002451382793)) ;
#90249 = CARTESIAN_POINT('Ctrl Pts',(-20.1803630188248,30.1184706960307,122.116477795654)) ;
#90250 = CARTESIAN_POINT('Ctrl Pts',(-20.392566350984,30.1284156204096,122.269087188915)) ;
#90251 = CARTESIAN_POINT('Ctrl Pts',(-20.5767324875527,30.1384605063203,122.458162856591)) ;
#90252 = CARTESIAN_POINT('Ctrl Pts',(-20.7227801654869,30.1483226100329,122.67228121434)) ;
#90253 = CARTESIAN_POINT('Ctrl Pts',(-20.8312983726913,30.1583141738574,122.911353552395)) ;
#90254 = CARTESIAN_POINT('Ctrl Pts',(-20.8961724450446,30.1682469819203,123.164186294995)) ;
#90255 = CARTESIAN_POINT('Ctrl Pts',(-20.916810994507,30.1781840841566,123.424522266059)) ;
#90256 = CARTESIAN_POINT('Ctrl Pts',(-20.8912996042722,30.188236530427,123.687434835979)) ;
#90257 = CARTESIAN_POINT('Ctrl Pts',(-20.8223241947769,30.1980826460086,123.936840767883)) ;
#90258 = CARTESIAN_POINT('Ctrl Pts',(-20.7091987850365,30.2081306657235,124.17541152145)) ;
#90259 = CARTESIAN_POINT('Ctrl Pts',(-20.5576650602483,30.2180726173524,124.388259700238)) ;
#90260 = CARTESIAN_POINT('Ctrl Pts',(-20.3719976932811,30.2280113983515,124.57195695698)) ;
#90261 = CARTESIAN_POINT('Ctrl Pts',(-20.1552718930415,30.2380374470776,124.721755575099)) ;
#90262 = CARTESIAN_POINT('Ctrl Pts',(-19.9192454996909,30.2479243074858,124.830442864662)) ;
#90263 = CARTESIAN_POINT('Ctrl Pts',(-19.6643659591417,30.2579555826176,124.897557475444)) ;
#90264 = CARTESIAN_POINT('Ctrl Pts',(-19.4055132729224,30.267838559918,124.919346689653)) ;
#90265 = CARTESIAN_POINT('Ctrl Pts',(-19.1423742851105,30.2778954133252,124.895462225033)) ;
#90266 = CARTESIAN_POINT('Ctrl Pts',(-18.8081585492134,30.2910636544011,124.805348478367)) ;
#90267 = CARTESIAN_POINT('Ctrl Pts',(-18.4999606060616,30.3044646836276,124.627109350704)) ;
#90268 = CARTESIAN_POINT('Ctrl Pts',(-18.2548402508357,30.3176776003585,124.381034742561)) ;
#90269 = CARTESIAN_POINT('Ctrl Pts',(-18.1049154570646,30.3276059948117,124.167570645998)) ;
#90270 = CARTESIAN_POINT('Ctrl Pts',(-17.9935223888196,30.3375874949398,123.930052646589)) ;
#90271 = CARTESIAN_POINT('Ctrl Pts',(-17.9250251231697,30.3476280382099,123.675258459608)) ;
#90272 = CARTESIAN_POINT('Ctrl Pts',(-17.9019089621538,30.357477369993,123.417459308466)) ;
#90273 = CARTESIAN_POINT('Ctrl Pts',(-17.9235593814897,30.3674727744647,123.155687344675)) ;
#90274 = CARTESIAN_POINT('Ctrl Pts',(-17.9909293206155,30.3774891019133,122.901233828562)) ;
#90275 = CARTESIAN_POINT('Ctrl Pts',(-18.1363619700471,30.3907127590798,122.585590307536)) ;
#90276 = CARTESIAN_POINT('Ctrl Pts',(-18.3617445260575,30.4040070504692,122.313580619713)) ;
#90277 = CARTESIAN_POINT('Ctrl Pts',(-18.6465310373536,30.4172914014007,122.111548083525)) ;
#90278 = CARTESIAN_POINT('Ctrl Pts',(-18.8832363601411,30.4272637824625,121.999174549586)) ;
#90279 = CARTESIAN_POINT('Ctrl Pts',(-19.1341844428468,30.4371721620881,121.929596295639)) ;
#90280 = CARTESIAN_POINT('Ctrl Pts',(-19.3971607833827,30.4472261608362,121.904405542938)) ;
#90281 = CARTESIAN_POINT('Ctrl Pts',(-19.6555624151399,30.4570883579525,121.924666180462)) ;
#90282 = CARTESIAN_POINT('Ctrl Pts',(-19.9952854684949,30.4704354843266,122.01183022792)) ;
#90283 = CARTESIAN_POINT('Ctrl Pts',(-20.3783427936636,30.486972449968,122.227450317524)) ;
#90284 = CARTESIAN_POINT('Ctrl Pts',(-20.6669629084573,30.5036070541419,122.562246315872)) ;
#90285 = CARTESIAN_POINT('Ctrl Pts',(-20.8186251415275,30.5168968473846,122.876913691283)) ;
#90286 = CARTESIAN_POINT('Ctrl Pts',(-20.8898702450345,30.526849478644,123.128536989928)) ;
#90287 = CARTESIAN_POINT('Ctrl Pts',(-20.9166526278365,30.5368014459487,123.388718812429)) ;
#90288 = CARTESIAN_POINT('Ctrl Pts',(-20.8911983771875,30.5501687044125,123.739033428064)) ;
#90289 = CARTESIAN_POINT('Ctrl Pts',(-20.7477475189037,30.5666855163617,124.154053346653)) ;
#90290 = CARTESIAN_POINT('Ctrl Pts',(-20.4126988443248,30.586711411368,124.567435413989)) ;
#90291 = CARTESIAN_POINT('Ctrl Pts',(-19.9614671654052,30.6065221414982,124.838987072851)) ;
#90292 = CARTESIAN_POINT('Ctrl Pts',(-19.4406806653169,30.626499357628,124.942199667842)) ;
#90293 = CARTESIAN_POINT('Ctrl Pts',(-18.9173904837054,30.6464262330233,124.86074682562)) ;
#90294 = CARTESIAN_POINT('Ctrl Pts',(-18.4548551754709,30.6662476944996,124.608403042469)) ;
#90295 = CARTESIAN_POINT('Ctrl Pts',(-18.1021138578036,30.6863220123089,124.208208372338)) ;
#90296 = CARTESIAN_POINT('Ctrl Pts',(-17.9097086793361,30.7061699813168,123.716866447982)) ;
#90297 = CARTESIAN_POINT('Ctrl Pts',(-17.8953715490996,30.72611701538,123.187016557676)) ;
#90298 = CARTESIAN_POINT('Ctrl Pts',(-18.0624519723751,30.7460129663522,122.685261153681)) ;
#90299 = CARTESIAN_POINT('Ctrl Pts',(-18.3899873246686,30.7659084459704,122.270164037835)) ;
#90300 = CARTESIAN_POINT('Ctrl Pts',(-18.8408813750857,30.7858645569352,121.990764998331)) ;
#90301 = CARTESIAN_POINT('Ctrl Pts',(-19.3586318139167,30.8057691049752,121.882458783378)) ;
#90302 = CARTESIAN_POINT('Ctrl Pts',(-19.8818185744041,30.8256432292943,121.955925643777)) ;
#90303 = CARTESIAN_POINT('Ctrl Pts',(-20.3522474723433,30.8456977592933,122.206355579186)) ;
#90304 = CARTESIAN_POINT('Ctrl Pts',(-20.7048311303731,30.8655052730533,122.59744630561)) ;
#90305 = CARTESIAN_POINT('Ctrl Pts',(-20.9055172328141,30.885488628821,123.089116826482)) ;
#90306 = CARTESIAN_POINT('Ctrl Pts',(-20.9255113800788,30.905406931405,123.618128166974)) ;
#90307 = CARTESIAN_POINT('Ctrl Pts',(-20.7655078140649,30.9252751468507,124.121480433858)) ;
#90308 = CARTESIAN_POINT('Ctrl Pts',(-20.4398813109932,30.945325463647,124.543131309097)) ;
#90309 = CARTESIAN_POINT('Ctrl Pts',(-19.9961416301673,30.9651015255295,124.825243045067)) ;
#90310 = CARTESIAN_POINT('Ctrl Pts',(-19.4760428857146,30.9851561312219,124.940890724397)) ;
#90311 = CARTESIAN_POINT('Ctrl Pts',(-18.9542245242808,31.0049498203778,124.872803577724)) ;
#90312 = CARTESIAN_POINT('Ctrl Pts',(-18.4824553574321,31.0249165119722,124.630033633571)) ;
#90313 = CARTESIAN_POINT('Ctrl Pts',(-18.1224338999949,31.0448765577232,124.240259071478)) ;
#90314 = CARTESIAN_POINT('Ctrl Pts',(-17.9173964213131,31.0647748178734,123.752794316431)) ;
#90315 = CARTESIAN_POINT('Ctrl Pts',(-17.8903757638579,31.0846697334226,123.22473469265)) ;
#90316 = CARTESIAN_POINT('Ctrl Pts',(-18.0448284170245,31.1045799138362,122.718600932171)) ;
#90317 = CARTESIAN_POINT('Ctrl Pts',(-18.3629565328079,31.1245157129505,122.29484956572)) ;
#90318 = CARTESIAN_POINT('Ctrl Pts',(-18.8066023023989,31.1444535746046,122.005048043472)) ;
#90319 = CARTESIAN_POINT('Ctrl Pts',(-19.3219837707938,31.1643726212422,121.883821949317)) ;
#90320 = CARTESIAN_POINT('Ctrl Pts',(-19.8485586474663,31.1843215192964,121.945761987751)) ;
#90321 = CARTESIAN_POINT('Ctrl Pts',(-20.3214530576657,31.2042273467395,122.183047702527)) ;
#90322 = CARTESIAN_POINT('Ctrl Pts',(-20.62457405632,31.2208100421048,122.502904725448)) ;
#90323 = CARTESIAN_POINT('Ctrl Pts',(-20.7912398187945,31.2340842558284,122.809407390215)) ;
#90324 = CARTESIAN_POINT('Ctrl Pts',(-20.8750277230681,31.2441309750277,123.059747682737)) ;
#90325 = CARTESIAN_POINT('Ctrl Pts',(-20.9135794146644,31.2539750096734,123.315566077138)) ;
#90326 = CARTESIAN_POINT('Ctrl Pts',(-20.9056166911276,31.267309394578,123.665879105346)) ;
#90327 = CARTESIAN_POINT('Ctrl Pts',(-20.7817240069621,31.2838966118777,124.089024590941)) ;
#90328 = CARTESIAN_POINT('Ctrl Pts',(-20.5204927418564,31.3005298239156,124.44560763796)) ;
#90329 = CARTESIAN_POINT('Ctrl Pts',(-20.2482842473179,31.3138122661878,124.664159228814)) ;
#90330 = CARTESIAN_POINT('Ctrl Pts',(-20.0203552489676,31.323718154102,124.789870365395)) ;
#90331 = CARTESIAN_POINT('Ctrl Pts',(-19.7720861356419,31.3337065722071,124.875118114952)) ;
#90332 = CARTESIAN_POINT('Ctrl Pts',(-19.5118369240493,31.3437299994459,124.915827009597)) ;
#90333 = CARTESIAN_POINT('Ctrl Pts',(-19.2516219194721,31.3536344305629,124.910938614496)) ;
#90334 = CARTESIAN_POINT('Ctrl Pts',(-18.9093544512018,31.3668975831733,124.844874070695)) ;
#90335 = CARTESIAN_POINT('Ctrl Pts',(-18.5909341743351,31.3802224810772,124.689988959161)) ;
#90336 = CARTESIAN_POINT('Ctrl Pts',(-18.3276472878309,31.3934782246928,124.461818204276)) ;
#90337 = CARTESIAN_POINT('Ctrl Pts',(-18.1623509832731,31.4034375981401,124.258944934311)) ;
#90338 = CARTESIAN_POINT('Ctrl Pts',(-18.0346692467731,31.4133814220671,124.030912426066)) ;
#90339 = CARTESIAN_POINT('Ctrl Pts',(-17.9478499345261,31.4234293662144,123.781565182109)) ;
#90340 = CARTESIAN_POINT('Ctrl Pts',(-17.9062405916385,31.4332803374325,123.526042263013)) ;
#90341 = CARTESIAN_POINT('Ctrl Pts',(-17.9089961332649,31.4432521548746,123.264037869211)) ;
#90342 = CARTESIAN_POINT('Ctrl Pts',(-17.9573713255669,31.4532475771667,123.0058246328)) ;
#90343 = CARTESIAN_POINT('Ctrl Pts',(-18.0504365475839,31.4632806422904,122.759146467247)) ;
#90344 = CARTESIAN_POINT('Ctrl Pts',(-18.182455819894,31.4731459749556,122.53603494168)) ;
#90345 = CARTESIAN_POINT('Ctrl Pts',(-18.3522600986835,31.4831065175532,122.336826203529)) ;
#90346 = CARTESIAN_POINT('Ctrl Pts',(-18.555825302581,31.4931402030549,122.169258613365)) ;
#90347 = CARTESIAN_POINT('Ctrl Pts',(-18.7818081775691,31.5030250350452,122.04108939127)) ;
#90348 = CARTESIAN_POINT('Ctrl Pts',(-19.0310789742768,31.513092461805,121.952582039014)) ;
#90349 = CARTESIAN_POINT('Ctrl Pts',(-19.2860425398375,31.5229309509638,121.909432534115)) ;
#90350 = CARTESIAN_POINT('Ctrl Pts',(-19.5504588373335,31.532994432154,121.910897207184)) ;
#90351 = CARTESIAN_POINT('Ctrl Pts',(-19.806252038689,31.5428885899691,121.957687925717)) ;
#90352 = CARTESIAN_POINT('Ctrl Pts',(-20.0513987980626,31.5528304467134,122.047929059202)) ;
#90353 = CARTESIAN_POINT('Ctrl Pts',(-20.2786389120805,31.5628329243848,122.180116472421)) ;
#90354 = CARTESIAN_POINT('Ctrl Pts',(-20.4798154738035,31.5728677286891,122.350583181619)) ;
#90355 = CARTESIAN_POINT('Ctrl Pts',(-20.6455040679005,31.5827126055348,122.549301249805)) ;
#90356 = CARTESIAN_POINT('Ctrl Pts',(-20.7764127766709,31.5926984850903,122.776686313643)) ;
#90357 = CARTESIAN_POINT('Ctrl Pts',(-20.8656033287989,31.6026332154488,123.022106958682)) ;
#90358 = CARTESIAN_POINT('Ctrl Pts',(-20.9111243111444,31.6126910277617,123.282421856098)) ;
#90359 = CARTESIAN_POINT('Ctrl Pts',(-20.9112068367647,31.6225116198861,123.540539997943)) ;
#90360 = CARTESIAN_POINT('Ctrl Pts',(-20.865687331279,31.6325782054958,123.801079440899)) ;
#90361 = CARTESIAN_POINT('Ctrl Pts',(-20.7770317266897,31.6424777860777,124.045722854565)) ;
#90362 = CARTESIAN_POINT('Ctrl Pts',(-20.6453936142839,31.6525293857559,124.274672946805)) ;
#90363 = CARTESIAN_POINT('Ctrl Pts',(-20.4790792984421,31.6624035721729,124.473913961419)) ;
#90364 = CARTESIAN_POINT('Ctrl Pts',(-20.2772197656373,31.6724600480538,124.644405849723)) ;
#90365 = CARTESIAN_POINT('Ctrl Pts',(-20.0524976022664,31.6823529793564,124.775234014397)) ;
#90366 = CARTESIAN_POINT('Ctrl Pts',(-19.8043940631741,31.692415758069,124.866611670972)) ;
#90367 = CARTESIAN_POINT('Ctrl Pts',(-19.5498389701363,31.7022582836502,124.912638260607)) ;
#90368 = CARTESIAN_POINT('Ctrl Pts',(-19.287331714963,31.7122490490751,124.914410642322)) ;
#90369 = CARTESIAN_POINT('Ctrl Pts',(-19.0300907670381,31.7221771250731,124.870797527224)) ;
#90370 = CARTESIAN_POINT('Ctrl Pts',(-18.7826960536114,31.7321650354601,124.783086226261)) ;
#90371 = CARTESIAN_POINT('Ctrl Pts',(-18.5534309522588,31.7422009475851,124.652751134591)) ;
#90372 = CARTESIAN_POINT('Ctrl Pts',(-18.353644514985,31.7520559604328,124.487929296874)) ;
#90373 = CARTESIAN_POINT('Ctrl Pts',(-18.1828179715406,31.762054906349,124.288330075696)) ;
#90374 = CARTESIAN_POINT('Ctrl Pts',(-18.0503460097519,31.771951818797,124.064468215422)) ;
#90375 = CARTESIAN_POINT('Ctrl Pts',(-17.9573008027146,31.7820056168905,123.817225770989)) ;
#90376 = CARTESIAN_POINT('Ctrl Pts',(-17.9093501306192,31.7918865377172,123.562001493347)) ;
#90377 = CARTESIAN_POINT('Ctrl Pts',(-17.9059334517401,31.8018910637149,123.299145753374)) ;
#90378 = CARTESIAN_POINT('Ctrl Pts',(-17.9482120491376,31.8118750273324,123.040161685246)) ;
#90379 = CARTESIAN_POINT('Ctrl Pts',(-18.0355138245975,31.8219146678837,122.791213968382)) ;
#90380 = CARTESIAN_POINT('Ctrl Pts',(-18.1619308507885,31.8317586934984,122.565514127231)) ;
#90381 = CARTESIAN_POINT('Ctrl Pts',(-18.3274742184349,31.8417496993158,122.361724868883)) ;
#90382 = CARTESIAN_POINT('Ctrl Pts',(-18.5272092718872,31.8517874908479,122.189426042634)) ;
#90383 = CARTESIAN_POINT('Ctrl Pts',(-18.7492365418585,31.8616318906363,122.05662983357)) ;
#90384 = CARTESIAN_POINT('Ctrl Pts',(-18.9941697641335,31.8716166911931,121.962618647792)) ;
#90385 = CARTESIAN_POINT('Ctrl Pts',(-19.2505857843533,31.8815562146042,121.912666206365)) ;
#90386 = CARTESIAN_POINT('Ctrl Pts',(-19.5143572467387,31.8915959337052,121.908010594915)) ;
#90387 = CARTESIAN_POINT('Ctrl Pts',(-19.771053035124,31.9014841056245,121.94848018403)) ;
#90388 = CARTESIAN_POINT('Ctrl Pts',(-20.0194783206586,31.9114736680415,122.033298650539)) ;
#90389 = CARTESIAN_POINT('Ctrl Pts',(-20.2485944427228,31.9214320402362,122.159742447755)) ;
#90390 = CARTESIAN_POINT('Ctrl Pts',(-20.4514867933735,31.9313321144669,122.322607169725)) ;
#90391 = CARTESIAN_POINT('Ctrl Pts',(-20.6255075792033,31.9413782108405,122.521118480551)) ;
#90392 = CARTESIAN_POINT('Ctrl Pts',(-20.7605689119132,31.9512867948376,122.743753647204)) ;
#90393 = CARTESIAN_POINT('Ctrl Pts',(-20.8563432165643,31.9612973734285,122.988771599216)) ;
#90394 = CARTESIAN_POINT('Ctrl Pts',(-20.9076937965973,31.9713265315413,123.247285998441)) ;
#90395 = CARTESIAN_POINT('Ctrl Pts',(-20.9136494977614,31.9811794133794,123.506125048581)) ;
#90396 = CARTESIAN_POINT('Ctrl Pts',(-20.8749431252904,31.9911389745304,123.764982177503)) ;
#90397 = CARTESIAN_POINT('Ctrl Pts',(-20.7907719543159,32.0011774091195,124.014974716044)) ;
#90398 = CARTESIAN_POINT('Ctrl Pts',(-20.66695264249,32.0110506813466,124.243030789615)) ;
#90399 = CARTESIAN_POINT('Ctrl Pts',(-20.5021399302121,32.0211239233402,124.450109642599)) ;
#90400 = CARTESIAN_POINT('Ctrl Pts',(-20.3089945095504,32.0309442548732,124.621352168166)) ;
#90401 = CARTESIAN_POINT('Ctrl Pts',(-20.0834973590324,32.0410229161,124.760153885266)) ;
#90402 = CARTESIAN_POINT('Ctrl Pts',(-19.8427881240408,32.0508745113942,124.855626446842)) ;
#90403 = CARTESIAN_POINT('Ctrl Pts',(-19.5836101770202,32.060947646623,124.909232373603)) ;
#90404 = CARTESIAN_POINT('Ctrl Pts',(-19.3250477235278,32.0707900821481,124.91680672433)) ;
#90405 = CARTESIAN_POINT('Ctrl Pts',(-19.0654135129984,32.0807708512815,124.879716005305)) ;
#90406 = CARTESIAN_POINT('Ctrl Pts',(-18.8153951069858,32.0907879525253,124.797342091289)) ;
#90407 = CARTESIAN_POINT('Ctrl Pts',(-18.5862068913827,32.1006764001272,124.674829079308)) ;
#90408 = CARTESIAN_POINT('Ctrl Pts',(-18.3783323865825,32.110732114308,124.511717380021)) ;
#90409 = CARTESIAN_POINT('Ctrl Pts',(-18.20504643639,32.1206073207219,124.318515886017)) ;
#90410 = CARTESIAN_POINT('Ctrl Pts',(-18.0657523054065,32.1306023731946,124.095843008576)) ;
#90411 = CARTESIAN_POINT('Ctrl Pts',(-17.9673624393521,32.1406242571567,123.851536926118)) ;
#90412 = CARTESIAN_POINT('Ctrl Pts',(-17.9132447511668,32.150528229686,123.596960929366)) ;
#90413 = CARTESIAN_POINT('Ctrl Pts',(-17.9036966014167,32.1605167263469,123.334645288358)) ;
#90414 = CARTESIAN_POINT('Ctrl Pts',(-17.939924691972,32.1704805235949,123.07533896734)) ;
#90415 = CARTESIAN_POINT('Ctrl Pts',(-18.0195480393415,32.1803845469029,122.827524176256)) ;
#90416 = CARTESIAN_POINT('Ctrl Pts',(-18.1430776002173,32.1904450502245,122.593816083373)) ;
#90417 = CARTESIAN_POINT('Ctrl Pts',(-18.3015440658301,32.2002855853644,122.389414603507)) ;
#90418 = CARTESIAN_POINT('Ctrl Pts',(-18.4971343102704,32.210347806069,122.211511240556)) ;
#90419 = CARTESIAN_POINT('Ctrl Pts',(-18.7171578358292,32.2202449598452,122.072795116102)) ;
#90420 = CARTESIAN_POINT('Ctrl Pts',(-18.9584036223106,32.2301760932307,121.973254778566)) ;
#90421 = CARTESIAN_POINT('Ctrl Pts',(-19.2161862551315,32.2402184683764,121.916771627792)) ;
#90422 = CARTESIAN_POINT('Ctrl Pts',(-19.4757653790532,32.2501044061426,121.905874060276)) ;
#90423 = CARTESIAN_POINT('Ctrl Pts',(-19.7361743618916,32.2601002491274,121.940186996512)) ;
#90424 = CARTESIAN_POINT('Ctrl Pts',(-19.9853445011283,32.270042227006,122.01880797192)) ;
#90425 = CARTESIAN_POINT('Ctrl Pts',(-20.2176224237473,32.280001601487,122.139380240724)) ;
#90426 = CARTESIAN_POINT('Ctrl Pts',(-20.4263292540062,32.2899982173208,122.298965348353)) ;
#90427 = CARTESIAN_POINT('Ctrl Pts',(-20.6045437074103,32.3000324358943,122.49330330733)) ;
#90428 = CARTESIAN_POINT('Ctrl Pts',(-20.7440160089712,32.3098855031049,122.711454247693)) ;
#90429 = CARTESIAN_POINT('Ctrl Pts',(-20.8452761241106,32.3198457609825,122.952809541801)) ;
#90430 = CARTESIAN_POINT('Ctrl Pts',(-20.9031915155856,32.3298747876881,123.209934123648)) ;
#90431 = CARTESIAN_POINT('Ctrl Pts',(-20.9155108381836,32.3397849947225,123.470061362045)) ;
#90432 = CARTESIAN_POINT('Ctrl Pts',(-20.8830729146311,32.3497199053701,123.729125220497)) ;
#90433 = CARTESIAN_POINT('Ctrl Pts',(-20.8050925575432,32.3597610355494,123.98120077394)) ;
#90434 = CARTESIAN_POINT('Ctrl Pts',(-20.6865290803088,32.3696481759193,124.212412477173)) ;
#90435 = CARTESIAN_POINT('Ctrl Pts',(-20.5283214706852,32.3796404534553,124.421965720278)) ;
#90436 = CARTESIAN_POINT('Ctrl Pts',(-20.3368987653535,32.3895889967236,124.600050795474)) ;
#90437 = CARTESIAN_POINT('Ctrl Pts',(-20.1179553075885,32.3995256715408,124.742318590014)) ;
#90438 = CARTESIAN_POINT('Ctrl Pts',(-19.8765857645309,32.4095090924772,124.845198491733)) ;
#90439 = CARTESIAN_POINT('Ctrl Pts',(-19.6194540624684,32.4195514076664,124.904530262006)) ;
#90440 = CARTESIAN_POINT('Ctrl Pts',(-19.3612323588906,32.4293917251056,124.918456384701)) ;
#90441 = CARTESIAN_POINT('Ctrl Pts',(-19.0995012622624,32.4394214291631,124.887349726659)) ;
#90442 = CARTESIAN_POINT('Ctrl Pts',(-18.8475761386304,32.4494423858856,124.81065894568)) ;
#90443 = CARTESIAN_POINT('Ctrl Pts',(-18.6160938856141,32.4593089281892,124.693811732837)) ;
#90444 = CARTESIAN_POINT('Ctrl Pts',(-18.4041445829569,32.4693800281344,124.535355939284)) ;
#90445 = CARTESIAN_POINT('Ctrl Pts',(-18.2270297897121,32.4792221023119,124.346861724585)) ;
#90446 = CARTESIAN_POINT('Ctrl Pts',(-18.0828270949522,32.489182896899,124.128411540511)) ;
#90447 = CARTESIAN_POINT('Ctrl Pts',(-17.978420138532,32.4992207697998,123.88617867698)) ;
#90448 = CARTESIAN_POINT('Ctrl Pts',(-17.918171831887,32.5090950553439,123.633750736518)) ;
#90449 = CARTESIAN_POINT('Ctrl Pts',(-17.9023810135821,32.5191648057578,123.369635645094)) ;
#90450 = CARTESIAN_POINT('Ctrl Pts',(-17.9318454096663,32.5289980902925,123.112890613939)) ;
#90451 = CARTESIAN_POINT('Ctrl Pts',(-18.0061909068655,32.5390284310925,122.860013828916)) ;
#90452 = CARTESIAN_POINT('Ctrl Pts',(-18.1240350153628,32.5490603550921,122.624176778822)) ;
#90453 = CARTESIAN_POINT('Ctrl Pts',(-18.2773901023668,32.558888890028,122.416362824848)) ;
#90454 = CARTESIAN_POINT('Ctrl Pts',(-18.4671549519202,32.5688826677927,122.234811814169)) ;
#90455 = CARTESIAN_POINT('Ctrl Pts',(-18.6865982599419,32.5789103782782,122.088899208413)) ;
#90456 = CARTESIAN_POINT('Ctrl Pts',(-18.9245545564035,32.5887987891122,121.984478210373)) ;
#90457 = CARTESIAN_POINT('Ctrl Pts',(-19.179155033595,32.5987756396477,121.921970498854)) ;
#90458 = CARTESIAN_POINT('Ctrl Pts',(-19.4411893341139,32.6087674361982,121.904567510373)) ;
#90459 = CARTESIAN_POINT('Ctrl Pts',(-19.703326580114,32.6188034422919,121.933365758691)) ;
#90460 = CARTESIAN_POINT('Ctrl Pts',(-19.9519587960283,32.6286541765547,122.005505794216)) ;
#90461 = CARTESIAN_POINT('Ctrl Pts',(-20.1877508005523,32.6386454350829,122.120918680607)) ;
#90462 = CARTESIAN_POINT('Ctrl Pts',(-20.3985123625034,32.6485633299861,122.274300781478)) ;
#90463 = CARTESIAN_POINT('Ctrl Pts',(-20.5814614274393,32.6585914716491,122.463947516891)) ;
#90464 = CARTESIAN_POINT('Ctrl Pts',(-20.7267096138185,32.668476639765,122.679326125919)) ;
#90465 = CARTESIAN_POINT('Ctrl Pts',(-20.8340502982722,32.678466003271,122.918892802554)) ;
#90466 = CARTESIAN_POINT('Ctrl Pts',(-20.8979545030379,32.6885071382811,123.174908117759)) ;
#90467 = CARTESIAN_POINT('Ctrl Pts',(-20.9164761609195,32.6983398064691,123.432631238316)) ;
#90468 = CARTESIAN_POINT('Ctrl Pts',(-20.8902807920564,32.7083337094236,123.693949516132)) ;
#90469 = CARTESIAN_POINT('Ctrl Pts',(-20.8183191956796,32.7183629945081,123.947496333409)) ;
#90470 = CARTESIAN_POINT('Ctrl Pts',(-20.7055639452945,32.72823852295,124.181255541168)) ;
#90471 = CARTESIAN_POINT('Ctrl Pts',(-20.5522820009705,32.7382388055661,124.394679958423)) ;
#90472 = CARTESIAN_POINT('Ctrl Pts',(-20.366031988061,32.7481508216231,124.57682210646)) ;
#90473 = CARTESIAN_POINT('Ctrl Pts',(-20.1482437968875,32.7581928969621,124.725815001188)) ;
#90474 = CARTESIAN_POINT('Ctrl Pts',(-19.9112655719754,32.7680927296182,124.8331936985)) ;
#90475 = CARTESIAN_POINT('Ctrl Pts',(-19.65704415951,32.7780851301962,124.898959513189)) ;
#90476 = CARTESIAN_POINT('Ctrl Pts',(-19.3941345542646,32.7881191519556,124.919203661167)) ;
#90477 = CARTESIAN_POINT('Ctrl Pts',(-19.1361107148346,32.7979837627968,124.894256925511)) ;
#90478 = CARTESIAN_POINT('Ctrl Pts',(-18.8829224544705,32.807976162258,124.824605397838)) ;
#90479 = CARTESIAN_POINT('Ctrl Pts',(-18.6449612635533,32.8180081155909,124.711138853319)) ;
#90480 = CARTESIAN_POINT('Ctrl Pts',(-18.4336192368535,32.8278744745325,124.560921747617)) ;
#90481 = CARTESIAN_POINT('Ctrl Pts',(-18.2490612673754,32.8378619500183,124.374355254994)) ;
#90482 = CARTESIAN_POINT('Ctrl Pts',(-18.1001820205622,32.8478068562068,124.159518606616)) ;
#90483 = CARTESIAN_POINT('Ctrl Pts',(-17.9899307415803,32.857851820867,123.919702152225)) ;
#90484 = CARTESIAN_POINT('Ctrl Pts',(-17.9239755325999,32.8677136277719,123.669054864759)) ;
#90485 = CARTESIAN_POINT('Ctrl Pts',(-17.9017602263012,32.8777063000777,123.407426433999)) ;
#90486 = CARTESIAN_POINT('Ctrl Pts',(-17.9251935246742,32.887634971023,123.147548631717)) ;
#90487 = CARTESIAN_POINT('Ctrl Pts',(-17.9931352135227,32.8975875132483,122.895003816011)) ;
#90488 = CARTESIAN_POINT('Ctrl Pts',(-18.1043312287972,32.9075888692442,122.656829799846)) ;
#90489 = CARTESIAN_POINT('Ctrl Pts',(-18.2558767004374,32.9176174815189,122.441233493131)) ;
#90490 = CARTESIAN_POINT('Ctrl Pts',(-18.4392492938704,32.9274818160684,122.257982555295)) ;
#90491 = CARTESIAN_POINT('Ctrl Pts',(-18.6541333399341,32.937474140145,122.107122522269)) ;
#90492 = CARTESIAN_POINT('Ctrl Pts',(-18.8904036310431,32.9474016325109,121.996414241407)) ;
#90493 = CARTESIAN_POINT('Ctrl Pts',(-19.144776160248,32.9574289910617,121.927756331862)) ;
#90494 = CARTESIAN_POINT('Ctrl Pts',(-19.4035634233285,32.9673154091128,121.904356292453)) ;
#90495 = CARTESIAN_POINT('Ctrl Pts',(-19.6662173972518,32.9773471438482,121.926427682475)) ;
#90496 = CARTESIAN_POINT('Ctrl Pts',(-19.9173873207107,32.9872287250915,121.992537401162)) ;
#90497 = CARTESIAN_POINT('Ctrl Pts',(-20.1575155915266,32.9972907031238,122.103143972169)) ;
#90498 = CARTESIAN_POINT('Ctrl Pts',(-20.370483550717,33.0071477814855,122.250663584042)) ;
#90499 = CARTESIAN_POINT('Ctrl Pts',(-20.5574852732715,33.0171423545915,122.435031329392)) ;
#90500 = CARTESIAN_POINT('Ctrl Pts',(-20.7087098909113,33.0270681508791,122.647604267584)) ;
#90501 = CARTESIAN_POINT('Ctrl Pts',(-20.8218893770371,33.0370935180488,122.885487342572)) ;
#90502 = CARTESIAN_POINT('Ctrl Pts',(-20.8912556584646,33.0469895977027,123.136134795138)) ;
#90503 = CARTESIAN_POINT('Ctrl Pts',(-20.9168234356785,33.0569846774083,123.397550614612)) ;
#90504 = CARTESIAN_POINT('Ctrl Pts',(-20.8961029605947,33.0670097652241,123.660183142044)) ;
#90505 = CARTESIAN_POINT('Ctrl Pts',(-20.8098991145045,33.0801935875914,123.99574300305)) ;
#90506 = CARTESIAN_POINT('Ctrl Pts',(-20.6369446858756,33.0935157057373,124.304678709047)) ;
#90507 = CARTESIAN_POINT('Ctrl Pts',(-20.3908204960889,33.1068949153649,124.555834602614)) ;
#90508 = CARTESIAN_POINT('Ctrl Pts',(-20.1809494793358,33.1167331526091,124.706837071298)) ;
#90509 = CARTESIAN_POINT('Ctrl Pts',(-19.942577781835,33.1268060758678,124.821869252031)) ;
#90510 = CARTESIAN_POINT('Ctrl Pts',(-19.693263181732,33.1366627173229,124.892205355517)) ;
#90511 = CARTESIAN_POINT('Ctrl Pts',(-19.4322613230798,33.146648092829,124.919218109963)) ;
#90512 = CARTESIAN_POINT('Ctrl Pts',(-19.0841401970618,33.1599321242894,124.89401589364)) ;
#90513 = CARTESIAN_POINT('Ctrl Pts',(-18.6686887473864,33.1764509161598,124.751538820693)) ;
#90514 = CARTESIAN_POINT('Ctrl Pts',(-18.322123263724,33.1932366331664,124.470796884464)) ;
#90515 = CARTESIAN_POINT('Ctrl Pts',(-18.1195228019478,33.2063497816754,124.191941939277)) ;
#90516 = CARTESIAN_POINT('Ctrl Pts',(-18.0029823657326,33.2163853307556,123.955407109914)) ;
#90517 = CARTESIAN_POINT('Ctrl Pts',(-17.9301367991554,33.226401386935,123.70244375215)) ;
#90518 = CARTESIAN_POINT('Ctrl Pts',(-17.8928038233433,33.239579422801,123.358205398184)) ;
#90519 = CARTESIAN_POINT('Ctrl Pts',(-17.9589484139631,33.2561812999881,122.921862723111)) ;
#90520 = CARTESIAN_POINT('Ctrl Pts',(-18.2153509315473,33.276244444604,122.454328572859)) ;
#90521 = CARTESIAN_POINT('Ctrl Pts',(-18.610517617413,33.2960453346877,122.106659477122)) ;
#90522 = CARTESIAN_POINT('Ctrl Pts',(-19.1034981315604,33.3159884599664,121.912149478104)) ;
#90523 = CARTESIAN_POINT('Ctrl Pts',(-19.6321521720369,33.335886505086,121.897927841427)) ;
#90524 = CARTESIAN_POINT('Ctrl Pts',(-20.1341123261989,33.3557722647127,122.063632571961)) ;
#90525 = CARTESIAN_POINT('Ctrl Pts',(-20.5525339489159,33.3758374398926,122.394216721666)) ;
#90526 = CARTESIAN_POINT('Ctrl Pts',(-20.8296056794486,33.3956640829954,122.842560084467)) ;
#90527 = CARTESIAN_POINT('Ctrl Pts',(-20.9388743874097,33.4155727924438,123.360152546638)) ;
#90528 = CARTESIAN_POINT('Ctrl Pts',(-20.8648847574417,33.4355246294756,123.885402002908)) ;
#90529 = CARTESIAN_POINT('Ctrl Pts',(-20.6147318866576,33.4555331041787,124.35462141048)) ;
#90530 = CARTESIAN_POINT('Ctrl Pts',(-20.2239322170856,33.4753345629402,124.707141469447)) ;
#90531 = CARTESIAN_POINT('Ctrl Pts',(-19.7330000970732,33.4952914511762,124.907967316448)) ;
#90532 = CARTESIAN_POINT('Ctrl Pts',(-19.2022616264228,33.5152752885903,124.92803419319)) ;
#90533 = CARTESIAN_POINT('Ctrl Pts',(-18.7005637331334,33.5350837278112,124.768198422526)) ;
#90534 = CARTESIAN_POINT('Ctrl Pts',(-18.2796383911774,33.5550694371914,124.44444941678)) ;
#90535 = CARTESIAN_POINT('Ctrl Pts',(-17.9957682334727,33.5749389602067,123.998878153294)) ;
#90536 = CARTESIAN_POINT('Ctrl Pts',(-17.8804168309484,33.5949596993239,123.479617978128)) ;
#90537 = CARTESIAN_POINT('Ctrl Pts',(-17.9478193704265,33.6147637643009,122.957391827928)) ;
#90538 = CARTESIAN_POINT('Ctrl Pts',(-18.1922075876265,33.6348257280316,122.483648094758)) ;
#90539 = CARTESIAN_POINT('Ctrl Pts',(-18.5796761414085,33.6546589083201,122.126063706925)) ;
#90540 = CARTESIAN_POINT('Ctrl Pts',(-19.0672471785734,33.6745781056462,121.919993572332)) ;
#90541 = CARTESIAN_POINT('Ctrl Pts',(-19.5964794361335,33.6945161307595,121.892984850209)) ;
#90542 = CARTESIAN_POINT('Ctrl Pts',(-20.1019033803434,33.7143941768156,122.047027331049)) ;
#90543 = CARTESIAN_POINT('Ctrl Pts',(-20.5266212368,33.7343789111036,122.365892503823)) ;
#90544 = CARTESIAN_POINT('Ctrl Pts',(-20.8161596894946,33.7542897277821,122.809038474966)) ;
#90545 = CARTESIAN_POINT('Ctrl Pts',(-20.9372320691971,33.7742887033008,123.326476372936)) ;
#90546 = CARTESIAN_POINT('Ctrl Pts',(-20.8757063920879,33.794093623946,123.849357303765)) ;
#90547 = CARTESIAN_POINT('Ctrl Pts',(-20.6381117871144,33.8140775842373,124.324253054695)) ;
#90548 = CARTESIAN_POINT('Ctrl Pts',(-20.2542831223755,33.8339637879612,124.68776744017)) ;
#90549 = CARTESIAN_POINT('Ctrl Pts',(-19.7682875774795,33.8539129662844,124.899638859617)) ;
#90550 = CARTESIAN_POINT('Ctrl Pts',(-19.2403826918121,33.8738147655239,124.932749323291)) ;
#90551 = CARTESIAN_POINT('Ctrl Pts',(-18.7331049966278,33.8936933705763,124.784958195481)) ;
#90552 = CARTESIAN_POINT('Ctrl Pts',(-18.3035554846274,33.913725730302,124.470321163056)) ;
#90553 = CARTESIAN_POINT('Ctrl Pts',(-18.0587986989934,33.9303074562581,124.103799046386)) ;
#90554 = CARTESIAN_POINT('Ctrl Pts',(-17.9464440989299,33.943501626556,123.775801865132)) ;
#90555 = CARTESIAN_POINT('Ctrl Pts',(-17.891701854277,33.9568138046492,123.430280794334)) ;
#90556 = CARTESIAN_POINT('Ctrl Pts',(-17.937495113229,33.9733799842425,122.992341681738)) ;
#90557 = CARTESIAN_POINT('Ctrl Pts',(-18.1302774467429,33.9900081791027,122.594720028889)) ;
#90558 = CARTESIAN_POINT('Ctrl Pts',(-18.3588197435753,34.0032967608125,122.330608010279)) ;
#90559 = CARTESIAN_POINT('Ctrl Pts',(-18.5618595656554,34.0132650089161,122.165129183368)) ;
#90560 = CARTESIAN_POINT('Ctrl Pts',(-18.7891847096601,34.0231797651722,122.037806845521)) ;
#90561 = CARTESIAN_POINT('Ctrl Pts',(-19.0375192291355,34.0331929158234,121.950759748817)) ;
#90562 = CARTESIAN_POINT('Ctrl Pts',(-19.2972286630396,34.0432056230254,121.908570343025)) ;
#90563 = CARTESIAN_POINT('Ctrl Pts',(-19.6446460039,34.0564249117167,121.912596021897)) ;
#90564 = CARTESIAN_POINT('Ctrl Pts',(-20.0699254705713,34.0730435927147,122.03142792988)) ;
#90565 = CARTESIAN_POINT('Ctrl Pts',(-20.4284671618756,34.0896085004882,122.287092857787)) ;
#90566 = CARTESIAN_POINT('Ctrl Pts',(-20.6522378081821,34.103006972099,122.558923682417)) ;
#90567 = CARTESIAN_POINT('Ctrl Pts',(-20.779673548747,34.112848227586,122.78398886291)) ;
#90568 = CARTESIAN_POINT('Ctrl Pts',(-20.8678897526762,34.1228345431742,123.031102300472)) ;
#90569 = CARTESIAN_POINT('Ctrl Pts',(-20.9117788511624,34.1327711507606,123.288555336312)) ;
#90570 = CARTESIAN_POINT('Ctrl Pts',(-20.9101514532125,34.1428210181289,123.552623293535)) ;
#90571 = CARTESIAN_POINT('Ctrl Pts',(-20.863821952132,34.1526715128037,123.807324091934)) ;
#90572 = CARTESIAN_POINT('Ctrl Pts',(-20.7735256213535,34.1626433131982,124.053287870522)) ;
#90573 = CARTESIAN_POINT('Ctrl Pts',(-20.6415098394546,34.172639280224,124.280439245738)) ;
#90574 = CARTESIAN_POINT('Ctrl Pts',(-20.4711254085416,34.1826767396052,124.481765931649)) ;
#90575 = CARTESIAN_POINT('Ctrl Pts',(-20.2726263760509,34.1925174405059,124.647547741897)) ;
#90576 = CARTESIAN_POINT('Ctrl Pts',(-20.0438538007464,34.2025654617733,124.779381747442)) ;
#90577 = CARTESIAN_POINT('Ctrl Pts',(-19.7979948387222,34.212512854856,124.868199817644)) ;
#90578 = CARTESIAN_POINT('Ctrl Pts',(-19.5415398597008,34.2224230009024,124.913598266864)) ;
#90579 = CARTESIAN_POINT('Ctrl Pts',(-19.2772295562355,34.232481914752,124.913481740672)) ;
#90580 = CARTESIAN_POINT('Ctrl Pts',(-19.0224749494035,34.2423226850413,124.868818922004)) ;
#90581 = CARTESIAN_POINT('Ctrl Pts',(-18.7738170634932,34.2523855546199,124.778924498811)) ;
#90582 = CARTESIAN_POINT('Ctrl Pts',(-18.5484380725391,34.2622798777504,124.649212333765)) ;
#90583 = CARTESIAN_POINT('Ctrl Pts',(-18.3476405758638,34.2722216848449,124.482118201079)) ;
#90584 = CARTESIAN_POINT('Ctrl Pts',(-18.1777564580938,34.2822241958002,124.281491322928)) ;
#90585 = CARTESIAN_POINT('Ctrl Pts',(-18.0452449011872,34.2922589166186,124.053519923631)) ;
#90586 = CARTESIAN_POINT('Ctrl Pts',(-17.9556349074693,34.3021040941243,123.810796881849)) ;
#90587 = CARTESIAN_POINT('Ctrl Pts',(-17.9083784162444,34.3120888545254,123.552736052031)) ;
#90588 = CARTESIAN_POINT('Ctrl Pts',(-17.9065296697451,34.3220277608418,123.291519123483)) ;
#90589 = CARTESIAN_POINT('Ctrl Pts',(-17.9505964036269,34.3320699884775,123.031352463089)) ;
#90590 = CARTESIAN_POINT('Ctrl Pts',(-18.037624931531,34.3419552000619,122.786560063066)) ;
#90591 = CARTESIAN_POINT('Ctrl Pts',(-18.1669823934787,34.3519541302638,122.557890019545)) ;
#90592 = CARTESIAN_POINT('Ctrl Pts',(-18.3326161325234,34.3618715531743,122.356617211244)) ;
#90593 = CARTESIAN_POINT('Ctrl Pts',(-18.5332582552476,34.371919485253,122.185024436481)) ;
#90594 = CARTESIAN_POINT('Ctrl Pts',(-18.7567288565943,34.3817968610624,122.052891702144)) ;
#90595 = CARTESIAN_POINT('Ctrl Pts',(-19.0039582074564,34.3918507542303,121.959841830907)) ;
#90596 = CARTESIAN_POINT('Ctrl Pts',(-19.2595239194454,34.4017443774836,121.911772148145)) ;
#90597 = CARTESIAN_POINT('Ctrl Pts',(-19.5238983005659,34.4118069711066,121.908716657906)) ;
#90598 = CARTESIAN_POINT('Ctrl Pts',(-19.7791766052678,34.4216495450957,121.950552116811)) ;
#90599 = CARTESIAN_POINT('Ctrl Pts',(-20.0271336820024,34.4316403019786,122.036751836133)) ;
#90600 = CARTESIAN_POINT('Ctrl Pts',(-20.254936747224,34.4415683637365,122.163955290834)) ;
#90601 = CARTESIAN_POINT('Ctrl Pts',(-20.4586999823896,34.4515563396257,122.329419432095)) ;
#90602 = CARTESIAN_POINT('Ctrl Pts',(-20.6311135230344,34.4615920039821,122.528971921844)) ;
#90603 = CARTESIAN_POINT('Ctrl Pts',(-20.7641991432005,34.4714479424018,122.751184316972)) ;
#90604 = CARTESIAN_POINT('Ctrl Pts',(-20.8583766148853,34.4814434337987,122.996362053338)) ;
#90605 = CARTESIAN_POINT('Ctrl Pts',(-20.9082075537525,34.4913532387521,123.251982490847)) ;
#90606 = CARTESIAN_POINT('Ctrl Pts',(-20.9133731041675,34.5013654610189,123.515048494353)) ;
#90607 = CARTESIAN_POINT('Ctrl Pts',(-20.8722117287927,34.5113933417117,123.775338285339)) ;
#90608 = CARTESIAN_POINT('Ctrl Pts',(-20.7883656546394,34.5212497376943,124.020406248148)) ;
#90609 = CARTESIAN_POINT('Ctrl Pts',(-20.6615835386418,34.5312745348743,124.251337874107)) ;
#90610 = CARTESIAN_POINT('Ctrl Pts',(-20.4960213753757,34.5413054648581,124.456471359235)) ;
#90611 = CARTESIAN_POINT('Ctrl Pts',(-20.3013678063014,34.5511500673668,124.626861391942)) ;
#90612 = CARTESIAN_POINT('Ctrl Pts',(-20.0771540029309,34.5611409185909,124.763475181664)) ;
#90613 = CARTESIAN_POINT('Ctrl Pts',(-19.8312684979688,34.5711787516021,124.858978848205)) ;
#90614 = CARTESIAN_POINT('Ctrl Pts',(-19.577597721108,34.5810231400675,124.909794407279)) ;
#90615 = CARTESIAN_POINT('Ctrl Pts',(-19.3153254135936,34.5910079444371,124.916395570921)) ;
#90616 = CARTESIAN_POINT('Ctrl Pts',(-19.0569804860377,34.6009474639199,124.87763585839)) ;
#90617 = CARTESIAN_POINT('Ctrl Pts',(-18.806866607614,34.6109871949213,124.793729916711)) ;
#90618 = CARTESIAN_POINT('Ctrl Pts',(-18.5785256075441,34.6208753231676,124.669671687923)) ;
#90619 = CARTESIAN_POINT('Ctrl Pts',(-18.3728209709373,34.6308650483761,124.506586268412)) ;
#90620 = CARTESIAN_POINT('Ctrl Pts',(-18.1992525056931,34.6408228130776,124.31075898755)) ;
#90621 = CARTESIAN_POINT('Ctrl Pts',(-18.0625580666762,34.6507251544896,124.089319343284)) ;
#90622 = CARTESIAN_POINT('Ctrl Pts',(-17.9650433992383,34.660769350196,123.844056094203)) ;
#90623 = CARTESIAN_POINT('Ctrl Pts',(-17.9122901221407,34.6706767509553,123.589085907757)) ;
#90624 = CARTESIAN_POINT('Ctrl Pts',(-17.9040671219944,34.6806873508296,123.326142620746)) ;
#90625 = CARTESIAN_POINT('Ctrl Pts',(-17.942203265216,34.6907176467418,123.065322697016)) ;
#90626 = CARTESIAN_POINT('Ctrl Pts',(-18.0232493114111,34.7005724263915,122.819373677744)) ;
#90627 = CARTESIAN_POINT('Ctrl Pts',(-18.1463519672124,34.710529754609,122.588461269854)) ;
#90628 = CARTESIAN_POINT('Ctrl Pts',(-18.309353042108,34.7205687875159,122.381049743484)) ;
#90629 = CARTESIAN_POINT('Ctrl Pts',(-18.5023659383517,34.7304418994052,122.207599723295)) ;
#90630 = CARTESIAN_POINT('Ctrl Pts',(-18.7269874138073,34.7405151844323,122.06763353317)) ;
#90631 = CARTESIAN_POINT('Ctrl Pts',(-18.966311174259,34.7503355041691,121.970921603636)) ;
#90632 = CARTESIAN_POINT('Ctrl Pts',(-19.2252615250139,34.7604141695475,121.915607928114)) ;
#90633 = CARTESIAN_POINT('Ctrl Pts',(-19.4840428530472,34.7702657600313,121.906215757302)) ;
#90634 = CARTESIAN_POINT('Ctrl Pts',(-19.7462130095486,34.7803389103502,121.942457891797)) ;
#90635 = CARTESIAN_POINT('Ctrl Pts',(-19.9923964312408,34.7901812903253,122.021867293698)) ;
#90636 = CARTESIAN_POINT('Ctrl Pts',(-20.224633402004,34.8001622665683,122.143734711503)) ;
#90637 = CARTESIAN_POINT('Ctrl Pts',(-20.4326722972678,34.8101785949236,122.305014175264)) ;
#90638 = CARTESIAN_POINT('Ctrl Pts',(-20.6076836467507,34.8200763919147,122.497420427446)) ;
#90639 = CARTESIAN_POINT('Ctrl Pts',(-20.7486352078836,34.8300889486468,122.719624524635)) ;
#90640 = CARTESIAN_POINT('Ctrl Pts',(-20.8484693509522,34.8401209834933,122.963608083388)) ;
#90641 = CARTESIAN_POINT('Ctrl Pts',(-20.9039852822509,34.8499603843087,123.216169118791)) ;
#90642 = CARTESIAN_POINT('Ctrl Pts',(-20.915252015336,34.8600261699603,123.480416453755)) ;
#90643 = CARTESIAN_POINT('Ctrl Pts',(-20.8809428954112,34.8699166250749,123.738080890662)) ;
#90644 = CARTESIAN_POINT('Ctrl Pts',(-20.8021590268459,34.8799087437107,123.988551842107)) ;
#90645 = CARTESIAN_POINT('Ctrl Pts',(-20.6812162451853,34.8898715704737,124.220748500845)) ;
#90646 = CARTESIAN_POINT('Ctrl Pts',(-20.5232363311893,34.8997758537466,124.427621791333)) ;
#90647 = CARTESIAN_POINT('Ctrl Pts',(-20.328602748606,34.9098362876937,124.606497029424)) ;
#90648 = CARTESIAN_POINT('Ctrl Pts',(-20.1108581510111,34.9196768403669,124.746063981003)) ;
#90649 = CARTESIAN_POINT('Ctrl Pts',(-19.8670007279919,34.9297390603126,124.848234310547)) ;
#90650 = CARTESIAN_POINT('Ctrl Pts',(-19.6132374871759,34.9396361995912,124.9052994767)) ;
#90651 = CARTESIAN_POINT('Ctrl Pts',(-19.352586866818,34.9495673917262,124.918345206172)) ;
#90652 = CARTESIAN_POINT('Ctrl Pts',(-19.0907761598874,34.9596095463713,124.885281266899)) ;
#90653 = CARTESIAN_POINT('Ctrl Pts',(-18.8424935087745,34.9694963073906,124.808663455936)) ;
#90654 = CARTESIAN_POINT('Ctrl Pts',(-18.6085514013706,34.9794956091078,124.689074670539)) ;
#90655 = CARTESIAN_POINT('Ctrl Pts',(-18.4004100503073,34.9894164072746,124.532024155764)) ;
#90656 = CARTESIAN_POINT('Ctrl Pts',(-18.220695374879,34.9994504608713,124.339108184459)) ;
#90657 = CARTESIAN_POINT('Ctrl Pts',(-18.0786234259347,35.0093735784377,124.120391230864)) ;
#90658 = CARTESIAN_POINT('Ctrl Pts',(-17.9753990929057,35.0194297019368,123.877150159267)) ;
#90659 = CARTESIAN_POINT('Ctrl Pts',(-17.917104068257,35.0292751435917,123.62506345845)) ;
#90660 = CARTESIAN_POINT('Ctrl Pts',(-17.9024452588224,35.0392374447158,123.36369174523)) ;
#90661 = CARTESIAN_POINT('Ctrl Pts',(-17.933946461117,35.0492659239909,123.102025569632)) ;
#90662 = CARTESIAN_POINT('Ctrl Pts',(-18.0094085575674,35.0591762775006,122.852777323591)) ;
#90663 = CARTESIAN_POINT('Ctrl Pts',(-18.1266927602278,35.0691111496778,122.619516835167)) ;
#90664 = CARTESIAN_POINT('Ctrl Pts',(-18.2845521812503,35.0791522872635,122.408084929037)) ;
#90665 = CARTESIAN_POINT('Ctrl Pts',(-18.4736704054688,35.0890394364781,122.22989810543)) ;
#90666 = CARTESIAN_POINT('Ctrl Pts',(-18.6928945527343,35.0990316712291,122.085390254205)) ;
#90667 = CARTESIAN_POINT('Ctrl Pts',(-18.932889746988,35.1089803767921,121.9816540539)) ;
#90668 = CARTESIAN_POINT('Ctrl Pts',(-19.1868087710443,35.1189164452158,121.92087877605)) ;
#90669 = CARTESIAN_POINT('Ctrl Pts',(-19.4487510389459,35.1289021294316,121.904734357307)) ;
#90670 = CARTESIAN_POINT('Ctrl Pts',(-19.7108597155161,35.1389425560002,121.934890399688)) ;
#90671 = CARTESIAN_POINT('Ctrl Pts',(-19.9588218803458,35.148781669464,122.008182230702)) ;
#90672 = CARTESIAN_POINT('Ctrl Pts',(-20.195037968623,35.1588114036398,122.125114451366)) ;
#90673 = CARTESIAN_POINT('Ctrl Pts',(-20.4067898564085,35.1688335031457,122.281715086655)) ;
#90674 = CARTESIAN_POINT('Ctrl Pts',(-20.5858406931206,35.1787019430391,122.46934344386)) ;
#90675 = CARTESIAN_POINT('Ctrl Pts',(-20.7324825930465,35.1887708077248,122.689561854867)) ;
#90676 = CARTESIAN_POINT('Ctrl Pts',(-20.8362960938539,35.1986134808234,122.926479912635)) ;
#90677 = CARTESIAN_POINT('Ctrl Pts',(-20.899055079425,35.2085741149858,123.180594616481)) ;
#90678 = CARTESIAN_POINT('Ctrl Pts',(-20.9163568869125,35.2186120306639,123.44380305098)) ;
#90679 = CARTESIAN_POINT('Ctrl Pts',(-20.8886337721967,35.2284863055234,123.701836099716)) ;
#90680 = CARTESIAN_POINT('Ctrl Pts',(-20.815106074293,35.2385560558985,123.956001024207)) ;
#90681 = CARTESIAN_POINT('Ctrl Pts',(-20.701400325098,35.248389351273,124.188072701268)) ;
#90682 = CARTESIAN_POINT('Ctrl Pts',(-20.5466987675831,35.2584196487526,124.401475805769)) ;
#90683 = CARTESIAN_POINT('Ctrl Pts',(-20.3567063540923,35.2684517351941,124.584263100217)) ;
#90684 = CARTESIAN_POINT('Ctrl Pts',(-20.1426513521819,35.278279663683,124.72875221101)) ;
#90685 = CARTESIAN_POINT('Ctrl Pts',(-19.9030046171071,35.2882757047938,124.836324512499)) ;
#90686 = CARTESIAN_POINT('Ctrl Pts',(-19.6474276615906,35.298301516895,124.900352262788)) ;
#90687 = CARTESIAN_POINT('Ctrl Pts',(-19.3882751938659,35.3081887517898,124.919108279541)) ;
#90688 = CARTESIAN_POINT('Ctrl Pts',(-19.1274391236298,35.3181656180008,124.892776277121)) ;
#90689 = CARTESIAN_POINT('Ctrl Pts',(-18.8746646646945,35.3281585618726,124.821468377364)) ;
#90690 = CARTESIAN_POINT('Ctrl Pts',(-18.6372430900327,35.338196484544,124.706562893995)) ;
#90691 = CARTESIAN_POINT('Ctrl Pts',(-18.4271550056594,35.3480449488057,124.555385469111)) ;
#90692 = CARTESIAN_POINT('Ctrl Pts',(-18.2435829818069,35.3580368155497,124.367696236912)) ;
#90693 = CARTESIAN_POINT('Ctrl Pts',(-18.0963252747795,35.3679545475909,124.152615497661)) ;
#90694 = CARTESIAN_POINT('Ctrl Pts',(-17.9874096726993,35.3779827324862,123.912669454081)) ;
#90695 = CARTESIAN_POINT('Ctrl Pts',(-17.9226347534564,35.387867890535,123.66109622289)) ;
#90696 = CARTESIAN_POINT('Ctrl Pts',(-17.9016765666423,35.3978572510767,123.39941901094)) ;
#90697 = CARTESIAN_POINT('Ctrl Pts',(-17.9271558083283,35.4078984080111,123.136781335397)) ;
#90698 = CARTESIAN_POINT('Ctrl Pts',(-17.9959687525466,35.4177309914662,122.88772650032)) ;
#90699 = CARTESIAN_POINT('Ctrl Pts',(-18.1081319471754,35.4277252114282,122.650247800051)) ;
#90700 = CARTESIAN_POINT('Ctrl Pts',(-18.2607849253877,35.4377533132155,122.435427774985)) ;
#90701 = CARTESIAN_POINT('Ctrl Pts',(-18.4453853520115,35.4476332578386,122.252848690864)) ;
#90702 = CARTESIAN_POINT('Ctrl Pts',(-18.6610214269731,35.4576235843956,122.103123520847)) ;
#90703 = CARTESIAN_POINT('Ctrl Pts',(-18.8982196683709,35.4675645160499,121.993647605999)) ;
#90704 = CARTESIAN_POINT('Ctrl Pts',(-19.1519136468404,35.4775516345528,121.926344805637)) ;
#90705 = CARTESIAN_POINT('Ctrl Pts',(-19.4146479680384,35.48758496745,121.904428438846)) ;
#90706 = CARTESIAN_POINT('Ctrl Pts',(-19.6729148068661,35.4974510718947,121.927562236653)) ;
#90707 = CARTESIAN_POINT('Ctrl Pts',(-19.9282737618614,35.5075171857751,121.996483449793)) ;
#90708 = CARTESIAN_POINT('Ctrl Pts',(-20.1628377208178,35.5173731975435,122.106361679407)) ;
#90709 = CARTESIAN_POINT('Ctrl Pts',(-20.3781660934209,35.5273679011748,122.256744946492)) ;
#90710 = CARTESIAN_POINT('Ctrl Pts',(-20.5644031071723,35.5373992368997,122.443319308297)) ;
#90711 = CARTESIAN_POINT('Ctrl Pts',(-20.7132753997824,35.5472657621033,122.655613795221)) ;
#90712 = CARTESIAN_POINT('Ctrl Pts',(-20.824735991116,35.5572531901491,122.893195278124)) ;
#90713 = CARTESIAN_POINT('Ctrl Pts',(-20.8931143715501,35.5671981198355,123.145473611636)) ;
#90714 = CARTESIAN_POINT('Ctrl Pts',(-20.916731989703,35.5772430379441,123.408359549251)) ;
#90715 = CARTESIAN_POINT('Ctrl Pts',(-20.8949804435051,35.587105007558,123.66662867698)) ;
#90716 = CARTESIAN_POINT('Ctrl Pts',(-20.8283478671713,35.5970970755792,123.920587710675)) ;
#90717 = CARTESIAN_POINT('Ctrl Pts',(-20.719243324381,35.6070280009538,124.157679141684)) ;
#90718 = CARTESIAN_POINT('Ctrl Pts',(-20.5707147508326,35.6169786291772,124.372871095378)) ;
#90719 = CARTESIAN_POINT('Ctrl Pts',(-20.3862369565019,35.6269788682363,124.560073078809)) ;
#90720 = CARTESIAN_POINT('Ctrl Pts',(-20.1712640574126,35.6370073236055,124.712497104667)) ;
#90721 = CARTESIAN_POINT('Ctrl Pts',(-19.9370958263856,35.6468733581888,124.823815964018)) ;
#90722 = CARTESIAN_POINT('Ctrl Pts',(-19.6841078343026,35.6568656799362,124.894073754451)) ;
#90723 = CARTESIAN_POINT('Ctrl Pts',(-19.4242931282444,35.6667979696132,124.919232541197)) ;
#90724 = CARTESIAN_POINT('Ctrl Pts',(-19.1622457507477,35.676799614584,124.89901214049)) ;
#90725 = CARTESIAN_POINT('Ctrl Pts',(-18.8234350299955,35.690112248,124.811793581749)) ;
#90726 = CARTESIAN_POINT('Ctrl Pts',(-18.5168964604078,35.7033439973816,124.639445590766)) ;
#90727 = CARTESIAN_POINT('Ctrl Pts',(-18.2664225908945,35.7166672621986,124.394805388771)) ;
#90728 = CARTESIAN_POINT('Ctrl Pts',(-18.1147450135693,35.7265429684163,124.184207203932)) ;
#90729 = CARTESIAN_POINT('Ctrl Pts',(-18.0003454842561,35.7365325595163,123.947960343234)) ;
#90730 = CARTESIAN_POINT('Ctrl Pts',(-17.9289701667244,35.7464596559717,123.697008534527)) ;
#90731 = CARTESIAN_POINT('Ctrl Pts',(-17.9019627690378,35.7564848044763,123.434969684401)) ;
#90732 = CARTESIAN_POINT('Ctrl Pts',(-17.9204625057985,35.766380458623,123.175558526549)) ;
#90733 = CARTESIAN_POINT('Ctrl Pts',(-17.9840399510721,35.7763839930012,122.920505986074)) ;
#90734 = CARTESIAN_POINT('Ctrl Pts',(-18.0907912526402,35.7863691314413,122.680759611974)) ;
#90735 = CARTESIAN_POINT('Ctrl Pts',(-18.2384845563749,35.7964050560366,122.462276828214)) ;
#90736 = CARTESIAN_POINT('Ctrl Pts',(-18.4182832581623,35.8062563314643,122.276022071899)) ;
#90737 = CARTESIAN_POINT('Ctrl Pts',(-18.6302545916797,35.8162485926257,122.121024656498)) ;
#90738 = CARTESIAN_POINT('Ctrl Pts',(-18.8673155093982,35.8262884766433,122.005244450248)) ;
#90739 = CARTESIAN_POINT('Ctrl Pts',(-19.1155599860478,35.8361232511457,121.93323039927)) ;
#90740 = CARTESIAN_POINT('Ctrl Pts',(-19.3787662820051,35.846199632166,121.90464170685)) ;
#90741 = CARTESIAN_POINT('Ctrl Pts',(-19.6369856027935,35.8560459053166,121.921721200336)) ;
#90742 = CARTESIAN_POINT('Ctrl Pts',(-19.9782318745606,35.8694104266019,122.004755386422)) ;
#90743 = CARTESIAN_POINT('Ctrl Pts',(-20.2860781894191,35.8826166710363,122.173358222392)) ;
#90744 = CARTESIAN_POINT('Ctrl Pts',(-20.5388194305417,35.8958816257135,122.413415383819)) ;
#90745 = CARTESIAN_POINT('Ctrl Pts',(-20.6954518663001,35.9059139062652,122.625487616004)) ;
#90746 = CARTESIAN_POINT('Ctrl Pts',(-20.8114494728934,35.9158226397831,122.858608403369)) ;
#90747 = CARTESIAN_POINT('Ctrl Pts',(-20.8860782708486,35.9257601906506,123.108875396054)) ;
#90748 = CARTESIAN_POINT('Ctrl Pts',(-20.9161752733181,35.9357900382445,123.370700554843)) ;
#90749 = CARTESIAN_POINT('Ctrl Pts',(-20.8957731929268,35.949025178165,123.717991080168)) ;
#90750 = CARTESIAN_POINT('Ctrl Pts',(-20.7562782646861,35.9656936425361,124.138331425498)) ;
#90751 = CARTESIAN_POINT('Ctrl Pts',(-20.4290918169683,35.98556465441,124.553143935095)) ;
#90752 = CARTESIAN_POINT('Ctrl Pts',(-20.0516669376428,36.002271738793,124.786848654509)) ;
#90753 = CARTESIAN_POINT('Ctrl Pts',(-19.7200488034031,36.0154490201036,124.886772678737)) ;
#90754 = CARTESIAN_POINT('Ctrl Pts',(-19.3739896601812,36.0287164806177,124.929104605177)) ;
#90755 = CARTESIAN_POINT('Ctrl Pts',(-18.9367256618785,36.0453303713049,124.867571649377)) ;
#90756 = CARTESIAN_POINT('Ctrl Pts',(-18.4683585867537,36.0652791707323,124.618963683723)) ;
#90757 = CARTESIAN_POINT('Ctrl Pts',(-18.1135879764182,36.0852002822632,124.2260271695)) ;
#90758 = CARTESIAN_POINT('Ctrl Pts',(-17.9136719684102,36.1050667304361,123.737230065052)) ;
#90759 = CARTESIAN_POINT('Ctrl Pts',(-17.8927126209991,36.1250930770532,123.205433374261)) ;
#90760 = CARTESIAN_POINT('Ctrl Pts',(-18.0533007215964,36.1449551214427,122.702455916173)) ;
#90761 = CARTESIAN_POINT('Ctrl Pts',(-18.3764776353452,36.1649004241238,122.282339628229)) ;
#90762 = CARTESIAN_POINT('Ctrl Pts',(-18.8226158877263,36.1847957311827,121.998462474444)) ;
#90763 = CARTESIAN_POINT('Ctrl Pts',(-19.3385842783177,36.2046890013503,121.882951679264)) ;
#90764 = CARTESIAN_POINT('Ctrl Pts',(-19.8648495105545,36.2246545940308,121.950798037064)) ;
#90765 = CARTESIAN_POINT('Ctrl Pts',(-20.334465653922,36.2445299177156,122.192756268591)) ;
#90766 = CARTESIAN_POINT('Ctrl Pts',(-20.6955169132806,36.2645049802905,122.582020760569)) ;
#90767 = CARTESIAN_POINT('Ctrl Pts',(-20.9010738348726,36.2844573899217,123.070861900805)) ;
#90768 = CARTESIAN_POINT('Ctrl Pts',(-20.9283436001929,36.3042934441578,123.597363126459)) ;
#90769 = CARTESIAN_POINT('Ctrl Pts',(-20.7737705212242,36.3242713555753,124.10534582472)) ;
#90770 = CARTESIAN_POINT('Ctrl Pts',(-20.4556033727974,36.3441894050788,124.528410951894)) ;
#90771 = CARTESIAN_POINT('Ctrl Pts',(-20.0139153720363,36.3640575488469,124.818025234808)) ;
#90772 = CARTESIAN_POINT('Ctrl Pts',(-19.4952301669597,36.3841084054342,124.939796977761)) ;
#90773 = CARTESIAN_POINT('Ctrl Pts',(-18.9729215440468,36.4038888418901,124.878628473693)) ;
#90774 = CARTESIAN_POINT('Ctrl Pts',(-18.4967651240595,36.4239188975679,124.640802577976)) ;
#90775 = CARTESIAN_POINT('Ctrl Pts',(-18.1335848516454,36.4438000027427,124.25686352696)) ;
#90776 = CARTESIAN_POINT('Ctrl Pts',(-17.9219195474901,36.4636804651105,123.77277946085)) ;
#90777 = CARTESIAN_POINT('Ctrl Pts',(-17.8881151233781,36.4836656122549,123.242666380459)) ;
#90778 = CARTESIAN_POINT('Ctrl Pts',(-18.0366553794252,36.5035561907912,122.73529278596)) ;
#90779 = CARTESIAN_POINT('Ctrl Pts',(-18.3487072158258,36.5234502106656,122.308453160384)) ;
#90780 = CARTESIAN_POINT('Ctrl Pts',(-18.7881486981132,36.543371655392,122.013243316393)) ;
#90781 = CARTESIAN_POINT('Ctrl Pts',(-19.3013483876729,36.5632697934474,121.884892286894)) ;
#90782 = CARTESIAN_POINT('Ctrl Pts',(-19.8317595038524,36.5833405486635,121.940839429391)) ;
#90783 = CARTESIAN_POINT('Ctrl Pts',(-20.3047244450388,36.6031260987147,122.170976388332)) ;
#90784 = CARTESIAN_POINT('Ctrl Pts',(-20.6751961018729,36.6231091735921,122.551414789717)) ;
#90785 = CARTESIAN_POINT('Ctrl Pts',(-20.8920876251874,36.643018256238,123.034079238211)) ;
#90786 = CARTESIAN_POINT('Ctrl Pts',(-20.9326736949197,36.6628768153608,123.560393777446)) ;
#90787 = CARTESIAN_POINT('Ctrl Pts',(-20.7893507745121,36.6829202591995,124.073361851782)) ;
#90788 = CARTESIAN_POINT('Ctrl Pts',(-20.5344135959182,36.6994203239287,124.430349947457)) ;
#90789 = CARTESIAN_POINT('Ctrl Pts',(-20.2630412458369,36.7128100637776,124.654248532504)) ;
#90790 = CARTESIAN_POINT('Ctrl Pts',(-20.0376657911243,36.722666964986,124.781998493706)) ;
#90791 = CARTESIAN_POINT('Ctrl Pts',(-19.790451891043,36.7326584908325,124.870339079412)) ;
#90792 = CARTESIAN_POINT('Ctrl Pts',(-19.5333205208731,36.7425831712835,124.914226210988)) ;
#90793 = CARTESIAN_POINT('Ctrl Pts',(-19.2702961550599,36.7525937613279,124.912889798325)) ;
#90794 = CARTESIAN_POINT('Ctrl Pts',(-18.9272992756477,36.7658530220315,124.851022900053)) ;
#90795 = CARTESIAN_POINT('Ctrl Pts',(-18.6064416437255,36.7792040971818,124.699737523157)) ;
#90796 = CARTESIAN_POINT('Ctrl Pts',(-18.3413179144251,36.7924104064166,124.475682143339)) ;
#90797 = CARTESIAN_POINT('Ctrl Pts',(-18.1729500479038,36.8023972400069,124.274423037726)) ;
#90798 = CARTESIAN_POINT('Ctrl Pts',(-18.0423739740692,36.812349967503,124.047750299169)) ;
#90799 = CARTESIAN_POINT('Ctrl Pts',(-17.952518013425,36.8223980643446,123.799486638763)) ;
#90800 = CARTESIAN_POINT('Ctrl Pts',(-17.907757267272,36.8322395212164,123.544740945739)) ;
#90801 = CARTESIAN_POINT('Ctrl Pts',(-17.9073502062391,36.8422257881299,123.282355578864)) ;
#90802 = CARTESIAN_POINT('Ctrl Pts',(-17.9521694205823,36.8521623890303,123.025063136411)) ;
#90803 = CARTESIAN_POINT('Ctrl Pts',(-18.0420963058471,36.8622123318174,122.776771029239)) ;
#90804 = CARTESIAN_POINT('Ctrl Pts',(-18.1710052785227,36.8720625315031,122.552279193621)) ;
#90805 = CARTESIAN_POINT('Ctrl Pts',(-18.3384408575299,36.8820354364352,122.350698607091)) ;
#90806 = CARTESIAN_POINT('Ctrl Pts',(-18.5389463808558,36.8920338109148,122.18084427361)) ;
#90807 = CARTESIAN_POINT('Ctrl Pts',(-18.7664541058527,36.9020539847848,122.048279786072)) ;
#90808 = CARTESIAN_POINT('Ctrl Pts',(-19.0105222002321,36.9119550287268,121.95809778858)) ;
#90809 = CARTESIAN_POINT('Ctrl Pts',(-19.268728383313,36.9219438324511,121.910847088745)) ;
#90810 = CARTESIAN_POINT('Ctrl Pts',(-19.5305939085291,36.9319092992829,121.909337770446)) ;
#90811 = CARTESIAN_POINT('Ctrl Pts',(-19.7872824216961,36.9418128615559,121.95243202349)) ;
#90812 = CARTESIAN_POINT('Ctrl Pts',(-20.0363517848326,36.9518735394339,122.041006819332)) ;
#90813 = CARTESIAN_POINT('Ctrl Pts',(-20.2614482794892,36.9617138373834,122.1683698474)) ;
#90814 = CARTESIAN_POINT('Ctrl Pts',(-20.4656746860891,36.9717768322928,122.336311677907)) ;
#90815 = CARTESIAN_POINT('Ctrl Pts',(-20.6346325844978,36.9816711264399,122.533982970242)) ;
#90816 = CARTESIAN_POINT('Ctrl Pts',(-20.7679155889213,36.9916129241368,122.758650934849)) ;
#90817 = CARTESIAN_POINT('Ctrl Pts',(-20.8608421966797,37.0016155016659,123.004571300072)) ;
#90818 = CARTESIAN_POINT('Ctrl Pts',(-20.9094048501918,37.011649965587,123.26374268831)) ;
#90819 = CARTESIAN_POINT('Ctrl Pts',(-20.9125815920894,37.0214961041081,123.522477689503)) ;
#90820 = CARTESIAN_POINT('Ctrl Pts',(-20.8707936127288,37.0314772773451,123.781401079755)) ;
#90821 = CARTESIAN_POINT('Ctrl Pts',(-20.7848638119868,37.0414295713023,124.028425816195)) ;
#90822 = CARTESIAN_POINT('Ctrl Pts',(-20.6570438981956,37.0514283664369,124.258022088148)) ;
#90823 = CARTESIAN_POINT('Ctrl Pts',(-20.4902612991329,37.0614674746977,124.462411340172)) ;
#90824 = CARTESIAN_POINT('Ctrl Pts',(-20.2951235539568,37.0712924161369,124.631500866346)) ;
#90825 = CARTESIAN_POINT('Ctrl Pts',(-20.0686616200432,37.0813471032113,124.767597084672)) ;
#90826 = CARTESIAN_POINT('Ctrl Pts',(-19.8245710827869,37.0912899081514,124.860842297865)) ;
#90827 = CARTESIAN_POINT('Ctrl Pts',(-19.5691588004271,37.1011936941479,124.910878499083)) ;
#90828 = CARTESIAN_POINT('Ctrl Pts',(-19.3052063233042,37.1112405107127,124.915717087351)) ;
#90829 = CARTESIAN_POINT('Ctrl Pts',(-19.0482495106725,37.1211360301914,124.875491392646)) ;
#90830 = CARTESIAN_POINT('Ctrl Pts',(-18.7981148297119,37.1311981155158,124.789869782215)) ;
#90831 = CARTESIAN_POINT('Ctrl Pts',(-18.5715632075335,37.1410408264737,124.664999559399)) ;
#90832 = CARTESIAN_POINT('Ctrl Pts',(-18.3667645398744,37.1510315437798,124.500772902301)) ;
#90833 = CARTESIAN_POINT('Ctrl Pts',(-18.1946815226206,37.1609596268764,124.304654257152)) ;
#90834 = CARTESIAN_POINT('Ctrl Pts',(-18.0580587042926,37.1709475569881,124.080530224495)) ;
#90835 = CARTESIAN_POINT('Ctrl Pts',(-17.9623882859192,37.1809833831154,123.834772735687)) ;
#90836 = CARTESIAN_POINT('Ctrl Pts',(-17.9113591892937,37.190838720229,123.580846703996)) ;
#90837 = CARTESIAN_POINT('Ctrl Pts',(-17.9046918793828,37.2008364550792,123.318229679078)) ;
#90838 = CARTESIAN_POINT('Ctrl Pts',(-17.9432929783789,37.2107443590637,123.060725439739)) ;
#90839 = CARTESIAN_POINT('Ctrl Pts',(-18.0264609446868,37.2207554336121,122.811128639324)) ;
#90840 = CARTESIAN_POINT('Ctrl Pts',(-18.1523845768401,37.2307832891477,122.579637946315)) ;
#90841 = CARTESIAN_POINT('Ctrl Pts',(-18.313434602913,37.240640883053,122.376742009224)) ;
#90842 = CARTESIAN_POINT('Ctrl Pts',(-18.510241481172,37.2506675698911,122.201537057415)) ;
#90843 = CARTESIAN_POINT('Ctrl Pts',(-18.7348729634303,37.2606962390448,122.063695449204)) ;
#90844 = CARTESIAN_POINT('Ctrl Pts',(-18.9753445770678,37.2705414473262,121.96828080011)) ;
#90845 = CARTESIAN_POINT('Ctrl Pts',(-19.2323500330995,37.2805321362893,121.914602131553)) ;
#90846 = CARTESIAN_POINT('Ctrl Pts',(-19.4960202224024,37.2905700125716,121.9069126897)) ;
#90847 = CARTESIAN_POINT('Ctrl Pts',(-19.7520669609929,37.3004143902138,121.943940420464)) ;
#90848 = CARTESIAN_POINT('Ctrl Pts',(-20.0014193408441,37.3103991946052,122.025510816322)) ;
#90849 = CARTESIAN_POINT('Ctrl Pts',(-20.2318871717339,37.3203387248238,122.148511202845)) ;
#90850 = CARTESIAN_POINT('Ctrl Pts',(-20.4394866075736,37.3303784128607,122.311296862849)) ;
#90851 = CARTESIAN_POINT('Ctrl Pts',(-20.6131300585679,37.340266702229,122.504635758308)) ;
#90852 = CARTESIAN_POINT('Ctrl Pts',(-20.7523750420527,37.3502558259138,122.727153728378)) ;
#90853 = CARTESIAN_POINT('Ctrl Pts',(-20.8503938939143,37.3602158355884,122.969841158144)) ;
#90854 = CARTESIAN_POINT('Ctrl Pts',(-20.9050687368293,37.3701162652927,123.224212899945)) ;
#90855 = CARTESIAN_POINT('Ctrl Pts',(-20.9148721088486,37.3801593466994,123.487941036205)) ;
#90856 = CARTESIAN_POINT('Ctrl Pts',(-20.8792246033343,37.390066740607,123.745859387518)) ;
#90857 = CARTESIAN_POINT('Ctrl Pts',(-20.7989609173973,37.4000784715962,123.996417274373)) ;
#90858 = CARTESIAN_POINT('Ctrl Pts',(-20.6756955451906,37.410110689311,124.22947112403)) ;
#90859 = CARTESIAN_POINT('Ctrl Pts',(-20.51702591384,37.4199631985572,124.434050623572)) ;
#90860 = CARTESIAN_POINT('Ctrl Pts',(-20.3237233572184,37.4299211351002,124.610450271903)) ;
#90861 = CARTESIAN_POINT('Ctrl Pts',(-20.1007000293467,37.4399600051085,124.751331487019)) ;
#90862 = CARTESIAN_POINT('Ctrl Pts',(-19.8607616035958,37.4498331602667,124.850169231509)) ;
#90863 = CARTESIAN_POINT('Ctrl Pts',(-19.602246757542,37.4599064351164,124.906872980276)) ;
#90864 = CARTESIAN_POINT('Ctrl Pts',(-19.3443562287078,37.4697267522938,124.917896850224)) ;
#90865 = CARTESIAN_POINT('Ctrl Pts',(-19.0818283552624,37.4798054380873,124.883340221226)) ;
#90866 = CARTESIAN_POINT('Ctrl Pts',(-18.8348322832029,37.4896569494704,124.805570098911)) ;
#90867 = CARTESIAN_POINT('Ctrl Pts',(-18.599913832951,37.499730395777,124.683655014206)) ;
#90868 = CARTESIAN_POINT('Ctrl Pts',(-18.3945253990698,37.5095716709017,124.526446904205)) ;
#90869 = CARTESIAN_POINT('Ctrl Pts',(-18.2164310699433,37.5195567705585,124.333775949038)) ;
#90870 = CARTESIAN_POINT('Ctrl Pts',(-18.0744621012236,37.5295642466928,124.11237858257)) ;
#90871 = CARTESIAN_POINT('Ctrl Pts',(-17.9737434063258,37.5394868344017,123.871874033015)) ;
#90872 = CARTESIAN_POINT('Ctrl Pts',(-17.9155198712875,37.5494734386751,123.615951736417)) ;
#90873 = CARTESIAN_POINT('Ctrl Pts',(-17.9030442398782,37.5595135670092,123.352424180443)) ;
#90874 = CARTESIAN_POINT('Ctrl Pts',(-17.9352929472443,37.5693530015426,123.095845830502)) ;
#90875 = CARTESIAN_POINT('Ctrl Pts',(-18.0131166461626,37.5794170560336,122.843116592569)) ;
#90876 = CARTESIAN_POINT('Ctrl Pts',(-18.1316981730949,37.5893079752708,122.611787994209)) ;
#90877 = CARTESIAN_POINT('Ctrl Pts',(-18.2897770295622,37.5992999685768,122.402140602484)) ;
#90878 = CARTESIAN_POINT('Ctrl Pts',(-18.4814669497025,37.6092628325361,122.223821161659)) ;
#90879 = CARTESIAN_POINT('Ctrl Pts',(-18.6995802858491,37.6191670923539,122.081762570876)) ;
#90880 = CARTESIAN_POINT('Ctrl Pts',(-18.9428624159537,37.6292275829253,121.978356993375)) ;
#90881 = CARTESIAN_POINT('Ctrl Pts',(-19.1947597030667,37.6390679325563,121.919723653256)) ;
#90882 = CARTESIAN_POINT('Ctrl Pts',(-19.4587639337918,37.6491309080463,121.905087450184)) ;
#90883 = CARTESIAN_POINT('Ctrl Pts',(-19.7169360685854,37.6590252281897,121.936206707452)) ;
#90884 = CARTESIAN_POINT('Ctrl Pts',(-19.9671186320429,37.6689669413213,122.011348625595)) ;
#90885 = CARTESIAN_POINT('Ctrl Pts',(-20.2020080675906,37.6789698311154,122.129443636696)) ;
#90886 = CARTESIAN_POINT('Ctrl Pts',(-20.4132615576,37.6890096882759,122.287457794107)) ;
#90887 = CARTESIAN_POINT('Ctrl Pts',(-20.5904502427968,37.6988338691135,122.475251891521)) ;
#90888 = CARTESIAN_POINT('Ctrl Pts',(-20.735982916264,37.7088908426167,122.69583339334)) ;
#90889 = CARTESIAN_POINT('Ctrl Pts',(-20.8393694687883,37.7188189668038,122.93539179218)) ;
#90890 = CARTESIAN_POINT('Ctrl Pts',(-20.9004226762574,37.7287726618772,123.18974167518)) ;
#90891 = CARTESIAN_POINT('Ctrl Pts',(-20.9161571182402,37.7388188554525,123.453273135493)) ;
#90892 = CARTESIAN_POINT('Ctrl Pts',(-20.8867385875313,37.7486669578124,123.710392738064)) ;
#90893 = CARTESIAN_POINT('Ctrl Pts',(-20.8130541065125,37.75862854604,123.96157704454)) ;
#90894 = CARTESIAN_POINT('Ctrl Pts',(-20.6957843077402,37.7686572161963,124.197608569847)) ;
#90895 = CARTESIAN_POINT('Ctrl Pts',(-20.5412434271641,37.778567519078,124.407217781717)) ;
#90896 = CARTESIAN_POINT('Ctrl Pts',(-20.352645450369,37.7885024028859,124.58776383537)) ;
#90897 = CARTESIAN_POINT('Ctrl Pts',(-20.133119143806,37.7985435445765,124.734158279139)) ;
#90898 = CARTESIAN_POINT('Ctrl Pts',(-19.895266526059,37.8084306657405,124.838762309883)) ;
#90899 = CARTESIAN_POINT('Ctrl Pts',(-19.6403142341081,37.818423008589,124.901552440905)) ;
#90900 = CARTESIAN_POINT('Ctrl Pts',(-19.3794511200074,37.828371309813,124.918971337681)) ;
#90901 = CARTESIAN_POINT('Ctrl Pts',(-19.1197938910939,37.8383088874951,124.891242488897)) ;
#90902 = CARTESIAN_POINT('Ctrl Pts',(-18.8675519902502,37.8482954619457,124.818740589761)) ;
#90903 = CARTESIAN_POINT('Ctrl Pts',(-18.6308845594972,37.8583242718541,124.702791487369)) ;
#90904 = CARTESIAN_POINT('Ctrl Pts',(-18.4209911500482,37.8682025931609,124.550044711612)) ;
#90905 = CARTESIAN_POINT('Ctrl Pts',(-18.2382893834789,37.8781942405083,124.361450555223)) ;
#90906 = CARTESIAN_POINT('Ctrl Pts',(-18.0909361216224,37.8882287639461,124.142780458619)) ;
#90907 = CARTESIAN_POINT('Ctrl Pts',(-17.9851082426078,37.8980921208247,123.90613973582)) ;
#90908 = CARTESIAN_POINT('Ctrl Pts',(-17.9206158973704,37.908162347505,123.649512993499)) ;
#90909 = CARTESIAN_POINT('Ctrl Pts',(-17.9021014477694,37.9180046556397,123.391519278401)) ;
#90910 = CARTESIAN_POINT('Ctrl Pts',(-17.9280213893312,37.9279653876631,123.131054268142)) ;
#90911 = CARTESIAN_POINT('Ctrl Pts',(-17.9998223639555,37.9380032768612,122.877238454483)) ;
#90912 = CARTESIAN_POINT('Ctrl Pts',(-18.1123180047447,37.94787755978,122.643370168163)) ;
#90913 = CARTESIAN_POINT('Ctrl Pts',(-18.2666811956989,37.9579473043975,122.428479079685)) ;
#90914 = CARTESIAN_POINT('Ctrl Pts',(-18.4515097019627,37.9677806147431,122.247856374346)) ;
#90915 = CARTESIAN_POINT('Ctrl Pts',(-18.6687188341038,37.9778108580958,122.098544975013)) ;
#90916 = CARTESIAN_POINT('Ctrl Pts',(-18.9089398495734,37.9878431460742,121.989907265577)) ;
#90917 = CARTESIAN_POINT('Ctrl Pts',(-19.1589973603507,37.9976703225423,121.925371796745)) ;
#90918 = CARTESIAN_POINT('Ctrl Pts',(-19.4210528476622,38.0076757054092,121.904329796489)) ;
#90919 = CARTESIAN_POINT('Ctrl Pts',(-19.6822603276462,38.0176583444019,121.929146579502)) ;
#90920 = CARTESIAN_POINT('Ctrl Pts',(-19.9365866650456,38.0277024115385,121.999661380241)) ;
#90921 = CARTESIAN_POINT('Ctrl Pts',(-20.1697455284941,38.0375236303425,122.110354265076)) ;
#90922 = CARTESIAN_POINT('Ctrl Pts',(-20.3851407356152,38.0475604692805,122.262573522578)) ;
#90923 = CARTESIAN_POINT('Ctrl Pts',(-20.5700791380799,38.0575848813783,122.450185779491)) ;
#90924 = CARTESIAN_POINT('Ctrl Pts',(-20.7175310391498,38.0674369657836,122.663002255422)) ;
#90925 = CARTESIAN_POINT('Ctrl Pts',(-20.8276645507075,38.0774278625268,122.901301885871)) ;
#90926 = CARTESIAN_POINT('Ctrl Pts',(-20.8944393360025,38.0873458544277,123.153269837169)) ;
#90927 = CARTESIAN_POINT('Ctrl Pts',(-20.916752709306,38.0973739698847,123.415831037644)) ;
#90928 = CARTESIAN_POINT('Ctrl Pts',(-20.89358187262,38.1072591458268,123.674574253975)) ;
#90929 = CARTESIAN_POINT('Ctrl Pts',(-20.8257391871181,38.1172485042337,123.928171654191)) ;
#90930 = CARTESIAN_POINT('Ctrl Pts',(-20.7138167717013,38.127289651814,124.167129479311)) ;
#90931 = CARTESIAN_POINT('Ctrl Pts',(-20.5656061454427,38.1371222748204,124.378785103182)) ;
#90932 = CARTESIAN_POINT('Ctrl Pts',(-20.3804240799344,38.1471163459312,124.565013167833)) ;
#90933 = CARTESIAN_POINT('Ctrl Pts',(-20.1646606886898,38.1571450035721,124.716368185705)) ;
#90934 = CARTESIAN_POINT('Ctrl Pts',(-19.9294754177371,38.1670293297649,124.826601817947)) ;
#90935 = CARTESIAN_POINT('Ctrl Pts',(-19.6768051124309,38.1769950732555,124.89551183432)) ;
#90936 = CARTESIAN_POINT('Ctrl Pts',(-19.4143545698229,38.1870234523867,124.919272831667)) ;
#90937 = CARTESIAN_POINT('Ctrl Pts',(-19.155026247405,38.1969242985936,124.897774472843)) ;
#90938 = CARTESIAN_POINT('Ctrl Pts',(-18.899449911136,38.2069829560107,124.830469885562)) ;
#90939 = CARTESIAN_POINT('Ctrl Pts',(-18.6640472589483,38.2168405187926,124.72223521876)) ;
#90940 = CARTESIAN_POINT('Ctrl Pts',(-18.4464297173287,38.2269089213458,124.571809104608)) ;
#90941 = CARTESIAN_POINT('Ctrl Pts',(-18.262192640318,38.2367643200854,124.389754401548)) ;
#90942 = CARTESIAN_POINT('Ctrl Pts',(-18.1096196037123,38.2467591871593,124.175968694404)) ;
#90943 = CARTESIAN_POINT('Ctrl Pts',(-17.9965795627306,38.2567904821428,123.937817735641)) ;
#90944 = CARTESIAN_POINT('Ctrl Pts',(-17.9273563602029,38.2666570068693,123.687937654047)) ;
#90945 = CARTESIAN_POINT('Ctrl Pts',(-17.9018527032758,38.276644477565,123.426751350671)) ;
#90946 = CARTESIAN_POINT('Ctrl Pts',(-17.9218607437343,38.2865892371289,123.166140198543)) ;
#90947 = CARTESIAN_POINT('Ctrl Pts',(-17.9876155290226,38.2966347930777,122.910504235427)) ;
#90948 = CARTESIAN_POINT('Ctrl Pts',(-18.0945121468168,38.3064943814529,122.674449960714)) ;
#90949 = CARTESIAN_POINT('Ctrl Pts',(-18.2424996480843,38.3164953365889,122.457313423853)) ;
#90950 = CARTESIAN_POINT('Ctrl Pts',(-18.4240798301571,38.3263995638665,122.270788969546)) ;
#90951 = CARTESIAN_POINT('Ctrl Pts',(-18.6381236155899,38.3364416407616,122.116493175448)) ;
#90952 = CARTESIAN_POINT('Ctrl Pts',(-18.8725441547087,38.3463492534478,122.003091772094)) ;
#90953 = CARTESIAN_POINT('Ctrl Pts',(-19.1267212481479,38.3564037840635,121.931068647469)) ;
#90954 = CARTESIAN_POINT('Ctrl Pts',(-19.3845339848272,38.3662645706124,121.904631230091)) ;
#90955 = CARTESIAN_POINT('Ctrl Pts',(-19.6464652984615,38.3762583256834,121.92312229318)) ;
#90956 = CARTESIAN_POINT('Ctrl Pts',(-19.8995750129763,38.3861836859234,121.986273003471)) ;
#90957 = CARTESIAN_POINT('Ctrl Pts',(-20.140272020409,38.3962116153187,122.093470120755)) ;
#90958 = CARTESIAN_POINT('Ctrl Pts',(-20.3558252995868,38.406097882118,122.238568442777)) ;
#90959 = CARTESIAN_POINT('Ctrl Pts',(-20.5456984409777,38.4161296510163,122.42138753169)) ;
#90960 = CARTESIAN_POINT('Ctrl Pts',(-20.698877922451,38.4260112468599,122.631132419724)) ;
#90961 = CARTESIAN_POINT('Ctrl Pts',(-20.8154213762224,38.4360731323278,122.8684346522)) ;
#90962 = CARTESIAN_POINT('Ctrl Pts',(-20.8875986677405,38.4459305663467,123.117253823727)) ;
#90963 = CARTESIAN_POINT('Ctrl Pts',(-20.9164045121782,38.4559238093887,123.378246907377)) ;
#90964 = CARTESIAN_POINT('Ctrl Pts',(-20.8995775457113,38.465854570275,123.638690081529)) ;
#90965 = CARTESIAN_POINT('Ctrl Pts',(-20.816850334482,38.4792035624722,123.979625573362)) ;
#90966 = CARTESIAN_POINT('Ctrl Pts',(-20.6476612787041,38.4924719352886,124.289010646964)) ;
#90967 = CARTESIAN_POINT('Ctrl Pts',(-20.4070708455003,38.505754876673,124.541958141041)) ;
#90968 = CARTESIAN_POINT('Ctrl Pts',(-20.1946437063502,38.5157976625152,124.698532719528)) ;
#90969 = CARTESIAN_POINT('Ctrl Pts',(-19.9628978193437,38.5256476050673,124.813858968729)) ;
#90970 = CARTESIAN_POINT('Ctrl Pts',(-19.7111423066587,38.5356448379863,124.888916493239)) ;
#90971 = CARTESIAN_POINT('Ctrl Pts',(-19.4496444734046,38.5456597333208,124.918770576671)) ;
#90972 = CARTESIAN_POINT('Ctrl Pts',(-19.102347554309,38.558899409959,124.897958325602)) ;
#90973 = CARTESIAN_POINT('Ctrl Pts',(-18.6847987628518,38.5754466343643,124.759928991449)) ;
#90974 = CARTESIAN_POINT('Ctrl Pts',(-18.3371659709119,38.5920940714954,124.486215378783)) ;
#90975 = CARTESIAN_POINT('Ctrl Pts',(-18.1282833266673,38.6053835689736,124.206304846633)) ;
#90976 = CARTESIAN_POINT('Ctrl Pts',(-18.0108766480719,38.615256976796,123.974924396754)) ;
#90977 = CARTESIAN_POINT('Ctrl Pts',(-17.9340194463027,38.6253093543887,123.722198205263)) ;
#90978 = CARTESIAN_POINT('Ctrl Pts',(-17.9027887073884,38.6352130079296,123.463801752552)) ;
#90979 = CARTESIAN_POINT('Ctrl Pts',(-17.9163242119673,38.6451572769249,123.202860594878)) ;
#90980 = CARTESIAN_POINT('Ctrl Pts',(-17.9947872688244,38.6584882852576,122.861360560677)) ;
#90981 = CARTESIAN_POINT('Ctrl Pts',(-18.2021257874539,38.6751098657819,122.471340515978)) ;
#90982 = CARTESIAN_POINT('Ctrl Pts',(-18.5280196716949,38.6916525364803,122.176175599121)) ;
#90983 = CARTESIAN_POINT('Ctrl Pts',(-18.84008875281,38.7050016960432,122.015952826464)) ;
#90984 = CARTESIAN_POINT('Ctrl Pts',(-19.1721179105993,38.7182298462027,121.912874830925)) ;
#90985 = CARTESIAN_POINT('Ctrl Pts',(-19.6137093351474,38.7348605233402,121.89504706836)) ;
#90986 = CARTESIAN_POINT('Ctrl Pts',(-20.1178745686584,38.7547634626283,122.055405875493)) ;
#90987 = CARTESIAN_POINT('Ctrl Pts',(-20.5372564996866,38.7746663292316,122.377645054216)) ;
#90988 = CARTESIAN_POINT('Ctrl Pts',(-20.8224486031123,38.7945794943364,122.823633412691)) ;
#90989 = CARTESIAN_POINT('Ctrl Pts',(-20.9381893408,38.8146153234777,123.343346667635)) ;
#90990 = CARTESIAN_POINT('Ctrl Pts',(-20.8706660685584,38.8344338983558,123.865874261203)) ;
#90991 = CARTESIAN_POINT('Ctrl Pts',(-20.627922443163,38.8544041993978,124.337692899044)) ;
#90992 = CARTESIAN_POINT('Ctrl Pts',(-20.2401234229137,38.8742957317623,124.69730681963)) ;
#90993 = CARTESIAN_POINT('Ctrl Pts',(-19.7497967047093,38.8943188295789,124.903871868757)) ;
#90994 = CARTESIAN_POINT('Ctrl Pts',(-19.2242573161077,38.9141155824988,124.930795625851)) ;
#90995 = CARTESIAN_POINT('Ctrl Pts',(-18.7165907441389,38.9340766709876,124.776879006077)) ;
#90996 = CARTESIAN_POINT('Ctrl Pts',(-18.2921488184441,38.9540549399198,124.457746589565)) ;
#90997 = CARTESIAN_POINT('Ctrl Pts',(-18.0037947360342,38.9738749547108,124.016952429214)) ;
#90998 = CARTESIAN_POINT('Ctrl Pts',(-17.8810979198861,38.9938133639626,123.501394794737)) ;
#90999 = CARTESIAN_POINT('Ctrl Pts',(-17.9432262389664,39.013860481355,122.972141220867)) ;
#91000 = CARTESIAN_POINT('Ctrl Pts',(-18.179999474083,39.0337067271889,122.500852961374)) ;
#91001 = CARTESIAN_POINT('Ctrl Pts',(-18.5620692319856,39.0535556957009,122.137036795423)) ;
#91002 = CARTESIAN_POINT('Ctrl Pts',(-19.0504584844477,39.0736059980122,121.923948334636)) ;
#91003 = CARTESIAN_POINT('Ctrl Pts',(-19.5767211389698,39.0934409204434,121.8907738155)) ;
#91004 = CARTESIAN_POINT('Ctrl Pts',(-20.0851205819504,39.1133713216693,122.038805273945)) ;
#91005 = CARTESIAN_POINT('Ctrl Pts',(-20.5122385328754,39.1332562670282,122.350424357377)) ;
#91006 = CARTESIAN_POINT('Ctrl Pts',(-20.8092718181263,39.1533288751795,122.793463019832)) ;
#91007 = CARTESIAN_POINT('Ctrl Pts',(-20.9356236783323,39.1731201915077,123.304163853874)) ;
#91008 = CARTESIAN_POINT('Ctrl Pts',(-20.8812715084831,39.1930849812749,123.831959781897)) ;
#91009 = CARTESIAN_POINT('Ctrl Pts',(-20.6486431634336,39.2130679370252,124.309427208045)) ;
#91010 = CARTESIAN_POINT('Ctrl Pts',(-20.2711039549004,39.2328764590014,124.676430038506)) ;
#91011 = CARTESIAN_POINT('Ctrl Pts',(-19.7870902404589,39.2528620337372,124.894984520865)) ;
#91012 = CARTESIAN_POINT('Ctrl Pts',(-19.2600307895484,39.2727446738056,124.934952427669)) ;
#91013 = CARTESIAN_POINT('Ctrl Pts',(-18.7492190934437,39.2926999859375,124.792610565746)) ;
#91014 = CARTESIAN_POINT('Ctrl Pts',(-18.3190388924115,39.3125743425453,124.485911249285)) ;
#91015 = CARTESIAN_POINT('Ctrl Pts',(-18.0175162438669,39.3325565494064,124.048781584885)) ;
#91016 = CARTESIAN_POINT('Ctrl Pts',(-17.8838364996547,39.3524876273563,123.536075517646)) ;
#91017 = CARTESIAN_POINT('Ctrl Pts',(-17.9330377132969,39.3724146022113,123.008847051512)) ;
#91018 = CARTESIAN_POINT('Ctrl Pts',(-18.1572602607085,39.3922470611602,122.531726093143)) ;
#91019 = CARTESIAN_POINT('Ctrl Pts',(-18.4706715836701,39.4089047453354,122.219175253551)) ;
#91020 = CARTESIAN_POINT('Ctrl Pts',(-18.7724853140679,39.4221539692425,122.045409139846)) ;
#91021 = CARTESIAN_POINT('Ctrl Pts',(-19.0206746467771,39.4322029906937,121.95528639923)) ;
#91022 = CARTESIAN_POINT('Ctrl Pts',(-19.2758714027625,39.4420629989242,121.910414373671)) ;
#91023 = CARTESIAN_POINT('Ctrl Pts',(-19.6249850662901,39.4553465121488,121.909430053781)) ;
#91024 = CARTESIAN_POINT('Ctrl Pts',(-20.0524695157253,39.4719924311496,122.023204765113)) ;
#91025 = CARTESIAN_POINT('Ctrl Pts',(-20.4138864148045,39.4885464089657,122.274186137911)) ;
#91026 = CARTESIAN_POINT('Ctrl Pts',(-20.6406300091737,39.5019061379373,122.542218010001)) ;
#91027 = CARTESIAN_POINT('Ctrl Pts',(-20.7717096169385,39.511799189734,122.766754046185)) ;
#91028 = CARTESIAN_POINT('Ctrl Pts',(-20.8630087660866,39.521789155015,123.012860662966)) ;
#91029 = CARTESIAN_POINT('Ctrl Pts',(-20.9101748143691,39.5317410358759,123.270138684946)) ;
#91030 = CARTESIAN_POINT('Ctrl Pts',(-20.9117456673708,39.5417893875677,123.534165997582)) ;
#91031 = CARTESIAN_POINT('Ctrl Pts',(-20.8686552536552,39.5516306716739,123.789195920828)) ;
#91032 = CARTESIAN_POINT('Ctrl Pts',(-20.7812002337361,39.5616173747996,124.036586790097)) ;
#91033 = CARTESIAN_POINT('Ctrl Pts',(-20.6528795142412,39.571552403617,124.264016264375)) ;
#91034 = CARTESIAN_POINT('Ctrl Pts',(-20.4848907700779,39.5816081985239,124.46795141361)) ;
#91035 = CARTESIAN_POINT('Ctrl Pts',(-20.2887891671277,39.5914365618132,124.636091146284)) ;
#91036 = CARTESIAN_POINT('Ctrl Pts',(-20.0614641234576,39.6014975317111,124.771025787529)) ;
#91037 = CARTESIAN_POINT('Ctrl Pts',(-19.8176332037188,39.6114118106009,124.862898597772)) ;
#91038 = CARTESIAN_POINT('Ctrl Pts',(-19.5592282819904,39.6214208050691,124.912002571716)) ;
#91039 = CARTESIAN_POINT('Ctrl Pts',(-19.2956754516133,39.6314506396329,124.914961194742)) ;
#91040 = CARTESIAN_POINT('Ctrl Pts',(-19.0399610301937,39.6413088697051,124.873328894269)) ;
#91041 = CARTESIAN_POINT('Ctrl Pts',(-18.7918272427075,39.6513075754475,124.787030713098)) ;
#91042 = CARTESIAN_POINT('Ctrl Pts',(-18.5646041239284,39.6612022313663,124.660518202869)) ;
#91043 = CARTESIAN_POINT('Ctrl Pts',(-18.3594891226658,39.6712652957503,124.493676816178)) ;
#91044 = CARTESIAN_POINT('Ctrl Pts',(-18.1900268540481,39.6811049540302,124.298315227073)) ;
#91045 = CARTESIAN_POINT('Ctrl Pts',(-18.053792583236,39.691168121112,124.071699946612)) ;
#91046 = CARTESIAN_POINT('Ctrl Pts',(-17.960749315,39.7010623662391,123.828876199066)) ;
#91047 = CARTESIAN_POINT('Ctrl Pts',(-17.9103583441189,39.7110041878437,123.572554229599)) ;
#91048 = CARTESIAN_POINT('Ctrl Pts',(-17.9051091078073,39.7210067187618,123.309715572966)) ;
#91049 = CARTESIAN_POINT('Ctrl Pts',(-17.9461034213345,39.7310413452193,123.049236091637)) ;
#91050 = CARTESIAN_POINT('Ctrl Pts',(-18.0297068679523,39.7408868802057,122.804375715976)) ;
#91051 = CARTESIAN_POINT('Ctrl Pts',(-18.1557911659349,39.7508703050448,122.574330051635)) ;
#91052 = CARTESIAN_POINT('Ctrl Pts',(-18.3194197366641,39.7608206954098,122.370358879002)) ;
#91053 = CARTESIAN_POINT('Ctrl Pts',(-18.5166895154144,39.7708183357069,122.1968019572)) ;
#91054 = CARTESIAN_POINT('Ctrl Pts',(-18.7422717110751,39.7808574162701,122.06004045278)) ;
#91055 = CARTESIAN_POINT('Ctrl Pts',(-18.9827757053251,39.7906835670392,121.966001404595)) ;
#91056 = CARTESIAN_POINT('Ctrl Pts',(-19.241779151991,39.8007401419683,121.913550884301)) ;
#91057 = CARTESIAN_POINT('Ctrl Pts',(-19.5029424763994,39.8106806813486,121.907401203059)) ;
#91058 = CARTESIAN_POINT('Ctrl Pts',(-19.7603853137432,39.820585074325,121.945742920367)) ;
#91059 = CARTESIAN_POINT('Ctrl Pts',(-20.0107266937267,39.8306317285299,122.029537599121)) ;
#91060 = CARTESIAN_POINT('Ctrl Pts',(-20.2393968682051,39.8405272904683,122.153454191526)) ;
#91061 = CARTESIAN_POINT('Ctrl Pts',(-20.4464414983218,39.8505893683139,122.317864784386)) ;
#91062 = CARTESIAN_POINT('Ctrl Pts',(-20.6181263774124,39.8604320667276,122.511365345899)) ;
#91063 = CARTESIAN_POINT('Ctrl Pts',(-20.7561382322086,39.8704228416891,122.734672291079)) ;
#91064 = CARTESIAN_POINT('Ctrl Pts',(-20.8526500680807,39.8803507067082,122.97707426249)) ;
#91065 = CARTESIAN_POINT('Ctrl Pts',(-20.9063594910296,39.8903394514744,123.234019741878)) ;
#91066 = CARTESIAN_POINT('Ctrl Pts',(-20.9142878541207,39.9003722370613,123.497555642552)) ;
#91067 = CARTESIAN_POINT('Ctrl Pts',(-20.8772279525817,39.910238921682,123.754170693425)) ;
#91068 = CARTESIAN_POINT('Ctrl Pts',(-20.7961043668712,39.9202008138451,124.003076881027)) ;
#91069 = CARTESIAN_POINT('Ctrl Pts',(-20.6717493071348,39.9302342907577,124.2355665129)) ;
#91070 = CARTESIAN_POINT('Ctrl Pts',(-20.5116325782537,39.940118632006,124.440138606861)) ;
#91071 = CARTESIAN_POINT('Ctrl Pts',(-20.3149883606172,39.9501815741271,124.61689780952)) ;
#91072 = CARTESIAN_POINT('Ctrl Pts',(-20.0953995131372,39.9600319757467,124.754007658767)) ;
#91073 = CARTESIAN_POINT('Ctrl Pts',(-19.8513143447031,39.9700588645364,124.853250471539)) ;
#91074 = CARTESIAN_POINT('Ctrl Pts',(-19.5934970141475,39.9800874794926,124.907943166141)) ;
#91075 = CARTESIAN_POINT('Ctrl Pts',(-19.3349601607156,39.9899327026126,124.917361759063)) ;
#91076 = CARTESIAN_POINT('Ctrl Pts',(-19.0748122096571,39.9999233864186,124.881915578707)) ;
#91077 = CARTESIAN_POINT('Ctrl Pts',(-18.8237784515497,40.009961268491,124.800902625927)) ;
#91078 = CARTESIAN_POINT('Ctrl Pts',(-18.5948964274932,40.0198056281299,124.68030432098)) ;
#91079 = CARTESIAN_POINT('Ctrl Pts',(-18.3872328665451,40.0297904987446,124.519971576075)) ;
#91080 = CARTESIAN_POINT('Ctrl Pts',(-18.2112308942488,40.0397297820733,124.326928042325)) ;
#91081 = CARTESIAN_POINT('Ctrl Pts',(-18.0701011370966,40.0497703914464,124.10401924585)) ;
#91082 = CARTESIAN_POINT('Ctrl Pts',(-17.9711747293191,40.0596552423596,123.863797270785)) ;
#91083 = CARTESIAN_POINT('Ctrl Pts',(-17.914507891847,40.0696571985284,123.607177988291)) ;
#91084 = CARTESIAN_POINT('Ctrl Pts',(-17.9031408318448,40.0795757952489,123.346733888948)) ;
#91085 = CARTESIAN_POINT('Ctrl Pts',(-17.9376487606401,40.0896226173247,123.085016388873)) ;
#91086 = CARTESIAN_POINT('Ctrl Pts',(-18.0155031495141,40.0994968984374,122.837438413162)) ;
#91087 = CARTESIAN_POINT('Ctrl Pts',(-18.1371591486748,40.109551098482,122.602950598639)) ;
#91088 = CARTESIAN_POINT('Ctrl Pts',(-18.2951196454476,40.1194465281173,122.396320882415)) ;
#91089 = CARTESIAN_POINT('Ctrl Pts',(-18.4896702718675,40.1295081564346,122.217309891194)) ;
#91090 = CARTESIAN_POINT('Ctrl Pts',(-18.7075627861497,40.1393527852645,122.077821066016)) ;
#91091 = CARTESIAN_POINT('Ctrl Pts',(-18.9487886325186,40.1493128328701,121.976254285154)) ;
#91092 = CARTESIAN_POINT('Ctrl Pts',(-19.2060965362213,40.1593511390442,121.918165822933)) ;
#91093 = CARTESIAN_POINT('Ctrl Pts',(-19.4652798129029,40.1692244384768,121.905341126692)) ;
#91094 = CARTESIAN_POINT('Ctrl Pts',(-19.7278620306309,40.1792977000631,121.938443177458)) ;
#91095 = CARTESIAN_POINT('Ctrl Pts',(-19.9745652121543,40.1891179260198,122.014376604329)) ;
#91096 = CARTESIAN_POINT('Ctrl Pts',(-20.210384152523,40.1991969899593,122.134825848413)) ;
#91097 = CARTESIAN_POINT('Ctrl Pts',(-20.4170898719692,40.2090470799791,122.290751429487)) ;
#91098 = CARTESIAN_POINT('Ctrl Pts',(-20.5976846428322,40.2191258335929,122.484401518764)) ;
#91099 = CARTESIAN_POINT('Ctrl Pts',(-20.7384649199968,40.2289473008524,122.700793862279)) ;
#91100 = CARTESIAN_POINT('Ctrl Pts',(-20.8423732928383,40.23901289921,122.943977873275)) ;
#91101 = CARTESIAN_POINT('Ctrl Pts',(-20.9014655130511,40.2489155549847,123.197477874162)) ;
#91102 = CARTESIAN_POINT('Ctrl Pts',(-20.9159315140315,40.2589663808143,123.461152741984)) ;
#91103 = CARTESIAN_POINT('Ctrl Pts',(-20.8851862687562,40.2688405851532,123.718866407652)) ;
#91104 = CARTESIAN_POINT('Ctrl Pts',(-20.8087033848994,40.2789130351923,123.972210529531)) ;
#91105 = CARTESIAN_POINT('Ctrl Pts',(-20.6924508708633,40.2887420519658,124.202923123241)) ;
#91106 = CARTESIAN_POINT('Ctrl Pts',(-20.534514449587,40.2988088978806,124.415095541138)) ;
#91107 = CARTESIAN_POINT('Ctrl Pts',(-20.3453419288887,40.3086990691824,124.593367187674)) ;
#91108 = CARTESIAN_POINT('Ctrl Pts',(-20.126206043176,40.3186912628062,124.738011905012)) ;
#91109 = CARTESIAN_POINT('Ctrl Pts',(-19.8858849575961,40.3286540734297,124.841878589706)) ;
#91110 = CARTESIAN_POINT('Ctrl Pts',(-19.6328023115127,40.3385583462731,124.902733214097)) ;
#91111 = CARTESIAN_POINT('Ctrl Pts',(-19.368941004048,40.3486188380777,124.918739240953)) ;
#91112 = CARTESIAN_POINT('Ctrl Pts',(-19.111948949925,40.3584591697501,124.889672424697)) ;
#91113 = CARTESIAN_POINT('Ctrl Pts',(-18.8582728174585,40.3685222158418,124.815092864794)) ;
#91114 = CARTESIAN_POINT('Ctrl Pts',(-18.6254185641157,40.3784162715369,124.699353388829)) ;
#91115 = CARTESIAN_POINT('Ctrl Pts',(-18.414789936686,40.3883589718599,124.544790683395)) ;
#91116 = CARTESIAN_POINT('Ctrl Pts',(-18.2329762001901,40.3983647127875,124.354801620633)) ;
#91117 = CARTESIAN_POINT('Ctrl Pts',(-18.0869571139645,40.408385623303,124.135661151696)) ;
#91118 = CARTESIAN_POINT('Ctrl Pts',(-17.982299068752,40.418276358753,123.897735676412)) ;
#91119 = CARTESIAN_POINT('Ctrl Pts',(-17.9195403076832,40.4282678994818,123.64278976609)) ;
#91120 = CARTESIAN_POINT('Ctrl Pts',(-17.9021523398952,40.4382157599035,123.381951195381)) ;
#91121 = CARTESIAN_POINT('Ctrl Pts',(-17.9298041725074,40.4481624290898,123.122015017719)) ;
#91122 = CARTESIAN_POINT('Ctrl Pts',(-18.0031779584756,40.4582105052254,122.868371382531)) ;
#91123 = CARTESIAN_POINT('Ctrl Pts',(-18.1169687224454,40.468058103231,122.635944200235)) ;
#91124 = CARTESIAN_POINT('Ctrl Pts',(-18.2704811318407,40.4780198263155,122.423910978732)) ;
#91125 = CARTESIAN_POINT('Ctrl Pts',(-18.4599935581485,40.4880484613985,122.240750173216)) ;
#91126 = CARTESIAN_POINT('Ctrl Pts',(-18.6757822343563,40.4979587697165,122.094962047602)) ;
#91127 = CARTESIAN_POINT('Ctrl Pts',(-18.9139355025239,40.5078936668524,121.987961124184)) ;
#91128 = CARTESIAN_POINT('Ctrl Pts',(-19.1697997287511,40.517934749795,121.923493244547)) ;
#91129 = CARTESIAN_POINT('Ctrl Pts',(-19.428950366049,40.5278220926232,121.904543523959)) ;
#91130 = CARTESIAN_POINT('Ctrl Pts',(-19.6901959445774,40.5378136075626,121.930704214457)) ;
#91131 = CARTESIAN_POINT('Ctrl Pts',(-19.9419057770973,40.5477649987591,122.001654050665)) ;
#91132 = CARTESIAN_POINT('Ctrl Pts',(-20.1772160470658,40.5576975320917,122.114605806638)) ;
#91133 = CARTESIAN_POINT('Ctrl Pts',(-20.390773351119,40.5676946899911,122.267599496389)) ;
#91134 = CARTESIAN_POINT('Ctrl Pts',(-20.5744051539528,40.5776797001546,122.455089020715)) ;
#91135 = CARTESIAN_POINT('Ctrl Pts',(-20.723188468568,40.5877225267244,122.673023900318)) ;
#91136 = CARTESIAN_POINT('Ctrl Pts',(-20.8301426365293,40.5975527610294,122.908217068064)) ;
#91137 = CARTESIAN_POINT('Ctrl Pts',(-20.8963379142863,40.607628786264,123.164540306248)) ;
#91138 = CARTESIAN_POINT('Ctrl Pts',(-20.9167055563444,40.6174810227549,123.422701150021)) ;
#91139 = CARTESIAN_POINT('Ctrl Pts',(-20.891615051151,40.627554229189,123.686179366379)) ;
#91140 = CARTESIAN_POINT('Ctrl Pts',(-20.8226924038434,40.6373957386962,123.935469529968)) ;
#91141 = CARTESIAN_POINT('Ctrl Pts',(-20.7110845119955,40.647356685476,124.172237837628)) ;
#91142 = CARTESIAN_POINT('Ctrl Pts',(-20.5584645897465,40.657394514276,124.387376516039)) ;
#91143 = CARTESIAN_POINT('Ctrl Pts',(-20.3741751702042,40.6672688240305,124.570098190474)) ;
#91144 = CARTESIAN_POINT('Ctrl Pts',(-20.1567868434197,40.6773385217037,124.720922673687)) ;
#91145 = CARTESIAN_POINT('Ctrl Pts',(-19.9221561017423,40.6871719929911,124.829257549577)) ;
#91146 = CARTESIAN_POINT('Ctrl Pts',(-19.6675134133936,40.697201639521,124.897250208865)) ;
#91147 = CARTESIAN_POINT('Ctrl Pts',(-19.404726915787,40.7072361538484,124.919206335434)) ;
#91148 = CARTESIAN_POINT('Ctrl Pts',(-19.1475426653616,40.7170614393193,124.896320551621)) ;
#91149 = CARTESIAN_POINT('Ctrl Pts',(-18.8935848410147,40.7270656808678,124.828449926807)) ;
#91150 = CARTESIAN_POINT('Ctrl Pts',(-18.6557571219536,40.7370483259469,124.717619979883)) ;
#91151 = CARTESIAN_POINT('Ctrl Pts',(-18.4396753878514,40.7470935230384,124.566036174496)) ;
#91152 = CARTESIAN_POINT('Ctrl Pts',(-18.2569837011254,40.7569166387985,124.383646814928)) ;
#91153 = CARTESIAN_POINT('Ctrl Pts',(-18.1050079926846,40.7669512505988,124.168150561838)) ;
#91154 = CARTESIAN_POINT('Ctrl Pts',(-17.9935267427077,40.776976259372,123.929445084339)) ;
#91155 = CARTESIAN_POINT('Ctrl Pts',(-17.9258202753636,40.7868281842135,123.679551402899)) ;
#91156 = CARTESIAN_POINT('Ctrl Pts',(-17.9018056354857,40.7968191225363,123.418132469691)) ;
#91157 = CARTESIAN_POINT('Ctrl Pts',(-17.9232248951131,40.8067371076827,123.158348244679)) ;
#91158 = CARTESIAN_POINT('Ctrl Pts',(-17.9900857838276,40.8167652085782,122.903464281987)) ;
#91159 = CARTESIAN_POINT('Ctrl Pts',(-18.0985313024471,40.8266504495208,122.667402977687)) ;
#91160 = CARTESIAN_POINT('Ctrl Pts',(-18.2473410925538,40.8366395624874,122.451144336104)) ;
#91161 = CARTESIAN_POINT('Ctrl Pts',(-18.4328177933568,40.8466816268282,122.263433343905)) ;
#91162 = CARTESIAN_POINT('Ctrl Pts',(-18.6432373021323,40.8565108282327,122.113605035665)) ;
#91163 = CARTESIAN_POINT('Ctrl Pts',(-18.8804063338663,40.8665176689909,122.000080751744)) ;
#91164 = CARTESIAN_POINT('Ctrl Pts',(-19.1333087574883,40.8765051931828,121.929728664348)) ;
#91165 = CARTESIAN_POINT('Ctrl Pts',(-19.3956374933461,40.8865348389914,121.904438993338)) ;
#91166 = CARTESIAN_POINT('Ctrl Pts',(-19.6543707145139,40.8964088697302,121.924454848222)) ;
#91167 = CARTESIAN_POINT('Ctrl Pts',(-19.9089008937694,40.9064081925943,121.989579416378)) ;
#91168 = CARTESIAN_POINT('Ctrl Pts',(-20.1463240582721,40.9163190281699,122.096753063302)) ;
#91169 = CARTESIAN_POINT('Ctrl Pts',(-20.3645193729387,40.9263732761439,122.245676406375)) ;
#91170 = CARTESIAN_POINT('Ctrl Pts',(-20.5501419901856,40.9362320204066,122.42647707007)) ;
#91171 = CARTESIAN_POINT('Ctrl Pts',(-20.7048457015326,40.9463001064796,122.641065679255)) ;
#91172 = CARTESIAN_POINT('Ctrl Pts',(-20.8175173641889,40.9561555896591,122.874289210237)) ;
#91173 = CARTESIAN_POINT('Ctrl Pts',(-20.8897275055665,40.9661504354533,123.126813177261)) ;
#91174 = CARTESIAN_POINT('Ctrl Pts',(-20.9165302141604,40.9761817311159,123.389064120819)) ;
#91175 = CARTESIAN_POINT('Ctrl Pts',(-20.898116848103,40.9860482744057,123.647700931821)) ;
#91176 = CARTESIAN_POINT('Ctrl Pts',(-20.8347236238339,40.9960356701691,123.902356200774)) ;
#91177 = CARTESIAN_POINT('Ctrl Pts',(-20.7286285702455,41.0059807108991,124.141239921477)) ;
#91178 = CARTESIAN_POINT('Ctrl Pts',(-20.5811211598771,41.0160252171158,124.360105227099)) ;
#91179 = CARTESIAN_POINT('Ctrl Pts',(-20.4012876880261,41.0258887232531,124.546811663943)) ;
#91180 = CARTESIAN_POINT('Ctrl Pts',(-20.1893463018213,41.0358815840892,124.701796997942)) ;
#91181 = CARTESIAN_POINT('Ctrl Pts',(-19.9552720707621,41.0458077778081,124.816998522553)) ;
#91182 = CARTESIAN_POINT('Ctrl Pts',(-19.7024899327944,41.0558267038407,124.890516309692)) ;
#91183 = CARTESIAN_POINT('Ctrl Pts',(-19.4434540809893,41.0657417032083,124.918982353563)) ;
#91184 = CARTESIAN_POINT('Ctrl Pts',(-19.179821038914,41.0757964747656,124.901749795245)) ;
#91185 = CARTESIAN_POINT('Ctrl Pts',(-18.9280800412219,41.0856554370632,124.840372296681)) ;
#91186 = CARTESIAN_POINT('Ctrl Pts',(-18.6874351062413,41.095649680901,124.735268941808)) ;
#91187 = CARTESIAN_POINT('Ctrl Pts',(-18.4700684891871,41.1055749103252,124.591037888929)) ;
#91188 = CARTESIAN_POINT('Ctrl Pts',(-18.2791378076578,41.1156028742167,124.409455504001)) ;
#91189 = CARTESIAN_POINT('Ctrl Pts',(-18.1245883806122,41.1254891338471,124.20057485489)) ;
#91190 = CARTESIAN_POINT('Ctrl Pts',(-18.0068635292268,41.1355208969249,123.964745548738)) ;
#91191 = CARTESIAN_POINT('Ctrl Pts',(-17.9327293076382,41.1454025232191,123.715825423128)) ;
#91192 = CARTESIAN_POINT('Ctrl Pts',(-17.9023394171472,41.1554642927052,123.453203976772)) ;
#91193 = CARTESIAN_POINT('Ctrl Pts',(-17.9176211064176,41.1653221602007,123.194569188612)) ;
#91194 = CARTESIAN_POINT('Ctrl Pts',(-17.9778112462982,41.1753137853181,122.939023648064)) ;
#91195 = CARTESIAN_POINT('Ctrl Pts',(-18.0809522301768,41.1852505844263,122.699110258918)) ;
#91196 = CARTESIAN_POINT('Ctrl Pts',(-18.2246372961258,41.1952414139836,122.479365383899)) ;
#91197 = CARTESIAN_POINT('Ctrl Pts',(-18.4051031632681,41.2052646496968,122.287492545493)) ;
#91198 = CARTESIAN_POINT('Ctrl Pts',(-18.6133310445568,41.215160997726,122.131695698258)) ;
#91199 = CARTESIAN_POINT('Ctrl Pts',(-18.8473975521708,41.2251505602285,122.012807543813)) ;
#91200 = CARTESIAN_POINT('Ctrl Pts',(-19.0999569107167,41.235190867913,121.936495551711)) ;
#91201 = CARTESIAN_POINT('Ctrl Pts',(-19.35673862267,41.2450331712602,121.905316610654)) ;
#91202 = CARTESIAN_POINT('Ctrl Pts',(-19.619750139844,41.2550568795393,121.919098001981)) ;
#91203 = CARTESIAN_POINT('Ctrl Pts',(-19.9583979422888,41.268279057007,121.997129854709)) ;
#91204 = CARTESIAN_POINT('Ctrl Pts',(-20.2706317559911,41.2815716420663,122.162222495001)) ;
#91205 = CARTESIAN_POINT('Ctrl Pts',(-20.5265422578919,41.2948564979879,122.399798532575)) ;
#91206 = CARTESIAN_POINT('Ctrl Pts',(-20.6848531440753,41.3048287251607,122.608586988607)) ;
#91207 = CARTESIAN_POINT('Ctrl Pts',(-20.8041778753836,41.3147373415997,122.840061396327)) ;
#91208 = CARTESIAN_POINT('Ctrl Pts',(-20.8825078353512,41.3247905469834,123.092342498857)) ;
#91209 = CARTESIAN_POINT('Ctrl Pts',(-20.9153911019207,41.3346556807437,123.349517175633)) ;
#91210 = CARTESIAN_POINT('Ctrl Pts',(-20.8994532016943,41.34799473837,123.699671410169)) ;
#91211 = CARTESIAN_POINT('Ctrl Pts',(-20.7662682588357,41.3645639257032,124.119498420051)) ;
#91212 = CARTESIAN_POINT('Ctrl Pts',(-20.4969289351474,41.3812090655542,124.470369460942)) ;
#91213 = CARTESIAN_POINT('Ctrl Pts',(-20.2201112015402,41.3944813680276,124.682651973969)) ;
#91214 = CARTESIAN_POINT('Ctrl Pts',(-19.9875982884763,41.4044623314752,124.803972762843)) ;
#91215 = CARTESIAN_POINT('Ctrl Pts',(-19.738528944689,41.4144041635445,124.882935891262)) ;
#91216 = CARTESIAN_POINT('Ctrl Pts',(-19.3916330563447,41.42772373276,124.929305565793)) ;
#91217 = CARTESIAN_POINT('Ctrl Pts',(-18.9557211738586,41.4442538876927,124.873625074331)) ;
#91218 = CARTESIAN_POINT('Ctrl Pts',(-18.4827898293542,41.4642756131848,124.629964635199)) ;
#91219 = CARTESIAN_POINT('Ctrl Pts',(-18.1247913754587,41.4840870097916,124.243659355812)) ;
#91220 = CARTESIAN_POINT('Ctrl Pts',(-17.9175945300158,41.5040722585005,123.754695417451)) ;
#91221 = CARTESIAN_POINT('Ctrl Pts',(-17.8901702572938,41.5239663211364,123.226570828249)) ;
#91222 = CARTESIAN_POINT('Ctrl Pts',(-18.0441233573117,41.54389800031,122.719693569398)) ;
#91223 = CARTESIAN_POINT('Ctrl Pts',(-18.3626064665209,41.563862054782,122.295289089254)) ;
#91224 = CARTESIAN_POINT('Ctrl Pts',(-18.8047488016914,41.5837429565449,122.005904879941)) ;
#91225 = CARTESIAN_POINT('Ctrl Pts',(-19.320432669292,41.6036816181533,121.883949466073)) ;
#91226 = CARTESIAN_POINT('Ctrl Pts',(-19.845694207807,41.6235781434086,121.945081447372)) ;
#91227 = CARTESIAN_POINT('Ctrl Pts',(-20.3189427672172,41.6434731818629,122.181005425179)) ;
#91228 = CARTESIAN_POINT('Ctrl Pts',(-20.6844409401465,41.663437005169,122.565598444425)) ;
#91229 = CARTESIAN_POINT('Ctrl Pts',(-20.8961948389639,41.6833111292981,123.049559754929)) ;
#91230 = CARTESIAN_POINT('Ctrl Pts',(-20.930750337764,41.7032862050253,123.5793623284)) ;
#91231 = CARTESIAN_POINT('Ctrl Pts',(-20.7818779747331,41.7232397743819,124.088362609543)) ;
#91232 = CARTESIAN_POINT('Ctrl Pts',(-20.4708653827436,41.7430776845698,124.514126207426)) ;
#91233 = CARTESIAN_POINT('Ctrl Pts',(-20.0305044149458,41.7630535131407,124.810712363069)) ;
#91234 = CARTESIAN_POINT('Ctrl Pts',(-19.5167523633582,41.782971557851,124.938278605792)) ;
#91235 = CARTESIAN_POINT('Ctrl Pts',(-18.9912886178478,41.8028418036386,124.884326486846)) ;
#91236 = CARTESIAN_POINT('Ctrl Pts',(-18.5120647055615,41.8228908067382,124.651624297318)) ;
#91237 = CARTESIAN_POINT('Ctrl Pts',(-18.1453880278503,41.842670047979,124.274702004828)) ;
#91238 = CARTESIAN_POINT('Ctrl Pts',(-17.9259851440591,41.8627001116879,123.789780611659)) ;
#91239 = CARTESIAN_POINT('Ctrl Pts',(-17.8863697134436,41.8825823965899,123.262746959437)) ;
#91240 = CARTESIAN_POINT('Ctrl Pts',(-18.0275326386484,41.9024646974829,122.753560552606)) ;
#91241 = CARTESIAN_POINT('Ctrl Pts',(-18.3357088896958,41.9224478071012,122.320980688982)) ;
#91242 = CARTESIAN_POINT('Ctrl Pts',(-18.7710306130654,41.9423382024791,122.02096992026)) ;
#91243 = CARTESIAN_POINT('Ctrl Pts',(-19.2824613005974,41.9622349925134,121.886735352838)) ;
#91244 = CARTESIAN_POINT('Ctrl Pts',(-19.8096884308124,41.982152046455,121.934563073507)) ;
#91245 = CARTESIAN_POINT('Ctrl Pts',(-20.2909909356095,42.0021555946585,122.16058890975)) ;
#91246 = CARTESIAN_POINT('Ctrl Pts',(-20.6644231854792,42.0220938883111,122.53654694601)) ;
#91247 = CARTESIAN_POINT('Ctrl Pts',(-20.8870221312374,42.041915375744,123.014039318309)) ;
#91248 = CARTESIAN_POINT('Ctrl Pts',(-20.9342135131919,42.0618937687349,123.542870872687)) ;
#91249 = CARTESIAN_POINT('Ctrl Pts',(-20.7983116521925,42.0817921503486,124.05406099751)) ;
#91250 = CARTESIAN_POINT('Ctrl Pts',(-20.5470876259133,42.0983750810785,124.416078628644)) ;
#91251 = CARTESIAN_POINT('Ctrl Pts',(-20.2810340791425,42.1116493166673,124.641785333089)) ;
#91252 = CARTESIAN_POINT('Ctrl Pts',(-20.0530711216127,42.1216957341235,124.774894284612)) ;
#91253 = CARTESIAN_POINT('Ctrl Pts',(-19.8104700418555,42.1315409593428,124.864850290018)) ;
#91254 = CARTESIAN_POINT('Ctrl Pts',(-19.4658985569829,42.1448759303822,124.928521275722)) ;
#91255 = CARTESIAN_POINT('Ctrl Pts',(-19.0264447066916,42.1614587871748,124.893669283051)) ;
#91256 = CARTESIAN_POINT('Ctrl Pts',(-18.6239261419113,42.1781017895242,124.710472536037)) ;
#91257 = CARTESIAN_POINT('Ctrl Pts',(-18.3550087789404,42.1913455205559,124.489421557899)) ;
#91258 = CARTESIAN_POINT('Ctrl Pts',(-18.1831612885463,42.2013999152305,124.288789628079)) ;
#91259 = CARTESIAN_POINT('Ctrl Pts',(-18.0512749568523,42.2112409766191,124.066279127092)) ;
#91260 = CARTESIAN_POINT('Ctrl Pts',(-17.9577303156056,42.2213072009756,123.818889092396)) ;
#91261 = CARTESIAN_POINT('Ctrl Pts',(-17.9095286836072,42.2311878138952,123.563707583519)) ;
#91262 = CARTESIAN_POINT('Ctrl Pts',(-17.9058337757334,42.2411811070548,123.301162738247)) ;
#91263 = CARTESIAN_POINT('Ctrl Pts',(-17.9475195177784,42.2511321152785,123.042958068114)) ;
#91264 = CARTESIAN_POINT('Ctrl Pts',(-18.0344126776209,42.2611806296404,122.793630948039)) ;
#91265 = CARTESIAN_POINT('Ctrl Pts',(-18.1603920215042,42.2710221357031,122.56773601956)) ;
#91266 = CARTESIAN_POINT('Ctrl Pts',(-18.3255845008848,42.2810077883328,122.363897258987)) ;
#91267 = CARTESIAN_POINT('Ctrl Pts',(-18.5227313519484,42.2909467971777,122.192513006054)) ;
#91268 = CARTESIAN_POINT('Ctrl Pts',(-18.7489176532003,42.3009877224707,122.056676120919)) ;
#91269 = CARTESIAN_POINT('Ctrl Pts',(-18.9915477533087,42.3108780442256,121.96343274295)) ;
#91270 = CARTESIAN_POINT('Ctrl Pts',(-19.2492897392915,42.320874017559,121.912831427002)) ;
#91271 = CARTESIAN_POINT('Ctrl Pts',(-19.510238542724,42.3308054171411,121.90776329539)) ;
#91272 = CARTESIAN_POINT('Ctrl Pts',(-19.7700878324599,42.3408109576181,121.948013744856)) ;
#91273 = CARTESIAN_POINT('Ctrl Pts',(-20.0195067969403,42.3508439415494,122.033453514433)) ;
#91274 = CARTESIAN_POINT('Ctrl Pts',(-20.2464693982846,42.3606995723763,122.158262805078)) ;
#91275 = CARTESIAN_POINT('Ctrl Pts',(-20.4514198298294,42.3706989745694,122.322645616245)) ;
#91276 = CARTESIAN_POINT('Ctrl Pts',(-20.6231827987995,42.3805934439305,122.517917638285)) ;
#91277 = CARTESIAN_POINT('Ctrl Pts',(-20.7606195436203,42.3906565580947,122.743793366782)) ;
#91278 = CARTESIAN_POINT('Ctrl Pts',(-20.8549120164977,42.4004962038111,122.984609559958)) ;
#91279 = CARTESIAN_POINT('Ctrl Pts',(-20.9074321966083,42.4105593713669,123.243754099235)) ;
#91280 = CARTESIAN_POINT('Ctrl Pts',(-20.9138270218801,42.4204536271617,123.503714919927)) ;
#91281 = CARTESIAN_POINT('Ctrl Pts',(-20.8755128410189,42.4303954056214,123.762117252756)) ;
#91282 = CARTESIAN_POINT('Ctrl Pts',(-20.7924756140901,42.4403980984516,124.011553585451)) ;
#91283 = CARTESIAN_POINT('Ctrl Pts',(-20.6666672130897,42.4504321204054,124.243274149404)) ;
#91284 = CARTESIAN_POINT('Ctrl Pts',(-20.5058796969663,42.4602799114944,124.446064360107)) ;
#91285 = CARTESIAN_POINT('Ctrl Pts',(-20.3101026092512,42.4702614360435,124.62060077918)) ;
#91286 = CARTESIAN_POINT('Ctrl Pts',(-20.0876687178098,42.4802106595344,124.758029297087)) ;
#91287 = CARTESIAN_POINT('Ctrl Pts',(-19.8436792195384,42.490208315751,124.855531589647)) ;
#91288 = CARTESIAN_POINT('Ctrl Pts',(-19.5853068270162,42.500248528806,124.908912389975)) ;
#91289 = CARTESIAN_POINT('Ctrl Pts',(-19.3271481560831,42.5100765760823,124.917023207503)) ;
#91290 = CARTESIAN_POINT('Ctrl Pts',(-19.065587620381,42.5201309231147,124.879749670527)) ;
#91291 = CARTESIAN_POINT('Ctrl Pts',(-18.8174156782774,42.5300720594432,124.798125360101)) ;
#91292 = CARTESIAN_POINT('Ctrl Pts',(-18.5876622498009,42.5399762925229,124.675821006536)) ;
#91293 = CARTESIAN_POINT('Ctrl Pts',(-18.3798098223478,42.5500229893665,124.513062959193)) ;
#91294 = CARTESIAN_POINT('Ctrl Pts',(-18.205809991047,42.5599185406468,124.319751471792)) ;
#91295 = CARTESIAN_POINT('Ctrl Pts',(-18.0657424005529,42.5699806184863,124.095520805029)) ;
#91296 = CARTESIAN_POINT('Ctrl Pts',(-17.9687323982393,42.5798233275824,123.855713961264)) ;
#91297 = CARTESIAN_POINT('Ctrl Pts',(-17.9134293922222,42.5898140598208,123.599092869816)) ;
#91298 = CARTESIAN_POINT('Ctrl Pts',(-17.9036266135817,42.5997420850496,123.338364905447)) ;
#91299 = CARTESIAN_POINT('Ctrl Pts',(-17.9390160350888,42.6097302317001,123.078277461847)) ;
#91300 = CARTESIAN_POINT('Ctrl Pts',(-18.0197861525379,42.6197652495401,122.827237976155)) ;
#91301 = CARTESIAN_POINT('Ctrl Pts',(-18.140582591483,42.6296300466453,122.597876275323)) ;
#91302 = CARTESIAN_POINT('Ctrl Pts',(-18.3003156640756,42.6395907790014,122.390498248251)) ;
#91303 = CARTESIAN_POINT('Ctrl Pts',(-18.4953259743341,42.6496242413984,122.213054154998)) ;
#91304 = CARTESIAN_POINT('Ctrl Pts',(-18.7147012146566,42.6595097756098,122.073852925735)) ;
#91305 = CARTESIAN_POINT('Ctrl Pts',(-18.9592157983849,42.6695746162898,121.973094770652)) ;
#91306 = CARTESIAN_POINT('Ctrl Pts',(-19.211976927808,42.6794227480187,121.917420334612)) ;
#91307 = CARTESIAN_POINT('Ctrl Pts',(-19.4752162394926,42.6894502450088,121.905599515675)) ;
#91308 = CARTESIAN_POINT('Ctrl Pts',(-19.7364643783176,42.6994786970539,121.940363154748)) ;
#91309 = CARTESIAN_POINT('Ctrl Pts',(-19.983240895575,42.709323963618,122.018027966902)) ;
#91310 = CARTESIAN_POINT('Ctrl Pts',(-20.2165165477863,42.7193146365589,122.138509322655)) ;
#91311 = CARTESIAN_POINT('Ctrl Pts',(-20.42595149829,42.7293525186474,122.298877797518)) ;
#91312 = CARTESIAN_POINT('Ctrl Pts',(-20.6012619502332,42.739196889087,122.489133616188)) ;
#91313 = CARTESIAN_POINT('Ctrl Pts',(-20.7432777778674,42.7491817164824,122.709727782596)) ;
#91314 = CARTESIAN_POINT('Ctrl Pts',(-20.8445084625415,42.7591211618877,122.950553007713)) ;
#91315 = CARTESIAN_POINT('Ctrl Pts',(-20.902884175201,42.7691611661736,123.207827740318)) ;
#91316 = CARTESIAN_POINT('Ctrl Pts',(-20.9156867364475,42.7790482753592,123.467365079687)) ;
#91317 = CARTESIAN_POINT('Ctrl Pts',(-20.8831915581267,42.7890483352617,123.728098704159)) ;
#91318 = CARTESIAN_POINT('Ctrl Pts',(-20.8067445599132,42.7989657511764,123.977299323762)) ;
#91319 = CARTESIAN_POINT('Ctrl Pts',(-20.686612406926,42.8090125659172,124.212363180922)) ;
#91320 = CARTESIAN_POINT('Ctrl Pts',(-20.5303690658562,42.8188880431139,124.419630089936)) ;
#91321 = CARTESIAN_POINT('Ctrl Pts',(-20.337202917031,42.8289441388351,124.599902985176)) ;
#91322 = CARTESIAN_POINT('Ctrl Pts',(-20.1192329290402,42.8388373008502,124.741697871364)) ;
#91323 = CARTESIAN_POINT('Ctrl Pts',(-19.8759728300273,42.8488995368728,124.845270931614)) ;
#91324 = CARTESIAN_POINT('Ctrl Pts',(-19.6239615863206,42.8587440025017,124.903774649878)) ;
#91325 = CARTESIAN_POINT('Ctrl Pts',(-19.3626527477167,42.8687040952058,124.91873716026)) ;
#91326 = CARTESIAN_POINT('Ctrl Pts',(-19.1007442432168,42.8787423841869,124.887345479684)) ;
#91327 = CARTESIAN_POINT('Ctrl Pts',(-18.852219395114,42.8886157072931,124.812672988231)) ;
#91328 = CARTESIAN_POINT('Ctrl Pts',(-18.6158652448163,42.8986888913782,124.693587821864)) ;
#91329 = CARTESIAN_POINT('Ctrl Pts',(-18.408809846254,42.9085094036661,124.539447907291)) ;
#91330 = CARTESIAN_POINT('Ctrl Pts',(-18.2269164681603,42.9185873997819,124.347038540938)) ;
#91331 = CARTESIAN_POINT('Ctrl Pts',(-18.0843140642102,42.9284414747652,124.130813462835)) ;
#91332 = CARTESIAN_POINT('Ctrl Pts',(-17.9790106190544,42.9385053563489,123.888269164773)) ;
#91333 = CARTESIAN_POINT('Ctrl Pts',(-17.9185491680014,42.9483887823227,123.635632007947)) ;
#91334 = CARTESIAN_POINT('Ctrl Pts',(-17.9022737750403,42.9583893862437,123.373377146627)) ;
#91335 = CARTESIAN_POINT('Ctrl Pts',(-17.9313895259165,42.9683091705816,123.114278441424)) ;
#91336 = CARTESIAN_POINT('Ctrl Pts',(-18.0060320164047,42.9783565209384,122.861060709944)) ;
#91337 = CARTESIAN_POINT('Ctrl Pts',(-18.1212870190588,42.9882338631727,122.628427841327)) ;
#91338 = CARTESIAN_POINT('Ctrl Pts',(-18.2781351229889,42.9983037442474,122.415360927794)) ;
#91339 = CARTESIAN_POINT('Ctrl Pts',(-18.4649150055318,43.008133449449,122.2368543242)) ;
#91340 = CARTESIAN_POINT('Ctrl Pts',(-18.6847596765535,43.0182001106154,122.089792158768)) ;
#91341 = CARTESIAN_POINT('Ctrl Pts',(-18.9226931773935,43.0280903324827,121.985125306975)) ;
#91342 = CARTESIAN_POINT('Ctrl Pts',(-19.1776048761138,43.0380825085929,121.922176627254)) ;
#91343 = CARTESIAN_POINT('Ctrl Pts',(-19.4388303799402,43.0480453387055,121.904745061404)) ;
#91344 = CARTESIAN_POINT('Ctrl Pts',(-19.697682792419,43.0579495511058,121.932114404861)) ;
#91345 = CARTESIAN_POINT('Ctrl Pts',(-19.951683312586,43.0680102651937,122.005359612903)) ;
#91346 = CARTESIAN_POINT('Ctrl Pts',(-20.1841105631504,43.0778497681765,122.118753970002)) ;
#91347 = CARTESIAN_POINT('Ctrl Pts',(-20.3982269814349,43.0879159067429,122.274016136349)) ;
#91348 = CARTESIAN_POINT('Ctrl Pts',(-20.5787646114016,43.0977984212289,122.460756397599)) ;
#91349 = CARTESIAN_POINT('Ctrl Pts',(-20.7261333194938,43.1077907205845,122.678042925821)) ;
#91350 = CARTESIAN_POINT('Ctrl Pts',(-20.833206366185,43.1177437875379,122.916721805344)) ;
#91351 = CARTESIAN_POINT('Ctrl Pts',(-20.897614117175,43.1277784957431,123.172416207021)) ;
#91352 = CARTESIAN_POINT('Ctrl Pts',(-20.9165610195701,43.1376667166473,123.43159275742)) ;
#91353 = CARTESIAN_POINT('Ctrl Pts',(-20.8903677843384,43.1476611396777,123.692911928234)) ;
#91354 = CARTESIAN_POINT('Ctrl Pts',(-20.8194444690435,43.1576064791239,123.944458675462)) ;
#91355 = CARTESIAN_POINT('Ctrl Pts',(-20.7063781227187,43.1675538237352,124.180161559428)) ;
#91356 = CARTESIAN_POINT('Ctrl Pts',(-20.5523346077461,43.1776017191462,124.394608128497)) ;
#91357 = CARTESIAN_POINT('Ctrl Pts',(-20.3673072274807,43.1874493646256,124.575539263631)) ;
#91358 = CARTESIAN_POINT('Ctrl Pts',(-20.1516760965307,43.1974110785396,124.723955111939)) ;
#91359 = CARTESIAN_POINT('Ctrl Pts',(-19.9117864879595,43.2074397028305,124.833114513842)) ;
#91360 = CARTESIAN_POINT('Ctrl Pts',(-19.6596450451628,43.2173500634872,124.898260239512)) ;
#91361 = CARTESIAN_POINT('Ctrl Pts',(-19.3994169455173,43.2272847620605,124.919374953537)) ;
#91362 = CARTESIAN_POINT('Ctrl Pts',(-19.1367199893783,43.2373265869147,124.894463864514)) ;
#91363 = CARTESIAN_POINT('Ctrl Pts',(-18.886225085537,43.2472111606591,124.825627198555)) ;
#91364 = CARTESIAN_POINT('Ctrl Pts',(-18.6486227140851,43.2572130100223,124.713331619215)) ;
#91365 = CARTESIAN_POINT('Ctrl Pts',(-18.4357298701924,43.2671323115963,124.562855492148)) ;
#91366 = CARTESIAN_POINT('Ctrl Pts',(-18.2499252216547,43.2771764199416,124.375414816484)) ;
#91367 = CARTESIAN_POINT('Ctrl Pts',(-18.1017967666107,43.2870608433839,124.162024125329)) ;
#91368 = CARTESIAN_POINT('Ctrl Pts',(-17.9909876140739,43.2970772052933,123.923254596581)) ;
#91369 = CARTESIAN_POINT('Ctrl Pts',(-17.923859840719,43.3071138607987,123.668202194077)) ;
#91370 = CARTESIAN_POINT('Ctrl Pts',(-17.9017809512743,43.316943990988,123.410789908408)) ;
#91371 = CARTESIAN_POINT('Ctrl Pts',(-17.9252094807461,43.3270200440779,123.14709156434)) ;
#91372 = CARTESIAN_POINT('Ctrl Pts',(-17.9924299188192,43.3368722732637,122.897006470178)) ;
#91373 = CARTESIAN_POINT('Ctrl Pts',(-18.1042679823455,43.346945481063,122.657125718903)) ;
#91374 = CARTESIAN_POINT('Ctrl Pts',(-18.2526600247285,43.3567869924144,122.445286955059)) ;
#91375 = CARTESIAN_POINT('Ctrl Pts',(-18.4370833480714,43.3667479304519,122.259535607649)) ;
#91376 = CARTESIAN_POINT('Ctrl Pts',(-18.6529137116503,43.3767857923769,122.107894632329)) ;
#91377 = CARTESIAN_POINT('Ctrl Pts',(-18.8877318802292,43.386659978374,121.997399835187)) ;
#91378 = CARTESIAN_POINT('Ctrl Pts',(-19.1430767424442,43.3967301379519,121.928047356041)) ;
#91379 = CARTESIAN_POINT('Ctrl Pts',(-19.4003939023348,43.4065618853777,121.904482946936)) ;
#91380 = CARTESIAN_POINT('Ctrl Pts',(-19.6632619536359,43.416597965449,121.925714449018)) ;
#91381 = CARTESIAN_POINT('Ctrl Pts',(-19.9178244791952,43.4266150123015,121.992789588399)) ;
#91382 = CARTESIAN_POINT('Ctrl Pts',(-20.1538536760543,43.4364972704681,122.101114447307)) ;
#91383 = CARTESIAN_POINT('Ctrl Pts',(-20.3699131764678,43.4464849532645,122.250085365114)) ;
#91384 = CARTESIAN_POINT('Ctrl Pts',(-20.5562534234135,43.4564316099812,122.433448480984)) ;
#91385 = CARTESIAN_POINT('Ctrl Pts',(-20.7093464656126,43.4664886680613,122.648845014339)) ;
#91386 = CARTESIAN_POINT('Ctrl Pts',(-20.8203630654668,43.4763068476108,122.881767028925)) ;
#91387 = CARTESIAN_POINT('Ctrl Pts',(-20.8914610512173,43.4863427820498,123.135729585425)) ;
#91388 = CARTESIAN_POINT('Ctrl Pts',(-20.9166029199042,43.4963674364788,123.397974203455)) ;
#91389 = CARTESIAN_POINT('Ctrl Pts',(-20.8967578932332,43.5062194560583,123.656117782256)) ;
#91390 = CARTESIAN_POINT('Ctrl Pts',(-20.831881508292,43.5162103697732,123.910494310723)) ;
#91391 = CARTESIAN_POINT('Ctrl Pts',(-20.7247399963963,43.5261283586128,124.148122891889)) ;
#91392 = CARTESIAN_POINT('Ctrl Pts',(-20.5764179652717,43.5361564693436,124.365922998669)) ;
#91393 = CARTESIAN_POINT('Ctrl Pts',(-20.3952122093275,43.546041667252,124.552066450949)) ;
#91394 = CARTESIAN_POINT('Ctrl Pts',(-20.1825938294097,43.55603094252,124.706038954203)) ;
#91395 = CARTESIAN_POINT('Ctrl Pts',(-19.9449996926765,43.5660724006895,124.820834858962)) ;
#91396 = CARTESIAN_POINT('Ctrl Pts',(-19.6965069343808,43.5759038644778,124.89159240592)) ;
#91397 = CARTESIAN_POINT('Ctrl Pts',(-19.4350698137697,43.5859087967817,124.919173839307)) ;
#91398 = CARTESIAN_POINT('Ctrl Pts',(-19.1732351295058,43.5958951606764,124.900827612683)) ;
#91399 = CARTESIAN_POINT('Ctrl Pts',(-18.9175770787377,43.6059247895623,124.836838031948)) ;
#91400 = CARTESIAN_POINT('Ctrl Pts',(-18.6804371598066,43.6158000116707,124.731369996855)) ;
#91401 = CARTESIAN_POINT('Ctrl Pts',(-18.4623477415022,43.6258012240678,124.584774106996)) ;
#91402 = CARTESIAN_POINT('Ctrl Pts',(-18.2745444168899,43.6357098033033,124.404343207406)) ;
#91403 = CARTESIAN_POINT('Ctrl Pts',(-18.1187722259552,43.6457646558593,124.190964881095)) ;
#91404 = CARTESIAN_POINT('Ctrl Pts',(-18.004380821327,43.6556232381341,123.958462580893)) ;
#91405 = CARTESIAN_POINT('Ctrl Pts',(-17.9304301319305,43.6656913675768,123.704467954817)) ;
#91406 = CARTESIAN_POINT('Ctrl Pts',(-17.9023257120292,43.6755468392659,123.446983659363)) ;
#91407 = CARTESIAN_POINT('Ctrl Pts',(-17.9188088681527,43.6855416876521,123.18485588981)) ;
#91408 = CARTESIAN_POINT('Ctrl Pts',(-17.9813360998204,43.6955729844366,122.928761468334)) ;
#91409 = CARTESIAN_POINT('Ctrl Pts',(-18.0852611565216,43.7054395206467,122.691208548975)) ;
#91410 = CARTESIAN_POINT('Ctrl Pts',(-18.2302389701534,43.7154269436075,122.472461402679)) ;
#91411 = CARTESIAN_POINT('Ctrl Pts',(-18.4101746479847,43.7253718826273,122.282878179321)) ;
#91412 = CARTESIAN_POINT('Ctrl Pts',(-18.6224381752842,43.7354167684873,122.125988815331)) ;
#91413 = CARTESIAN_POINT('Ctrl Pts',(-18.8545304610227,43.7452853035735,122.010266829846)) ;
#91414 = CARTESIAN_POINT('Ctrl Pts',(-19.1054170228572,43.7552511715802,121.935180988231)) ;
#91415 = CARTESIAN_POINT('Ctrl Pts',(-19.3670753403128,43.7652738190327,121.904915997745)) ;
#91416 = CARTESIAN_POINT('Ctrl Pts',(-19.6273895696262,43.7751974580403,121.920314786866)) ;
#91417 = CARTESIAN_POINT('Ctrl Pts',(-19.8817360875412,43.785140183046,121.980191368914)) ;
#91418 = CARTESIAN_POINT('Ctrl Pts',(-20.1241540955357,43.7951857890979,122.084667591629)) ;
#91419 = CARTESIAN_POINT('Ctrl Pts',(-20.3408919295591,43.805047211619,122.226772581987)) ;
#91420 = CARTESIAN_POINT('Ctrl Pts',(-20.5324564346371,43.8150407800682,122.406363357882)) ;
#91421 = CARTESIAN_POINT('Ctrl Pts',(-20.6890092975618,43.8249662508235,122.615035530979)) ;
#91422 = CARTESIAN_POINT('Ctrl Pts',(-20.8081450016785,43.8349939247794,122.850047539463)) ;
#91423 = CARTESIAN_POINT('Ctrl Pts',(-20.8838536120231,43.8448811028211,123.098633773252)) ;
#91424 = CARTESIAN_POINT('Ctrl Pts',(-20.9158727010176,43.8549094821892,123.360180929265)) ;
#91425 = CARTESIAN_POINT('Ctrl Pts',(-20.9023154130468,43.8648037249107,123.61987110098)) ;
#91426 = CARTESIAN_POINT('Ctrl Pts',(-20.8237526627658,43.8781566415616,123.961832644244)) ;
#91427 = CARTESIAN_POINT('Ctrl Pts',(-20.659605419344,43.8913591593083,124.272026060151)) ;
#91428 = CARTESIAN_POINT('Ctrl Pts',(-20.4209894341323,43.9047150645893,124.529371523142)) ;
#91429 = CARTESIAN_POINT('Ctrl Pts',(-20.2138465893309,43.9146117132271,124.686685290461)) ;
#91430 = CARTESIAN_POINT('Ctrl Pts',(-19.9790841361338,43.9246598512796,124.807515218539)) ;
#91431 = CARTESIAN_POINT('Ctrl Pts',(-19.7308190710791,43.9345508114574,124.884524562432)) ;
#91432 = CARTESIAN_POINT('Ctrl Pts',(-19.4703839376697,43.9445436473341,124.918248825918)) ;
#91433 = CARTESIAN_POINT('Ctrl Pts',(-19.2068845324014,43.9545827423357,124.905579235426)) ;
#91434 = CARTESIAN_POINT('Ctrl Pts',(-18.9545857300593,43.9644200981869,124.849099649171)) ;
#91435 = CARTESIAN_POINT('Ctrl Pts',(-18.6296690897415,43.9778130461176,124.713956490856)) ;
#91436 = CARTESIAN_POINT('Ctrl Pts',(-18.3520981743961,43.9909797225445,124.500694921199)) ;
#91437 = CARTESIAN_POINT('Ctrl Pts',(-18.1378620138643,44.0043645039513,124.221797775786)) ;
#91438 = CARTESIAN_POINT('Ctrl Pts',(-18.0179672616378,44.0142262865952,123.991995123024)) ;
#91439 = CARTESIAN_POINT('Ctrl Pts',(-17.9383259095293,44.0242254345482,123.741642443432)) ;
#91440 = CARTESIAN_POINT('Ctrl Pts',(-17.9034476011342,44.0341282271653,123.483699776961)) ;
#91441 = CARTESIAN_POINT('Ctrl Pts',(-17.9141092543276,44.0441778070562,123.219886940427)) ;
#91442 = CARTESIAN_POINT('Ctrl Pts',(-17.987359893705,44.0573648808657,122.881047522662)) ;
#91443 = CARTESIAN_POINT('Ctrl Pts',(-18.1910325351083,44.0741176708369,122.485294726917)) ;
#91444 = CARTESIAN_POINT('Ctrl Pts',(-18.5127079665964,44.0906063229316,122.187409946864)) ;
#91445 = CARTESIAN_POINT('Ctrl Pts',(-18.8227881728284,44.103963149115,122.02310778574)) ;
#91446 = CARTESIAN_POINT('Ctrl Pts',(-19.0702563997621,44.1138595339929,121.942965399191)) ;
#91447 = CARTESIAN_POINT('Ctrl Pts',(-19.3306048043616,44.1238660485134,121.906491121348)) ;
#91448 = CARTESIAN_POINT('Ctrl Pts',(-19.6771635039031,44.1370561720298,121.917876124668)) ;
#91449 = CARTESIAN_POINT('Ctrl Pts',(-20.1033013954012,44.1538227331793,122.047686667172)) ;
#91450 = CARTESIAN_POINT('Ctrl Pts',(-20.5238929989773,44.1736072218874,122.363542810504)) ;
#91451 = CARTESIAN_POINT('Ctrl Pts',(-20.815011621917,44.1935526694839,122.806412748844)) ;
#91452 = CARTESIAN_POINT('Ctrl Pts',(-20.9368621718498,44.2134643316398,123.321424916447)) ;
#91453 = CARTESIAN_POINT('Ctrl Pts',(-20.8768657552607,44.2333565236587,123.846793390736)) ;
#91454 = CARTESIAN_POINT('Ctrl Pts',(-20.6387805843268,44.2533976542133,124.323200523711)) ;
#91455 = CARTESIAN_POINT('Ctrl Pts',(-20.2567572002547,44.2732159888289,124.686031568202)) ;
#91456 = CARTESIAN_POINT('Ctrl Pts',(-19.7707167595738,44.2931885540485,124.899018477373)) ;
#91457 = CARTESIAN_POINT('Ctrl Pts',(-19.243012073421,44.3130777702201,124.933377526462)) ;
#91458 = CARTESIAN_POINT('Ctrl Pts',(-18.7322499924567,44.3331013445428,124.784342715249)) ;
#91459 = CARTESIAN_POINT('Ctrl Pts',(-18.3074523247711,44.352898507631,124.473689351128)) ;
#91460 = CARTESIAN_POINT('Ctrl Pts',(-18.0107208479656,44.3728640014548,124.033892370887)) ;
#91461 = CARTESIAN_POINT('Ctrl Pts',(-17.8825301084476,44.3928177091962,123.519135613177)) ;
#91462 = CARTESIAN_POINT('Ctrl Pts',(-17.9375131053142,44.4127250859228,122.993014954846)) ;
#91463 = CARTESIAN_POINT('Ctrl Pts',(-18.1669119070672,44.4325772974714,122.517754743088)) ;
#91464 = CARTESIAN_POINT('Ctrl Pts',(-18.5491999521954,44.4526496844171,122.145668046979)) ;
#91465 = CARTESIAN_POINT('Ctrl Pts',(-19.0301389700753,44.4724875540574,121.9295612266)) ;
#91466 = CARTESIAN_POINT('Ctrl Pts',(-19.556112431027,44.4923382086105,121.888236492257)) ;
#91467 = CARTESIAN_POINT('Ctrl Pts',(-20.0695268056747,44.512390142951,122.031046366895)) ;
#91468 = CARTESIAN_POINT('Ctrl Pts',(-20.4987446170897,44.532223330517,122.337261350157)) ;
#91469 = CARTESIAN_POINT('Ctrl Pts',(-20.7998380093603,44.5521525427477,122.772809047979)) ;
#91470 = CARTESIAN_POINT('Ctrl Pts',(-20.9346380609838,44.5720375079621,123.284047944812)) ;
#91471 = CARTESIAN_POINT('Ctrl Pts',(-20.8856425940297,44.5921112491067,123.815212598448)) ;
#91472 = CARTESIAN_POINT('Ctrl Pts',(-20.6614851629729,44.6119044308871,124.291227274791)) ;
#91473 = CARTESIAN_POINT('Ctrl Pts',(-20.2863772074548,44.6318671388898,124.666405427892)) ;
#91474 = CARTESIAN_POINT('Ctrl Pts',(-19.8046798286043,44.6518500906322,124.8901432235)) ;
#91475 = CARTESIAN_POINT('Ctrl Pts',(-19.2801648941078,44.6716607104044,124.936716143029)) ;
#91476 = CARTESIAN_POINT('Ctrl Pts',(-18.7667918531497,44.6916444264373,124.800971420717)) ;
#91477 = CARTESIAN_POINT('Ctrl Pts',(-18.332633623527,44.7115258903346,124.499523849295)) ;
#91478 = CARTESIAN_POINT('Ctrl Pts',(-18.0261041134591,44.731481220179,124.066823654643)) ;
#91479 = CARTESIAN_POINT('Ctrl Pts',(-17.8857718639008,44.7513566809845,123.557460531844)) ;
#91480 = CARTESIAN_POINT('Ctrl Pts',(-17.9275871464799,44.771341001036,123.028016369146)) ;
#91481 = CARTESIAN_POINT('Ctrl Pts',(-18.1472823916272,44.7912690338256,122.54594681577)) ;
#91482 = CARTESIAN_POINT('Ctrl Pts',(-18.4563072638141,44.8078777957654,122.230852995871)) ;
#91483 = CARTESIAN_POINT('Ctrl Pts',(-18.7544344166136,44.8210654344555,122.054104346629)) ;
#91484 = CARTESIAN_POINT('Ctrl Pts',(-18.9997577413404,44.8310518688156,121.960933276629)) ;
#91485 = CARTESIAN_POINT('Ctrl Pts',(-19.2582000487417,44.841061242775,121.911919172374)) ;
#91486 = CARTESIAN_POINT('Ctrl Pts',(-19.6074259157018,44.8543512763403,121.90718231146)) ;
#91487 = CARTESIAN_POINT('Ctrl Pts',(-20.0350744145889,44.8709452640027,122.015110092288)) ;
#91488 = CARTESIAN_POINT('Ctrl Pts',(-20.4010334172279,44.8875775192782,122.263044894367)) ;
#91489 = CARTESIAN_POINT('Ctrl Pts',(-20.6289076195677,44.9008199029461,122.52606867887)) ;
#91490 = CARTESIAN_POINT('Ctrl Pts',(-20.7634193394176,44.9107341111735,122.749205301052)) ;
#91491 = CARTESIAN_POINT('Ctrl Pts',(-20.8581992855926,44.9207907504452,122.995881649194)) ;
#91492 = CARTESIAN_POINT('Ctrl Pts',(-20.9079626866539,44.9306365568653,123.249811042525)) ;
#91493 = CARTESIAN_POINT('Ctrl Pts',(-20.9134321153544,44.9406815564985,123.513714183674)) ;
#91494 = CARTESIAN_POINT('Ctrl Pts',(-20.8594529735354,44.9539625788713,123.85851431483)) ;
#91495 = CARTESIAN_POINT('Ctrl Pts',(-20.7185138341195,44.9671600253959,124.179729076087)) ;
#91496 = CARTESIAN_POINT('Ctrl Pts',(-20.4978542341181,44.9805743232029,124.454653630732)) ;
#91497 = CARTESIAN_POINT('Ctrl Pts',(-20.3035482186063,44.9904133886056,124.625258093541)) ;
#91498 = CARTESIAN_POINT('Ctrl Pts',(-20.0797292255048,45.0003965948833,124.762068121514)) ;
#91499 = CARTESIAN_POINT('Ctrl Pts',(-19.8362653995539,45.0103478297961,124.857563683997)) ;
#91500 = CARTESIAN_POINT('Ctrl Pts',(-19.5787021577369,45.0203488294977,124.90990497468)) ;
#91501 = CARTESIAN_POINT('Ctrl Pts',(-19.3151704808666,45.0303801752851,124.916336383632)) ;
#91502 = CARTESIAN_POINT('Ctrl Pts',(-19.059076565559,45.0402339399901,124.877961736359)) ;
#91503 = CARTESIAN_POINT('Ctrl Pts',(-18.8104579041759,45.0502045936584,124.795331193507)) ;
#91504 = CARTESIAN_POINT('Ctrl Pts',(-18.5792936637788,45.0602018373156,124.670414452979)) ;
#91505 = CARTESIAN_POINT('Ctrl Pts',(-18.372843216216,45.0702352932598,124.506439042019)) ;
#91506 = CARTESIAN_POINT('Ctrl Pts',(-18.2007560512662,45.0800907975602,124.312851502277)) ;
#91507 = CARTESIAN_POINT('Ctrl Pts',(-18.0626513107753,45.0900902338463,124.08934966355)) ;
#91508 = CARTESIAN_POINT('Ctrl Pts',(-17.966160872868,45.0999846933622,123.847847223486)) ;
#91509 = CARTESIAN_POINT('Ctrl Pts',(-17.9122601551696,45.1100478128138,123.588997131048)) ;
#91510 = CARTESIAN_POINT('Ctrl Pts',(-17.9040157128179,45.1198874472258,123.330510182851)) ;
#91511 = CARTESIAN_POINT('Ctrl Pts',(-17.9412701233928,45.1299506547116,123.068734224408)) ;
#91512 = CARTESIAN_POINT('Ctrl Pts',(-18.0222577929814,45.1398447620908,122.821630638561)) ;
#91513 = CARTESIAN_POINT('Ctrl Pts',(-18.1448705736183,45.1497870942832,122.590953885684)) ;
#91514 = CARTESIAN_POINT('Ctrl Pts',(-18.3065622324811,45.1597877205982,122.383723321206)) ;
#91515 = CARTESIAN_POINT('Ctrl Pts',(-18.502862990913,45.1698294548801,122.207402005079)) ;
#91516 = CARTESIAN_POINT('Ctrl Pts',(-18.7217059912546,45.1796548808292,122.070339801105)) ;
#91517 = CARTESIAN_POINT('Ctrl Pts',(-18.966474765151,45.1897117073569,121.970725354272)) ;
#91518 = CARTESIAN_POINT('Ctrl Pts',(-19.2216074988033,45.1996391404784,121.916190939513)) ;
#91519 = CARTESIAN_POINT('Ctrl Pts',(-19.4828944941186,45.2095891328847,121.906015436364)) ;
#91520 = CARTESIAN_POINT('Ctrl Pts',(-19.7446272926651,45.2196443339587,121.942195083293)) ;
#91521 = CARTESIAN_POINT('Ctrl Pts',(-19.9904565700812,45.229466608011,122.020960921677)) ;
#91522 = CARTESIAN_POINT('Ctrl Pts',(-20.2244926759389,45.2395225019702,122.143638300963)) ;
#91523 = CARTESIAN_POINT('Ctrl Pts',(-20.4310152546762,45.2494632238153,122.303624668569)) ;
#91524 = CARTESIAN_POINT('Ctrl Pts',(-20.6065787562621,45.2593675679019,122.495779589979)) ;
#91525 = CARTESIAN_POINT('Ctrl Pts',(-20.7479598031112,45.2694142352014,122.718723494218)) ;
#91526 = CARTESIAN_POINT('Ctrl Pts',(-20.847214873449,45.2793097936513,122.959126759267)) ;
#91527 = CARTESIAN_POINT('Ctrl Pts',(-20.9041452558885,45.289371872356,123.217307547921)) ;
#91528 = CARTESIAN_POINT('Ctrl Pts',(-20.9152880545128,45.2992145708218,123.475752573775)) ;
#91529 = CARTESIAN_POINT('Ctrl Pts',(-20.8815017658848,45.3092053447163,123.736083691839)) ;
#91530 = CARTESIAN_POINT('Ctrl Pts',(-20.803464341165,45.3191332139512,123.985045208885)) ;
#91531 = CARTESIAN_POINT('Ctrl Pts',(-20.6830597025419,45.329121942921,124.218310172985)) ;
#91532 = CARTESIAN_POINT('Ctrl Pts',(-20.5228027489551,45.3391613449048,124.427867674991)) ;
#91533 = CARTESIAN_POINT('Ctrl Pts',(-20.3327730605954,45.3490015126416,124.603267061586)) ;
#91534 = CARTESIAN_POINT('Ctrl Pts',(-20.1108060666027,45.3590497230161,124.746272176201)) ;
#91535 = CARTESIAN_POINT('Ctrl Pts',(-19.8696532867426,45.3689968933038,124.847160076547)) ;
#91536 = CARTESIAN_POINT('Ctrl Pts',(-19.6157459454995,45.3789077415589,124.90519559881)) ;
#91537 = CARTESIAN_POINT('Ctrl Pts',(-19.3518125734357,45.3889640692367,124.918205064877)) ;
#91538 = CARTESIAN_POINT('Ctrl Pts',(-19.0949419766038,45.3988144820052,124.886084607511)) ;
#91539 = CARTESIAN_POINT('Ctrl Pts',(-18.8429458077784,45.4088413678389,124.809102515911)) ;
#91540 = CARTESIAN_POINT('Ctrl Pts',(-18.6084007715185,45.4188699834697,124.688897924885)) ;
#91541 = CARTESIAN_POINT('Ctrl Pts',(-18.4018578835291,45.4287152068472,124.533108889477)) ;
#91542 = CARTESIAN_POINT('Ctrl Pts',(-18.2223677576914,45.4387058889488,124.341493091567)) ;
#91543 = CARTESIAN_POINT('Ctrl Pts',(-18.0786949591788,45.4487437775813,124.120270887316)) ;
#91544 = CARTESIAN_POINT('Ctrl Pts',(-17.9771820255855,45.4585881126844,123.882309246234)) ;
#91545 = CARTESIAN_POINT('Ctrl Pts',(-17.9171992662685,45.4685730748819,123.62689961788)) ;
#91546 = CARTESIAN_POINT('Ctrl Pts',(-17.9024172623288,45.4785120164153,123.366094931073)) ;
#91547 = CARTESIAN_POINT('Ctrl Pts',(-17.9335377045302,45.4885539013867,123.104071689988)) ;
#91548 = CARTESIAN_POINT('Ctrl Pts',(-18.0083583615695,45.498440449295,122.855243316233)) ;
#91549 = CARTESIAN_POINT('Ctrl Pts',(-18.1261441567159,45.508434374795,122.620545045069)) ;
#91550 = CARTESIAN_POINT('Ctrl Pts',(-18.2819302055561,45.5183704659215,122.410950315548)) ;
#91551 = CARTESIAN_POINT('Ctrl Pts',(-18.4735027254418,45.5283997349014,122.229995789476)) ;
#91552 = CARTESIAN_POINT('Ctrl Pts',(-18.690241481066,45.5382821174607,122.086859617476)) ;
#91553 = CARTESIAN_POINT('Ctrl Pts',(-18.9325349471609,45.5483346345486,121.981703543276)) ;
#91554 = CARTESIAN_POINT('Ctrl Pts',(-19.185413729496,45.5582287553725,121.921034104185)) ;
#91555 = CARTESIAN_POINT('Ctrl Pts',(-19.4493049697019,45.5682907347929,121.904866941073)) ;
#91556 = CARTESIAN_POINT('Ctrl Pts',(-19.7063630081236,45.5781352680218,121.934093132553)) ;
#91557 = CARTESIAN_POINT('Ctrl Pts',(-19.9576058706028,45.5880953469281,122.007462571973)) ;
#91558 = CARTESIAN_POINT('Ctrl Pts',(-20.1938981415272,45.5981336235007,122.124711964626)) ;
#91559 = CARTESIAN_POINT('Ctrl Pts',(-20.4030909048024,45.6080070100386,122.278267729606)) ;
#91560 = CARTESIAN_POINT('Ctrl Pts',(-20.5859499300167,45.6180799528056,122.469592306891)) ;
#91561 = CARTESIAN_POINT('Ctrl Pts',(-20.7294620067179,45.6279013669339,122.684171707813)) ;
#91562 = CARTESIAN_POINT('Ctrl Pts',(-20.836469961144,45.6379759970062,122.92628036698)) ;
#91563 = CARTESIAN_POINT('Ctrl Pts',(-20.8984204591589,45.6478426343231,123.178089581566)) ;
#91564 = CARTESIAN_POINT('Ctrl Pts',(-20.9166539511471,45.6578661796949,123.440853736035)) ;
#91565 = CARTESIAN_POINT('Ctrl Pts',(-20.8883451902421,45.6678919312121,123.702810647261)) ;
#91566 = CARTESIAN_POINT('Ctrl Pts',(-20.8166655858108,45.6777455182215,123.951620064222)) ;
#91567 = CARTESIAN_POINT('Ctrl Pts',(-20.7020665615135,45.6877224784494,124.187438612339)) ;
#91568 = CARTESIAN_POINT('Ctrl Pts',(-20.5472320226334,45.6977436214779,124.400440473039)) ;
#91569 = CARTESIAN_POINT('Ctrl Pts',(-20.3607129644231,45.7076262274978,124.581203675269)) ;
#91570 = CARTESIAN_POINT('Ctrl Pts',(-20.1416041543845,45.7176946981305,124.729442692636)) ;
#91571 = CARTESIAN_POINT('Ctrl Pts',(-19.9058440233542,45.7275247813142,124.835139992)) ;
#91572 = CARTESIAN_POINT('Ctrl Pts',(-19.6494558792354,45.7375913409946,124.900127141566)) ;
#91573 = CARTESIAN_POINT('Ctrl Pts',(-19.3902123872049,45.7474815908238,124.919112847795)) ;
#91574 = CARTESIAN_POINT('Ctrl Pts',(-19.1289348372093,45.7574737565726,124.893103063459)) ;
#91575 = CARTESIAN_POINT('Ctrl Pts',(-18.8769434953996,45.7674366001687,124.822088336448)) ;
#91576 = CARTESIAN_POINT('Ctrl Pts',(-18.6421852615433,45.7773407689965,124.709652708434)) ;
#91577 = CARTESIAN_POINT('Ctrl Pts',(-18.4273528974957,45.7874016438908,124.555606852268)) ;
#91578 = CARTESIAN_POINT('Ctrl Pts',(-18.2462968796542,45.7972405472202,124.370967398921)) ;
#91579 = CARTESIAN_POINT('Ctrl Pts',(-18.0964786782735,45.8073089235941,124.152936536302)) ;
#91580 = CARTESIAN_POINT('Ctrl Pts',(-17.9888851621427,45.8171895402267,123.916582846629)) ;
#91581 = CARTESIAN_POINT('Ctrl Pts',(-17.9227453188288,45.8271807004557,123.662532284139)) ;
#91582 = CARTESIAN_POINT('Ctrl Pts',(-17.9017535244661,45.8371337738878,123.401780145108)) ;
#91583 = CARTESIAN_POINT('Ctrl Pts',(-17.9266404178476,45.8471696095005,123.139247618234)) ;
#91584 = CARTESIAN_POINT('Ctrl Pts',(-17.9955552265189,45.8570597362306,122.888631027566)) ;
#91585 = CARTESIAN_POINT('Ctrl Pts',(-18.1076934818933,45.8670519179999,122.651211136144)) ;
#91586 = CARTESIAN_POINT('Ctrl Pts',(-18.2587304245374,45.8769978579744,122.437900289644)) ;
#91587 = CARTESIAN_POINT('Ctrl Pts',(-18.4441704878577,45.8869450417339,122.253645296691)) ;
#91588 = CARTESIAN_POINT('Ctrl Pts',(-18.6611101574099,45.8969929800242,122.103131587065)) ;
#91589 = CARTESIAN_POINT('Ctrl Pts',(-18.8960272898149,45.9068406148377,121.994572618097)) ;
#91590 = CARTESIAN_POINT('Ctrl Pts',(-19.148898873225,45.9168023285357,121.926896838604)) ;
#91591 = CARTESIAN_POINT('Ctrl Pts',(-19.4114894160667,45.9268309643569,121.904333417555)) ;
#91592 = CARTESIAN_POINT('Ctrl Pts',(-19.6708912056313,45.9367412791087,121.92734461787)) ;
#91593 = CARTESIAN_POINT('Ctrl Pts',(-19.9231784918885,45.9466761497713,121.994557839022)) ;
#91594 = CARTESIAN_POINT('Ctrl Pts',(-20.1623713001247,45.9567173321731,122.10595274913)) ;
#91595 = CARTESIAN_POINT('Ctrl Pts',(-20.3754171966407,45.9666043036378,122.254712550326)) ;
#91596 = CARTESIAN_POINT('Ctrl Pts',(-20.5616853384859,45.9766037359004,122.440014625736)) ;
#91597 = CARTESIAN_POINT('Ctrl Pts',(-20.7119304588546,45.986523801157,122.65309125952)) ;
#91598 = CARTESIAN_POINT('Ctrl Pts',(-20.8242304858689,45.9965606537412,122.891731631287)) ;
#91599 = CARTESIAN_POINT('Ctrl Pts',(-20.8925312466949,46.0064733130812,123.143117767075)) ;
#91600 = CARTESIAN_POINT('Ctrl Pts',(-20.9169022735991,46.0164645249961,123.404558617935)) ;
#91601 = CARTESIAN_POINT('Ctrl Pts',(-20.8948119575861,46.0265061663992,123.667495012575)) ;
#91602 = CARTESIAN_POINT('Ctrl Pts',(-20.8294454785966,46.0363349606062,123.917414465479)) ;
#91603 = CARTESIAN_POINT('Ctrl Pts',(-20.7191022663443,46.0464113717275,124.158067817818)) ;
#91604 = CARTESIAN_POINT('Ctrl Pts',(-20.5720475565284,46.05626350477,124.371223090758)) ;
#91605 = CARTESIAN_POINT('Ctrl Pts',(-20.3863654461432,46.0663367391113,124.559830827429)) ;
#91606 = CARTESIAN_POINT('Ctrl Pts',(-20.1756244871386,46.0761782404379,124.709777652691)) ;
#91607 = CARTESIAN_POINT('Ctrl Pts',(-19.9396627498854,46.0861391920327,124.823081201135)) ;
#91608 = CARTESIAN_POINT('Ctrl Pts',(-19.6855248863959,46.0961770097533,124.893729687363)) ;
#91609 = CARTESIAN_POINT('Ctrl Pts',(-19.427262518452,46.1060513590104,124.919247547046)) ;
#91610 = CARTESIAN_POINT('Ctrl Pts',(-19.1634478041723,46.1161209097526,124.899133803632)) ;
#91611 = CARTESIAN_POINT('Ctrl Pts',(-18.9130319171502,46.1259549292612,124.835182189416)) ;
#91612 = CARTESIAN_POINT('Ctrl Pts',(-18.6724817634697,46.1359890838408,124.727205773932)) ;
#91613 = CARTESIAN_POINT('Ctrl Pts',(-18.4550722737311,46.1460050096632,124.57881549919)) ;
#91614 = CARTESIAN_POINT('Ctrl Pts',(-18.2689263313037,46.1558872648575,124.397725200321)) ;
#91615 = CARTESIAN_POINT('Ctrl Pts',(-18.1151695920916,46.1658760713684,124.185010592068)) ;
#91616 = CARTESIAN_POINT('Ctrl Pts',(-18.0009343743277,46.1758246386311,123.949804922474)) ;
#91617 = CARTESIAN_POINT('Ctrl Pts',(-17.9287986502812,46.1858794439331,123.695642276881)) ;
#91618 = CARTESIAN_POINT('Ctrl Pts',(-17.9021457183122,46.1956982271967,123.438981604419)) ;
#91619 = CARTESIAN_POINT('Ctrl Pts',(-17.920160334372,46.2057339995573,123.175874359375)) ;
#91620 = CARTESIAN_POINT('Ctrl Pts',(-17.984249977082,46.2157586985859,122.920340925666)) ;
#91621 = CARTESIAN_POINT('Ctrl Pts',(-18.0893591005861,46.225610701845,122.683731790801)) ;
#91622 = CARTESIAN_POINT('Ctrl Pts',(-18.2356413391738,46.2356016362422,122.465745544367)) ;
#91623 = CARTESIAN_POINT('Ctrl Pts',(-18.4161423749505,46.2455195586733,122.277688444646)) ;
#91624 = CARTESIAN_POINT('Ctrl Pts',(-18.6288192425981,46.2555479143556,122.122101309996)) ;
#91625 = CARTESIAN_POINT('Ctrl Pts',(-18.8618561314838,46.2654321988662,122.007348465011)) ;
#91626 = CARTESIAN_POINT('Ctrl Pts',(-19.1138378721338,46.2754248827741,121.933438370644)) ;
#91627 = CARTESIAN_POINT('Ctrl Pts',(-19.3758193880109,46.2854536197818,121.904757212364)) ;
#91628 = CARTESIAN_POINT('Ctrl Pts',(-19.6350724012937,46.2953390164107,121.921411675567)) ;
#91629 = CARTESIAN_POINT('Ctrl Pts',(-19.8901659266548,46.3053269018246,121.983092596544)) ;
#91630 = CARTESIAN_POINT('Ctrl Pts',(-20.1298859961201,46.3152776044852,122.087654097686)) ;
#91631 = CARTESIAN_POINT('Ctrl Pts',(-20.3496387002322,46.3253179225826,122.233636338155)) ;
#91632 = CARTESIAN_POINT('Ctrl Pts',(-20.5377696612843,46.3351924879158,122.412406684327)) ;
#91633 = CARTESIAN_POINT('Ctrl Pts',(-20.6941818778816,46.3451921479769,122.623513973067)) ;
#91634 = CARTESIAN_POINT('Ctrl Pts',(-20.8107624841862,46.3551011431446,122.856409152193)) ;
#91635 = CARTESIAN_POINT('Ctrl Pts',(-20.8861223158461,46.3651558843079,123.109617925359)) ;
#91636 = CARTESIAN_POINT('Ctrl Pts',(-20.9160894530664,46.3750144962217,123.366999052458)) ;
#91637 = CARTESIAN_POINT('Ctrl Pts',(-20.90075393306,46.385082618501,123.631095083211)) ;
#91638 = CARTESIAN_POINT('Ctrl Pts',(-20.8410490247791,46.3949380892042,123.883133457476)) ;
#91639 = CARTESIAN_POINT('Ctrl Pts',(-20.7377739074065,46.4049329486976,124.124622613945)) ;
#91640 = CARTESIAN_POINT('Ctrl Pts',(-20.5931317991477,46.4149642020395,124.345013634199)) ;
#91641 = CARTESIAN_POINT('Ctrl Pts',(-20.4156811920431,46.4248309009126,124.534077171764)) ;
#91642 = CARTESIAN_POINT('Ctrl Pts',(-20.2058603225502,46.4348177166638,124.691672146936)) ;
#91643 = CARTESIAN_POINT('Ctrl Pts',(-19.9727878453625,46.4447649218593,124.810106319578)) ;
#91644 = CARTESIAN_POINT('Ctrl Pts',(-19.7203014995016,46.4548079099855,124.886878521839)) ;
#91645 = CARTESIAN_POINT('Ctrl Pts',(-19.462892547754,46.464675264607,124.918244909157)) ;
#91646 = CARTESIAN_POINT('Ctrl Pts',(-19.2013450743715,46.4746411579051,124.905008550705)) ;
#91647 = CARTESIAN_POINT('Ctrl Pts',(-18.9446202495613,46.4846649352812,124.845948246086)) ;
#91648 = CARTESIAN_POINT('Ctrl Pts',(-18.7044304082566,46.4945904832129,124.744281867912)) ;
#91649 = CARTESIAN_POINT('Ctrl Pts',(-18.4848534110883,46.5045309596339,124.60274474947)) ;
#91650 = CARTESIAN_POINT('Ctrl Pts',(-18.2913765899753,46.5145771692968,124.423144114639)) ;
#91651 = CARTESIAN_POINT('Ctrl Pts',(-18.1347125364933,46.5244384259586,124.216689383634)) ;
#91652 = CARTESIAN_POINT('Ctrl Pts',(-18.0143126829843,46.5344320542339,123.983335039586)) ;
#91653 = CARTESIAN_POINT('Ctrl Pts',(-17.9366394008495,46.5443574515441,123.734298668841)) ;
#91654 = CARTESIAN_POINT('Ctrl Pts',(-17.9030455996264,46.5543853594543,123.472960192196)) ;
#91655 = CARTESIAN_POINT('Ctrl Pts',(-17.9149012642186,46.5642716751235,123.213390481439)) ;
#91656 = CARTESIAN_POINT('Ctrl Pts',(-17.972325349276,46.5743032700273,122.956144198347)) ;
#91657 = CARTESIAN_POINT('Ctrl Pts',(-18.0718482092479,46.584185512979,122.716230515682)) ;
#91658 = CARTESIAN_POINT('Ctrl Pts',(-18.2138880944537,46.5942449840088,122.493315287928)) ;
#91659 = CARTESIAN_POINT('Ctrl Pts',(-18.3891039122629,46.604111428672,122.302179808622)) ;
#91660 = CARTESIAN_POINT('Ctrl Pts',(-18.596403594826,46.6140775531207,122.142134294108)) ;
#91661 = CARTESIAN_POINT('Ctrl Pts',(-18.8300357306055,46.6241077965118,122.020104455616)) ;
#91662 = CARTESIAN_POINT('Ctrl Pts',(-19.0777840409719,46.6340008314649,121.941221742418)) ;
#91663 = CARTESIAN_POINT('Ctrl Pts',(-19.3395213808909,46.6440517457017,121.905936560177)) ;
#91664 = CARTESIAN_POINT('Ctrl Pts',(-19.5992144386022,46.6539415719263,121.916434213114)) ;
#91665 = CARTESIAN_POINT('Ctrl Pts',(-19.9417614873954,46.6672763869732,121.990497581648)) ;
#91666 = CARTESIAN_POINT('Ctrl Pts',(-20.2554096954557,46.6805534781447,122.152105027392)) ;
#91667 = CARTESIAN_POINT('Ctrl Pts',(-20.5136667534488,46.693801766743,122.385643139726)) ;
#91668 = CARTESIAN_POINT('Ctrl Pts',(-20.6757363842069,46.7038566082371,122.594281387087)) ;
#91669 = CARTESIAN_POINT('Ctrl Pts',(-20.7967988624566,46.7136875975446,122.822559708019)) ;
#91670 = CARTESIAN_POINT('Ctrl Pts',(-20.8785312557402,46.7237641618679,123.074384834974)) ;
#91671 = CARTESIAN_POINT('Ctrl Pts',(-20.9144702982914,46.7336134870018,123.33073485832)) ;
#91672 = CARTESIAN_POINT('Ctrl Pts',(-20.9029684187357,46.7469614866391,123.681333495441)) ;
#91673 = CARTESIAN_POINT('Ctrl Pts',(-20.7745139330427,46.7635462461757,124.102969724517)) ;
#91674 = CARTESIAN_POINT('Ctrl Pts',(-20.5110315388571,46.7801147975237,124.4557847313)) ;
#91675 = CARTESIAN_POINT('Ctrl Pts',(-20.23514044175,46.7934746223427,124.672959741583)) ;
#91676 = CARTESIAN_POINT('Ctrl Pts',(-20.0058449666823,46.8033800311734,124.796184304861)) ;
#91677 = CARTESIAN_POINT('Ctrl Pts',(-19.7574240387125,46.8133400577574,124.878527441293)) ;
#91678 = CARTESIAN_POINT('Ctrl Pts',(-19.4127438329402,46.8265976419427,124.929510558515)) ;
#91679 = CARTESIAN_POINT('Ctrl Pts',(-18.9730785233433,46.8432488534374,124.87894995727)) ;
#91680 = CARTESIAN_POINT('Ctrl Pts',(-18.4995437565153,46.8631670675477,124.642323373345)) ;
#91681 = CARTESIAN_POINT('Ctrl Pts',(-18.1350267198472,46.8830448307685,124.259795228635)) ;
#91682 = CARTESIAN_POINT('Ctrl Pts',(-17.9219959153182,46.9030574985557,123.772520415574)) ;
#91683 = CARTESIAN_POINT('Ctrl Pts',(-17.8878670522062,46.9228700212223,123.246943798671)) ;
#91684 = CARTESIAN_POINT('Ctrl Pts',(-18.035546506357,46.9428533212222,122.736872230293)) ;
#91685 = CARTESIAN_POINT('Ctrl Pts',(-18.3474461325361,46.9627475983235,122.309804698334)) ;
#91686 = CARTESIAN_POINT('Ctrl Pts',(-18.7866677876835,46.9826803600813,122.013601770197)) ;
#91687 = CARTESIAN_POINT('Ctrl Pts',(-19.3015657425341,47.002646365846,121.885203552185)) ;
#91688 = CARTESIAN_POINT('Ctrl Pts',(-19.8271303436553,47.0225248980109,121.939603120483)) ;
#91689 = CARTESIAN_POINT('Ctrl Pts',(-20.3041868868379,47.0424645646712,122.170298147785)) ;
#91690 = CARTESIAN_POINT('Ctrl Pts',(-20.6732403950815,47.0623594393166,122.549057326393)) ;
#91691 = CARTESIAN_POINT('Ctrl Pts',(-20.8914282381446,47.0822665786099,123.030940138027)) ;
#91692 = CARTESIAN_POINT('Ctrl Pts',(-20.9330126326835,47.1021771266884,123.558665033763)) ;
#91693 = CARTESIAN_POINT('Ctrl Pts',(-20.7897985089648,47.1222457120455,124.072348596256)) ;
#91694 = CARTESIAN_POINT('Ctrl Pts',(-20.4845832960142,47.1420275093603,124.500664842063)) ;
#91695 = CARTESIAN_POINT('Ctrl Pts',(-20.0473415775769,47.1620350563049,124.802948543256)) ;
#91696 = CARTESIAN_POINT('Ctrl Pts',(-19.5376373388019,47.1818567946077,124.936737621714)) ;
#91697 = CARTESIAN_POINT('Ctrl Pts',(-19.0088143994453,47.2018368145119,124.889159509882)) ;
#91698 = CARTESIAN_POINT('Ctrl Pts',(-18.5296831814101,47.2217542657741,124.664016484713)) ;
#91699 = CARTESIAN_POINT('Ctrl Pts',(-18.156054658413,47.2416291869468,124.290549692997)) ;
#91700 = CARTESIAN_POINT('Ctrl Pts',(-17.9309560929439,47.2616535554976,123.808318679437)) ;
#91701 = CARTESIAN_POINT('Ctrl Pts',(-17.8844429064027,47.2815202398711,123.282262426708)) ;
#91702 = CARTESIAN_POINT('Ctrl Pts',(-18.0199062073946,47.3014640617173,122.769851703785)) ;
#91703 = CARTESIAN_POINT('Ctrl Pts',(-18.321723185349,47.3213714309688,122.335270498965)) ;
#91704 = CARTESIAN_POINT('Ctrl Pts',(-18.7524373240201,47.3412461287155,122.029471467672)) ;
#91705 = CARTESIAN_POINT('Ctrl Pts',(-19.2643995478987,47.3612280712373,121.888115658735)) ;
#91706 = CARTESIAN_POINT('Ctrl Pts',(-19.7916438055128,47.3811307381481,121.930221264192)) ;
#91707 = CARTESIAN_POINT('Ctrl Pts',(-20.2724952367668,47.4009860956868,122.147830932133)) ;
#91708 = CARTESIAN_POINT('Ctrl Pts',(-20.6536636578321,47.4210501344028,122.52065673183)) ;
#91709 = CARTESIAN_POINT('Ctrl Pts',(-20.8822481029672,47.4409053141279,122.996516067802)) ;
#91710 = CARTESIAN_POINT('Ctrl Pts',(-20.935436165233,47.4608854187923,123.524678358585)) ;
#91711 = CARTESIAN_POINT('Ctrl Pts',(-20.8068403946321,47.4806945239621,124.035381850163)) ;
#91712 = CARTESIAN_POINT('Ctrl Pts',(-20.5095795524021,47.5006871443028,124.475622450521)) ;
#91713 = CARTESIAN_POINT('Ctrl Pts',(-20.1539694207839,47.5172266268069,124.734264236863)) ;
#91714 = CARTESIAN_POINT('Ctrl Pts',(-19.8262823346885,47.5305909448711,124.860472249389)) ;
#91715 = CARTESIAN_POINT('Ctrl Pts',(-19.485405542771,47.5438085473726,124.927559945783)) ;
#91716 = CARTESIAN_POINT('Ctrl Pts',(-19.0437703200357,47.5604661416504,124.898016262381)) ;
#91717 = CARTESIAN_POINT('Ctrl Pts',(-18.5604499932118,47.5803318436921,124.685212590745)) ;
#91718 = CARTESIAN_POINT('Ctrl Pts',(-18.2406362283115,47.5969615703822,124.380257695188)) ;
#91719 = CARTESIAN_POINT('Ctrl Pts',(-18.0589404833083,47.61025068552,124.081950760843)) ;
#91720 = CARTESIAN_POINT('Ctrl Pts',(-17.9633474747988,47.6202150324971,123.838187618009)) ;
#91721 = CARTESIAN_POINT('Ctrl Pts',(-17.9115445460179,47.6301434004986,123.582486569596)) ;
#91722 = CARTESIAN_POINT('Ctrl Pts',(-17.9020103793018,47.6434268335873,123.233497874318)) ;
#91723 = CARTESIAN_POINT('Ctrl Pts',(-18.005095080809,47.6600789113277,122.803114333347)) ;
#91724 = CARTESIAN_POINT('Ctrl Pts',(-18.247209882945,47.6766302806285,122.435837759358)) ;
#91725 = CARTESIAN_POINT('Ctrl Pts',(-18.50783847541,47.6899177087775,122.203427580766)) ;
#91726 = CARTESIAN_POINT('Ctrl Pts',(-18.7324805385707,47.6999622484776,122.064856373526)) ;
#91727 = CARTESIAN_POINT('Ctrl Pts',(-18.9727568592771,47.7098050903014,121.969045673601)) ;
#91728 = CARTESIAN_POINT('Ctrl Pts',(-19.2294948681427,47.7197893745484,121.915068774287)) ;
#91729 = CARTESIAN_POINT('Ctrl Pts',(-19.4908350255121,47.7297390199475,121.906573088993)) ;
#91730 = CARTESIAN_POINT('Ctrl Pts',(-19.7510324518848,47.7397387816359,121.943450958025)) ;
#91731 = CARTESIAN_POINT('Ctrl Pts',(-20.001511154546,47.7497701275948,122.025612884837)) ;
#91732 = CARTESIAN_POINT('Ctrl Pts',(-20.2300186287295,47.7596250820719,122.147499644092)) ;
#91733 = CARTESIAN_POINT('Ctrl Pts',(-20.4366754769559,47.7695976200724,122.308615609026)) ;
#91734 = CARTESIAN_POINT('Ctrl Pts',(-20.612644360831,47.7795926138074,122.503667729469)) ;
#91735 = CARTESIAN_POINT('Ctrl Pts',(-20.7523101013191,47.7896266726015,122.727299317315)) ;
#91736 = CARTESIAN_POINT('Ctrl Pts',(-20.8496668786128,47.7994820154245,122.967319880366)) ;
#91737 = CARTESIAN_POINT('Ctrl Pts',(-20.904992548046,47.8094814947701,123.224157421193)) ;
#91738 = CARTESIAN_POINT('Ctrl Pts',(-20.9150779626639,47.8193759435254,123.484026654786)) ;
#91739 = CARTESIAN_POINT('Ctrl Pts',(-20.879224101965,47.8294390629599,123.745986877431)) ;
#91740 = CARTESIAN_POINT('Ctrl Pts',(-20.8004688342771,47.8392787082011,123.992322380341)) ;
#91741 = CARTESIAN_POINT('Ctrl Pts',(-20.6777398160996,47.8493418723872,124.226526704695)) ;
#91742 = CARTESIAN_POINT('Ctrl Pts',(-20.5187066498922,47.859236142136,124.432268221858)) ;
#91743 = CARTESIAN_POINT('Ctrl Pts',(-20.3259668872383,47.8691778681498,124.608589479913)) ;
#91744 = CARTESIAN_POINT('Ctrl Pts',(-20.1041808999464,47.8791807568092,124.749765186793)) ;
#91745 = CARTESIAN_POINT('Ctrl Pts',(-19.8602299792522,47.8892206056032,124.850187093091)) ;
#91746 = CARTESIAN_POINT('Ctrl Pts',(-19.6081642424219,47.8990448210641,124.906094643254)) ;
#91747 = CARTESIAN_POINT('Ctrl Pts',(-19.3441702977261,47.9091016645576,124.918019813108)) ;
#91748 = CARTESIAN_POINT('Ctrl Pts',(-19.0854703555384,47.9190302739536,124.884016066394)) ;
#91749 = CARTESIAN_POINT('Ctrl Pts',(-18.835802023627,47.9289821579915,124.806127703608)) ;
#91750 = CARTESIAN_POINT('Ctrl Pts',(-18.6013347301841,47.9390351107991,124.684442693465)) ;
#91751 = CARTESIAN_POINT('Ctrl Pts',(-18.3960367832778,47.9488579872653,124.527928911458)) ;
#91752 = CARTESIAN_POINT('Ctrl Pts',(-18.2165695066782,47.9589137198354,124.333990312506)) ;
#91753 = CARTESIAN_POINT('Ctrl Pts',(-18.0755119524271,47.9688544848231,124.114102984926)) ;
#91754 = CARTESIAN_POINT('Ctrl Pts',(-17.97439677815,47.9787588177287,123.874266207495)) ;
#91755 = CARTESIAN_POINT('Ctrl Pts',(-17.9157978478123,47.9888054866094,123.616858452994)) ;
#91756 = CARTESIAN_POINT('Ctrl Pts',(-17.9027391893822,47.9987010499152,123.357099240434)) ;
#91757 = CARTESIAN_POINT('Ctrl Pts',(-17.9355139727328,48.0087631076155,123.094756208375)) ;
#91758 = CARTESIAN_POINT('Ctrl Pts',(-18.0115247975341,48.018605885243,122.847487885336)) ;
#91759 = CARTESIAN_POINT('Ctrl Pts',(-18.130499270546,48.0285963634949,122.613492148444)) ;
#91760 = CARTESIAN_POINT('Ctrl Pts',(-18.2873849531134,48.0385253361384,122.404982545336)) ;
#91761 = CARTESIAN_POINT('Ctrl Pts',(-18.4789956662502,48.048516473018,122.225477178445)) ;
#91762 = CARTESIAN_POINT('Ctrl Pts',(-18.6997215251481,48.0585385905069,122.081788244482)) ;
#91763 = CARTESIAN_POINT('Ctrl Pts',(-18.9390060894404,48.0684391009091,121.979633386977)) ;
#91764 = CARTESIAN_POINT('Ctrl Pts',(-19.1945602868354,48.0784280936552,121.9196516612)) ;
#91765 = CARTESIAN_POINT('Ctrl Pts',(-19.4560251777434,48.0883933377058,121.905170872972)) ;
#91766 = CARTESIAN_POINT('Ctrl Pts',(-19.714544749918,48.098297602219,121.935512588317)) ;
#91767 = CARTESIAN_POINT('Ctrl Pts',(-19.9676521572524,48.1083556939172,122.01159018475)) ;
#91768 = CARTESIAN_POINT('Ctrl Pts',(-20.1989410280847,48.1182056343456,122.127843264376)) ;
#91769 = CARTESIAN_POINT('Ctrl Pts',(-20.4106352779193,48.1282326455192,122.284734900046)) ;
#91770 = CARTESIAN_POINT('Ctrl Pts',(-20.5914129661359,48.1382612321312,122.476515291714)) ;
#91771 = CARTESIAN_POINT('Ctrl Pts',(-20.7338940826546,48.1481064462439,122.692453451488)) ;
#91772 = CARTESIAN_POINT('Ctrl Pts',(-20.8388889355934,48.1580971944235,122.933098046713)) ;
#91773 = CARTESIAN_POINT('Ctrl Pts',(-20.9002278538488,48.168134828009,123.189645406397)) ;
#91774 = CARTESIAN_POINT('Ctrl Pts',(-20.9162157833847,48.1779801172218,123.447878692139)) ;
#91775 = CARTESIAN_POINT('Ctrl Pts',(-20.8873032918651,48.1879615180277,123.708561008633)) ;
#91776 = CARTESIAN_POINT('Ctrl Pts',(-20.8137139164343,48.1979137510176,123.959536527466)) ;
#91777 = CARTESIAN_POINT('Ctrl Pts',(-20.6974226162219,48.2079125624742,124.195182186014)) ;
#91778 = CARTESIAN_POINT('Ctrl Pts',(-20.5409679874558,48.2179516664049,124.40758088976)) ;
#91779 = CARTESIAN_POINT('Ctrl Pts',(-20.3544447338278,48.2277766088242,124.58612785741)) ;
#91780 = CARTESIAN_POINT('Ctrl Pts',(-20.1350015577314,48.2378312963002,124.733273340073)) ;
#91781 = CARTESIAN_POINT('Ctrl Pts',(-19.8958290741237,48.247774098657,124.838493759771)) ;
#91782 = CARTESIAN_POINT('Ctrl Pts',(-19.6432087007226,48.2576778945968,124.901118420341)) ;
#91783 = CARTESIAN_POINT('Ctrl Pts',(-19.3798197798372,48.2677246739718,124.919026044654)) ;
#91784 = CARTESIAN_POINT('Ctrl Pts',(-19.1211868057863,48.2776203322664,124.891570258685)) ;
#91785 = CARTESIAN_POINT('Ctrl Pts',(-18.8671159689922,48.287681899517,124.818466322481)) ;
#91786 = CARTESIAN_POINT('Ctrl Pts',(-18.6346672337003,48.2975265439543,124.704882074842)) ;
#91787 = CARTESIAN_POINT('Ctrl Pts',(-18.4224774448849,48.307486590197,124.551645752143)) ;
#91788 = CARTESIAN_POINT('Ctrl Pts',(-18.2390630273348,48.3175248862154,124.362065332604)) ;
#91789 = CARTESIAN_POINT('Ctrl Pts',(-18.0933378214402,48.3273982276337,124.147345292635)) ;
#91790 = CARTESIAN_POINT('Ctrl Pts',(-17.9850701345174,48.337471331433,123.905844629381)) ;
#91791 = CARTESIAN_POINT('Ctrl Pts',(-17.9216618145417,48.3472921465519,123.655621239189)) ;
#91792 = CARTESIAN_POINT('Ctrl Pts',(-17.9018739629238,48.3573690116299,123.391601343181)) ;
#91793 = CARTESIAN_POINT('Ctrl Pts',(-17.9277813877702,48.3672337512852,123.133631857944)) ;
#91794 = CARTESIAN_POINT('Ctrl Pts',(-17.9985353622652,48.3772561545265,122.879946100013)) ;
#91795 = CARTESIAN_POINT('Ctrl Pts',(-18.1129061323741,48.387281878815,122.642581869023)) ;
#91796 = CARTESIAN_POINT('Ctrl Pts',(-18.2637423254893,48.3971366618363,122.432087433426)) ;
#91797 = CARTESIAN_POINT('Ctrl Pts',(-18.4507029295602,48.4071155055596,122.248197667358)) ;
#91798 = CARTESIAN_POINT('Ctrl Pts',(-18.6678616263483,48.4171343977962,122.099352690164)) ;
#91799 = CARTESIAN_POINT('Ctrl Pts',(-18.9041396211026,48.4270176068372,121.991439850928)) ;
#91800 = CARTESIAN_POINT('Ctrl Pts',(-19.1602260657838,48.4370859161774,121.925097919403)) ;
#91801 = CARTESIAN_POINT('Ctrl Pts',(-19.4177670696848,48.4469160415101,121.904413532861)) ;
#91802 = CARTESIAN_POINT('Ctrl Pts',(-19.6811181172093,48.4569825938871,121.928996874006)) ;
#91803 = CARTESIAN_POINT('Ctrl Pts',(-19.9317618895005,48.4668728307808,121.997882966823)) ;
#91804 = CARTESIAN_POINT('Ctrl Pts',(-20.1692610222621,48.4768650555748,122.109851831293)) ;
#91805 = CARTESIAN_POINT('Ctrl Pts',(-20.3829445510021,48.4868276759257,122.261113657658)) ;
#91806 = CARTESIAN_POINT('Ctrl Pts',(-20.5665261218062,48.4967326786889,122.445666071956)) ;
#91807 = CARTESIAN_POINT('Ctrl Pts',(-20.7173958030492,48.506790441087,122.662655601088)) ;
#91808 = CARTESIAN_POINT('Ctrl Pts',(-20.8262238273378,48.5166409604658,122.897552034887)) ;
#91809 = CARTESIAN_POINT('Ctrl Pts',(-20.8943829996658,48.526672537464,123.152189944527)) ;
#91810 = CARTESIAN_POINT('Ctrl Pts',(-20.9167426169127,48.5366822725689,123.414312273892)) ;
#91811 = CARTESIAN_POINT('Ctrl Pts',(-20.8937179531658,48.5465918491952,123.673683390135)) ;
#91812 = CARTESIAN_POINT('Ctrl Pts',(-20.8265228052753,48.5565192350519,123.925774756106)) ;
#91813 = CARTESIAN_POINT('Ctrl Pts',(-20.7150907300863,48.5665641695422,124.165059353475)) ;
#91814 = CARTESIAN_POINT('Ctrl Pts',(-20.5663090616085,48.5764501017301,124.378048058078)) ;
#91815 = CARTESIAN_POINT('Ctrl Pts',(-20.3811550715041,48.5864434076831,124.564263272707)) ;
#91816 = CARTESIAN_POINT('Ctrl Pts',(-20.1674323885774,48.596389045465,124.714704721664)) ;
#91817 = CARTESIAN_POINT('Ctrl Pts',(-19.9310127579831,48.6063363138109,124.826259865705)) ;
#91818 = CARTESIAN_POINT('Ctrl Pts',(-19.6762062907194,48.616384215948,124.895474138505)) ;
#91819 = CARTESIAN_POINT('Ctrl Pts',(-19.4185018206962,48.6262319107882,124.919135372387)) ;
#91820 = CARTESIAN_POINT('Ctrl Pts',(-19.157566898572,48.6361934205326,124.898267563706)) ;
#91821 = CARTESIAN_POINT('Ctrl Pts',(-18.9025619508575,48.6462228121415,124.831614773843)) ;
#91822 = CARTESIAN_POINT('Ctrl Pts',(-18.6658627752509,48.6561303076962,124.723165141493)) ;
#91823 = CARTESIAN_POINT('Ctrl Pts',(-18.4504930203598,48.6660756993592,124.575141126783)) ;
#91824 = CARTESIAN_POINT('Ctrl Pts',(-18.2628876791554,48.6760776169566,124.391000597497)) ;
#91825 = CARTESIAN_POINT('Ctrl Pts',(-18.1099535759632,48.6861176845088,124.176032718824)) ;
#91826 = CARTESIAN_POINT('Ctrl Pts',(-17.9985528130765,48.6959419959486,123.943106599342)) ;
#91827 = CARTESIAN_POINT('Ctrl Pts',(-17.9273154063796,48.7059982371047,123.688649150822)) ;
#91828 = CARTESIAN_POINT('Ctrl Pts',(-17.9019656863292,48.7159291588403,123.428879136997)) ;
#91829 = CARTESIAN_POINT('Ctrl Pts',(-17.9215938866681,48.7258723949166,123.168352780034)) ;
#91830 = CARTESIAN_POINT('Ctrl Pts',(-17.9861802002328,48.735853678929,122.914090093812)) ;
#91831 = CARTESIAN_POINT('Ctrl Pts',(-18.0949989715361,48.7458979805547,122.673647794656)) ;
#91832 = CARTESIAN_POINT('Ctrl Pts',(-18.2402534708388,48.7557260617741,122.460043836669)) ;
#91833 = CARTESIAN_POINT('Ctrl Pts',(-18.4247849710024,48.7658026646233,122.270203460101)) ;
#91834 = CARTESIAN_POINT('Ctrl Pts',(-18.6347065996334,48.7756547437418,122.118569547531)) ;
#91835 = CARTESIAN_POINT('Ctrl Pts',(-18.8728105251633,48.7857280020508,122.002995475702)) ;
#91836 = CARTESIAN_POINT('Ctrl Pts',(-19.1215857423761,48.7955694614311,121.932239761547)) ;
#91837 = CARTESIAN_POINT('Ctrl Pts',(-19.3818649812545,48.8055305568434,121.904458482012)) ;
#91838 = CARTESIAN_POINT('Ctrl Pts',(-19.6449795161499,48.8155678412401,121.922944960723)) ;
#91839 = CARTESIAN_POINT('Ctrl Pts',(-19.8969273677844,48.8254441799754,121.985379683799)) ;
#91840 = CARTESIAN_POINT('Ctrl Pts',(-20.1386336262622,48.8355063061287,122.092521249283)) ;
#91841 = CARTESIAN_POINT('Ctrl Pts',(-20.3539244509202,48.8453744801052,122.237144739534)) ;
#91842 = CARTESIAN_POINT('Ctrl Pts',(-20.543755011927,48.855380028609,122.419026520356)) ;
#91843 = CARTESIAN_POINT('Ctrl Pts',(-20.6987419364052,48.8653626605046,122.630740739498)) ;
#91844 = CARTESIAN_POINT('Ctrl Pts',(-20.8150482287937,48.8754066029264,122.867653599729)) ;
#91845 = CARTESIAN_POINT('Ctrl Pts',(-20.8872135170498,48.8852347509536,123.115640682786)) ;
#91846 = CARTESIAN_POINT('Ctrl Pts',(-20.9165222913364,48.8952246183279,123.376523659417)) ;
#91847 = CARTESIAN_POINT('Ctrl Pts',(-20.8993147872527,48.9052683572834,123.639900737698)) ;
#91848 = CARTESIAN_POINT('Ctrl Pts',(-20.8385460028974,48.9150901058214,123.890749443944)) ;
#91849 = CARTESIAN_POINT('Ctrl Pts',(-20.7334926344583,48.9251250834311,124.132629488794)) ;
#91850 = CARTESIAN_POINT('Ctrl Pts',(-20.5875669348054,48.9351499961888,124.351974416172)) ;
#91851 = CARTESIAN_POINT('Ctrl Pts',(-20.4093201184437,48.9450019392826,124.539749635484)) ;
#91852 = CARTESIAN_POINT('Ctrl Pts',(-20.1985093079883,48.9549929006117,124.696195980077)) ;
#91853 = CARTESIAN_POINT('Ctrl Pts',(-19.9654731355136,48.9649107754802,124.812985422573)) ;
#91854 = CARTESIAN_POINT('Ctrl Pts',(-19.7129807407904,48.9749392944814,124.888406605347)) ;
#91855 = CARTESIAN_POINT('Ctrl Pts',(-19.4549910732823,48.9848229732793,124.918538485184)) ;
#91856 = CARTESIAN_POINT('Ctrl Pts',(-19.1927471785049,48.994817916719,124.903825171715)) ;
#91857 = CARTESIAN_POINT('Ctrl Pts',(-18.9363271652186,49.0048447705414,124.84316892203)) ;
#91858 = CARTESIAN_POINT('Ctrl Pts',(-18.6976274329194,49.0147289348803,124.740719075366)) ;
#91859 = CARTESIAN_POINT('Ctrl Pts',(-18.4778974629818,49.0247170329227,124.597194644998)) ;
#91860 = CARTESIAN_POINT('Ctrl Pts',(-18.2869925249069,49.0346681393798,124.418428962904)) ;
#91861 = CARTESIAN_POINT('Ctrl Pts',(-18.1286921061756,49.0447131905479,124.207206823015)) ;
#91862 = CARTESIAN_POINT('Ctrl Pts',(-18.0115110053641,49.0545749509062,123.976053919716)) ;
#91863 = CARTESIAN_POINT('Ctrl Pts',(-17.9347018565793,49.0645377677367,123.725760547945)) ;
#91864 = CARTESIAN_POINT('Ctrl Pts',(-17.9027372037974,49.0745724490174,123.464015962194)) ;
#91865 = CARTESIAN_POINT('Ctrl Pts',(-17.9160561245772,49.0844574787982,123.204553334292)) ;
#91866 = CARTESIAN_POINT('Ctrl Pts',(-17.9753271704611,49.0945230721962,122.946810192394)) ;
#91867 = CARTESIAN_POINT('Ctrl Pts',(-18.0759231780919,49.1043622405577,122.708574067968)) ;
#91868 = CARTESIAN_POINT('Ctrl Pts',(-18.2192006262921,49.1144248382992,122.486356375471)) ;
#91869 = CARTESIAN_POINT('Ctrl Pts',(-18.3961652533745,49.1243218507061,122.2957392912)) ;
#91870 = CARTESIAN_POINT('Ctrl Pts',(-18.6037154643153,49.1342531725317,122.137521228201)) ;
#91871 = CARTESIAN_POINT('Ctrl Pts',(-18.8382964268997,49.1442949352862,122.016665264985)) ;
#91872 = CARTESIAN_POINT('Ctrl Pts',(-19.0864079744247,49.1541831341769,121.939390497466)) ;
#91873 = CARTESIAN_POINT('Ctrl Pts',(-19.3468353464452,49.1641770727768,121.905608425672)) ;
#91874 = CARTESIAN_POINT('Ctrl Pts',(-19.6078151277302,49.1741178938136,121.91751361713)) ;
#91875 = CARTESIAN_POINT('Ctrl Pts',(-19.8632816579453,49.1840772761019,121.974327396906)) ;
#91876 = CARTESIAN_POINT('Ctrl Pts',(-20.1060322896982,49.1940750357542,122.074891251936)) ;
#91877 = CARTESIAN_POINT('Ctrl Pts',(-20.3282620364892,49.2041111719565,122.21690786839)) ;
#91878 = CARTESIAN_POINT('Ctrl Pts',(-20.5190808378173,49.2139619694474,122.391836817215)) ;
#91879 = CARTESIAN_POINT('Ctrl Pts',(-20.6790012985683,49.2239228345237,122.599055308519)) ;
#91880 = CARTESIAN_POINT('Ctrl Pts',(-20.8010708002223,49.2339517021541,122.832645696346)) ;
#91881 = CARTESIAN_POINT('Ctrl Pts',(-20.879853818226,49.2438619382905,123.080862806442)) ;
#91882 = CARTESIAN_POINT('Ctrl Pts',(-20.9151078932877,49.253796891605,123.339559285952)) ;
#91883 = CARTESIAN_POINT('Ctrl Pts',(-20.9045592317714,49.2638378220146,123.603207119489)) ;
#91884 = CARTESIAN_POINT('Ctrl Pts',(-20.8494077535675,49.2737257187962,123.857140794924)) ;
#91885 = CARTESIAN_POINT('Ctrl Pts',(-20.7504505562724,49.2837151704549,124.100280633098)) ;
#91886 = CARTESIAN_POINT('Ctrl Pts',(-20.6110277047872,49.2936742608203,124.321756486501)) ;
#91887 = CARTESIAN_POINT('Ctrl Pts',(-20.4368338343713,49.3035715731266,124.514921157602)) ;
#91888 = CARTESIAN_POINT('Ctrl Pts',(-20.2284024122809,49.3136279990268,124.677354927092)) ;
#91889 = CARTESIAN_POINT('Ctrl Pts',(-19.9992830178138,49.3234980016166,124.798974471006)) ;
#91890 = CARTESIAN_POINT('Ctrl Pts',(-19.7493901780766,49.3335019347938,124.880531822233)) ;
#91891 = CARTESIAN_POINT('Ctrl Pts',(-19.4894780018953,49.3434891952577,124.917271202357)) ;
#91892 = CARTESIAN_POINT('Ctrl Pts',(-19.2261559513639,49.3535162468434,124.908135759446)) ;
#91893 = CARTESIAN_POINT('Ctrl Pts',(-18.9718205949569,49.3634073366695,124.854401512994)) ;
#91894 = CARTESIAN_POINT('Ctrl Pts',(-18.6475387787366,49.3767050914506,124.724316756299)) ;
#91895 = CARTESIAN_POINT('Ctrl Pts',(-18.3663439177842,49.3899031510587,124.514527900887)) ;
#91896 = CARTESIAN_POINT('Ctrl Pts',(-18.1484048267078,49.4032998916279,124.238071111464)) ;
#91897 = CARTESIAN_POINT('Ctrl Pts',(-18.0253527815644,49.4131708037013,124.009661322498)) ;
#91898 = CARTESIAN_POINT('Ctrl Pts',(-17.9421985890326,49.4232443654695,123.758399347314)) ;
#91899 = CARTESIAN_POINT('Ctrl Pts',(-17.9045673262481,49.4330657780578,123.502999840485)) ;
#91900 = CARTESIAN_POINT('Ctrl Pts',(-17.9117874809025,49.4431397952888,123.238428805641)) ;
#91901 = CARTESIAN_POINT('Ctrl Pts',(-17.9808625993538,49.4562985822534,122.899526034126)) ;
#91902 = CARTESIAN_POINT('Ctrl Pts',(-18.1386493012278,49.4696646853476,122.58136729471)) ;
#91903 = CARTESIAN_POINT('Ctrl Pts',(-18.3706579537025,49.4829786202367,122.319337160576)) ;
#91904 = CARTESIAN_POINT('Ctrl Pts',(-18.5739338777232,49.4928786596841,122.157029405636)) ;
#91905 = CARTESIAN_POINT('Ctrl Pts',(-18.8036238095851,49.5028430628186,122.031257984843)) ;
#91906 = CARTESIAN_POINT('Ctrl Pts',(-19.05335921375,49.5128730299398,121.946955300818)) ;
#91907 = CARTESIAN_POINT('Ctrl Pts',(-19.3105895258516,49.5227753065488,121.907692131419)) ;
#91908 = CARTESIAN_POINT('Ctrl Pts',(-19.6591707264257,49.536041235718,121.91483615231)) ;
#91909 = CARTESIAN_POINT('Ctrl Pts',(-20.0833606626239,49.5526627668244,122.037946979199)) ;
#91910 = CARTESIAN_POINT('Ctrl Pts',(-20.5104593674055,49.5725375954691,122.348915166531)) ;
#91911 = CARTESIAN_POINT('Ctrl Pts',(-20.7582535736872,49.5892108035709,122.716248365857)) ;
#91912 = CARTESIAN_POINT('Ctrl Pts',(-20.8714352247518,49.6024619285522,123.045592382337)) ;
#91913 = CARTESIAN_POINT('Ctrl Pts',(-20.9269354813126,49.615704247373,123.389194785708)) ;
#91914 = CARTESIAN_POINT('Ctrl Pts',(-20.8811511581855,49.6324374877125,123.831492590155)) ;
#91915 = CARTESIAN_POINT('Ctrl Pts',(-20.6511878464973,49.6522666359005,124.305812689138)) ;
#91916 = CARTESIAN_POINT('Ctrl Pts',(-20.2723991280832,49.6721913310011,124.675727471051)) ;
#91917 = CARTESIAN_POINT('Ctrl Pts',(-19.7899488954886,49.6921145595845,124.894193343067)) ;
#91918 = CARTESIAN_POINT('Ctrl Pts',(-19.2619611266706,49.7120416987106,124.935069014905)) ;
#91919 = CARTESIAN_POINT('Ctrl Pts',(-18.7527411075181,49.7319181613263,124.794310345686)) ;
#91920 = CARTESIAN_POINT('Ctrl Pts',(-18.3198072271694,49.7518953899316,124.486931020539)) ;
#91921 = CARTESIAN_POINT('Ctrl Pts',(-18.018710731692,49.7718302479053,124.050908756306)) ;
#91922 = CARTESIAN_POINT('Ctrl Pts',(-17.8842375144528,49.7917266968361,123.539519466163)) ;
#91923 = CARTESIAN_POINT('Ctrl Pts',(-17.9318221676816,49.8116479809027,123.012164589738)) ;
#91924 = CARTESIAN_POINT('Ctrl Pts',(-18.1570615290371,49.8316046305737,122.531918504927)) ;
#91925 = CARTESIAN_POINT('Ctrl Pts',(-18.5309830443767,49.8514819236853,122.158801133981)) ;
#91926 = CARTESIAN_POINT('Ctrl Pts',(-19.0095255521828,49.8713683959137,121.934252429302)) ;
#91927 = CARTESIAN_POINT('Ctrl Pts',(-19.5406391317515,49.8914299618377,121.886868078949)) ;
#91928 = CARTESIAN_POINT('Ctrl Pts',(-20.0501878146875,49.9112703693785,122.022537685724)) ;
#91929 = CARTESIAN_POINT('Ctrl Pts',(-20.4843856180674,49.9311216933514,122.322319927731)) ;
#91930 = CARTESIAN_POINT('Ctrl Pts',(-20.7926218042951,49.9511749633028,122.757047288943)) ;
#91931 = CARTESIAN_POINT('Ctrl Pts',(-20.9325314728205,49.9709956206862,123.265078314232)) ;
#91932 = CARTESIAN_POINT('Ctrl Pts',(-20.8912422361684,49.9909670420167,123.794102750068)) ;
#91933 = CARTESIAN_POINT('Ctrl Pts',(-20.672728228111,50.0108605343804,124.275780483601)) ;
#91934 = CARTESIAN_POINT('Ctrl Pts',(-20.3004875803372,50.0308846206214,124.65599343755)) ;
#91935 = CARTESIAN_POINT('Ctrl Pts',(-19.8260699488102,50.0506894997343,124.884165170859)) ;
#91936 = CARTESIAN_POINT('Ctrl Pts',(-19.2984073272745,50.0706485154322,124.938579634073)) ;
#91937 = CARTESIAN_POINT('Ctrl Pts',(-18.7834458131184,50.0906345390612,124.808287005669)) ;
#91938 = CARTESIAN_POINT('Ctrl Pts',(-18.3471380862029,50.1104430348217,124.513561025804)) ;
#91939 = CARTESIAN_POINT('Ctrl Pts',(-18.034433731144,50.1304256739273,124.08441134622)) ;
#91940 = CARTESIAN_POINT('Ctrl Pts',(-17.8877548058213,50.1503071217213,123.576622519046)) ;
#91941 = CARTESIAN_POINT('Ctrl Pts',(-17.9228590595857,50.1702635884589,123.047489138174)) ;
#91942 = CARTESIAN_POINT('Ctrl Pts',(-18.135325664709,50.1901409854144,122.563692670579)) ;
#91943 = CARTESIAN_POINT('Ctrl Pts',(-18.5017404753757,50.2101229315897,122.179326787256)) ;
#91944 = CARTESIAN_POINT('Ctrl Pts',(-18.9763311717451,50.2300520306265,121.94386229144)) ;
#91945 = CARTESIAN_POINT('Ctrl Pts',(-19.5025542136779,50.2499806538391,121.884425032197)) ;
#91946 = CARTESIAN_POINT('Ctrl Pts',(-20.0154098113017,50.2698149779455,122.006618943828)) ;
#91947 = CARTESIAN_POINT('Ctrl Pts',(-20.3852796718983,50.2864672653289,122.249530478733)) ;
#91948 = CARTESIAN_POINT('Ctrl Pts',(-20.6170613698565,50.2997277663511,122.509825199118)) ;
#91949 = CARTESIAN_POINT('Ctrl Pts',(-20.7555282047836,50.3097292435524,122.733215342447)) ;
#91950 = CARTESIAN_POINT('Ctrl Pts',(-20.8529948357394,50.3197612644119,122.978175098663)) ;
#91951 = CARTESIAN_POINT('Ctrl Pts',(-20.9058575761444,50.3296248081375,123.231923138614)) ;
#91952 = CARTESIAN_POINT('Ctrl Pts',(-20.9146380480463,50.3395935218076,123.493747759478)) ;
#91953 = CARTESIAN_POINT('Ctrl Pts',(-20.8648603610188,50.3529392692113,123.840886646443)) ;
#91954 = CARTESIAN_POINT('Ctrl Pts',(-20.7281950716831,50.366089824284,124.162613928907)) ;
#91955 = CARTESIAN_POINT('Ctrl Pts',(-20.5118305427497,50.3794752048338,124.439920066173)) ;
#91956 = CARTESIAN_POINT('Ctrl Pts',(-20.3188172284818,50.3893631408267,124.613934022329)) ;
#91957 = CARTESIAN_POINT('Ctrl Pts',(-20.0965116250302,50.3993543306393,124.753570663319)) ;
#91958 = CARTESIAN_POINT('Ctrl Pts',(-19.8542622927966,50.4093064291776,124.852232186328)) ;
#91959 = CARTESIAN_POINT('Ctrl Pts',(-19.5961633789181,50.4193526856281,124.907673196293)) ;
#91960 = CARTESIAN_POINT('Ctrl Pts',(-19.3375104748675,50.4292021330222,124.917455726656)) ;
#91961 = CARTESIAN_POINT('Ctrl Pts',(-19.0780426601325,50.4391647855174,124.882591527256)) ;
#91962 = CARTESIAN_POINT('Ctrl Pts',(-18.8271559377994,50.4491878711595,124.802384290233)) ;
#91963 = CARTESIAN_POINT('Ctrl Pts',(-18.5961209801117,50.4591129869164,124.681281420803)) ;
#91964 = CARTESIAN_POINT('Ctrl Pts',(-18.3870807334424,50.4691654653163,124.519806842714)) ;
#91965 = CARTESIAN_POINT('Ctrl Pts',(-18.2126501072753,50.479016964019,124.32847873655)) ;
#91966 = CARTESIAN_POINT('Ctrl Pts',(-18.0718501454337,50.4889887032215,124.107511530402)) ;
#91967 = CARTESIAN_POINT('Ctrl Pts',(-17.9713211447881,50.4989839109872,123.864801095388)) ;
#91968 = CARTESIAN_POINT('Ctrl Pts',(-17.9145692121074,50.5090179124563,123.607321569366)) ;
#91969 = CARTESIAN_POINT('Ctrl Pts',(-17.9031710447773,50.5188732705486,123.348557997671)) ;
#91970 = CARTESIAN_POINT('Ctrl Pts',(-17.9370086645265,50.5288727461419,123.088017414384)) ;
#91971 = CARTESIAN_POINT('Ctrl Pts',(-18.0144915110239,50.538767194637,122.839763225874)) ;
#91972 = CARTESIAN_POINT('Ctrl Pts',(-18.1359636490848,50.5488303188647,122.604915926376)) ;
#91973 = CARTESIAN_POINT('Ctrl Pts',(-18.2926316435237,50.5586699451933,122.399152962944)) ;
#91974 = CARTESIAN_POINT('Ctrl Pts',(-18.486678321847,50.5687331802363,122.219538927624)) ;
#91975 = CARTESIAN_POINT('Ctrl Pts',(-18.7053988201739,50.5786271854703,122.078904883828)) ;
#91976 = CARTESIAN_POINT('Ctrl Pts',(-18.9460659097001,50.5885698986861,121.977250669726)) ;
#91977 = CARTESIAN_POINT('Ctrl Pts',(-19.2023861460661,50.5985756384843,121.918495735838)) ;
#91978 = CARTESIAN_POINT('Ctrl Pts',(-19.4653940518091,50.6085965406307,121.9054168295)) ;
#91979 = CARTESIAN_POINT('Ctrl Pts',(-19.7233358092848,50.6184873106796,121.937482828107)) ;
#91980 = CARTESIAN_POINT('Ctrl Pts',(-19.9744185614306,50.6284787214593,122.014246082198)) ;
#91981 = CARTESIAN_POINT('Ctrl Pts',(-20.2073144805598,50.6384270671238,122.133004263277)) ;
#91982 = CARTESIAN_POINT('Ctrl Pts',(-20.4163335012571,50.648371925185,122.289918302436)) ;
#91983 = CARTESIAN_POINT('Ctrl Pts',(-20.5965902441456,50.6584267605779,122.483081634732)) ;
#91984 = CARTESIAN_POINT('Ctrl Pts',(-20.7376425347096,50.6682491326794,122.69928261909)) ;
#91985 = CARTESIAN_POINT('Ctrl Pts',(-20.8418429067607,50.6783050001231,122.942107997445)) ;
#91986 = CARTESIAN_POINT('Ctrl Pts',(-20.9011591134657,50.688245729981,123.196526972203)) ;
#91987 = CARTESIAN_POINT('Ctrl Pts',(-20.9161606255222,50.6981500685321,123.456374885143)) ;
#91988 = CARTESIAN_POINT('Ctrl Pts',(-20.8852161971234,50.7081967499607,123.718548743211)) ;
#91989 = CARTESIAN_POINT('Ctrl Pts',(-20.8105731784495,50.7180922574299,123.967693866746)) ;
#91990 = CARTESIAN_POINT('Ctrl Pts',(-20.6918696445542,50.7281545259285,124.203934788214)) ;
#91991 = CARTESIAN_POINT('Ctrl Pts',(-20.5374931111289,50.7379965161991,124.411487122097)) ;
#91992 = CARTESIAN_POINT('Ctrl Pts',(-20.3469886042085,50.7479899330801,124.592192301977)) ;
#91993 = CARTESIAN_POINT('Ctrl Pts',(-20.129467915059,50.7579144209322,124.736132155614)) ;
#91994 = CARTESIAN_POINT('Ctrl Pts',(-19.8886030526091,50.7679140548407,124.841138181418)) ;
#91995 = CARTESIAN_POINT('Ctrl Pts',(-19.6334526076263,50.7779001650975,124.902666745097)) ;
#91996 = CARTESIAN_POINT('Ctrl Pts',(-19.370234794874,50.7879361162846,124.9187595243)) ;
#91997 = CARTESIAN_POINT('Ctrl Pts',(-19.1128081761444,50.7977927546194,124.889819939285)) ;
#91998 = CARTESIAN_POINT('Ctrl Pts',(-18.8606967834269,50.8077917146974,124.815928138923)) ;
#91999 = CARTESIAN_POINT('Ctrl Pts',(-18.6274830798784,50.8176869450112,124.700806449973)) ;
#92000 = CARTESIAN_POINT('Ctrl Pts',(-18.4143788196718,50.8277474574798,124.544393204072)) ;
#92001 = CARTESIAN_POINT('Ctrl Pts',(-18.2353627908807,50.837596749026,124.357426939128)) ;
#92002 = CARTESIAN_POINT('Ctrl Pts',(-18.0883925533693,50.8476239349582,124.138724931857)) ;
#92003 = CARTESIAN_POINT('Ctrl Pts',(-17.9822394761601,50.8576524714175,123.897495737677)) ;
#92004 = CARTESIAN_POINT('Ctrl Pts',(-17.9202588837812,50.8674977113825,123.646321073152)) ;
#92005 = CARTESIAN_POINT('Ctrl Pts',(-17.9018714931078,50.8774884063057,123.384414305504)) ;
#92006 = CARTESIAN_POINT('Ctrl Pts',(-17.9299486548859,50.8875262270643,123.122130520275)) ;
#92007 = CARTESIAN_POINT('Ctrl Pts',(-18.0013103641566,50.8973708208412,122.873455872908)) ;
#92008 = CARTESIAN_POINT('Ctrl Pts',(-18.1158568183376,50.9073548162173,122.637438180659)) ;
#92009 = CARTESIAN_POINT('Ctrl Pts',(-18.2691496553917,50.9173038647787,122.425625938668)) ;
#92010 = CARTESIAN_POINT('Ctrl Pts',(-18.4576995104374,50.9273063037532,122.242469851909)) ;
#92011 = CARTESIAN_POINT('Ctrl Pts',(-18.675790127976,50.9373275450496,122.094857283506)) ;
#92012 = CARTESIAN_POINT('Ctrl Pts',(-18.9129857115445,50.9472202234891,121.988448302435)) ;
#92013 = CARTESIAN_POINT('Ctrl Pts',(-19.1674288630117,50.9572102774367,121.923807401294)) ;
#92014 = CARTESIAN_POINT('Ctrl Pts',(-19.42840760001,50.9671686385852,121.904576356759)) ;
#92015 = CARTESIAN_POINT('Ctrl Pts',(-19.6873151025459,50.97706826547,121.930161648276)) ;
#92016 = CARTESIAN_POINT('Ctrl Pts',(-19.9415317404535,50.9871161622734,122.001441737826)) ;
#92017 = CARTESIAN_POINT('Ctrl Pts',(-20.1760473918664,50.9970115199094,122.11388903272)) ;
#92018 = CARTESIAN_POINT('Ctrl Pts',(-20.3909934475873,51.0070731723661,122.267820853643)) ;
#92019 = CARTESIAN_POINT('Ctrl Pts',(-20.5720124432176,51.016917776638,122.452660571482)) ;
#92020 = CARTESIAN_POINT('Ctrl Pts',(-20.7206679475832,51.026877898336,122.668085454437)) ;
#92021 = CARTESIAN_POINT('Ctrl Pts',(-20.8300463265181,51.0369159326985,122.908118283207)) ;
#92022 = CARTESIAN_POINT('Ctrl Pts',(-20.8954797450795,51.046790245285,123.159253141407)) ;
#92023 = CARTESIAN_POINT('Ctrl Pts',(-20.9167078074931,51.0568597260677,123.422979437591)) ;
#92024 = CARTESIAN_POINT('Ctrl Pts',(-20.8925366127019,51.0666940620848,123.68030532245)) ;
#92025 = CARTESIAN_POINT('Ctrl Pts',(-20.8233738618489,51.076727019813,123.934719313341)) ;
#92026 = CARTESIAN_POINT('Ctrl Pts',(-20.7105654023123,51.0867474183882,124.172661102908)) ;
#92027 = CARTESIAN_POINT('Ctrl Pts',(-20.5610356799522,51.0966129921594,124.384475866047)) ;
#92028 = CARTESIAN_POINT('Ctrl Pts',(-20.3732440668846,51.1066818668155,124.570842766502)) ;
#92029 = CARTESIAN_POINT('Ctrl Pts',(-20.1607562670967,51.116527297721,124.718478795522)) ;
#92030 = CARTESIAN_POINT('Ctrl Pts',(-19.9230357260641,51.1265069225917,124.829213605734)) ;
#92031 = CARTESIAN_POINT('Ctrl Pts',(-19.6685786829973,51.1365256055058,124.896772999361)) ;
#92032 = CARTESIAN_POINT('Ctrl Pts',(-19.4098095174621,51.1464088706896,124.919373434)) ;
#92033 = CARTESIAN_POINT('Ctrl Pts',(-19.1462888986317,51.156477164781,124.896167375007)) ;
#92034 = CARTESIAN_POINT('Ctrl Pts',(-18.8966808735186,51.1663072949663,124.829451529774)) ;
#92035 = CARTESIAN_POINT('Ctrl Pts',(-18.6567504696124,51.1763738431815,124.718134366409)) ;
#92036 = CARTESIAN_POINT('Ctrl Pts',(-18.4436238223543,51.1862640918701,124.569323332905)) ;
#92037 = CARTESIAN_POINT('Ctrl Pts',(-18.2573048544974,51.1962562736461,124.384316168399)) ;
#92038 = CARTESIAN_POINT('Ctrl Pts',(-18.1065797448196,51.2062190542739,124.170249228209)) ;
#92039 = CARTESIAN_POINT('Ctrl Pts',(-17.9953654455778,51.2161234589477,123.934908116965)) ;
#92040 = CARTESIAN_POINT('Ctrl Pts',(-17.925826600637,51.2261834534267,123.679876469333)) ;
#92041 = CARTESIAN_POINT('Ctrl Pts',(-17.9019091868143,51.2360320753965,123.422152612981)) ;
#92042 = CARTESIAN_POINT('Ctrl Pts',(-17.9229023529744,51.2460625148083,123.15941586086)) ;
#92043 = CARTESIAN_POINT('Ctrl Pts',(-17.9895839704234,51.2560722304431,122.904933300777)) ;
#92044 = CARTESIAN_POINT('Ctrl Pts',(-18.0981009034146,51.2659829831357,122.668199754966)) ;
#92045 = CARTESIAN_POINT('Ctrl Pts',(-18.2458319639415,51.2759122560821,122.453101902059)) ;
#92046 = CARTESIAN_POINT('Ctrl Pts',(-18.4308984169478,51.2859549474748,122.264969338689)) ;
#92047 = CARTESIAN_POINT('Ctrl Pts',(-18.6424005039535,51.2958414806923,122.114056148567)) ;
#92048 = CARTESIAN_POINT('Ctrl Pts',(-18.8792033416488,51.3058346256243,122.000563484601)) ;
#92049 = CARTESIAN_POINT('Ctrl Pts',(-19.1309552845419,51.3157803064608,121.930339339444)) ;
#92050 = CARTESIAN_POINT('Ctrl Pts',(-19.3910775718894,51.3257275636094,121.904356869132)) ;
#92051 = CARTESIAN_POINT('Ctrl Pts',(-19.6543533589848,51.3357754674813,121.924427076619)) ;
#92052 = CARTESIAN_POINT('Ctrl Pts',(-19.9051120288232,51.3456231665793,121.988392795178)) ;
#92053 = CARTESIAN_POINT('Ctrl Pts',(-20.144008897239,51.355584657558,122.095399647996)) ;
#92054 = CARTESIAN_POINT('Ctrl Pts',(-20.3619945141337,51.3656141199719,122.24356719647)) ;
#92055 = CARTESIAN_POINT('Ctrl Pts',(-20.5487308944332,51.3755213510718,122.424986082512)) ;
#92056 = CARTESIAN_POINT('Ctrl Pts',(-20.7021540436023,51.3854677297493,122.636582411564)) ;
#92057 = CARTESIAN_POINT('Ctrl Pts',(-20.8172786899295,51.3954724985581,122.872977021104)) ;
#92058 = CARTESIAN_POINT('Ctrl Pts',(-20.889429832364,51.4054936195783,123.126239425325)) ;
#92059 = CARTESIAN_POINT('Ctrl Pts',(-20.9164566681768,51.4153844854309,123.384761481474)) ;
#92060 = CARTESIAN_POINT('Ctrl Pts',(-20.8983887932973,51.4253752941902,123.646672004827)) ;
#92061 = CARTESIAN_POINT('Ctrl Pts',(-20.835318400747,51.4353259523705,123.900458111221)) ;
#92062 = CARTESIAN_POINT('Ctrl Pts',(-20.7296282507546,51.4452621620126,124.139202828454)) ;
#92063 = CARTESIAN_POINT('Ctrl Pts',(-20.5836546019347,51.4552453287375,124.357227797165)) ;
#92064 = CARTESIAN_POINT('Ctrl Pts',(-20.4006303942084,51.4652891259478,124.547361584233)) ;
#92065 = CARTESIAN_POINT('Ctrl Pts',(-20.192254850081,51.4751173421161,124.700025669877)) ;
#92066 = CARTESIAN_POINT('Ctrl Pts',(-19.9548227665226,51.4851939095853,124.81714527759)) ;
#92067 = CARTESIAN_POINT('Ctrl Pts',(-19.7062541409025,51.4950459952747,124.889764801909)) ;
#92068 = CARTESIAN_POINT('Ctrl Pts',(-19.4431990726262,51.5051192626801,124.918970553885)) ;
#92069 = CARTESIAN_POINT('Ctrl Pts',(-19.1850914917787,51.5149606791037,124.902372431121)) ;
#92070 = CARTESIAN_POINT('Ctrl Pts',(-18.9305244646705,51.5249219372464,124.841424401148)) ;
#92071 = CARTESIAN_POINT('Ctrl Pts',(-18.6887877930121,51.5349586136784,124.735942523709)) ;
#92072 = CARTESIAN_POINT('Ctrl Pts',(-18.4722292764915,51.5448372215422,124.592733444186)) ;
#92073 = CARTESIAN_POINT('Ctrl Pts',(-18.2803671864941,51.554897450181,124.410900084706)) ;
#92074 = CARTESIAN_POINT('Ctrl Pts',(-18.1259134655434,51.5647644343418,124.202585813997)) ;
#92075 = CARTESIAN_POINT('Ctrl Pts',(-18.0079247984675,51.5747700005945,123.96764851309)) ;
#92076 = CARTESIAN_POINT('Ctrl Pts',(-17.9327258735387,51.5847537890091,123.716244471843)) ;
#92077 = CARTESIAN_POINT('Ctrl Pts',(-17.9024259130523,51.5947996458117,123.454016015245)) ;
#92078 = CARTESIAN_POINT('Ctrl Pts',(-17.917439480721,51.6046255230277,123.196237952779)) ;
#92079 = CARTESIAN_POINT('Ctrl Pts',(-17.9771454730441,51.614615998869,122.940577894991)) ;
#92080 = CARTESIAN_POINT('Ctrl Pts',(-18.0815215144472,51.6246595747678,122.698158310666)) ;
#92081 = CARTESIAN_POINT('Ctrl Pts',(-18.2227516785276,51.6344813670658,122.482120314041)) ;
#92082 = CARTESIAN_POINT('Ctrl Pts',(-18.40270986864,51.6445163326917,122.289358503398)) ;
#92083 = CARTESIAN_POINT('Ctrl Pts',(-18.6136393360001,51.6545412496248,122.13151278075)) ;
#92084 = CARTESIAN_POINT('Ctrl Pts',(-18.8444580637235,51.6643931880009,122.014234397312)) ;
#92085 = CARTESIAN_POINT('Ctrl Pts',(-19.0954754548516,51.6743841640256,121.9373786769)) ;
#92086 = CARTESIAN_POINT('Ctrl Pts',(-19.3541618616858,51.6843019848293,121.905328500858)) ;
#92087 = CARTESIAN_POINT('Ctrl Pts',(-19.617334158459,51.6943307053939,121.918784864329)) ;
#92088 = CARTESIAN_POINT('Ctrl Pts',(-19.8705294306841,51.7042136320031,121.976713058442)) ;
#92089 = CARTESIAN_POINT('Ctrl Pts',(-20.1128710137296,51.7142179171226,122.078557970596)) ;
#92090 = CARTESIAN_POINT('Ctrl Pts',(-20.3334390737872,51.7242015983304,122.220706430317)) ;
#92091 = CARTESIAN_POINT('Ctrl Pts',(-20.526827334217,51.7342425970603,122.400195572372)) ;
#92092 = CARTESIAN_POINT('Ctrl Pts',(-20.6831082514724,51.7440750419275,122.60596620502)) ;
#92093 = CARTESIAN_POINT('Ctrl Pts',(-20.8039234261917,51.7540700403578,122.839180993671)) ;
#92094 = CARTESIAN_POINT('Ctrl Pts',(-20.8821642141018,51.7641015891074,123.090935669259)) ;
#92095 = CARTESIAN_POINT('Ctrl Pts',(-20.915271599229,51.7739669674129,123.348051007155)) ;
#92096 = CARTESIAN_POINT('Ctrl Pts',(-20.9038525681082,51.7839288148732,123.609596824492)) ;
#92097 = CARTESIAN_POINT('Ctrl Pts',(-20.8463633745007,51.7939637556874,123.866947061797)) ;
#92098 = CARTESIAN_POINT('Ctrl Pts',(-20.7469611887257,51.8038487167046,124.106982513468)) ;
#92099 = CARTESIAN_POINT('Ctrl Pts',(-20.6048348390858,51.8139143256234,124.330017808425)) ;
#92100 = CARTESIAN_POINT('Ctrl Pts',(-20.4302962655908,51.8237535006651,124.520838097593)) ;
#92101 = CARTESIAN_POINT('Ctrl Pts',(-20.2209018146829,51.833816056165,124.682277389154)) ;
#92102 = CARTESIAN_POINT('Ctrl Pts',(-19.9903358407335,51.843713230858,124.802662438006)) ;
#92103 = CARTESIAN_POINT('Ctrl Pts',(-19.7418135968401,51.8536439457813,124.882280836008)) ;
#92104 = CARTESIAN_POINT('Ctrl Pts',(-19.4802517626863,51.8636879738589,124.917639362177)) ;
#92105 = CARTESIAN_POINT('Ctrl Pts',(-19.2206361067492,51.8735741757122,124.907413635339)) ;
#92106 = CARTESIAN_POINT('Ctrl Pts',(-18.9639533078119,51.8835673421791,124.852066742979)) ;
#92107 = CARTESIAN_POINT('Ctrl Pts',(-18.7220007871068,51.8935068131662,124.753573074232)) ;
#92108 = CARTESIAN_POINT('Ctrl Pts',(-18.4991343218233,51.9035233275204,124.613563016952)) ;
#92109 = CARTESIAN_POINT('Ctrl Pts',(-18.3054534957154,51.9134533539972,124.438628708333)) ;
#92110 = CARTESIAN_POINT('Ctrl Pts',(-18.1432387360808,51.9235058895067,124.230157322887)) ;
#92111 = CARTESIAN_POINT('Ctrl Pts',(-18.02207359166,51.9333522927264,124.001515921378)) ;
#92112 = CARTESIAN_POINT('Ctrl Pts',(-17.9407164669733,51.9433143355804,123.752702026381)) ;
#92113 = CARTESIAN_POINT('Ctrl Pts',(-17.9038854280585,51.9533428863711,123.491731120395)) ;
#92114 = CARTESIAN_POINT('Ctrl Pts',(-17.912731672611,51.9632532120887,123.231460267867)) ;
#92115 = CARTESIAN_POINT('Ctrl Pts',(-17.966105221735,51.9731881239183,122.975886847945)) ;
#92116 = CARTESIAN_POINT('Ctrl Pts',(-18.0642983867156,51.9832291306864,122.730978652853)) ;
#92117 = CARTESIAN_POINT('Ctrl Pts',(-18.2012613019034,51.9931167635186,122.510155194213)) ;
#92118 = CARTESIAN_POINT('Ctrl Pts',(-18.3759219646091,52.0031071946166,122.314162879866)) ;
#92119 = CARTESIAN_POINT('Ctrl Pts',(-18.5813424888858,52.0130626311739,122.152141812982)) ;
#92120 = CARTESIAN_POINT('Ctrl Pts',(-18.8104988520299,52.0229735792732,122.028393562061)) ;
#92121 = CARTESIAN_POINT('Ctrl Pts',(-19.0601248152919,52.0329856553709,121.945174289692)) ;
#92122 = CARTESIAN_POINT('Ctrl Pts',(-19.3208342889526,52.0430129774459,121.907035972771)) ;
#92123 = CARTESIAN_POINT('Ctrl Pts',(-19.5798702658014,52.0528717524,121.913965038983)) ;
#92124 = CARTESIAN_POINT('Ctrl Pts',(-19.9254189752122,52.0662979452124,121.984776021455)) ;
#92125 = CARTESIAN_POINT('Ctrl Pts',(-20.2369069489131,52.0793819609939,122.139699278538)) ;
#92126 = CARTESIAN_POINT('Ctrl Pts',(-20.5025007000134,52.0928554097491,122.373739586692)) ;
#92127 = CARTESIAN_POINT('Ctrl Pts',(-20.663502478955,52.1026883675549,122.575893701772)) ;
#92128 = CARTESIAN_POINT('Ctrl Pts',(-20.7895447714591,52.1126516410056,122.80536324698)) ;
#92129 = CARTESIAN_POINT('Ctrl Pts',(-20.8739174433946,52.1226887148236,123.055264793137)) ;
#92130 = CARTESIAN_POINT('Ctrl Pts',(-20.913466812998,52.1325637178352,123.311769299998)) ;
#92131 = CARTESIAN_POINT('Ctrl Pts',(-20.907759863983,52.1426313974614,123.576238886036)) ;
#92132 = CARTESIAN_POINT('Ctrl Pts',(-20.8575136474615,52.1524722476791,123.829949405008)) ;
#92133 = CARTESIAN_POINT('Ctrl Pts',(-20.7314604670083,52.1658084461551,124.156927153833)) ;
#92134 = CARTESIAN_POINT('Ctrl Pts',(-20.5246587062285,52.1790259699695,124.440942087782)) ;
#92135 = CARTESIAN_POINT('Ctrl Pts',(-20.2524006445835,52.1923608964608,124.661535277277)) ;
#92136 = CARTESIAN_POINT('Ctrl Pts',(-20.0229908221438,52.2023439970554,124.788885516254)) ;
#92137 = CARTESIAN_POINT('Ctrl Pts',(-19.7733578676333,52.212388772955,124.874606471109)) ;
#92138 = CARTESIAN_POINT('Ctrl Pts',(-19.5185625305117,52.2222066961409,124.91526712013)) ;
#92139 = CARTESIAN_POINT('Ctrl Pts',(-19.2545108614186,52.2322560100963,124.911509845062)) ;
#92140 = CARTESIAN_POINT('Ctrl Pts',(-18.9112692834644,52.2455597507188,124.845226243308)) ;
#92141 = CARTESIAN_POINT('Ctrl Pts',(-18.5163692561841,52.2620499461955,124.6549048869)) ;
#92142 = CARTESIAN_POINT('Ctrl Pts',(-18.2061367720864,52.2787691111201,124.336934261931)) ;
#92143 = CARTESIAN_POINT('Ctrl Pts',(-18.0368883651409,52.2919301047903,124.035235554106)) ;
#92144 = CARTESIAN_POINT('Ctrl Pts',(-17.9492083451138,52.3019263268955,123.78763251036)) ;
#92145 = CARTESIAN_POINT('Ctrl Pts',(-17.9063157112242,52.3119501664292,123.527728946304)) ;
#92146 = CARTESIAN_POINT('Ctrl Pts',(-17.9093488352234,52.3251434884225,123.181008469196)) ;
#92147 = CARTESIAN_POINT('Ctrl Pts',(-18.0271239216375,52.3418026601998,122.754229453944)) ;
#92148 = CARTESIAN_POINT('Ctrl Pts',(-18.3339431995994,52.3617128356855,122.323055504623)) ;
#92149 = CARTESIAN_POINT('Ctrl Pts',(-18.7684450300349,52.3816028235299,122.021837292416)) ;
#92150 = CARTESIAN_POINT('Ctrl Pts',(-19.2825994094008,52.4016082715447,121.886694009092)) ;
#92151 = CARTESIAN_POINT('Ctrl Pts',(-19.8078170341868,52.421444665572,121.934185674863)) ;
#92152 = CARTESIAN_POINT('Ctrl Pts',(-20.289256959109,52.4414524594687,122.159679285256)) ;
#92153 = CARTESIAN_POINT('Ctrl Pts',(-20.6617455226346,52.4612790957627,122.532558034168)) ;
#92154 = CARTESIAN_POINT('Ctrl Pts',(-20.8871676648136,52.4812580387165,123.013320567925)) ;
#92155 = CARTESIAN_POINT('Ctrl Pts',(-20.9339425757462,52.5011898405856,123.540934620001)) ;
#92156 = CARTESIAN_POINT('Ctrl Pts',(-20.8002546271562,52.5210141410831,124.050758632293)) ;
#92157 = CARTESIAN_POINT('Ctrl Pts',(-20.495952731629,52.5411101424229,124.489450915891)) ;
#92158 = CARTESIAN_POINT('Ctrl Pts',(-20.0674306833606,52.5608685585269,124.793545669361)) ;
#92159 = CARTESIAN_POINT('Ctrl Pts',(-19.5529252626636,52.580962251411,124.935529369241)) ;
#92160 = CARTESIAN_POINT('Ctrl Pts',(-19.2053368719646,52.5940732173177,124.907896808842)) ;
#92161 = CARTESIAN_POINT('Ctrl Pts',(-19.0351230767564,52.6007865921055,124.864328531831)) ;
#92162 = CARTESIAN_POINT('Ctrl Pts',(-20.5445227346514,11.6199309704797,123.023213403245)) ;
#92163 = CARTESIAN_POINT('Ctrl Pts',(-20.5894944903278,11.6265578212978,123.154538008635)) ;
#92164 = CARTESIAN_POINT('Ctrl Pts',(-20.6334264846015,11.6397884477788,123.432369762605)) ;
#92165 = CARTESIAN_POINT('Ctrl Pts',(-20.5528870652718,11.6597640690375,123.849424031788)) ;
#92166 = CARTESIAN_POINT('Ctrl Pts',(-20.335194670966,11.6796814039394,124.212661043596)) ;
#92167 = CARTESIAN_POINT('Ctrl Pts',(-20.0078996672985,11.6995546806554,124.480006178853)) ;
#92168 = CARTESIAN_POINT('Ctrl Pts',(-19.6059595960299,11.7195791708194,124.620366670198)) ;
#92169 = CARTESIAN_POINT('Ctrl Pts',(-19.1834847167275,11.7394470119701,124.615091675808)) ;
#92170 = CARTESIAN_POINT('Ctrl Pts',(-18.7864894845612,11.7593926628497,124.466037547562)) ;
#92171 = CARTESIAN_POINT('Ctrl Pts',(-18.4649119653887,11.7792980634666,124.190860821467)) ;
#92172 = CARTESIAN_POINT('Ctrl Pts',(-18.2561386171959,11.799172291283,123.823451738956)) ;
#92173 = CARTESIAN_POINT('Ctrl Pts',(-18.1848458737542,11.8191580821606,123.404512084067)) ;
#92174 = CARTESIAN_POINT('Ctrl Pts',(-18.2606755610484,11.8390523248204,122.988387677173)) ;
#92175 = CARTESIAN_POINT('Ctrl Pts',(-18.4728669365122,11.8589310408924,122.622775076827)) ;
#92176 = CARTESIAN_POINT('Ctrl Pts',(-18.799957735148,11.878970490737,122.349782358275)) ;
#92177 = CARTESIAN_POINT('Ctrl Pts',(-19.1972060310392,11.8988336522749,122.205994913541)) ;
#92178 = CARTESIAN_POINT('Ctrl Pts',(-19.6218870457641,11.9188130202891,122.20615905977)) ;
#92179 = CARTESIAN_POINT('Ctrl Pts',(-20.0180120514052,11.9386236008119,122.34965257654)) ;
#92180 = CARTESIAN_POINT('Ctrl Pts',(-20.3444465319008,11.9586045290975,122.621438236603)) ;
#92181 = CARTESIAN_POINT('Ctrl Pts',(-20.5574196891661,11.9784972009669,122.986936080641)) ;
#92182 = CARTESIAN_POINT('Ctrl Pts',(-20.6337267052267,11.9984235312541,123.403693647051)) ;
#92183 = CARTESIAN_POINT('Ctrl Pts',(-20.5626962506009,12.0183940853463,123.822338761092)) ;
#92184 = CARTESIAN_POINT('Ctrl Pts',(-20.3894978612787,12.034925924434,124.128191012563)) ;
#92185 = CARTESIAN_POINT('Ctrl Pts',(-20.1931346813434,12.0482656632615,124.328472306739)) ;
#92186 = CARTESIAN_POINT('Ctrl Pts',(-20.0213926302728,12.0582979054801,124.450877152138)) ;
#92187 = CARTESIAN_POINT('Ctrl Pts',(-19.8344383779008,12.0681556061236,124.540321539624)) ;
#92188 = CARTESIAN_POINT('Ctrl Pts',(-19.6322019782122,12.0781474707628,124.597064388761)) ;
#92189 = CARTESIAN_POINT('Ctrl Pts',(-19.4246153322092,12.088070020523,124.617642787167)) ;
#92190 = CARTESIAN_POINT('Ctrl Pts',(-19.1462130031105,12.1013477940164,124.597251023731)) ;
#92191 = CARTESIAN_POINT('Ctrl Pts',(-18.8783247840957,12.114695132957,124.503674877243)) ;
#92192 = CARTESIAN_POINT('Ctrl Pts',(-18.6486087161095,12.1279023647502,124.347609590522)) ;
#92193 = CARTESIAN_POINT('Ctrl Pts',(-18.4978177422815,12.1378894808399,124.201561840989)) ;
#92194 = CARTESIAN_POINT('Ctrl Pts',(-18.3749666561639,12.1478403864197,124.032184068499)) ;
#92195 = CARTESIAN_POINT('Ctrl Pts',(-18.2826817593171,12.1578954884271,123.842034948984)) ;
#92196 = CARTESIAN_POINT('Ctrl Pts',(-18.2257950816562,12.1677171617482,123.643518261886)) ;
#92197 = CARTESIAN_POINT('Ctrl Pts',(-18.2033811742633,12.1777756328231,123.433271579607)) ;
#92198 = CARTESIAN_POINT('Ctrl Pts',(-18.2179067683536,12.1877002439996,123.225110804427)) ;
#92199 = CARTESIAN_POINT('Ctrl Pts',(-18.2846782998038,12.2009775829,122.954100941105)) ;
#92200 = CARTESIAN_POINT('Ctrl Pts',(-18.4211173081076,12.2142764621376,122.706459212318)) ;
#92201 = CARTESIAN_POINT('Ctrl Pts',(-18.6137339222405,12.2275153343083,122.505496739314)) ;
#92202 = CARTESIAN_POINT('Ctrl Pts',(-18.7832480718907,12.2375219524449,122.380910624351)) ;
#92203 = CARTESIAN_POINT('Ctrl Pts',(-18.9724531322104,12.2475528975064,122.28779225172)) ;
#92204 = CARTESIAN_POINT('Ctrl Pts',(-19.1713357060114,12.2574090708583,122.229594631958)) ;
#92205 = CARTESIAN_POINT('Ctrl Pts',(-19.3802130015109,12.2674083418211,122.206224196306)) ;
#92206 = CARTESIAN_POINT('Ctrl Pts',(-19.587865646609,12.2773027935785,122.21909984271)) ;
#92207 = CARTESIAN_POINT('Ctrl Pts',(-19.7934896821476,12.2873661093878,122.268715027323)) ;
#92208 = CARTESIAN_POINT('Ctrl Pts',(-19.9832142650933,12.2972049661274,122.351202095469)) ;
#92209 = CARTESIAN_POINT('Ctrl Pts',(-20.1597895100835,12.307271087945,122.467780803607)) ;
#92210 = CARTESIAN_POINT('Ctrl Pts',(-20.3106265987992,12.3171543156693,122.610717010097)) ;
#92211 = CARTESIAN_POINT('Ctrl Pts',(-20.4360240844988,12.3271437769481,122.779153372951)) ;
#92212 = CARTESIAN_POINT('Ctrl Pts',(-20.5299739138694,12.3371074873745,122.966382465082)) ;
#92213 = CARTESIAN_POINT('Ctrl Pts',(-20.5903897233038,12.3471024901054,123.167652551721)) ;
#92214 = CARTESIAN_POINT('Ctrl Pts',(-20.6147102753088,12.3571388211157,123.377230955125)) ;
#92215 = CARTESIAN_POINT('Ctrl Pts',(-20.6028463785135,12.366985050458,123.583902306401)) ;
#92216 = CARTESIAN_POINT('Ctrl Pts',(-20.55499669517,12.3769705487333,123.78826882071)) ;
#92217 = CARTESIAN_POINT('Ctrl Pts',(-20.4729187867284,12.3869054517162,123.980370474057)) ;
#92218 = CARTESIAN_POINT('Ctrl Pts',(-20.357202174755,12.3969629548115,124.157299802648)) ;
#92219 = CARTESIAN_POINT('Ctrl Pts',(-20.2161112271615,12.406784611182,124.308089113549)) ;
#92220 = CARTESIAN_POINT('Ctrl Pts',(-20.0473094933482,12.4168406738471,124.435340831555)) ;
#92221 = CARTESIAN_POINT('Ctrl Pts',(-19.8609443801348,12.4267813385503,124.529924426438)) ;
#92222 = CARTESIAN_POINT('Ctrl Pts',(-19.661913020913,12.4366857424989,124.591112791133)) ;
#92223 = CARTESIAN_POINT('Ctrl Pts',(-19.4523192188681,12.4467322274924,124.61704985095)) ;
#92224 = CARTESIAN_POINT('Ctrl Pts',(-19.244505090046,12.4566284553041,124.606538219516)) ;
#92225 = CARTESIAN_POINT('Ctrl Pts',(-19.038368143445,12.4666880388676,124.559383118642)) ;
#92226 = CARTESIAN_POINT('Ctrl Pts',(-18.8475319973023,12.4765400485364,124.478858162415)) ;
#92227 = CARTESIAN_POINT('Ctrl Pts',(-18.6712600321161,12.486502579976,124.365762071947)) ;
#92228 = CARTESIAN_POINT('Ctrl Pts',(-18.5164450101254,12.4965341282154,124.2225425962)) ;
#92229 = CARTESIAN_POINT('Ctrl Pts',(-18.3904774875118,12.5064255394284,124.057089554792)) ;
#92230 = CARTESIAN_POINT('Ctrl Pts',(-18.293606379704,12.5164417931364,123.870112765132)) ;
#92231 = CARTESIAN_POINT('Ctrl Pts',(-18.2310247401732,12.5264718959811,123.668752585858)) ;
#92232 = CARTESIAN_POINT('Ctrl Pts',(-18.2044223869209,12.5363283449348,123.463240844313)) ;
#92233 = CARTESIAN_POINT('Ctrl Pts',(-18.2137782919258,12.5463273557071,123.253271994429)) ;
#92234 = CARTESIAN_POINT('Ctrl Pts',(-18.2587650999899,12.5562225726251,123.050131413911)) ;
#92235 = CARTESIAN_POINT('Ctrl Pts',(-18.3396685918713,12.5662830879825,122.854741766294)) ;
#92236 = CARTESIAN_POINT('Ctrl Pts',(-18.4508077372585,12.5761323813695,122.680014247902)) ;
#92237 = CARTESIAN_POINT('Ctrl Pts',(-18.5927131357453,12.5861595570495,122.524134244484)) ;
#92238 = CARTESIAN_POINT('Ctrl Pts',(-18.7599030448378,12.5961881326767,122.395673642162)) ;
#92239 = CARTESIAN_POINT('Ctrl Pts',(-18.9432361413831,12.6060332262226,122.299636183444)) ;
#92240 = CARTESIAN_POINT('Ctrl Pts',(-19.143231548689,12.6160244676544,122.235427961324)) ;
#92241 = CARTESIAN_POINT('Ctrl Pts',(-19.3523277802074,12.6260602487976,122.207228145607)) ;
#92242 = CARTESIAN_POINT('Ctrl Pts',(-19.5592861451502,12.6359124545273,122.21533000764)) ;
#92243 = CARTESIAN_POINT('Ctrl Pts',(-19.7640842288228,12.6458745486443,122.259137338286)) ;
#92244 = CARTESIAN_POINT('Ctrl Pts',(-19.9592496327906,12.6558971094714,122.338556576803)) ;
#92245 = CARTESIAN_POINT('Ctrl Pts',(-20.1360993033801,12.665824881123,122.449432036472)) ;
#92246 = CARTESIAN_POINT('Ctrl Pts',(-20.2927583986931,12.6758672652478,122.590938510581)) ;
#92247 = CARTESIAN_POINT('Ctrl Pts',(-20.4205737162939,12.6857564893184,122.754925391399)) ;
#92248 = CARTESIAN_POINT('Ctrl Pts',(-20.5192984754898,12.6957457374858,122.940270425406)) ;
#92249 = CARTESIAN_POINT('Ctrl Pts',(-20.5839903499472,12.7057043145277,123.139379566424)) ;
#92250 = CARTESIAN_POINT('Ctrl Pts',(-20.6134664462127,12.715603883619,123.345414238047)) ;
#92251 = CARTESIAN_POINT('Ctrl Pts',(-20.6065457688213,12.725651795703,123.556518045616)) ;
#92252 = CARTESIAN_POINT('Ctrl Pts',(-20.5638845268326,12.7355471500102,123.760161210046)) ;
#92253 = CARTESIAN_POINT('Ctrl Pts',(-20.4852609822995,12.7456088005014,123.956508878827)) ;
#92254 = CARTESIAN_POINT('Ctrl Pts',(-20.3761562392932,12.7554534159639,124.132387479674)) ;
#92255 = CARTESIAN_POINT('Ctrl Pts',(-20.2371197672901,12.7654134948653,124.288952076224)) ;
#92256 = CARTESIAN_POINT('Ctrl Pts',(-20.0714719977901,12.7754516892237,124.419691962734)) ;
#92257 = CARTESIAN_POINT('Ctrl Pts',(-19.8888380147407,12.7853254046233,124.518402099819)) ;
#92258 = CARTESIAN_POINT('Ctrl Pts',(-19.6879341559414,12.7953971141575,124.585176374158)) ;
#92259 = CARTESIAN_POINT('Ctrl Pts',(-19.4834367028135,12.80522955461,124.615443528027)) ;
#92260 = CARTESIAN_POINT('Ctrl Pts',(-19.2726059179426,12.8152613755354,124.610216782179)) ;
#92261 = CARTESIAN_POINT('Ctrl Pts',(-19.066233358849,12.825281745421,124.567919596225)) ;
#92262 = CARTESIAN_POINT('Ctrl Pts',(-18.8731330036246,12.8351485165548,124.492120682358)) ;
#92263 = CARTESIAN_POINT('Ctrl Pts',(-18.6925009420882,12.8452192877441,124.381720161414)) ;
#92264 = CARTESIAN_POINT('Ctrl Pts',(-18.5373294413364,12.8550624482657,124.244796187377)) ;
#92265 = CARTESIAN_POINT('Ctrl Pts',(-18.405965860316,12.8650426814522,124.081200769751)) ;
#92266 = CARTESIAN_POINT('Ctrl Pts',(-18.3049709875459,12.8750612014873,123.896379551838)) ;
#92267 = CARTESIAN_POINT('Ctrl Pts',(-18.2380816514897,12.884944509871,123.699636080652)) ;
#92268 = CARTESIAN_POINT('Ctrl Pts',(-18.2058768851209,12.8950127940418,123.49046826295)) ;
#92269 = CARTESIAN_POINT('Ctrl Pts',(-18.2101289812869,12.9048429207095,123.283817080971)) ;
#92270 = CARTESIAN_POINT('Ctrl Pts',(-18.2508798494434,12.914909492916,123.076180845837)) ;
#92271 = CARTESIAN_POINT('Ctrl Pts',(-18.3258687904528,12.9247996491567,122.882224430381)) ;
#92272 = CARTESIAN_POINT('Ctrl Pts',(-18.4340994943442,12.9347921767331,122.702192267854)) ;
#92273 = CARTESIAN_POINT('Ctrl Pts',(-18.5716617642104,12.9447536666074,122.544287781033)) ;
#92274 = CARTESIAN_POINT('Ctrl Pts',(-18.7334032826049,12.9546628884946,122.412979815522)) ;
#92275 = CARTESIAN_POINT('Ctrl Pts',(-18.9180668962006,12.964711468305,122.310402911689)) ;
#92276 = CARTESIAN_POINT('Ctrl Pts',(-19.1144428404073,12.974594442775,122.242506577825)) ;
#92277 = CARTESIAN_POINT('Ctrl Pts',(-19.3218591967594,12.9845893539177,122.208921815214)) ;
#92278 = CARTESIAN_POINT('Ctrl Pts',(-19.5325086925485,12.9946097404913,122.212159430771)) ;
#92279 = CARTESIAN_POINT('Ctrl Pts',(-19.7371141602649,13.0045198443484,122.251364318688)) ;
#92280 = CARTESIAN_POINT('Ctrl Pts',(-19.9323647416642,13.0144475565583,122.325127276843)) ;
#92281 = CARTESIAN_POINT('Ctrl Pts',(-20.1138238542012,13.0244906663255,122.43305488188)) ;
#92282 = CARTESIAN_POINT('Ctrl Pts',(-20.271392834906,13.0343770867811,122.568612045325)) ;
#92283 = CARTESIAN_POINT('Ctrl Pts',(-20.4047144556346,13.0443702643867,122.730961891438)) ;
#92284 = CARTESIAN_POINT('Ctrl Pts',(-20.5072674195486,13.0543159272906,122.913174162945)) ;
#92285 = CARTESIAN_POINT('Ctrl Pts',(-20.5770419750784,13.0642632234958,123.110324439017)) ;
#92286 = CARTESIAN_POINT('Ctrl Pts',(-20.6116395103525,13.0743109890737,123.318702092503)) ;
#92287 = CARTESIAN_POINT('Ctrl Pts',(-20.609736311941,13.0841592022913,123.525730665591)) ;
#92288 = CARTESIAN_POINT('Ctrl Pts',(-20.5721675728708,13.0941187750854,123.731713474569)) ;
#92289 = CARTESIAN_POINT('Ctrl Pts',(-20.49849609699,13.1041553961179,123.929428907478)) ;
#92290 = CARTESIAN_POINT('Ctrl Pts',(-20.3935412625952,13.1140359109283,124.108708072959)) ;
#92291 = CARTESIAN_POINT('Ctrl Pts',(-20.256803522262,13.1240885622353,124.269810817987)) ;
#92292 = CARTESIAN_POINT('Ctrl Pts',(-20.0967179660429,13.1339839605153,124.402720826304)) ;
#92293 = CARTESIAN_POINT('Ctrl Pts',(-19.9132627916011,13.1440340822214,124.507479233927)) ;
#92294 = CARTESIAN_POINT('Ctrl Pts',(-19.7176528780897,13.1539183617633,124.577663668273)) ;
#92295 = CARTESIAN_POINT('Ctrl Pts',(-19.5106451886869,13.1639131430553,124.613591987952)) ;
#92296 = CARTESIAN_POINT('Ctrl Pts',(-19.3014971588943,13.173860988242,124.612953430792)) ;
#92297 = CARTESIAN_POINT('Ctrl Pts',(-19.0958408347169,13.1837979516294,124.576354555244)) ;
#92298 = CARTESIAN_POINT('Ctrl Pts',(-18.8986217867637,13.1937809163667,124.504501871259)) ;
#92299 = CARTESIAN_POINT('Ctrl Pts',(-18.7160044802564,13.2038247677823,124.398546770036)) ;
#92300 = CARTESIAN_POINT('Ctrl Pts',(-18.5576688200036,13.213652969117,124.265752345939)) ;
#92301 = CARTESIAN_POINT('Ctrl Pts',(-18.4214089685337,13.2237295417151,124.103605374704)) ;
#92302 = CARTESIAN_POINT('Ctrl Pts',(-18.3176012012084,13.2335816217226,123.924323648453)) ;
#92303 = CARTESIAN_POINT('Ctrl Pts',(-18.2447624006463,13.2436549067267,123.72550920738)) ;
#92304 = CARTESIAN_POINT('Ctrl Pts',(-18.208451810443,13.2534962584372,123.521808408546)) ;
#92305 = CARTESIAN_POINT('Ctrl Pts',(-18.2072839695112,13.2634577578337,123.312402302002)) ;
#92306 = CARTESIAN_POINT('Ctrl Pts',(-18.2431243993998,13.2734935339637,123.104477477949)) ;
#92307 = CARTESIAN_POINT('Ctrl Pts',(-18.313266330403,13.2833819606013,122.908785022229)) ;
#92308 = CARTESIAN_POINT('Ctrl Pts',(-18.4173025005469,13.2933972826762,122.725719708377)) ;
#92309 = CARTESIAN_POINT('Ctrl Pts',(-18.5521194854302,13.3034276315764,122.563574882499)) ;
#92310 = CARTESIAN_POINT('Ctrl Pts',(-18.7097686111955,13.3132710071831,122.429528077292)) ;
#92311 = CARTESIAN_POINT('Ctrl Pts',(-18.8914413302913,13.3233004440802,122.322502843686)) ;
#92312 = CARTESIAN_POINT('Ctrl Pts',(-19.0891909613697,13.3333323220132,122.249169485467)) ;
#92313 = CARTESIAN_POINT('Ctrl Pts',(-19.2923910333282,13.3431619451186,122.211639193978)) ;
#92314 = CARTESIAN_POINT('Ctrl Pts',(-19.502393832661,13.3531514162717,122.209303795918)) ;
#92315 = CARTESIAN_POINT('Ctrl Pts',(-19.7106448636121,13.3631952650341,122.244181269422)) ;
#92316 = CARTESIAN_POINT('Ctrl Pts',(-19.9054181897071,13.3730169705658,122.312725988821)) ;
#92317 = CARTESIAN_POINT('Ctrl Pts',(-20.0894923568458,13.3830520103936,122.415798365004)) ;
#92318 = CARTESIAN_POINT('Ctrl Pts',(-20.2523425372492,13.3930767172851,122.549585325473)) ;
#92319 = CARTESIAN_POINT('Ctrl Pts',(-20.3874635134863,13.4029294216258,122.706578422699)) ;
#92320 = CARTESIAN_POINT('Ctrl Pts',(-20.4950348439509,13.4129175438335,122.886895979639)) ;
#92321 = CARTESIAN_POINT('Ctrl Pts',(-20.5692346947087,13.4228460139408,123.081995305985)) ;
#92322 = CARTESIAN_POINT('Ctrl Pts',(-20.6090140362735,13.432834991108,123.288203344706)) ;
#92323 = CARTESIAN_POINT('Ctrl Pts',(-20.6120399406672,13.4428727983877,123.499202411649)) ;
#92324 = CARTESIAN_POINT('Ctrl Pts',(-20.5793586418842,13.452719099251,123.703608133179)) ;
#92325 = CARTESIAN_POINT('Ctrl Pts',(-20.5108933572167,13.4627448426303,123.902954077039)) ;
#92326 = CARTESIAN_POINT('Ctrl Pts',(-20.4083206395446,13.4727757090693,124.087214524616)) ;
#92327 = CARTESIAN_POINT('Ctrl Pts',(-20.2782096665818,13.4826130678681,124.247959027508)) ;
#92328 = CARTESIAN_POINT('Ctrl Pts',(-20.1200757179898,13.4926050288019,124.386233234674)) ;
#92329 = CARTESIAN_POINT('Ctrl Pts',(-19.9393814428224,13.5026373913584,124.49503121546)) ;
#92330 = CARTESIAN_POINT('Ctrl Pts',(-19.7459291056501,13.5125025519328,124.569766299206)) ;
#92331 = CARTESIAN_POINT('Ctrl Pts',(-19.5405428766504,13.5224644565105,124.610756191711)) ;
#92332 = CARTESIAN_POINT('Ctrl Pts',(-19.3296341394368,13.5324993865863,124.615150409196)) ;
#92333 = CARTESIAN_POINT('Ctrl Pts',(-19.1241882593552,13.5423843334399,124.583680283996)) ;
#92334 = CARTESIAN_POINT('Ctrl Pts',(-18.9238050394512,13.5524500097513,124.515772546314)) ;
#92335 = CARTESIAN_POINT('Ctrl Pts',(-18.7422738965292,13.5622889293862,124.416547647665)) ;
#92336 = CARTESIAN_POINT('Ctrl Pts',(-18.5769211989035,13.5723524391207,124.284614914722)) ;
#92337 = CARTESIAN_POINT('Ctrl Pts',(-18.4394438861558,13.5822460522824,124.128499673236)) ;
#92338 = CARTESIAN_POINT('Ctrl Pts',(-18.3301649112488,13.5921900590958,123.950314429451)) ;
#92339 = CARTESIAN_POINT('Ctrl Pts',(-18.2529317702578,13.6021910134501,123.754727546131)) ;
#92340 = CARTESIAN_POINT('Ctrl Pts',(-18.2110520035819,13.6122297711424,123.547897327596)) ;
#92341 = CARTESIAN_POINT('Ctrl Pts',(-18.2053814428901,13.6220539553124,123.341422778142)) ;
#92342 = CARTESIAN_POINT('Ctrl Pts',(-18.2360559572279,13.6321120209118,123.132225921939)) ;
#92343 = CARTESIAN_POINT('Ctrl Pts',(-18.3020120677171,13.6420420676865,122.934144610065)) ;
#92344 = CARTESIAN_POINT('Ctrl Pts',(-18.4010833770443,13.6519935100237,122.749875864742)) ;
#92345 = CARTESIAN_POINT('Ctrl Pts',(-18.5321101585894,13.6620403072029,122.584217084689)) ;
#92346 = CARTESIAN_POINT('Ctrl Pts',(-18.6866603271967,13.671888247883,122.446457937948)) ;
#92347 = CARTESIAN_POINT('Ctrl Pts',(-18.8644655503016,13.6818498792256,122.335821822434)) ;
#92348 = CARTESIAN_POINT('Ctrl Pts',(-19.0602066261718,13.6918785386015,122.257452037881)) ;
#92349 = CARTESIAN_POINT('Ctrl Pts',(-19.2641111645517,13.7017888414897,122.214707825771)) ;
#92350 = CARTESIAN_POINT('Ctrl Pts',(-19.4728545144785,13.7117237360519,122.20745340348)) ;
#92351 = CARTESIAN_POINT('Ctrl Pts',(-19.6818574037471,13.7217648347188,122.237057214757)) ;
#92352 = CARTESIAN_POINT('Ctrl Pts',(-19.8795330996557,13.7316521172232,122.301367089129)) ;
#92353 = CARTESIAN_POINT('Ctrl Pts',(-20.0651234113588,13.7416438577337,122.399728612142)) ;
#92354 = CARTESIAN_POINT('Ctrl Pts',(-20.2301072815395,13.7515944069691,122.528359355941)) ;
#92355 = CARTESIAN_POINT('Ctrl Pts',(-20.3702567984072,13.7615300846039,122.683224869918)) ;
#92356 = CARTESIAN_POINT('Ctrl Pts',(-20.4821496556636,13.7715155023967,122.860862904044)) ;
#92357 = CARTESIAN_POINT('Ctrl Pts',(-20.5615945408518,13.7815442952672,123.0561577358)) ;
#92358 = CARTESIAN_POINT('Ctrl Pts',(-20.6054790317027,13.7914238064952,123.259164226479)) ;
#92359 = CARTESIAN_POINT('Ctrl Pts',(-20.6140230823703,13.8014173431681,123.469094191305)) ;
#92360 = CARTESIAN_POINT('Ctrl Pts',(-20.585445224323,13.811449611432,123.678050048262)) ;
#92361 = CARTESIAN_POINT('Ctrl Pts',(-20.5225142881585,13.8213135734378,123.87566527456)) ;
#92362 = CARTESIAN_POINT('Ctrl Pts',(-20.4242668998113,13.8313836347827,124.063166872024)) ;
#92363 = CARTESIAN_POINT('Ctrl Pts',(-20.2978535284329,13.8412259991315,124.226991218957)) ;
#92364 = CARTESIAN_POINT('Ctrl Pts',(-20.1436080829852,13.8511866716339,124.368614446249)) ;
#92365 = CARTESIAN_POINT('Ctrl Pts',(-19.9655216287888,13.8612247427017,124.481821965117)) ;
#92366 = CARTESIAN_POINT('Ctrl Pts',(-19.7737943270889,13.8710983576622,124.561451063385)) ;
#92367 = CARTESIAN_POINT('Ctrl Pts',(-19.5671347818474,13.8811705922434,124.607418828005)) ;
#92368 = CARTESIAN_POINT('Ctrl Pts',(-19.3607740702346,13.8909946106922,124.616812785889)) ;
#92369 = CARTESIAN_POINT('Ctrl Pts',(-19.1509484011636,13.9010595316682,124.58986547138)) ;
#92370 = CARTESIAN_POINT('Ctrl Pts',(-18.885742263977,13.914269829963,124.507190963404)) ;
#92371 = CARTESIAN_POINT('Ctrl Pts',(-18.6462438685015,13.9275852766949,124.356328792661)) ;
#92372 = CARTESIAN_POINT('Ctrl Pts',(-18.4564443634539,13.9408755219622,124.151228756277)) ;
#92373 = CARTESIAN_POINT('Ctrl Pts',(-18.342158496396,13.9509262715693,123.973546314054)) ;
#92374 = CARTESIAN_POINT('Ctrl Pts',(-18.2619972946885,13.9607388785516,123.783433874635)) ;
#92375 = CARTESIAN_POINT('Ctrl Pts',(-18.2145910925196,13.9708099765458,123.577110199186)) ;
#92376 = CARTESIAN_POINT('Ctrl Pts',(-18.2041343921619,13.9806995493207,123.369451365273)) ;
#92377 = CARTESIAN_POINT('Ctrl Pts',(-18.2378551925476,13.993969656124,123.092490222189)) ;
#92378 = CARTESIAN_POINT('Ctrl Pts',(-18.3698703473456,14.0105863430465,122.764819038362)) ;
#92379 = CARTESIAN_POINT('Ctrl Pts',(-18.6050453003926,14.0271603863627,122.502296275381)) ;
#92380 = CARTESIAN_POINT('Ctrl Pts',(-18.8388900954275,14.0404569537945,122.349191219826)) ;
#92381 = CARTESIAN_POINT('Ctrl Pts',(-19.0327140636966,14.0504870173719,122.266120699076)) ;
#92382 = CARTESIAN_POINT('Ctrl Pts',(-19.2351925600069,14.0603809092212,122.218606664563)) ;
#92383 = CARTESIAN_POINT('Ctrl Pts',(-19.5133779733471,14.0736336650067,122.202020467964)) ;
#92384 = CARTESIAN_POINT('Ctrl Pts',(-19.861630213909,14.0903617699992,122.274027261423)) ;
#92385 = CARTESIAN_POINT('Ctrl Pts',(-20.2206980924579,14.1101926064777,122.495229552412)) ;
#92386 = CARTESIAN_POINT('Ctrl Pts',(-20.4846805942354,14.1301179983678,122.82648134403)) ;
#92387 = CARTESIAN_POINT('Ctrl Pts',(-20.6197806891536,14.1500432117198,123.228098261421)) ;
#92388 = CARTESIAN_POINT('Ctrl Pts',(-20.6098292151628,14.1699682252049,123.651592199698)) ;
#92389 = CARTESIAN_POINT('Ctrl Pts',(-20.4568502730151,14.1898446969049,124.045589490744)) ;
#92390 = CARTESIAN_POINT('Ctrl Pts',(-20.1773267785576,14.2098240148138,124.365478534255)) ;
#92391 = CARTESIAN_POINT('Ctrl Pts',(-19.8060955662964,14.2297570183898,124.57004462274)) ;
#92392 = CARTESIAN_POINT('Ctrl Pts',(-19.3882614282935,14.2496522884175,124.635961689666)) ;
#92393 = CARTESIAN_POINT('Ctrl Pts',(-18.9723460075604,14.2695736263233,124.555651033609)) ;
#92394 = CARTESIAN_POINT('Ctrl Pts',(-18.6081837258384,14.2895312495895,124.337753529704)) ;
#92395 = CARTESIAN_POINT('Ctrl Pts',(-18.3412613634703,14.3094110815467,124.010077065692)) ;
#92396 = CARTESIAN_POINT('Ctrl Pts',(-18.2010168508074,14.3292929328436,123.611189475518)) ;
#92397 = CARTESIAN_POINT('Ctrl Pts',(-18.2061577248165,14.3493639499474,123.184511236421)) ;
#92398 = CARTESIAN_POINT('Ctrl Pts',(-18.3545971695844,14.3691711737005,122.790298921947)) ;
#92399 = CARTESIAN_POINT('Ctrl Pts',(-18.6302230516465,14.3891523092693,122.46703788842)) ;
#92400 = CARTESIAN_POINT('Ctrl Pts',(-18.9990325033521,14.4090798026085,122.258519623265)) ;
#92401 = CARTESIAN_POINT('Ctrl Pts',(-19.414530819844,14.4289004639663,122.187301272222)) ;
#92402 = CARTESIAN_POINT('Ctrl Pts',(-19.8347873766851,14.4489976531881,122.263805862817)) ;
#92403 = CARTESIAN_POINT('Ctrl Pts',(-20.198042463916,14.4687613321965,122.475491438185)) ;
#92404 = CARTESIAN_POINT('Ctrl Pts',(-20.4713802055925,14.4888186108695,122.802607800385)) ;
#92405 = CARTESIAN_POINT('Ctrl Pts',(-20.6146598595421,14.5086140346169,123.198496313193)) ;
#92406 = CARTESIAN_POINT('Ctrl Pts',(-20.6155549975082,14.5285776793445,123.622927843257)) ;
#92407 = CARTESIAN_POINT('Ctrl Pts',(-20.4704264877456,14.5485611706186,124.022283184246)) ;
#92408 = CARTESIAN_POINT('Ctrl Pts',(-20.2007731307762,14.5683686657679,124.345851921621)) ;
#92409 = CARTESIAN_POINT('Ctrl Pts',(-19.8340285534317,14.588351256488,124.560210082333)) ;
#92410 = CARTESIAN_POINT('Ctrl Pts',(-19.4180417092248,14.6082339104793,124.636132918058)) ;
#92411 = CARTESIAN_POINT('Ctrl Pts',(-18.9996610722391,14.6281921553423,124.565621343336)) ;
#92412 = CARTESIAN_POINT('Ctrl Pts',(-18.6317274635194,14.6480677423839,124.357590409106)) ;
#92413 = CARTESIAN_POINT('Ctrl Pts',(-18.3552455165215,14.6680486305192,124.03505471784)) ;
#92414 = CARTESIAN_POINT('Ctrl Pts',(-18.2060499281887,14.6879837716302,123.638243803978)) ;
#92415 = CARTESIAN_POINT('Ctrl Pts',(-18.2009208909695,14.7078957896413,123.214931994148)) ;
#92416 = CARTESIAN_POINT('Ctrl Pts',(-18.3399791205184,14.7277840078848,122.815553042048)) ;
#92417 = CARTESIAN_POINT('Ctrl Pts',(-18.5625223078794,14.7443823117317,122.541718669557)) ;
#92418 = CARTESIAN_POINT('Ctrl Pts',(-18.7884690167792,14.7576549016346,122.377905209627)) ;
#92419 = CARTESIAN_POINT('Ctrl Pts',(-18.9775554419719,14.7676623165854,122.28567841915)) ;
#92420 = CARTESIAN_POINT('Ctrl Pts',(-19.1798597979953,14.777669663318,122.227857687537)) ;
#92421 = CARTESIAN_POINT('Ctrl Pts',(-19.4571939480099,14.7909360231196,122.198758994379)) ;
#92422 = CARTESIAN_POINT('Ctrl Pts',(-19.8041248709221,14.8074506807426,122.253102924327)) ;
#92423 = CARTESIAN_POINT('Ctrl Pts',(-20.1135388548329,14.8240481139852,122.422674400155)) ;
#92424 = CARTESIAN_POINT('Ctrl Pts',(-20.31615452797,14.8373961111302,122.616914640427)) ;
#92425 = CARTESIAN_POINT('Ctrl Pts',(-20.4392738972615,14.8472918654818,122.784604403516)) ;
#92426 = CARTESIAN_POINT('Ctrl Pts',(-20.5324949220167,14.8572798194132,122.972739489712)) ;
#92427 = CARTESIAN_POINT('Ctrl Pts',(-20.5915500287685,14.8672370431179,123.173594463917)) ;
#92428 = CARTESIAN_POINT('Ctrl Pts',(-20.6149140597736,14.8772725896746,123.383260968004)) ;
#92429 = CARTESIAN_POINT('Ctrl Pts',(-20.6018719765782,14.8871597009507,123.590723482903)) ;
#92430 = CARTESIAN_POINT('Ctrl Pts',(-20.552821477757,14.8971511060515,123.794956581303)) ;
#92431 = CARTESIAN_POINT('Ctrl Pts',(-20.4693756424494,14.9070967272663,123.98667131504)) ;
#92432 = CARTESIAN_POINT('Ctrl Pts',(-20.354214645291,14.9170459755346,124.161292960662)) ;
#92433 = CARTESIAN_POINT('Ctrl Pts',(-20.2089133571514,14.9270924707032,124.314566354854)) ;
#92434 = CARTESIAN_POINT('Ctrl Pts',(-20.0426093916053,14.9369438134948,124.43801767961)) ;
#92435 = CARTESIAN_POINT('Ctrl Pts',(-19.8554010834805,14.9469155936221,124.532309421632)) ;
#92436 = CARTESIAN_POINT('Ctrl Pts',(-19.6541309256762,14.9569107935998,124.592800420983)) ;
#92437 = CARTESIAN_POINT('Ctrl Pts',(-19.4446257916061,14.9669447852959,124.617258985423)) ;
#92438 = CARTESIAN_POINT('Ctrl Pts',(-19.2377471565128,14.9768001902684,124.60551410532)) ;
#92439 = CARTESIAN_POINT('Ctrl Pts',(-19.0330947053247,14.9867994881141,124.557625447812)) ;
#92440 = CARTESIAN_POINT('Ctrl Pts',(-18.8417260095209,14.9966946007193,124.475969739033)) ;
#92441 = CARTESIAN_POINT('Ctrl Pts',(-18.6645920863028,15.0067552462543,124.360440257622)) ;
#92442 = CARTESIAN_POINT('Ctrl Pts',(-18.5133454930013,15.0166041232435,124.219009634951)) ;
#92443 = CARTESIAN_POINT('Ctrl Pts',(-18.3862687789312,15.0266328343371,124.050778467038)) ;
#92444 = CARTESIAN_POINT('Ctrl Pts',(-18.290833943396,15.0366622355932,123.8627585743)) ;
#92445 = CARTESIAN_POINT('Ctrl Pts',(-18.2302119029256,15.0465024273892,123.664964952641)) ;
#92446 = CARTESIAN_POINT('Ctrl Pts',(-18.2040500545488,15.0565058565822,123.456316133071)) ;
#92447 = CARTESIAN_POINT('Ctrl Pts',(-18.2145657258036,15.0664913690484,123.246616906617)) ;
#92448 = CARTESIAN_POINT('Ctrl Pts',(-18.26178794317,15.0765324654324,123.040892381752)) ;
#92449 = CARTESIAN_POINT('Ctrl Pts',(-18.3421420908844,15.0863756613834,122.850175892976)) ;
#92450 = CARTESIAN_POINT('Ctrl Pts',(-18.4556407699615,15.0963619724378,122.673598924012)) ;
#92451 = CARTESIAN_POINT('Ctrl Pts',(-18.5972860801751,15.1062966576955,122.520057462546)) ;
#92452 = CARTESIAN_POINT('Ctrl Pts',(-18.7655513685597,15.1163542189126,122.392067431198)) ;
#92453 = CARTESIAN_POINT('Ctrl Pts',(-18.9489772358709,15.1261758605212,122.29720460344)) ;
#92454 = CARTESIAN_POINT('Ctrl Pts',(-19.1506365364957,15.1362319241121,122.233796786245)) ;
#92455 = CARTESIAN_POINT('Ctrl Pts',(-19.3579112071296,15.1461725998739,122.207051934719)) ;
#92456 = CARTESIAN_POINT('Ctrl Pts',(-19.5659421416025,15.1560769586623,122.21601478593)) ;
#92457 = CARTESIAN_POINT('Ctrl Pts',(-19.7721296999546,15.1661236132381,122.261734136403)) ;
#92458 = CARTESIAN_POINT('Ctrl Pts',(-19.964427665596,15.1760192078809,122.341192189689)) ;
#92459 = CARTESIAN_POINT('Ctrl Pts',(-20.1429244158312,15.1860811545378,122.454662033842)) ;
#92460 = CARTESIAN_POINT('Ctrl Pts',(-20.2957651291665,15.19593077847,122.59438375581)) ;
#92461 = CARTESIAN_POINT('Ctrl Pts',(-20.42401435777,15.2058940174998,122.759973307204)) ;
#92462 = CARTESIAN_POINT('Ctrl Pts',(-20.5219183117083,15.2159185922756,122.946614153896)) ;
#92463 = CARTESIAN_POINT('Ctrl Pts',(-20.5853737220608,15.2258371549633,123.145237954804)) ;
#92464 = CARTESIAN_POINT('Ctrl Pts',(-20.6139543237281,15.2358293416873,123.35336433036)) ;
#92465 = CARTESIAN_POINT('Ctrl Pts',(-20.6055500370855,15.2458641402715,123.564151637776)) ;
#92466 = CARTESIAN_POINT('Ctrl Pts',(-20.561819537419,15.2557193309452,123.766687353874)) ;
#92467 = CARTESIAN_POINT('Ctrl Pts',(-20.4827219328532,15.2657186790982,123.961418906488)) ;
#92468 = CARTESIAN_POINT('Ctrl Pts',(-20.3723321552261,15.2756138047733,124.137780670391)) ;
#92469 = CARTESIAN_POINT('Ctrl Pts',(-20.2306926442198,15.2856743477214,124.294818432688)) ;
#92470 = CARTESIAN_POINT('Ctrl Pts',(-20.0674780549609,15.2955236219883,124.422264719081)) ;
#92471 = CARTESIAN_POINT('Ctrl Pts',(-19.8815798759222,15.3055508465582,124.521651781092)) ;
#92472 = CARTESIAN_POINT('Ctrl Pts',(-19.6810377994886,15.315579245746,124.586740132725)) ;
#92473 = CARTESIAN_POINT('Ctrl Pts',(-19.4761222822697,15.3254249961595,124.615862633411)) ;
#92474 = CARTESIAN_POINT('Ctrl Pts',(-19.2662142458841,15.3354137865603,124.609449914559)) ;
#92475 = CARTESIAN_POINT('Ctrl Pts',(-19.0595807364649,15.34545871496,124.565927889753)) ;
#92476 = CARTESIAN_POINT('Ctrl Pts',(-18.8677446724703,15.3552831997489,124.489355662704)) ;
#92477 = CARTESIAN_POINT('Ctrl Pts',(-18.687818222948,15.3653405972901,124.378336136723)) ;
#92478 = CARTESIAN_POINT('Ctrl Pts',(-18.5321217638704,15.3752666888763,124.239371247625)) ;
#92479 = CARTESIAN_POINT('Ctrl Pts',(-18.4021311831631,15.3852214740209,124.075359071023)) ;
#92480 = CARTESIAN_POINT('Ctrl Pts',(-18.3019733073139,15.3952588436785,123.889627376393)) ;
#92481 = CARTESIAN_POINT('Ctrl Pts',(-18.2364143071113,15.4051476538001,123.69233545093)) ;
#92482 = CARTESIAN_POINT('Ctrl Pts',(-18.2054278164718,15.4151370128512,123.48463093245)) ;
#92483 = CARTESIAN_POINT('Ctrl Pts',(-18.2111153558979,15.4250955603073,123.275354647825)) ;
#92484 = CARTESIAN_POINT('Ctrl Pts',(-18.2523061561099,15.4349951368583,123.071338456214)) ;
#92485 = CARTESIAN_POINT('Ctrl Pts',(-18.3294907665845,15.445043048689,122.874729180045)) ;
#92486 = CARTESIAN_POINT('Ctrl Pts',(-18.4378567487714,15.4549383965496,122.697113519463)) ;
#92487 = CARTESIAN_POINT('Ctrl Pts',(-18.5776691245229,15.4650000730808,122.538410375695)) ;
#92488 = CARTESIAN_POINT('Ctrl Pts',(-18.739350149088,15.4748445908299,122.409198110722)) ;
#92489 = CARTESIAN_POINT('Ctrl Pts',(-18.9227807417284,15.4848050345447,122.308206356016)) ;
#92490 = CARTESIAN_POINT('Ctrl Pts',(-19.1226076666943,15.4948418673629,122.24045140119)) ;
#92491 = CARTESIAN_POINT('Ctrl Pts',(-19.3278520306524,15.5047206641097,122.208586054028)) ;
#92492 = CARTESIAN_POINT('Ctrl Pts',(-19.5392660626703,15.5147799802381,122.212851541918)) ;
#92493 = CARTESIAN_POINT('Ctrl Pts',(-19.742865967899,15.5246504269913,122.252995247253)) ;
#92494 = CARTESIAN_POINT('Ctrl Pts',(-19.9389930492034,15.5346430652493,122.328273329601)) ;
#92495 = CARTESIAN_POINT('Ctrl Pts',(-20.1195385360491,15.5446750807973,122.437273842859)) ;
#92496 = CARTESIAN_POINT('Ctrl Pts',(-20.2761009054303,15.5545409371038,122.573347746441)) ;
#92497 = CARTESIAN_POINT('Ctrl Pts',(-20.4093380126393,15.564610226573,122.737816255523)) ;
#92498 = CARTESIAN_POINT('Ctrl Pts',(-20.5097308345635,15.5744537841243,122.918789549077)) ;
#92499 = CARTESIAN_POINT('Ctrl Pts',(-20.5787544431515,15.5844339109121,123.116917366312)) ;
#92500 = CARTESIAN_POINT('Ctrl Pts',(-20.6120581084781,15.594452459512,123.324883592933)) ;
#92501 = CARTESIAN_POINT('Ctrl Pts',(-20.6092324216664,15.6043357600352,123.532667468491)) ;
#92502 = CARTESIAN_POINT('Ctrl Pts',(-20.5695642818333,15.6144040470834,123.74054907884)) ;
#92503 = CARTESIAN_POINT('Ctrl Pts',(-20.4963848100476,15.624234170102,123.933856050978)) ;
#92504 = CARTESIAN_POINT('Ctrl Pts',(-20.3884819764366,15.6343007540273,124.115873435557)) ;
#92505 = CARTESIAN_POINT('Ctrl Pts',(-20.2528965593543,15.6441908670418,124.273541533496)) ;
#92506 = CARTESIAN_POINT('Ctrl Pts',(-20.0906428612495,15.6541835558044,124.406954200408)) ;
#92507 = CARTESIAN_POINT('Ctrl Pts',(-19.9081751825224,15.6641444441602,124.509724862271)) ;
#92508 = CARTESIAN_POINT('Ctrl Pts',(-19.7116275705627,15.6740623890402,124.579282836513)) ;
#92509 = CARTESIAN_POINT('Ctrl Pts',(-19.5041324121698,15.6840701421364,124.61421493708)) ;
#92510 = CARTESIAN_POINT('Ctrl Pts',(-19.2932685807458,15.6941012360955,124.612157280621)) ;
#92511 = CARTESIAN_POINT('Ctrl Pts',(-19.0896398763648,15.7039492041234,124.574676428328)) ;
#92512 = CARTESIAN_POINT('Ctrl Pts',(-18.8913605611505,15.7140111602493,124.501020788793)) ;
#92513 = CARTESIAN_POINT('Ctrl Pts',(-18.7119475879741,15.7239083718504,124.395627509335)) ;
#92514 = CARTESIAN_POINT('Ctrl Pts',(-18.5525797792541,15.7338395385151,124.260752918388)) ;
#92515 = CARTESIAN_POINT('Ctrl Pts',(-18.4177343552575,15.7438817227192,124.098313868556)) ;
#92516 = CARTESIAN_POINT('Ctrl Pts',(-18.3146251620328,15.7537683909724,123.917832449407)) ;
#92517 = CARTESIAN_POINT('Ctrl Pts',(-18.243339460562,15.7637615029506,123.720221201578)) ;
#92518 = CARTESIAN_POINT('Ctrl Pts',(-18.2076942595841,15.7737071805665,123.514192378456)) ;
#92519 = CARTESIAN_POINT('Ctrl Pts',(-18.2079375211867,15.7836544835514,123.305059117356)) ;
#92520 = CARTESIAN_POINT('Ctrl Pts',(-18.2450857165185,15.7937022072982,123.097121744275)) ;
#92521 = CARTESIAN_POINT('Ctrl Pts',(-18.3161807824206,15.8035505810607,122.902670809947)) ;
#92522 = CARTESIAN_POINT('Ctrl Pts',(-18.4205216430959,15.8135095535064,122.721154082513)) ;
#92523 = CARTESIAN_POINT('Ctrl Pts',(-18.5561610131422,15.8235484153876,122.559473819216)) ;
#92524 = CARTESIAN_POINT('Ctrl Pts',(-18.7150408738432,15.8334270195594,122.425695002758)) ;
#92525 = CARTESIAN_POINT('Ctrl Pts',(-18.8977929149903,15.8434785607627,122.319658597131)) ;
#92526 = CARTESIAN_POINT('Ctrl Pts',(-19.0931359801776,15.853373958743,122.248009867756)) ;
#92527 = CARTESIAN_POINT('Ctrl Pts',(-19.3010940919877,15.8634251912883,122.210689226876)) ;
#92528 = CARTESIAN_POINT('Ctrl Pts',(-19.5089537259741,15.8733113819126,122.210030665111)) ;
#92529 = CARTESIAN_POINT('Ctrl Pts',(-19.7159988935587,15.8833039212284,122.245467028621)) ;
#92530 = CARTESIAN_POINT('Ctrl Pts',(-19.9128808209097,15.8932523671231,122.316077247556)) ;
#92531 = CARTESIAN_POINT('Ctrl Pts',(-20.0944193281804,15.903189169655,122.419404585991)) ;
#92532 = CARTESIAN_POINT('Ctrl Pts',(-20.2562110175083,15.9131721771063,122.553127824227)) ;
#92533 = CARTESIAN_POINT('Ctrl Pts',(-20.3928269463298,15.9232160185211,122.714098594079)) ;
#92534 = CARTESIAN_POINT('Ctrl Pts',(-20.497578377328,15.933044217145,122.892232453388)) ;
#92535 = CARTESIAN_POINT('Ctrl Pts',(-20.5717018245707,15.9431208105873,123.090636598625)) ;
#92536 = CARTESIAN_POINT('Ctrl Pts',(-20.60951097072,15.9529728099288,123.29432257899)) ;
#92537 = CARTESIAN_POINT('Ctrl Pts',(-20.6115947155634,15.9630463967527,123.506054649006)) ;
#92538 = CARTESIAN_POINT('Ctrl Pts',(-20.5776393618552,15.9728866218502,123.710139972596)) ;
#92539 = CARTESIAN_POINT('Ctrl Pts',(-20.5085933061261,15.9828523258788,123.907927922325)) ;
#92540 = CARTESIAN_POINT('Ctrl Pts',(-20.4053465886935,15.9928789591854,124.091716966723)) ;
#92541 = CARTESIAN_POINT('Ctrl Pts',(-20.2733736049024,16.0027932548972,124.253036026863)) ;
#92542 = CARTESIAN_POINT('Ctrl Pts',(-20.1144504097341,16.0127815435897,124.390304177468)) ;
#92543 = CARTESIAN_POINT('Ctrl Pts',(-19.9330154783584,16.022820276748,124.498096907349)) ;
#92544 = CARTESIAN_POINT('Ctrl Pts',(-19.7395811261346,16.0326636085756,124.57162559323)) ;
#92545 = CARTESIAN_POINT('Ctrl Pts',(-19.5326001890915,16.0426913344552,124.61165647205)) ;
#92546 = CARTESIAN_POINT('Ctrl Pts',(-19.3217012772387,16.0527236708437,124.614568734802)) ;
#92547 = CARTESIAN_POINT('Ctrl Pts',(-19.1176631555562,16.0625531711444,124.58191586368)) ;
#92548 = CARTESIAN_POINT('Ctrl Pts',(-18.918992265536,16.0725426750611,124.513822087023)) ;
#92549 = CARTESIAN_POINT('Ctrl Pts',(-18.7344293125495,16.0825865155735,124.411248264033)) ;
#92550 = CARTESIAN_POINT('Ctrl Pts',(-18.5738358453558,16.0924082213416,124.281460878498)) ;
#92551 = CARTESIAN_POINT('Ctrl Pts',(-18.4348819010564,16.102443268474,124.122718726248)) ;
#92552 = CARTESIAN_POINT('Ctrl Pts',(-18.3262087689728,16.1124679459109,123.942139001591)) ;
#92553 = CARTESIAN_POINT('Ctrl Pts',(-18.2514329563652,16.1223207607653,123.748970519295)) ;
#92554 = CARTESIAN_POINT('Ctrl Pts',(-18.2104254293155,16.1323084703729,123.543056586751)) ;
#92555 = CARTESIAN_POINT('Ctrl Pts',(-18.2058105598047,16.1422384803669,123.334340214107)) ;
#92556 = CARTESIAN_POINT('Ctrl Pts',(-18.2373758696945,16.1522282355861,123.126705726276)) ;
#92557 = CARTESIAN_POINT('Ctrl Pts',(-18.305019353964,16.162254844269,122.927059279513)) ;
#92558 = CARTESIAN_POINT('Ctrl Pts',(-18.4046805537866,16.1721387842908,122.744731978536)) ;
#92559 = CARTESIAN_POINT('Ctrl Pts',(-18.5354936500919,16.1821280118293,122.580436411234)) ;
#92560 = CARTESIAN_POINT('Ctrl Pts',(-18.6939750793531,16.192170882353,122.440936931886)) ;
#92561 = CARTESIAN_POINT('Ctrl Pts',(-18.8703193497203,16.2020032691084,122.33309622009)) ;
#92562 = CARTESIAN_POINT('Ctrl Pts',(-19.0656339202826,16.21199656228,122.255709959275)) ;
#92563 = CARTESIAN_POINT('Ctrl Pts',(-19.2723178754718,16.2220285679285,122.213677943216)) ;
#92564 = CARTESIAN_POINT('Ctrl Pts',(-19.4796281174885,16.2318938238974,122.208007210553)) ;
#92565 = CARTESIAN_POINT('Ctrl Pts',(-19.6868865960668,16.2418557038049,122.23813162295)) ;
#92566 = CARTESIAN_POINT('Ctrl Pts',(-19.8870996977889,16.2518906371668,122.304588583264)) ;
#92567 = CARTESIAN_POINT('Ctrl Pts',(-20.0701600670117,16.2617755955461,122.403012887225)) ;
#92568 = CARTESIAN_POINT('Ctrl Pts',(-20.236252850506,16.2718412224688,122.534076878473)) ;
#92569 = CARTESIAN_POINT('Ctrl Pts',(-20.3740988627179,16.2816803281331,122.688345897485)) ;
#92570 = CARTESIAN_POINT('Ctrl Pts',(-20.4857489174629,16.2917431431385,122.868002488116)) ;
#92571 = CARTESIAN_POINT('Ctrl Pts',(-20.5630460710818,16.3016393491872,123.061183039418)) ;
#92572 = CARTESIAN_POINT('Ctrl Pts',(-20.6063783438916,16.3115801722124,123.265604158338)) ;
#92573 = CARTESIAN_POINT('Ctrl Pts',(-20.6136572717799,16.3215847551911,123.475829776473)) ;
#92574 = CARTESIAN_POINT('Ctrl Pts',(-20.5840255669465,16.3316056496358,123.684401378321)) ;
#92575 = CARTESIAN_POINT('Ctrl Pts',(-20.5197138580458,16.3414975702252,123.882172231323)) ;
#92576 = CARTESIAN_POINT('Ctrl Pts',(-20.4213081312752,16.3514910025706,124.067785910372)) ;
#92577 = CARTESIAN_POINT('Ctrl Pts',(-20.2927295521724,16.3614366074705,124.232664564836)) ;
#92578 = CARTESIAN_POINT('Ctrl Pts',(-20.1377257011545,16.371383880952,124.373060345475)) ;
#92579 = CARTESIAN_POINT('Ctrl Pts',(-19.9587972936868,16.3814317954284,124.485325647766)) ;
#92580 = CARTESIAN_POINT('Ctrl Pts',(-19.7670525971543,16.3912794357757,124.563399294681)) ;
#92581 = CARTESIAN_POINT('Ctrl Pts',(-19.5624702538789,16.4012411511523,124.608137599496)) ;
#92582 = CARTESIAN_POINT('Ctrl Pts',(-19.3517882231378,16.4112697747251,124.616465588715)) ;
#92583 = CARTESIAN_POINT('Ctrl Pts',(-19.1453379508177,16.4211801367915,124.588489760527)) ;
#92584 = CARTESIAN_POINT('Ctrl Pts',(-18.9462094865371,16.4311148304439,124.525456505747)) ;
#92585 = CARTESIAN_POINT('Ctrl Pts',(-18.759167106785,16.4411566735718,124.427586025699)) ;
#92586 = CARTESIAN_POINT('Ctrl Pts',(-18.5944416876923,16.4510411791422,124.300871709702)) ;
#92587 = CARTESIAN_POINT('Ctrl Pts',(-18.4524057546357,16.4610432829274,124.145859449179)) ;
#92588 = CARTESIAN_POINT('Ctrl Pts',(-18.3402079875807,16.4709616343424,123.970062250184)) ;
#92589 = CARTESIAN_POINT('Ctrl Pts',(-18.259272916945,16.4810092903633,123.774984953265)) ;
#92590 = CARTESIAN_POINT('Ctrl Pts',(-18.214000026434,16.4908804833915,123.572415370534)) ;
#92591 = CARTESIAN_POINT('Ctrl Pts',(-18.2043727827825,16.500946196535,123.361070103728)) ;
#92592 = CARTESIAN_POINT('Ctrl Pts',(-18.2307852503669,16.5107986571077,123.155574634655)) ;
#92593 = CARTESIAN_POINT('Ctrl Pts',(-18.3149326179074,16.5242271198303,122.886171955467)) ;
#92594 = CARTESIAN_POINT('Ctrl Pts',(-18.4633058127872,16.5373080673473,122.650748595137)) ;
#92595 = CARTESIAN_POINT('Ctrl Pts',(-18.6709271702637,16.5507825655819,122.45819153009)) ;
#92596 = CARTESIAN_POINT('Ctrl Pts',(-18.844772245183,16.5606146691914,122.346294242523)) ;
#92597 = CARTESIAN_POINT('Ctrl Pts',(-19.0376048516113,16.570580572318,122.264442649281)) ;
#92598 = CARTESIAN_POINT('Ctrl Pts',(-19.2431084492467,16.5806079816283,122.217330837706)) ;
#92599 = CARTESIAN_POINT('Ctrl Pts',(-19.4511660916749,16.5905190129948,122.206685716486)) ;
#92600 = CARTESIAN_POINT('Ctrl Pts',(-19.7276789075163,16.6037633206159,122.240089314737)) ;
#92601 = CARTESIAN_POINT('Ctrl Pts',(-20.0569137775014,16.620463803287,122.372795345681)) ;
#92602 = CARTESIAN_POINT('Ctrl Pts',(-20.3183354751437,16.6369706324428,122.607173302249)) ;
#92603 = CARTESIAN_POINT('Ctrl Pts',(-20.4717078563946,16.6502812606804,122.841129281592)) ;
#92604 = CARTESIAN_POINT('Ctrl Pts',(-20.5546945603432,16.6602738242205,123.034165773958)) ;
#92605 = CARTESIAN_POINT('Ctrl Pts',(-20.6028174061506,16.6703039072221,123.239432220823)) ;
#92606 = CARTESIAN_POINT('Ctrl Pts',(-20.6188287734652,16.6834775112198,123.515992234632)) ;
#92607 = CARTESIAN_POINT('Ctrl Pts',(-20.5476980246839,16.7001152164512,123.862375258934)) ;
#92608 = CARTESIAN_POINT('Ctrl Pts',(-20.3266353919911,16.7199969790187,124.222885277575)) ;
#92609 = CARTESIAN_POINT('Ctrl Pts',(-20.0488095001874,16.7366933312352,124.443797374202)) ;
#92610 = CARTESIAN_POINT('Ctrl Pts',(-19.7952425804301,16.7498503590243,124.554332607942)) ;
#92611 = CARTESIAN_POINT('Ctrl Pts',(-19.5219786846243,16.7632277136678,124.620786198231)) ;
#92612 = CARTESIAN_POINT('Ctrl Pts',(-19.1705567065255,16.7797585479266,124.612580136977)) ;
#92613 = CARTESIAN_POINT('Ctrl Pts',(-18.7748001955681,16.7997232376697,124.459120947067)) ;
#92614 = CARTESIAN_POINT('Ctrl Pts',(-18.456169900626,16.8196397310933,124.180166285516)) ;
#92615 = CARTESIAN_POINT('Ctrl Pts',(-18.2513765417998,16.8395294504429,123.810101465255)) ;
#92616 = CARTESIAN_POINT('Ctrl Pts',(-18.1851276829267,16.8595361800907,123.389957374541)) ;
#92617 = CARTESIAN_POINT('Ctrl Pts',(-18.2652600268736,16.8793742337376,122.975738508735)) ;
#92618 = CARTESIAN_POINT('Ctrl Pts',(-18.4831734060332,16.8993675719512,122.610816739563)) ;
#92619 = CARTESIAN_POINT('Ctrl Pts',(-18.811001815802,16.9192503713578,122.343752254667)) ;
#92620 = CARTESIAN_POINT('Ctrl Pts',(-19.2100490940889,16.9391425522766,122.203910312485)) ;
#92621 = CARTESIAN_POINT('Ctrl Pts',(-19.6333307049043,16.9590447307716,122.207929486996)) ;
#92622 = CARTESIAN_POINT('Ctrl Pts',(-20.0320401542686,16.9790820419754,122.357765050694)) ;
#92623 = CARTESIAN_POINT('Ctrl Pts',(-20.3526643510395,16.9988944835162,122.631302217642)) ;
#92624 = CARTESIAN_POINT('Ctrl Pts',(-20.5630417913117,17.0189597242511,123.002232943253)) ;
#92625 = CARTESIAN_POINT('Ctrl Pts',(-20.6335141763589,17.038716929107,123.41657830206)) ;
#92626 = CARTESIAN_POINT('Ctrl Pts',(-20.558006365627,17.0587502017527,123.83557544901)) ;
#92627 = CARTESIAN_POINT('Ctrl Pts',(-20.3461518752294,17.0785631102065,124.199927876101)) ;
#92628 = CARTESIAN_POINT('Ctrl Pts',(-20.0203444599083,17.0985592563339,124.472800792273)) ;
#92629 = CARTESIAN_POINT('Ctrl Pts',(-19.6233799466001,17.1184210095564,124.617465604791)) ;
#92630 = CARTESIAN_POINT('Ctrl Pts',(-19.1967646146023,17.1384895266845,124.617721479536)) ;
#92631 = CARTESIAN_POINT('Ctrl Pts',(-18.8003376032294,17.1583203996814,124.473776890643)) ;
#92632 = CARTESIAN_POINT('Ctrl Pts',(-18.474755985943,17.178242310498,124.202953838831)) ;
#92633 = CARTESIAN_POINT('Ctrl Pts',(-18.2610777094718,17.1981717539333,123.836937803985)) ;
#92634 = CARTESIAN_POINT('Ctrl Pts',(-18.1850738363319,17.2180814240497,123.420547760837)) ;
#92635 = CARTESIAN_POINT('Ctrl Pts',(-18.2548695109545,17.2379547813126,123.003739169527)) ;
#92636 = CARTESIAN_POINT('Ctrl Pts',(-18.4639625203726,17.2579463159305,122.633712831633)) ;
#92637 = CARTESIAN_POINT('Ctrl Pts',(-18.7847202958821,17.2778119333413,122.358779484358)) ;
#92638 = CARTESIAN_POINT('Ctrl Pts',(-19.1821149054444,17.2977928631695,122.208575251661)) ;
#92639 = CARTESIAN_POINT('Ctrl Pts',(-19.6060391887632,17.3177313252526,122.203480342946)) ;
#92640 = CARTESIAN_POINT('Ctrl Pts',(-20.0055818061372,17.3376235184743,122.342419897881)) ;
#92641 = CARTESIAN_POINT('Ctrl Pts',(-20.334784776262,17.3575942335097,122.610483376116)) ;
#92642 = CARTESIAN_POINT('Ctrl Pts',(-20.5517123729197,17.3774039051758,122.971652127387)) ;
#92643 = CARTESIAN_POINT('Ctrl Pts',(-20.6333779841196,17.397397121867,123.38868425828)) ;
#92644 = CARTESIAN_POINT('Ctrl Pts',(-20.5685930892492,17.4172480340634,123.805942383604)) ;
#92645 = CARTESIAN_POINT('Ctrl Pts',(-20.362939525817,17.4373226403824,124.179848021517)) ;
#92646 = CARTESIAN_POINT('Ctrl Pts',(-20.0986114574795,17.4538392722657,124.411232690189)) ;
#92647 = CARTESIAN_POINT('Ctrl Pts',(-19.8472361244034,17.4671779799598,124.535422018461)) ;
#92648 = CARTESIAN_POINT('Ctrl Pts',(-19.648695502256,17.4770203542681,124.59379753623)) ;
#92649 = CARTESIAN_POINT('Ctrl Pts',(-19.4386608921935,17.4870753742509,124.617501313402)) ;
#92650 = CARTESIAN_POINT('Ctrl Pts',(-19.1610336465222,17.5003075309084,124.600234914191)) ;
#92651 = CARTESIAN_POINT('Ctrl Pts',(-18.8258946716868,17.5169224982536,124.488350036976)) ;
#92652 = CARTESIAN_POINT('Ctrl Pts',(-18.5495768861815,17.5335170852648,124.269022343617)) ;
#92653 = CARTESIAN_POINT('Ctrl Pts',(-18.3833597626593,17.5467506536201,124.045859160823)) ;
#92654 = CARTESIAN_POINT('Ctrl Pts',(-18.2885301460445,17.5567942714288,123.857229876977)) ;
#92655 = CARTESIAN_POINT('Ctrl Pts',(-18.2287562532625,17.5666811956636,123.658135390516)) ;
#92656 = CARTESIAN_POINT('Ctrl Pts',(-18.2038373026383,17.5766718501104,123.449600371017)) ;
#92657 = CARTESIAN_POINT('Ctrl Pts',(-18.2155183685981,17.5866336085644,123.240489044656)) ;
#92658 = CARTESIAN_POINT('Ctrl Pts',(-18.279242571354,17.5999734736316,122.967369587735)) ;
#92659 = CARTESIAN_POINT('Ctrl Pts',(-18.4130348186502,17.6132822565449,122.718034113314)) ;
#92660 = CARTESIAN_POINT('Ctrl Pts',(-18.6026066359748,17.626478013989,122.515468739054)) ;
#92661 = CARTESIAN_POINT('Ctrl Pts',(-18.7697373043821,17.6364398976655,122.389261069262)) ;
#92662 = CARTESIAN_POINT('Ctrl Pts',(-18.9579188750606,17.6464830071801,122.293522035345)) ;
#92663 = CARTESIAN_POINT('Ctrl Pts',(-19.1559640195152,17.6563352571794,122.232844539116)) ;
#92664 = CARTESIAN_POINT('Ctrl Pts',(-19.3639322621533,17.6663067941298,122.2066607369)) ;
#92665 = CARTESIAN_POINT('Ctrl Pts',(-19.5738409368387,17.6763020596074,122.217029727047)) ;
#92666 = CARTESIAN_POINT('Ctrl Pts',(-19.779447249497,17.686336032481,122.26411039526)) ;
#92667 = CARTESIAN_POINT('Ctrl Pts',(-19.9704605312748,17.6961914472433,122.344426643971)) ;
#92668 = CARTESIAN_POINT('Ctrl Pts',(-20.1472770617746,17.7061907247522,122.458056115993)) ;
#92669 = CARTESIAN_POINT('Ctrl Pts',(-20.3002748821021,17.7160859089151,122.599059950491)) ;
#92670 = CARTESIAN_POINT('Ctrl Pts',(-20.4285143353315,17.7261462885559,122.767212180967)) ;
#92671 = CARTESIAN_POINT('Ctrl Pts',(-20.5237126912126,17.735996157564,122.951130309144)) ;
#92672 = CARTESIAN_POINT('Ctrl Pts',(-20.5871207120821,17.7460277187719,123.152253498345)) ;
#92673 = CARTESIAN_POINT('Ctrl Pts',(-20.614169464625,17.7560381676542,123.360978680568)) ;
#92674 = CARTESIAN_POINT('Ctrl Pts',(-20.6048963808325,17.7659449070712,123.569036052388)) ;
#92675 = CARTESIAN_POINT('Ctrl Pts',(-20.5598938017532,17.7758829231397,123.773047845721)) ;
#92676 = CARTESIAN_POINT('Ctrl Pts',(-20.4797271625852,17.7858881695908,123.96753801668)) ;
#92677 = CARTESIAN_POINT('Ctrl Pts',(-20.3663978026102,17.7959222306471,124.14544500573)) ;
#92678 = CARTESIAN_POINT('Ctrl Pts',(-20.2268317347825,17.8057673117052,124.298300993795)) ;
#92679 = CARTESIAN_POINT('Ctrl Pts',(-20.0607767182021,17.8157531176587,124.42668993648)) ;
#92680 = CARTESIAN_POINT('Ctrl Pts',(-19.8759066227852,17.8256879382129,124.523963674661)) ;
#92681 = CARTESIAN_POINT('Ctrl Pts',(-19.6745057962594,17.8357454633451,124.588245908723)) ;
#92682 = CARTESIAN_POINT('Ctrl Pts',(-19.4699075152098,17.8455671139965,124.616238143836)) ;
#92683 = CARTESIAN_POINT('Ctrl Pts',(-19.2586565360455,17.8556231775012,124.608486329999)) ;
#92684 = CARTESIAN_POINT('Ctrl Pts',(-19.0543868810221,17.8655638445652,124.564306967429)) ;
#92685 = CARTESIAN_POINT('Ctrl Pts',(-18.8613551760711,17.8754682382312,124.486226474479)) ;
#92686 = CARTESIAN_POINT('Ctrl Pts',(-18.6823712514696,17.8855147619942,124.374127325253)) ;
#92687 = CARTESIAN_POINT('Ctrl Pts',(-18.5277423281328,17.8954108450105,124.234883371212)) ;
#92688 = CARTESIAN_POINT('Ctrl Pts',(-18.3975181430784,17.9054775442406,124.068106619042)) ;
#92689 = CARTESIAN_POINT('Ctrl Pts',(-18.3003841394302,17.9153011546416,123.885816198438)) ;
#92690 = CARTESIAN_POINT('Ctrl Pts',(-18.2345288001946,17.9253570148191,123.684957633441)) ;
#92691 = CARTESIAN_POINT('Ctrl Pts',(-18.2051746045371,17.9352901611241,123.478179415023)) ;
#92692 = CARTESIAN_POINT('Ctrl Pts',(-18.2117492800176,17.9452354168947,123.269226637619)) ;
#92693 = CARTESIAN_POINT('Ctrl Pts',(-18.2545138749042,17.9552187153331,123.063722393022)) ;
#92694 = CARTESIAN_POINT('Ctrl Pts',(-18.332982546595,17.9652558954798,122.867858865701)) ;
#92695 = CARTESIAN_POINT('Ctrl Pts',(-18.4419876923002,17.9751104481892,122.691657865086)) ;
#92696 = CARTESIAN_POINT('Ctrl Pts',(-18.5817046930857,17.9851099666366,122.534632669291)) ;
#92697 = CARTESIAN_POINT('Ctrl Pts',(-18.7447605573555,17.9950050490986,122.405396565275)) ;
#92698 = CARTESIAN_POINT('Ctrl Pts',(-18.9307947177022,18.0050655946047,122.304828643302)) ;
#92699 = CARTESIAN_POINT('Ctrl Pts',(-19.1272549252657,18.0149149018527,122.239367986776)) ;
#92700 = CARTESIAN_POINT('Ctrl Pts',(-19.3356951723123,18.0249419919401,122.207938380922)) ;
#92701 = CARTESIAN_POINT('Ctrl Pts',(-19.5464637005293,18.034970896077,122.213739547083)) ;
#92702 = CARTESIAN_POINT('Ctrl Pts',(-19.7492771163832,18.0448147611763,122.254862768678)) ;
#92703 = CARTESIAN_POINT('Ctrl Pts',(-19.9450396627883,18.0548105878847,122.331265516331)) ;
#92704 = CARTESIAN_POINT('Ctrl Pts',(-20.1248922039138,18.0648358045337,122.441153300508)) ;
#92705 = CARTESIAN_POINT('Ctrl Pts',(-20.2809828150676,18.0747256366913,122.578506474062)) ;
#92706 = CARTESIAN_POINT('Ctrl Pts',(-20.41239798799,18.0847164927761,122.742346642746)) ;
#92707 = CARTESIAN_POINT('Ctrl Pts',(-20.5128750333095,18.0946615873689,122.925697207635)) ;
#92708 = CARTESIAN_POINT('Ctrl Pts',(-20.5804101806714,18.104613491137,123.123726265295)) ;
#92709 = CARTESIAN_POINT('Ctrl Pts',(-20.6126233193585,18.1146498906065,123.332244159599)) ;
#92710 = CARTESIAN_POINT('Ctrl Pts',(-20.6083596579032,18.1245389606951,123.540106535664)) ;
#92711 = CARTESIAN_POINT('Ctrl Pts',(-20.5680335657877,18.134528250066,123.746199619181)) ;
#92712 = CARTESIAN_POINT('Ctrl Pts',(-20.4926226175527,18.1444868162757,123.941500160299)) ;
#92713 = CARTESIAN_POINT('Ctrl Pts',(-20.3855172756073,18.1543863874925,124.119959362233)) ;
#92714 = CARTESIAN_POINT('Ctrl Pts',(-20.2469737795764,18.1644343019068,124.279390768898)) ;
#92715 = CARTESIAN_POINT('Ctrl Pts',(-20.0854054780524,18.1743296447674,124.410486987501)) ;
#92716 = CARTESIAN_POINT('Ctrl Pts',(-19.9005352677414,18.1843913387148,124.513234865981)) ;
#92717 = CARTESIAN_POINT('Ctrl Pts',(-19.7049301084551,18.194235791799,124.580875659365)) ;
#92718 = CARTESIAN_POINT('Ctrl Pts',(-19.4982739713939,18.2041964767574,124.614633529283)) ;
#92719 = CARTESIAN_POINT('Ctrl Pts',(-19.2873016161751,18.2142324092659,124.611621181168)) ;
#92720 = CARTESIAN_POINT('Ctrl Pts',(-19.0830713036951,18.224121024954,124.572810361902)) ;
#92721 = CARTESIAN_POINT('Ctrl Pts',(-18.8860432075107,18.2341354340964,124.498576095596)) ;
#92722 = CARTESIAN_POINT('Ctrl Pts',(-18.7048498609844,18.2441692430542,124.39059329917)) ;
#92723 = CARTESIAN_POINT('Ctrl Pts',(-18.5479908132321,18.2539996973104,124.255995858726)) ;
#92724 = CARTESIAN_POINT('Ctrl Pts',(-18.4135763511044,18.2640773648886,124.092282642532)) ;
#92725 = CARTESIAN_POINT('Ctrl Pts',(-18.3118235018209,18.2739292330109,123.911832242753)) ;
#92726 = CARTESIAN_POINT('Ctrl Pts',(-18.2412636867744,18.2840022705762,123.712204349942)) ;
#92727 = CARTESIAN_POINT('Ctrl Pts',(-18.2072562031298,18.2938448239271,123.508079054221)) ;
#92728 = CARTESIAN_POINT('Ctrl Pts',(-18.2085295943525,18.3038252194205,123.298272684557)) ;
#92729 = CARTESIAN_POINT('Ctrl Pts',(-18.2467612388088,18.3138436973983,123.091156447569)) ;
#92730 = CARTESIAN_POINT('Ctrl Pts',(-18.3189753705069,18.3237270117044,122.8963045179)) ;
#92731 = CARTESIAN_POINT('Ctrl Pts',(-18.4259403030239,18.3337953142431,122.713693116947)) ;
#92732 = CARTESIAN_POINT('Ctrl Pts',(-18.5596026738779,18.3436253615166,122.556032941135)) ;
#92733 = CARTESIAN_POINT('Ctrl Pts',(-18.7222139779359,18.3536922329321,122.420633676743)) ;
#92734 = CARTESIAN_POINT('Ctrl Pts',(-18.9027321027321,18.3635812717311,122.317447011611)) ;
#92735 = CARTESIAN_POINT('Ctrl Pts',(-19.1003668831419,18.3735779698652,122.246036932868)) ;
#92736 = CARTESIAN_POINT('Ctrl Pts',(-19.3065323749865,18.3835303955772,122.210267849344)) ;
#92737 = CARTESIAN_POINT('Ctrl Pts',(-19.5155137773644,18.3934716978101,122.210548411513)) ;
#92738 = CARTESIAN_POINT('Ctrl Pts',(-19.7222189729129,18.4034549368941,122.247050235139)) ;
#92739 = CARTESIAN_POINT('Ctrl Pts',(-19.9203917704967,18.4134937384627,122.319582320814)) ;
#92740 = CARTESIAN_POINT('Ctrl Pts',(-20.0997259303789,18.4233418445843,122.423079545611)) ;
#92741 = CARTESIAN_POINT('Ctrl Pts',(-20.2618814150769,18.4334020401596,122.558833845978)) ;
#92742 = CARTESIAN_POINT('Ctrl Pts',(-20.3956744568318,18.4432997234711,122.718208693815)) ;
#92743 = CARTESIAN_POINT('Ctrl Pts',(-20.5006998407244,18.453230763845,122.898646677112)) ;
#92744 = CARTESIAN_POINT('Ctrl Pts',(-20.5733935717876,18.4632729815016,123.096852667896)) ;
#92745 = CARTESIAN_POINT('Ctrl Pts',(-20.6101416798205,18.4731596422356,123.301436558527)) ;
#92746 = CARTESIAN_POINT('Ctrl Pts',(-20.6111685275753,18.4831527508381,123.511509867575)) ;
#92747 = CARTESIAN_POINT('Ctrl Pts',(-20.5757926440106,18.4930984494763,123.717585350536)) ;
#92748 = CARTESIAN_POINT('Ctrl Pts',(-20.5055613986537,18.5030456717474,123.914572326248)) ;
#92749 = CARTESIAN_POINT('Ctrl Pts',(-20.4009471294435,18.5130936973275,124.098082350297)) ;
#92750 = CARTESIAN_POINT('Ctrl Pts',(-20.2688858815582,18.5229409444704,124.257508846386)) ;
#92751 = CARTESIAN_POINT('Ctrl Pts',(-20.1097243873236,18.5329041215612,124.39366353997)) ;
#92752 = CARTESIAN_POINT('Ctrl Pts',(-19.9279709104709,18.5429338425946,124.500552449565)) ;
#92753 = CARTESIAN_POINT('Ctrl Pts',(-19.7329558518841,18.5528383101275,124.573584975196)) ;
#92754 = CARTESIAN_POINT('Ctrl Pts',(-19.5257968398549,18.5628627959572,124.612170958543)) ;
#92755 = CARTESIAN_POINT('Ctrl Pts',(-19.3175695775789,18.5727666310811,124.614349950138)) ;
#92756 = CARTESIAN_POINT('Ctrl Pts',(-19.1091146716,18.5828178217911,124.579889396335)) ;
#92757 = CARTESIAN_POINT('Ctrl Pts',(-18.9130619976657,18.5927022644494,124.510943603526)) ;
#92758 = CARTESIAN_POINT('Ctrl Pts',(-18.7298124080229,18.6026952723013,124.408243913293)) ;
#92759 = CARTESIAN_POINT('Ctrl Pts',(-18.5679260386757,18.6126435920176,124.275805094592)) ;
#92760 = CARTESIAN_POINT('Ctrl Pts',(-18.4314461503668,18.622580430727,124.117671389572)) ;
#92761 = CARTESIAN_POINT('Ctrl Pts',(-18.3237491434459,18.6325634196466,123.937505549307)) ;
#92762 = CARTESIAN_POINT('Ctrl Pts',(-18.2488966463023,18.6426072990107,123.740090399413)) ;
#92763 = CARTESIAN_POINT('Ctrl Pts',(-18.209813068051,18.6524353643691,123.537170757403)) ;
#92764 = CARTESIAN_POINT('Ctrl Pts',(-18.206385155789,18.6625124529241,123.325393218201)) ;
#92765 = CARTESIAN_POINT('Ctrl Pts',(-18.238909571519,18.6723626050803,123.120828018811)) ;
#92766 = CARTESIAN_POINT('Ctrl Pts',(-18.3079228948117,18.6824430855327,122.920512684699)) ;
#92767 = CARTESIAN_POINT('Ctrl Pts',(-18.4078474591112,18.6922575833015,122.739938990814)) ;
#92768 = CARTESIAN_POINT('Ctrl Pts',(-18.540643272446,18.7023258793217,122.575174082538)) ;
#92769 = CARTESIAN_POINT('Ctrl Pts',(-18.6974620081295,18.7122247118044,122.438290139689)) ;
#92770 = CARTESIAN_POINT('Ctrl Pts',(-18.8783200201035,18.722277591819,122.329027980495)) ;
#92771 = CARTESIAN_POINT('Ctrl Pts',(-19.071821712519,18.7321474073151,122.254003571519)) ;
#92772 = CARTESIAN_POINT('Ctrl Pts',(-19.2795064905227,18.7422200883979,122.212846727025)) ;
#92773 = CARTESIAN_POINT('Ctrl Pts',(-19.4861884068662,18.7520525669689,122.208399678899)) ;
#92774 = CARTESIAN_POINT('Ctrl Pts',(-19.6946842005538,18.762083200955,122.239936671409)) ;
#92775 = CARTESIAN_POINT('Ctrl Pts',(-19.8943770937063,18.7721147581741,122.307793552659)) ;
#92776 = CARTESIAN_POINT('Ctrl Pts',(-20.0757189680045,18.7819444670458,122.406859087493)) ;
#92777 = CARTESIAN_POINT('Ctrl Pts',(-20.240134989661,18.7919339158479,122.537526730082)) ;
#92778 = CARTESIAN_POINT('Ctrl Pts',(-20.3797167170314,18.801977768248,122.695962331067)) ;
#92779 = CARTESIAN_POINT('Ctrl Pts',(-20.4876019724467,18.81179948158,122.872018741494)) ;
#92780 = CARTESIAN_POINT('Ctrl Pts',(-20.5654043884981,18.8218344865687,123.068115037575)) ;
#92781 = CARTESIAN_POINT('Ctrl Pts',(-20.6073616902904,18.8318593250163,123.274657332635)) ;
#92782 = CARTESIAN_POINT('Ctrl Pts',(-20.6131682480769,18.8417115379715,123.481700357491)) ;
#92783 = CARTESIAN_POINT('Ctrl Pts',(-20.5828695031209,18.8517014941653,123.689507408445)) ;
#92784 = CARTESIAN_POINT('Ctrl Pts',(-20.5173663478567,18.8616296044486,123.887689661944)) ;
#92785 = CARTESIAN_POINT('Ctrl Pts',(-20.4181397973166,18.8716182045281,124.072765157157)) ;
#92786 = CARTESIAN_POINT('Ctrl Pts',(-20.287563655019,18.8816447964556,124.238246495347)) ;
#92787 = CARTESIAN_POINT('Ctrl Pts',(-20.1326099286412,18.8915299245198,124.376719376746)) ;
#92788 = CARTESIAN_POINT('Ctrl Pts',(-19.9543134225387,18.9015210419933,124.487770822266)) ;
#92789 = CARTESIAN_POINT('Ctrl Pts',(-19.7583197977327,18.9115616578451,124.566149255982)) ;
#92790 = CARTESIAN_POINT('Ctrl Pts',(-19.5560396588162,18.9213946486988,124.608747665617)) ;
#92791 = CARTESIAN_POINT('Ctrl Pts',(-19.3460913770336,18.9313877801491,124.616289970544)) ;
#92792 = CARTESIAN_POINT('Ctrl Pts',(-19.1372600770967,18.9414198285845,124.586714093607)) ;
#92793 = CARTESIAN_POINT('Ctrl Pts',(-18.9400108926563,18.9512850751269,124.522664185328)) ;
#92794 = CARTESIAN_POINT('Ctrl Pts',(-18.7547919702159,18.9612469499537,124.424901736679)) ;
#92795 = CARTESIAN_POINT('Ctrl Pts',(-18.5883738302612,18.971281913065,124.2952601066)) ;
#92796 = CARTESIAN_POINT('Ctrl Pts',(-18.448819046263,18.9811667575274,124.141239790597)) ;
#92797 = CARTESIAN_POINT('Ctrl Pts',(-18.3361799499564,18.9912328103682,123.962131075838)) ;
#92798 = CARTESIAN_POINT('Ctrl Pts',(-18.257920565973,19.0010703262771,123.770652739752)) ;
#92799 = CARTESIAN_POINT('Ctrl Pts',(-18.2128628976887,19.011139074386,123.563864375363)) ;
#92800 = CARTESIAN_POINT('Ctrl Pts',(-18.2046274740072,19.021019591417,123.35627632858)) ;
#92801 = CARTESIAN_POINT('Ctrl Pts',(-18.2324438398586,19.0310107783515,123.14811114272)) ;
#92802 = CARTESIAN_POINT('Ctrl Pts',(-18.2957268717079,19.0409638446264,122.948631979712)) ;
#92803 = CARTESIAN_POINT('Ctrl Pts',(-18.3935294235557,19.050999682159,122.761704016059)) ;
#92804 = CARTESIAN_POINT('Ctrl Pts',(-18.5203397037647,19.0608898083705,122.596912724645)) ;
#92805 = CARTESIAN_POINT('Ctrl Pts',(-18.6751751381442,19.0708819902784,122.454963144696)) ;
#92806 = CARTESIAN_POINT('Ctrl Pts',(-18.8515331380732,19.080827930217,122.342630525861)) ;
#92807 = CARTESIAN_POINT('Ctrl Pts',(-19.0445885349267,19.0907751139811,122.262219655988)) ;
#92808 = CARTESIAN_POINT('Ctrl Pts',(-19.2507744154612,19.1008230522886,122.2163232578)) ;
#92809 = CARTESIAN_POINT('Ctrl Pts',(-19.4575916342668,19.1106706870288,122.206936574544)) ;
#92810 = CARTESIAN_POINT('Ctrl Pts',(-19.6653476661059,19.1206324010027,122.233259211876)) ;
#92811 = CARTESIAN_POINT('Ctrl Pts',(-19.8666639016408,19.1306610357935,122.29593385509)) ;
#92812 = CARTESIAN_POINT('Ctrl Pts',(-20.051840008439,19.1405713543906,122.391400489081)) ;
#92813 = CARTESIAN_POINT('Ctrl Pts',(-20.2183835287999,19.1505062107021,122.517455364573)) ;
#92814 = CARTESIAN_POINT('Ctrl Pts',(-20.3618707267679,19.1605474466628,122.672277305996)) ;
#92815 = CARTESIAN_POINT('Ctrl Pts',(-20.4746969685949,19.1704342182428,122.84686466971)) ;
#92816 = CARTESIAN_POINT('Ctrl Pts',(-20.5566359490332,19.180434396949,123.040441287818)) ;
#92817 = CARTESIAN_POINT('Ctrl Pts',(-20.6035192128641,19.1903516751586,123.243629824238)) ;
#92818 = CARTESIAN_POINT('Ctrl Pts',(-20.6144848714803,19.2003989215723,123.45454051426)) ;
#92819 = CARTESIAN_POINT('Ctrl Pts',(-20.5893212820512,19.2102728105536,123.66062268631)) ;
#92820 = CARTESIAN_POINT('Ctrl Pts',(-20.5277315285585,19.2203348281341,123.862966148539)) ;
#92821 = CARTESIAN_POINT('Ctrl Pts',(-20.4337173847183,19.2302058898684,124.047986049992)) ;
#92822 = CARTESIAN_POINT('Ctrl Pts',(-20.3079299377085,19.2401999532287,124.216278219142)) ;
#92823 = CARTESIAN_POINT('Ctrl Pts',(-20.1539324571469,19.2502321112621,124.360376363104)) ;
#92824 = CARTESIAN_POINT('Ctrl Pts',(-19.9804428304959,19.2600959875023,124.474010306699)) ;
#92825 = CARTESIAN_POINT('Ctrl Pts',(-19.785918102539,19.2701665021406,124.557511631259)) ;
#92826 = CARTESIAN_POINT('Ctrl Pts',(-19.5845187324554,19.2800071390815,124.604891315488)) ;
#92827 = CARTESIAN_POINT('Ctrl Pts',(-19.3753707846235,19.2899742679217,124.617420940457)) ;
#92828 = CARTESIAN_POINT('Ctrl Pts',(-19.166242834232,19.2999882410463,124.593109638195)) ;
#92829 = CARTESIAN_POINT('Ctrl Pts',(-18.8985887014101,19.3132729749095,124.51325325629)) ;
#92830 = CARTESIAN_POINT('Ctrl Pts',(-18.6588871766436,19.3264982396243,124.366249593857)) ;
#92831 = CARTESIAN_POINT('Ctrl Pts',(-18.4660700120822,19.3398087621792,124.163476304628)) ;
#92832 = CARTESIAN_POINT('Ctrl Pts',(-18.3496595368789,19.3498374070813,123.987691601634)) ;
#92833 = CARTESIAN_POINT('Ctrl Pts',(-18.2666103013183,19.3597184394352,123.797281986948)) ;
#92834 = CARTESIAN_POINT('Ctrl Pts',(-18.2169671242081,19.3696994121153,123.59340792941)) ;
#92835 = CARTESIAN_POINT('Ctrl Pts',(-18.2036560598774,19.3796805397013,123.384012285161)) ;
#92836 = CARTESIAN_POINT('Ctrl Pts',(-18.2339327119865,19.3929237299627,123.107171028627)) ;
#92837 = CARTESIAN_POINT('Ctrl Pts',(-18.3623905823458,19.4095917253235,122.776996485116)) ;
#92838 = CARTESIAN_POINT('Ctrl Pts',(-18.5937075244846,19.4261122253356,122.512484155667)) ;
#92839 = CARTESIAN_POINT('Ctrl Pts',(-18.8258991005238,19.4394252416516,122.356364000433)) ;
#92840 = CARTESIAN_POINT('Ctrl Pts',(-19.0164084985625,19.4493417998846,122.271584814231)) ;
#92841 = CARTESIAN_POINT('Ctrl Pts',(-19.220935191191,19.4593694681874,122.220706883488)) ;
#92842 = CARTESIAN_POINT('Ctrl Pts',(-19.4974374171098,19.4725500579321,122.20084547395)) ;
#92843 = CARTESIAN_POINT('Ctrl Pts',(-19.8469033690404,19.4892981970515,122.268339913805)) ;
#92844 = CARTESIAN_POINT('Ctrl Pts',(-20.2084084568038,19.509092939562,122.484283598971)) ;
#92845 = CARTESIAN_POINT('Ctrl Pts',(-20.4779908515016,19.5291373323708,122.814197913215)) ;
#92846 = CARTESIAN_POINT('Ctrl Pts',(-20.6171058529899,19.5489765146695,123.21255429909)) ;
#92847 = CARTESIAN_POINT('Ctrl Pts',(-20.612955760874,19.5689018383624,123.636097734435)) ;
#92848 = CARTESIAN_POINT('Ctrl Pts',(-20.464422625464,19.5888254764139,124.032909263132)) ;
#92849 = CARTESIAN_POINT('Ctrl Pts',(-20.1895544218666,19.6087503498795,124.355231271546)) ;
#92850 = CARTESIAN_POINT('Ctrl Pts',(-19.8222577775006,19.6286289569584,124.564437287591)) ;
#92851 = CARTESIAN_POINT('Ctrl Pts',(-19.4036149738155,19.6486063997904,124.636299304902)) ;
#92852 = CARTESIAN_POINT('Ctrl Pts',(-18.9865388828078,19.668538247875,124.560857265651)) ;
#92853 = CARTESIAN_POINT('Ctrl Pts',(-18.6207629984845,19.6884335162176,124.348399195064)) ;
#92854 = CARTESIAN_POINT('Ctrl Pts',(-18.3486870513789,19.7083560146297,124.023705471699)) ;
#92855 = CARTESIAN_POINT('Ctrl Pts',(-18.2035743919588,19.7283154965057,123.624866853166)) ;
#92856 = CARTESIAN_POINT('Ctrl Pts',(-18.2031996570763,19.7481932489651,123.202277382126)) ;
#92857 = CARTESIAN_POINT('Ctrl Pts',(-18.3460020872728,19.7680750396997,122.804297775666)) ;
#92858 = CARTESIAN_POINT('Ctrl Pts',(-18.6192054318381,19.7881483785506,122.476459335084)) ;
#92859 = CARTESIAN_POINT('Ctrl Pts',(-18.9830159386754,19.8079528457864,122.264237742757)) ;
#92860 = CARTESIAN_POINT('Ctrl Pts',(-19.4008365480292,19.8279361861942,122.187322330753)) ;
#92861 = CARTESIAN_POINT('Ctrl Pts',(-19.8183361695826,19.8478511507922,122.258043599631)) ;
#92862 = CARTESIAN_POINT('Ctrl Pts',(-20.1864345402117,19.8677196855086,122.465512844636)) ;
#92863 = CARTESIAN_POINT('Ctrl Pts',(-20.4635252854284,19.8877720697203,122.789401568453)) ;
#92864 = CARTESIAN_POINT('Ctrl Pts',(-20.6120084940387,19.9075460335095,123.182939631322)) ;
#92865 = CARTESIAN_POINT('Ctrl Pts',(-20.6176871989571,19.9276004125309,123.609141307482)) ;
#92866 = CARTESIAN_POINT('Ctrl Pts',(-20.4791319038262,19.9473971501041,124.006748510168)) ;
#92867 = CARTESIAN_POINT('Ctrl Pts',(-20.2119683630544,19.9673649624556,124.336599946701)) ;
#92868 = CARTESIAN_POINT('Ctrl Pts',(-19.8479480211113,19.9873239385206,124.554908158912)) ;
#92869 = CARTESIAN_POINT('Ctrl Pts',(-19.43276586831,20.007218856798,124.63587693085)) ;
#92870 = CARTESIAN_POINT('Ctrl Pts',(-19.0147876330479,20.0271151692483,124.57082106987)) ;
#92871 = CARTESIAN_POINT('Ctrl Pts',(-18.6435959232996,20.0470231026225,124.3672967635)) ;
#92872 = CARTESIAN_POINT('Ctrl Pts',(-18.3636276541747,20.0669729929109,124.048670462292)) ;
#92873 = CARTESIAN_POINT('Ctrl Pts',(-18.2093280448244,20.0868502234122,123.655155528142)) ;
#92874 = CARTESIAN_POINT('Ctrl Pts',(-18.1983048045241,20.1068328922832,123.230434038346)) ;
#92875 = CARTESIAN_POINT('Ctrl Pts',(-18.3328374001003,20.1267657788636,122.828470876827)) ;
#92876 = CARTESIAN_POINT('Ctrl Pts',(-18.5959298858172,20.1466785248815,122.496768303889)) ;
#92877 = CARTESIAN_POINT('Ctrl Pts',(-18.8956764765838,20.1632482462234,122.311681543742)) ;
#92878 = CARTESIAN_POINT('Ctrl Pts',(-19.1634853725372,20.1765482575283,122.231185626866)) ;
#92879 = CARTESIAN_POINT('Ctrl Pts',(-19.4404546659707,20.1898184452782,122.19809994678)) ;
#92880 = CARTESIAN_POINT('Ctrl Pts',(-19.7904976855071,20.2064458276436,122.24823930975)) ;
#92881 = CARTESIAN_POINT('Ctrl Pts',(-20.1021495885334,20.2230681173888,122.414851945115)) ;
#92882 = CARTESIAN_POINT('Ctrl Pts',(-20.3055386175486,20.2363133317834,122.605073534047)) ;
#92883 = CARTESIAN_POINT('Ctrl Pts',(-20.4311937960424,20.246225296744,122.771317113162)) ;
#92884 = CARTESIAN_POINT('Ctrl Pts',(-20.5272487078393,20.2562839199085,122.959681452955)) ;
#92885 = CARTESIAN_POINT('Ctrl Pts',(-20.5881006030648,20.2661240340243,123.157431331348)) ;
#92886 = CARTESIAN_POINT('Ctrl Pts',(-20.6144821807902,20.2761898189819,123.367363495084)) ;
#92887 = CARTESIAN_POINT('Ctrl Pts',(-20.6041090142429,20.2860731367698,123.574910063301)) ;
#92888 = CARTESIAN_POINT('Ctrl Pts',(-20.5578169059943,20.2960625746284,123.779732855571)) ;
#92889 = CARTESIAN_POINT('Ctrl Pts',(-20.4767917203888,20.3060262886811,123.972907200865)) ;
#92890 = CARTESIAN_POINT('Ctrl Pts',(-20.3632827563932,20.3160213003403,124.149756073502)) ;
#92891 = CARTESIAN_POINT('Ctrl Pts',(-20.2199777193418,20.3260575920346,124.304604687197)) ;
#92892 = CARTESIAN_POINT('Ctrl Pts',(-20.0553288039776,20.335903969728,124.43008623397)) ;
#92893 = CARTESIAN_POINT('Ctrl Pts',(-19.8690271796921,20.3458889138787,124.526746895698)) ;
#92894 = CARTESIAN_POINT('Ctrl Pts',(-19.6697103347289,20.3558258850087,124.589424862788)) ;
#92895 = CARTESIAN_POINT('Ctrl Pts',(-19.4602253129189,20.3658756696404,124.616732470545)) ;
#92896 = CARTESIAN_POINT('Ctrl Pts',(-19.2533240604051,20.3757261317179,124.60759574013)) ;
#92897 = CARTESIAN_POINT('Ctrl Pts',(-19.0485801942449,20.3856981452383,124.5626614221)) ;
#92898 = CARTESIAN_POINT('Ctrl Pts',(-18.8542534156056,20.3956932923577,124.482625679858)) ;
#92899 = CARTESIAN_POINT('Ctrl Pts',(-18.6762666665279,20.4057272620938,124.369439159579)) ;
#92900 = CARTESIAN_POINT('Ctrl Pts',(-18.5231567827763,20.4155828077644,124.229814805404)) ;
#92901 = CARTESIAN_POINT('Ctrl Pts',(-18.3945758011845,20.4255815647777,124.063565077421)) ;
#92902 = CARTESIAN_POINT('Ctrl Pts',(-18.2976014683267,20.4354787000148,123.879441178517)) ;
#92903 = CARTESIAN_POINT('Ctrl Pts',(-18.2330490446719,20.4455317958545,123.678215667784)) ;
#92904 = CARTESIAN_POINT('Ctrl Pts',(-18.2048744098774,20.4554153045851,123.472337909635)) ;
#92905 = CARTESIAN_POINT('Ctrl Pts',(-18.2124727941934,20.4654101772312,123.262357966266)) ;
#92906 = CARTESIAN_POINT('Ctrl Pts',(-18.2568500139879,20.4754301388669,123.05642219874)) ;
#92907 = CARTESIAN_POINT('Ctrl Pts',(-18.3352337516257,20.4853355026667,122.863498934385)) ;
#92908 = CARTESIAN_POINT('Ctrl Pts',(-18.4459506926061,20.4952760902742,122.686271473277)) ;
#92909 = CARTESIAN_POINT('Ctrl Pts',(-18.5865698044583,20.5052789083749,122.529879028359)) ;
#92910 = CARTESIAN_POINT('Ctrl Pts',(-18.7529194278954,20.515313620099,122.400158061147)) ;
#92911 = CARTESIAN_POINT('Ctrl Pts',(-18.9355983775793,20.5251585268363,122.302840174493)) ;
#92912 = CARTESIAN_POINT('Ctrl Pts',(-19.1350505969826,20.5351443794053,122.237440607211)) ;
#92913 = CARTESIAN_POINT('Ctrl Pts',(-19.341816666676,20.5450791878184,122.207660399939)) ;
#92914 = CARTESIAN_POINT('Ctrl Pts',(-19.5531166856646,20.5551367148994,122.214501577073)) ;
#92915 = CARTESIAN_POINT('Ctrl Pts',(-19.7552823842387,20.5649583698965,122.25660977831)) ;
#92916 = CARTESIAN_POINT('Ctrl Pts',(-19.9517518356033,20.5750144140696,122.334626537221)) ;
#92917 = CARTESIAN_POINT('Ctrl Pts',(-20.129451145617,20.5849551541147,122.444634049195)) ;
#92918 = CARTESIAN_POINT('Ctrl Pts',(-20.2852058385497,20.5948592751876,122.582819934933)) ;
#92919 = CARTESIAN_POINT('Ctrl Pts',(-20.4163627074734,20.6049068163418,122.748380027418)) ;
#92920 = CARTESIAN_POINT('Ctrl Pts',(-20.5154483150305,20.6148055679422,122.931410766274)) ;
#92921 = CARTESIAN_POINT('Ctrl Pts',(-20.5823151997651,20.624854046908,123.131775210439)) ;
#92922 = CARTESIAN_POINT('Ctrl Pts',(-20.6129012294485,20.6347415439918,123.337400833468)) ;
#92923 = CARTESIAN_POINT('Ctrl Pts',(-20.6076505390634,20.6447346342898,123.547403029367)) ;
#92924 = CARTESIAN_POINT('Ctrl Pts',(-20.5661097282757,20.6546868043501,123.752476414149)) ;
#92925 = CARTESIAN_POINT('Ctrl Pts',(-20.4899748034318,20.6646252242646,123.947032280125)) ;
#92926 = CARTESIAN_POINT('Ctrl Pts',(-20.3808873625602,20.6746103543502,124.126405169006)) ;
#92927 = CARTESIAN_POINT('Ctrl Pts',(-20.2413837782578,20.6846470437643,124.284693812174)) ;
#92928 = CARTESIAN_POINT('Ctrl Pts',(-20.079686612651,20.6945017277568,124.414245628095)) ;
#92929 = CARTESIAN_POINT('Ctrl Pts',(-19.8954680780183,20.7045012118047,124.515444101744)) ;
#92930 = CARTESIAN_POINT('Ctrl Pts',(-19.6985589528749,20.7143963005816,124.582645265439)) ;
#92931 = CARTESIAN_POINT('Ctrl Pts',(-19.4895929944476,20.7244568552277,124.615139995607)) ;
#92932 = CARTESIAN_POINT('Ctrl Pts',(-19.2825548327521,20.7343061196006,124.611063575598)) ;
#92933 = CARTESIAN_POINT('Ctrl Pts',(-19.075615702001,20.7443333720484,124.57090628253)) ;
#92934 = CARTESIAN_POINT('Ctrl Pts',(-18.8789572197511,20.7543616696186,124.494897181618)) ;
#92935 = CARTESIAN_POINT('Ctrl Pts',(-18.7015724822061,20.7642077986246,124.38822692672)) ;
#92936 = CARTESIAN_POINT('Ctrl Pts',(-18.5427085218804,20.7742017039867,124.250730190685)) ;
#92937 = CARTESIAN_POINT('Ctrl Pts',(-18.4100202997382,20.7842258016697,124.087002462897)) ;
#92938 = CARTESIAN_POINT('Ctrl Pts',(-18.3089182753878,20.7941156295238,123.905320005835)) ;
#92939 = CARTESIAN_POINT('Ctrl Pts',(-18.2399098922842,20.8041076109542,123.706924571269)) ;
#92940 = CARTESIAN_POINT('Ctrl Pts',(-18.2065962288079,20.81405461572,123.500477659669)) ;
#92941 = CARTESIAN_POINT('Ctrl Pts',(-18.2092510420346,20.8240042671098,123.291312990658)) ;
#92942 = CARTESIAN_POINT('Ctrl Pts',(-18.2486917521182,20.8340412700872,123.084028440035)) ;
#92943 = CARTESIAN_POINT('Ctrl Pts',(-18.3222881522907,20.8439301785222,122.889587486507)) ;
#92944 = CARTESIAN_POINT('Ctrl Pts',(-18.4292737419995,20.8539195109997,122.708880730536)) ;
#92945 = CARTESIAN_POINT('Ctrl Pts',(-18.5657078577571,20.8638780664368,122.550089103636)) ;
#92946 = CARTESIAN_POINT('Ctrl Pts',(-18.7263705662023,20.8737776376373,122.417776084193)) ;
#92947 = CARTESIAN_POINT('Ctrl Pts',(-18.9102889662095,20.8838255628893,122.313916753173)) ;
#92948 = CARTESIAN_POINT('Ctrl Pts',(-19.106418162168,20.8937208624153,122.244464761771)) ;
#92949 = CARTESIAN_POINT('Ctrl Pts',(-19.3150200502788,20.9037827188633,122.20952718984)) ;
#92950 = CARTESIAN_POINT('Ctrl Pts',(-19.5219709300208,20.9136265652799,122.211259221192)) ;
#92951 = CARTESIAN_POINT('Ctrl Pts',(-19.7280504585221,20.923589514408,122.248639607825)) ;
#92952 = CARTESIAN_POINT('Ctrl Pts',(-19.9258060260669,20.933623550836,122.322083785571)) ;
#92953 = CARTESIAN_POINT('Ctrl Pts',(-20.1052484445707,20.943510977794,122.426997611352)) ;
#92954 = CARTESIAN_POINT('Ctrl Pts',(-20.2660567174591,20.9535254121304,122.562908261672)) ;
#92955 = CARTESIAN_POINT('Ctrl Pts',(-20.4006745637189,20.9635603567653,122.725323843914)) ;
#92956 = CARTESIAN_POINT('Ctrl Pts',(-20.5034505527534,20.9733927067963,122.904697980723)) ;
#92957 = CARTESIAN_POINT('Ctrl Pts',(-20.5752878262504,20.9834681459136,123.103919059865)) ;
#92958 = CARTESIAN_POINT('Ctrl Pts',(-20.6107746352119,20.9933206111482,123.308030768185)) ;
#92959 = CARTESIAN_POINT('Ctrl Pts',(-20.6104406120429,21.003393488725,123.519758493893)) ;
#92960 = CARTESIAN_POINT('Ctrl Pts',(-20.574159530213,21.0132360849175,123.723492672765)) ;
#92961 = CARTESIAN_POINT('Ctrl Pts',(-20.5027305980759,21.0232164690328,123.920769582225)) ;
#92962 = CARTESIAN_POINT('Ctrl Pts',(-20.3973760508536,21.0332349496816,124.103140675449)) ;
#92963 = CARTESIAN_POINT('Ctrl Pts',(-20.2641044963282,21.043118264682,124.262579969479)) ;
#92964 = CARTESIAN_POINT('Ctrl Pts',(-20.1021843516698,21.0531865617724,124.39885224005)) ;
#92965 = CARTESIAN_POINT('Ctrl Pts',(-19.9234578857869,21.0630166301447,124.502677746142)) ;
#92966 = CARTESIAN_POINT('Ctrl Pts',(-19.7249073728143,21.0730834226131,124.575830404009)) ;
#92967 = CARTESIAN_POINT('Ctrl Pts',(-19.5202526014126,21.0829727561017,124.612656971211)) ;
#92968 = CARTESIAN_POINT('Ctrl Pts',(-19.3100164219051,21.0929748875177,124.613728177772)) ;
#92969 = CARTESIAN_POINT('Ctrl Pts',(-19.104313532682,21.1028987571387,124.578676687678)) ;
#92970 = CARTESIAN_POINT('Ctrl Pts',(-18.9055379818956,21.1129422726559,124.507558469863)) ;
#92971 = CARTESIAN_POINT('Ctrl Pts',(-18.7248962749074,21.1228244855442,124.404861360721)) ;
#92972 = CARTESIAN_POINT('Ctrl Pts',(-18.5618819563526,21.1328925627636,124.269913203078)) ;
#92973 = CARTESIAN_POINT('Ctrl Pts',(-18.4277131905557,21.1427310674978,124.112452222884)) ;
#92974 = CARTESIAN_POINT('Ctrl Pts',(-18.3203059258031,21.1527938359272,123.930225142098)) ;
#92975 = CARTESIAN_POINT('Ctrl Pts',(-18.2475914361445,21.16269082921,123.735266093475)) ;
#92976 = CARTESIAN_POINT('Ctrl Pts',(-18.2090196056802,21.1726220568447,123.53007978399)) ;
#92977 = CARTESIAN_POINT('Ctrl Pts',(-18.206865902174,21.1826642154869,123.318975246632)) ;
#92978 = CARTESIAN_POINT('Ctrl Pts',(-18.2407188874795,21.1925509250179,123.113892030568)) ;
#92979 = CARTESIAN_POINT('Ctrl Pts',(-18.31006688254,21.2025438974465,122.915594107731)) ;
#92980 = CARTESIAN_POINT('Ctrl Pts',(-18.4123920866279,21.2124900919831,122.733245377864)) ;
#92981 = CARTESIAN_POINT('Ctrl Pts',(-18.5444723439432,21.2224354668346,122.571139731623)) ;
#92982 = CARTESIAN_POINT('Ctrl Pts',(-18.7046180314311,21.2324903861945,122.433199211354)) ;
#92983 = CARTESIAN_POINT('Ctrl Pts',(-18.8819052194526,21.242311905638,122.32730255838)) ;
#92984 = CARTESIAN_POINT('Ctrl Pts',(-19.0795341225873,21.2523776744049,122.251751654709)) ;
#92985 = CARTESIAN_POINT('Ctrl Pts',(-19.2839833999298,21.26227959606,122.21237155369)) ;
#92986 = CARTESIAN_POINT('Ctrl Pts',(-19.4950720949198,21.272322654881,122.208856213682)) ;
#92987 = CARTESIAN_POINT('Ctrl Pts',(-19.7007256999796,21.2822286489237,122.241706218892)) ;
#92988 = CARTESIAN_POINT('Ctrl Pts',(-19.8983768064677,21.2921664220055,122.309400713787)) ;
#92989 = CARTESIAN_POINT('Ctrl Pts',(-20.0830478736539,21.3022067857378,122.411625288748)) ;
#92990 = CARTESIAN_POINT('Ctrl Pts',(-20.2447725390836,21.3120941294613,122.542225491342)) ;
#92991 = CARTESIAN_POINT('Ctrl Pts',(-20.3830581645172,21.32208636003,122.700338499816)) ;
#92992 = CARTESIAN_POINT('Ctrl Pts',(-20.4912786799857,21.3320348878136,122.879326370199)) ;
#92993 = CARTESIAN_POINT('Ctrl Pts',(-20.5669519562482,21.3419716715369,123.074021933852)) ;
#92994 = CARTESIAN_POINT('Ctrl Pts',(-20.6081294035069,21.3519546723339,123.27984423291)) ;
#92995 = CARTESIAN_POINT('Ctrl Pts',(-20.612582513455,21.3619985591746,123.490926845496)) ;
#92996 = CARTESIAN_POINT('Ctrl Pts',(-20.5814885242902,21.3718265827492,123.695222667967)) ;
#92997 = CARTESIAN_POINT('Ctrl Pts',(-20.5138274751525,21.3819038309628,123.895933159285)) ;
#92998 = CARTESIAN_POINT('Ctrl Pts',(-20.4147142104138,21.3917533862681,124.077802364795)) ;
#92999 = CARTESIAN_POINT('Ctrl Pts',(-20.2825949674431,21.4018360944658,124.243492472331)) ;
#93000 = CARTESIAN_POINT('Ctrl Pts',(-20.1280211187702,21.4116486873923,124.380174251512)) ;
#93001 = CARTESIAN_POINT('Ctrl Pts',(-19.9477576259279,21.4217158796502,124.490980574694)) ;
#93002 = CARTESIAN_POINT('Ctrl Pts',(-19.7541625513692,21.4316147091128,124.567467521575)) ;
#93003 = CARTESIAN_POINT('Ctrl Pts',(-19.5471445694448,21.441668700303,124.609901982404)) ;
#93004 = CARTESIAN_POINT('Ctrl Pts',(-19.3396514879245,21.4515404250862,124.615828021974)) ;
#93005 = CARTESIAN_POINT('Ctrl Pts',(-19.1302180618309,21.4616108672164,124.585090730345)) ;
#93006 = CARTESIAN_POINT('Ctrl Pts',(-18.9339576917746,21.4714439456467,124.520098552817)) ;
#93007 = CARTESIAN_POINT('Ctrl Pts',(-18.7480491375377,21.4814744191481,124.420590545696)) ;
#93008 = CARTESIAN_POINT('Ctrl Pts',(-18.5825887816303,21.4915060184468,124.289804563175)) ;
#93009 = CARTESIAN_POINT('Ctrl Pts',(-18.4448685819792,21.501335719485,124.135752812325)) ;
#93010 = CARTESIAN_POINT('Ctrl Pts',(-18.33367553148,21.5113251575414,123.95758788387)) ;
#93011 = CARTESIAN_POINT('Ctrl Pts',(-18.2551799398272,21.5213690607575,123.761568607706)) ;
#93012 = CARTESIAN_POINT('Ctrl Pts',(-18.2124473470775,21.531190581571,123.559558762886)) ;
#93013 = CARTESIAN_POINT('Ctrl Pts',(-18.2047822889441,21.5412263058181,123.34872005525)) ;
#93014 = CARTESIAN_POINT('Ctrl Pts',(-18.234346097043,21.5512484597506,123.140091282783)) ;
#93015 = CARTESIAN_POINT('Ctrl Pts',(-18.2983110621091,21.5611106915079,122.942886810719)) ;
#93016 = CARTESIAN_POINT('Ctrl Pts',(-18.3959902964386,21.5710697619658,122.757690821319)) ;
#93017 = CARTESIAN_POINT('Ctrl Pts',(-18.5255720550115,21.581104934342,122.591216512545)) ;
#93018 = CARTESIAN_POINT('Ctrl Pts',(-18.6794900206826,21.5909853195003,122.451700738858)) ;
#93019 = CARTESIAN_POINT('Ctrl Pts',(-18.8583520010264,21.6010420340942,122.339007617028)) ;
#93020 = CARTESIAN_POINT('Ctrl Pts',(-19.0506455463803,21.6109213026663,122.260495050718)) ;
#93021 = CARTESIAN_POINT('Ctrl Pts',(-19.2558150100151,21.6209122601519,122.215517104527)) ;
#93022 = CARTESIAN_POINT('Ctrl Pts',(-19.4667419928137,21.6309529187871,122.207269166301)) ;
#93023 = CARTESIAN_POINT('Ctrl Pts',(-19.671611306749,21.6407858984951,122.234836706111)) ;
#93024 = CARTESIAN_POINT('Ctrl Pts',(-19.8719733222595,21.6507790317448,122.29800611631)) ;
#93025 = CARTESIAN_POINT('Ctrl Pts',(-20.0588577647068,21.6608110841282,122.395778370731)) ;
#93026 = CARTESIAN_POINT('Ctrl Pts',(-20.2232889185199,21.6706763130795,122.522158713432)) ;
#93027 = CARTESIAN_POINT('Ctrl Pts',(-20.3650985195692,21.6806382543227,122.676281555765)) ;
#93028 = CARTESIAN_POINT('Ctrl Pts',(-20.4785231200122,21.6906729693595,122.854145180264)) ;
#93029 = CARTESIAN_POINT('Ctrl Pts',(-20.5584654849309,21.7005587397035,123.046012225195)) ;
#93030 = CARTESIAN_POINT('Ctrl Pts',(-20.6046775909707,21.7106213370923,123.252424731187)) ;
#93031 = CARTESIAN_POINT('Ctrl Pts',(-20.6142383738088,21.7204717489275,123.459306777541)) ;
#93032 = CARTESIAN_POINT('Ctrl Pts',(-20.587797478846,21.7304989182135,123.668438871735)) ;
#93033 = CARTESIAN_POINT('Ctrl Pts',(-20.5249128780641,21.7405263989276,123.869661185407)) ;
#93034 = CARTESIAN_POINT('Ctrl Pts',(-20.4301887540128,21.7503694515069,124.053631115925)) ;
#93035 = CARTESIAN_POINT('Ctrl Pts',(-20.3034636380379,21.7603633549455,124.221213703478)) ;
#93036 = CARTESIAN_POINT('Ctrl Pts',(-20.1487862324558,21.7703904777219,124.364442194746)) ;
#93037 = CARTESIAN_POINT('Ctrl Pts',(-19.9741429213597,21.780281182614,124.47730256004)) ;
#93038 = CARTESIAN_POINT('Ctrl Pts',(-19.780720987989,21.7902732094643,124.559229104381)) ;
#93039 = CARTESIAN_POINT('Ctrl Pts',(-19.5769360767532,21.8002191909528,124.606050632827)) ;
#93040 = CARTESIAN_POINT('Ctrl Pts',(-19.3681010650657,21.8101663635748,124.617200646608)) ;
#93041 = CARTESIAN_POINT('Ctrl Pts',(-19.1584464126587,21.8202143049009,124.591432573086)) ;
#93042 = CARTESIAN_POINT('Ctrl Pts',(-18.9604177626516,21.8300619387087,124.531049432518)) ;
#93043 = CARTESIAN_POINT('Ctrl Pts',(-18.7734573807133,21.8400236533937,124.436702689739)) ;
#93044 = CARTESIAN_POINT('Ctrl Pts',(-18.6047340145598,21.8500522862723,124.310256630304)) ;
#93045 = CARTESIAN_POINT('Ctrl Pts',(-18.4621942150218,21.8599626118074,124.158312586549)) ;
#93046 = CARTESIAN_POINT('Ctrl Pts',(-18.3474585442045,21.8698974422791,123.983782756746)) ;
#93047 = CARTESIAN_POINT('Ctrl Pts',(-18.2640502912331,21.8799387746611,123.78985926928)) ;
#93048 = CARTESIAN_POINT('Ctrl Pts',(-18.2162240830318,21.8898316480999,123.58745555314)) ;
#93049 = CARTESIAN_POINT('Ctrl Pts',(-18.2036438407707,21.8998008139178,123.378240612157)) ;
#93050 = CARTESIAN_POINT('Ctrl Pts',(-18.2280682294196,21.9098295476343,123.168844784421)) ;
#93051 = CARTESIAN_POINT('Ctrl Pts',(-18.3069945112889,21.9230220664055,122.902886831599)) ;
#93052 = CARTESIAN_POINT('Ctrl Pts',(-18.4552999600095,21.9363819344482,122.660697707315)) ;
#93053 = CARTESIAN_POINT('Ctrl Pts',(-18.6570216056765,21.949607271597,122.469325654628)) ;
#93054 = CARTESIAN_POINT('Ctrl Pts',(-18.8316797947684,21.9595884974377,122.353021524023)) ;
#93055 = CARTESIAN_POINT('Ctrl Pts',(-19.0250825772389,21.9696240644205,122.268736505731)) ;
#93056 = CARTESIAN_POINT('Ctrl Pts',(-19.2265882388558,21.9794871423826,122.219744505604)) ;
#93057 = CARTESIAN_POINT('Ctrl Pts',(-19.4378387744727,21.9895574411837,122.206163830183)) ;
#93058 = CARTESIAN_POINT('Ctrl Pts',(-19.643505555205,21.9993997397515,122.228957332354)) ;
#93059 = CARTESIAN_POINT('Ctrl Pts',(-19.8446819721285,22.0093604379213,122.287067936604)) ;
#93060 = CARTESIAN_POINT('Ctrl Pts',(-20.033984583094,22.0193984721008,122.38031752728)) ;
#93061 = CARTESIAN_POINT('Ctrl Pts',(-20.2016926408589,22.0292722089473,122.502684395899)) ;
#93062 = CARTESIAN_POINT('Ctrl Pts',(-20.348434425126,22.0393439928725,122.655289376748)) ;
#93063 = CARTESIAN_POINT('Ctrl Pts',(-20.4637741378317,22.0491761140737,122.826843918411)) ;
#93064 = CARTESIAN_POINT('Ctrl Pts',(-20.5497920398545,22.0592091380992,123.01942208058)) ;
#93065 = CARTESIAN_POINT('Ctrl Pts',(-20.6004603830163,22.0692250182958,123.223814326905)) ;
#93066 = CARTESIAN_POINT('Ctrl Pts',(-20.6150640025834,22.07910853739,123.431083510187)) ;
#93067 = CARTESIAN_POINT('Ctrl Pts',(-20.593494061192,22.0890989497537,123.639987676486)) ;
#93068 = CARTESIAN_POINT('Ctrl Pts',(-20.5172182747527,22.1023621129571,123.908212271559)) ;
#93069 = CARTESIAN_POINT('Ctrl Pts',(-20.3727555111962,22.1156396832083,124.150777474727)) ;
#93070 = CARTESIAN_POINT('Ctrl Pts',(-20.1718123417911,22.1289699857149,124.346093874613)) ;
#93071 = CARTESIAN_POINT('Ctrl Pts',(-19.9998410396279,22.1388686675313,124.463290461051)) ;
#93072 = CARTESIAN_POINT('Ctrl Pts',(-19.8085084880358,22.1488581825789,124.549850711102)) ;
#93073 = CARTESIAN_POINT('Ctrl Pts',(-19.6058755401531,22.1588062343539,124.601655314269)) ;
#93074 = CARTESIAN_POINT('Ctrl Pts',(-19.3975125045008,22.1687476376324,124.617740356275)) ;
#93075 = CARTESIAN_POINT('Ctrl Pts',(-19.1194368110391,22.1820343024133,124.590882680961)) ;
#93076 = CARTESIAN_POINT('Ctrl Pts',(-18.7886603018455,22.1986447240681,124.467217873756)) ;
#93077 = CARTESIAN_POINT('Ctrl Pts',(-18.4662721824699,22.2185559863189,124.192767655879)) ;
#93078 = CARTESIAN_POINT('Ctrl Pts',(-18.2564052108504,22.2385001154838,123.824248329154)) ;
#93079 = CARTESIAN_POINT('Ctrl Pts',(-18.1850298167595,22.258423278089,123.406724031906)) ;
#93080 = CARTESIAN_POINT('Ctrl Pts',(-18.2596166140788,22.2783134004955,122.990368787933)) ;
#93081 = CARTESIAN_POINT('Ctrl Pts',(-18.4732461778433,22.2983183540956,122.622623813905)) ;
#93082 = CARTESIAN_POINT('Ctrl Pts',(-18.7967224956911,22.3181566111112,122.351774759817)) ;
#93083 = CARTESIAN_POINT('Ctrl Pts',(-19.1960528209252,22.3381509118978,122.206072263074)) ;
#93084 = CARTESIAN_POINT('Ctrl Pts',(-19.6188774949697,22.3580361539422,122.205770409329)) ;
#93085 = CARTESIAN_POINT('Ctrl Pts',(-20.0166123708548,22.3779111004182,122.348576452915)) ;
#93086 = CARTESIAN_POINT('Ctrl Pts',(-20.3441439289911,22.3979441703592,122.620968139664)) ;
#93087 = CARTESIAN_POINT('Ctrl Pts',(-20.5570158953908,22.4178326772596,122.986324907579)) ;
#93088 = CARTESIAN_POINT('Ctrl Pts',(-20.63376602721,22.4376875370409,123.401523750881)) ;
#93089 = CARTESIAN_POINT('Ctrl Pts',(-20.5628771445942,22.4577383708286,123.821821360625)) ;
#93090 = CARTESIAN_POINT('Ctrl Pts',(-20.3561025774124,22.4775043127179,124.187848336613)) ;
#93091 = CARTESIAN_POINT('Ctrl Pts',(-20.0335850425227,22.4975170441772,124.465242851692)) ;
#93092 = CARTESIAN_POINT('Ctrl Pts',(-19.6377262102583,22.5174098791208,124.614575343707)) ;
#93093 = CARTESIAN_POINT('Ctrl Pts',(-19.2145950747695,22.5373169024603,124.620562106581)) ;
#93094 = CARTESIAN_POINT('Ctrl Pts',(-18.8143052159409,22.557232167361,124.482124393492)) ;
#93095 = CARTESIAN_POINT('Ctrl Pts',(-18.4838083293935,22.5772638595207,124.213504396817)) ;
#93096 = CARTESIAN_POINT('Ctrl Pts',(-18.266814494246,22.5971069060937,123.851612989797)) ;
#93097 = CARTESIAN_POINT('Ctrl Pts',(-18.1851080172229,22.6170234539935,123.436153599146)) ;
#93098 = CARTESIAN_POINT('Ctrl Pts',(-18.2502202399435,22.6369556969848,123.017333953264)) ;
#93099 = CARTESIAN_POINT('Ctrl Pts',(-18.4538259242092,22.6568595317941,122.646346956215)) ;
#93100 = CARTESIAN_POINT('Ctrl Pts',(-18.7714168946977,22.6767599319816,122.366744911555)) ;
#93101 = CARTESIAN_POINT('Ctrl Pts',(-19.166285915724,22.6967096083609,122.211749714372)) ;
#93102 = CARTESIAN_POINT('Ctrl Pts',(-19.589972383929,22.7166421325813,122.200906821069)) ;
#93103 = CARTESIAN_POINT('Ctrl Pts',(-19.9918128903869,22.7365621415675,122.334876945434)) ;
#93104 = CARTESIAN_POINT('Ctrl Pts',(-20.3243318664466,22.7565190477437,122.598424801624)) ;
#93105 = CARTESIAN_POINT('Ctrl Pts',(-20.5465556808839,22.7764048872452,122.958240044023)) ;
#93106 = CARTESIAN_POINT('Ctrl Pts',(-20.6329370095497,22.796376059381,123.373906325153)) ;
#93107 = CARTESIAN_POINT('Ctrl Pts',(-20.5733229208069,22.8161902563654,123.791036866964)) ;
#93108 = CARTESIAN_POINT('Ctrl Pts',(-20.3738395604906,22.8361714423337,124.16606417652)) ;
#93109 = CARTESIAN_POINT('Ctrl Pts',(-20.1119254984363,22.8527469477229,124.401935987589)) ;
#93110 = CARTESIAN_POINT('Ctrl Pts',(-19.8627907051398,22.8660563955865,124.529374391931)) ;
#93111 = CARTESIAN_POINT('Ctrl Pts',(-19.5941634357807,22.8794240933631,124.611788225759)) ;
#93112 = CARTESIAN_POINT('Ctrl Pts',(-19.2437164503592,22.895914665029,124.624712075177)) ;
#93113 = CARTESIAN_POINT('Ctrl Pts',(-18.8402567476097,22.9158349373618,124.496012765143)) ;
#93114 = CARTESIAN_POINT('Ctrl Pts',(-18.5605856920532,22.9324519730828,124.280092618968)) ;
#93115 = CARTESIAN_POINT('Ctrl Pts',(-18.3909770737706,22.9457428233639,124.057986522721)) ;
#93116 = CARTESIAN_POINT('Ctrl Pts',(-18.2945642787171,22.9557118685184,123.871929176122)) ;
#93117 = CARTESIAN_POINT('Ctrl Pts',(-18.2319237526866,22.965615259152,123.673347903885)) ;
#93118 = CARTESIAN_POINT('Ctrl Pts',(-18.2044109629437,22.9756730452647,123.46372521076)) ;
#93119 = CARTESIAN_POINT('Ctrl Pts',(-18.2133455804091,22.9855250819144,123.256767938928)) ;
#93120 = CARTESIAN_POINT('Ctrl Pts',(-18.2735481450176,22.9988902060576,122.982370184821)) ;
#93121 = CARTESIAN_POINT('Ctrl Pts',(-18.4029730647199,23.0121162690207,122.732648967479)) ;
#93122 = CARTESIAN_POINT('Ctrl Pts',(-18.5911586333151,23.0254199173029,122.525747384851)) ;
#93123 = CARTESIAN_POINT('Ctrl Pts',(-18.7572840479438,23.0354114484659,122.397160345166)) ;
#93124 = CARTESIAN_POINT('Ctrl Pts',(-18.9442034529857,23.0454508962652,122.29917135121)) ;
#93125 = CARTESIAN_POINT('Ctrl Pts',(-19.1413113374311,23.0552946717791,122.236069991854)) ;
#93126 = CARTESIAN_POINT('Ctrl Pts',(-19.3492334981036,23.0652803131667,122.207338844066)) ;
#93127 = CARTESIAN_POINT('Ctrl Pts',(-19.5580294696131,23.0752170975285,122.21499628788)) ;
#93128 = CARTESIAN_POINT('Ctrl Pts',(-19.7645716223827,23.0852669319959,122.2593847219)) ;
#93129 = CARTESIAN_POINT('Ctrl Pts',(-19.956478859204,23.095117381499,122.337250989053)) ;
#93130 = CARTESIAN_POINT('Ctrl Pts',(-20.1343708699036,23.1050893954811,122.448127388525)) ;
#93131 = CARTESIAN_POINT('Ctrl Pts',(-20.2906970657554,23.1150845533282,122.588593762462)) ;
#93132 = CARTESIAN_POINT('Ctrl Pts',(-20.4205292649936,23.1251184796919,122.754827851092)) ;
#93133 = CARTESIAN_POINT('Ctrl Pts',(-20.5180699479816,23.1349741881243,122.937651944192)) ;
#93134 = CARTESIAN_POINT('Ctrl Pts',(-20.5835848106388,23.144972337463,123.137338627828)) ;
#93135 = CARTESIAN_POINT('Ctrl Pts',(-20.6133315601013,23.1548717406366,123.343349279498)) ;
#93136 = CARTESIAN_POINT('Ctrl Pts',(-20.6068042955674,23.164922937525,123.554533958808)) ;
#93137 = CARTESIAN_POINT('Ctrl Pts',(-20.5644542804558,23.1748052613379,123.757945285797)) ;
#93138 = CARTESIAN_POINT('Ctrl Pts',(-20.4869988566023,23.1848001569945,123.953265947771)) ;
#93139 = CARTESIAN_POINT('Ctrl Pts',(-20.3762451153194,23.194821256377,124.13249196555)) ;
#93140 = CARTESIAN_POINT('Ctrl Pts',(-20.2377780682512,23.2047285242391,124.288078667815)) ;
#93141 = CARTESIAN_POINT('Ctrl Pts',(-20.0741559131026,23.2146668680644,124.41798671846)) ;
#93142 = CARTESIAN_POINT('Ctrl Pts',(-19.8892906416545,23.2246702873648,124.518297175793)) ;
#93143 = CARTESIAN_POINT('Ctrl Pts',(-19.6891176860214,23.2347048380719,124.584849932306)) ;
#93144 = CARTESIAN_POINT('Ctrl Pts',(-19.4844008567411,23.2445497876775,124.615406104496)) ;
#93145 = CARTESIAN_POINT('Ctrl Pts',(-19.2745631934654,23.2545356297904,124.610269779593)) ;
#93146 = CARTESIAN_POINT('Ctrl Pts',(-19.0697563387047,23.2644704371595,124.569121010592)) ;
#93147 = CARTESIAN_POINT('Ctrl Pts',(-18.8729354077247,23.2745279788728,124.49194530849)) ;
#93148 = CARTESIAN_POINT('Ctrl Pts',(-18.6965271275385,23.284349576385,124.384596043654)) ;
#93149 = CARTESIAN_POINT('Ctrl Pts',(-18.537505207443,23.2944058358654,124.245310914228)) ;
#93150 = CARTESIAN_POINT('Ctrl Pts',(-18.4068828184235,23.3043457721658,124.082183809851)) ;
#93151 = CARTESIAN_POINT('Ctrl Pts',(-18.3063569604988,23.3142528929102,123.899773364579)) ;
#93152 = CARTESIAN_POINT('Ctrl Pts',(-18.238182102266,23.3242957988355,123.699954793539)) ;
#93153 = CARTESIAN_POINT('Ctrl Pts',(-18.2061315888392,23.3342035799347,123.494134506193)) ;
#93154 = CARTESIAN_POINT('Ctrl Pts',(-18.2099782467636,23.3442139489371,123.283713240502)) ;
#93155 = CARTESIAN_POINT('Ctrl Pts',(-18.2508047878305,23.3542447875059,123.076824776893)) ;
#93156 = CARTESIAN_POINT('Ctrl Pts',(-18.3252380526444,23.3640976271456,122.883518211052)) ;
#93157 = CARTESIAN_POINT('Ctrl Pts',(-18.4332307006835,23.3740856283106,122.703457545309)) ;
#93158 = CARTESIAN_POINT('Ctrl Pts',(-18.570043155712,23.3840144472898,122.545803263845)) ;
#93159 = CARTESIAN_POINT('Ctrl Pts',(-18.7328941528992,23.3940021500121,122.413240967094)) ;
#93160 = CARTESIAN_POINT('Ctrl Pts',(-18.9173305839693,23.4040381498147,122.310793637475)) ;
#93161 = CARTESIAN_POINT('Ctrl Pts',(-19.1130661739556,23.4138930196162,122.242836710272)) ;
#93162 = CARTESIAN_POINT('Ctrl Pts',(-19.3205318000607,23.4238924500397,122.209140767178)) ;
#93163 = CARTESIAN_POINT('Ctrl Pts',(-19.5285765182959,23.433787567505,122.211727966587)) ;
#93164 = CARTESIAN_POINT('Ctrl Pts',(-19.7363643453883,23.4438480610219,122.251054376304)) ;
#93165 = CARTESIAN_POINT('Ctrl Pts',(-19.9300969267165,23.4536975412231,122.324201636643)) ;
#93166 = CARTESIAN_POINT('Ctrl Pts',(-20.1116481432256,23.4637239914869,122.431297533579)) ;
#93167 = CARTESIAN_POINT('Ctrl Pts',(-20.2715506693218,23.473755281965,122.568801972181)) ;
#93168 = CARTESIAN_POINT('Ctrl Pts',(-20.4029659088239,23.4835966696168,122.728604725613)) ;
#93169 = CARTESIAN_POINT('Ctrl Pts',(-20.5066563534772,23.4936000705081,122.911544063028)) ;
#93170 = CARTESIAN_POINT('Ctrl Pts',(-20.5768108983585,23.5035844532992,123.109415497325)) ;
#93171 = CARTESIAN_POINT('Ctrl Pts',(-20.6115256227708,23.5136235433126,123.317573246483)) ;
#93172 = CARTESIAN_POINT('Ctrl Pts',(-20.6098969894375,23.5234693522218,123.52457158236)) ;
#93173 = CARTESIAN_POINT('Ctrl Pts',(-20.5722509395659,23.5334537750408,123.731041347267)) ;
#93174 = CARTESIAN_POINT('Ctrl Pts',(-20.4997174059433,23.543393400282,123.927042123842)) ;
#93175 = CARTESIAN_POINT('Ctrl Pts',(-20.3931719197641,23.5534330898006,124.109223143745)) ;
#93176 = CARTESIAN_POINT('Ctrl Pts',(-20.2587341895538,23.5633212782192,124.267797382914)) ;
#93177 = CARTESIAN_POINT('Ctrl Pts',(-20.0974322543525,23.5733108042213,124.402272320034)) ;
#93178 = CARTESIAN_POINT('Ctrl Pts',(-19.9157158970275,23.5832693055765,124.506233898799)) ;
#93179 = CARTESIAN_POINT('Ctrl Pts',(-19.7200317318683,23.5931688995801,124.577135520212)) ;
#93180 = CARTESIAN_POINT('Ctrl Pts',(-19.511958597003,23.6032167877014,124.613440420387)) ;
#93181 = CARTESIAN_POINT('Ctrl Pts',(-19.3038931117637,23.613112212947,124.613234240594)) ;
#93182 = CARTESIAN_POINT('Ctrl Pts',(-19.0956394360566,23.6231736036475,124.576334619288)) ;
#93183 = CARTESIAN_POINT('Ctrl Pts',(-18.9011715211872,23.6330191873342,124.505414756995)) ;
#93184 = CARTESIAN_POINT('Ctrl Pts',(-18.7195047168646,23.6429821606434,124.401196107756)) ;
#93185 = CARTESIAN_POINT('Ctrl Pts',(-18.5578392233142,23.6530078274692,124.265939530275)) ;
#93186 = CARTESIAN_POINT('Ctrl Pts',(-18.4235465577687,23.6629223053355,124.106543747631)) ;
#93187 = CARTESIAN_POINT('Ctrl Pts',(-18.3178150771585,23.6729108200105,123.9250945317)) ;
#93188 = CARTESIAN_POINT('Ctrl Pts',(-18.2452273886237,23.6829549309259,123.726824520025)) ;
#93189 = CARTESIAN_POINT('Ctrl Pts',(-18.2084622209874,23.6927830685205,123.523473745696)) ;
#93190 = CARTESIAN_POINT('Ctrl Pts',(-18.2074439778871,23.7028596365794,123.31167785126)) ;
#93191 = CARTESIAN_POINT('Ctrl Pts',(-18.2423298104587,23.7127117984836,123.107467698959)) ;
#93192 = CARTESIAN_POINT('Ctrl Pts',(-18.3135158811486,23.7227847604404,122.908064141033)) ;
#93193 = CARTESIAN_POINT('Ctrl Pts',(-18.4159003030267,23.7326273224433,122.728227460704)) ;
#93194 = CARTESIAN_POINT('Ctrl Pts',(-18.5492444985137,23.7426077589371,122.56624045852)) ;
#93195 = CARTESIAN_POINT('Ctrl Pts',(-18.7095634099869,23.7526260642615,122.429654359688)) ;
#93196 = CARTESIAN_POINT('Ctrl Pts',(-18.888529532284,23.762510028181,122.324026238617)) ;
#93197 = CARTESIAN_POINT('Ctrl Pts',(-19.0866746849107,23.7725759049195,122.249802045763)) ;
#93198 = CARTESIAN_POINT('Ctrl Pts',(-19.2900277703076,23.7824150057804,122.211839220089)) ;
#93199 = CARTESIAN_POINT('Ctrl Pts',(-19.5009280169213,23.7924480886462,122.209188897855)) ;
#93200 = CARTESIAN_POINT('Ctrl Pts',(-19.7087890814224,23.8024697739216,122.243680915572)) ;
#93201 = CARTESIAN_POINT('Ctrl Pts',(-19.9045118580242,23.8123364690201,122.31233133179)) ;
#93202 = CARTESIAN_POINT('Ctrl Pts',(-20.0873423992775,23.8222963587547,122.414410667244)) ;
#93203 = CARTESIAN_POINT('Ctrl Pts',(-20.2506734014014,23.8323313465801,122.547919056241)) ;
#93204 = CARTESIAN_POINT('Ctrl Pts',(-20.3865972372764,23.8422180506544,122.705203000666)) ;
#93205 = CARTESIAN_POINT('Ctrl Pts',(-20.4949915022532,23.8522831948873,122.886893090087)) ;
#93206 = CARTESIAN_POINT('Ctrl Pts',(-20.5687253459054,23.8621224856159,123.080191817205)) ;
#93207 = CARTESIAN_POINT('Ctrl Pts',(-20.6089362319602,23.8721850430543,123.28785664052)) ;
#93208 = CARTESIAN_POINT('Ctrl Pts',(-20.6121978990031,23.8820820943064,123.495909786969)) ;
#93209 = CARTESIAN_POINT('Ctrl Pts',(-20.5798621479707,23.8920133010547,123.702170605702)) ;
#93210 = CARTESIAN_POINT('Ctrl Pts',(-20.5112278120771,23.9020554852735,123.901818256384)) ;
#93211 = CARTESIAN_POINT('Ctrl Pts',(-20.4106814625519,23.9119421133844,124.083739072873)) ;
#93212 = CARTESIAN_POINT('Ctrl Pts',(-20.2789510402383,23.9219353859168,124.247385499214)) ;
#93213 = CARTESIAN_POINT('Ctrl Pts',(-20.1215140193318,23.9318804614583,124.384961368838)) ;
#93214 = CARTESIAN_POINT('Ctrl Pts',(-19.9427040588716,23.9418300121866,124.493512735114)) ;
#93215 = CARTESIAN_POINT('Ctrl Pts',(-19.7459483725956,23.9518693470345,124.569858320534)) ;
#93216 = CARTESIAN_POINT('Ctrl Pts',(-19.5420958579486,23.9617554859785,124.610447514314)) ;
#93217 = CARTESIAN_POINT('Ctrl Pts',(-19.3319860693722,23.9717535989522,124.61534345927)) ;
#93218 = CARTESIAN_POINT('Ctrl Pts',(-19.1257788355429,23.9816733613046,124.584048463693)) ;
#93219 = CARTESIAN_POINT('Ctrl Pts',(-18.9257658599301,23.9917127569173,124.516694255687)) ;
#93220 = CARTESIAN_POINT('Ctrl Pts',(-18.7429093614432,24.0016219427055,124.416883451877)) ;
#93221 = CARTESIAN_POINT('Ctrl Pts',(-18.5793682570161,24.011557126863,124.286955917705)) ;
#93222 = CARTESIAN_POINT('Ctrl Pts',(-18.4395550076449,24.0215981842489,124.12880714073)) ;
#93223 = CARTESIAN_POINT('Ctrl Pts',(-18.3308792312625,24.0314853422822,123.95160799929)) ;
#93224 = CARTESIAN_POINT('Ctrl Pts',(-18.2534953404692,24.0414776219581,123.756326967307)) ;
#93225 = CARTESIAN_POINT('Ctrl Pts',(-18.2114309389755,24.0514261390032,123.551439534161)) ;
#93226 = CARTESIAN_POINT('Ctrl Pts',(-18.2052935463612,24.0613629165736,123.342645080243)) ;
#93227 = CARTESIAN_POINT('Ctrl Pts',(-18.2353874848655,24.0713459527205,123.134912288496)) ;
#93228 = CARTESIAN_POINT('Ctrl Pts',(-18.3018447079775,24.0813897043143,122.934516760273)) ;
#93229 = CARTESIAN_POINT('Ctrl Pts',(-18.3995390927353,24.0912182335268,122.75241029189)) ;
#93230 = CARTESIAN_POINT('Ctrl Pts',(-18.5304446989063,24.1012935944355,122.585941046542)) ;
#93231 = CARTESIAN_POINT('Ctrl Pts',(-18.6848541056234,24.1111501933227,122.447684995541)) ;
#93232 = CARTESIAN_POINT('Ctrl Pts',(-18.8644224668532,24.1212131873406,122.335908353526)) ;
#93233 = CARTESIAN_POINT('Ctrl Pts',(-19.0571387458606,24.1310911216301,122.258444830493)) ;
#93234 = CARTESIAN_POINT('Ctrl Pts',(-19.2627622836008,24.1410917691882,122.214785949569)) ;
#93235 = CARTESIAN_POINT('Ctrl Pts',(-19.4711725606285,24.1510096156262,122.207393834254)) ;
#93236 = CARTESIAN_POINT('Ctrl Pts',(-19.6803970262427,24.1610607326319,122.236738184022)) ;
#93237 = CARTESIAN_POINT('Ctrl Pts',(-19.8778824262284,24.1709314679425,122.30059392637)) ;
#93238 = CARTESIAN_POINT('Ctrl Pts',(-20.064951432352,24.1810021751855,122.399666043339)) ;
#93239 = CARTESIAN_POINT('Ctrl Pts',(-20.2281336989988,24.1908351826373,122.526602593629)) ;
#93240 = CARTESIAN_POINT('Ctrl Pts',(-20.3700097469884,24.2008656749396,122.682600116585)) ;
#93241 = CARTESIAN_POINT('Ctrl Pts',(-20.4821469033699,24.210897270013,122.861226293759)) ;
#93242 = CARTESIAN_POINT('Ctrl Pts',(-20.5603565412622,24.2207269691513,123.052490631286)) ;
#93243 = CARTESIAN_POINT('Ctrl Pts',(-20.605497599656,24.2307164190328,123.257597882604)) ;
#93244 = CARTESIAN_POINT('Ctrl Pts',(-20.6138517566313,24.2407602768485,123.468583717357)) ;
#93245 = CARTESIAN_POINT('Ctrl Pts',(-20.5864978803967,24.2505819674387,123.67324701416)) ;
#93246 = CARTESIAN_POINT('Ctrl Pts',(-20.523154702789,24.2606170579791,123.874478638428)) ;
#93247 = CARTESIAN_POINT('Ctrl Pts',(-20.4254304104399,24.2706415769618,124.061214670623)) ;
#93248 = CARTESIAN_POINT('Ctrl Pts',(-20.2991788111832,24.280501422372,124.225596457457)) ;
#93249 = CARTESIAN_POINT('Ctrl Pts',(-20.1451299023672,24.2904611986877,124.367416555609)) ;
#93250 = CARTESIAN_POINT('Ctrl Pts',(-19.967433449482,24.3004893960023,124.48086059044)) ;
#93251 = CARTESIAN_POINT('Ctrl Pts',(-19.7751577866426,24.3103969382926,124.560990104297)) ;
#93252 = CARTESIAN_POINT('Ctrl Pts',(-19.5693703408195,24.3204295888565,124.607155031469)) ;
#93253 = CARTESIAN_POINT('Ctrl Pts',(-19.3617967608512,24.3303135452832,124.616805532041)) ;
#93254 = CARTESIAN_POINT('Ctrl Pts',(-19.1534319572427,24.340303246645,124.590503035312)) ;
#93255 = CARTESIAN_POINT('Ctrl Pts',(-18.9519051680494,24.350344241921,124.527673626041)) ;
#93256 = CARTESIAN_POINT('Ctrl Pts',(-18.7680835678611,24.3601771311894,124.433119432297)) ;
#93257 = CARTESIAN_POINT('Ctrl Pts',(-18.6004240971246,24.3701702895568,124.30652665652)) ;
#93258 = CARTESIAN_POINT('Ctrl Pts',(-18.4570479671225,24.3802023319089,124.151838394843)) ;
#93259 = CARTESIAN_POINT('Ctrl Pts',(-18.3444058748891,24.3900675758674,123.977707913837)) ;
#93260 = CARTESIAN_POINT('Ctrl Pts',(-18.2623662487685,24.4000294671134,123.785008650239)) ;
#93261 = CARTESIAN_POINT('Ctrl Pts',(-18.2150227216315,24.4100643671318,123.579434985754)) ;
#93262 = CARTESIAN_POINT('Ctrl Pts',(-18.2039108267018,24.4199494475464,123.371890116164)) ;
#93263 = CARTESIAN_POINT('Ctrl Pts',(-18.2294765751654,24.4300146196713,123.161866621655)) ;
#93264 = CARTESIAN_POINT('Ctrl Pts',(-18.2896850181631,24.4398618543947,122.963774150421)) ;
#93265 = CARTESIAN_POINT('Ctrl Pts',(-18.3846631867251,24.4498926657125,122.775510294794)) ;
#93266 = CARTESIAN_POINT('Ctrl Pts',(-18.5109890562497,24.459902281626,122.607182353693)) ;
#93267 = CARTESIAN_POINT('Ctrl Pts',(-18.662934415357,24.4698130610297,122.464645988719)) ;
#93268 = CARTESIAN_POINT('Ctrl Pts',(-18.8373840590184,24.4797423268187,122.349990522936)) ;
#93269 = CARTESIAN_POINT('Ctrl Pts',(-19.0313351993538,24.4897850201314,122.266594737188)) ;
#93270 = CARTESIAN_POINT('Ctrl Pts',(-19.2336139949417,24.4996715528261,122.218758536611)) ;
#93271 = CARTESIAN_POINT('Ctrl Pts',(-19.4433196957446,24.5096646979294,122.206287817069)) ;
#93272 = CARTESIAN_POINT('Ctrl Pts',(-19.651016738765,24.5196103786034,122.230384482874)) ;
#93273 = CARTESIAN_POINT('Ctrl Pts',(-19.8515383300851,24.5295576362302,122.289780446404)) ;
#93274 = CARTESIAN_POINT('Ctrl Pts',(-20.0404730317858,24.5396055383516,122.384240055457)) ;
#93275 = CARTESIAN_POINT('Ctrl Pts',(-20.2068658200132,24.5494532439733,122.507427686497)) ;
#93276 = CARTESIAN_POINT('Ctrl Pts',(-20.3514609588066,24.5594147106074,122.658908405433)) ;
#93277 = CARTESIAN_POINT('Ctrl Pts',(-20.4681229484062,24.5694442638756,122.834556332122)) ;
#93278 = CARTESIAN_POINT('Ctrl Pts',(-20.5515899993242,24.579351155903,123.025376842839)) ;
#93279 = CARTESIAN_POINT('Ctrl Pts',(-20.6012474646981,24.5892988000161,123.228509354833)) ;
#93280 = CARTESIAN_POINT('Ctrl Pts',(-20.6150856716365,24.5992988430449,123.438313400664)) ;
#93281 = CARTESIAN_POINT('Ctrl Pts',(-20.5918280654159,24.6093376090389,123.648058203408)) ;
#93282 = CARTESIAN_POINT('Ctrl Pts',(-20.5341801356447,24.6191626710612,123.846419055393)) ;
#93283 = CARTESIAN_POINT('Ctrl Pts',(-20.4411613876781,24.6292172183875,124.036215827864)) ;
#93284 = CARTESIAN_POINT('Ctrl Pts',(-20.3176758980808,24.6391604618367,124.204890744429)) ;
#93285 = CARTESIAN_POINT('Ctrl Pts',(-20.1678533644699,24.6490626334446,124.349428636448)) ;
#93286 = CARTESIAN_POINT('Ctrl Pts',(-19.992519974302,24.6591154690548,124.467412207897)) ;
#93287 = CARTESIAN_POINT('Ctrl Pts',(-19.8028366254906,24.6689885267404,124.551709340961)) ;
#93288 = CARTESIAN_POINT('Ctrl Pts',(-19.5990412262366,24.678983788266,124.602912203678)) ;
#93289 = CARTESIAN_POINT('Ctrl Pts',(-19.3887859392486,24.6890091576865,124.617620934042)) ;
#93290 = CARTESIAN_POINT('Ctrl Pts',(-19.1819726876381,24.6988989902131,124.596169219307)) ;
#93291 = CARTESIAN_POINT('Ctrl Pts',(-18.9130614669707,24.7121969610225,124.519808891188)) ;
#93292 = CARTESIAN_POINT('Ctrl Pts',(-18.6717642855586,24.7253953561317,124.376402129123)) ;
#93293 = CARTESIAN_POINT('Ctrl Pts',(-18.4752738471407,24.7387907984112,124.174746595898)) ;
#93294 = CARTESIAN_POINT('Ctrl Pts',(-18.358224596792,24.7486666366501,124.003215096803)) ;
#93295 = CARTESIAN_POINT('Ctrl Pts',(-18.2710748545679,24.7587280392479,123.810519368002)) ;
#93296 = CARTESIAN_POINT('Ctrl Pts',(-18.2196533486992,24.768593096183,123.609567259137)) ;
#93297 = CARTESIAN_POINT('Ctrl Pts',(-18.2032987696929,24.7786051921318,123.399749506451)) ;
#93298 = CARTESIAN_POINT('Ctrl Pts',(-18.2303147037854,24.7918825012772,123.121871295648)) ;
#93299 = CARTESIAN_POINT('Ctrl Pts',(-18.3537922199677,24.8084815267845,122.791296707492)) ;
#93300 = CARTESIAN_POINT('Ctrl Pts',(-18.5827030725049,24.8250805748176,122.522606050233)) ;
#93301 = CARTESIAN_POINT('Ctrl Pts',(-18.8116927441516,24.8383239868485,122.36428598268)) ;
#93302 = CARTESIAN_POINT('Ctrl Pts',(-19.0034240176672,24.8483614145369,122.276149956217)) ;
#93303 = CARTESIAN_POINT('Ctrl Pts',(-19.2048453140622,24.8582657164925,122.223388070652)) ;
#93304 = CARTESIAN_POINT('Ctrl Pts',(-19.4827946985258,24.8715325564677,122.199905670602)) ;
#93305 = CARTESIAN_POINT('Ctrl Pts',(-19.8307376184793,24.8881587545576,122.262279593846)) ;
#93306 = CARTESIAN_POINT('Ctrl Pts',(-20.1971584959203,24.9080778699411,122.474694806873)) ;
#93307 = CARTESIAN_POINT('Ctrl Pts',(-20.4241107575517,24.9246842930753,122.745253284733)) ;
#93308 = CARTESIAN_POINT('Ctrl Pts',(-20.5421825626076,24.937980513571,122.998571458746)) ;
#93309 = CARTESIAN_POINT('Ctrl Pts',(-20.6149656124445,24.9512493459124,123.267944637777)) ;
#93310 = CARTESIAN_POINT('Ctrl Pts',(-20.6152703456339,24.9679405939455,123.622747521554)) ;
#93311 = CARTESIAN_POINT('Ctrl Pts',(-20.4723050323629,24.9877503256183,124.019012698152)) ;
#93312 = CARTESIAN_POINT('Ctrl Pts',(-20.2011037571206,25.0077279329469,124.345923766588)) ;
#93313 = CARTESIAN_POINT('Ctrl Pts',(-19.8352018509868,25.0276542420047,124.559424873862)) ;
#93314 = CARTESIAN_POINT('Ctrl Pts',(-19.4208025231487,25.0474711021694,124.636316301746)) ;
#93315 = CARTESIAN_POINT('Ctrl Pts',(-18.9994693482614,25.0675709177634,124.565580439574)) ;
#93316 = CARTESIAN_POINT('Ctrl Pts',(-18.6335309066038,25.087327881646,124.358919176826)) ;
#93317 = CARTESIAN_POINT('Ctrl Pts',(-18.3557823456024,25.1073648077154,124.036055559741)) ;
#93318 = CARTESIAN_POINT('Ctrl Pts',(-18.2066757173654,25.127234390097,123.640645069707)) ;
#93319 = CARTESIAN_POINT('Ctrl Pts',(-18.2003787407319,25.1471389618501,123.217548707811)) ;
#93320 = CARTESIAN_POINT('Ctrl Pts',(-18.3392640527357,25.1670915640486,122.816604006415)) ;
#93321 = CARTESIAN_POINT('Ctrl Pts',(-18.606064346536,25.1870010550189,122.488044036896)) ;
#93322 = CARTESIAN_POINT('Ctrl Pts',(-18.9674597842372,25.2068524237183,122.269771232825)) ;
#93323 = CARTESIAN_POINT('Ctrl Pts',(-19.3863525061292,25.2269326198543,122.187636259562)) ;
#93324 = CARTESIAN_POINT('Ctrl Pts',(-19.8024619383338,25.2467335634297,122.252489157475)) ;
#93325 = CARTESIAN_POINT('Ctrl Pts',(-20.1751760750366,25.2667175399392,122.456396705223)) ;
#93326 = CARTESIAN_POINT('Ctrl Pts',(-20.4545282748226,25.2866335029148,122.774650929317)) ;
#93327 = CARTESIAN_POINT('Ctrl Pts',(-20.6092751092114,25.3065039377368,123.167880061189)) ;
#93328 = CARTESIAN_POINT('Ctrl Pts',(-20.6199281147208,25.3265542229698,123.593946344125)) ;
#93329 = CARTESIAN_POINT('Ctrl Pts',(-20.4868920076711,25.3463281917291,123.992971200165)) ;
#93330 = CARTESIAN_POINT('Ctrl Pts',(-20.2223887661916,25.3663846498487,124.327269621061)) ;
#93331 = CARTESIAN_POINT('Ctrl Pts',(-19.8640906712415,25.3861795328397,124.548347828565)) ;
#93332 = CARTESIAN_POINT('Ctrl Pts',(-19.4487333833075,25.406146188142,124.635759283439)) ;
#93333 = CARTESIAN_POINT('Ctrl Pts',(-19.0285707159707,25.4261051582185,124.575488744381)) ;
#93334 = CARTESIAN_POINT('Ctrl Pts',(-18.6553223916141,25.4460012458087,124.376405999239)) ;
#93335 = CARTESIAN_POINT('Ctrl Pts',(-18.372020461912,25.4658994157202,124.062217905803)) ;
#93336 = CARTESIAN_POINT('Ctrl Pts',(-18.2124360175169,25.4858052510873,123.670170425234)) ;
#93337 = CARTESIAN_POINT('Ctrl Pts',(-18.196193662723,25.5057551760253,123.246330053742)) ;
#93338 = CARTESIAN_POINT('Ctrl Pts',(-18.3247479722757,25.5256343659356,122.843621213655)) ;
#93339 = CARTESIAN_POINT('Ctrl Pts',(-18.5841090164375,25.5456156902162,122.507162512338)) ;
#93340 = CARTESIAN_POINT('Ctrl Pts',(-18.9420163018406,25.5655454744246,122.280112521784)) ;
#93341 = CARTESIAN_POINT('Ctrl Pts',(-19.3555125525114,25.5854654638154,122.188825953791)) ;
#93342 = CARTESIAN_POINT('Ctrl Pts',(-19.7742961587421,25.6053206591694,122.243020656991)) ;
#93343 = CARTESIAN_POINT('Ctrl Pts',(-20.1526865947328,25.6253666608287,122.43900938881)) ;
#93344 = CARTESIAN_POINT('Ctrl Pts',(-20.3906126005556,25.6418664080385,122.696940295105)) ;
#93345 = CARTESIAN_POINT('Ctrl Pts',(-20.5216824764747,25.6552550124866,122.946016251658)) ;
#93346 = CARTESIAN_POINT('Ctrl Pts',(-20.5849012167548,25.6651168408215,123.143472150751)) ;
#93347 = CARTESIAN_POINT('Ctrl Pts',(-20.6138255672022,25.6750829835791,123.351002241802)) ;
#93348 = CARTESIAN_POINT('Ctrl Pts',(-20.6032059149139,25.688444729704,123.631608389714)) ;
#93349 = CARTESIAN_POINT('Ctrl Pts',(-20.5008843479732,25.7048990586591,123.966371588591)) ;
#93350 = CARTESIAN_POINT('Ctrl Pts',(-20.2867255675478,25.7216663037074,124.25115815757)) ;
#93351 = CARTESIAN_POINT('Ctrl Pts',(-20.0681057515217,25.7348528689815,124.421840372913)) ;
#93352 = CARTESIAN_POINT('Ctrl Pts',(-19.8829958093437,25.7448423277261,124.520903011801)) ;
#93353 = CARTESIAN_POINT('Ctrl Pts',(-19.6841239651198,25.7547961002072,124.586158616998)) ;
#93354 = CARTESIAN_POINT('Ctrl Pts',(-19.4750312685853,25.7648439167398,124.615997659692)) ;
#93355 = CARTESIAN_POINT('Ctrl Pts',(-19.2682136272315,25.7746854498623,124.609461719131)) ;
#93356 = CARTESIAN_POINT('Ctrl Pts',(-19.0626573534037,25.784671692082,124.566942362516)) ;
#93357 = CARTESIAN_POINT('Ctrl Pts',(-18.8684723007839,25.7946083155069,124.489834630106)) ;
#93358 = CARTESIAN_POINT('Ctrl Pts',(-18.6887022668486,25.8046581928899,124.378870939841)) ;
#93359 = CARTESIAN_POINT('Ctrl Pts',(-18.5339300730627,25.8145086316675,124.241258946451)) ;
#93360 = CARTESIAN_POINT('Ctrl Pts',(-18.4034137139114,25.8244806456362,124.077232539093)) ;
#93361 = CARTESIAN_POINT('Ctrl Pts',(-18.3031245285065,25.8344758142623,123.892541794129)) ;
#93362 = CARTESIAN_POINT('Ctrl Pts',(-18.2364238705708,25.8445096975235,123.692438326714)) ;
#93363 = CARTESIAN_POINT('Ctrl Pts',(-18.205714018985,25.8543655675869,123.487510321506)) ;
#93364 = CARTESIAN_POINT('Ctrl Pts',(-18.2107938731432,25.864363113504,123.277414588518)) ;
#93365 = CARTESIAN_POINT('Ctrl Pts',(-18.2518456767253,25.8742712404033,123.073191361483)) ;
#93366 = CARTESIAN_POINT('Ctrl Pts',(-18.3281771028742,25.8842816119255,122.877061463729)) ;
#93367 = CARTESIAN_POINT('Ctrl Pts',(-18.4380159492977,25.8943120546729,122.697063911336)) ;
#93368 = CARTESIAN_POINT('Ctrl Pts',(-18.5745552119274,25.9041600072262,122.5414142025)) ;
#93369 = CARTESIAN_POINT('Ctrl Pts',(-18.7394363200053,25.9142226762471,122.408905143924)) ;
#93370 = CARTESIAN_POINT('Ctrl Pts',(-18.9218264083034,25.9241170517111,122.308852272964)) ;
#93371 = CARTESIAN_POINT('Ctrl Pts',(-19.1195394323681,25.9340588500292,122.241151655408)) ;
#93372 = CARTESIAN_POINT('Ctrl Pts',(-19.3273054241059,25.9440613437565,122.208523083542)) ;
#93373 = CARTESIAN_POINT('Ctrl Pts',(-19.5382116668081,25.9540961422634,122.212809762193)) ;
#93374 = CARTESIAN_POINT('Ctrl Pts',(-19.7413463382716,25.9639410262428,122.252542610422)) ;
#93375 = CARTESIAN_POINT('Ctrl Pts',(-19.9373601162425,25.9739268830608,122.327621634574)) ;
#93376 = CARTESIAN_POINT('Ctrl Pts',(-20.1165785383608,25.9838616972356,122.434952368301)) ;
#93377 = CARTESIAN_POINT('Ctrl Pts',(-20.2762122449541,25.9939191970209,122.573557383154)) ;
#93378 = CARTESIAN_POINT('Ctrl Pts',(-20.4065114706152,26.0037409554392,122.733766868605)) ;
#93379 = CARTESIAN_POINT('Ctrl Pts',(-20.5097347090899,26.0137966132232,122.918234290482)) ;
#93380 = CARTESIAN_POINT('Ctrl Pts',(-20.5782258756147,26.0237387954033,123.115721371548)) ;
#93381 = CARTESIAN_POINT('Ctrl Pts',(-20.6118871272014,26.033644004098,123.321218153653)) ;
#93382 = CARTESIAN_POINT('Ctrl Pts',(-20.6092537917906,26.0436857950604,123.532308255911)) ;
#93383 = CARTESIAN_POINT('Ctrl Pts',(-20.5705521089808,26.0535935695326,123.73698203017)) ;
#93384 = CARTESIAN_POINT('Ctrl Pts',(-20.4964939731295,26.0636050697602,123.934001627949)) ;
#93385 = CARTESIAN_POINT('Ctrl Pts',(-20.3887491022585,26.0736378301529,124.115324540153)) ;
#93386 = CARTESIAN_POINT('Ctrl Pts',(-20.2539283372818,26.0834883992878,124.272523599289)) ;
#93387 = CARTESIAN_POINT('Ctrl Pts',(-20.0918867933303,26.0934770088177,124.406059622827)) ;
#93388 = CARTESIAN_POINT('Ctrl Pts',(-19.9101964338395,26.1034056648418,124.508820927901)) ;
#93389 = CARTESIAN_POINT('Ctrl Pts',(-19.7123664598678,26.1133934110196,124.579225538772)) ;
#93390 = CARTESIAN_POINT('Ctrl Pts',(-19.5042772685736,26.1234293999554,124.614026056989)) ;
#93391 = CARTESIAN_POINT('Ctrl Pts',(-19.2970856456385,26.133284269769,124.612543958889)) ;
#93392 = CARTESIAN_POINT('Ctrl Pts',(-19.0903087822269,26.1432837110107,124.574850516544)) ;
#93393 = CARTESIAN_POINT('Ctrl Pts',(-18.8951319256074,26.1531787851908,124.502774169454)) ;
#93394 = CARTESIAN_POINT('Ctrl Pts',(-18.712492759328,26.1632394410305,124.396160191167)) ;
#93395 = CARTESIAN_POINT('Ctrl Pts',(-18.5544270484986,26.1730883152261,124.262395161111)) ;
#93396 = CARTESIAN_POINT('Ctrl Pts',(-18.4191734859892,26.1831170271894,124.100664930615)) ;
#93397 = CARTESIAN_POINT('Ctrl Pts',(-18.3145428694467,26.1931464277725,123.917602948853)) ;
#93398 = CARTESIAN_POINT('Ctrl Pts',(-18.2441983081728,26.2029866213893,123.723055479142)) ;
#93399 = CARTESIAN_POINT('Ctrl Pts',(-18.2077335916709,26.2129900439645,123.515958829332)) ;
#93400 = CARTESIAN_POINT('Ctrl Pts',(-18.207849919895,26.2229755810576,123.305996114384)) ;
#93401 = CARTESIAN_POINT('Ctrl Pts',(-18.2448224450821,26.2330165855444,123.098185958019)) ;
#93402 = CARTESIAN_POINT('Ctrl Pts',(-18.315637546413,26.2428601244856,122.903720935698)) ;
#93403 = CARTESIAN_POINT('Ctrl Pts',(-18.4202262131104,26.2528451554764,122.721750406657)) ;
#93404 = CARTESIAN_POINT('Ctrl Pts',(-18.5541826302326,26.2627846179984,122.561338916307)) ;
#93405 = CARTESIAN_POINT('Ctrl Pts',(-18.7155638139311,26.2728243502222,122.425330541335)) ;
#93406 = CARTESIAN_POINT('Ctrl Pts',(-18.8953261424376,26.2827125305394,122.320904799776)) ;
#93407 = CARTESIAN_POINT('Ctrl Pts',(-19.0923360066842,26.2927020462419,122.248179871716)) ;
#93408 = CARTESIAN_POINT('Ctrl Pts',(-19.29836965637,26.3026605968966,122.211042573258)) ;
#93409 = CARTESIAN_POINT('Ctrl Pts',(-19.506496121546,26.3125600040016,122.20972967354)) ;
#93410 = CARTESIAN_POINT('Ctrl Pts',(-19.7147275262977,26.3226085904179,122.245179238404)) ;
#93411 = CARTESIAN_POINT('Ctrl Pts',(-19.9106882308818,26.3325014093824,122.314976928487)) ;
#93412 = CARTESIAN_POINT('Ctrl Pts',(-20.0947008159812,26.3425725269122,122.419616587146)) ;
#93413 = CARTESIAN_POINT('Ctrl Pts',(-20.2538532201277,26.3523882208783,122.551030461718)) ;
#93414 = CARTESIAN_POINT('Ctrl Pts',(-20.3913677815839,26.3624545983756,122.711830813516)) ;
#93415 = CARTESIAN_POINT('Ctrl Pts',(-20.497080515863,26.3723535844574,122.891149584899)) ;
#93416 = CARTESIAN_POINT('Ctrl Pts',(-20.5712377326743,26.3824077644509,123.089035325503)) ;
#93417 = CARTESIAN_POINT('Ctrl Pts',(-20.6094217264944,26.3922785773836,123.293057111888)) ;
#93418 = CARTESIAN_POINT('Ctrl Pts',(-20.6116385942479,26.4023524782374,123.504781098235)) ;
#93419 = CARTESIAN_POINT('Ctrl Pts',(-20.5781656742403,26.4121726336241,123.708548551579)) ;
#93420 = CARTESIAN_POINT('Ctrl Pts',(-20.5082435413236,26.4222513405763,123.908510156717)) ;
#93421 = CARTESIAN_POINT('Ctrl Pts',(-20.4070109794574,26.4321029291151,124.089251298327)) ;
#93422 = CARTESIAN_POINT('Ctrl Pts',(-20.2731855957276,26.4421760456401,124.253326756013)) ;
#93423 = CARTESIAN_POINT('Ctrl Pts',(-20.1165101320345,26.4520185627359,124.388517157775)) ;
#93424 = CARTESIAN_POINT('Ctrl Pts',(-19.9366357026689,26.4619990242899,124.49652523591)) ;
#93425 = CARTESIAN_POINT('Ctrl Pts',(-19.7398462849515,26.4720172742807,124.571568687572)) ;
#93426 = CARTESIAN_POINT('Ctrl Pts',(-19.5358433540864,26.4819014344744,124.611196186289)) ;
#93427 = CARTESIAN_POINT('Ctrl Pts',(-19.3242969728162,26.4919665814494,124.614819305316)) ;
#93428 = CARTESIAN_POINT('Ctrl Pts',(-19.1199162896328,26.5018084050902,124.582500426852)) ;
#93429 = CARTESIAN_POINT('Ctrl Pts',(-18.9203549014018,26.5118378775511,124.51444423306)) ;
#93430 = CARTESIAN_POINT('Ctrl Pts',(-18.7359669975799,26.5218647328131,124.412277185117)) ;
#93431 = CARTESIAN_POINT('Ctrl Pts',(-18.5748099226721,26.5317079829236,124.282461831563)) ;
#93432 = CARTESIAN_POINT('Ctrl Pts',(-18.4355916456644,26.5417564225068,124.123583572549)) ;
#93433 = CARTESIAN_POINT('Ctrl Pts',(-18.3274329386578,26.5517059167547,123.944547268293)) ;
#93434 = CARTESIAN_POINT('Ctrl Pts',(-18.2517329103904,26.5616137724807,123.750483520398)) ;
#93435 = CARTESIAN_POINT('Ctrl Pts',(-18.2104800380329,26.5716732491306,123.543086602686)) ;
#93436 = CARTESIAN_POINT('Ctrl Pts',(-18.2056838550714,26.5815140585393,123.336232067944)) ;
#93437 = CARTESIAN_POINT('Ctrl Pts',(-18.2373097240745,26.5915762088401,123.127093681525)) ;
#93438 = CARTESIAN_POINT('Ctrl Pts',(-18.3038768776856,26.6014733699627,122.929948794933)) ;
#93439 = CARTESIAN_POINT('Ctrl Pts',(-18.4033896561337,26.6114045443667,122.746410755063)) ;
#93440 = CARTESIAN_POINT('Ctrl Pts',(-18.5348932882933,26.6214467480918,122.581254053194)) ;
#93441 = CARTESIAN_POINT('Ctrl Pts',(-18.6905332621863,26.6313333305222,122.443483756373)) ;
#93442 = CARTESIAN_POINT('Ctrl Pts',(-18.8694457020264,26.6413267662705,122.333371781551)) ;
#93443 = CARTESIAN_POINT('Ctrl Pts',(-19.0638389458024,26.6512712346287,122.25643179021)) ;
#93444 = CARTESIAN_POINT('Ctrl Pts',(-19.2687173484361,26.6612230508743,122.213994242932)) ;
#93445 = CARTESIAN_POINT('Ctrl Pts',(-19.4796376314532,26.6712604869887,122.207914894634)) ;
#93446 = CARTESIAN_POINT('Ctrl Pts',(-19.6852953687343,26.6811454461651,122.237889874322)) ;
#93447 = CARTESIAN_POINT('Ctrl Pts',(-19.8849208385928,26.691143564377,122.303615139944)) ;
#93448 = CARTESIAN_POINT('Ctrl Pts',(-20.0687823899887,26.701064496889,122.40213114507)) ;
#93449 = CARTESIAN_POINT('Ctrl Pts',(-20.2347433719469,26.7111057971111,122.532576201675)) ;
#93450 = CARTESIAN_POINT('Ctrl Pts',(-20.3736041235756,26.721012715501,122.687807479836)) ;
#93451 = CARTESIAN_POINT('Ctrl Pts',(-20.4842302721718,26.7309485072101,122.864990307838)) ;
#93452 = CARTESIAN_POINT('Ctrl Pts',(-20.5630380467698,26.740989401788,123.060813841052)) ;
#93453 = CARTESIAN_POINT('Ctrl Pts',(-20.606131212989,26.7508766035018,123.264168783375)) ;
#93454 = CARTESIAN_POINT('Ctrl Pts',(-20.6136841228083,26.7608688712634,123.474087428869)) ;
#93455 = CARTESIAN_POINT('Ctrl Pts',(-20.5847396526001,26.7708173922852,123.681235914656)) ;
#93456 = CARTESIAN_POINT('Ctrl Pts',(-20.5206329141074,26.7807541658629,123.880040207961)) ;
#93457 = CARTESIAN_POINT('Ctrl Pts',(-20.4227399059421,26.790737214004,124.065715809931)) ;
#93458 = CARTESIAN_POINT('Ctrl Pts',(-20.2930387524076,26.800780921614,124.232307345616)) ;
#93459 = CARTESIAN_POINT('Ctrl Pts',(-20.1400189052404,26.8106096147673,124.371201732946)) ;
#93460 = CARTESIAN_POINT('Ctrl Pts',(-19.9609582162376,26.8206843638968,124.484270411322)) ;
#93461 = CARTESIAN_POINT('Ctrl Pts',(-19.7689924318858,26.8305496896923,124.562839075184)) ;
#93462 = CARTESIAN_POINT('Ctrl Pts',(-19.5632221684136,26.8405718640493,124.608103780006)) ;
#93463 = CARTESIAN_POINT('Ctrl Pts',(-19.3525933509381,26.8505979172562,124.616438892034)) ;
#93464 = CARTESIAN_POINT('Ctrl Pts',(-19.1472930179978,26.8604516141025,124.588899906443)) ;
#93465 = CARTESIAN_POINT('Ctrl Pts',(-18.9475623242253,26.8704110188554,124.526053167389)) ;
#93466 = CARTESIAN_POINT('Ctrl Pts',(-18.7604973127127,26.8804492645603,124.428392120626)) ;
#93467 = CARTESIAN_POINT('Ctrl Pts',(-18.595707038093,26.8903234487224,124.302108746629)) ;
#93468 = CARTESIAN_POINT('Ctrl Pts',(-18.4526112031336,26.9003932318603,124.146135573112)) ;
#93469 = CARTESIAN_POINT('Ctrl Pts',(-18.3413269230795,26.910226486881,123.971898783901)) ;
#93470 = CARTESIAN_POINT('Ctrl Pts',(-18.2598539373914,26.9202569130127,123.777409910827)) ;
#93471 = CARTESIAN_POINT('Ctrl Pts',(-18.2139770922715,26.9302885251997,123.571552183316)) ;
#93472 = CARTESIAN_POINT('Ctrl Pts',(-18.2043014628448,26.9401182220543,123.365141874546)) ;
#93473 = CARTESIAN_POINT('Ctrl Pts',(-18.2304203523033,26.9501076639568,123.156756810279)) ;
#93474 = CARTESIAN_POINT('Ctrl Pts',(-18.2931717636035,26.9601515559725,122.955144115483)) ;
#93475 = CARTESIAN_POINT('Ctrl Pts',(-18.3874551637717,26.9699731177417,122.771448988579)) ;
#93476 = CARTESIAN_POINT('Ctrl Pts',(-18.5145023549983,26.9800086893659,122.603007690826)) ;
#93477 = CARTESIAN_POINT('Ctrl Pts',(-18.6691989364535,26.9900379636477,122.459740110803)) ;
#93478 = CARTESIAN_POINT('Ctrl Pts',(-18.8426716613453,26.9998718007664,122.347266613141)) ;
#93479 = CARTESIAN_POINT('Ctrl Pts',(-19.0371543491445,27.0099241968545,122.26460097273)) ;
#93480 = CARTESIAN_POINT('Ctrl Pts',(-19.2407489171137,27.0198609638051,122.217766396637)) ;
#93481 = CARTESIAN_POINT('Ctrl Pts',(-19.4492892613563,27.0297951987843,122.206457880832)) ;
#93482 = CARTESIAN_POINT('Ctrl Pts',(-19.6584787688609,27.0398189621111,122.231885051993)) ;
#93483 = CARTESIAN_POINT('Ctrl Pts',(-19.8573566469168,27.0497053034958,122.292260658762)) ;
#93484 = CARTESIAN_POINT('Ctrl Pts',(-20.044884241241,27.0596943522627,122.386795146687)) ;
#93485 = CARTESIAN_POINT('Ctrl Pts',(-20.2137587515915,27.0697355729601,122.513457842224)) ;
#93486 = CARTESIAN_POINT('Ctrl Pts',(-20.3553226201596,27.079568213138,122.664084460365)) ;
#93487 = CARTESIAN_POINT('Ctrl Pts',(-20.4709452079467,27.089562142446,122.839511283669)) ;
#93488 = CARTESIAN_POINT('Ctrl Pts',(-20.5542369537336,27.0995913501265,123.033209534524)) ;
#93489 = CARTESIAN_POINT('Ctrl Pts',(-20.6022223085313,27.1094671618306,123.235220662591)) ;
#93490 = CARTESIAN_POINT('Ctrl Pts',(-20.6147833778332,27.119466388802,123.445032111531)) ;
#93491 = CARTESIAN_POINT('Ctrl Pts',(-20.5911307340941,27.1293758699577,123.652044212278)) ;
#93492 = CARTESIAN_POINT('Ctrl Pts',(-20.5310228623009,27.1394291002586,123.85464405997)) ;
#93493 = CARTESIAN_POINT('Ctrl Pts',(-20.4384382021735,27.1492997168097,124.040371924575)) ;
#93494 = CARTESIAN_POINT('Ctrl Pts',(-20.3135085808993,27.1593213785417,124.210019681239)) ;
#93495 = CARTESIAN_POINT('Ctrl Pts',(-20.1606599163486,27.1693441917228,124.355074884069)) ;
#93496 = CARTESIAN_POINT('Ctrl Pts',(-19.9878844325135,27.1792113561828,124.469859477735)) ;
#93497 = CARTESIAN_POINT('Ctrl Pts',(-19.7955493981892,27.1892047984027,124.554411463994)) ;
#93498 = CARTESIAN_POINT('Ctrl Pts',(-19.5905834003514,27.199236472003,124.604073131123)) ;
#93499 = CARTESIAN_POINT('Ctrl Pts',(-19.3835855502156,27.209102907116,124.617490989983)) ;
#93500 = CARTESIAN_POINT('Ctrl Pts',(-19.174870121098,27.2190903576491,124.594828115843)) ;
#93501 = CARTESIAN_POINT('Ctrl Pts',(-18.9740333028024,27.2290352874771,124.536610653904)) ;
#93502 = CARTESIAN_POINT('Ctrl Pts',(-18.7845669174795,27.2390801825322,124.443394505868)) ;
#93503 = CARTESIAN_POINT('Ctrl Pts',(-18.6171298557573,27.248942244218,124.321093509513)) ;
#93504 = CARTESIAN_POINT('Ctrl Pts',(-18.4713020979858,27.2589339670049,124.16992654863)) ;
#93505 = CARTESIAN_POINT('Ctrl Pts',(-18.3546885531147,27.2688661812449,123.996714378362)) ;
#93506 = CARTESIAN_POINT('Ctrl Pts',(-18.269419645282,27.2788054998106,123.805941861315)) ;
#93507 = CARTESIAN_POINT('Ctrl Pts',(-18.2182240150851,27.2888496745865,123.601084899487)) ;
#93508 = CARTESIAN_POINT('Ctrl Pts',(-18.2035200670347,27.2987202286514,123.394096871546)) ;
#93509 = CARTESIAN_POINT('Ctrl Pts',(-18.2245812279825,27.3086852110056,123.185662484473)) ;
#93510 = CARTESIAN_POINT('Ctrl Pts',(-18.2821983669197,27.3187159138954,122.982815593457)) ;
#93511 = CARTESIAN_POINT('Ctrl Pts',(-18.3726338901219,27.3286082539206,122.795512181265)) ;
#93512 = CARTESIAN_POINT('Ctrl Pts',(-18.4961446714917,27.3386614870806,122.624043166509)) ;
#93513 = CARTESIAN_POINT('Ctrl Pts',(-18.6449201037129,27.3485427315573,122.479010000241)) ;
#93514 = CARTESIAN_POINT('Ctrl Pts',(-18.8191075332246,27.3585758524284,122.360127390189)) ;
#93515 = CARTESIAN_POINT('Ctrl Pts',(-19.0083749934577,27.3684570627034,122.274409088522)) ;
#93516 = CARTESIAN_POINT('Ctrl Pts',(-19.2132499375298,27.3785191384728,122.221874637997)) ;
#93517 = CARTESIAN_POINT('Ctrl Pts',(-19.4198941729344,27.3883761968545,122.205962714109)) ;
#93518 = CARTESIAN_POINT('Ctrl Pts',(-19.6290171503523,27.3983707521435,122.226026766799)) ;
#93519 = CARTESIAN_POINT('Ctrl Pts',(-19.8301684040698,27.408296639679,122.281656756404)) ;
#93520 = CARTESIAN_POINT('Ctrl Pts',(-20.0204729359765,27.4183216596743,122.372190073882)) ;
#93521 = CARTESIAN_POINT('Ctrl Pts',(-20.1900416051017,27.428219036778,122.492787717248)) ;
#93522 = CARTESIAN_POINT('Ctrl Pts',(-20.337791395253,27.4382092738588,122.642064176377)) ;
#93523 = CARTESIAN_POINT('Ctrl Pts',(-20.4575937675202,27.4482458866676,122.815752566344)) ;
#93524 = CARTESIAN_POINT('Ctrl Pts',(-20.5440949710146,27.4580957700856,123.003904331342)) ;
#93525 = CARTESIAN_POINT('Ctrl Pts',(-20.5978342575629,27.4680993869881,123.207208424136)) ;
#93526 = CARTESIAN_POINT('Ctrl Pts',(-20.6153220020921,27.4780887987532,123.416522213151)) ;
#93527 = CARTESIAN_POINT('Ctrl Pts',(-20.596019200136,27.4881075600981,123.626239460963)) ;
#93528 = CARTESIAN_POINT('Ctrl Pts',(-20.5232688664798,27.5013262354791,123.894499714109)) ;
#93529 = CARTESIAN_POINT('Ctrl Pts',(-20.3813539407397,27.5146365427238,124.139308036254)) ;
#93530 = CARTESIAN_POINT('Ctrl Pts',(-20.1842224998878,27.5278742089498,124.33573047354)) ;
#93531 = CARTESIAN_POINT('Ctrl Pts',(-20.0135550279124,27.5377939043605,124.45559248642)) ;
#93532 = CARTESIAN_POINT('Ctrl Pts',(-19.8220507976566,27.5478467713591,124.544956171201)) ;
#93533 = CARTESIAN_POINT('Ctrl Pts',(-19.6219766811352,27.5577021796884,124.598870302969)) ;
#93534 = CARTESIAN_POINT('Ctrl Pts',(-19.4118114679212,27.5677408113649,124.617912525349)) ;
#93535 = CARTESIAN_POINT('Ctrl Pts',(-19.1331437800941,27.581042993632,124.594057344109)) ;
#93536 = CARTESIAN_POINT('Ctrl Pts',(-18.8021120088637,27.5975880067148,124.475053992695)) ;
#93537 = CARTESIAN_POINT('Ctrl Pts',(-18.5297401940674,27.614240022791,124.2488161865)) ;
#93538 = CARTESIAN_POINT('Ctrl Pts',(-18.3691043286755,27.6274631136963,124.021959188954)) ;
#93539 = CARTESIAN_POINT('Ctrl Pts',(-18.279074765685,27.6374240732556,123.832881312923)) ;
#93540 = CARTESIAN_POINT('Ctrl Pts',(-18.2231429882255,27.6474488700067,123.62969511615)) ;
#93541 = CARTESIAN_POINT('Ctrl Pts',(-18.1966274879579,27.6606733174025,123.352901549836)) ;
#93542 = CARTESIAN_POINT('Ctrl Pts',(-18.2547427228421,27.6773071021016,123.004090311411)) ;
#93543 = CARTESIAN_POINT('Ctrl Pts',(-18.462654194708,27.6972097688266,122.635456439597)) ;
#93544 = CARTESIAN_POINT('Ctrl Pts',(-18.7834264639891,27.7171099966084,122.359556189311)) ;
#93545 = CARTESIAN_POINT('Ctrl Pts',(-19.1793576793878,27.7370274841399,122.209266164679)) ;
#93546 = CARTESIAN_POINT('Ctrl Pts',(-19.6030851389282,27.7569570099568,122.20284220471)) ;
#93547 = CARTESIAN_POINT('Ctrl Pts',(-20.0042034113001,27.7769192778431,122.341703290719)) ;
#93548 = CARTESIAN_POINT('Ctrl Pts',(-20.3326268774774,27.7968094727953,122.608069909733)) ;
#93549 = CARTESIAN_POINT('Ctrl Pts',(-20.5514322995273,27.8166997175416,122.970098508782)) ;
#93550 = CARTESIAN_POINT('Ctrl Pts',(-20.6334273803088,27.836774090104,123.388925968865)) ;
#93551 = CARTESIAN_POINT('Ctrl Pts',(-20.5686426007761,27.8565594674643,123.804655277717)) ;
#93552 = CARTESIAN_POINT('Ctrl Pts',(-20.3652778235273,27.8765213415315,124.177163759721)) ;
#93553 = CARTESIAN_POINT('Ctrl Pts',(-20.0460050432722,27.896501317022,124.45743847941)) ;
#93554 = CARTESIAN_POINT('Ctrl Pts',(-19.6538578338986,27.9163137468999,124.61141438612)) ;
#93555 = CARTESIAN_POINT('Ctrl Pts',(-19.229262390193,27.9362938549902,124.622968495663)) ;
#93556 = CARTESIAN_POINT('Ctrl Pts',(-18.8278347516187,27.9561882385874,124.48928119194)) ;
#93557 = CARTESIAN_POINT('Ctrl Pts',(-18.4954921617374,27.9761151665647,124.22662108976)) ;
#93558 = CARTESIAN_POINT('Ctrl Pts',(-18.2725085713634,27.9960100238659,123.867030699903)) ;
#93559 = CARTESIAN_POINT('Ctrl Pts',(-18.1854382342553,28.0160492174695,123.449977253235)) ;
#93560 = CARTESIAN_POINT('Ctrl Pts',(-18.2454140966573,28.0358891853803,123.032366941405)) ;
#93561 = CARTESIAN_POINT('Ctrl Pts',(-18.4440438223456,28.0558040023444,122.658441047315)) ;
#93562 = CARTESIAN_POINT('Ctrl Pts',(-18.7589841925782,28.0757462477406,122.374568986743)) ;
#93563 = CARTESIAN_POINT('Ctrl Pts',(-19.1503542322998,28.0956182958551,122.215058271776)) ;
#93564 = CARTESIAN_POINT('Ctrl Pts',(-19.5753982482705,28.1156293608092,122.198881833983)) ;
#93565 = CARTESIAN_POINT('Ctrl Pts',(-19.976924777418,28.1354408851129,122.326892971449)) ;
#93566 = CARTESIAN_POINT('Ctrl Pts',(-20.3149986104091,28.1555360970762,122.587908851649)) ;
#93567 = CARTESIAN_POINT('Ctrl Pts',(-20.540244932059,28.175316820996,122.943300131366)) ;
#93568 = CARTESIAN_POINT('Ctrl Pts',(-20.632541211871,28.1953078966388,123.358060932043)) ;
#93569 = CARTESIAN_POINT('Ctrl Pts',(-20.5777379932695,28.2151898356818,123.777357946779)) ;
#93570 = CARTESIAN_POINT('Ctrl Pts',(-20.3829565043216,28.2351424401851,124.154169171674)) ;
#93571 = CARTESIAN_POINT('Ctrl Pts',(-20.0720352876919,28.2550413089158,124.441191772874)) ;
#93572 = CARTESIAN_POINT('Ctrl Pts',(-19.6822521549889,28.2749347087253,124.605274930316)) ;
#93573 = CARTESIAN_POINT('Ctrl Pts',(-19.2594119704509,28.2948438395654,124.627173961872)) ;
#93574 = CARTESIAN_POINT('Ctrl Pts',(-18.8522720945946,28.3148759393289,124.502181134798)) ;
#93575 = CARTESIAN_POINT('Ctrl Pts',(-18.5715058354891,28.3314080124984,124.290597893153)) ;
#93576 = CARTESIAN_POINT('Ctrl Pts',(-18.3986989765231,28.3447433531043,124.06986111569)) ;
#93577 = CARTESIAN_POINT('Ctrl Pts',(-18.3010384376066,28.3545859116441,123.887414284966)) ;
#93578 = CARTESIAN_POINT('Ctrl Pts',(-18.2349738070104,28.364637818494,123.686701670905)) ;
#93579 = CARTESIAN_POINT('Ctrl Pts',(-18.1952065129706,28.3778863328849,123.411043207663)) ;
#93580 = CARTESIAN_POINT('Ctrl Pts',(-18.2364119327605,28.3944855078326,123.060489114664)) ;
#93581 = CARTESIAN_POINT('Ctrl Pts',(-18.3945320732476,28.4110742936277,122.745246270374)) ;
#93582 = CARTESIAN_POINT('Ctrl Pts',(-18.5797843255288,28.4243501099696,122.536445693784)) ;
#93583 = CARTESIAN_POINT('Ctrl Pts',(-18.7438859525293,28.4343239607634,122.4059105653)) ;
#93584 = CARTESIAN_POINT('Ctrl Pts',(-18.9292775705451,28.4443529928558,122.305499193489)) ;
#93585 = CARTESIAN_POINT('Ctrl Pts',(-19.1264647249251,28.4542431183577,122.239514286115)) ;
#93586 = CARTESIAN_POINT('Ctrl Pts',(-19.3341633471274,28.4642355966292,122.208177516446)) ;
#93587 = CARTESIAN_POINT('Ctrl Pts',(-19.5433409170049,28.4741868117266,122.213247363974)) ;
#93588 = CARTESIAN_POINT('Ctrl Pts',(-19.7503773115582,28.4842353134817,122.255121671424)) ;
#93589 = CARTESIAN_POINT('Ctrl Pts',(-19.9430718837078,28.4940766630984,122.330508480184)) ;
#93590 = CARTESIAN_POINT('Ctrl Pts',(-20.1225389941562,28.5040629541187,122.439381413048)) ;
#93591 = CARTESIAN_POINT('Ctrl Pts',(-20.2797114114342,28.5139995658473,122.577040974791)) ;
#93592 = CARTESIAN_POINT('Ctrl Pts',(-20.4119681889468,28.5240494412148,122.74177821394)) ;
#93593 = CARTESIAN_POINT('Ctrl Pts',(-20.5117487646178,28.5338998997503,122.923259406257)) ;
#93594 = CARTESIAN_POINT('Ctrl Pts',(-20.5798319652677,28.543871836703,123.121510243996)) ;
#93595 = CARTESIAN_POINT('Ctrl Pts',(-20.6125111709449,28.5538672936351,123.329122137551)) ;
#93596 = CARTESIAN_POINT('Ctrl Pts',(-20.6083934035512,28.5639001006882,123.539989223304)) ;
#93597 = CARTESIAN_POINT('Ctrl Pts',(-20.5686972957421,28.5737599872782,123.743449587553)) ;
#93598 = CARTESIAN_POINT('Ctrl Pts',(-20.493679365146,28.5837490678434,123.939575708559)) ;
#93599 = CARTESIAN_POINT('Ctrl Pts',(-20.3863550900639,28.5936805470526,124.118678024695)) ;
#93600 = CARTESIAN_POINT('Ctrl Pts',(-20.2490702128718,28.6036664064985,124.277521451169)) ;
#93601 = CARTESIAN_POINT('Ctrl Pts',(-20.0852249792083,28.6137045571457,124.410502596884)) ;
#93602 = CARTESIAN_POINT('Ctrl Pts',(-19.9044472059089,28.6235526476501,124.51145879854)) ;
#93603 = CARTESIAN_POINT('Ctrl Pts',(-19.7047579306307,28.6336135561681,124.581118064971)) ;
#93604 = CARTESIAN_POINT('Ctrl Pts',(-19.4993889315201,28.6435084033261,124.614351432884)) ;
#93605 = CARTESIAN_POINT('Ctrl Pts',(-19.290422284636,28.6534500753711,124.61196471871)) ;
#93606 = CARTESIAN_POINT('Ctrl Pts',(-19.0837190965764,28.6634526024966,124.573165459585)) ;
#93607 = CARTESIAN_POINT('Ctrl Pts',(-18.8864143900725,28.673487393684,124.498528915288)) ;
#93608 = CARTESIAN_POINT('Ctrl Pts',(-18.7082976391662,28.6833322735432,124.393092627413)) ;
#93609 = CARTESIAN_POINT('Ctrl Pts',(-18.5487226700083,28.6933181541616,124.256732099038)) ;
#93610 = CARTESIAN_POINT('Ctrl Pts',(-18.41576941784,28.7032528772548,124.095604644476)) ;
#93611 = CARTESIAN_POINT('Ctrl Pts',(-18.3117412138791,28.713310717566,123.911553889218)) ;
#93612 = CARTESIAN_POINT('Ctrl Pts',(-18.2425809970135,28.7231312049625,123.716996800082)) ;
#93613 = CARTESIAN_POINT('Ctrl Pts',(-18.207077110529,28.7331916063077,123.508522426706)) ;
#93614 = CARTESIAN_POINT('Ctrl Pts',(-18.2085773478426,28.7431225718606,123.299723942256)) ;
#93615 = CARTESIAN_POINT('Ctrl Pts',(-18.245873377285,28.753061434197,123.094155479306)) ;
#93616 = CARTESIAN_POINT('Ctrl Pts',(-18.3185218475417,28.7630471651232,122.897169941774)) ;
#93617 = CARTESIAN_POINT('Ctrl Pts',(-18.4248524147212,28.7730715505507,122.715235116159)) ;
#93618 = CARTESIAN_POINT('Ctrl Pts',(-18.5592956161916,28.7829748349039,122.556229872053)) ;
#93619 = CARTESIAN_POINT('Ctrl Pts',(-18.7218419116847,28.7930348394819,122.420962440775)) ;
#93620 = CARTESIAN_POINT('Ctrl Pts',(-18.9014184995494,28.802878108551,122.31808641314)) ;
#93621 = CARTESIAN_POINT('Ctrl Pts',(-19.098834322819,28.8128686741587,122.246460343991)) ;
#93622 = CARTESIAN_POINT('Ctrl Pts',(-19.3044348672317,28.8227968059375,122.210453578129)) ;
#93623 = CARTESIAN_POINT('Ctrl Pts',(-19.5144210408558,28.8327846930185,122.210327947691)) ;
#93624 = CARTESIAN_POINT('Ctrl Pts',(-19.7221546515197,28.8428206425871,122.247189649512)) ;
#93625 = CARTESIAN_POINT('Ctrl Pts',(-19.9168982030281,28.852675528966,122.317939833791)) ;
#93626 = CARTESIAN_POINT('Ctrl Pts',(-20.099129252199,28.8626749433138,122.422673266323)) ;
#93627 = CARTESIAN_POINT('Ctrl Pts',(-20.2589220409907,28.8725701085043,122.555925365975)) ;
#93628 = CARTESIAN_POINT('Ctrl Pts',(-20.3953335885789,28.8826304271963,122.717517984113)) ;
#93629 = CARTESIAN_POINT('Ctrl Pts',(-20.4995231303443,28.8924805589724,122.896499760927)) ;
#93630 = CARTESIAN_POINT('Ctrl Pts',(-20.5728206210608,28.9025111294226,123.094215195434)) ;
#93631 = CARTESIAN_POINT('Ctrl Pts',(-20.6101551335493,28.9125252800954,123.301419328339)) ;
#93632 = CARTESIAN_POINT('Ctrl Pts',(-20.6112719043652,28.9224182136408,123.509400270056)) ;
#93633 = CARTESIAN_POINT('Ctrl Pts',(-20.5761577703993,28.9324077276311,123.71643445623)) ;
#93634 = CARTESIAN_POINT('Ctrl Pts',(-20.5059948079295,28.9423614982835,123.913612659648)) ;
#93635 = CARTESIAN_POINT('Ctrl Pts',(-20.4015456859858,28.9524092669441,124.097194214206)) ;
#93636 = CARTESIAN_POINT('Ctrl Pts',(-20.2697350876435,28.9622509933839,124.256700935986)) ;
#93637 = CARTESIAN_POINT('Ctrl Pts',(-20.1102649496919,28.9722365102067,124.393174748905)) ;
#93638 = CARTESIAN_POINT('Ctrl Pts',(-19.9303421294312,28.9821758419022,124.499490582477)) ;
#93639 = CARTESIAN_POINT('Ctrl Pts',(-19.7327438594632,28.9922156115997,124.573634327147)) ;
#93640 = CARTESIAN_POINT('Ctrl Pts',(-19.5283969535556,29.0021037728485,124.611863915237)) ;
#93641 = CARTESIAN_POINT('Ctrl Pts',(-19.3184081587635,29.0120933273509,124.614447514576)) ;
#93642 = CARTESIAN_POINT('Ctrl Pts',(-19.111830298825,29.0220517418745,124.580478875303)) ;
#93643 = CARTESIAN_POINT('Ctrl Pts',(-18.9152650713988,29.0319516547039,124.512040435847)) ;
#93644 = CARTESIAN_POINT('Ctrl Pts',(-18.7309320569869,29.0419983543538,124.408967920607)) ;
#93645 = CARTESIAN_POINT('Ctrl Pts',(-18.5695640219657,29.0518982146594,124.277476297858)) ;
#93646 = CARTESIAN_POINT('Ctrl Pts',(-18.4313829008868,29.0619496188649,124.117644033422)) ;
#93647 = CARTESIAN_POINT('Ctrl Pts',(-18.3247938377839,29.071830655786,123.939309454891)) ;
#93648 = CARTESIAN_POINT('Ctrl Pts',(-18.2496549087805,29.0818304879635,123.743005230981)) ;
#93649 = CARTESIAN_POINT('Ctrl Pts',(-18.2098864002276,29.0917484909484,123.538288222219)) ;
#93650 = CARTESIAN_POINT('Ctrl Pts',(-18.2062893402772,29.101799796823,123.327044380579)) ;
#93651 = CARTESIAN_POINT('Ctrl Pts',(-18.2385895898733,29.1116696202145,123.122034275269)) ;
#93652 = CARTESIAN_POINT('Ctrl Pts',(-18.3073743298631,29.1217437862648,122.921775498464)) ;
#93653 = CARTESIAN_POINT('Ctrl Pts',(-18.4071229719738,29.1315638704064,122.740968848258)) ;
#93654 = CARTESIAN_POINT('Ctrl Pts',(-18.5399452806073,29.1416425971423,122.575947060432)) ;
#93655 = CARTESIAN_POINT('Ctrl Pts',(-18.6958377939681,29.1514941777918,122.439518109468)) ;
#93656 = CARTESIAN_POINT('Ctrl Pts',(-18.8768647285279,29.1615673060902,122.329703311083)) ;
#93657 = CARTESIAN_POINT('Ctrl Pts',(-19.0697539715149,29.1714097839817,122.254755402957)) ;
#93658 = CARTESIAN_POINT('Ctrl Pts',(-19.2754083401487,29.1813903905797,122.213189337778)) ;
#93659 = CARTESIAN_POINT('Ctrl Pts',(-19.4859556253967,29.1914080995985,122.208340236175)) ;
#93660 = CARTESIAN_POINT('Ctrl Pts',(-19.6914902087443,29.2012942786359,122.239308640532)) ;
#93661 = CARTESIAN_POINT('Ctrl Pts',(-19.891914245863,29.2113518912083,122.306617578102)) ;
#93662 = CARTESIAN_POINT('Ctrl Pts',(-20.0742975022799,29.2212282845804,122.405879044779)) ;
#93663 = CARTESIAN_POINT('Ctrl Pts',(-20.2389379215443,29.2312233127309,122.536433065238)) ;
#93664 = CARTESIAN_POINT('Ctrl Pts',(-20.3785081239884,29.2412440595769,122.694246111613)) ;
#93665 = CARTESIAN_POINT('Ctrl Pts',(-20.4874550726902,29.2511461282432,122.871631017611)) ;
#93666 = CARTESIAN_POINT('Ctrl Pts',(-20.5649217144082,29.2611368680629,123.066861291378)) ;
#93667 = CARTESIAN_POINT('Ctrl Pts',(-20.6070427330823,29.2711000642732,123.272029769209)) ;
#93668 = CARTESIAN_POINT('Ctrl Pts',(-20.6133815278886,29.2810042485733,123.480169259069)) ;
#93669 = CARTESIAN_POINT('Ctrl Pts',(-20.5828416977269,29.2910647089642,123.689429189581)) ;
#93670 = CARTESIAN_POINT('Ctrl Pts',(-20.5181178875756,29.300905254835,123.885951501947)) ;
#93671 = CARTESIAN_POINT('Ctrl Pts',(-20.418311802327,29.3109674755468,124.072440554193)) ;
#93672 = CARTESIAN_POINT('Ctrl Pts',(-20.2895938220547,29.3208646185633,124.23593029093)) ;
#93673 = CARTESIAN_POINT('Ctrl Pts',(-20.1343856308271,29.3307957949805,124.375570781385)) ;
#93674 = CARTESIAN_POINT('Ctrl Pts',(-19.9551847138739,29.3408380087591,124.487181178999)) ;
#93675 = CARTESIAN_POINT('Ctrl Pts',(-19.7624071884746,29.3507245489619,124.564908193393)) ;
#93676 = CARTESIAN_POINT('Ctrl Pts',(-19.5569568086276,29.3607181435673,124.608773532661)) ;
#93677 = CARTESIAN_POINT('Ctrl Pts',(-19.3480261657817,29.3706620187248,124.616231477838)) ;
#93678 = CARTESIAN_POINT('Ctrl Pts',(-19.1406146804274,29.3806225548397,124.587525954481)) ;
#93679 = CARTESIAN_POINT('Ctrl Pts',(-18.9405437862277,29.3906191581624,124.523120304653)) ;
#93680 = CARTESIAN_POINT('Ctrl Pts',(-18.7541801489327,29.4006522411169,124.424343515166)) ;
#93681 = CARTESIAN_POINT('Ctrl Pts',(-18.5906535250111,29.4105034098184,124.297265234718)) ;
#93682 = CARTESIAN_POINT('Ctrl Pts',(-18.4496497544564,29.4204659005173,124.142407012302)) ;
#93683 = CARTESIAN_POINT('Ctrl Pts',(-18.3371454253762,29.4304943289351,123.964090346421)) ;
#93684 = CARTESIAN_POINT('Ctrl Pts',(-18.258197296594,29.4404046962996,123.771290942474)) ;
#93685 = CARTESIAN_POINT('Ctrl Pts',(-18.2132772397129,29.4503395639147,123.56731028171)) ;
#93686 = CARTESIAN_POINT('Ctrl Pts',(-18.2045597757948,29.4603807058938,123.35640066755)) ;
#93687 = CARTESIAN_POINT('Ctrl Pts',(-18.2320230286963,29.4702678420969,123.150352720058)) ;
#93688 = CARTESIAN_POINT('Ctrl Pts',(-18.295171910792,29.4802601245003,122.950015162677)) ;
#93689 = CARTESIAN_POINT('Ctrl Pts',(-18.3917861917968,29.4902086524655,122.76450500273)) ;
#93690 = CARTESIAN_POINT('Ctrl Pts',(-18.5187400411332,29.5001453836277,122.598627806259)) ;
#93691 = CARTESIAN_POINT('Ctrl Pts',(-18.6731408343567,29.5101285944876,122.45643033864)) ;
#93692 = CARTESIAN_POINT('Ctrl Pts',(-18.851110948505,29.5201716936375,122.342866870043)) ;
#93693 = CARTESIAN_POINT('Ctrl Pts',(-19.0418426894045,29.5300026579124,122.263194748433)) ;
#93694 = CARTESIAN_POINT('Ctrl Pts',(-19.2483822535319,29.5400755102984,122.21659540203)) ;
#93695 = CARTESIAN_POINT('Ctrl Pts',(-19.4555494026138,29.5499396380101,122.206807368119)) ;
#93696 = CARTESIAN_POINT('Ctrl Pts',(-19.6646004617306,29.559961840145,122.233040551303)) ;
#93697 = CARTESIAN_POINT('Ctrl Pts',(-19.8658933921423,29.5699890331134,122.295687395274)) ;
#93698 = CARTESIAN_POINT('Ctrl Pts',(-20.0501682924116,29.5798446270804,122.390377333857)) ;
#93699 = CARTESIAN_POINT('Ctrl Pts',(-20.2172985588075,29.5898017989457,122.516433218997)) ;
#93700 = CARTESIAN_POINT('Ctrl Pts',(-20.3608933785458,29.5998406429441,122.671082957337)) ;
#93701 = CARTESIAN_POINT('Ctrl Pts',(-20.4739033940063,29.6097146668197,122.845240474739)) ;
#93702 = CARTESIAN_POINT('Ctrl Pts',(-20.5565361370567,29.6197844928101,123.040115238253)) ;
#93703 = CARTESIAN_POINT('Ctrl Pts',(-20.6030779835527,29.6296177367074,123.241551193442)) ;
#93704 = CARTESIAN_POINT('Ctrl Pts',(-20.6147495285708,29.6396481644804,123.452092271116)) ;
#93705 = CARTESIAN_POINT('Ctrl Pts',(-20.5890726666387,29.6496797812255,123.661431321394)) ;
#93706 = CARTESIAN_POINT('Ctrl Pts',(-20.52909832052,29.6595094582063,123.859172832372)) ;
#93707 = CARTESIAN_POINT('Ctrl Pts',(-20.4347319780937,29.6694989750462,124.046795681918)) ;
#93708 = CARTESIAN_POINT('Ctrl Pts',(-20.3081181811144,29.679542587186,124.2157670466)) ;
#93709 = CARTESIAN_POINT('Ctrl Pts',(-20.1577705367842,29.6893651935213,124.357328493109)) ;
#93710 = CARTESIAN_POINT('Ctrl Pts',(-19.981608723437,29.6994034234205,124.473517346011)) ;
#93711 = CARTESIAN_POINT('Ctrl Pts',(-19.7882588157214,29.7094144582124,124.556686172734)) ;
#93712 = CARTESIAN_POINT('Ctrl Pts',(-19.5858185589827,29.7193121891796,124.604791883907)) ;
#93713 = CARTESIAN_POINT('Ctrl Pts',(-19.3761865286974,29.72930181703,124.617404592721)) ;
#93714 = CARTESIAN_POINT('Ctrl Pts',(-19.1682644871485,29.739257607476,124.593435204746)) ;
#93715 = CARTESIAN_POINT('Ctrl Pts',(-18.9681109946795,29.7491850060381,124.53427779116)) ;
#93716 = CARTESIAN_POINT('Ctrl Pts',(-18.7794620969067,29.759210601148,124.440297308764)) ;
#93717 = CARTESIAN_POINT('Ctrl Pts',(-18.6122766523615,29.7690964518175,124.316833192583)) ;
#93718 = CARTESIAN_POINT('Ctrl Pts',(-18.4672078455864,29.7790856316617,124.164980786501)) ;
#93719 = CARTESIAN_POINT('Ctrl Pts',(-18.3504739229804,29.7891268187653,123.989097081875)) ;
#93720 = CARTESIAN_POINT('Ctrl Pts',(-18.2674956322341,29.7989594622413,123.799773766715)) ;
#93721 = CARTESIAN_POINT('Ctrl Pts',(-18.2172642416538,29.8089534119507,123.595763802256)) ;
#93722 = CARTESIAN_POINT('Ctrl Pts',(-18.2036130491131,29.8189825347273,123.385360239602)) ;
#93723 = CARTESIAN_POINT('Ctrl Pts',(-18.2260199316204,29.8288586656459,123.178935368539)) ;
#93724 = CARTESIAN_POINT('Ctrl Pts',(-18.2843970103714,29.838856700663,122.977040721748)) ;
#93725 = CARTESIAN_POINT('Ctrl Pts',(-18.3760423191995,29.8487706304217,122.789820229446)) ;
#93726 = CARTESIAN_POINT('Ctrl Pts',(-18.5003433731899,29.8588138181595,122.619168157881)) ;
#93727 = CARTESIAN_POINT('Ctrl Pts',(-18.6502274266148,29.8687136602998,122.474753639408)) ;
#93728 = CARTESIAN_POINT('Ctrl Pts',(-18.8242469481258,29.8787049271078,122.357118255651)) ;
#93729 = CARTESIAN_POINT('Ctrl Pts',(-19.0169820186433,29.8887370292398,122.27146823907)) ;
#93730 = CARTESIAN_POINT('Ctrl Pts',(-19.2182167130968,29.8986039101946,122.221158081447)) ;
#93731 = CARTESIAN_POINT('Ctrl Pts',(-19.4277225562127,29.9085957014827,122.205867869987)) ;
#93732 = CARTESIAN_POINT('Ctrl Pts',(-19.6374978319252,29.9186278173942,122.227678697654)) ;
#93733 = CARTESIAN_POINT('Ctrl Pts',(-19.8370434622058,29.9284941341943,122.284323905425)) ;
#93734 = CARTESIAN_POINT('Ctrl Pts',(-20.0261335324257,29.9384816156679,122.37554305375)) ;
#93735 = CARTESIAN_POINT('Ctrl Pts',(-20.1958973076224,29.9484265400468,122.497628705408)) ;
#93736 = CARTESIAN_POINT('Ctrl Pts',(-20.3432317683155,29.9584714259575,122.648887749471)) ;
#93737 = CARTESIAN_POINT('Ctrl Pts',(-20.4600715091523,29.96833352967,122.820180932939)) ;
#93738 = CARTESIAN_POINT('Ctrl Pts',(-20.5468880523419,29.9783250934945,123.011437822122)) ;
#93739 = CARTESIAN_POINT('Ctrl Pts',(-20.5987893949161,29.9882579015574,123.213703298745)) ;
#93740 = CARTESIAN_POINT('Ctrl Pts',(-20.6153024480754,29.9981950037937,123.42197176182)) ;
#93741 = CARTESIAN_POINT('Ctrl Pts',(-20.5948955430994,30.0082474500641,123.632302018946)) ;
#93742 = CARTESIAN_POINT('Ctrl Pts',(-20.5397174255888,30.0180935656457,123.831827142723)) ;
#93743 = CARTESIAN_POINT('Ctrl Pts',(-20.4492191323458,30.0281415853606,124.022684697215)) ;
#93744 = CARTESIAN_POINT('Ctrl Pts',(-20.3279940404039,30.0380835369896,124.192964442128)) ;
#93745 = CARTESIAN_POINT('Ctrl Pts',(-20.1794617902803,30.0480223179886,124.339923783225)) ;
#93746 = CARTESIAN_POINT('Ctrl Pts',(-20.0060824903379,30.0580483667147,124.459764500437)) ;
#93747 = CARTESIAN_POINT('Ctrl Pts',(-19.8172623374216,30.0679352271229,124.546716323164)) ;
#93748 = CARTESIAN_POINT('Ctrl Pts',(-19.6133595715434,30.0779665022547,124.600410234333)) ;
#93749 = CARTESIAN_POINT('Ctrl Pts',(-19.406276769601,30.0878494795551,124.617843641432)) ;
#93750 = CARTESIAN_POINT('Ctrl Pts',(-19.1957687734416,30.0979063329623,124.598739082674)) ;
#93751 = CARTESIAN_POINT('Ctrl Pts',(-18.9283788438819,30.1110745740382,124.526647204317)) ;
#93752 = CARTESIAN_POINT('Ctrl Pts',(-18.6818038862875,30.1244756032648,124.384037954286)) ;
#93753 = CARTESIAN_POINT('Ctrl Pts',(-18.4857400702449,30.1376885199956,124.187208658776)) ;
#93754 = CARTESIAN_POINT('Ctrl Pts',(-18.3657914331037,30.1476169144488,124.016432936301)) ;
#93755 = CARTESIAN_POINT('Ctrl Pts',(-18.27667684773,30.157598414577,123.826421025304)) ;
#93756 = CARTESIAN_POINT('Ctrl Pts',(-18.2218764202102,30.1676389578471,123.622585918991)) ;
#93757 = CARTESIAN_POINT('Ctrl Pts',(-18.2033813668389,30.1774882896302,123.416346847631)) ;
#93758 = CARTESIAN_POINT('Ctrl Pts',(-18.2206996479079,30.1874836941018,123.206928562474)) ;
#93759 = CARTESIAN_POINT('Ctrl Pts',(-18.2745929305749,30.1975000215504,123.00336725188)) ;
#93760 = CARTESIAN_POINT('Ctrl Pts',(-18.3909391324748,30.210723678717,122.750841262503)) ;
#93761 = CARTESIAN_POINT('Ctrl Pts',(-18.5712709750288,30.2240179701063,122.533213120822)) ;
#93762 = CARTESIAN_POINT('Ctrl Pts',(-18.7990627197262,30.2373023210378,122.371616517048)) ;
#93763 = CARTESIAN_POINT('Ctrl Pts',(-18.9884333932997,30.2472747020996,122.281709419626)) ;
#93764 = CARTESIAN_POINT('Ctrl Pts',(-19.1891893546642,30.2571830817252,122.226046303007)) ;
#93765 = CARTESIAN_POINT('Ctrl Pts',(-19.3995715842747,30.2672370804733,122.205891859953)) ;
#93766 = CARTESIAN_POINT('Ctrl Pts',(-19.6062894044217,30.2770992775896,122.222096038525)) ;
#93767 = CARTESIAN_POINT('Ctrl Pts',(-19.8780882299461,30.2904464039637,122.291836869342)) ;
#93768 = CARTESIAN_POINT('Ctrl Pts',(-20.1845057827148,30.3069833696052,122.464304689986)) ;
#93769 = CARTESIAN_POINT('Ctrl Pts',(-20.4154425890932,30.3236179737791,122.732190513317)) ;
#93770 = CARTESIAN_POINT('Ctrl Pts',(-20.5367456008995,30.3369077670217,122.983880984554)) ;
#93771 = CARTESIAN_POINT('Ctrl Pts',(-20.5937491456457,30.3468603982811,123.185188491695)) ;
#93772 = CARTESIAN_POINT('Ctrl Pts',(-20.6151760929136,30.3568123655858,123.393329243809)) ;
#93773 = CARTESIAN_POINT('Ctrl Pts',(-20.594811477217,30.3701796240496,123.673593988513)) ;
#93774 = CARTESIAN_POINT('Ctrl Pts',(-20.4800576800383,30.3866964359988,124.005597356428)) ;
#93775 = CARTESIAN_POINT('Ctrl Pts',(-20.2120200574859,30.4067223310052,124.33630959658)) ;
#93776 = CARTESIAN_POINT('Ctrl Pts',(-19.8510357062947,30.4265330611353,124.553553092756)) ;
#93777 = CARTESIAN_POINT('Ctrl Pts',(-19.4344067851742,30.4465102772652,124.636126295456)) ;
#93778 = CARTESIAN_POINT('Ctrl Pts',(-19.0157736830144,30.4664371526604,124.570966794701)) ;
#93779 = CARTESIAN_POINT('Ctrl Pts',(-18.6457429963977,30.4862586141367,124.369093095067)) ;
#93780 = CARTESIAN_POINT('Ctrl Pts',(-18.363548673946,30.506332931946,124.048939383576)) ;
#93781 = CARTESIAN_POINT('Ctrl Pts',(-18.2096218900021,30.5261809009539,123.65586546792)) ;
#93782 = CARTESIAN_POINT('Ctrl Pts',(-18.1981503669756,30.5461279350171,123.231985052549)) ;
#93783 = CARTESIAN_POINT('Ctrl Pts',(-18.3318134408227,30.5660238859893,122.830579187293)) ;
#93784 = CARTESIAN_POINT('Ctrl Pts',(-18.5938415450344,30.5859193656075,122.498499856498)) ;
#93785 = CARTESIAN_POINT('Ctrl Pts',(-18.9545567012551,30.6058754765723,122.274979593225)) ;
#93786 = CARTESIAN_POINT('Ctrl Pts',(-19.3687580575178,30.6257800246123,122.188333583499)) ;
#93787 = CARTESIAN_POINT('Ctrl Pts',(-19.787309036188,30.6456541489314,122.247107330277)) ;
#93788 = CARTESIAN_POINT('Ctrl Pts',(-20.1636515869746,30.6657086789304,122.447450821914)) ;
#93789 = CARTESIAN_POINT('Ctrl Pts',(-20.4457200252673,30.6855161926904,122.760325311286)) ;
#93790 = CARTESIAN_POINT('Ctrl Pts',(-20.6062681553037,30.7054995484582,123.153662234623)) ;
#93791 = CARTESIAN_POINT('Ctrl Pts',(-20.6222628106825,30.7254178510421,123.576872328483)) ;
#93792 = CARTESIAN_POINT('Ctrl Pts',(-20.4942581051629,30.7452860664878,123.979555005816)) ;
#93793 = CARTESIAN_POINT('Ctrl Pts',(-20.2337561496977,30.7653363832841,124.31687450115)) ;
#93794 = CARTESIAN_POINT('Ctrl Pts',(-19.8787615933975,30.7851124451666,124.542563590445)) ;
#93795 = CARTESIAN_POINT('Ctrl Pts',(-19.4626826204921,30.8051670508591,124.635079577957)) ;
#93796 = CARTESIAN_POINT('Ctrl Pts',(-19.0452264153691,30.8249607400149,124.580607497338)) ;
#93797 = CARTESIAN_POINT('Ctrl Pts',(-18.6678121500625,30.8449274316093,124.386388946373)) ;
#93798 = CARTESIAN_POINT('Ctrl Pts',(-18.3797967323023,30.8648874773603,124.074567315355)) ;
#93799 = CARTESIAN_POINT('Ctrl Pts',(-18.2157690972036,30.8847857375105,123.684593681658)) ;
#93800 = CARTESIAN_POINT('Ctrl Pts',(-18.1941557059431,30.9046806530597,123.262145127519)) ;
#93801 = CARTESIAN_POINT('Ctrl Pts',(-18.3177212165592,30.9245908334733,122.857238599372)) ;
#93802 = CARTESIAN_POINT('Ctrl Pts',(-18.5722267685181,30.9445266325876,122.518239395623)) ;
#93803 = CARTESIAN_POINT('Ctrl Pts',(-18.9271455247788,30.9644644942417,122.286400946768)) ;
#93804 = CARTESIAN_POINT('Ctrl Pts',(-19.3394522574525,30.9843835408794,122.189424102124)) ;
#93805 = CARTESIAN_POINT('Ctrl Pts',(-19.7607105590053,31.0043324389335,122.238978391336)) ;
#93806 = CARTESIAN_POINT('Ctrl Pts',(-20.1390295702679,31.0242382663766,122.428816668531)) ;
#93807 = CARTESIAN_POINT('Ctrl Pts',(-20.3815086749295,31.0408209617419,122.684686173166)) ;
#93808 = CARTESIAN_POINT('Ctrl Pts',(-20.5148524519088,31.0540951754655,122.929906849042)) ;
#93809 = CARTESIAN_POINT('Ctrl Pts',(-20.5818785615782,31.0641418946649,123.130173465987)) ;
#93810 = CARTESIAN_POINT('Ctrl Pts',(-20.612716569486,31.0739859293105,123.334840505386)) ;
#93811 = CARTESIAN_POINT('Ctrl Pts',(-20.6063535960019,31.0873203142151,123.615037179933)) ;
#93812 = CARTESIAN_POINT('Ctrl Pts',(-20.507219363072,31.1039075315148,123.953619647069)) ;
#93813 = CARTESIAN_POINT('Ctrl Pts',(-20.298254731138,31.1205407435527,124.238840949928)) ;
#93814 = CARTESIAN_POINT('Ctrl Pts',(-20.0804677766212,31.1338231858249,124.413704891428)) ;
#93815 = CARTESIAN_POINT('Ctrl Pts',(-19.8981272530352,31.1437290737391,124.514266945286)) ;
#93816 = CARTESIAN_POINT('Ctrl Pts',(-19.6995096734775,31.1537174918443,124.582464176278)) ;
#93817 = CARTESIAN_POINT('Ctrl Pts',(-19.4913126073824,31.163740919083,124.615029422645)) ;
#93818 = CARTESIAN_POINT('Ctrl Pts',(-19.2831318881171,31.1736453502,124.611113982746)) ;
#93819 = CARTESIAN_POINT('Ctrl Pts',(-19.0093613876071,31.1869085028104,124.55827225687)) ;
#93820 = CARTESIAN_POINT('Ctrl Pts',(-18.7546009692031,31.2002334007143,124.434360468631)) ;
#93821 = CARTESIAN_POINT('Ctrl Pts',(-18.5439609812997,31.2134891443299,124.251809930995)) ;
#93822 = CARTESIAN_POINT('Ctrl Pts',(-18.411728227131,31.2234485177772,124.08951227342)) ;
#93823 = CARTESIAN_POINT('Ctrl Pts',(-18.3095841664041,31.2333923417042,123.907084589066)) ;
#93824 = CARTESIAN_POINT('Ctrl Pts',(-18.2401310461763,31.2434402858515,123.707606262789)) ;
#93825 = CARTESIAN_POINT('Ctrl Pts',(-18.2068457678084,31.2532912570697,123.503187613083)) ;
#93826 = CARTESIAN_POINT('Ctrl Pts',(-18.20905246238,31.2632630745117,123.293584227072)) ;
#93827 = CARTESIAN_POINT('Ctrl Pts',(-18.2477548076841,31.2732584968038,123.087014109771)) ;
#93828 = CARTESIAN_POINT('Ctrl Pts',(-18.3222090846656,31.2832915619275,122.889672405857)) ;
#93829 = CARTESIAN_POINT('Ctrl Pts',(-18.4278263479908,31.2931568945927,122.711184480995)) ;
#93830 = CARTESIAN_POINT('Ctrl Pts',(-18.5636713784596,31.3031174371903,122.551819024002)) ;
#93831 = CARTESIAN_POINT('Ctrl Pts',(-18.7265249519125,31.313151122692,122.417766687849)) ;
#93832 = CARTESIAN_POINT('Ctrl Pts',(-18.9073121476128,31.3230359546823,122.315233347034)) ;
#93833 = CARTESIAN_POINT('Ctrl Pts',(-19.1067295589491,31.3331033814421,122.244429547417)) ;
#93834 = CARTESIAN_POINT('Ctrl Pts',(-19.3107004512961,31.342941870601,122.209912168655)) ;
#93835 = CARTESIAN_POINT('Ctrl Pts',(-19.5222335142052,31.3530053517911,122.211086088931)) ;
#93836 = CARTESIAN_POINT('Ctrl Pts',(-19.7268674194447,31.3628995096062,122.248520775876)) ;
#93837 = CARTESIAN_POINT('Ctrl Pts',(-19.9229838875696,31.3728413663505,122.320715620495)) ;
#93838 = CARTESIAN_POINT('Ctrl Pts',(-20.1047748499077,31.3828438440219,122.426467358544)) ;
#93839 = CARTESIAN_POINT('Ctrl Pts',(-20.2657147069535,31.3928786483262,122.562842390076)) ;
#93840 = CARTESIAN_POINT('Ctrl Pts',(-20.3982636565813,31.4027235251719,122.721817859034)) ;
#93841 = CARTESIAN_POINT('Ctrl Pts',(-20.5029887534451,31.4127094047274,122.903726837913)) ;
#93842 = CARTESIAN_POINT('Ctrl Pts',(-20.5743391725136,31.4226441350859,123.10006380969)) ;
#93843 = CARTESIAN_POINT('Ctrl Pts',(-20.6107539159003,31.4327019473988,123.308316182202)) ;
#93844 = CARTESIAN_POINT('Ctrl Pts',(-20.6108179022155,31.4425225395232,123.514810058563)) ;
#93845 = CARTESIAN_POINT('Ctrl Pts',(-20.5744003078764,31.452589125133,123.72324139053)) ;
#93846 = CARTESIAN_POINT('Ctrl Pts',(-20.5034740799045,31.4624887057148,123.918955059756)) ;
#93847 = CARTESIAN_POINT('Ctrl Pts',(-20.3981618169355,31.472540305393,124.102114221002)) ;
#93848 = CARTESIAN_POINT('Ctrl Pts',(-20.2651091885193,31.48241449181,124.261505375485)) ;
#93849 = CARTESIAN_POINT('Ctrl Pts',(-20.1036202261952,31.4924709676909,124.397897467867)) ;
#93850 = CARTESIAN_POINT('Ctrl Pts',(-19.9238419339266,31.5023638989935,124.502558096768)) ;
#93851 = CARTESIAN_POINT('Ctrl Pts',(-19.7253582990717,31.5124266777062,124.575658467027)) ;
#93852 = CARTESIAN_POINT('Ctrl Pts',(-19.5217145691087,31.5222692032873,124.612477742698)) ;
#93853 = CARTESIAN_POINT('Ctrl Pts',(-19.3117088928933,31.5322599687122,124.613893836297)) ;
#93854 = CARTESIAN_POINT('Ctrl Pts',(-19.1059168231698,31.5421880447102,124.579001619905)) ;
#93855 = CARTESIAN_POINT('Ctrl Pts',(-18.9080017720923,31.5521759550973,124.508830986681)) ;
#93856 = CARTESIAN_POINT('Ctrl Pts',(-18.7245905279759,31.5622118672222,124.404561299914)) ;
#93857 = CARTESIAN_POINT('Ctrl Pts',(-18.5647630549477,31.5720668800699,124.272702953155)) ;
#93858 = CARTESIAN_POINT('Ctrl Pts',(-18.4281031702416,31.5820658259861,124.113022565623)) ;
#93859 = CARTESIAN_POINT('Ctrl Pts',(-18.3221273012406,31.5919627384341,123.933932741942)) ;
#93860 = CARTESIAN_POINT('Ctrl Pts',(-18.2476926082371,31.6020165365276,123.736138071533)) ;
#93861 = CARTESIAN_POINT('Ctrl Pts',(-18.2093337816089,31.6118974573543,123.531959013268)) ;
#93862 = CARTESIAN_POINT('Ctrl Pts',(-18.2066019685682,31.6219019833521,123.321674479705)) ;
#93863 = CARTESIAN_POINT('Ctrl Pts',(-18.2404263407543,31.6318859469695,123.114487635351)) ;
#93864 = CARTESIAN_POINT('Ctrl Pts',(-18.3102692992162,31.6419255875208,122.91532989079)) ;
#93865 = CARTESIAN_POINT('Ctrl Pts',(-18.4114038129035,31.6517696131355,122.734771558271)) ;
#93866 = CARTESIAN_POINT('Ctrl Pts',(-18.5438394807162,31.6617606189529,122.571741140915)) ;
#93867 = CARTESIAN_POINT('Ctrl Pts',(-18.7036285848506,31.6717984104851,122.433903147432)) ;
#93868 = CARTESIAN_POINT('Ctrl Pts',(-18.8812503177922,31.6816428102735,122.327667870573)) ;
#93869 = CARTESIAN_POINT('Ctrl Pts',(-19.0771971755672,31.6916276108302,122.252460208954)) ;
#93870 = CARTESIAN_POINT('Ctrl Pts',(-19.2823298077936,31.7015671342414,122.21249959101)) ;
#93871 = CARTESIAN_POINT('Ctrl Pts',(-19.4933471182147,31.7116068533424,122.208776390442)) ;
#93872 = CARTESIAN_POINT('Ctrl Pts',(-19.6987028225727,31.7214950252616,122.241153193864)) ;
#93873 = CARTESIAN_POINT('Ctrl Pts',(-19.8974425155665,31.7314845876786,122.309009005677)) ;
#93874 = CARTESIAN_POINT('Ctrl Pts',(-20.0807345289444,31.7414429598733,122.410164926042)) ;
#93875 = CARTESIAN_POINT('Ctrl Pts',(-20.2430472008146,31.751343034104,122.540457091883)) ;
#93876 = CARTESIAN_POINT('Ctrl Pts',(-20.3822631308276,31.7613891304776,122.699266960412)) ;
#93877 = CARTESIAN_POINT('Ctrl Pts',(-20.4903109489229,31.7712977144747,122.877375084969)) ;
#93878 = CARTESIAN_POINT('Ctrl Pts',(-20.566929490437,31.7813082930656,123.073389758785)) ;
#93879 = CARTESIAN_POINT('Ctrl Pts',(-20.6080089158008,31.7913374511785,123.280201568448)) ;
#93880 = CARTESIAN_POINT('Ctrl Pts',(-20.6127724616542,31.8011903330165,123.487271818897)) ;
#93881 = CARTESIAN_POINT('Ctrl Pts',(-20.581806626969,31.8111498941675,123.694357030942)) ;
#93882 = CARTESIAN_POINT('Ctrl Pts',(-20.5144687823656,31.8211883287566,123.894350895927)) ;
#93883 = CARTESIAN_POINT('Ctrl Pts',(-20.415413063055,31.8310616009837,124.076794583067)) ;
#93884 = CARTESIAN_POINT('Ctrl Pts',(-20.2835620404911,31.8411348429773,124.242457424024)) ;
#93885 = CARTESIAN_POINT('Ctrl Pts',(-20.1290461488142,31.8509551745104,124.379450070107)) ;
#93886 = CARTESIAN_POINT('Ctrl Pts',(-19.9486477522964,31.8610338357371,124.490491065507)) ;
#93887 = CARTESIAN_POINT('Ctrl Pts',(-19.7560811050293,31.8708854310314,124.566868118361)) ;
#93888 = CARTESIAN_POINT('Ctrl Pts',(-19.5487382827828,31.8809585662602,124.609752344747)) ;
#93889 = CARTESIAN_POINT('Ctrl Pts',(-19.3418894357439,31.8908010017852,124.615811183682)) ;
#93890 = CARTESIAN_POINT('Ctrl Pts',(-19.1341823671792,31.9007817709186,124.586138256737)) ;
#93891 = CARTESIAN_POINT('Ctrl Pts',(-18.9341677996777,31.9107988721625,124.520238635541)) ;
#93892 = CARTESIAN_POINT('Ctrl Pts',(-18.7508181677505,31.9206873197643,124.422228288085)) ;
#93893 = CARTESIAN_POINT('Ctrl Pts',(-18.5845186028101,31.9307430339452,124.291738473027)) ;
#93894 = CARTESIAN_POINT('Ctrl Pts',(-18.4458907438833,31.940618240359,124.137177719014)) ;
#93895 = CARTESIAN_POINT('Ctrl Pts',(-18.3344556958182,31.9506132928317,123.959039423795)) ;
#93896 = CARTESIAN_POINT('Ctrl Pts',(-18.2557440922024,31.9606351767938,123.763594402639)) ;
#93897 = CARTESIAN_POINT('Ctrl Pts',(-18.2124503481654,31.9705391493231,123.559934304139)) ;
#93898 = CARTESIAN_POINT('Ctrl Pts',(-18.2048119891636,31.980527645984,123.350081973959)) ;
#93899 = CARTESIAN_POINT('Ctrl Pts',(-18.2337946115859,31.990491443232,123.142637302614)) ;
#93900 = CARTESIAN_POINT('Ctrl Pts',(-18.2974930953008,32.00039546654,122.944386197689)) ;
#93901 = CARTESIAN_POINT('Ctrl Pts',(-18.3963169602381,32.0104559698617,122.757419517568)) ;
#93902 = CARTESIAN_POINT('Ctrl Pts',(-18.5230894198488,32.0202965050015,122.593899269698)) ;
#93903 = CARTESIAN_POINT('Ctrl Pts',(-18.6795617836755,32.0303587257061,122.451576324891)) ;
#93904 = CARTESIAN_POINT('Ctrl Pts',(-18.8555799237942,32.0402558794824,122.340603849521)) ;
#93905 = CARTESIAN_POINT('Ctrl Pts',(-19.0485759335199,32.0501870128678,122.260971589894)) ;
#93906 = CARTESIAN_POINT('Ctrl Pts',(-19.2548021702129,32.0602293880136,122.21578488518)) ;
#93907 = CARTESIAN_POINT('Ctrl Pts',(-19.4624645914711,32.0701153257797,122.207066666525)) ;
#93908 = CARTESIAN_POINT('Ctrl Pts',(-19.6707916606036,32.0801111687645,122.234516690486)) ;
#93909 = CARTESIAN_POINT('Ctrl Pts',(-19.8701273889737,32.0900531466432,122.297413037221)) ;
#93910 = CARTESIAN_POINT('Ctrl Pts',(-20.055949568507,32.1000125211241,122.393870336215)) ;
#93911 = CARTESIAN_POINT('Ctrl Pts',(-20.2229151924571,32.1100091369579,122.521538014779)) ;
#93912 = CARTESIAN_POINT('Ctrl Pts',(-20.3654870724293,32.1200433555314,122.6770082414)) ;
#93913 = CARTESIAN_POINT('Ctrl Pts',(-20.4770646674535,32.129896422742,122.851527849583)) ;
#93914 = CARTESIAN_POINT('Ctrl Pts',(-20.5580731723028,32.1398566806196,123.044611510919)) ;
#93915 = CARTESIAN_POINT('Ctrl Pts',(-20.6044060123665,32.1498857073252,123.250311138346)) ;
#93916 = CARTESIAN_POINT('Ctrl Pts',(-20.6142619787569,32.1597959143596,123.458412203081)) ;
#93917 = CARTESIAN_POINT('Ctrl Pts',(-20.5883124116075,32.1697308250073,123.665662854138)) ;
#93918 = CARTESIAN_POINT('Ctrl Pts',(-20.5259287030354,32.1797719551865,123.867323632054)) ;
#93919 = CARTESIAN_POINT('Ctrl Pts',(-20.4310789187822,32.1896590955564,124.052292571989)) ;
#93920 = CARTESIAN_POINT('Ctrl Pts',(-20.304513568402,32.1996513730924,124.219935519192)) ;
#93921 = CARTESIAN_POINT('Ctrl Pts',(-20.1513762537152,32.2095999163607,124.362403856439)) ;
#93922 = CARTESIAN_POINT('Ctrl Pts',(-19.976222390719,32.2195365911779,124.476218544844)) ;
#93923 = CARTESIAN_POINT('Ctrl Pts',(-19.7831273118122,32.2295200121143,124.558523255501)) ;
#93924 = CARTESIAN_POINT('Ctrl Pts',(-19.5774220081885,32.2395623273035,124.60598952607)) ;
#93925 = CARTESIAN_POINT('Ctrl Pts',(-19.370845783349,32.2494026447427,124.617131308985)) ;
#93926 = CARTESIAN_POINT('Ctrl Pts',(-19.1614606932978,32.2594323488002,124.592247049421)) ;
#93927 = CARTESIAN_POINT('Ctrl Pts',(-18.9599203041336,32.2694533055227,124.530895300264)) ;
#93928 = CARTESIAN_POINT('Ctrl Pts',(-18.7747348258612,32.2793198478263,124.437418896063)) ;
#93929 = CARTESIAN_POINT('Ctrl Pts',(-18.6051744995746,32.2893909477715,124.310654941653)) ;
#93930 = CARTESIAN_POINT('Ctrl Pts',(-18.4634825926305,32.2992330219491,124.159861061519)) ;
#93931 = CARTESIAN_POINT('Ctrl Pts',(-18.3481195405836,32.3091938165361,123.985101895507)) ;
#93932 = CARTESIAN_POINT('Ctrl Pts',(-18.2645928561442,32.3192316894369,123.791315971168)) ;
#93933 = CARTESIAN_POINT('Ctrl Pts',(-18.2163931560725,32.329105974981,123.589374702714)) ;
#93934 = CARTESIAN_POINT('Ctrl Pts',(-18.2037592119265,32.3391757253949,123.378082427202)) ;
#93935 = CARTESIAN_POINT('Ctrl Pts',(-18.227329317313,32.3490090099296,123.172687270205)) ;
#93936 = CARTESIAN_POINT('Ctrl Pts',(-18.286804334451,32.3590393507296,122.970385364036)) ;
#93937 = CARTESIAN_POINT('Ctrl Pts',(-18.3810784901195,32.3690712747292,122.781715083692)) ;
#93938 = CARTESIAN_POINT('Ctrl Pts',(-18.5037608147932,32.3788998096651,122.615463900118)) ;
#93939 = CARTESIAN_POINT('Ctrl Pts',(-18.6555715303038,32.3888935874298,122.470222048311)) ;
#93940 = CARTESIAN_POINT('Ctrl Pts',(-18.831125396415,32.3989212979154,122.353490733339)) ;
#93941 = CARTESIAN_POINT('Ctrl Pts',(-19.0214892135476,32.4088097087493,122.269952809508)) ;
#93942 = CARTESIAN_POINT('Ctrl Pts',(-19.2251690134222,32.4187865592849,122.219945129683)) ;
#93943 = CARTESIAN_POINT('Ctrl Pts',(-19.4347962245961,32.4287783558353,122.206021141122)) ;
#93944 = CARTESIAN_POINT('Ctrl Pts',(-19.644506261985,32.438814361929,122.229058208528)) ;
#93945 = CARTESIAN_POINT('Ctrl Pts',(-19.8434117000005,32.4486650961918,122.286768450551)) ;
#93946 = CARTESIAN_POINT('Ctrl Pts',(-20.0320459339982,32.45865635472,122.379097167223)) ;
#93947 = CARTESIAN_POINT('Ctrl Pts',(-20.20065583118,32.4685742496232,122.501801180577)) ;
#93948 = CARTESIAN_POINT('Ctrl Pts',(-20.3470163566351,32.4786023912863,122.653517378883)) ;
#93949 = CARTESIAN_POINT('Ctrl Pts',(-20.4632160358938,32.4884875594021,122.825818794577)) ;
#93950 = CARTESIAN_POINT('Ctrl Pts',(-20.5490902320439,32.4984769229081,123.017471259713)) ;
#93951 = CARTESIAN_POINT('Ctrl Pts',(-20.600215334556,32.5085180579182,123.222283152939)) ;
#93952 = CARTESIAN_POINT('Ctrl Pts',(-20.6150344433959,32.5183507261062,123.428460755687)) ;
#93953 = CARTESIAN_POINT('Ctrl Pts',(-20.5940801019573,32.5283446290607,123.637515476195)) ;
#93954 = CARTESIAN_POINT('Ctrl Pts',(-20.5365126203396,32.5383739141452,123.84035345709)) ;
#93955 = CARTESIAN_POINT('Ctrl Pts',(-20.4463103931362,32.5482494425871,124.027361177851)) ;
#93956 = CARTESIAN_POINT('Ctrl Pts',(-20.3236864942559,32.5582497252032,124.198101790075)) ;
#93957 = CARTESIAN_POINT('Ctrl Pts',(-20.1746881469823,32.5681617412602,124.343816676878)) ;
#93958 = CARTESIAN_POINT('Ctrl Pts',(-20.0004586794093,32.5782038165992,124.463012680978)) ;
#93959 = CARTESIAN_POINT('Ctrl Pts',(-19.8108772885679,32.5881036492553,124.548917301885)) ;
#93960 = CARTESIAN_POINT('Ctrl Pts',(-19.6075007703568,32.5980960498334,124.601531937198)) ;
#93961 = CARTESIAN_POINT('Ctrl Pts',(-19.3971732299059,32.6081300715927,124.617729269594)) ;
#93962 = CARTESIAN_POINT('Ctrl Pts',(-19.1907544289852,32.6179946824339,124.597773975522)) ;
#93963 = CARTESIAN_POINT('Ctrl Pts',(-18.9882033401432,32.6279870818951,124.542054825909)) ;
#93964 = CARTESIAN_POINT('Ctrl Pts',(-18.7978334954326,32.638019035228,124.451283460562)) ;
#93965 = CARTESIAN_POINT('Ctrl Pts',(-18.628758986435,32.6478853941696,124.331111736303)) ;
#93966 = CARTESIAN_POINT('Ctrl Pts',(-18.4811111490169,32.6578728696554,124.181860126214)) ;
#93967 = CARTESIAN_POINT('Ctrl Pts',(-18.3620060824983,32.6678177758439,124.009992191636)) ;
#93968 = CARTESIAN_POINT('Ctrl Pts',(-18.2738030986385,32.6778627405042,123.818139912872)) ;
#93969 = CARTESIAN_POINT('Ctrl Pts',(-18.2210369220025,32.687724547409,123.617622964085)) ;
#93970 = CARTESIAN_POINT('Ctrl Pts',(-18.2032624857516,32.6977172197148,123.408320481454)) ;
#93971 = CARTESIAN_POINT('Ctrl Pts',(-18.2220069176133,32.7076458906601,123.20041822076)) ;
#93972 = CARTESIAN_POINT('Ctrl Pts',(-18.2763580861567,32.7175984328854,122.998381912179)) ;
#93973 = CARTESIAN_POINT('Ctrl Pts',(-18.3653128531859,32.7275997888813,122.807841810315)) ;
#93974 = CARTESIAN_POINT('Ctrl Pts',(-18.4865473980735,32.737628401156,122.635363522157)) ;
#93975 = CARTESIAN_POINT('Ctrl Pts',(-18.6332437506047,32.7474927357055,122.488761340732)) ;
#93976 = CARTESIAN_POINT('Ctrl Pts',(-18.8051496446684,32.7574850597821,122.36807151102)) ;
#93977 = CARTESIAN_POINT('Ctrl Pts',(-18.9941648299301,32.767412552148,122.279502896723)) ;
#93978 = CARTESIAN_POINT('Ctrl Pts',(-19.1976622179447,32.7774399106988,122.224574409958)) ;
#93979 = CARTESIAN_POINT('Ctrl Pts',(-19.4046917324504,32.7873263287499,122.2058521457)) ;
#93980 = CARTESIAN_POINT('Ctrl Pts',(-19.6148150461169,32.7973580634853,122.223507004572)) ;
#93981 = CARTESIAN_POINT('Ctrl Pts',(-19.8157515091835,32.8072396447286,122.276392589365)) ;
#93982 = CARTESIAN_POINT('Ctrl Pts',(-20.0078550070822,32.8173016227609,122.364875768334)) ;
#93983 = CARTESIAN_POINT('Ctrl Pts',(-20.1782306508466,32.8271587011226,122.482889602471)) ;
#93984 = CARTESIAN_POINT('Ctrl Pts',(-20.3278335781113,32.8371532742286,122.63038217435)) ;
#93985 = CARTESIAN_POINT('Ctrl Pts',(-20.4488151036229,32.8470790705162,122.800439225397)) ;
#93986 = CARTESIAN_POINT('Ctrl Pts',(-20.5393606750725,32.857104437686,122.990744699707)) ;
#93987 = CARTESIAN_POINT('Ctrl Pts',(-20.5948558931184,32.8670005173398,123.191261961852)) ;
#93988 = CARTESIAN_POINT('Ctrl Pts',(-20.6153122258122,32.8769955970454,123.400395012648)) ;
#93989 = CARTESIAN_POINT('Ctrl Pts',(-20.5987383876886,32.8870206848612,123.61049872856)) ;
#93990 = CARTESIAN_POINT('Ctrl Pts',(-20.5297765684024,32.9002045072285,123.878959402027)) ;
#93991 = CARTESIAN_POINT('Ctrl Pts',(-20.3913921904728,32.9135266253744,124.126130710772)) ;
#93992 = CARTESIAN_POINT('Ctrl Pts',(-20.19452440354,32.926905835002,124.327020138545)) ;
#93993 = CARTESIAN_POINT('Ctrl Pts',(-20.0266226033983,32.9367440722462,124.44783150031)) ;
#93994 = CARTESIAN_POINT('Ctrl Pts',(-19.8359283011779,32.946816995505,124.539857209982)) ;
#93995 = CARTESIAN_POINT('Ctrl Pts',(-19.636475161509,32.9566736369601,124.596128301881)) ;
#93996 = CARTESIAN_POINT('Ctrl Pts',(-19.4276788172328,32.9666590124661,124.617742244852)) ;
#93997 = CARTESIAN_POINT('Ctrl Pts',(-19.1491574998988,32.9799430439266,124.597574269333)) ;
#93998 = CARTESIAN_POINT('Ctrl Pts',(-18.8168323648983,32.9964618357969,124.483616253666)) ;
#93999 = CARTESIAN_POINT('Ctrl Pts',(-18.5395293019572,33.0132475528035,124.258981058193)) ;
#94000 = CARTESIAN_POINT('Ctrl Pts',(-18.3774838302802,33.0263607013125,124.03593563537)) ;
#94001 = CARTESIAN_POINT('Ctrl Pts',(-18.2842424376634,33.0363962503927,123.846700449347)) ;
#94002 = CARTESIAN_POINT('Ctrl Pts',(-18.2259657532557,33.0464123065721,123.644335341061)) ;
#94003 = CARTESIAN_POINT('Ctrl Pts',(-18.1960980277627,33.0595903424381,123.368929108419)) ;
#94004 = CARTESIAN_POINT('Ctrl Pts',(-18.249009068452,33.0761922196252,123.019870829491)) ;
#94005 = CARTESIAN_POINT('Ctrl Pts',(-18.4541282278557,33.0962553642411,122.645836767002)) ;
#94006 = CARTESIAN_POINT('Ctrl Pts',(-18.7702599399458,33.1160562543248,122.367699508077)) ;
#94007 = CARTESIAN_POINT('Ctrl Pts',(-19.1646436097345,33.1359993796035,122.212088074681)) ;
#94008 = CARTESIAN_POINT('Ctrl Pts',(-19.5875674444081,33.1558974247231,122.200707746855)) ;
#94009 = CARTESIAN_POINT('Ctrl Pts',(-19.9891372297378,33.1757831843499,122.333269321232)) ;
#94010 = CARTESIAN_POINT('Ctrl Pts',(-20.3238757638564,33.1958483595298,122.597734163642)) ;
#94011 = CARTESIAN_POINT('Ctrl Pts',(-20.5455361464889,33.2156750026326,122.956408640357)) ;
#94012 = CARTESIAN_POINT('Ctrl Pts',(-20.6329532940323,33.2355837120809,123.370483063395)) ;
#94013 = CARTESIAN_POINT('Ctrl Pts',(-20.5737633317445,33.2555355491127,123.790683278414)) ;
#94014 = CARTESIAN_POINT('Ctrl Pts',(-20.3736428549386,33.2755440238159,124.166059655806)) ;
#94015 = CARTESIAN_POINT('Ctrl Pts',(-20.0610026351362,33.2953454825774,124.448078284443)) ;
#94016 = CARTESIAN_POINT('Ctrl Pts',(-19.6682567912983,33.3153023708133,124.608739938884)) ;
#94017 = CARTESIAN_POINT('Ctrl Pts',(-19.2436658991202,33.3352862082274,124.624794629549)) ;
#94018 = CARTESIAN_POINT('Ctrl Pts',(-18.8423051955773,33.3550946474483,124.496925784689)) ;
#94019 = CARTESIAN_POINT('Ctrl Pts',(-18.5055646804555,33.3750803568285,124.23792646132)) ;
#94020 = CARTESIAN_POINT('Ctrl Pts',(-18.2784679309149,33.3949498798438,123.881467993648)) ;
#94021 = CARTESIAN_POINT('Ctrl Pts',(-18.1861872022792,33.414970618961,123.466059954206)) ;
#94022 = CARTESIAN_POINT('Ctrl Pts',(-18.2401103646195,33.434774683938,123.04827687891)) ;
#94023 = CARTESIAN_POINT('Ctrl Pts',(-18.4356216338899,33.4548366476687,122.669283035996)) ;
#94024 = CARTESIAN_POINT('Ctrl Pts',(-18.7455985363762,33.4746698279572,122.383215081559)) ;
#94025 = CARTESIAN_POINT('Ctrl Pts',(-19.1356568720352,33.4945890252833,122.218360374469)) ;
#94026 = CARTESIAN_POINT('Ctrl Pts',(-19.5590433618675,33.5145270503966,122.196755247906)) ;
#94027 = CARTESIAN_POINT('Ctrl Pts',(-19.9633828670812,33.5344050964527,122.319991735649)) ;
#94028 = CARTESIAN_POINT('Ctrl Pts',(-20.3031557635292,33.5543898307408,122.575085905004)) ;
#94029 = CARTESIAN_POINT('Ctrl Pts',(-20.5347847173385,33.5743006474192,122.929604659567)) ;
#94030 = CARTESIAN_POINT('Ctrl Pts',(-20.6316400602913,33.594299622938,123.343555625924)) ;
#94031 = CARTESIAN_POINT('Ctrl Pts',(-20.5824164230939,33.6141045435832,123.76186141104)) ;
#94032 = CARTESIAN_POINT('Ctrl Pts',(-20.3923377698782,33.6340885038744,124.141776622175)) ;
#94033 = CARTESIAN_POINT('Ctrl Pts',(-20.0852720477215,33.6539747075983,124.432586156203)) ;
#94034 = CARTESIAN_POINT('Ctrl Pts',(-19.6964740225764,33.6739238859215,124.602080267117)) ;
#94035 = CARTESIAN_POINT('Ctrl Pts',(-19.2741491376864,33.6938256851611,124.628564548105)) ;
#94036 = CARTESIAN_POINT('Ctrl Pts',(-18.8683285448155,33.7137042902134,124.510329651204)) ;
#94037 = CARTESIAN_POINT('Ctrl Pts',(-18.5246878694578,33.7337366499391,124.25860986934)) ;
#94038 = CARTESIAN_POINT('Ctrl Pts',(-18.3288960189047,33.7503183758952,123.965412227586)) ;
#94039 = CARTESIAN_POINT('Ctrl Pts',(-18.2390050907731,33.7635125461931,123.702986209671)) ;
#94040 = CARTESIAN_POINT('Ctrl Pts',(-18.1952156177926,33.7768247242863,123.426625334164)) ;
#94041 = CARTESIAN_POINT('Ctrl Pts',(-18.2318570630628,33.7933909038797,123.076205385333)) ;
#94042 = CARTESIAN_POINT('Ctrl Pts',(-18.3860721862211,33.8100190987398,122.758154709291)) ;
#94043 = CARTESIAN_POINT('Ctrl Pts',(-18.5689208252892,33.8233076804496,122.546840432234)) ;
#94044 = CARTESIAN_POINT('Ctrl Pts',(-18.7313513600234,33.8332759285532,122.414464321672)) ;
#94045 = CARTESIAN_POINT('Ctrl Pts',(-18.9132140980837,33.8431906848093,122.3126070292)) ;
#94046 = CARTESIAN_POINT('Ctrl Pts',(-19.1118793081902,33.8532038354605,122.242971307664)) ;
#94047 = CARTESIAN_POINT('Ctrl Pts',(-19.3196579468143,33.8632165426625,122.209223877592)) ;
#94048 = CARTESIAN_POINT('Ctrl Pts',(-19.5975383974733,33.8764358313538,122.212437339034)) ;
#94049 = CARTESIAN_POINT('Ctrl Pts',(-19.9378289154735,33.8930545123519,122.307523681823)) ;
#94050 = CARTESIAN_POINT('Ctrl Pts',(-20.2246132383355,33.9096194201253,122.512032246006)) ;
#94051 = CARTESIAN_POINT('Ctrl Pts',(-20.4036557241936,33.9230178917362,122.729519796154)) ;
#94052 = CARTESIAN_POINT('Ctrl Pts',(-20.5055966782541,33.9328591472231,122.90956884558)) ;
#94053 = CARTESIAN_POINT('Ctrl Pts',(-20.5761690139135,33.9428454628113,123.107261429492)) ;
#94054 = CARTESIAN_POINT('Ctrl Pts',(-20.611277650306,33.9527820703977,123.313223876353)) ;
#94055 = CARTESIAN_POINT('Ctrl Pts',(-20.6099735810756,33.962831937766,123.524478262439)) ;
#94056 = CARTESIAN_POINT('Ctrl Pts',(-20.5729077462783,33.9726824324408,123.728238382038)) ;
#94057 = CARTESIAN_POINT('Ctrl Pts',(-20.5006686095977,33.9826542328353,123.925008548222)) ;
#94058 = CARTESIAN_POINT('Ctrl Pts',(-20.3950540740797,33.9926501998612,124.10672846331)) ;
#94059 = CARTESIAN_POINT('Ctrl Pts',(-20.2587448232907,34.0026876592423,124.267788333487)) ;
#94060 = CARTESIAN_POINT('Ctrl Pts',(-20.0999443163612,34.0125283601431,124.400411931469)) ;
#94061 = CARTESIAN_POINT('Ctrl Pts',(-19.9169251629919,34.0225763814104,124.505877195558)) ;
#94062 = CARTESIAN_POINT('Ctrl Pts',(-19.7202373371653,34.0325237744931,124.576929500884)) ;
#94063 = CARTESIAN_POINT('Ctrl Pts',(-19.5150731670735,34.0424339205395,124.613246052084)) ;
#94064 = CARTESIAN_POINT('Ctrl Pts',(-19.3036248985833,34.0524928343891,124.613150607423)) ;
#94065 = CARTESIAN_POINT('Ctrl Pts',(-19.0998219185754,34.0623336046784,124.577418243024)) ;
#94066 = CARTESIAN_POINT('Ctrl Pts',(-18.9008963171724,34.0723964742571,124.505500639989)) ;
#94067 = CARTESIAN_POINT('Ctrl Pts',(-18.7205944492889,34.0822907973875,124.40172913725)) ;
#94068 = CARTESIAN_POINT('Ctrl Pts',(-18.5599579858126,34.092232604482,124.268052319502)) ;
#94069 = CARTESIAN_POINT('Ctrl Pts',(-18.4240523603938,34.1022351154374,124.107549491577)) ;
#94070 = CARTESIAN_POINT('Ctrl Pts',(-18.3180449838166,34.1122698362557,123.925171270293)) ;
#94071 = CARTESIAN_POINT('Ctrl Pts',(-18.2463591434105,34.1221150137615,123.730992524548)) ;
#94072 = CARTESIAN_POINT('Ctrl Pts',(-18.2085560215957,34.1320997741625,123.524543616155)) ;
#94073 = CARTESIAN_POINT('Ctrl Pts',(-18.2070790891431,34.1420386804789,123.315570306909)) ;
#94074 = CARTESIAN_POINT('Ctrl Pts',(-18.2423345297915,34.1520809081147,123.107437286142)) ;
#94075 = CARTESIAN_POINT('Ctrl Pts',(-18.3119591437577,34.161966119699,122.911604453223)) ;
#94076 = CARTESIAN_POINT('Ctrl Pts',(-18.415446825498,34.171965049901,122.72866948783)) ;
#94077 = CARTESIAN_POINT('Ctrl Pts',(-18.5479551287003,34.1818824728114,122.567652773556)) ;
#94078 = CARTESIAN_POINT('Ctrl Pts',(-18.7084701859392,34.1919304048901,122.430380021291)) ;
#94079 = CARTESIAN_POINT('Ctrl Pts',(-18.8872472220811,34.2018077806995,122.324675785591)) ;
#94080 = CARTESIAN_POINT('Ctrl Pts',(-19.0850314864428,34.2118616738674,122.250237672845)) ;
#94081 = CARTESIAN_POINT('Ctrl Pts',(-19.2894839484304,34.2217552971207,122.211783907528)) ;
#94082 = CARTESIAN_POINT('Ctrl Pts',(-19.500983623054,34.2318178907437,122.209341438125)) ;
#94083 = CARTESIAN_POINT('Ctrl Pts',(-19.7052052740949,34.2416604647328,122.242811570821)) ;
#94084 = CARTESIAN_POINT('Ctrl Pts',(-19.9035702084726,34.2516512216157,122.311773010739)) ;
#94085 = CARTESIAN_POINT('Ctrl Pts',(-20.0858114345933,34.2615792833737,122.413537168771)) ;
#94086 = CARTESIAN_POINT('Ctrl Pts',(-20.2488208114656,34.2715672592628,122.545909741737)) ;
#94087 = CARTESIAN_POINT('Ctrl Pts',(-20.3867503154781,34.2816029236193,122.705552972762)) ;
#94088 = CARTESIAN_POINT('Ctrl Pts',(-20.4932169372038,34.2914588620389,122.883323157237)) ;
#94089 = CARTESIAN_POINT('Ctrl Pts',(-20.5685573075516,34.3014543534358,123.079465833174)) ;
#94090 = CARTESIAN_POINT('Ctrl Pts',(-20.6084203311563,34.3113641583893,123.283961980646)) ;
#94091 = CARTESIAN_POINT('Ctrl Pts',(-20.612551191493,34.321376380656,123.494414775506)) ;
#94092 = CARTESIAN_POINT('Ctrl Pts',(-20.5796204265789,34.3314042613489,123.70264639722)) ;
#94093 = CARTESIAN_POINT('Ctrl Pts',(-20.5125423192558,34.3412606573315,123.898699495706)) ;
#94094 = CARTESIAN_POINT('Ctrl Pts',(-20.4111153088233,34.3512854545114,124.083444098484)) ;
#94095 = CARTESIAN_POINT('Ctrl Pts',(-20.2786642846804,34.3613163844952,124.247549916826)) ;
#94096 = CARTESIAN_POINT('Ctrl Pts',(-20.12294110075,34.3711609870039,124.383860206377)) ;
#94097 = CARTESIAN_POINT('Ctrl Pts',(-19.9435694725039,34.381151838228,124.493149976291)) ;
#94098 = CARTESIAN_POINT('Ctrl Pts',(-19.7468604255009,34.3911896712392,124.569551549301)) ;
#94099 = CARTESIAN_POINT('Ctrl Pts',(-19.5439244481446,34.4010340597047,124.610202431211)) ;
#94100 = CARTESIAN_POINT('Ctrl Pts',(-19.334106769113,34.4110188640742,124.615482055725)) ;
#94101 = CARTESIAN_POINT('Ctrl Pts',(-19.1274314473435,34.4209583835571,124.58447308908)) ;
#94102 = CARTESIAN_POINT('Ctrl Pts',(-18.9273406435302,34.4309981145584,124.51734707445)) ;
#94103 = CARTESIAN_POINT('Ctrl Pts',(-18.7446690953426,34.4408862428047,124.418099734678)) ;
#94104 = CARTESIAN_POINT('Ctrl Pts',(-18.580106238274,34.4508759680132,124.287630599597)) ;
#94105 = CARTESIAN_POINT('Ctrl Pts',(-18.4412525947142,34.4608337327147,124.130968239248)) ;
#94106 = CARTESIAN_POINT('Ctrl Pts',(-18.3318983126126,34.4707360741267,123.953816562447)) ;
#94107 = CARTESIAN_POINT('Ctrl Pts',(-18.2538875112348,34.4807802698331,123.757605424471)) ;
#94108 = CARTESIAN_POINT('Ctrl Pts',(-18.2116860626356,34.4906876705924,123.553629701475)) ;
#94109 = CARTESIAN_POINT('Ctrl Pts',(-18.2051086171753,34.5006982704667,123.343275079587)) ;
#94110 = CARTESIAN_POINT('Ctrl Pts',(-18.235618607737,34.5107285663789,123.134619214814)) ;
#94111 = CARTESIAN_POINT('Ctrl Pts',(-18.3004560701024,34.5205833460286,122.937861271904)) ;
#94112 = CARTESIAN_POINT('Ctrl Pts',(-18.3989387244169,34.5305406742461,122.753132054691)) ;
#94113 = CARTESIAN_POINT('Ctrl Pts',(-18.529340384314,34.540579707153,122.587203293824)) ;
#94114 = CARTESIAN_POINT('Ctrl Pts',(-18.6837505633702,34.5504528190423,122.448444472105)) ;
#94115 = CARTESIAN_POINT('Ctrl Pts',(-18.8634484664736,34.5605261040694,122.336472032955)) ;
#94116 = CARTESIAN_POINT('Ctrl Pts',(-19.0549065955958,34.5703464238062,122.259103635501)) ;
#94117 = CARTESIAN_POINT('Ctrl Pts',(-19.2620673866874,34.5804250891846,122.214853277882)) ;
#94118 = CARTESIAN_POINT('Ctrl Pts',(-19.4690914175572,34.5902766796684,122.207340232116)) ;
#94119 = CARTESIAN_POINT('Ctrl Pts',(-19.6788278083087,34.6003498299873,122.23633458092)) ;
#94120 = CARTESIAN_POINT('Ctrl Pts',(-19.8757732790517,34.6101922099624,122.299862332221)) ;
#94121 = CARTESIAN_POINT('Ctrl Pts',(-20.0615624570117,34.6201731862054,122.39735650265)) ;
#94122 = CARTESIAN_POINT('Ctrl Pts',(-20.22799325484,34.6301895145607,122.526380463607)) ;
#94123 = CARTESIAN_POINT('Ctrl Pts',(-20.3680014912739,34.6400873115519,122.680305163105)) ;
#94124 = CARTESIAN_POINT('Ctrl Pts',(-20.4807624680601,34.6500998682839,122.858068591646)) ;
#94125 = CARTESIAN_POINT('Ctrl Pts',(-20.5606293910211,34.6601319031304,123.053255712585)) ;
#94126 = CARTESIAN_POINT('Ctrl Pts',(-20.6050415862944,34.6699713039459,123.255303457443)) ;
#94127 = CARTESIAN_POINT('Ctrl Pts',(-20.6140547312464,34.6800370895974,123.466701640251)) ;
#94128 = CARTESIAN_POINT('Ctrl Pts',(-20.5866072640144,34.689927544712,123.672832323993)) ;
#94129 = CARTESIAN_POINT('Ctrl Pts',(-20.5235800847125,34.6999196633478,123.873208878292)) ;
#94130 = CARTESIAN_POINT('Ctrl Pts',(-20.4268258454947,34.7098824901109,124.05896578674)) ;
#94131 = CARTESIAN_POINT('Ctrl Pts',(-20.3004423413682,34.7197867733837,124.224463799547)) ;
#94132 = CARTESIAN_POINT('Ctrl Pts',(-20.1447352025341,34.7298472073308,124.367564111217)) ;
#94133 = CARTESIAN_POINT('Ctrl Pts',(-19.9705405095534,34.739687760004,124.479217029164)) ;
#94134 = CARTESIAN_POINT('Ctrl Pts',(-19.7754543274216,34.7497499799497,124.560953476253)) ;
#94135 = CARTESIAN_POINT('Ctrl Pts',(-19.5724445177316,34.7596471192283,124.606605437042)) ;
#94136 = CARTESIAN_POINT('Ctrl Pts',(-19.3639246090716,34.7695783113634,124.617042218712)) ;
#94137 = CARTESIAN_POINT('Ctrl Pts',(-19.1544758574248,34.7796204660084,124.590591195082)) ;
#94138 = CARTESIAN_POINT('Ctrl Pts',(-18.9558505145138,34.7895072270277,124.529297402871)) ;
#94139 = CARTESIAN_POINT('Ctrl Pts',(-18.7686968083178,34.799506528745,124.433626692028)) ;
#94140 = CARTESIAN_POINT('Ctrl Pts',(-18.6021840247918,34.8094273269117,124.307986921244)) ;
#94141 = CARTESIAN_POINT('Ctrl Pts',(-18.4584119572292,34.8194613805084,124.153654294584)) ;
#94142 = CARTESIAN_POINT('Ctrl Pts',(-18.3447544148885,34.8293844980748,123.978681451143)) ;
#94143 = CARTESIAN_POINT('Ctrl Pts',(-18.2621745210567,34.839440621574,123.784088516026)) ;
#94144 = CARTESIAN_POINT('Ctrl Pts',(-18.2155383722637,34.8492860632288,123.582420343788)) ;
#94145 = CARTESIAN_POINT('Ctrl Pts',(-18.2038107378069,34.8592483643529,123.373323368424)) ;
#94146 = CARTESIAN_POINT('Ctrl Pts',(-18.2290111919867,34.8692768436281,123.163990289439)) ;
#94147 = CARTESIAN_POINT('Ctrl Pts',(-18.2893801467277,34.8791871971377,122.964592206024)) ;
#94148 = CARTESIAN_POINT('Ctrl Pts',(-18.3832066359481,34.8891220693149,122.777983967689)) ;
#94149 = CARTESIAN_POINT('Ctrl Pts',(-18.5094937411179,34.8991632069006,122.608837933746)) ;
#94150 = CARTESIAN_POINT('Ctrl Pts',(-18.6607872390357,34.9090503561152,122.466288539234)) ;
#94151 = CARTESIAN_POINT('Ctrl Pts',(-18.8361659801269,34.9190425908663,122.350681679079)) ;
#94152 = CARTESIAN_POINT('Ctrl Pts',(-19.0281614277122,34.9289912964292,122.267692173335)) ;
#94153 = CARTESIAN_POINT('Ctrl Pts',(-19.2312959474012,34.9389273648529,122.219071222119)) ;
#94154 = CARTESIAN_POINT('Ctrl Pts',(-19.4408495024323,34.9489130490687,122.206154757217)) ;
#94155 = CARTESIAN_POINT('Ctrl Pts',(-19.6505366751232,34.9589534756374,122.230278766843)) ;
#94156 = CARTESIAN_POINT('Ctrl Pts',(-19.8489056304027,34.9687925891011,122.288911017026)) ;
#94157 = CARTESIAN_POINT('Ctrl Pts',(-20.0378790588203,34.9788223232769,122.382455859527)) ;
#94158 = CARTESIAN_POINT('Ctrl Pts',(-20.2072811356501,34.9888444227828,122.507735639608)) ;
#94159 = CARTESIAN_POINT('Ctrl Pts',(-20.3505219569194,34.9987128626763,122.657836929404)) ;
#94160 = CARTESIAN_POINT('Ctrl Pts',(-20.4678365377331,35.0087817273619,122.834011313283)) ;
#94161 = CARTESIAN_POINT('Ctrl Pts',(-20.5508879058607,35.0186244004605,123.023544378056)) ;
#94162 = CARTESIAN_POINT('Ctrl Pts',(-20.6010962673067,35.0285850346229,123.226835516513)) ;
#94163 = CARTESIAN_POINT('Ctrl Pts',(-20.6149388907068,35.0386229503011,123.437402293427)) ;
#94164 = CARTESIAN_POINT('Ctrl Pts',(-20.5927617556655,35.0484972251605,123.64382806409)) ;
#94165 = CARTESIAN_POINT('Ctrl Pts',(-20.533940744717,35.0585669755356,123.847160626017)) ;
#94166 = CARTESIAN_POINT('Ctrl Pts',(-20.4429777659414,35.0684002709101,124.032817622277)) ;
#94167 = CARTESIAN_POINT('Ctrl Pts',(-20.3192176608534,35.0784305683898,124.203541018578)) ;
#94168 = CARTESIAN_POINT('Ctrl Pts',(-20.167224581628,35.0884626548312,124.349771836117)) ;
#94169 = CARTESIAN_POINT('Ctrl Pts',(-19.995982217517,35.0982905833201,124.465363727968)) ;
#94170 = CARTESIAN_POINT('Ctrl Pts',(-19.8042655773191,35.1082866244309,124.551422942232)) ;
#94171 = CARTESIAN_POINT('Ctrl Pts',(-19.5998043362001,35.1183124365321,124.602646562785)) ;
#94172 = CARTESIAN_POINT('Ctrl Pts',(-19.392483135136,35.1281996714269,124.61765284484)) ;
#94173 = CARTESIAN_POINT('Ctrl Pts',(-19.1838143214605,35.138176537638,124.596588861163)) ;
#94174 = CARTESIAN_POINT('Ctrl Pts',(-18.9815944355793,35.1481694815098,124.539544123873)) ;
#94175 = CARTESIAN_POINT('Ctrl Pts',(-18.7916564364344,35.1582074041811,124.447621099837)) ;
#94176 = CARTESIAN_POINT('Ctrl Pts',(-18.6235856865479,35.1680558684428,124.326680955003)) ;
#94177 = CARTESIAN_POINT('Ctrl Pts',(-18.4767269403657,35.1780477351868,124.176530858899)) ;
#94178 = CARTESIAN_POINT('Ctrl Pts',(-18.3589196063816,35.187965467228,124.004467621855)) ;
#94179 = CARTESIAN_POINT('Ctrl Pts',(-18.2717855263324,35.1979936521233,123.81251148209)) ;
#94180 = CARTESIAN_POINT('Ctrl Pts',(-18.2199640334134,35.2078788101721,123.611253905476)) ;
#94181 = CARTESIAN_POINT('Ctrl Pts',(-18.2031956371847,35.2178681707138,123.401912409714)) ;
#94182 = CARTESIAN_POINT('Ctrl Pts',(-18.2235772720183,35.2279093276482,123.191802025504)) ;
#94183 = CARTESIAN_POINT('Ctrl Pts',(-18.2786256484142,35.2377419111033,122.992558402953)) ;
#94184 = CARTESIAN_POINT('Ctrl Pts',(-18.368354396515,35.2477361310653,122.802574696056)) ;
#94185 = CARTESIAN_POINT('Ctrl Pts',(-18.4904752618844,35.2577642328526,122.630717578869)) ;
#94186 = CARTESIAN_POINT('Ctrl Pts',(-18.6381538690012,35.2676441774757,122.484653314994)) ;
#94187 = CARTESIAN_POINT('Ctrl Pts',(-18.810661504175,35.2776345040327,122.364871614765)) ;
#94188 = CARTESIAN_POINT('Ctrl Pts',(-19.0004190147032,35.287575435687,122.277289202281)) ;
#94189 = CARTESIAN_POINT('Ctrl Pts',(-19.2033735677859,35.2975625541899,122.223445030743)) ;
#94190 = CARTESIAN_POINT('Ctrl Pts',(-19.4135608790343,35.3075958870871,122.205909966767)) ;
#94191 = CARTESIAN_POINT('Ctrl Pts',(-19.6201740321461,35.3174619915319,122.224414931314)) ;
#94192 = CARTESIAN_POINT('Ctrl Pts',(-19.8244618434658,35.3275281054122,122.279549956183)) ;
#94193 = CARTESIAN_POINT('Ctrl Pts',(-20.0121134275938,35.3373841171806,122.367450475576)) ;
#94194 = CARTESIAN_POINT('Ctrl Pts',(-20.1843772800445,35.3473788208119,122.487755297153)) ;
#94195 = CARTESIAN_POINT('Ctrl Pts',(-20.3333683555164,35.3574101565368,122.637013322784)) ;
#94196 = CARTESIAN_POINT('Ctrl Pts',(-20.452467682773,35.3672766817405,122.806847362227)) ;
#94197 = CARTESIAN_POINT('Ctrl Pts',(-20.5416380634157,35.3772641097863,122.996911545237)) ;
#94198 = CARTESIAN_POINT('Ctrl Pts',(-20.5963428038988,35.3872090394727,123.19873346646)) ;
#94199 = CARTESIAN_POINT('Ctrl Pts',(-20.6152390421331,35.3972539575812,123.409042039138)) ;
#94200 = CARTESIAN_POINT('Ctrl Pts',(-20.5978399936746,35.4071159271951,123.615657183607)) ;
#94201 = CARTESIAN_POINT('Ctrl Pts',(-20.544536085097,35.4171079952163,123.818824897124)) ;
#94202 = CARTESIAN_POINT('Ctrl Pts',(-20.4572545241193,35.4270389205909,124.008498798573)) ;
#94203 = CARTESIAN_POINT('Ctrl Pts',(-20.3384335703723,35.4369895488143,124.180653521946)) ;
#94204 = CARTESIAN_POINT('Ctrl Pts',(-20.1908529589591,35.4469897878734,124.33041662932)) ;
#94205 = CARTESIAN_POINT('Ctrl Pts',(-20.0188759708664,35.4570182432426,124.452357639647)) ;
#94206 = CARTESIAN_POINT('Ctrl Pts',(-19.8315424534969,35.4668842778259,124.541414633258)) ;
#94207 = CARTESIAN_POINT('Ctrl Pts',(-19.6291530073058,35.4768765995733,124.597623086158)) ;
#94208 = CARTESIAN_POINT('Ctrl Pts',(-19.4213004974954,35.4868088892503,124.617752074069)) ;
#94209 = CARTESIAN_POINT('Ctrl Pts',(-19.2116664499479,35.4968105342211,124.601578995507)) ;
#94210 = CARTESIAN_POINT('Ctrl Pts',(-18.9405974517021,35.5101231676371,124.53180213647)) ;
#94211 = CARTESIAN_POINT('Ctrl Pts',(-18.6953540228748,35.5233549170187,124.393908226192)) ;
#94212 = CARTESIAN_POINT('Ctrl Pts',(-18.4950059156847,35.5366781818358,124.198224853695)) ;
#94213 = CARTESIAN_POINT('Ctrl Pts',(-18.3736553940196,35.5465538880534,124.029742286232)) ;
#94214 = CARTESIAN_POINT('Ctrl Pts',(-18.2821355436399,35.5565434791535,123.840747243636)) ;
#94215 = CARTESIAN_POINT('Ctrl Pts',(-18.2250326582066,35.5664705756089,123.639986013485)) ;
#94216 = CARTESIAN_POINT('Ctrl Pts',(-18.2034246479505,35.5764957241134,123.430355343543)) ;
#94217 = CARTESIAN_POINT('Ctrl Pts',(-18.2182221832867,35.5863913782601,123.222826157615)) ;
#94218 = CARTESIAN_POINT('Ctrl Pts',(-18.2690819887798,35.5963949126383,123.018783641525)) ;
#94219 = CARTESIAN_POINT('Ctrl Pts',(-18.3544809937856,35.6063800510784,122.826985667331)) ;
#94220 = CARTESIAN_POINT('Ctrl Pts',(-18.472633727841,35.6164159756738,122.652198283196)) ;
#94221 = CARTESIAN_POINT('Ctrl Pts',(-18.6164712344706,35.6262672511014,122.503192800069)) ;
#94222 = CARTESIAN_POINT('Ctrl Pts',(-18.7860470108393,35.6362595122628,122.379193128309)) ;
#94223 = CARTESIAN_POINT('Ctrl Pts',(-18.9756946767603,35.6462993962804,122.286567038597)) ;
#94224 = CARTESIAN_POINT('Ctrl Pts',(-19.1742898648837,35.6561341707828,122.228953637349)) ;
#94225 = CARTESIAN_POINT('Ctrl Pts',(-19.384854864519,35.6662105518031,122.206080561557)) ;
#94226 = CARTESIAN_POINT('Ctrl Pts',(-19.5914292540954,35.6760568249538,122.21974207516)) ;
#94227 = CARTESIAN_POINT('Ctrl Pts',(-19.8644346438615,35.689421346239,122.28616654284)) ;
#94228 = CARTESIAN_POINT('Ctrl Pts',(-20.1107389994271,35.7026275906734,122.421071166414)) ;
#94229 = CARTESIAN_POINT('Ctrl Pts',(-20.31289569483,35.7158925453506,122.613085924931)) ;
#94230 = CARTESIAN_POINT('Ctrl Pts',(-20.4382108480598,35.7259248259023,122.782748300882)) ;
#94231 = CARTESIAN_POINT('Ctrl Pts',(-20.5310088705917,35.7358335594202,122.969242542732)) ;
#94232 = CARTESIAN_POINT('Ctrl Pts',(-20.5907141773858,35.7457711102877,123.169457067613)) ;
#94233 = CARTESIAN_POINT('Ctrl Pts',(-20.6147942179348,35.7558009578817,123.378913702247)) ;
#94234 = CARTESIAN_POINT('Ctrl Pts',(-20.598471691995,35.7690360978021,123.656761562465)) ;
#94235 = CARTESIAN_POINT('Ctrl Pts',(-20.4868792880066,35.7857045621733,123.993019501835)) ;
#94236 = CARTESIAN_POINT('Ctrl Pts',(-20.2251471753778,35.8055755740472,124.324870618107)) ;
#94237 = CARTESIAN_POINT('Ctrl Pts',(-19.9231598977756,35.8222826584301,124.511857504342)) ;
#94238 = CARTESIAN_POINT('Ctrl Pts',(-19.6579097068022,35.8354599397407,124.591780242991)) ;
#94239 = CARTESIAN_POINT('Ctrl Pts',(-19.3810458831154,35.8487274002548,124.625650252468)) ;
#94240 = CARTESIAN_POINT('Ctrl Pts',(-19.0312456986032,35.865341290942,124.576426819404)) ;
#94241 = CARTESIAN_POINT('Ctrl Pts',(-18.6565465864892,35.8852900903694,124.377542753024)) ;
#94242 = CARTESIAN_POINT('Ctrl Pts',(-18.3727285742286,35.9052112019003,124.063195064491)) ;
#94243 = CARTESIAN_POINT('Ctrl Pts',(-18.2127928629799,35.9250776500732,123.672157267493)) ;
#94244 = CARTESIAN_POINT('Ctrl Pts',(-18.1960231038597,35.9451039966903,123.246720272053)) ;
#94245 = CARTESIAN_POINT('Ctrl Pts',(-18.324491777266,35.9649660410798,122.844336458212)) ;
#94246 = CARTESIAN_POINT('Ctrl Pts',(-18.5830322138588,35.984911343761,122.508241861677)) ;
#94247 = CARTESIAN_POINT('Ctrl Pts',(-18.9399428040037,36.0048066508198,122.281138146652)) ;
#94248 = CARTESIAN_POINT('Ctrl Pts',(-19.3527184258083,36.0246999209875,122.188728146812)) ;
#94249 = CARTESIAN_POINT('Ctrl Pts',(-19.7737311453565,36.0446655136679,122.243004299579)) ;
#94250 = CARTESIAN_POINT('Ctrl Pts',(-20.1494256886425,36.0645408373527,122.436571014083)) ;
#94251 = CARTESIAN_POINT('Ctrl Pts',(-20.4382670267908,36.0845158999277,122.747982676867)) ;
#94252 = CARTESIAN_POINT('Ctrl Pts',(-20.6027131365231,36.1044683095588,123.13905599893)) ;
#94253 = CARTESIAN_POINT('Ctrl Pts',(-20.6245287238263,36.1243043637949,123.560259112784)) ;
#94254 = CARTESIAN_POINT('Ctrl Pts',(-20.5008694097332,36.1442822752124,123.966645271116)) ;
#94255 = CARTESIAN_POINT('Ctrl Pts',(-20.2463345181827,36.1642003247159,124.305097725016)) ;
#94256 = CARTESIAN_POINT('Ctrl Pts',(-19.8929821410224,36.184068468484,124.536788661941)) ;
#94257 = CARTESIAN_POINT('Ctrl Pts',(-19.4780341435189,36.2041193250713,124.634204632469)) ;
#94258 = CARTESIAN_POINT('Ctrl Pts',(-19.060185282991,36.2238997615272,124.585267869156)) ;
#94259 = CARTESIAN_POINT('Ctrl Pts',(-18.6792614121707,36.243929817205,124.39500532448)) ;
#94260 = CARTESIAN_POINT('Ctrl Pts',(-18.3887179287721,36.2638109223798,124.087851926812)) ;
#94261 = CARTESIAN_POINT('Ctrl Pts',(-18.2193877315781,36.2836913847476,123.700582700507)) ;
#94262 = CARTESIAN_POINT('Ctrl Pts',(-18.1923469123526,36.303676531892,123.276491971302)) ;
#94263 = CARTESIAN_POINT('Ctrl Pts',(-18.3111820591187,36.3235671104283,122.870593111507)) ;
#94264 = CARTESIAN_POINT('Ctrl Pts',(-18.5608265214419,36.3434611303027,122.529122738286)) ;
#94265 = CARTESIAN_POINT('Ctrl Pts',(-18.9123819811256,36.3633825750291,122.292957365866)) ;
#94266 = CARTESIAN_POINT('Ctrl Pts',(-19.3229431016927,36.3832807130846,122.190279954938)) ;
#94267 = CARTESIAN_POINT('Ctrl Pts',(-19.7472712121546,36.4033514683006,122.235041107038)) ;
#94268 = CARTESIAN_POINT('Ctrl Pts',(-20.1256425048648,36.4231370183519,122.419154459229)) ;
#94269 = CARTESIAN_POINT('Ctrl Pts',(-20.4220170919712,36.4431200932292,122.723507834447)) ;
#94270 = CARTESIAN_POINT('Ctrl Pts',(-20.5955265060614,36.4630291758752,123.109641805405)) ;
#94271 = CARTESIAN_POINT('Ctrl Pts',(-20.6279926946846,36.4828877349979,123.530692392537)) ;
#94272 = CARTESIAN_POINT('Ctrl Pts',(-20.5133248607848,36.5029311788366,123.941072248336)) ;
#94273 = CARTESIAN_POINT('Ctrl Pts',(-20.3093892008094,36.5194312435658,124.226640164465)) ;
#94274 = CARTESIAN_POINT('Ctrl Pts',(-20.0922743624117,36.5328209834147,124.405775190964)) ;
#94275 = CARTESIAN_POINT('Ctrl Pts',(-19.9119758940525,36.5426778846231,124.50796979735)) ;
#94276 = CARTESIAN_POINT('Ctrl Pts',(-19.7142026000164,36.5526694104696,124.578640998708)) ;
#94277 = CARTESIAN_POINT('Ctrl Pts',(-19.5084996701913,36.5625940909206,124.613748998774)) ;
#94278 = CARTESIAN_POINT('Ctrl Pts',(-19.2980711955176,36.572604680965,124.612675114737)) ;
#94279 = CARTESIAN_POINT('Ctrl Pts',(-19.0237189426049,36.5858639416687,124.563191698684)) ;
#94280 = CARTESIAN_POINT('Ctrl Pts',(-18.7670047191078,36.5992150168189,124.442157992016)) ;
#94281 = CARTESIAN_POINT('Ctrl Pts',(-18.5548978247711,36.6124213260537,124.262901583435)) ;
#94282 = CARTESIAN_POINT('Ctrl Pts',(-18.4202072442688,36.622408159644,124.101894853874)) ;
#94283 = CARTESIAN_POINT('Ctrl Pts',(-18.315747816348,36.6323608871401,123.92055502923)) ;
#94284 = CARTESIAN_POINT('Ctrl Pts',(-18.2438653268003,36.6424089839817,123.721943551495)) ;
#94285 = CARTESIAN_POINT('Ctrl Pts',(-18.2080589031175,36.6522504408535,123.518146535911)) ;
#94286 = CARTESIAN_POINT('Ctrl Pts',(-18.2077355281506,36.662236707767,123.3082383145)) ;
#94287 = CARTESIAN_POINT('Ctrl Pts',(-18.2435931093309,36.6721733086674,123.102404801807)) ;
#94288 = CARTESIAN_POINT('Ctrl Pts',(-18.3155367278071,36.6822232514545,122.903771931115)) ;
#94289 = CARTESIAN_POINT('Ctrl Pts',(-18.4186658169043,36.6920734511402,122.724179668782)) ;
#94290 = CARTESIAN_POINT('Ctrl Pts',(-18.5526159505733,36.7020463560723,122.562916709314)) ;
#94291 = CARTESIAN_POINT('Ctrl Pts',(-18.7130217748443,36.712044730552,122.427034994894)) ;
#94292 = CARTESIAN_POINT('Ctrl Pts',(-18.8950290521288,36.7220649044219,122.320985373851)) ;
#94293 = CARTESIAN_POINT('Ctrl Pts',(-19.0902841742662,36.7319659483639,122.248841931777)) ;
#94294 = CARTESIAN_POINT('Ctrl Pts',(-19.2968494423397,36.7419547520882,122.211043582712)) ;
#94295 = CARTESIAN_POINT('Ctrl Pts',(-19.5063417767204,36.7519202189201,122.209838370568)) ;
#94296 = CARTESIAN_POINT('Ctrl Pts',(-19.7116920199838,36.761823781193,122.244315917006)) ;
#94297 = CARTESIAN_POINT('Ctrl Pts',(-19.9109467915122,36.771884459071,122.315177857541)) ;
#94298 = CARTESIAN_POINT('Ctrl Pts',(-20.0910226160667,36.7817247570205,122.417070031681)) ;
#94299 = CARTESIAN_POINT('Ctrl Pts',(-20.2544023838609,36.7917877519299,122.551425204695)) ;
#94300 = CARTESIAN_POINT('Ctrl Pts',(-20.3895668613944,36.8016820460771,122.709563463652)) ;
#94301 = CARTESIAN_POINT('Ctrl Pts',(-20.4961913136118,36.8116238437739,122.889298746272)) ;
#94302 = CARTESIAN_POINT('Ctrl Pts',(-20.5705305835063,36.821626421303,123.086035728919)) ;
#94303 = CARTESIAN_POINT('Ctrl Pts',(-20.6093785768272,36.8316608852241,123.293373251743)) ;
#94304 = CARTESIAN_POINT('Ctrl Pts',(-20.6119178337736,36.8415070237452,123.500360827497)) ;
#94305 = CARTESIAN_POINT('Ctrl Pts',(-20.5784854232737,36.8514881969822,123.707499070501)) ;
#94306 = CARTESIAN_POINT('Ctrl Pts',(-20.5097396908624,36.8614404909394,123.905117972074)) ;
#94307 = CARTESIAN_POINT('Ctrl Pts',(-20.407482017507,36.871439286074,124.088793923392)) ;
#94308 = CARTESIAN_POINT('Ctrl Pts',(-20.2740542798669,36.8814783943348,124.252304034423)) ;
#94309 = CARTESIAN_POINT('Ctrl Pts',(-20.1179432190855,36.891303335774,124.387573713535)) ;
#94310 = CARTESIAN_POINT('Ctrl Pts',(-19.9367725759517,36.9013580228484,124.496449032076)) ;
#94311 = CARTESIAN_POINT('Ctrl Pts',(-19.7414996675405,36.9113008277885,124.571043200714)) ;
#94312 = CARTESIAN_POINT('Ctrl Pts',(-19.5371698887816,36.921204613785,124.611070181007)) ;
#94313 = CARTESIAN_POINT('Ctrl Pts',(-19.3260077881404,36.9312514303498,124.614939096116)) ;
#94314 = CARTESIAN_POINT('Ctrl Pts',(-19.1204430965301,36.9411469498285,124.582756712928)) ;
#94315 = CARTESIAN_POINT('Ctrl Pts',(-18.9203358370429,36.951209035153,124.51425755505)) ;
#94316 = CARTESIAN_POINT('Ctrl Pts',(-18.7390960653192,36.9610517461109,124.414360045597)) ;
#94317 = CARTESIAN_POINT('Ctrl Pts',(-18.5752583735253,36.9710424634169,124.282977394768)) ;
#94318 = CARTESIAN_POINT('Ctrl Pts',(-18.4375935817298,36.9809705465135,124.126081575226)) ;
#94319 = CARTESIAN_POINT('Ctrl Pts',(-18.3282968902032,36.9909584766253,123.946781567266)) ;
#94320 = CARTESIAN_POINT('Ctrl Pts',(-18.2517622222027,37.0009943027526,123.750174853186)) ;
#94321 = CARTESIAN_POINT('Ctrl Pts',(-18.21094080092,37.0108496398662,123.547034402322)) ;
#94322 = CARTESIAN_POINT('Ctrl Pts',(-18.2056086306045,37.0208473747163,123.336940861703)) ;
#94323 = CARTESIAN_POINT('Ctrl Pts',(-18.2364910695432,37.0307552787008,123.130938239226)) ;
#94324 = CARTESIAN_POINT('Ctrl Pts',(-18.3030269286301,37.0407663532492,122.931261335082)) ;
#94325 = CARTESIAN_POINT('Ctrl Pts',(-18.4037673321845,37.0507942087849,122.746069536931)) ;
#94326 = CARTESIAN_POINT('Ctrl Pts',(-18.5326081036751,37.0606518026901,122.583754403293)) ;
#94327 = CARTESIAN_POINT('Ctrl Pts',(-18.6900546143818,37.0706784895282,122.443591540943)) ;
#94328 = CARTESIAN_POINT('Ctrl Pts',(-18.8697606942828,37.0807071586819,122.3333196009)) ;
#94329 = CARTESIAN_POINT('Ctrl Pts',(-19.0621377136588,37.0905523669633,122.256989628151)) ;
#94330 = CARTESIAN_POINT('Ctrl Pts',(-19.2677422078546,37.1005430559265,122.214048078359)) ;
#94331 = CARTESIAN_POINT('Ctrl Pts',(-19.47867850993,37.1105809322087,122.207898021882)) ;
#94332 = CARTESIAN_POINT('Ctrl Pts',(-19.6835147698545,37.120425309851,122.23752146593)) ;
#94333 = CARTESIAN_POINT('Ctrl Pts',(-19.882996079095,37.1304101142424,122.302778957761)) ;
#94334 = CARTESIAN_POINT('Ctrl Pts',(-20.067369358765,37.1403496444609,122.401180186944)) ;
#94335 = CARTESIAN_POINT('Ctrl Pts',(-20.2334482035673,37.1503893324978,122.531409803417)) ;
#94336 = CARTESIAN_POINT('Ctrl Pts',(-20.3723615313859,37.1602776218661,122.686081213826)) ;
#94337 = CARTESIAN_POINT('Ctrl Pts',(-20.4837564475809,37.1702667455509,122.864096057991)) ;
#94338 = CARTESIAN_POINT('Ctrl Pts',(-20.5621702859723,37.1802267552255,123.0582461287)) ;
#94339 = CARTESIAN_POINT('Ctrl Pts',(-20.6059089775534,37.1901271849298,123.26174306091)) ;
#94340 = CARTESIAN_POINT('Ctrl Pts',(-20.6137506161671,37.2001702663365,123.472725765684)) ;
#94341 = CARTESIAN_POINT('Ctrl Pts',(-20.5852316490187,37.2100776602442,123.679059652411)) ;
#94342 = CARTESIAN_POINT('Ctrl Pts',(-20.5210198031363,37.2200893912333,123.879505634922)) ;
#94343 = CARTESIAN_POINT('Ctrl Pts',(-20.4224065161209,37.2301216089481,124.065948284503)) ;
#94344 = CARTESIAN_POINT('Ctrl Pts',(-20.2954706478781,37.2399741181943,124.229610475779)) ;
#94345 = CARTESIAN_POINT('Ctrl Pts',(-20.1408283407611,37.2499320547373,124.370729348929)) ;
#94346 = CARTESIAN_POINT('Ctrl Pts',(-19.9624090787008,37.2599709247456,124.483433619568)) ;
#94347 = CARTESIAN_POINT('Ctrl Pts',(-19.770458867892,37.2698440799038,124.562502735803)) ;
#94348 = CARTESIAN_POINT('Ctrl Pts',(-19.563646481703,37.2799173547535,124.607865009529)) ;
#94349 = CARTESIAN_POINT('Ctrl Pts',(-19.3573352708199,37.2897376719309,124.616683319758)) ;
#94350 = CARTESIAN_POINT('Ctrl Pts',(-19.1473126860865,37.2998163577244,124.589037296444)) ;
#94351 = CARTESIAN_POINT('Ctrl Pts',(-18.9497170318197,37.3096678691075,124.526820893084)) ;
#94352 = CARTESIAN_POINT('Ctrl Pts',(-18.7617822357577,37.3197413154142,124.42928813137)) ;
#94353 = CARTESIAN_POINT('Ctrl Pts',(-18.597472760088,37.3295825905389,124.303521853965)) ;
#94354 = CARTESIAN_POINT('Ctrl Pts',(-18.4549977478559,37.3395676901956,124.14938498897)) ;
#94355 = CARTESIAN_POINT('Ctrl Pts',(-18.3414230173114,37.3495751663299,123.972266878599)) ;
#94356 = CARTESIAN_POINT('Ctrl Pts',(-18.2608487024426,37.3594977540389,123.779863642835)) ;
#94357 = CARTESIAN_POINT('Ctrl Pts',(-18.2142702336131,37.3694843583122,123.575125917761)) ;
#94358 = CARTESIAN_POINT('Ctrl Pts',(-18.2042901750797,37.3795244866463,123.364303702255)) ;
#94359 = CARTESIAN_POINT('Ctrl Pts',(-18.230089300167,37.3893639211797,123.159042239126)) ;
#94360 = CARTESIAN_POINT('Ctrl Pts',(-18.292348591222,37.3994279756707,122.956858629565)) ;
#94361 = CARTESIAN_POINT('Ctrl Pts',(-18.3872136846563,37.4093188949079,122.77179662496)) ;
#94362 = CARTESIAN_POINT('Ctrl Pts',(-18.5136767800856,37.4193108882139,122.604078934525)) ;
#94363 = CARTESIAN_POINT('Ctrl Pts',(-18.6670285892271,37.4292737521732,122.461423780996)) ;
#94364 = CARTESIAN_POINT('Ctrl Pts',(-18.8415186482353,37.439178011991,122.34777734917)) ;
#94365 = CARTESIAN_POINT('Ctrl Pts',(-19.0361446502019,37.4492385025624,122.265052864531)) ;
#94366 = CARTESIAN_POINT('Ctrl Pts',(-19.2376613352379,37.4590788521934,122.218146467935)) ;
#94367 = CARTESIAN_POINT('Ctrl Pts',(-19.4488650147915,37.4691418276835,122.206437417777)) ;
#94368 = CARTESIAN_POINT('Ctrl Pts',(-19.655401912625,37.4790361478268,122.231332710315)) ;
#94369 = CARTESIAN_POINT('Ctrl Pts',(-19.8555475304082,37.4889778609584,122.291445911466)) ;
#94370 = CARTESIAN_POINT('Ctrl Pts',(-20.0434590938242,37.4989807507526,122.385921675626)) ;
#94371 = CARTESIAN_POINT('Ctrl Pts',(-20.2124620638897,37.509020607913,122.512333007315)) ;
#94372 = CARTESIAN_POINT('Ctrl Pts',(-20.3542123192198,37.5188447887507,122.662567186041)) ;
#94373 = CARTESIAN_POINT('Ctrl Pts',(-20.4706388940175,37.5289017622539,122.839032422264)) ;
#94374 = CARTESIAN_POINT('Ctrl Pts',(-20.5533481377994,37.5388298864409,123.030678499673)) ;
#94375 = CARTESIAN_POINT('Ctrl Pts',(-20.6021910243834,37.5487835815143,123.234157885621)) ;
#94376 = CARTESIAN_POINT('Ctrl Pts',(-20.6147789290021,37.5588297750896,123.444983226702)) ;
#94377 = CARTESIAN_POINT('Ctrl Pts',(-20.5912446307406,37.5686778774495,123.650677843784)) ;
#94378 = CARTESIAN_POINT('Ctrl Pts',(-20.5322977294256,37.5786394656771,123.851625109879)) ;
#94379 = CARTESIAN_POINT('Ctrl Pts',(-20.4384823229094,37.5886681358334,124.040450631407)) ;
#94380 = CARTESIAN_POINT('Ctrl Pts',(-20.3148504709201,37.5985784387151,124.208137758696)) ;
#94381 = CARTESIAN_POINT('Ctrl Pts',(-20.1639729630822,37.608513322523,124.352574750252)) ;
#94382 = CARTESIAN_POINT('Ctrl Pts',(-19.9883521541963,37.6185544642137,124.469690929429)) ;
#94383 = CARTESIAN_POINT('Ctrl Pts',(-19.7980711005547,37.6284415853776,124.553374455304)) ;
#94384 = CARTESIAN_POINT('Ctrl Pts',(-19.5941096168226,37.6384339282262,124.603607299162)) ;
#94385 = CARTESIAN_POINT('Ctrl Pts',(-19.3854196090159,37.6483822294501,124.617543166686)) ;
#94386 = CARTESIAN_POINT('Ctrl Pts',(-19.1776942445068,37.6583198071322,124.59536101191)) ;
#94387 = CARTESIAN_POINT('Ctrl Pts',(-18.9759006440841,37.6683063815828,124.537360444332)) ;
#94388 = CARTESIAN_POINT('Ctrl Pts',(-18.7865662535122,37.6783351914913,124.44460190326)) ;
#94389 = CARTESIAN_POINT('Ctrl Pts',(-18.6186516713856,37.6882135127981,124.322405731051)) ;
#94390 = CARTESIAN_POINT('Ctrl Pts',(-18.4724895997512,37.6982051601455,124.171531255687)) ;
#94391 = CARTESIAN_POINT('Ctrl Pts',(-18.3546061642673,37.7082396835832,123.996595633162)) ;
#94392 = CARTESIAN_POINT('Ctrl Pts',(-18.2699432637342,37.7181030404618,123.807284330611)) ;
#94393 = CARTESIAN_POINT('Ctrl Pts',(-18.2183482689039,37.7281732671421,123.601982903703)) ;
#94394 = CARTESIAN_POINT('Ctrl Pts',(-18.2035357130047,37.7380155752768,123.395589044217)) ;
#94395 = CARTESIAN_POINT('Ctrl Pts',(-18.2242703516,37.7479763073002,123.187217231748)) ;
#94396 = CARTESIAN_POINT('Ctrl Pts',(-18.2817100316851,37.7580141964983,122.984164159135)) ;
#94397 = CARTESIAN_POINT('Ctrl Pts',(-18.3717050421418,37.7678884794172,122.797069705704)) ;
#94398 = CARTESIAN_POINT('Ctrl Pts',(-18.4951947219653,37.7779582240346,122.625155864398)) ;
#94399 = CARTESIAN_POINT('Ctrl Pts',(-18.6430558845432,37.7877915343803,122.48065748324)) ;
#94400 = CARTESIAN_POINT('Ctrl Pts',(-18.8168224196288,37.7978217777329,122.361207121415)) ;
#94401 = CARTESIAN_POINT('Ctrl Pts',(-19.0089987621036,37.8078540657113,122.274295745002)) ;
#94402 = CARTESIAN_POINT('Ctrl Pts',(-19.2090434153419,37.8176812421794,122.22266624776)) ;
#94403 = CARTESIAN_POINT('Ctrl Pts',(-19.418687613471,37.8276866250463,122.205831123494)) ;
#94404 = CARTESIAN_POINT('Ctrl Pts',(-19.6276535689647,37.837669264039,122.225683029359)) ;
#94405 = CARTESIAN_POINT('Ctrl Pts',(-19.8311151455432,37.8477133311756,122.282093503812)) ;
#94406 = CARTESIAN_POINT('Ctrl Pts',(-20.0176419945496,37.8575345499796,122.370645995862)) ;
#94407 = CARTESIAN_POINT('Ctrl Pts',(-20.189959189523,37.8675713889177,122.492420091095)) ;
#94408 = CARTESIAN_POINT('Ctrl Pts',(-20.3379110108571,37.8775958010154,122.642508840557)) ;
#94409 = CARTESIAN_POINT('Ctrl Pts',(-20.455873413021,37.8874478854207,122.812760429535)) ;
#94410 = CARTESIAN_POINT('Ctrl Pts',(-20.5439817121948,37.8974387821639,123.003399294509)) ;
#94411 = CARTESIAN_POINT('Ctrl Pts',(-20.5974030957695,37.9073567740648,123.204972770783)) ;
#94412 = CARTESIAN_POINT('Ctrl Pts',(-20.6152555329901,37.9173848895218,123.415021611092)) ;
#94413 = CARTESIAN_POINT('Ctrl Pts',(-20.5967206689066,37.927270065464,123.622015755364)) ;
#94414 = CARTESIAN_POINT('Ctrl Pts',(-20.5424483524076,37.9372594238708,123.824894035704)) ;
#94415 = CARTESIAN_POINT('Ctrl Pts',(-20.4529119954387,37.9473005714511,124.01606111414)) ;
#94416 = CARTESIAN_POINT('Ctrl Pts',(-20.3343454418545,37.9571331944576,124.185386044338)) ;
#94417 = CARTESIAN_POINT('Ctrl Pts',(-20.1862012412486,37.9671272655683,124.334369804642)) ;
#94418 = CARTESIAN_POINT('Ctrl Pts',(-20.0135915966174,37.9771559232092,124.455455360965)) ;
#94419 = CARTESIAN_POINT('Ctrl Pts',(-19.8254446591091,37.987040249402,124.543643786109)) ;
#94420 = CARTESIAN_POINT('Ctrl Pts',(-19.6233091240943,37.9970059928926,124.598773682631)) ;
#94421 = CARTESIAN_POINT('Ctrl Pts',(-19.413348853934,38.0070343720238,124.61778442774)) ;
#94422 = CARTESIAN_POINT('Ctrl Pts',(-19.2058864365111,38.0169352182307,124.600587770321)) ;
#94423 = CARTESIAN_POINT('Ctrl Pts',(-19.001424766505,38.0269938756478,124.546746006836)) ;
#94424 = CARTESIAN_POINT('Ctrl Pts',(-18.8131022714077,38.0368514384297,124.460160333376)) ;
#94425 = CARTESIAN_POINT('Ctrl Pts',(-18.6390069711874,38.0469198409829,124.339821058919)) ;
#94426 = CARTESIAN_POINT('Ctrl Pts',(-18.4916162272033,38.0567752397225,124.19417910208)) ;
#94427 = CARTESIAN_POINT('Ctrl Pts',(-18.3695561098639,38.0667701067964,124.023151838683)) ;
#94428 = CARTESIAN_POINT('Ctrl Pts',(-18.2791222072154,38.0768014017799,123.832631960833)) ;
#94429 = CARTESIAN_POINT('Ctrl Pts',(-18.2237417192545,38.0866679265065,123.63272885643)) ;
#94430 = CARTESIAN_POINT('Ctrl Pts',(-18.2033366603829,38.0966553972022,123.423780120613)) ;
#94431 = CARTESIAN_POINT('Ctrl Pts',(-18.2193409243599,38.106600156766,123.215291220018)) ;
#94432 = CARTESIAN_POINT('Ctrl Pts',(-18.2719426736711,38.1166457127149,123.010781898798)) ;
#94433 = CARTESIAN_POINT('Ctrl Pts',(-18.3574578509409,38.12650530109,122.821937896345)) ;
#94434 = CARTESIAN_POINT('Ctrl Pts',(-18.4758459936712,38.136506256226,122.648227483148)) ;
#94435 = CARTESIAN_POINT('Ctrl Pts',(-18.6211084110624,38.1464104835036,122.499006529391)) ;
#94436 = CARTESIAN_POINT('Ctrl Pts',(-18.7923421380688,38.1564525603987,122.375568101982)) ;
#94437 = CARTESIAN_POINT('Ctrl Pts',(-18.9798774392675,38.1663601730849,122.284845061643)) ;
#94438 = CARTESIAN_POINT('Ctrl Pts',(-19.1832185039879,38.1764147037006,122.227224424834)) ;
#94439 = CARTESIAN_POINT('Ctrl Pts',(-19.3894682522631,38.1862754902495,122.206072297823)) ;
#94440 = CARTESIAN_POINT('Ctrl Pts',(-19.5990134009756,38.1962692453206,122.220862900909)) ;
#94441 = CARTESIAN_POINT('Ctrl Pts',(-19.8015016142954,38.2061946055606,122.271381265112)) ;
#94442 = CARTESIAN_POINT('Ctrl Pts',(-19.9940600894447,38.2162225349558,122.357136882958)) ;
#94443 = CARTESIAN_POINT('Ctrl Pts',(-20.1665038918111,38.2261088017551,122.473213620408)) ;
#94444 = CARTESIAN_POINT('Ctrl Pts',(-20.3184039299682,38.2361405706534,122.619467232324)) ;
#94445 = CARTESIAN_POINT('Ctrl Pts',(-20.4409493063373,38.246022166497,122.787261758585)) ;
#94446 = CARTESIAN_POINT('Ctrl Pts',(-20.534186053703,38.256084051965,122.977102546347)) ;
#94447 = CARTESIAN_POINT('Ctrl Pts',(-20.5919300858513,38.2659414859838,123.17615703249)) ;
#94448 = CARTESIAN_POINT('Ctrl Pts',(-20.6149768459741,38.2759347290258,123.384952025093)) ;
#94449 = CARTESIAN_POINT('Ctrl Pts',(-20.601518044384,38.2858654899121,123.593303693139)) ;
#94450 = CARTESIAN_POINT('Ctrl Pts',(-20.5353365143575,38.2992144821093,123.866067761415)) ;
#94451 = CARTESIAN_POINT('Ctrl Pts',(-20.3999665225162,38.3124828549258,124.11359517286)) ;
#94452 = CARTESIAN_POINT('Ctrl Pts',(-20.2075244309159,38.3257657963101,124.315918886567)) ;
#94453 = CARTESIAN_POINT('Ctrl Pts',(-20.0375783875477,38.3358085821523,124.441187536565)) ;
#94454 = CARTESIAN_POINT('Ctrl Pts',(-19.8521843982202,38.3456585247044,124.533448788137)) ;
#94455 = CARTESIAN_POINT('Ctrl Pts',(-19.6507787179192,38.3556557576234,124.59349689104)) ;
#94456 = CARTESIAN_POINT('Ctrl Pts',(-19.4415865176942,38.3656706529579,124.617384094743)) ;
#94457 = CARTESIAN_POINT('Ctrl Pts',(-19.1637206293595,38.3789103295961,124.600727750445)) ;
#94458 = CARTESIAN_POINT('Ctrl Pts',(-18.8297225787506,38.3954575540015,124.490328714374)) ;
#94459 = CARTESIAN_POINT('Ctrl Pts',(-18.5515626138001,38.4121049911325,124.271315950757)) ;
#94460 = CARTESIAN_POINT('Ctrl Pts',(-18.3844931449848,38.4253944886108,124.047426550123)) ;
#94461 = CARTESIAN_POINT('Ctrl Pts',(-18.2905580247647,38.4352678964331,123.862315124557)) ;
#94462 = CARTESIAN_POINT('Ctrl Pts',(-18.2290723599006,38.4453202740258,123.660137252255)) ;
#94463 = CARTESIAN_POINT('Ctrl Pts',(-18.2040857486396,38.4552239275667,123.453418477981)) ;
#94464 = CARTESIAN_POINT('Ctrl Pts',(-18.214910209593,38.465168196562,123.244668963896)) ;
#94465 = CARTESIAN_POINT('Ctrl Pts',(-18.2776890327656,38.4784992048947,122.971450485448)) ;
#94466 = CARTESIAN_POINT('Ctrl Pts',(-18.4435332627468,38.495120785419,122.659461049717)) ;
#94467 = CARTESIAN_POINT('Ctrl Pts',(-18.704296009692,38.5116634561174,122.423288645421)) ;
#94468 = CARTESIAN_POINT('Ctrl Pts',(-18.9539077831196,38.5250126156803,122.295137360365)) ;
#94469 = CARTESIAN_POINT('Ctrl Pts',(-19.2195501392417,38.5382407658398,122.212666362541)) ;
#94470 = CARTESIAN_POINT('Ctrl Pts',(-19.5728079711518,38.5548714429773,122.198403766473)) ;
#94471 = CARTESIAN_POINT('Ctrl Pts',(-19.976146658423,38.5747743822654,122.326687099106)) ;
#94472 = CARTESIAN_POINT('Ctrl Pts',(-20.3116532871837,38.5946772488687,122.584476695311)) ;
#94473 = CARTESIAN_POINT('Ctrl Pts',(-20.5398098955763,38.6145904139735,122.941266434743)) ;
#94474 = CARTESIAN_POINT('Ctrl Pts',(-20.6324050425988,38.6346262431149,123.357036122555)) ;
#94475 = CARTESIAN_POINT('Ctrl Pts',(-20.5783887869263,38.6544448179929,123.775059980348)) ;
#94476 = CARTESIAN_POINT('Ctrl Pts',(-20.3841956533743,38.6744151190349,124.152516163581)) ;
#94477 = CARTESIAN_POINT('Ctrl Pts',(-20.073957019028,38.6943066513995,124.440209371613)) ;
#94478 = CARTESIAN_POINT('Ctrl Pts',(-19.6816966154287,38.714329749216,124.605463094587)) ;
#94479 = CARTESIAN_POINT('Ctrl Pts',(-19.2612630755405,38.7341265021359,124.627003828453)) ;
#94480 = CARTESIAN_POINT('Ctrl Pts',(-18.8551290904291,38.7540875906247,124.50387119971)) ;
#94481 = CARTESIAN_POINT('Ctrl Pts',(-18.5155747208721,38.7740658595569,124.248566076367)) ;
#94482 = CARTESIAN_POINT('Ctrl Pts',(-18.2848896984767,38.7938858743479,123.895929221417)) ;
#94483 = CARTESIAN_POINT('Ctrl Pts',(-18.1867323093592,38.8138242835997,123.483482278785)) ;
#94484 = CARTESIAN_POINT('Ctrl Pts',(-18.2364347422349,38.8338714009922,123.060080100057)) ;
#94485 = CARTESIAN_POINT('Ctrl Pts',(-18.4258542295812,38.853717646826,122.683047614378)) ;
#94486 = CARTESIAN_POINT('Ctrl Pts',(-18.731512097542,38.873566615338,122.391994315492)) ;
#94487 = CARTESIAN_POINT('Ctrl Pts',(-19.1222233612243,38.8936169176493,122.22152470631)) ;
#94488 = CARTESIAN_POINT('Ctrl Pts',(-19.543235364252,38.9134518400806,122.194986119466)) ;
#94489 = CARTESIAN_POINT('Ctrl Pts',(-19.9499551551053,38.9333822413064,122.313413194632)) ;
#94490 = CARTESIAN_POINT('Ctrl Pts',(-20.2916490712342,38.9532671866653,122.562710767896)) ;
#94491 = CARTESIAN_POINT('Ctrl Pts',(-20.5292736704849,38.9733397948167,122.917142233502)) ;
#94492 = CARTESIAN_POINT('Ctrl Pts',(-20.6303535211115,38.9931311111448,123.325705227082)) ;
#94493 = CARTESIAN_POINT('Ctrl Pts',(-20.58686894099,39.0130959009121,123.747941927736)) ;
#94494 = CARTESIAN_POINT('Ctrl Pts',(-20.4007639214894,39.0330788566624,124.129914872048)) ;
#94495 = CARTESIAN_POINT('Ctrl Pts',(-20.0987294817913,39.0528873786385,124.423515961885)) ;
#94496 = CARTESIAN_POINT('Ctrl Pts',(-19.7115170894291,39.0728729533743,124.598356596514)) ;
#94497 = CARTESIAN_POINT('Ctrl Pts',(-19.2898685978214,39.0927555934427,124.630327657411)) ;
#94498 = CARTESIAN_POINT('Ctrl Pts',(-18.881219954821,39.1127109055746,124.516450708816)) ;
#94499 = CARTESIAN_POINT('Ctrl Pts',(-18.5370774718083,39.1325852621824,124.271087878377)) ;
#94500 = CARTESIAN_POINT('Ctrl Pts',(-18.2958623645042,39.1525674690435,123.921382047478)) ;
#94501 = CARTESIAN_POINT('Ctrl Pts',(-18.188922682226,39.1724985469935,123.511215574697)) ;
#94502 = CARTESIAN_POINT('Ctrl Pts',(-18.2282858959202,39.1924255218484,123.089434355908)) ;
#94503 = CARTESIAN_POINT('Ctrl Pts',(-18.4076743420481,39.2122579807973,122.707733371159)) ;
#94504 = CARTESIAN_POINT('Ctrl Pts',(-18.6583859348494,39.2289156649725,122.457712360878)) ;
#94505 = CARTESIAN_POINT('Ctrl Pts',(-18.899856718345,39.2421648888796,122.318686734846)) ;
#94506 = CARTESIAN_POINT('Ctrl Pts',(-19.0984024083367,39.2522139103308,122.246593165114)) ;
#94507 = CARTESIAN_POINT('Ctrl Pts',(-19.3025722169409,39.2620739185613,122.21069862246)) ;
#94508 = CARTESIAN_POINT('Ctrl Pts',(-19.5818091443414,39.2753574317859,122.209905164307)) ;
#94509 = CARTESIAN_POINT('Ctrl Pts',(-19.923863738097,39.2920033507868,122.300944035455)) ;
#94510 = CARTESIAN_POINT('Ctrl Pts',(-20.212949843861,39.3085573286028,122.501708285792)) ;
#94511 = CARTESIAN_POINT('Ctrl Pts',(-20.3943693525762,39.3219170575744,122.716154726011)) ;
#94512 = CARTESIAN_POINT('Ctrl Pts',(-20.4992257353742,39.3318101093711,122.895780909833)) ;
#94513 = CARTESIAN_POINT('Ctrl Pts',(-20.5722643826613,39.3418000746522,123.092667970751)) ;
#94514 = CARTESIAN_POINT('Ctrl Pts',(-20.6099946182295,39.351751955513,123.298490502121)) ;
#94515 = CARTESIAN_POINT('Ctrl Pts',(-20.6112491588045,39.3618003072048,123.509712360783)) ;
#94516 = CARTESIAN_POINT('Ctrl Pts',(-20.5767745748545,39.371641591311,123.713735938484)) ;
#94517 = CARTESIAN_POINT('Ctrl Pts',(-20.5068084537327,39.3816282944367,123.91164782318)) ;
#94518 = CARTESIAN_POINT('Ctrl Pts',(-20.4041499408619,39.3915633232541,124.093590241754)) ;
#94519 = CARTESIAN_POINT('Ctrl Pts',(-20.2697572274367,39.401619118161,124.256736889901)) ;
#94520 = CARTESIAN_POINT('Ctrl Pts',(-20.1128745603871,39.4114474814503,124.391246892535)) ;
#94521 = CARTESIAN_POINT('Ctrl Pts',(-19.9310134092115,39.4215084513482,124.499192648327)) ;
#94522 = CARTESIAN_POINT('Ctrl Pts',(-19.7359479774225,39.431422730238,124.5726887504)) ;
#94523 = CARTESIAN_POINT('Ctrl Pts',(-19.5292236814562,39.4414317247063,124.61196971549)) ;
#94524 = CARTESIAN_POINT('Ctrl Pts',(-19.318381422526,39.45146155927,124.614334355691)) ;
#94525 = CARTESIAN_POINT('Ctrl Pts',(-19.1138104319035,39.4613197893422,124.581026332675)) ;
#94526 = CARTESIAN_POINT('Ctrl Pts',(-18.9153042039635,39.4713184950847,124.511985701486)) ;
#94527 = CARTESIAN_POINT('Ctrl Pts',(-18.7335269690382,39.4812131510035,124.410773863355)) ;
#94528 = CARTESIAN_POINT('Ctrl Pts',(-18.56943634765,39.4912762153874,124.27729901204)) ;
#94529 = CARTESIAN_POINT('Ctrl Pts',(-18.4338684117393,39.5011158736673,124.121008549129)) ;
#94530 = CARTESIAN_POINT('Ctrl Pts',(-18.3248828460409,39.5111790407491,123.9397151691)) ;
#94531 = CARTESIAN_POINT('Ctrl Pts',(-18.2504503765499,39.5210732858762,123.745455632953)) ;
#94532 = CARTESIAN_POINT('Ctrl Pts',(-18.2101397435108,39.5310151074809,123.540397852165)) ;
#94533 = CARTESIAN_POINT('Ctrl Pts',(-18.205942485578,39.5410176383989,123.330126951138)) ;
#94534 = CARTESIAN_POINT('Ctrl Pts',(-18.2387400810565,39.5510522648564,123.121743690453)) ;
#94535 = CARTESIAN_POINT('Ctrl Pts',(-18.3056247092528,39.5608977998429,122.925856505686)) ;
#94536 = CARTESIAN_POINT('Ctrl Pts',(-18.4064939010015,39.5708812246819,122.741821095179)) ;
#94537 = CARTESIAN_POINT('Ctrl Pts',(-18.5373982428774,39.580831615047,122.578645626432)) ;
#94538 = CARTESIAN_POINT('Ctrl Pts',(-18.6952153507087,39.590829255344,122.439801676693)) ;
#94539 = CARTESIAN_POINT('Ctrl Pts',(-18.8756822378047,39.6008683359072,122.330394244485)) ;
#94540 = CARTESIAN_POINT('Ctrl Pts',(-19.0680855983055,39.6106944866763,122.255165125294)) ;
#94541 = CARTESIAN_POINT('Ctrl Pts',(-19.2752888340513,39.6207510616055,122.21320663692)) ;
#94542 = CARTESIAN_POINT('Ctrl Pts',(-19.4842192743884,39.6306916009857,122.208288938117)) ;
#94543 = CARTESIAN_POINT('Ctrl Pts',(-19.6901728368781,39.6405959939621,122.23896416273)) ;
#94544 = CARTESIAN_POINT('Ctrl Pts',(-19.8904453983697,39.650642648167,122.306001788215)) ;
#94545 = CARTESIAN_POINT('Ctrl Pts',(-20.0733802115196,39.6605382101054,122.405136530258)) ;
#94546 = CARTESIAN_POINT('Ctrl Pts',(-20.239014832524,39.670600287951,122.536666603804)) ;
#94547 = CARTESIAN_POINT('Ctrl Pts',(-20.3763608522466,39.6804429863648,122.691467796565)) ;
#94548 = CARTESIAN_POINT('Ctrl Pts',(-20.4867687217227,39.6904337613262,122.870114185754)) ;
#94549 = CARTESIAN_POINT('Ctrl Pts',(-20.563976360036,39.7003616263453,123.06403607056)) ;
#94550 = CARTESIAN_POINT('Ctrl Pts',(-20.6069421620117,39.7103503711115,123.269592670156)) ;
#94551 = CARTESIAN_POINT('Ctrl Pts',(-20.6132830463092,39.7203831566985,123.480421504479)) ;
#94552 = CARTESIAN_POINT('Ctrl Pts',(-20.5836334775982,39.7302498413191,123.685712607016)) ;
#94553 = CARTESIAN_POINT('Ctrl Pts',(-20.518733142917,39.7402117334822,123.884836785975)) ;
#94554 = CARTESIAN_POINT('Ctrl Pts',(-20.4192475547195,39.7502452103948,124.070827748899)) ;
#94555 = CARTESIAN_POINT('Ctrl Pts',(-20.2911532789775,39.7601295516431,124.234483917297)) ;
#94556 = CARTESIAN_POINT('Ctrl Pts',(-20.1338366585851,39.7701924937642,124.375890200317)) ;
#94557 = CARTESIAN_POINT('Ctrl Pts',(-19.9581654376488,39.7800428953838,124.485576269177)) ;
#94558 = CARTESIAN_POINT('Ctrl Pts',(-19.7628967146071,39.7900697841735,124.564969156338)) ;
#94559 = CARTESIAN_POINT('Ctrl Pts',(-19.5566424600458,39.8000983991297,124.608721741187)) ;
#94560 = CARTESIAN_POINT('Ctrl Pts',(-19.34981381734,39.8099436222498,124.616255061362)) ;
#94561 = CARTESIAN_POINT('Ctrl Pts',(-19.1416957983259,39.8199343060557,124.587896768431)) ;
#94562 = CARTESIAN_POINT('Ctrl Pts',(-18.9408691509651,39.8299721881281,124.523084945167)) ;
#94563 = CARTESIAN_POINT('Ctrl Pts',(-18.7577650189888,39.839816547767,124.42660549306)) ;
#94564 = CARTESIAN_POINT('Ctrl Pts',(-18.5916351240008,39.8498014183817,124.298338388516)) ;
#94565 = CARTESIAN_POINT('Ctrl Pts',(-18.4508347820377,39.8597407017104,124.143903025515)) ;
#94566 = CARTESIAN_POINT('Ctrl Pts',(-18.337932004996,39.8697813110835,123.965575193897)) ;
#94567 = CARTESIAN_POINT('Ctrl Pts',(-18.2587923235217,39.8796661619968,123.773397832722)) ;
#94568 = CARTESIAN_POINT('Ctrl Pts',(-18.2134600339638,39.8896681181656,123.568102263173)) ;
#94569 = CARTESIAN_POINT('Ctrl Pts',(-18.2043675449943,39.899586714886,123.359747507517)) ;
#94570 = CARTESIAN_POINT('Ctrl Pts',(-18.2319750519706,39.9096335369618,123.150373488916)) ;
#94571 = CARTESIAN_POINT('Ctrl Pts',(-18.294259354094,39.9195078180745,122.952312235387)) ;
#94572 = CARTESIAN_POINT('Ctrl Pts',(-18.3915851916145,39.9295620181191,122.76472228793)) ;
#94573 = CARTESIAN_POINT('Ctrl Pts',(-18.5179539634958,39.9394574477544,122.599419731205)) ;
#94574 = CARTESIAN_POINT('Ctrl Pts',(-18.6735953495587,39.9495190760717,122.456211511714)) ;
#94575 = CARTESIAN_POINT('Ctrl Pts',(-18.847909017395,39.9593637049016,122.344621876972)) ;
#94576 = CARTESIAN_POINT('Ctrl Pts',(-19.040889665129,39.9693237525072,122.263369324957)) ;
#94577 = CARTESIAN_POINT('Ctrl Pts',(-19.2467363166001,39.9793620586813,122.216899420079)) ;
#94578 = CARTESIAN_POINT('Ctrl Pts',(-19.4540820779037,39.989235358114,122.206640501949)) ;
#94579 = CARTESIAN_POINT('Ctrl Pts',(-19.6641480891953,39.9993086197002,122.23312299692)) ;
#94580 = CARTESIAN_POINT('Ctrl Pts',(-19.8615092289753,40.0091288456569,122.29387007229)) ;
#94581 = CARTESIAN_POINT('Ctrl Pts',(-20.050164410473,40.0192079095964,122.390230244533)) ;
#94582 = CARTESIAN_POINT('Ctrl Pts',(-20.2155277469042,40.0290579996162,122.51497058454)) ;
#94583 = CARTESIAN_POINT('Ctrl Pts',(-20.3600033759325,40.03913675323,122.669891358918)) ;
#94584 = CARTESIAN_POINT('Ctrl Pts',(-20.4726264296346,40.0489582204895,122.84300447148)) ;
#94585 = CARTESIAN_POINT('Ctrl Pts',(-20.5557528197922,40.0590238188471,123.037552140448)) ;
#94586 = CARTESIAN_POINT('Ctrl Pts',(-20.6030259582916,40.0689264746218,123.240351541043)) ;
#94587 = CARTESIAN_POINT('Ctrl Pts',(-20.6145983084236,40.0789773004515,123.451291677188)) ;
#94588 = CARTESIAN_POINT('Ctrl Pts',(-20.5900018228788,40.0888515047903,123.657461638171)) ;
#94589 = CARTESIAN_POINT('Ctrl Pts',(-20.5288150346182,40.0989239548294,123.860137146693)) ;
#94590 = CARTESIAN_POINT('Ctrl Pts',(-20.435813281628,40.1087529716029,124.044705968251)) ;
#94591 = CARTESIAN_POINT('Ctrl Pts',(-20.3094637582039,40.1188198175177,124.214444012367)) ;
#94592 = CARTESIAN_POINT('Ctrl Pts',(-20.1581261550177,40.1287099888195,124.357060544978)) ;
#94593 = CARTESIAN_POINT('Ctrl Pts',(-19.982817511392,40.1387021824434,124.47277610636)) ;
#94594 = CARTESIAN_POINT('Ctrl Pts',(-19.7905608961819,40.1486649930668,124.555869120237)) ;
#94595 = CARTESIAN_POINT('Ctrl Pts',(-19.5880955015858,40.1585692659102,124.604552608596)) ;
#94596 = CARTESIAN_POINT('Ctrl Pts',(-19.3770061673514,40.1686297577149,124.617357351724)) ;
#94597 = CARTESIAN_POINT('Ctrl Pts',(-19.1714136948424,40.1784700893872,124.594104022115)) ;
#94598 = CARTESIAN_POINT('Ctrl Pts',(-18.9684724817499,40.1885331354789,124.534440358675)) ;
#94599 = CARTESIAN_POINT('Ctrl Pts',(-18.7821898037075,40.198427191174,124.441849153616)) ;
#94600 = CARTESIAN_POINT('Ctrl Pts',(-18.6136872008916,40.208369891497,124.318199456405)) ;
#94601 = CARTESIAN_POINT('Ctrl Pts',(-18.4682361054831,40.2183756324246,124.166208401796)) ;
#94602 = CARTESIAN_POINT('Ctrl Pts',(-18.3514207087649,40.2283965429401,123.990896073496)) ;
#94603 = CARTESIAN_POINT('Ctrl Pts',(-18.2676944149696,40.2382872783901,123.800556542411)) ;
#94604 = CARTESIAN_POINT('Ctrl Pts',(-18.2174871494906,40.2482788191189,123.596600054224)) ;
#94605 = CARTESIAN_POINT('Ctrl Pts',(-18.2035765205634,40.2582266795406,123.38792968964)) ;
#94606 = CARTESIAN_POINT('Ctrl Pts',(-18.2256975206144,40.2681733487269,123.179981160546)) ;
#94607 = CARTESIAN_POINT('Ctrl Pts',(-18.284396273702,40.2782214248625,122.977065964015)) ;
#94608 = CARTESIAN_POINT('Ctrl Pts',(-18.3754280331903,40.2880690228682,122.791125047696)) ;
#94609 = CARTESIAN_POINT('Ctrl Pts',(-18.4982372564915,40.2980307459526,122.621498409883)) ;
#94610 = CARTESIAN_POINT('Ctrl Pts',(-18.6498468908888,40.3080593810356,122.474969336951)) ;
#94611 = CARTESIAN_POINT('Ctrl Pts',(-18.8224769474675,40.3179696893537,122.358338779298)) ;
#94612 = CARTESIAN_POINT('Ctrl Pts',(-19.0129987885673,40.3279045864895,122.272737608116)) ;
#94613 = CARTESIAN_POINT('Ctrl Pts',(-19.2176901556967,40.3379456694321,122.221162637048)) ;
#94614 = CARTESIAN_POINT('Ctrl Pts',(-19.4250097860347,40.3478330122603,122.206002228677)) ;
#94615 = CARTESIAN_POINT('Ctrl Pts',(-19.6340061659135,40.3578245271997,122.226929966425)) ;
#94616 = CARTESIAN_POINT('Ctrl Pts',(-19.8353738299517,40.3677759183962,122.283688970992)) ;
#94617 = CARTESIAN_POINT('Ctrl Pts',(-20.0236219513541,40.3777084517288,122.37404934811)) ;
#94618 = CARTESIAN_POINT('Ctrl Pts',(-20.1944682236127,40.3877056096282,122.496443492551)) ;
#94619 = CARTESIAN_POINT('Ctrl Pts',(-20.3413742021362,40.3976906197917,122.64643432917)) ;
#94620 = CARTESIAN_POINT('Ctrl Pts',(-20.4604016269849,40.4077334463615,122.820781880567)) ;
#94621 = CARTESIAN_POINT('Ctrl Pts',(-20.5459653741827,40.4175636806665,123.008934961586)) ;
#94622 = CARTESIAN_POINT('Ctrl Pts',(-20.5989226586347,40.4276397059012,123.213993634072)) ;
#94623 = CARTESIAN_POINT('Ctrl Pts',(-20.6152177268763,40.437491942392,123.420521244242)) ;
#94624 = CARTESIAN_POINT('Ctrl Pts',(-20.595146375222,40.4475651488262,123.631304239716)) ;
#94625 = CARTESIAN_POINT('Ctrl Pts',(-20.540009566013,40.4574066583333,123.830735651141)) ;
#94626 = CARTESIAN_POINT('Ctrl Pts',(-20.4507245575497,40.4673676051131,124.020150554085)) ;
#94627 = CARTESIAN_POINT('Ctrl Pts',(-20.328629514598,40.4774054339132,124.192262261926)) ;
#94628 = CARTESIAN_POINT('Ctrl Pts',(-20.1811994533202,40.4872797436676,124.338439938895)) ;
#94629 = CARTESIAN_POINT('Ctrl Pts',(-20.0072892895941,40.4973494413408,124.459100732173)) ;
#94630 = CARTESIAN_POINT('Ctrl Pts',(-19.8195861713567,40.5071829126282,124.545769387066)) ;
#94631 = CARTESIAN_POINT('Ctrl Pts',(-19.6158723309425,40.5172125591581,124.600164943048)) ;
#94632 = CARTESIAN_POINT('Ctrl Pts',(-19.4056431711912,40.5272470734855,124.617731141067)) ;
#94633 = CARTESIAN_POINT('Ctrl Pts',(-19.1998966723173,40.5370723589564,124.599424024852)) ;
#94634 = CARTESIAN_POINT('Ctrl Pts',(-18.9967300833823,40.5470766005049,124.545129025177)) ;
#94635 = CARTESIAN_POINT('Ctrl Pts',(-18.8064674259358,40.557059245584,124.456466509944)) ;
#94636 = CARTESIAN_POINT('Ctrl Pts',(-18.6336011039915,40.5671044426755,124.335200583634)) ;
#94637 = CARTESIAN_POINT('Ctrl Pts',(-18.4874473744563,40.5769275584357,124.18929088824)) ;
#94638 = CARTESIAN_POINT('Ctrl Pts',(-18.3658653991529,40.5869621702359,124.016894776006)) ;
#94639 = CARTESIAN_POINT('Ctrl Pts',(-18.276679009699,40.5969871790091,123.825931021267)) ;
#94640 = CARTESIAN_POINT('Ctrl Pts',(-18.2225124725489,40.6068391038507,123.626017281028)) ;
#94641 = CARTESIAN_POINT('Ctrl Pts',(-18.2032990756932,40.6168300421734,123.416882426706)) ;
#94642 = CARTESIAN_POINT('Ctrl Pts',(-18.2204327216342,40.6267480273198,123.209055359799)) ;
#94643 = CARTESIAN_POINT('Ctrl Pts',(-18.2739197540757,40.6367761282153,123.005147720835)) ;
#94644 = CARTESIAN_POINT('Ctrl Pts',(-18.3606743245139,40.6466613691579,122.816298477163)) ;
#94645 = CARTESIAN_POINT('Ctrl Pts',(-18.4797205501909,40.6566504821245,122.643290611343)) ;
#94646 = CARTESIAN_POINT('Ctrl Pts',(-18.6281007030375,40.6666925464653,122.493120519007)) ;
#94647 = CARTESIAN_POINT('Ctrl Pts',(-18.7964346089522,40.6765217478698,122.373256814763)) ;
#94648 = CARTESIAN_POINT('Ctrl Pts',(-18.9861689428524,40.686528588628,122.282435666904)) ;
#94649 = CARTESIAN_POINT('Ctrl Pts',(-19.1884902469332,40.6965161128199,122.226152191325)) ;
#94650 = CARTESIAN_POINT('Ctrl Pts',(-19.3983530777978,40.7065457586286,122.205918577361)) ;
#94651 = CARTESIAN_POINT('Ctrl Pts',(-19.6053392656737,40.7164197893673,122.221929297566)) ;
#94652 = CARTESIAN_POINT('Ctrl Pts',(-19.8089638125381,40.7264191122314,122.274027018103)) ;
#94653 = CARTESIAN_POINT('Ctrl Pts',(-19.9989028221292,40.736329947807,122.359763953984)) ;
#94654 = CARTESIAN_POINT('Ctrl Pts',(-20.1734602714543,40.746384195781,122.478901030537)) ;
#94655 = CARTESIAN_POINT('Ctrl Pts',(-20.3219594084371,40.7562429400437,122.62353974604)) ;
#94656 = CARTESIAN_POINT('Ctrl Pts',(-20.4457241120794,40.7663110261167,122.795209533681)) ;
#94657 = CARTESIAN_POINT('Ctrl Pts',(-20.5358630666679,40.7761665092963,122.981787019375)) ;
#94658 = CARTESIAN_POINT('Ctrl Pts',(-20.593633206338,40.7861613550904,123.183805530835)) ;
#94659 = CARTESIAN_POINT('Ctrl Pts',(-20.6150774328527,40.796192650753,123.393606073718)) ;
#94660 = CARTESIAN_POINT('Ctrl Pts',(-20.6003488764673,40.8060591940429,123.600515261754)) ;
#94661 = CARTESIAN_POINT('Ctrl Pts',(-20.549636410078,40.8160465898062,123.804239901806)) ;
#94662 = CARTESIAN_POINT('Ctrl Pts',(-20.4647624174403,40.8259916305362,123.995347584397)) ;
#94663 = CARTESIAN_POINT('Ctrl Pts',(-20.3467582642971,40.8360361367529,124.170441043399)) ;
#94664 = CARTESIAN_POINT('Ctrl Pts',(-20.202893284739,40.8458996428903,124.319807451803)) ;
#94665 = CARTESIAN_POINT('Ctrl Pts',(-20.0333415385415,40.8558925037263,124.443797452948)) ;
#94666 = CARTESIAN_POINT('Ctrl Pts',(-19.8460832863042,40.8658186974453,124.535960572849)) ;
#94667 = CARTESIAN_POINT('Ctrl Pts',(-19.6438582328255,40.8758376234778,124.594776915068)) ;
#94668 = CARTESIAN_POINT('Ctrl Pts',(-19.436629966288,40.8857526228454,124.617551938887)) ;
#94669 = CARTESIAN_POINT('Ctrl Pts',(-19.2257233942955,40.8958073944027,124.603768109833)) ;
#94670 = CARTESIAN_POINT('Ctrl Pts',(-19.0243302771047,40.9056663567003,124.554668324937)) ;
#94671 = CARTESIAN_POINT('Ctrl Pts',(-18.8318134848253,40.9156606005381,124.470587726134)) ;
#94672 = CARTESIAN_POINT('Ctrl Pts',(-18.6579190371957,40.9255858299624,124.355204812774)) ;
#94673 = CARTESIAN_POINT('Ctrl Pts',(-18.5051729778743,40.9356137938538,124.209940570375)) ;
#94674 = CARTESIAN_POINT('Ctrl Pts',(-18.3815316830435,40.9455000534842,124.042837464841)) ;
#94675 = CARTESIAN_POINT('Ctrl Pts',(-18.2873498073833,40.9555318165621,123.85417507662)) ;
#94676 = CARTESIAN_POINT('Ctrl Pts',(-18.2280402867286,40.9654134428562,123.655039667147)) ;
#94677 = CARTESIAN_POINT('Ctrl Pts',(-18.2037261411978,40.9754752123424,123.444942837729)) ;
#94678 = CARTESIAN_POINT('Ctrl Pts',(-18.2159492443396,40.9853330798378,123.23803488184)) ;
#94679 = CARTESIAN_POINT('Ctrl Pts',(-18.2640991622364,40.9953247049552,123.033597970175)) ;
#94680 = CARTESIAN_POINT('Ctrl Pts',(-18.3466098904373,41.0052615040634,122.841666372435)) ;
#94681 = CARTESIAN_POINT('Ctrl Pts',(-18.4615560564106,41.0152523336208,122.665869282577)) ;
#94682 = CARTESIAN_POINT('Ctrl Pts',(-18.605927064442,41.025275569334,122.51236953615)) ;
#94683 = CARTESIAN_POINT('Ctrl Pts',(-18.7725080768488,41.0351719173631,122.387730228148)) ;
#94684 = CARTESIAN_POINT('Ctrl Pts',(-18.9597603021565,41.0451614798656,122.292617751821)) ;
#94685 = CARTESIAN_POINT('Ctrl Pts',(-19.1618068850491,41.0552017875502,122.231566043326)) ;
#94686 = CARTESIAN_POINT('Ctrl Pts',(-19.3672327471221,41.0650440908974,122.206620708451)) ;
#94687 = CARTESIAN_POINT('Ctrl Pts',(-19.5776399590884,41.0750677991764,122.217643519475)) ;
#94688 = CARTESIAN_POINT('Ctrl Pts',(-19.8485691529838,41.0882899766441,122.280066801218)) ;
#94689 = CARTESIAN_POINT('Ctrl Pts',(-20.0983814297562,41.1015825617034,122.412162007784)) ;
#94690 = CARTESIAN_POINT('Ctrl Pts',(-20.303073380294,41.114867417625,122.602192166436)) ;
#94691 = CARTESIAN_POINT('Ctrl Pts',(-20.4297314944804,41.1248396447978,122.769227524099)) ;
#94692 = CARTESIAN_POINT('Ctrl Pts',(-20.5251912714743,41.1347482612368,122.954404492746)) ;
#94693 = CARTESIAN_POINT('Ctrl Pts',(-20.5878572761394,41.1448014666205,123.156230134344)) ;
#94694 = CARTESIAN_POINT('Ctrl Pts',(-20.6141674244472,41.1546666003808,123.361965570932)) ;
#94695 = CARTESIAN_POINT('Ctrl Pts',(-20.6014118404237,41.1680056580072,123.642110925614)) ;
#94696 = CARTESIAN_POINT('Ctrl Pts',(-20.4948859078202,41.1845748453403,123.977938811576)) ;
#94697 = CARTESIAN_POINT('Ctrl Pts',(-20.2793745793678,41.2012199851913,124.258685783762)) ;
#94698 = CARTESIAN_POINT('Ctrl Pts',(-20.0579576413168,41.2144922876647,124.428476543224)) ;
#94699 = CARTESIAN_POINT('Ctrl Pts',(-19.8719402483463,41.2244732511124,124.5255422906)) ;
#94700 = CARTESIAN_POINT('Ctrl Pts',(-19.6726895718307,41.2344150831817,124.588712912963)) ;
#94701 = CARTESIAN_POINT('Ctrl Pts',(-19.3951595665634,41.2477346523971,124.625810172033)) ;
#94702 = CARTESIAN_POINT('Ctrl Pts',(-19.0464438591427,41.2642648073298,124.581269942614)) ;
#94703 = CARTESIAN_POINT('Ctrl Pts',(-18.6680925736183,41.2842865328219,124.38634423409)) ;
#94704 = CARTESIAN_POINT('Ctrl Pts',(-18.3816919054068,41.3040979294287,124.077301406411)) ;
#94705 = CARTESIAN_POINT('Ctrl Pts',(-18.2159313914178,41.3240831781376,123.686131229408)) ;
#94706 = CARTESIAN_POINT('Ctrl Pts',(-18.1939891820258,41.3439772407735,123.263630954678)) ;
#94707 = CARTESIAN_POINT('Ctrl Pts',(-18.3171494252576,41.3639089199471,122.858127898099)) ;
#94708 = CARTESIAN_POINT('Ctrl Pts',(-18.5719341117351,41.3838729744191,122.518602617013)) ;
#94709 = CARTESIAN_POINT('Ctrl Pts',(-18.925647690963,41.403753876182,122.287092819284)) ;
#94710 = CARTESIAN_POINT('Ctrl Pts',(-19.3381949379129,41.4236925377904,122.189526544458)) ;
#94711 = CARTESIAN_POINT('Ctrl Pts',(-19.7584054124552,41.4435890630457,122.238430586688)) ;
#94712 = CARTESIAN_POINT('Ctrl Pts',(-20.1370058269527,41.4634841015001,122.427169281719)) ;
#94713 = CARTESIAN_POINT('Ctrl Pts',(-20.4294053679111,41.4834479248061,122.734843310228)) ;
#94714 = CARTESIAN_POINT('Ctrl Pts',(-20.5988096691988,41.5033220489352,123.122013486235)) ;
#94715 = CARTESIAN_POINT('Ctrl Pts',(-20.6264542810702,41.5232971246625,123.545855807307)) ;
#94716 = CARTESIAN_POINT('Ctrl Pts',(-20.5073565762459,41.5432506940191,123.953056711382)) ;
#94717 = CARTESIAN_POINT('Ctrl Pts',(-20.2585449822176,41.5630886042069,124.293669103182)) ;
#94718 = CARTESIAN_POINT('Ctrl Pts',(-19.9062555480821,41.5830644327778,124.530937490507)) ;
#94719 = CARTESIAN_POINT('Ctrl Pts',(-19.4952527745966,41.6029824774881,124.632990018156)) ;
#94720 = CARTESIAN_POINT('Ctrl Pts',(-19.074880553393,41.6228527232758,124.589826696202)) ;
#94721 = CARTESIAN_POINT('Ctrl Pts',(-18.6915024510565,41.6429017263753,124.403663945132)) ;
#94722 = CARTESIAN_POINT('Ctrl Pts',(-18.3981608225191,41.6626809676162,124.102123352267)) ;
#94723 = CARTESIAN_POINT('Ctrl Pts',(-18.2226406505377,41.682711031325,123.714185617551)) ;
#94724 = CARTESIAN_POINT('Ctrl Pts',(-18.1909502367662,41.702593316227,123.292557485542)) ;
#94725 = CARTESIAN_POINT('Ctrl Pts',(-18.3038834095939,41.72247561712,122.885208119923)) ;
#94726 = CARTESIAN_POINT('Ctrl Pts',(-18.5504266881587,41.7424587267384,122.539145738283)) ;
#94727 = CARTESIAN_POINT('Ctrl Pts',(-18.8986863380999,41.7623491221162,122.299138995889)) ;
#94728 = CARTESIAN_POINT('Ctrl Pts',(-19.307832379014,41.7822459121505,122.191754243473)) ;
#94729 = CARTESIAN_POINT('Ctrl Pts',(-19.7296142472698,41.8021629660921,122.23001985925)) ;
#94730 = CARTESIAN_POINT('Ctrl Pts',(-20.1146546672758,41.8221665142956,122.41084364833)) ;
#94731 = CARTESIAN_POINT('Ctrl Pts',(-20.4133983983086,41.8421048079482,122.711612600344)) ;
#94732 = CARTESIAN_POINT('Ctrl Pts',(-20.5914741795715,41.8619262953812,123.093609322435)) ;
#94733 = CARTESIAN_POINT('Ctrl Pts',(-20.6292246792124,41.881904688372,123.516673333477)) ;
#94734 = CARTESIAN_POINT('Ctrl Pts',(-20.5204944182451,41.9018030699857,123.925630858836)) ;
#94735 = CARTESIAN_POINT('Ctrl Pts',(-20.3195273566345,41.9183860007156,124.215224343354)) ;
#94736 = CARTESIAN_POINT('Ctrl Pts',(-20.1066686455886,41.9316602363045,124.395804425527)) ;
#94737 = CARTESIAN_POINT('Ctrl Pts',(-19.9243029169326,41.9417066537607,124.502286315057)) ;
#94738 = CARTESIAN_POINT('Ctrl Pts',(-19.7302093112894,41.9515518789799,124.574250358946)) ;
#94739 = CARTESIAN_POINT('Ctrl Pts',(-19.4546062106336,41.9648868500193,124.625183233532)) ;
#94740 = CARTESIAN_POINT('Ctrl Pts',(-19.1029743251083,41.981469706812,124.597295458286)) ;
#94741 = CARTESIAN_POINT('Ctrl Pts',(-18.7810078469193,41.9981127091614,124.450748808051)) ;
#94742 = CARTESIAN_POINT('Ctrl Pts',(-18.5658476086863,42.011356440193,124.273892910701)) ;
#94743 = CARTESIAN_POINT('Ctrl Pts',(-18.428377019164,42.0214108348676,124.113388604921)) ;
#94744 = CARTESIAN_POINT('Ctrl Pts',(-18.3228682434027,42.0312518962562,123.935378215502)) ;
#94745 = CARTESIAN_POINT('Ctrl Pts',(-18.2480350752191,42.0413181206127,123.737465714565)) ;
#94746 = CARTESIAN_POINT('Ctrl Pts',(-18.2094758284378,42.0511987335323,123.533319948566)) ;
#94747 = CARTESIAN_POINT('Ctrl Pts',(-18.2065221821883,42.061192026692,123.323284104449)) ;
#94748 = CARTESIAN_POINT('Ctrl Pts',(-18.2398729840911,42.0711430349156,123.116720737839)) ;
#94749 = CARTESIAN_POINT('Ctrl Pts',(-18.30938960882,42.0811915492776,122.917259856404)) ;
#94750 = CARTESIAN_POINT('Ctrl Pts',(-18.4101750659709,42.0910330553402,122.736544979461)) ;
#94751 = CARTESIAN_POINT('Ctrl Pts',(-18.5423307667801,42.1010187079699,122.573475447401)) ;
#94752 = CARTESIAN_POINT('Ctrl Pts',(-18.7000496850121,42.1109577168148,122.436369784685)) ;
#94753 = CARTESIAN_POINT('Ctrl Pts',(-18.8809998458564,42.1209986421078,122.327702241158)) ;
#94754 = CARTESIAN_POINT('Ctrl Pts',(-19.0751046604833,42.1308889638627,122.253109674576)) ;
#94755 = CARTESIAN_POINT('Ctrl Pts',(-19.2812986190992,42.1408849371962,122.212630847308)) ;
#94756 = CARTESIAN_POINT('Ctrl Pts',(-19.4900576064491,42.1508163367782,122.208578595215)) ;
#94757 = CARTESIAN_POINT('Ctrl Pts',(-19.6979366331324,42.1608218772553,122.240781161984)) ;
#94758 = CARTESIAN_POINT('Ctrl Pts',(-19.8974710441243,42.1708548611866,122.309135104057)) ;
#94759 = CARTESIAN_POINT('Ctrl Pts',(-20.0790398796497,42.1807104920134,122.408984409925)) ;
#94760 = CARTESIAN_POINT('Ctrl Pts',(-20.2429987707596,42.1907098942066,122.540492356409)) ;
#94761 = CARTESIAN_POINT('Ctrl Pts',(-20.3804073459891,42.2006043635676,122.696711276599)) ;
#94762 = CARTESIAN_POINT('Ctrl Pts',(-20.4903548587185,42.2106674777319,122.877413039077)) ;
#94763 = CARTESIAN_POINT('Ctrl Pts',(-20.5657866675536,42.2205071234482,123.070066487545)) ;
#94764 = CARTESIAN_POINT('Ctrl Pts',(-20.6078006806299,42.230570291004,123.27738258839)) ;
#94765 = CARTESIAN_POINT('Ctrl Pts',(-20.6129143393689,42.2404645467989,123.485351033977)) ;
#94766 = CARTESIAN_POINT('Ctrl Pts',(-20.5822609059887,42.2504063252585,123.692072376071)) ;
#94767 = CARTESIAN_POINT('Ctrl Pts',(-20.5158291243726,42.2604090180887,123.891620705968)) ;
#94768 = CARTESIAN_POINT('Ctrl Pts',(-20.41518049129,42.2704430400425,124.076996133679)) ;
#94769 = CARTESIAN_POINT('Ctrl Pts',(-20.2865490886093,42.2802908311316,124.239226624219)) ;
#94770 = CARTESIAN_POINT('Ctrl Pts',(-20.1299261416797,42.2902723556806,124.378854116596)) ;
#94771 = CARTESIAN_POINT('Ctrl Pts',(-19.9519781208104,42.3002215791715,124.488795049372)) ;
#94772 = CARTESIAN_POINT('Ctrl Pts',(-19.7567858429726,42.3102192353881,124.566794957214)) ;
#94773 = CARTESIAN_POINT('Ctrl Pts',(-19.5500874564602,42.3202594484432,124.609497549694)) ;
#94774 = CARTESIAN_POINT('Ctrl Pts',(-19.3435610736037,42.3300874957194,124.615984150951)) ;
#94775 = CARTESIAN_POINT('Ctrl Pts',(-19.1343128394333,42.3401418427518,124.586163345048)) ;
#94776 = CARTESIAN_POINT('Ctrl Pts',(-18.9357761772501,42.3500829790803,124.520862041799)) ;
#94777 = CARTESIAN_POINT('Ctrl Pts',(-18.7519747205506,42.3599872121601,124.423017051762)) ;
#94778 = CARTESIAN_POINT('Ctrl Pts',(-18.5856939199172,42.3700339090037,124.292809021581)) ;
#94779 = CARTESIAN_POINT('Ctrl Pts',(-18.4464957962176,42.3799294602839,124.138158892235)) ;
#94780 = CARTESIAN_POINT('Ctrl Pts',(-18.334443279754,42.3899915381234,123.958773214365)) ;
#94781 = CARTESIAN_POINT('Ctrl Pts',(-18.256837301689,42.3998342472195,123.766927669182)) ;
#94782 = CARTESIAN_POINT('Ctrl Pts',(-18.2125966969504,42.4098249794579,123.561630551405)) ;
#94783 = CARTESIAN_POINT('Ctrl Pts',(-18.2047563018434,42.4197530046867,123.353048502693)) ;
#94784 = CARTESIAN_POINT('Ctrl Pts',(-18.2330695475224,42.4297411513373,123.14497892533)) ;
#94785 = CARTESIAN_POINT('Ctrl Pts',(-18.2976873818308,42.4397761691772,122.94414783446)) ;
#94786 = CARTESIAN_POINT('Ctrl Pts',(-18.3943257711655,42.4496409662824,122.760659909047)) ;
#94787 = CARTESIAN_POINT('Ctrl Pts',(-18.5221133525322,42.4596016986385,122.59475870461)) ;
#94788 = CARTESIAN_POINT('Ctrl Pts',(-18.6781228036103,42.4696351610355,122.452804645446)) ;
#94789 = CARTESIAN_POINT('Ctrl Pts',(-18.8536233329689,42.4795206952469,122.341445380712)) ;
#94790 = CARTESIAN_POINT('Ctrl Pts',(-19.0492358131818,42.4895855359269,122.260840291009)) ;
#94791 = CARTESIAN_POINT('Ctrl Pts',(-19.2514442452252,42.4994336676558,122.21630249578)) ;
#94792 = CARTESIAN_POINT('Ctrl Pts',(-19.462035792714,42.5094611646459,122.206847322069)) ;
#94793 = CARTESIAN_POINT('Ctrl Pts',(-19.6710341455677,42.519489616691,122.234659844104)) ;
#94794 = CARTESIAN_POINT('Ctrl Pts',(-19.8684540475682,42.5293348832551,122.296792877154)) ;
#94795 = CARTESIAN_POINT('Ctrl Pts',(-20.0550737957879,42.539325556196,122.39317911818)) ;
#94796 = CARTESIAN_POINT('Ctrl Pts',(-20.2226209287262,42.5493634382845,122.521475154618)) ;
#94797 = CARTESIAN_POINT('Ctrl Pts',(-20.3628676182926,42.5592078087242,122.673680073247)) ;
#94798 = CARTESIAN_POINT('Ctrl Pts',(-20.4764790775102,42.5691926361195,122.850155943323)) ;
#94799 = CARTESIAN_POINT('Ctrl Pts',(-20.5574622812338,42.5791320815248,123.042816214806)) ;
#94800 = CARTESIAN_POINT('Ctrl Pts',(-20.6041616161675,42.5891720858107,123.248636405187)) ;
#94801 = CARTESIAN_POINT('Ctrl Pts',(-20.6144023767689,42.5990591949964,123.456265586749)) ;
#94802 = CARTESIAN_POINT('Ctrl Pts',(-20.5884050739317,42.6090592548988,123.664852226601)) ;
#94803 = CARTESIAN_POINT('Ctrl Pts',(-20.527246558674,42.6189766708135,123.86421184067)) ;
#94804 = CARTESIAN_POINT('Ctrl Pts',(-20.4311397333606,42.6290234855543,124.0522625542)) ;
#94805 = CARTESIAN_POINT('Ctrl Pts',(-20.3061446920854,42.638898962751,124.218074754755)) ;
#94806 = CARTESIAN_POINT('Ctrl Pts',(-20.1516108964613,42.6489550584722,124.362292436574)) ;
#94807 = CARTESIAN_POINT('Ctrl Pts',(-19.9772349604992,42.6588482204873,124.475727074264)) ;
#94808 = CARTESIAN_POINT('Ctrl Pts',(-19.7826262393279,42.6689104565099,124.558584685798)) ;
#94809 = CARTESIAN_POINT('Ctrl Pts',(-19.5810180452714,42.6787549221389,124.605386432261)) ;
#94810 = CARTESIAN_POINT('Ctrl Pts',(-19.3719712941627,42.688715014843,124.617355628047)) ;
#94811 = CARTESIAN_POINT('Ctrl Pts',(-19.1624444705205,42.698753303824,124.592241358661)) ;
#94812 = CARTESIAN_POINT('Ctrl Pts',(-18.963625683238,42.7086266269302,124.532502862756)) ;
#94813 = CARTESIAN_POINT('Ctrl Pts',(-18.7745424256361,42.7186998110153,124.437233845792)) ;
#94814 = CARTESIAN_POINT('Ctrl Pts',(-18.6088995425854,42.7285203233033,124.313922067836)) ;
#94815 = CARTESIAN_POINT('Ctrl Pts',(-18.4633850738748,42.7385983194191,124.159993840772)) ;
#94816 = CARTESIAN_POINT('Ctrl Pts',(-18.3493042720735,42.7484523944023,123.987014281055)) ;
#94817 = CARTESIAN_POINT('Ctrl Pts',(-18.2650619448584,42.758516275986,123.792978353709)) ;
#94818 = CARTESIAN_POINT('Ctrl Pts',(-18.2166935674385,42.7683997019598,123.590869324844)) ;
#94819 = CARTESIAN_POINT('Ctrl Pts',(-18.2036737593463,42.7784003058808,123.381065517752)) ;
#94820 = CARTESIAN_POINT('Ctrl Pts',(-18.2269667434619,42.7883200902187,123.173787221887)) ;
#94821 = CARTESIAN_POINT('Ctrl Pts',(-18.2866812459217,42.7983674405756,122.971212989523)) ;
#94822 = CARTESIAN_POINT('Ctrl Pts',(-18.3788851943168,42.8082447828098,122.785107699103)) ;
#94823 = CARTESIAN_POINT('Ctrl Pts',(-18.5043642018314,42.8183146638845,122.614654132429)) ;
#94824 = CARTESIAN_POINT('Ctrl Pts',(-18.653787444883,42.8281443690862,122.4718499437)) ;
#94825 = CARTESIAN_POINT('Ctrl Pts',(-18.8296635825875,42.8382110302526,122.354200237369)) ;
#94826 = CARTESIAN_POINT('Ctrl Pts',(-19.0200097310949,42.8481012521199,122.270467356892)) ;
#94827 = CARTESIAN_POINT('Ctrl Pts',(-19.2239389577315,42.85809342823,122.220108591587)) ;
#94828 = CARTESIAN_POINT('Ctrl Pts',(-19.4329190104502,42.8680562583427,122.206163568861)) ;
#94829 = CARTESIAN_POINT('Ctrl Pts',(-19.6400001889169,42.877960470743,122.228059000419)) ;
#94830 = CARTESIAN_POINT('Ctrl Pts',(-19.8432008513187,42.8880211848308,122.286655338728)) ;
#94831 = CARTESIAN_POINT('Ctrl Pts',(-20.0291415866043,42.8978606878136,122.37737031045)) ;
#94832 = CARTESIAN_POINT('Ctrl Pts',(-20.2004350174569,42.90792682638,122.501580182519)) ;
#94833 = CARTESIAN_POINT('Ctrl Pts',(-20.3448645195168,42.9178093408661,122.650971714434)) ;
#94834 = CARTESIAN_POINT('Ctrl Pts',(-20.4627595278798,42.9278016402216,122.824800696927)) ;
#94835 = CARTESIAN_POINT('Ctrl Pts',(-20.5484179633364,42.937754707175,123.015743351538)) ;
#94836 = CARTESIAN_POINT('Ctrl Pts',(-20.5999443450742,42.9477894153802,123.220298951895)) ;
#94837 = CARTESIAN_POINT('Ctrl Pts',(-20.615102005062,42.9576776362844,123.427639323025)) ;
#94838 = CARTESIAN_POINT('Ctrl Pts',(-20.5941477423262,42.9676720593148,123.636694524985)) ;
#94839 = CARTESIAN_POINT('Ctrl Pts',(-20.5374094938443,42.977617398761,123.837931542936)) ;
#94840 = CARTESIAN_POINT('Ctrl Pts',(-20.4469569944454,42.9875647433723,124.026493617296)) ;
#94841 = CARTESIAN_POINT('Ctrl Pts',(-20.3237223456528,42.9976126387833,124.19805123647)) ;
#94842 = CARTESIAN_POINT('Ctrl Pts',(-20.1757015216844,43.0074602842627,124.342795648031)) ;
#94843 = CARTESIAN_POINT('Ctrl Pts',(-20.0031972602108,43.0174219981767,124.461528619492)) ;
#94844 = CARTESIAN_POINT('Ctrl Pts',(-19.8112857189198,43.0274506224676,124.548856647514)) ;
#94845 = CARTESIAN_POINT('Ctrl Pts',(-19.6095733787523,43.0373609831244,124.600973577748)) ;
#94846 = CARTESIAN_POINT('Ctrl Pts',(-19.4013914837202,43.0472956816976,124.617866016103)) ;
#94847 = CARTESIAN_POINT('Ctrl Pts',(-19.1912337061601,43.0573375065518,124.597937775619)) ;
#94848 = CARTESIAN_POINT('Ctrl Pts',(-18.9908384089771,43.0672220802963,124.542869343014)) ;
#94849 = CARTESIAN_POINT('Ctrl Pts',(-18.8007562850313,43.0772239296594,124.453033636457)) ;
#94850 = CARTESIAN_POINT('Ctrl Pts',(-18.6304420312896,43.0871432312335,124.332653761318)) ;
#94851 = CARTESIAN_POINT('Ctrl Pts',(-18.4817976082182,43.0971873395787,124.182701681001)) ;
#94852 = CARTESIAN_POINT('Ctrl Pts',(-18.3632946191163,43.107071763021,124.01199028503)) ;
#94853 = CARTESIAN_POINT('Ctrl Pts',(-18.2746464092805,43.1170881249304,123.820975075702)) ;
#94854 = CARTESIAN_POINT('Ctrl Pts',(-18.2209433761901,43.1271247804358,123.616933265616)) ;
#94855 = CARTESIAN_POINT('Ctrl Pts',(-18.2032793807501,43.1369549106252,123.411004657846)) ;
#94856 = CARTESIAN_POINT('Ctrl Pts',(-18.2220212330491,43.147030963715,123.200045552597)) ;
#94857 = CARTESIAN_POINT('Ctrl Pts',(-18.2757963269349,43.1568831929008,122.99997816041)) ;
#94858 = CARTESIAN_POINT('Ctrl Pts',(-18.3652659275181,43.1669564007001,122.808072809261)) ;
#94859 = CARTESIAN_POINT('Ctrl Pts',(-18.4839780874204,43.1767979120515,122.638602038038)) ;
#94860 = CARTESIAN_POINT('Ctrl Pts',(-18.6315156023104,43.1867588500891,122.49000028128)) ;
#94861 = CARTESIAN_POINT('Ctrl Pts',(-18.8041793061524,43.196796712014,122.36868648056)) ;
#94862 = CARTESIAN_POINT('Ctrl Pts',(-18.9920325642784,43.2066708980111,122.28028983119)) ;
#94863 = CARTESIAN_POINT('Ctrl Pts',(-19.1963083903937,43.216741057589,122.224806544877)) ;
#94864 = CARTESIAN_POINT('Ctrl Pts',(-19.4021609754784,43.2265728050148,122.205953810551)) ;
#94865 = CARTESIAN_POINT('Ctrl Pts',(-19.6124556219852,43.2366088850861,122.222937571931)) ;
#94866 = CARTESIAN_POINT('Ctrl Pts',(-19.8161059672516,43.2466259319386,122.276596411569)) ;
#94867 = CARTESIAN_POINT('Ctrl Pts',(-20.0049292539503,43.2565081901052,122.363254712889)) ;
#94868 = CARTESIAN_POINT('Ctrl Pts',(-20.1777775594488,43.2664958729016,122.482430141182)) ;
#94869 = CARTESIAN_POINT('Ctrl Pts',(-20.3268505573778,43.2764425296183,122.629119299835)) ;
#94870 = CARTESIAN_POINT('Ctrl Pts',(-20.4493262829934,43.2864995876985,122.801435822179)) ;
#94871 = CARTESIAN_POINT('Ctrl Pts',(-20.5381405109259,43.2963177672479,122.987771862628)) ;
#94872 = CARTESIAN_POINT('Ctrl Pts',(-20.5950205275203,43.3063537016869,123.190941543004)) ;
#94873 = CARTESIAN_POINT('Ctrl Pts',(-20.6151355410267,43.3163783561159,123.400737110765)) ;
#94874 = CARTESIAN_POINT('Ctrl Pts',(-20.5992612078394,43.3262303756954,123.607251294915)) ;
#94875 = CARTESIAN_POINT('Ctrl Pts',(-20.5473617854122,43.3362212894104,123.810752806261)) ;
#94876 = CARTESIAN_POINT('Ctrl Pts',(-20.4616503408457,43.3461392782499,124.000855965883)) ;
#94877 = CARTESIAN_POINT('Ctrl Pts',(-20.3429941407184,43.3561673889807,124.17509705493)) ;
#94878 = CARTESIAN_POINT('Ctrl Pts',(-20.1980312069958,43.3660525868891,124.324012622826)) ;
#94879 = CARTESIAN_POINT('Ctrl Pts',(-20.0279376979557,43.3760418621571,124.447192060781)) ;
#94880 = CARTESIAN_POINT('Ctrl Pts',(-19.8378630919995,43.3860833203266,124.539030412426)) ;
#94881 = CARTESIAN_POINT('Ctrl Pts',(-19.6390701343716,43.395914784115,124.595638016482)) ;
#94882 = CARTESIAN_POINT('Ctrl Pts',(-19.4299207018962,43.4059197164188,124.617705082687)) ;
#94883 = CARTESIAN_POINT('Ctrl Pts',(-19.2204529483863,43.4159060803136,124.603030015181)) ;
#94884 = CARTESIAN_POINT('Ctrl Pts',(-19.0159260281216,43.4259357091994,124.551840172303)) ;
#94885 = CARTESIAN_POINT('Ctrl Pts',(-18.8262138021633,43.4358109313078,124.46746772505)) ;
#94886 = CARTESIAN_POINT('Ctrl Pts',(-18.6517412398337,43.4458121437049,124.35019270089)) ;
#94887 = CARTESIAN_POINT('Ctrl Pts',(-18.5014974666198,43.4557207229405,124.205849688173)) ;
#94888 = CARTESIAN_POINT('Ctrl Pts',(-18.3768780504373,43.4657755754965,124.035148132085)) ;
#94889 = CARTESIAN_POINT('Ctrl Pts',(-18.2853633360531,43.4756341577712,123.849147653433)) ;
#94890 = CARTESIAN_POINT('Ctrl Pts',(-18.2262007819212,43.4857022872139,123.645952408235)) ;
#94891 = CARTESIAN_POINT('Ctrl Pts',(-18.2037152670099,43.495557758903,123.439965689953)) ;
#94892 = CARTESIAN_POINT('Ctrl Pts',(-18.2168996606046,43.5055526072893,123.230263419917)) ;
#94893 = CARTESIAN_POINT('Ctrl Pts',(-18.2669194341459,43.5155839040738,123.025387393044)) ;
#94894 = CARTESIAN_POINT('Ctrl Pts',(-18.350057379065,43.5254504402838,122.835344588144)) ;
#94895 = CARTESIAN_POINT('Ctrl Pts',(-18.4660377808378,43.5354378632447,122.660345763407)) ;
#94896 = CARTESIAN_POINT('Ctrl Pts',(-18.6099846283068,43.5453828022644,122.50867783323)) ;
#94897 = CARTESIAN_POINT('Ctrl Pts',(-18.7797941808117,43.5554276881244,122.383164603067)) ;
#94898 = CARTESIAN_POINT('Ctrl Pts',(-18.9654667474152,43.5652962232107,122.290585226605)) ;
#94899 = CARTESIAN_POINT('Ctrl Pts',(-19.166175253621,43.5752620912173,122.23051446461)) ;
#94900 = CARTESIAN_POINT('Ctrl Pts',(-19.3755016238856,43.5852847386698,122.206300298283)) ;
#94901 = CARTESIAN_POINT('Ctrl Pts',(-19.5837529479575,43.5952083776774,122.218617123038)) ;
#94902 = CARTESIAN_POINT('Ctrl Pts',(-19.7872305435204,43.6051511026832,122.266516185688)) ;
#94903 = CARTESIAN_POINT('Ctrl Pts',(-19.9811658118431,43.615196708735,122.350095121641)) ;
#94904 = CARTESIAN_POINT('Ctrl Pts',(-20.1545571238917,43.6250581312561,122.463777132953)) ;
#94905 = CARTESIAN_POINT('Ctrl Pts',(-20.3078102197578,43.6350516997053,122.607448076421)) ;
#94906 = CARTESIAN_POINT('Ctrl Pts',(-20.4330542470153,43.6449771704606,122.774384365223)) ;
#94907 = CARTESIAN_POINT('Ctrl Pts',(-20.5283647810184,43.6550048444165,122.962392977543)) ;
#94908 = CARTESIAN_POINT('Ctrl Pts',(-20.5889338449823,43.6648920224582,123.161260964783)) ;
#94909 = CARTESIAN_POINT('Ctrl Pts',(-20.6145511613344,43.6749204018264,123.370499311071)) ;
#94910 = CARTESIAN_POINT('Ctrl Pts',(-20.603708283792,43.6848146445478,123.57824797087)) ;
#94911 = CARTESIAN_POINT('Ctrl Pts',(-20.5408575434125,43.6981675611987,123.851835425045)) ;
#94912 = CARTESIAN_POINT('Ctrl Pts',(-20.4095228170576,43.7113700789455,124.100006492089)) ;
#94913 = CARTESIAN_POINT('Ctrl Pts',(-20.2186590844846,43.7247259842264,124.30584947481)) ;
#94914 = CARTESIAN_POINT('Ctrl Pts',(-20.0529407367941,43.7346226328643,124.431709404068)) ;
#94915 = CARTESIAN_POINT('Ctrl Pts',(-19.8651333436592,43.7446707709167,124.528373384689)) ;
#94916 = CARTESIAN_POINT('Ctrl Pts',(-19.6665214527056,43.7545617310945,124.589983515825)) ;
#94917 = CARTESIAN_POINT('Ctrl Pts',(-19.4581739203183,43.7645545669713,124.616965017307)) ;
#94918 = CARTESIAN_POINT('Ctrl Pts',(-19.2473737691811,43.7745936619728,124.606831454262)) ;
#94919 = CARTESIAN_POINT('Ctrl Pts',(-19.0455363121503,43.784431017824,124.561650497057)) ;
#94920 = CARTESIAN_POINT('Ctrl Pts',(-18.7855906921791,43.7978239657547,124.453535628183)) ;
#94921 = CARTESIAN_POINT('Ctrl Pts',(-18.5635139422216,43.8109906421817,124.282902191796)) ;
#94922 = CARTESIAN_POINT('Ctrl Pts',(-18.3921555658983,43.8243754235884,124.05982076316)) ;
#94923 = CARTESIAN_POINT('Ctrl Pts',(-18.2962311864038,43.8342372062323,123.875972351288)) ;
#94924 = CARTESIAN_POINT('Ctrl Pts',(-18.2325177060846,43.8442363541853,123.675693020138)) ;
#94925 = CARTESIAN_POINT('Ctrl Pts',(-18.2046131430209,43.8541391468024,123.46933726225)) ;
#94926 = CARTESIAN_POINT('Ctrl Pts',(-18.2131381453431,43.8641887266934,123.258291456471)) ;
#94927 = CARTESIAN_POINT('Ctrl Pts',(-18.2717478838939,43.8773758005028,122.987197867203)) ;
#94928 = CARTESIAN_POINT('Ctrl Pts',(-18.4346578307406,43.894128590474,122.670626737531)) ;
#94929 = CARTESIAN_POINT('Ctrl Pts',(-18.6920466360006,43.9106172425687,122.432275019255)) ;
#94930 = CARTESIAN_POINT('Ctrl Pts',(-18.9400675272099,43.9239740687521,122.300862325712)) ;
#94931 = CARTESIAN_POINT('Ctrl Pts',(-19.1380510126641,43.9338704536301,122.236740383754)) ;
#94932 = CARTESIAN_POINT('Ctrl Pts',(-19.3463246739333,43.9438769681505,122.207560048397)) ;
#94933 = CARTESIAN_POINT('Ctrl Pts',(-19.6235856775625,43.9570670916669,122.216668870961)) ;
#94934 = CARTESIAN_POINT('Ctrl Pts',(-19.9644818436407,43.9738336528165,122.320510334503)) ;
#94935 = CARTESIAN_POINT('Ctrl Pts',(-20.3009628920008,43.9936181415245,122.573194359598)) ;
#94936 = CARTESIAN_POINT('Ctrl Pts',(-20.5338593579288,44.013563589121,122.927488610448)) ;
#94937 = CARTESIAN_POINT('Ctrl Pts',(-20.6313432900852,44.0334752512769,123.339498293357)) ;
#94938 = CARTESIAN_POINT('Ctrl Pts',(-20.5833486167225,44.0533674432958,123.759794144768)) ;
#94939 = CARTESIAN_POINT('Ctrl Pts',(-20.3928831509426,44.0734085738504,124.140920763772)) ;
#94940 = CARTESIAN_POINT('Ctrl Pts',(-20.0872651227944,44.093226908466,124.431188469876)) ;
#94941 = CARTESIAN_POINT('Ctrl Pts',(-19.6984333457732,44.1131994736856,124.601580100911)) ;
#94942 = CARTESIAN_POINT('Ctrl Pts',(-19.2762687397461,44.1330886898572,124.629069312645)) ;
#94943 = CARTESIAN_POINT('Ctrl Pts',(-18.8676587652594,44.1531122641799,124.509843388215)) ;
#94944 = CARTESIAN_POINT('Ctrl Pts',(-18.5278179721396,44.1729094272682,124.261320737249)) ;
#94945 = CARTESIAN_POINT('Ctrl Pts',(-18.2904317837081,44.1928749210919,123.909483288494)) ;
#94946 = CARTESIAN_POINT('Ctrl Pts',(-18.1878781194109,44.2128286288334,123.497677701011)) ;
#94947 = CARTESIAN_POINT('Ctrl Pts',(-18.2318638131071,44.23273600556,123.076779952571)) ;
#94948 = CARTESIAN_POINT('Ctrl Pts',(-18.4153837347408,44.2525882171085,122.696570104589)) ;
#94949 = CARTESIAN_POINT('Ctrl Pts',(-18.7212134876534,44.2726606040542,122.398901422161)) ;
#94950 = CARTESIAN_POINT('Ctrl Pts',(-19.1059666063529,44.2924984736945,122.226014999044)) ;
#94951 = CARTESIAN_POINT('Ctrl Pts',(-19.5267471998441,44.3123491282477,122.192956248607)) ;
#94952 = CARTESIAN_POINT('Ctrl Pts',(-19.9374778624856,44.3324010625881,122.30720495541)) ;
#94953 = CARTESIAN_POINT('Ctrl Pts',(-20.2808529206033,44.3522342501541,122.552178926916)) ;
#94954 = CARTESIAN_POINT('Ctrl Pts',(-20.5217266142263,44.3721634623848,122.900618714666)) ;
#94955 = CARTESIAN_POINT('Ctrl Pts',(-20.6295648554186,44.3920484275992,123.309611341229)) ;
#94956 = CARTESIAN_POINT('Ctrl Pts',(-20.5903665695791,44.4121221687438,123.734542200108)) ;
#94957 = CARTESIAN_POINT('Ctrl Pts',(-20.4110378863135,44.4319153505242,124.115354713152)) ;
#94958 = CARTESIAN_POINT('Ctrl Pts',(-20.1109493418059,44.4518780585269,124.415495408752)) ;
#94959 = CARTESIAN_POINT('Ctrl Pts',(-19.7255902485524,44.4718610102694,124.594483394183)) ;
#94960 = CARTESIAN_POINT('Ctrl Pts',(-19.3059766594542,44.4916716300415,124.631738877851)) ;
#94961 = CARTESIAN_POINT('Ctrl Pts',(-18.8952789795798,44.5116553460744,124.523139920647)) ;
#94962 = CARTESIAN_POINT('Ctrl Pts',(-18.5479537567652,44.5315368099717,124.28197871897)) ;
#94963 = CARTESIAN_POINT('Ctrl Pts',(-18.3027327952688,44.5514921398161,123.935816420611)) ;
#94964 = CARTESIAN_POINT('Ctrl Pts',(-18.1904707624219,44.5713676006216,123.528324021289)) ;
#94965 = CARTESIAN_POINT('Ctrl Pts',(-18.2239254020228,44.5913519206731,123.104770226885)) ;
#94966 = CARTESIAN_POINT('Ctrl Pts',(-18.3996904677657,44.6112799534628,122.71911120197)) ;
#94967 = CARTESIAN_POINT('Ctrl Pts',(-18.6468965142443,44.6278887154025,122.467053011659)) ;
#94968 = CARTESIAN_POINT('Ctrl Pts',(-18.8854150868298,44.6410763540926,122.32564319516)) ;
#94969 = CARTESIAN_POINT('Ctrl Pts',(-19.0816688013698,44.6510627884528,122.251110504888)) ;
#94970 = CARTESIAN_POINT('Ctrl Pts',(-19.2884344373437,44.6610721624121,122.211902195328)) ;
#94971 = CARTESIAN_POINT('Ctrl Pts',(-19.5677616553926,44.6743621959774,122.208107590345)) ;
#94972 = CARTESIAN_POINT('Ctrl Pts',(-19.909946568067,44.6909561836399,122.294466869324)) ;
#94973 = CARTESIAN_POINT('Ctrl Pts',(-20.2026693922946,44.7075884389154,122.492797225526)) ;
#94974 = CARTESIAN_POINT('Ctrl Pts',(-20.3849910652847,44.7208308225832,122.703234545507)) ;
#94975 = CARTESIAN_POINT('Ctrl Pts',(-20.4925937469405,44.7307450308107,122.881741651042)) ;
#94976 = CARTESIAN_POINT('Ctrl Pts',(-20.5684167531968,44.7408016700823,123.079084895041)) ;
#94977 = CARTESIAN_POINT('Ctrl Pts',(-20.6082256062744,44.7506474765025,123.282226426836)) ;
#94978 = CARTESIAN_POINT('Ctrl Pts',(-20.612596699093,44.7606924761356,123.4933577631)) ;
#94979 = CARTESIAN_POINT('Ctrl Pts',(-20.5694218883815,44.7739734985084,123.769153441609)) ;
#94980 = CARTESIAN_POINT('Ctrl Pts',(-20.4566672831877,44.787170945033,124.026150744995)) ;
#94981 = CARTESIAN_POINT('Ctrl Pts',(-20.2801264821268,44.80058524284,124.246100686113)) ;
#94982 = CARTESIAN_POINT('Ctrl Pts',(-20.1246823390785,44.8104243082428,124.382580125368)) ;
#94983 = CARTESIAN_POINT('Ctrl Pts',(-19.9456254369474,44.8204075145204,124.492026841846)) ;
#94984 = CARTESIAN_POINT('Ctrl Pts',(-19.7508537581695,44.8303587494332,124.568420993934)) ;
#94985 = CARTESIAN_POINT('Ctrl Pts',(-19.5448027338605,44.8403597491349,124.610291848731)) ;
#94986 = CARTESIAN_POINT('Ctrl Pts',(-19.3339773939872,44.8503910949222,124.615434702964)) ;
#94987 = CARTESIAN_POINT('Ctrl Pts',(-19.1291026875363,44.8602448596272,124.584732769678)) ;
#94988 = CARTESIAN_POINT('Ctrl Pts',(-18.9302085569886,44.8702155132955,124.518626229001)) ;
#94989 = CARTESIAN_POINT('Ctrl Pts',(-18.7452782875516,44.8802127569528,124.418690892324)) ;
#94990 = CARTESIAN_POINT('Ctrl Pts',(-18.5801193571764,44.8902462128969,124.287508814741)) ;
#94991 = CARTESIAN_POINT('Ctrl Pts',(-18.4424514262048,44.9001017171973,124.132637434498)) ;
#94992 = CARTESIAN_POINT('Ctrl Pts',(-18.3319695722202,44.9101011534834,123.953834850659)) ;
#94993 = CARTESIAN_POINT('Ctrl Pts',(-18.2547793540301,44.9199956129993,123.760632273683)) ;
#94994 = CARTESIAN_POINT('Ctrl Pts',(-18.211660949245,44.930058732451,123.553551718447)) ;
#94995 = CARTESIAN_POINT('Ctrl Pts',(-18.2050676049964,44.939898366863,123.346762420649)) ;
#94996 = CARTESIAN_POINT('Ctrl Pts',(-18.2348732987409,44.9499615743488,123.137341924846)) ;
#94997 = CARTESIAN_POINT('Ctrl Pts',(-18.2996654380059,44.9598556817279,122.939659991958)) ;
#94998 = CARTESIAN_POINT('Ctrl Pts',(-18.3977574562744,44.9697980139203,122.755119782412)) ;
#94999 = CARTESIAN_POINT('Ctrl Pts',(-18.5271124178291,44.9797986402353,122.58933669533)) ;
#95000 = CARTESIAN_POINT('Ctrl Pts',(-18.6841544980773,44.9898403745172,122.448281242363)) ;
#95001 = CARTESIAN_POINT('Ctrl Pts',(-18.859229594049,44.9996658004663,122.338633544049)) ;
#95002 = CARTESIAN_POINT('Ctrl Pts',(-19.0550454607519,45.009722626994,122.258943891546)) ;
#95003 = CARTESIAN_POINT('Ctrl Pts',(-19.2591518340344,45.0196500601156,122.215318487338)) ;
#95004 = CARTESIAN_POINT('Ctrl Pts',(-19.4681812808614,45.0296000525218,122.207180133437)) ;
#95005 = CARTESIAN_POINT('Ctrl Pts',(-19.6775673181932,45.0396552535958,122.2361259376)) ;
#95006 = CARTESIAN_POINT('Ctrl Pts',(-19.8742295207309,45.0494775276481,122.299140357203)) ;
#95007 = CARTESIAN_POINT('Ctrl Pts',(-20.0614575634697,45.0595334216073,122.397284057892)) ;
#95008 = CARTESIAN_POINT('Ctrl Pts',(-20.226674164749,45.0694741434525,122.525274601464)) ;
#95009 = CARTESIAN_POINT('Ctrl Pts',(-20.3671232498211,45.079378487539,122.678999528342)) ;
#95010 = CARTESIAN_POINT('Ctrl Pts',(-20.4802264787641,45.0894251548385,122.857355770143)) ;
#95011 = CARTESIAN_POINT('Ctrl Pts',(-20.5596285796948,45.0993207132885,123.049678684539)) ;
#95012 = CARTESIAN_POINT('Ctrl Pts',(-20.605171036414,45.1093827919931,123.256223873062)) ;
#95013 = CARTESIAN_POINT('Ctrl Pts',(-20.6140833446589,45.1192254904589,123.462979282518)) ;
#95014 = CARTESIAN_POINT('Ctrl Pts',(-20.587052536111,45.1292162643534,123.671243804654)) ;
#95015 = CARTESIAN_POINT('Ctrl Pts',(-20.5246209802578,45.1391441335883,123.870412103344)) ;
#95016 = CARTESIAN_POINT('Ctrl Pts',(-20.4282957923679,45.1491328625582,124.057023143126)) ;
#95017 = CARTESIAN_POINT('Ctrl Pts',(-20.300088730677,45.1591722645419,124.224668107003)) ;
#95018 = CARTESIAN_POINT('Ctrl Pts',(-20.1480643896778,45.1690124322787,124.364985798958)) ;
#95019 = CARTESIAN_POINT('Ctrl Pts',(-19.9704897857701,45.1790606426532,124.479388556005)) ;
#95020 = CARTESIAN_POINT('Ctrl Pts',(-19.7775671927321,45.189007812941,124.560097139882)) ;
#95021 = CARTESIAN_POINT('Ctrl Pts',(-19.5744414816242,45.198918661196,124.606523875413)) ;
#95022 = CARTESIAN_POINT('Ctrl Pts',(-19.3632945233948,45.2089749888738,124.616929811313)) ;
#95023 = CARTESIAN_POINT('Ctrl Pts',(-19.1577990703498,45.2188254016423,124.591231954316)) ;
#95024 = CARTESIAN_POINT('Ctrl Pts',(-18.9562025405331,45.228852287476,124.529644851264)) ;
#95025 = CARTESIAN_POINT('Ctrl Pts',(-18.7685671992907,45.2388809031068,124.433479713796)) ;
#95026 = CARTESIAN_POINT('Ctrl Pts',(-18.6033345212596,45.2487261264844,124.308847809441)) ;
#95027 = CARTESIAN_POINT('Ctrl Pts',(-18.4597435365736,45.2587168085859,124.155554340347)) ;
#95028 = CARTESIAN_POINT('Ctrl Pts',(-18.3448064981045,45.2687546972184,123.978575669867)) ;
#95029 = CARTESIAN_POINT('Ctrl Pts',(-18.2635978150533,45.2785990323215,123.788206668154)) ;
#95030 = CARTESIAN_POINT('Ctrl Pts',(-18.2156129207493,45.2885839945191,123.583878862272)) ;
#95031 = CARTESIAN_POINT('Ctrl Pts',(-18.2037886149857,45.2985229360524,123.375235476111)) ;
#95032 = CARTESIAN_POINT('Ctrl Pts',(-18.2286862668487,45.3085648210239,123.165616917529)) ;
#95033 = CARTESIAN_POINT('Ctrl Pts',(-18.2885437806197,45.3184513689321,122.966555293898)) ;
#95034 = CARTESIAN_POINT('Ctrl Pts',(-18.3827734035262,45.3284452944321,122.778797331814)) ;
#95035 = CARTESIAN_POINT('Ctrl Pts',(-18.5074028841177,45.3383813855586,122.611122603817)) ;
#95036 = CARTESIAN_POINT('Ctrl Pts',(-18.6606617419149,45.3484106545385,122.466359785052)) ;
#95037 = CARTESIAN_POINT('Ctrl Pts',(-18.8340526690746,45.3582930370979,122.351852199141)) ;
#95038 = CARTESIAN_POINT('Ctrl Pts',(-19.0278880503773,45.3683455541857,122.267728236563)) ;
#95039 = CARTESIAN_POINT('Ctrl Pts',(-19.2301906008237,45.3782396750096,122.219193863499)) ;
#95040 = CARTESIAN_POINT('Ctrl Pts',(-19.4413039174828,45.38830165443,122.206261136697)) ;
#95041 = CARTESIAN_POINT('Ctrl Pts',(-19.6469491825146,45.398146187659,122.229642978978)) ;
#95042 = CARTESIAN_POINT('Ctrl Pts',(-19.8479428991622,45.4081062665652,122.288339189176)) ;
#95043 = CARTESIAN_POINT('Ctrl Pts',(-20.0369764252112,45.4181445431378,122.382139581479)) ;
#95044 = CARTESIAN_POINT('Ctrl Pts',(-20.2043294392257,45.4280179296757,122.504984302284)) ;
#95045 = CARTESIAN_POINT('Ctrl Pts',(-20.3506163047683,45.4380908724427,122.658044774767)) ;
#95046 = CARTESIAN_POINT('Ctrl Pts',(-20.4654246636601,45.4479122865711,122.829707674771)) ;
#95047 = CARTESIAN_POINT('Ctrl Pts',(-20.5510305647617,45.4579869166434,123.023395197919)) ;
#95048 = CARTESIAN_POINT('Ctrl Pts',(-20.6005900616309,45.4678535539602,123.224841786073)) ;
#95049 = CARTESIAN_POINT('Ctrl Pts',(-20.6151763361897,45.477877099332,123.43505318199)) ;
#95050 = CARTESIAN_POINT('Ctrl Pts',(-20.5925286407093,45.4879028508492,123.644618706423)) ;
#95051 = CARTESIAN_POINT('Ctrl Pts',(-20.535184701194,45.4977564378586,123.843665059279)) ;
#95052 = CARTESIAN_POINT('Ctrl Pts',(-20.4435052359796,45.5077333980865,124.032319483579)) ;
#95053 = CARTESIAN_POINT('Ctrl Pts',(-20.3196371816528,45.517754541115,124.202720679813)) ;
#95054 = CARTESIAN_POINT('Ctrl Pts',(-20.1704223024116,45.5276371471349,124.347330357567)) ;
#95055 = CARTESIAN_POINT('Ctrl Pts',(-19.9951347534933,45.5377056177676,124.46592141779)) ;
#95056 = CARTESIAN_POINT('Ctrl Pts',(-19.80652763825,45.5475357009513,124.55047845137)) ;
#95057 = CARTESIAN_POINT('Ctrl Pts',(-19.6014167542772,45.5576022606317,124.602468011462)) ;
#95058 = CARTESIAN_POINT('Ctrl Pts',(-19.3940227762553,45.5674925104609,124.617656228685)) ;
#95059 = CARTESIAN_POINT('Ctrl Pts',(-19.1850009207313,45.5774846762097,124.596848277277)) ;
#95060 = CARTESIAN_POINT('Ctrl Pts',(-18.9834082543819,45.5874475198058,124.540036396267)) ;
#95061 = CARTESIAN_POINT('Ctrl Pts',(-18.7956023609983,45.5973516886336,124.45008818612)) ;
#95062 = CARTESIAN_POINT('Ctrl Pts',(-18.623736295235,45.6074125635279,124.326851256807)) ;
#95063 = CARTESIAN_POINT('Ctrl Pts',(-18.4788923126259,45.6172514668573,124.179140534936)) ;
#95064 = CARTESIAN_POINT('Ctrl Pts',(-18.3590375189782,45.6273198432312,124.004715614886)) ;
#95065 = CARTESIAN_POINT('Ctrl Pts',(-18.2729630465884,45.6372004598639,123.815633502549)) ;
#95066 = CARTESIAN_POINT('Ctrl Pts',(-18.2200510520963,45.6471916200928,123.612393264672)) ;
#95067 = CARTESIAN_POINT('Ctrl Pts',(-18.2032574681038,45.6571446935249,123.403791977135)) ;
#95068 = CARTESIAN_POINT('Ctrl Pts',(-18.2231668387161,45.6671805291376,123.193765820803)) ;
#95069 = CARTESIAN_POINT('Ctrl Pts',(-18.278298264541,45.6770706558677,122.99327332114)) ;
#95070 = CARTESIAN_POINT('Ctrl Pts',(-18.3680085171694,45.6870628376371,122.80333742584)) ;
#95071 = CARTESIAN_POINT('Ctrl Pts',(-18.4888375636561,45.6970087776115,122.632688971449)) ;
#95072 = CARTESIAN_POINT('Ctrl Pts',(-18.637188992051,45.706955961371,122.485285003098)) ;
#95073 = CARTESIAN_POINT('Ctrl Pts',(-18.8107406957346,45.7170038996613,122.364873637851)) ;
#95074 = CARTESIAN_POINT('Ctrl Pts',(-18.9986732175206,45.7268515344749,122.278026568986)) ;
#95075 = CARTESIAN_POINT('Ctrl Pts',(-19.2009699760855,45.7368132481728,122.22388545414)) ;
#95076 = CARTESIAN_POINT('Ctrl Pts',(-19.4110424427331,45.746841883994,122.205834191296)) ;
#95077 = CARTESIAN_POINT('Ctrl Pts',(-19.6185632243262,45.7567521987458,122.224242549515)) ;
#95078 = CARTESIAN_POINT('Ctrl Pts',(-19.820392725705,45.7666870694084,122.278012302123)) ;
#95079 = CARTESIAN_POINT('Ctrl Pts',(-20.0117473837365,45.7767282518102,122.367127706858)) ;
#95080 = CARTESIAN_POINT('Ctrl Pts',(-20.1821838127246,45.7866152232749,122.486134490758)) ;
#95081 = CARTESIAN_POINT('Ctrl Pts',(-20.3311987926498,45.7966146555375,122.634375510774)) ;
#95082 = CARTESIAN_POINT('Ctrl Pts',(-20.4513952143733,45.8065347207942,122.804835855089)) ;
#95083 = CARTESIAN_POINT('Ctrl Pts',(-20.5412360456862,45.8165715733783,122.995747910381)) ;
#95084 = CARTESIAN_POINT('Ctrl Pts',(-20.5958772836658,45.8264842327183,123.196855969057)) ;
#95085 = CARTESIAN_POINT('Ctrl Pts',(-20.615375050569,45.8364754446332,123.406008392214)) ;
#95086 = CARTESIAN_POINT('Ctrl Pts',(-20.5977036104295,45.8465170860363,123.616357719273)) ;
#95087 = CARTESIAN_POINT('Ctrl Pts',(-20.5454116666777,45.8563458802434,123.816292415274)) ;
#95088 = CARTESIAN_POINT('Ctrl Pts',(-20.4571378687505,45.8664222913646,124.008815830626)) ;
#95089 = CARTESIAN_POINT('Ctrl Pts',(-20.3394955135026,45.8762744244071,124.179339825008)) ;
#95090 = CARTESIAN_POINT('Ctrl Pts',(-20.1909503753333,45.8863476587484,124.330227006031)) ;
#95091 = CARTESIAN_POINT('Ctrl Pts',(-20.0223590773789,45.896189160075,124.45018473356)) ;
#95092 = CARTESIAN_POINT('Ctrl Pts',(-19.8335905381555,45.9061501116698,124.540828594865)) ;
#95093 = CARTESIAN_POINT('Ctrl Pts',(-19.6302804589424,45.9161879293905,124.597348541929)) ;
#95094 = CARTESIAN_POINT('Ctrl Pts',(-19.4236714959756,45.9260622786475,124.617764021895)) ;
#95095 = CARTESIAN_POINT('Ctrl Pts',(-19.2126193484243,45.9361318293897,124.601674276228)) ;
#95096 = CARTESIAN_POINT('Ctrl Pts',(-19.0122873115152,45.9459658488983,124.550514505087)) ;
#95097 = CARTESIAN_POINT('Ctrl Pts',(-18.8198465129963,45.9560000034779,124.464134660922)) ;
#95098 = CARTESIAN_POINT('Ctrl Pts',(-18.6459181894139,45.9660159293003,124.345423530653)) ;
#95099 = CARTESIAN_POINT('Ctrl Pts',(-18.4970009713093,45.9758981844946,124.20055280957)) ;
#95100 = CARTESIAN_POINT('Ctrl Pts',(-18.3739944783542,45.9858869910055,124.030382117797)) ;
#95101 = CARTESIAN_POINT('Ctrl Pts',(-18.2826051031244,45.9958355582682,123.842218571449)) ;
#95102 = CARTESIAN_POINT('Ctrl Pts',(-18.224895071071,46.0058903635702,123.638888686045)) ;
#95103 = CARTESIAN_POINT('Ctrl Pts',(-18.2035713061239,46.0157091468338,123.433561311371)) ;
#95104 = CARTESIAN_POINT('Ctrl Pts',(-18.2179813427917,46.0257449191944,123.223075314158)) ;
#95105 = CARTESIAN_POINT('Ctrl Pts',(-18.2692515836051,46.035769618223,123.018648178243)) ;
#95106 = CARTESIAN_POINT('Ctrl Pts',(-18.3533370643761,46.0456216214821,122.829360944997)) ;
#95107 = CARTESIAN_POINT('Ctrl Pts',(-18.4703613636276,46.0556125558793,122.654971111735)) ;
#95108 = CARTESIAN_POINT('Ctrl Pts',(-18.6147606274529,46.0655304783104,122.504524563448)) ;
#95109 = CARTESIAN_POINT('Ctrl Pts',(-18.7849011160605,46.0755588339928,122.380053433214)) ;
#95110 = CARTESIAN_POINT('Ctrl Pts',(-18.9713293181431,46.0854431185033,122.288249837825)) ;
#95111 = CARTESIAN_POINT('Ctrl Pts',(-19.1729140808588,46.0954358024112,122.229120011602)) ;
#95112 = CARTESIAN_POINT('Ctrl Pts',(-19.3824991169952,46.1054645394189,122.206173308902)) ;
#95113 = CARTESIAN_POINT('Ctrl Pts',(-19.5899010934406,46.1153499360478,122.219495008975)) ;
#95114 = CARTESIAN_POINT('Ctrl Pts',(-19.7939762330509,46.1253378214617,122.268837873898)) ;
#95115 = CARTESIAN_POINT('Ctrl Pts',(-19.9857528109284,46.1352885241223,122.352485218337)) ;
#95116 = CARTESIAN_POINT('Ctrl Pts',(-20.161556069214,46.1453288422197,122.469269469153)) ;
#95117 = CARTESIAN_POINT('Ctrl Pts',(-20.3120617664578,46.155203407553,122.612283972621)) ;
#95118 = CARTESIAN_POINT('Ctrl Pts',(-20.4371930752356,46.165203067614,122.781168558695)) ;
#95119 = CARTESIAN_POINT('Ctrl Pts',(-20.5304591803611,46.1751120627818,122.967483465853)) ;
#95120 = CARTESIAN_POINT('Ctrl Pts',(-20.5907489831864,46.185166803945,123.170050000075)) ;
#95121 = CARTESIAN_POINT('Ctrl Pts',(-20.6147246475824,46.1950254158588,123.375954151209)) ;
#95122 = CARTESIAN_POINT('Ctrl Pts',(-20.602458271204,46.2050935381382,123.587231216781)) ;
#95123 = CARTESIAN_POINT('Ctrl Pts',(-20.55469644977,46.2149490088413,123.788861901964)) ;
#95124 = CARTESIAN_POINT('Ctrl Pts',(-20.4720783460226,46.2249438683347,123.982053991813)) ;
#95125 = CARTESIAN_POINT('Ctrl Pts',(-20.3563663912359,46.2349751216766,124.158367942863)) ;
#95126 = CARTESIAN_POINT('Ctrl Pts',(-20.2144077277106,46.2448418205497,124.309619918367)) ;
#95127 = CARTESIAN_POINT('Ctrl Pts',(-20.0465524037554,46.2548286363009,124.435697561144)) ;
#95128 = CARTESIAN_POINT('Ctrl Pts',(-19.8600955667998,46.2647758414964,124.530446740553)) ;
#95129 = CARTESIAN_POINT('Ctrl Pts',(-19.6581071039658,46.2748188296227,124.591866565516)) ;
#95130 = CARTESIAN_POINT('Ctrl Pts',(-19.4521805333531,46.2846861842441,124.616961782451)) ;
#95131 = CARTESIAN_POINT('Ctrl Pts',(-19.2429425557365,46.2946520775422,124.606374912702)) ;
#95132 = CARTESIAN_POINT('Ctrl Pts',(-19.0375622356336,46.3046758549183,124.559128812759)) ;
#95133 = CARTESIAN_POINT('Ctrl Pts',(-18.8454096797733,46.31460140285,124.477797809771)) ;
#95134 = CARTESIAN_POINT('Ctrl Pts',(-18.6697469855998,46.324541879271,124.364570062756)) ;
#95135 = CARTESIAN_POINT('Ctrl Pts',(-18.5149640326818,46.3345880889339,124.220891191222)) ;
#95136 = CARTESIAN_POINT('Ctrl Pts',(-18.3896311429389,46.3444493455957,124.055728922196)) ;
#95137 = CARTESIAN_POINT('Ctrl Pts',(-18.293309290402,46.354442973871,123.869046532394)) ;
#95138 = CARTESIAN_POINT('Ctrl Pts',(-18.2311685522443,46.3643683711812,123.66981820444)) ;
#95139 = CARTESIAN_POINT('Ctrl Pts',(-18.2042912858194,46.3743962790915,123.460747760287)) ;
#95140 = CARTESIAN_POINT('Ctrl Pts',(-18.2137735652892,46.3842825947606,123.253091982642)) ;
#95141 = CARTESIAN_POINT('Ctrl Pts',(-18.2597106191738,46.3943141896644,123.047294517772)) ;
#95142 = CARTESIAN_POINT('Ctrl Pts',(-18.3393268080078,46.4041964326161,122.855362755842)) ;
#95143 = CARTESIAN_POINT('Ctrl Pts',(-18.4529567773055,46.414255903646,122.677029418448)) ;
#95144 = CARTESIAN_POINT('Ctrl Pts',(-18.593127764121,46.4241223483091,122.524119521912)) ;
#95145 = CARTESIAN_POINT('Ctrl Pts',(-18.7589661169091,46.4340884727578,122.396081343942)) ;
#95146 = CARTESIAN_POINT('Ctrl Pts',(-18.94587076229,46.444118716149,122.298455525749)) ;
#95147 = CARTESIAN_POINT('Ctrl Pts',(-19.1440685803664,46.454011751102,122.235347185995)) ;
#95148 = CARTESIAN_POINT('Ctrl Pts',(-19.3534587786841,46.4640626653389,122.207116928678)) ;
#95149 = CARTESIAN_POINT('Ctrl Pts',(-19.5612106794145,46.4739524915634,122.215512482208)) ;
#95150 = CARTESIAN_POINT('Ctrl Pts',(-19.8352623928839,46.4872873066104,122.274761976514)) ;
#95151 = CARTESIAN_POINT('Ctrl Pts',(-20.0862027417132,46.5005643977818,122.404067085043)) ;
#95152 = CARTESIAN_POINT('Ctrl Pts',(-20.2927726800463,46.5138126863801,122.590867858062)) ;
#95153 = CARTESIAN_POINT('Ctrl Pts',(-20.4224375762287,46.5238675278742,122.757782621042)) ;
#95154 = CARTESIAN_POINT('Ctrl Pts',(-20.5192877126657,46.5336985171818,122.940402706794)) ;
#95155 = CARTESIAN_POINT('Ctrl Pts',(-20.584675695254,46.543775081505,123.141863716105)) ;
#95156 = CARTESIAN_POINT('Ctrl Pts',(-20.6134306365169,46.5536244066389,123.346938502244)) ;
#95157 = CARTESIAN_POINT('Ctrl Pts',(-20.6042235970705,46.5669724062762,123.627443254569)) ;
#95158 = CARTESIAN_POINT('Ctrl Pts',(-20.5014828458008,46.5835571658128,123.96471352082)) ;
#95159 = CARTESIAN_POINT('Ctrl Pts',(-20.2906566247989,46.6001257171609,124.247018966344)) ;
#95160 = CARTESIAN_POINT('Ctrl Pts',(-20.0699817614832,46.6134855419799,124.420721848801)) ;
#95161 = CARTESIAN_POINT('Ctrl Pts',(-19.8865379628429,46.6233909508105,124.519311216368)) ;
#95162 = CARTESIAN_POINT('Ctrl Pts',(-19.6878067636741,46.6333509773946,124.585185790603)) ;
#95163 = CARTESIAN_POINT('Ctrl Pts',(-19.412046265777,46.6466085615799,124.625974157288)) ;
#95164 = CARTESIAN_POINT('Ctrl Pts',(-19.0603317080607,46.6632597730745,124.585529966129)) ;
#95165 = CARTESIAN_POINT('Ctrl Pts',(-18.6814960639514,46.6831779871848,124.39623149894)) ;
#95166 = CARTESIAN_POINT('Ctrl Pts',(-18.3898810556828,46.7030557504057,124.090210943311)) ;
#95167 = CARTESIAN_POINT('Ctrl Pts',(-18.2194528936374,46.7230684181928,123.700392538323)) ;
#95168 = CARTESIAN_POINT('Ctrl Pts',(-18.192146649637,46.7428809408594,123.279930238495)) ;
#95169 = CARTESIAN_POINT('Ctrl Pts',(-18.3102874548359,46.7628642408593,122.871872061097)) ;
#95170 = CARTESIAN_POINT('Ctrl Pts',(-18.5598053137279,46.7827585179606,122.530215742655)) ;
#95171 = CARTESIAN_POINT('Ctrl Pts',(-18.9111817055603,46.8026912797184,122.293251036781)) ;
#95172 = CARTESIAN_POINT('Ctrl Pts',(-19.3230997389013,46.8226572854831,122.190530003981)) ;
#95173 = CARTESIAN_POINT('Ctrl Pts',(-19.743552728489,46.842535817648,122.234047595164)) ;
#95174 = CARTESIAN_POINT('Ctrl Pts',(-20.1251993127685,46.8624754843083,122.418602193788)) ;
#95175 = CARTESIAN_POINT('Ctrl Pts',(-20.4204440382174,46.8823703589537,122.721609165698)) ;
#95176 = CARTESIAN_POINT('Ctrl Pts',(-20.5949959092053,46.902277498247,123.107115871123)) ;
#95177 = CARTESIAN_POINT('Ctrl Pts',(-20.6282641723877,46.9221880463255,123.529296695929)) ;
#95178 = CARTESIAN_POINT('Ctrl Pts',(-20.5136941034275,46.9422566316827,123.940243017391)) ;
#95179 = CARTESIAN_POINT('Ctrl Pts',(-20.2695209088635,46.9620384289975,124.282898500784)) ;
#95180 = CARTESIAN_POINT('Ctrl Pts',(-19.9197275238897,46.982045975942,124.524725530521)) ;
#95181 = CARTESIAN_POINT('Ctrl Pts',(-19.5119619250136,47.0018677142448,124.631757161439)) ;
#95182 = CARTESIAN_POINT('Ctrl Pts',(-19.0889034196956,47.021847734149,124.593693802023)) ;
#95183 = CARTESIAN_POINT('Ctrl Pts',(-18.7055978572191,47.0417651854112,124.413578300062)) ;
#95184 = CARTESIAN_POINT('Ctrl Pts',(-18.4066951109051,47.0616401065839,124.114802890344)) ;
#95185 = CARTESIAN_POINT('Ctrl Pts',(-18.226617705254,47.0816644751348,123.729017723871)) ;
#95186 = CARTESIAN_POINT('Ctrl Pts',(-18.189408601878,47.1015311595082,123.308171256275)) ;
#95187 = CARTESIAN_POINT('Ctrl Pts',(-18.2977813628575,47.1214749813544,122.898242687212)) ;
#95188 = CARTESIAN_POINT('Ctrl Pts',(-18.5392371883832,47.141382350606,122.550578232716)) ;
#95189 = CARTESIAN_POINT('Ctrl Pts',(-18.8838108505728,47.1612570483527,122.305940543012)) ;
#95190 = CARTESIAN_POINT('Ctrl Pts',(-19.2933814550574,47.1812389908744,122.192858534516)) ;
#95191 = CARTESIAN_POINT('Ctrl Pts',(-19.7151773995363,47.2011416577852,122.226545847084)) ;
#95192 = CARTESIAN_POINT('Ctrl Pts',(-20.0998580309074,47.2209970153239,122.400636973891)) ;
#95193 = CARTESIAN_POINT('Ctrl Pts',(-20.4047901284186,47.2410610540399,122.698899639654)) ;
#95194 = CARTESIAN_POINT('Ctrl Pts',(-20.5876552099661,47.260916233765,123.079589215537)) ;
#95195 = CARTESIAN_POINT('Ctrl Pts',(-20.6302016757716,47.2808963384294,123.502119802794)) ;
#95196 = CARTESIAN_POINT('Ctrl Pts',(-20.5273230835641,47.3007054435992,123.910681564784)) ;
#95197 = CARTESIAN_POINT('Ctrl Pts',(-20.2895042513562,47.3206980639399,124.262875716145)) ;
#95198 = CARTESIAN_POINT('Ctrl Pts',(-20.0050353154875,47.337237546444,124.469774715203)) ;
#95199 = CARTESIAN_POINT('Ctrl Pts',(-19.7428588681219,47.3506018645082,124.570749567793)) ;
#95200 = CARTESIAN_POINT('Ctrl Pts',(-19.4702099178661,47.3638194670097,124.624411955368)) ;
#95201 = CARTESIAN_POINT('Ctrl Pts',(-19.1168449437706,47.3804770612875,124.600779206407)) ;
#95202 = CARTESIAN_POINT('Ctrl Pts',(-18.7302030844524,47.4003427633293,124.430524065223)) ;
#95203 = CARTESIAN_POINT('Ctrl Pts',(-18.4743682787184,47.4169724900193,124.18657910822)) ;
#95204 = CARTESIAN_POINT('Ctrl Pts',(-18.3289985873677,47.4302616051571,123.947912570718)) ;
#95205 = CARTESIAN_POINT('Ctrl Pts',(-18.2525289057736,47.4402259521342,123.752907821756)) ;
#95206 = CARTESIAN_POINT('Ctrl Pts',(-18.211089465491,47.4501543201357,123.54833464698)) ;
#95207 = CARTESIAN_POINT('Ctrl Pts',(-18.2034573471076,47.4634377532245,123.269197774288)) ;
#95208 = CARTESIAN_POINT('Ctrl Pts',(-18.2859430582896,47.4800898309648,122.924823240725)) ;
#95209 = CARTESIAN_POINT('Ctrl Pts',(-18.4796139718569,47.4966412002656,122.631051279502)) ;
#95210 = CARTESIAN_POINT('Ctrl Pts',(-18.6881383224874,47.5099286284146,122.445096775758)) ;
#95211 = CARTESIAN_POINT('Ctrl Pts',(-18.8678491667087,47.5199731681147,122.334247512461)) ;
#95212 = CARTESIAN_POINT('Ctrl Pts',(-19.060072139105,47.5298160099385,122.257599489778)) ;
#95213 = CARTESIAN_POINT('Ctrl Pts',(-19.2654626653682,47.5398002941855,122.214420612001)) ;
#95214 = CARTESIAN_POINT('Ctrl Pts',(-19.4745348865352,47.5497499395846,122.207626210746)) ;
#95215 = CARTESIAN_POINT('Ctrl Pts',(-19.6826924292241,47.559749701273,122.237130762337)) ;
#95216 = CARTESIAN_POINT('Ctrl Pts',(-19.8830746491751,47.5697810472319,122.302862428866)) ;
#95217 = CARTESIAN_POINT('Ctrl Pts',(-20.0658794802502,47.5796360017091,122.400373786008)) ;
#95218 = CARTESIAN_POINT('Ctrl Pts',(-20.2312035024251,47.5896085397096,122.529268274706)) ;
#95219 = CARTESIAN_POINT('Ctrl Pts',(-20.3719769005588,47.5996035334445,122.685311427216)) ;
#95220 = CARTESIAN_POINT('Ctrl Pts',(-20.4837075622632,47.6096375922386,122.864217867557)) ;
#95221 = CARTESIAN_POINT('Ctrl Pts',(-20.5615908356297,47.6194929350616,123.056234985806)) ;
#95222 = CARTESIAN_POINT('Ctrl Pts',(-20.6058491720803,47.6294924144072,123.261705418283)) ;
#95223 = CARTESIAN_POINT('Ctrl Pts',(-20.6139152854521,47.6393868631625,123.469600680338)) ;
#95224 = CARTESIAN_POINT('Ctrl Pts',(-20.5852299915617,47.649449982597,123.679168585818)) ;
#95225 = CARTESIAN_POINT('Ctrl Pts',(-20.5222237825288,47.6592896278382,123.876236002791)) ;
#95226 = CARTESIAN_POINT('Ctrl Pts',(-20.4240386183092,47.6693527920243,124.063598482172)) ;
#95227 = CARTESIAN_POINT('Ctrl Pts',(-20.2968105105558,47.6792470617731,124.228190143397)) ;
#95228 = CARTESIAN_POINT('Ctrl Pts',(-20.1426174094489,47.689188787787,124.369245425586)) ;
#95229 = CARTESIAN_POINT('Ctrl Pts',(-19.9651875360064,47.6991916764463,124.482184157737)) ;
#95230 = CARTESIAN_POINT('Ctrl Pts',(-19.7700259465885,47.7092315252403,124.56251968231)) ;
#95231 = CARTESIAN_POINT('Ctrl Pts',(-19.5683733928146,47.7190557407012,124.607243544029)) ;
#95232 = CARTESIAN_POINT('Ctrl Pts',(-19.357178076069,47.7291125841947,124.616781601142)) ;
#95233 = CARTESIAN_POINT('Ctrl Pts',(-19.1502186587645,47.7390411935907,124.589576536288)) ;
#95234 = CARTESIAN_POINT('Ctrl Pts',(-18.9504848199683,47.7489930776286,124.527263965266)) ;
#95235 = CARTESIAN_POINT('Ctrl Pts',(-18.7629118733579,47.7590460304362,124.429914058781)) ;
#95236 = CARTESIAN_POINT('Ctrl Pts',(-18.598675250349,47.7688689069024,124.304701793222)) ;
#95237 = CARTESIAN_POINT('Ctrl Pts',(-18.4551028240335,47.7789246394725,124.149549502336)) ;
#95238 = CARTESIAN_POINT('Ctrl Pts',(-18.342258643216,47.7888654044602,123.973638763673)) ;
#95239 = CARTESIAN_POINT('Ctrl Pts',(-18.2613684522872,47.7987697373658,123.781768983543)) ;
#95240 = CARTESIAN_POINT('Ctrl Pts',(-18.2144911981369,47.8088164062465,123.575842264473)) ;
#95241 = CARTESIAN_POINT('Ctrl Pts',(-18.2040462151194,47.8187119695523,123.368035264035)) ;
#95242 = CARTESIAN_POINT('Ctrl Pts',(-18.2302679710938,47.8287740272526,123.158160931914)) ;
#95243 = CARTESIAN_POINT('Ctrl Pts',(-18.2910782452796,47.8386168048801,122.960347495842)) ;
#95244 = CARTESIAN_POINT('Ctrl Pts',(-18.3862593754307,47.848607283132,122.773151851679)) ;
#95245 = CARTESIAN_POINT('Ctrl Pts',(-18.5117691333417,47.8585362557755,122.606345574257)) ;
#95246 = CARTESIAN_POINT('Ctrl Pts',(-18.6650588022171,47.8685273926551,122.462742646535)) ;
#95247 = CARTESIAN_POINT('Ctrl Pts',(-18.8416404848203,47.878549510144,122.34779300154)) ;
#95248 = CARTESIAN_POINT('Ctrl Pts',(-19.0330683440688,47.8884500205462,122.266070940275)) ;
#95249 = CARTESIAN_POINT('Ctrl Pts',(-19.2375119458177,47.8984390132923,122.218087240548)) ;
#95250 = CARTESIAN_POINT('Ctrl Pts',(-19.4466836947895,47.9084042573429,122.206504347222)) ;
#95251 = CARTESIAN_POINT('Ctrl Pts',(-19.6534986182555,47.9183085218561,122.230779256276)) ;
#95252 = CARTESIAN_POINT('Ctrl Pts',(-19.8559842467169,47.9283666135544,122.291642961633)) ;
#95253 = CARTESIAN_POINT('Ctrl Pts',(-20.0410138775998,47.9382165539828,122.384646487928)) ;
#95254 = CARTESIAN_POINT('Ctrl Pts',(-20.2103684173728,47.9482435651563,122.510161007995)) ;
#95255 = CARTESIAN_POINT('Ctrl Pts',(-20.3549894294798,47.9582721517683,122.663586471316)) ;
#95256 = CARTESIAN_POINT('Ctrl Pts',(-20.4689725582954,47.968117365881,122.83633708969)) ;
#95257 = CARTESIAN_POINT('Ctrl Pts',(-20.5529671107311,47.9781081140606,123.028853175399)) ;
#95258 = CARTESIAN_POINT('Ctrl Pts',(-20.6020368114241,47.9881457476461,123.234091515211)) ;
#95259 = CARTESIAN_POINT('Ctrl Pts',(-20.6148256883295,47.9979910368589,123.440677297005)) ;
#95260 = CARTESIAN_POINT('Ctrl Pts',(-20.5916944344883,48.0079724376648,123.649222795437)) ;
#95261 = CARTESIAN_POINT('Ctrl Pts',(-20.5328217909652,48.0179246706548,123.850002480386)) ;
#95262 = CARTESIAN_POINT('Ctrl Pts',(-20.4397876959879,48.0279234821114,124.038518366483)) ;
#95263 = CARTESIAN_POINT('Ctrl Pts',(-20.314622836636,48.0379625860421,124.208436635421)) ;
#95264 = CARTESIAN_POINT('Ctrl Pts',(-20.1654041864277,48.0477875284614,124.351272569223)) ;
#95265 = CARTESIAN_POINT('Ctrl Pts',(-19.9898488473911,48.0578422159373,124.468988134481)) ;
#95266 = CARTESIAN_POINT('Ctrl Pts',(-19.7985107732397,48.0677850182941,124.553163168136)) ;
#95267 = CARTESIAN_POINT('Ctrl Pts',(-19.5964148826951,48.0776888142339,124.603261719813)) ;
#95268 = CARTESIAN_POINT('Ctrl Pts',(-19.3857035042312,48.0877355936089,124.617586751517)) ;
#95269 = CARTESIAN_POINT('Ctrl Pts',(-19.1787979589594,48.0976312519035,124.595621176739)) ;
#95270 = CARTESIAN_POINT('Ctrl Pts',(-18.9755413219689,48.1076928191541,124.537136972001)) ;
#95271 = CARTESIAN_POINT('Ctrl Pts',(-18.7895837292006,48.1175374635914,124.446269126648)) ;
#95272 = CARTESIAN_POINT('Ctrl Pts',(-18.6198326590471,48.1274975098341,124.323679639637)) ;
#95273 = CARTESIAN_POINT('Ctrl Pts',(-18.4731016928409,48.1375358058525,124.172014573816)) ;
#95274 = CARTESIAN_POINT('Ctrl Pts',(-18.3565226921379,48.1474091472708,124.000238839827)) ;
#95275 = CARTESIAN_POINT('Ctrl Pts',(-18.2699091481293,48.1574822510701,123.807037664057)) ;
#95276 = CARTESIAN_POINT('Ctrl Pts',(-18.2191835116695,48.167303066189,123.606859972749)) ;
#95277 = CARTESIAN_POINT('Ctrl Pts',(-18.2033538657066,48.177379931267,123.395643649504)) ;
#95278 = CARTESIAN_POINT('Ctrl Pts',(-18.2240803927477,48.1872446709223,123.189269101295)) ;
#95279 = CARTESIAN_POINT('Ctrl Pts',(-18.2806840855766,48.1972670741636,122.986320600377)) ;
#95280 = CARTESIAN_POINT('Ctrl Pts',(-18.3721813471877,48.2072927984521,122.796429449923)) ;
#95281 = CARTESIAN_POINT('Ctrl Pts',(-18.4928501478917,48.2171475814734,122.62803509953)) ;
#95282 = CARTESIAN_POINT('Ctrl Pts',(-18.6424187240408,48.2271264251967,122.480923759467)) ;
#95283 = CARTESIAN_POINT('Ctrl Pts',(-18.8161459824294,48.2371453174333,122.361848194698)) ;
#95284 = CARTESIAN_POINT('Ctrl Pts',(-19.0051677361826,48.2470285264743,122.275518633424)) ;
#95285 = CARTESIAN_POINT('Ctrl Pts',(-19.2100373124816,48.2570968358145,122.222445400665)) ;
#95286 = CARTESIAN_POINT('Ctrl Pts',(-19.4160689133427,48.2669269611472,122.205898319605)) ;
#95287 = CARTESIAN_POINT('Ctrl Pts',(-19.6267500453631,48.2769935135242,122.225565266307)) ;
#95288 = CARTESIAN_POINT('Ctrl Pts',(-19.8272641782343,48.2868837504179,122.280674195166)) ;
#95289 = CARTESIAN_POINT('Ctrl Pts',(-20.0172632691335,48.2968759752119,122.370249342106)) ;
#95290 = CARTESIAN_POINT('Ctrl Pts',(-20.1882096752109,48.3068385955629,122.49125875939)) ;
#95291 = CARTESIAN_POINT('Ctrl Pts',(-20.3350743761044,48.316743598326,122.638900187718)) ;
#95292 = CARTESIAN_POINT('Ctrl Pts',(-20.4557702033646,48.3268013607242,122.81249208294)) ;
#95293 = CARTESIAN_POINT('Ctrl Pts',(-20.5428321220069,48.336651880103,123.000408221936)) ;
#95294 = CARTESIAN_POINT('Ctrl Pts',(-20.5973595966834,48.3466834571011,123.204118610426)) ;
#95295 = CARTESIAN_POINT('Ctrl Pts',(-20.6152472704688,48.3566931922061,123.413816441878)) ;
#95296 = CARTESIAN_POINT('Ctrl Pts',(-20.5968276470534,48.3666027688323,123.621312622451)) ;
#95297 = CARTESIAN_POINT('Ctrl Pts',(-20.5430718873729,48.376530154689,123.822985193419)) ;
#95298 = CARTESIAN_POINT('Ctrl Pts',(-20.453926297321,48.3865750891793,124.014413092725)) ;
#95299 = CARTESIAN_POINT('Ctrl Pts',(-20.3349016235534,48.3964610213672,124.184803456692)) ;
#95300 = CARTESIAN_POINT('Ctrl Pts',(-20.1867787673531,48.4064543273203,124.33377573262)) ;
#95301 = CARTESIAN_POINT('Ctrl Pts',(-20.0158011743362,48.4163999651021,124.454128850865)) ;
#95302 = CARTESIAN_POINT('Ctrl Pts',(-19.826666064814,48.426347233448,124.543373150093)) ;
#95303 = CARTESIAN_POINT('Ctrl Pts',(-19.622820788123,48.4363951355851,124.598744953665)) ;
#95304 = CARTESIAN_POINT('Ctrl Pts',(-19.4166583633309,48.4462428304253,124.617674236662)) ;
#95305 = CARTESIAN_POINT('Ctrl Pts',(-19.2079107407179,48.4562043401698,124.600980623908)) ;
#95306 = CARTESIAN_POINT('Ctrl Pts',(-19.003906573456,48.4662337317786,124.547658872427)) ;
#95307 = CARTESIAN_POINT('Ctrl Pts',(-18.8145476533878,48.4761412273334,124.460899967926)) ;
#95308 = CARTESIAN_POINT('Ctrl Pts',(-18.6422518472801,48.4860866189964,124.342481581082)) ;
#95309 = CARTESIAN_POINT('Ctrl Pts',(-18.4921671420408,48.4960885365937,124.195169742631)) ;
#95310 = CARTESIAN_POINT('Ctrl Pts',(-18.3698192894223,48.5061286041459,124.023195675752)) ;
#95311 = CARTESIAN_POINT('Ctrl Pts',(-18.2806985353055,48.5159529155857,123.83685620093)) ;
#95312 = CARTESIAN_POINT('Ctrl Pts',(-18.22370774052,48.5260091567418,123.633290226062)) ;
#95313 = CARTESIAN_POINT('Ctrl Pts',(-18.2034272666168,48.5359400784775,123.425474826601)) ;
#95314 = CARTESIAN_POINT('Ctrl Pts',(-18.2191289100318,48.5458833145537,123.217054156125)) ;
#95315 = CARTESIAN_POINT('Ctrl Pts',(-18.2707969945288,48.5558645985662,123.013643980208)) ;
#95316 = CARTESIAN_POINT('Ctrl Pts',(-18.3578513136604,48.5659089001918,122.821289657151)) ;
#95317 = CARTESIAN_POINT('Ctrl Pts',(-18.4740534559425,48.5757369814113,122.650406895591)) ;
#95318 = CARTESIAN_POINT('Ctrl Pts',(-18.6216781740436,48.5858135842604,122.498533643899)) ;
#95319 = CARTESIAN_POINT('Ctrl Pts',(-18.7896140709014,48.595665663379,122.377226252278)) ;
#95320 = CARTESIAN_POINT('Ctrl Pts',(-18.9800970249153,48.6057389216879,122.284765876167)) ;
#95321 = CARTESIAN_POINT('Ctrl Pts',(-19.1791159034556,48.6155803810682,122.228160560992)) ;
#95322 = CARTESIAN_POINT('Ctrl Pts',(-19.3873388361497,48.6255414764805,122.205934289696)) ;
#95323 = CARTESIAN_POINT('Ctrl Pts',(-19.5978306492619,48.6355787608773,122.220722308273)) ;
#95324 = CARTESIAN_POINT('Ctrl Pts',(-19.799388463471,48.6454550996125,122.270668660089)) ;
#95325 = CARTESIAN_POINT('Ctrl Pts',(-19.9927541999136,48.6555172257658,122.356380829401)) ;
#95326 = CARTESIAN_POINT('Ctrl Pts',(-20.1649868946281,48.6653853997423,122.472078082189)) ;
#95327 = CARTESIAN_POINT('Ctrl Pts',(-20.3168522676943,48.6753909482461,122.617582443954)) ;
#95328 = CARTESIAN_POINT('Ctrl Pts',(-20.4408428213035,48.6853735801417,122.786952855138)) ;
#95329 = CARTESIAN_POINT('Ctrl Pts',(-20.533889105216,48.6954175225635,122.976482672642)) ;
#95330 = CARTESIAN_POINT('Ctrl Pts',(-20.5916223940478,48.7052456705907,123.17487095886)) ;
#95331 = CARTESIAN_POINT('Ctrl Pts',(-20.6150709599507,48.7152355379651,123.383577027473)) ;
#95332 = CARTESIAN_POINT('Ctrl Pts',(-20.6013063806438,48.7252792769206,123.59427890037)) ;
#95333 = CARTESIAN_POINT('Ctrl Pts',(-20.5526930860455,48.7351010254585,123.794957259906)) ;
#95334 = CARTESIAN_POINT('Ctrl Pts',(-20.4686518829864,48.7451360030682,123.988462035549)) ;
#95335 = CARTESIAN_POINT('Ctrl Pts',(-20.3519125818634,48.7551609158259,124.163938838263)) ;
#95336 = CARTESIAN_POINT('Ctrl Pts',(-20.2093168668015,48.7650128589198,124.314159551624)) ;
#95337 = CARTESIAN_POINT('Ctrl Pts',(-20.0406693441658,48.7750038202489,124.439317914556)) ;
#95338 = CARTESIAN_POINT('Ctrl Pts',(-19.8542415899893,48.7849216951173,124.532750810719)) ;
#95339 = CARTESIAN_POINT('Ctrl Pts',(-19.6522481455534,48.7949502141185,124.593089434004)) ;
#95340 = CARTESIAN_POINT('Ctrl Pts',(-19.4458572034312,48.8048338929164,124.617196619224)) ;
#95341 = CARTESIAN_POINT('Ctrl Pts',(-19.2360620949914,48.8148288363561,124.605427829413)) ;
#95342 = CARTESIAN_POINT('Ctrl Pts',(-19.0309256562001,48.8248556901785,124.556904561977)) ;
#95343 = CARTESIAN_POINT('Ctrl Pts',(-18.8399656537912,48.8347398545175,124.474946592607)) ;
#95344 = CARTESIAN_POINT('Ctrl Pts',(-18.6641807496761,48.8447279525599,124.360128704613)) ;
#95345 = CARTESIAN_POINT('Ctrl Pts',(-18.5114556876915,48.8546790590169,124.217117736097)) ;
#95346 = CARTESIAN_POINT('Ctrl Pts',(-18.3848137965873,48.864724110185,124.048141101483)) ;
#95347 = CARTESIAN_POINT('Ctrl Pts',(-18.2910674776391,48.8745858705433,123.863220172721)) ;
#95348 = CARTESIAN_POINT('Ctrl Pts',(-18.2296182843222,48.8845486873738,123.662986258613)) ;
#95349 = CARTESIAN_POINT('Ctrl Pts',(-18.2040446117708,48.8945833686545,123.453590801485)) ;
#95350 = CARTESIAN_POINT('Ctrl Pts',(-18.2146977108724,48.9044683984353,123.246021045986)) ;
#95351 = CARTESIAN_POINT('Ctrl Pts',(-18.262112613018,48.9145339918333,123.039825965983)) ;
#95352 = CARTESIAN_POINT('Ctrl Pts',(-18.3425873201439,48.9243731601948,122.849236792747)) ;
#95353 = CARTESIAN_POINT('Ctrl Pts',(-18.4572075848471,48.9344357579363,122.671461421509)) ;
#95354 = CARTESIAN_POINT('Ctrl Pts',(-18.5987775296174,48.9443327703432,122.518966631599)) ;
#95355 = CARTESIAN_POINT('Ctrl Pts',(-18.7648162089244,48.9542640921688,122.392390623785)) ;
#95356 = CARTESIAN_POINT('Ctrl Pts',(-18.9524800333232,48.9643058549233,122.295703965336)) ;
#95357 = CARTESIAN_POINT('Ctrl Pts',(-19.1509683135226,48.974194053814,122.233882218668)) ;
#95358 = CARTESIAN_POINT('Ctrl Pts',(-19.3593098514268,48.9841879924139,122.206854423194)) ;
#95359 = CARTESIAN_POINT('Ctrl Pts',(-19.5680935855374,48.9941288134508,122.216376408398)) ;
#95360 = CARTESIAN_POINT('Ctrl Pts',(-19.7724671471724,49.004088195739,122.261825265473)) ;
#95361 = CARTESIAN_POINT('Ctrl Pts',(-19.9666684295254,49.0140859553913,122.342274294019)) ;
#95362 = CARTESIAN_POINT('Ctrl Pts',(-20.1444533832178,49.0241220915936,122.455885746671)) ;
#95363 = CARTESIAN_POINT('Ctrl Pts',(-20.2971096778046,49.0339728890845,122.595827077443)) ;
#95364 = CARTESIAN_POINT('Ctrl Pts',(-20.42504775658,49.0439337541608,122.761600423317)) ;
#95365 = CARTESIAN_POINT('Ctrl Pts',(-20.5227053078636,49.0539626217912,122.948471675384)) ;
#95366 = CARTESIAN_POINT('Ctrl Pts',(-20.5857337929231,49.0638728579276,123.14704453)) ;
#95367 = CARTESIAN_POINT('Ctrl Pts',(-20.6139392672823,49.0738078112422,123.354001305858)) ;
#95368 = CARTESIAN_POINT('Ctrl Pts',(-20.6055025787485,49.0838487416517,123.564919624935)) ;
#95369 = CARTESIAN_POINT('Ctrl Pts',(-20.5613836179293,49.0937366384333,123.768066917084)) ;
#95370 = CARTESIAN_POINT('Ctrl Pts',(-20.4822199689316,49.103726090092,123.962579586994)) ;
#95371 = CARTESIAN_POINT('Ctrl Pts',(-20.37068363497,49.1136851804574,124.139761405237)) ;
#95372 = CARTESIAN_POINT('Ctrl Pts',(-20.2313302399948,49.1235824927637,124.294294621323)) ;
#95373 = CARTESIAN_POINT('Ctrl Pts',(-20.0645865405684,49.133638918664,124.424243371079)) ;
#95374 = CARTESIAN_POINT('Ctrl Pts',(-19.8812921014099,49.1435089212537,124.521540995851)) ;
#95375 = CARTESIAN_POINT('Ctrl Pts',(-19.6813785176454,49.1535128544309,124.586788980192)) ;
#95376 = CARTESIAN_POINT('Ctrl Pts',(-19.4734493318863,49.1635001148948,124.616182759415)) ;
#95377 = CARTESIAN_POINT('Ctrl Pts',(-19.2627909630447,49.1735271664805,124.608876433313)) ;
#95378 = CARTESIAN_POINT('Ctrl Pts',(-19.0593248865046,49.1834182563066,124.565892059156)) ;
#95379 = CARTESIAN_POINT('Ctrl Pts',(-18.7998848677317,49.1967160110877,124.461822865144)) ;
#95380 = CARTESIAN_POINT('Ctrl Pts',(-18.5749110821987,49.2099140706958,124.293969457088)) ;
#95381 = CARTESIAN_POINT('Ctrl Pts',(-18.4005901022622,49.223310811265,124.072839397159)) ;
#95382 = CARTESIAN_POINT('Ctrl Pts',(-18.3021399164489,49.2331817233385,123.890105683798)) ;
#95383 = CARTESIAN_POINT('Ctrl Pts',(-18.2356163002858,49.2432552851066,123.689098892024)) ;
#95384 = CARTESIAN_POINT('Ctrl Pts',(-18.205508606502,49.2530766976949,123.484778341202)) ;
#95385 = CARTESIAN_POINT('Ctrl Pts',(-18.2112828047954,49.263150714926,123.273123359953)) ;
#95386 = CARTESIAN_POINT('Ctrl Pts',(-18.2665396821944,49.2763095018905,123.001992383128)) ;
#95387 = CARTESIAN_POINT('Ctrl Pts',(-18.3927903994223,49.2896756049847,122.747437406837)) ;
#95388 = CARTESIAN_POINT('Ctrl Pts',(-18.5783673105112,49.3029895398738,122.537851115961)) ;
#95389 = CARTESIAN_POINT('Ctrl Pts',(-18.7409926730701,49.3128895793212,122.40799514289)) ;
#95390 = CARTESIAN_POINT('Ctrl Pts',(-18.9247420206413,49.3228539824558,122.307378307647)) ;
#95391 = CARTESIAN_POINT('Ctrl Pts',(-19.1245308077183,49.3328839495769,122.239933879474)) ;
#95392 = CARTESIAN_POINT('Ctrl Pts',(-19.3303117943017,49.342786226186,122.208520853184)) ;
#95393 = CARTESIAN_POINT('Ctrl Pts',(-19.6091930994025,49.3560521553551,122.214236467048)) ;
#95394 = CARTESIAN_POINT('Ctrl Pts',(-19.9485296513228,49.3726736864615,122.312721965115)) ;
#95395 = CARTESIAN_POINT('Ctrl Pts',(-20.2902094521447,49.3925485151062,122.561479447863)) ;
#95396 = CARTESIAN_POINT('Ctrl Pts',(-20.4884697082381,49.4092217232081,122.855392698885)) ;
#95397 = CARTESIAN_POINT('Ctrl Pts',(-20.578996749337,49.4224728481893,123.118823560105)) ;
#95398 = CARTESIAN_POINT('Ctrl Pts',(-20.6234021124794,49.4357151670102,123.393723305564)) ;
#95399 = CARTESIAN_POINT('Ctrl Pts',(-20.5867774458657,49.4524484073496,123.747548085192)) ;
#95400 = CARTESIAN_POINT('Ctrl Pts',(-20.4028092707548,49.4722775555376,124.127010849328)) ;
#95401 = CARTESIAN_POINT('Ctrl Pts',(-20.0997798393814,49.4922022506382,124.422943948998)) ;
#95402 = CARTESIAN_POINT('Ctrl Pts',(-19.7138202488184,49.5121254792217,124.597719634898)) ;
#95403 = CARTESIAN_POINT('Ctrl Pts',(-19.2914296044062,49.5320526183478,124.630422657138)) ;
#95404 = CARTESIAN_POINT('Ctrl Pts',(-18.8840519429806,49.5519290809634,124.517817506517)) ;
#95405 = CARTESIAN_POINT('Ctrl Pts',(-18.5377035770347,49.5719063095687,124.27191546715)) ;
#95406 = CARTESIAN_POINT('Ctrl Pts',(-18.2968244731111,49.5918411675424,123.923098218903)) ;
#95407 = CARTESIAN_POINT('Ctrl Pts',(-18.1892441438947,49.6117376164732,123.513986113187)) ;
#95408 = CARTESIAN_POINT('Ctrl Pts',(-18.2273108370955,49.6316589005398,123.092101257408)) ;
#95409 = CARTESIAN_POINT('Ctrl Pts',(-18.4075016177291,49.6516155502108,122.707903558998)) ;
#95410 = CARTESIAN_POINT('Ctrl Pts',(-18.7066393674634,49.6714928433224,122.409408052842)) ;
#95411 = CARTESIAN_POINT('Ctrl Pts',(-19.0894747831973,49.6913793155508,122.229768574258)) ;
#95412 = CARTESIAN_POINT('Ctrl Pts',(-19.5143647801207,49.7114408814748,122.191861124704)) ;
#95413 = CARTESIAN_POINT('Ctrl Pts',(-19.9220057904957,49.7312812890156,122.300397275708)) ;
#95414 = CARTESIAN_POINT('Ctrl Pts',(-20.2693648000579,49.7511326129885,122.54022502922)) ;
#95415 = CARTESIAN_POINT('Ctrl Pts',(-20.5159525925647,49.77118588294,122.888006985456)) ;
#95416 = CARTESIAN_POINT('Ctrl Pts',(-20.6278796892875,49.7910065403233,123.294433975262)) ;
#95417 = CARTESIAN_POINT('Ctrl Pts',(-20.5948465336614,49.8109779616538,123.717653699581)) ;
#95418 = CARTESIAN_POINT('Ctrl Pts',(-20.4200331926624,49.8308714540175,124.102995975401)) ;
#95419 = CARTESIAN_POINT('Ctrl Pts',(-20.1222394105841,49.8508955402586,124.407164838694)) ;
#95420 = CARTESIAN_POINT('Ctrl Pts',(-19.7427027808656,49.8707004193714,124.589700995949)) ;
#95421 = CARTESIAN_POINT('Ctrl Pts',(-19.320572120998,49.8906594350693,124.633229800858)) ;
#95422 = CARTESIAN_POINT('Ctrl Pts',(-18.9086034132619,49.9106454586984,124.528993193034)) ;
#95423 = CARTESIAN_POINT('Ctrl Pts',(-18.5595577529917,49.9304539544589,124.293209163247)) ;
#95424 = CARTESIAN_POINT('Ctrl Pts',(-18.3093968681947,49.9504365935644,123.949887426195)) ;
#95425 = CARTESIAN_POINT('Ctrl Pts',(-18.1920567335,49.9703180413585,123.543654787052)) ;
#95426 = CARTESIAN_POINT('Ctrl Pts',(-18.2201436686759,49.990274508096,123.120348075344)) ;
#95427 = CARTESIAN_POINT('Ctrl Pts',(-18.3901206018369,50.0101519050516,122.733311854213)) ;
#95428 = CARTESIAN_POINT('Ctrl Pts',(-18.6832551201811,50.0301338512269,122.42582166897)) ;
#95429 = CARTESIAN_POINT('Ctrl Pts',(-19.0629301007364,50.0500629502636,122.23745376237)) ;
#95430 = CARTESIAN_POINT('Ctrl Pts',(-19.4839074729106,50.0699915734762,122.189906489592)) ;
#95431 = CARTESIAN_POINT('Ctrl Pts',(-19.894198197734,50.0898258975826,122.287670868876)) ;
#95432 = CARTESIAN_POINT('Ctrl Pts',(-20.1900712867489,50.106478184966,122.481987249183)) ;
#95433 = CARTESIAN_POINT('Ctrl Pts',(-20.3755131098878,50.1197386859883,122.690239071981)) ;
#95434 = CARTESIAN_POINT('Ctrl Pts',(-20.4862810538597,50.1297401631895,122.868949284785)) ;
#95435 = CARTESIAN_POINT('Ctrl Pts',(-20.5642531899787,50.139772184049,123.064919168219)) ;
#95436 = CARTESIAN_POINT('Ctrl Pts',(-20.6065416958673,50.1496357277746,123.267915697888)) ;
#95437 = CARTESIAN_POINT('Ctrl Pts',(-20.6135616640685,50.1596044414447,123.47738464972)) ;
#95438 = CARTESIAN_POINT('Ctrl Pts',(-20.5737479830051,50.1729501888484,123.755049879261)) ;
#95439 = CARTESIAN_POINT('Ctrl Pts',(-20.4644112620115,50.1861007439211,124.012460485703)) ;
#95440 = CARTESIAN_POINT('Ctrl Pts',(-20.2913079986546,50.199486124471,124.234313522455)) ;
#95441 = CARTESIAN_POINT('Ctrl Pts',(-20.1368976756591,50.2093740604638,124.373521069684)) ;
#95442 = CARTESIAN_POINT('Ctrl Pts',(-19.9590515319526,50.2193652502764,124.485228994249)) ;
#95443 = CARTESIAN_POINT('Ctrl Pts',(-19.7652513682256,50.2293173488147,124.564155979897)) ;
#95444 = CARTESIAN_POINT('Ctrl Pts',(-19.5587718065409,50.2393636052652,124.608506614691)) ;
#95445 = CARTESIAN_POINT('Ctrl Pts',(-19.3518493726821,50.2492130526593,124.616330380142)) ;
#95446 = CARTESIAN_POINT('Ctrl Pts',(-19.1442754869309,50.2591757051545,124.588436789505)) ;
#95447 = CARTESIAN_POINT('Ctrl Pts',(-18.9435668464815,50.2691987907966,124.524268865294)) ;
#95448 = CARTESIAN_POINT('Ctrl Pts',(-18.7587399819941,50.2791239065536,124.42738459836)) ;
#95449 = CARTESIAN_POINT('Ctrl Pts',(-18.5915092032389,50.2891763849534,124.298203175833)) ;
#95450 = CARTESIAN_POINT('Ctrl Pts',(-18.4519664352218,50.2990278836561,124.145139239257)) ;
#95451 = CARTESIAN_POINT('Ctrl Pts',(-18.3393284129575,50.3089996228586,123.968364344044)) ;
#95452 = CARTESIAN_POINT('Ctrl Pts',(-18.2589073101998,50.3189948306243,123.774195195946)) ;
#95453 = CARTESIAN_POINT('Ctrl Pts',(-18.2135079750364,50.3290288320934,123.568211118818)) ;
#95454 = CARTESIAN_POINT('Ctrl Pts',(-18.2043916892367,50.3388841901857,123.36120035134)) ;
#95455 = CARTESIAN_POINT('Ctrl Pts',(-18.2314639911044,50.348883665779,123.152768244065)) ;
#95456 = CARTESIAN_POINT('Ctrl Pts',(-18.2934523168804,50.3587781142741,122.95416575342)) ;
#95457 = CARTESIAN_POINT('Ctrl Pts',(-18.3906320141663,50.3688412385019,122.766288908924)) ;
#95458 = CARTESIAN_POINT('Ctrl Pts',(-18.5159679597529,50.3786808648305,122.601680134446)) ;
#95459 = CARTESIAN_POINT('Ctrl Pts',(-18.6712068113223,50.3887440998734,122.457990482356)) ;
#95460 = CARTESIAN_POINT('Ctrl Pts',(-18.8461841750949,50.3986381051075,122.345485237456)) ;
#95461 = CARTESIAN_POINT('Ctrl Pts',(-19.0387184829255,50.4085808183232,122.264163922882)) ;
#95462 = CARTESIAN_POINT('Ctrl Pts',(-19.2437750914236,50.4185865581214,122.217162068249)) ;
#95463 = CARTESIAN_POINT('Ctrl Pts',(-19.4541815050549,50.4286074602678,122.20670110388)) ;
#95464 = CARTESIAN_POINT('Ctrl Pts',(-19.6605343168355,50.4384982303167,122.232355979485)) ;
#95465 = CARTESIAN_POINT('Ctrl Pts',(-19.8613998056627,50.4484896410964,122.293768559807)) ;
#95466 = CARTESIAN_POINT('Ctrl Pts',(-20.0477153883951,50.4584379867609,122.388776883293)) ;
#95467 = CARTESIAN_POINT('Ctrl Pts',(-20.2149291845068,50.4683828448221,122.514309607201)) ;
#95468 = CARTESIAN_POINT('Ctrl Pts',(-20.3591331096358,50.478437680215,122.668841765407)) ;
#95469 = CARTESIAN_POINT('Ctrl Pts',(-20.4719728917269,50.4882600523165,122.841803140507)) ;
#95470 = CARTESIAN_POINT('Ctrl Pts',(-20.5553314025535,50.4983159197602,123.036064306596)) ;
#95471 = CARTESIAN_POINT('Ctrl Pts',(-20.6027823192923,50.5082566496181,123.239599688952)) ;
#95472 = CARTESIAN_POINT('Ctrl Pts',(-20.6147815729713,50.5181609881693,123.447477704609)) ;
#95473 = CARTESIAN_POINT('Ctrl Pts',(-20.5900240766022,50.5282076695977,123.657216644109)) ;
#95474 = CARTESIAN_POINT('Ctrl Pts',(-20.5303079538465,50.538103177067,123.856531744031)) ;
#95475 = CARTESIAN_POINT('Ctrl Pts',(-20.4353433398059,50.5481654455656,124.045523747245)) ;
#95476 = CARTESIAN_POINT('Ctrl Pts',(-20.3118410018698,50.5580074358362,124.211563922258)) ;
#95477 = CARTESIAN_POINT('Ctrl Pts',(-20.1594362473347,50.5680008527172,124.356126655464)) ;
#95478 = CARTESIAN_POINT('Ctrl Pts',(-19.9854190359377,50.5779253405694,124.471276809316)) ;
#95479 = CARTESIAN_POINT('Ctrl Pts',(-19.7927265255418,50.5879249744778,124.555279974465)) ;
#95480 = CARTESIAN_POINT('Ctrl Pts',(-19.588605893336,50.5979110847346,124.604501080592)) ;
#95481 = CARTESIAN_POINT('Ctrl Pts',(-19.3780314652536,50.6079470359217,124.61737350002)) ;
#95482 = CARTESIAN_POINT('Ctrl Pts',(-19.1720910958803,50.6178036742565,124.594220180838)) ;
#95483 = CARTESIAN_POINT('Ctrl Pts',(-18.9704025586501,50.6278026343345,124.535105154761)) ;
#95484 = CARTESIAN_POINT('Ctrl Pts',(-18.7838328447076,50.6376978646483,124.443006602214)) ;
#95485 = CARTESIAN_POINT('Ctrl Pts',(-18.6133502503988,50.647758377117,124.317874570504)) ;
#95486 = CARTESIAN_POINT('Ctrl Pts',(-18.4701391673336,50.6576076686631,124.168301047964)) ;
#95487 = CARTESIAN_POINT('Ctrl Pts',(-18.3525641925228,50.6676348545953,123.993338588389)) ;
#95488 = CARTESIAN_POINT('Ctrl Pts',(-18.2676431887012,50.6776633910547,123.800354530484)) ;
#95489 = CARTESIAN_POINT('Ctrl Pts',(-18.2180604076789,50.6875086310196,123.599415304129)) ;
#95490 = CARTESIAN_POINT('Ctrl Pts',(-18.2033518853956,50.6974993259428,123.38988994928)) ;
#95491 = CARTESIAN_POINT('Ctrl Pts',(-18.2258151174764,50.7075371467014,123.180062975056)) ;
#95492 = CARTESIAN_POINT('Ctrl Pts',(-18.2829055830036,50.7173817404784,122.981124546184)) ;
#95493 = CARTESIAN_POINT('Ctrl Pts',(-18.374543817564,50.7273657358544,122.792311148238)) ;
#95494 = CARTESIAN_POINT('Ctrl Pts',(-18.4971789128897,50.7373147844158,122.622862427556)) ;
#95495 = CARTESIAN_POINT('Ctrl Pts',(-18.6480196024587,50.7473172233904,122.476338505738)) ;
#95496 = CARTESIAN_POINT('Ctrl Pts',(-18.8224928562283,50.7573384646867,122.358249526149)) ;
#95497 = CARTESIAN_POINT('Ctrl Pts',(-19.012249182242,50.7672311431262,122.273123776154)) ;
#95498 = CARTESIAN_POINT('Ctrl Pts',(-19.2158038174537,50.7772211970739,122.221412222857)) ;
#95499 = CARTESIAN_POINT('Ctrl Pts',(-19.4245865506918,50.7871795582223,122.206028609236)) ;
#95500 = CARTESIAN_POINT('Ctrl Pts',(-19.6317117481237,50.7970791851072,122.226497823876)) ;
#95501 = CARTESIAN_POINT('Ctrl Pts',(-19.8350849358326,50.8071270819105,122.283522980139)) ;
#95502 = CARTESIAN_POINT('Ctrl Pts',(-20.0226963525784,50.8170224395465,122.37348142898)) ;
#95503 = CARTESIAN_POINT('Ctrl Pts',(-20.1946528136683,50.8270840920032,122.496627869575)) ;
#95504 = CARTESIAN_POINT('Ctrl Pts',(-20.339466545417,50.8369286962752,122.644499598143)) ;
#95505 = CARTESIAN_POINT('Ctrl Pts',(-20.4583900882012,50.8468888179732,122.816839654232)) ;
#95506 = CARTESIAN_POINT('Ctrl Pts',(-20.545892012549,50.8569268523357,123.008866414043)) ;
#95507 = CARTESIAN_POINT('Ctrl Pts',(-20.5982377476504,50.8668011649221,123.209773634667)) ;
#95508 = CARTESIAN_POINT('Ctrl Pts',(-20.6152194208443,50.8768706457048,123.420755060105)) ;
#95509 = CARTESIAN_POINT('Ctrl Pts',(-20.5958818093624,50.8867049817219,123.626614527352)) ;
#95510 = CARTESIAN_POINT('Ctrl Pts',(-20.5405510103418,50.8967379394501,123.830145656788)) ;
#95511 = CARTESIAN_POINT('Ctrl Pts',(-20.4503035287167,50.9067583380253,124.020498784439)) ;
#95512 = CARTESIAN_POINT('Ctrl Pts',(-20.330679811375,50.9166239117966,124.189949451206)) ;
#95513 = CARTESIAN_POINT('Ctrl Pts',(-20.1804458547993,50.9266927864526,124.339042768337)) ;
#95514 = CARTESIAN_POINT('Ctrl Pts',(-20.0104561974406,50.9365382173581,124.457150451308)) ;
#95515 = CARTESIAN_POINT('Ctrl Pts',(-19.8202798254585,50.9465178422288,124.545737839869)) ;
#95516 = CARTESIAN_POINT('Ctrl Pts',(-19.6167140496344,50.9565365251429,124.599784856543)) ;
#95517 = CARTESIAN_POINT('Ctrl Pts',(-19.4096995592073,50.9664197903268,124.617864751239)) ;
#95518 = CARTESIAN_POINT('Ctrl Pts',(-19.1988827726302,50.9764880844181,124.599299468508)) ;
#95519 = CARTESIAN_POINT('Ctrl Pts',(-18.9991976287175,50.9863182146035,124.545926791371)) ;
#95520 = CARTESIAN_POINT('Ctrl Pts',(-18.8072531202101,50.9963847628186,124.456872704251)) ;
#95521 = CARTESIAN_POINT('Ctrl Pts',(-18.6367526545896,51.0062750115072,124.337824122225)) ;
#95522 = CARTESIAN_POINT('Ctrl Pts',(-18.4876977017262,51.0162671932833,124.189818410515)) ;
#95523 = CARTESIAN_POINT('Ctrl Pts',(-18.367117992186,51.0262299739111,124.018565039215)) ;
#95524 = CARTESIAN_POINT('Ctrl Pts',(-18.2781469080694,51.0361343785848,123.830292810274)) ;
#95525 = CARTESIAN_POINT('Ctrl Pts',(-18.2225158456398,51.0461943730639,123.626267208626)) ;
#95526 = CARTESIAN_POINT('Ctrl Pts',(-18.2033820490551,51.0560429950336,123.420089240958)) ;
#95527 = CARTESIAN_POINT('Ctrl Pts',(-18.2201764733819,51.0660734344455,123.209899736072)) ;
#95528 = CARTESIAN_POINT('Ctrl Pts',(-18.2735217754488,51.0760831500802,123.006313725019)) ;
#95529 = CARTESIAN_POINT('Ctrl Pts',(-18.3603349820453,51.0859939027728,122.816927523553)) ;
#95530 = CARTESIAN_POINT('Ctrl Pts',(-18.4785193177454,51.0959231757192,122.64484961303)) ;
#95531 = CARTESIAN_POINT('Ctrl Pts',(-18.6265724883276,51.1059658671119,122.494343330129)) ;
#95532 = CARTESIAN_POINT('Ctrl Pts',(-18.795773334273,51.1158524003294,122.373613121916)) ;
#95533 = CARTESIAN_POINT('Ctrl Pts',(-18.9852153228182,51.1258455452615,122.282818780092)) ;
#95534 = CARTESIAN_POINT('Ctrl Pts',(-19.1866163420278,51.1357912260979,122.226639317315)) ;
#95535 = CARTESIAN_POINT('Ctrl Pts',(-19.3947136728631,51.1457384832465,122.20585296853)) ;
#95536 = CARTESIAN_POINT('Ctrl Pts',(-19.6053345284675,51.1557863871185,122.221908805865)) ;
#95537 = CARTESIAN_POINT('Ctrl Pts',(-19.8059404785661,51.1656340862164,122.273080716496)) ;
#95538 = CARTESIAN_POINT('Ctrl Pts',(-19.9970578886728,51.1755955771951,122.358685495831)) ;
#95539 = CARTESIAN_POINT('Ctrl Pts',(-20.1714467400249,51.1856250396091,122.477219151317)) ;
#95540 = CARTESIAN_POINT('Ctrl Pts',(-20.3208357163494,51.195532270709,122.62235336646)) ;
#95541 = CARTESIAN_POINT('Ctrl Pts',(-20.4435745138722,51.2054786493864,122.79162964494)) ;
#95542 = CARTESIAN_POINT('Ctrl Pts',(-20.5356748345117,51.2154834181952,122.980744956243)) ;
#95543 = CARTESIAN_POINT('Ctrl Pts',(-20.5933963625538,51.2255045392154,123.183354735425)) ;
#95544 = CARTESIAN_POINT('Ctrl Pts',(-20.6150184498712,51.2353954050681,123.39017151081)) ;
#95545 = CARTESIAN_POINT('Ctrl Pts',(-20.600564956353,51.2453862138273,123.599699814294)) ;
#95546 = CARTESIAN_POINT('Ctrl Pts',(-20.5501095068394,51.2553368720076,123.802728469495)) ;
#95547 = CARTESIAN_POINT('Ctrl Pts',(-20.4655583890161,51.2652730816497,123.993724128868)) ;
#95548 = CARTESIAN_POINT('Ctrl Pts',(-20.3487803717502,51.2752562483746,124.168144460775)) ;
#95549 = CARTESIAN_POINT('Ctrl Pts',(-20.2023615012466,51.285300045585,124.320252177703)) ;
#95550 = CARTESIAN_POINT('Ctrl Pts',(-20.0356625745698,51.2951282617532,124.44238355308)) ;
#95551 = CARTESIAN_POINT('Ctrl Pts',(-19.8457170438004,51.3052048292224,124.536080296056)) ;
#95552 = CARTESIAN_POINT('Ctrl Pts',(-19.6468633806885,51.3150569149118,124.594176632678)) ;
#95553 = CARTESIAN_POINT('Ctrl Pts',(-19.4364191272755,51.3251301823172,124.617542350763)) ;
#95554 = CARTESIAN_POINT('Ctrl Pts',(-19.2299340341238,51.3349715987408,124.604264987046)) ;
#95555 = CARTESIAN_POINT('Ctrl Pts',(-19.0262804267523,51.3449328568836,124.55550789222)) ;
#95556 = CARTESIAN_POINT('Ctrl Pts',(-18.8328905252114,51.3549695333155,124.471123425444)) ;
#95557 = CARTESIAN_POINT('Ctrl Pts',(-18.6596436743911,51.3648481411793,124.35655766273)) ;
#95558 = CARTESIAN_POINT('Ctrl Pts',(-18.5061529523948,51.3749083698181,124.211091751246)) ;
#95559 = CARTESIAN_POINT('Ctrl Pts',(-18.3825894276694,51.3847753539789,124.044441773673)) ;
#95560 = CARTESIAN_POINT('Ctrl Pts',(-18.288197267175,51.3947809202316,123.856492625025)) ;
#95561 = CARTESIAN_POINT('Ctrl Pts',(-18.2280368488677,51.4047647086462,123.655369961215)) ;
#95562 = CARTESIAN_POINT('Ctrl Pts',(-18.2037955447711,51.4148105654489,123.445587221076)) ;
#95563 = CARTESIAN_POINT('Ctrl Pts',(-18.2158049400224,51.4246364426648,123.239365717477)) ;
#95564 = CARTESIAN_POINT('Ctrl Pts',(-18.2635681718687,51.4346269185061,123.034837448249)) ;
#95565 = CARTESIAN_POINT('Ctrl Pts',(-18.3470677335809,51.4446704944049,122.840901106001)) ;
#95566 = CARTESIAN_POINT('Ctrl Pts',(-18.4600500292513,51.454492286703,122.668070699184)) ;
#95567 = CARTESIAN_POINT('Ctrl Pts',(-18.6040154233207,51.4645272523288,122.51386005426)) ;
#95568 = CARTESIAN_POINT('Ctrl Pts',(-18.7727580993655,51.4745521692619,122.387582243707)) ;
#95569 = CARTESIAN_POINT('Ctrl Pts',(-18.9574116237924,51.484404107638,122.293758448253)) ;
#95570 = CARTESIAN_POINT('Ctrl Pts',(-19.1582249069468,51.4943950836628,122.232272282288)) ;
#95571 = CARTESIAN_POINT('Ctrl Pts',(-19.365173365588,51.5043129044664,122.20663047978)) ;
#95572 = CARTESIAN_POINT('Ctrl Pts',(-19.5757113223788,51.514341625031,122.217393834986)) ;
#95573 = CARTESIAN_POINT('Ctrl Pts',(-19.7782673487064,51.5242245516402,122.263734531426)) ;
#95574 = CARTESIAN_POINT('Ctrl Pts',(-19.9721412615777,51.5342288367597,122.34520873911)) ;
#95575 = CARTESIAN_POINT('Ctrl Pts',(-20.1485965785602,51.5442125179675,122.458925892081)) ;
#95576 = CARTESIAN_POINT('Ctrl Pts',(-20.3033084560046,51.5542535166975,122.602515950188)) ;
#95577 = CARTESIAN_POINT('Ctrl Pts',(-20.4283341927033,51.5640859615646,122.767130736313)) ;
#95578 = CARTESIAN_POINT('Ctrl Pts',(-20.5249880222564,51.5740809599949,122.953701578692)) ;
#95579 = CARTESIAN_POINT('Ctrl Pts',(-20.5875824486003,51.5841125087445,123.155104791441)) ;
#95580 = CARTESIAN_POINT('Ctrl Pts',(-20.6140701868961,51.59397788705,123.360796238698)) ;
#95581 = CARTESIAN_POINT('Ctrl Pts',(-20.6049369881444,51.6039397345103,123.570032779427)) ;
#95582 = CARTESIAN_POINT('Ctrl Pts',(-20.5589475424587,51.6139746753246,123.775913423477)) ;
#95583 = CARTESIAN_POINT('Ctrl Pts',(-20.4794278297561,51.6238596363417,123.96794213985)) ;
#95584 = CARTESIAN_POINT('Ctrl Pts',(-20.3657283834297,51.6339252452606,124.146371557226)) ;
#95585 = CARTESIAN_POINT('Ctrl Pts',(-20.2260994109044,51.6437644203022,124.299028749051)) ;
#95586 = CARTESIAN_POINT('Ctrl Pts',(-20.0585850388737,51.6538269758022,124.428181896307)) ;
#95587 = CARTESIAN_POINT('Ctrl Pts',(-19.8741335395331,51.6637241504951,124.524491581243)) ;
#95588 = CARTESIAN_POINT('Ctrl Pts',(-19.6753166265995,51.6736548654184,124.588188265683)) ;
#95589 = CARTESIAN_POINT('Ctrl Pts',(-19.4660674185624,51.683698893496,124.616477182508)) ;
#95590 = CARTESIAN_POINT('Ctrl Pts',(-19.2583751492451,51.6935850953493,124.60829874282)) ;
#95591 = CARTESIAN_POINT('Ctrl Pts',(-19.0530285341832,51.7035782618161,124.56402336225)) ;
#95592 = CARTESIAN_POINT('Ctrl Pts',(-18.8594658749353,51.7135177328034,124.485230506411)) ;
#95593 = CARTESIAN_POINT('Ctrl Pts',(-18.6811715817189,51.7235342471575,124.373224323027)) ;
#95594 = CARTESIAN_POINT('Ctrl Pts',(-18.526225601504,51.7334642736344,124.233278631899)) ;
#95595 = CARTESIAN_POINT('Ctrl Pts',(-18.3964520613895,51.7435168091438,124.0665028494)) ;
#95596 = CARTESIAN_POINT('Ctrl Pts',(-18.2995181598263,51.7533632123635,123.883591037165)) ;
#95597 = CARTESIAN_POINT('Ctrl Pts',(-18.2344303622224,51.7633252552176,123.684540710865)) ;
#95598 = CARTESIAN_POINT('Ctrl Pts',(-18.2049633399143,51.7733538060082,123.475764330925)) ;
#95599 = CARTESIAN_POINT('Ctrl Pts',(-18.2120381052475,51.7832641317259,123.267547741061)) ;
#95600 = CARTESIAN_POINT('Ctrl Pts',(-18.2547347214392,51.7931990435554,123.063088648168)) ;
#95601 = CARTESIAN_POINT('Ctrl Pts',(-18.3332871597924,51.8032400503235,122.86716129288)) ;
#95602 = CARTESIAN_POINT('Ctrl Pts',(-18.442855514963,51.8131276831557,122.690501450574)) ;
#95603 = CARTESIAN_POINT('Ctrl Pts',(-18.5825823298511,51.8231181142538,122.533706140694)) ;
#95604 = CARTESIAN_POINT('Ctrl Pts',(-18.7469172782873,51.833073550811,122.404087562565)) ;
#95605 = CARTESIAN_POINT('Ctrl Pts',(-18.9302413211217,51.8429844989103,122.305087008928)) ;
#95606 = CARTESIAN_POINT('Ctrl Pts',(-19.1299410908847,51.852996575008,122.238509434989)) ;
#95607 = CARTESIAN_POINT('Ctrl Pts',(-19.3385091660018,51.863023897083,122.207996699255)) ;
#95608 = CARTESIAN_POINT('Ctrl Pts',(-19.5457346779231,51.8728826720372,122.213537180948)) ;
#95609 = CARTESIAN_POINT('Ctrl Pts',(-19.8221907089886,51.8863088648496,122.27018561231)) ;
#95610 = CARTESIAN_POINT('Ctrl Pts',(-20.0713995852697,51.899392880631,122.394141621416)) ;
#95611 = CARTESIAN_POINT('Ctrl Pts',(-20.2838395735766,51.9128663293862,122.581345072923)) ;
#95612 = CARTESIAN_POINT('Ctrl Pts',(-20.4126502387728,51.9226992871921,122.74307239301)) ;
#95613 = CARTESIAN_POINT('Ctrl Pts',(-20.5134840256695,51.9326625606427,122.92664557816)) ;
#95614 = CARTESIAN_POINT('Ctrl Pts',(-20.5809847507344,51.9426996344607,123.126566404722)) ;
#95615 = CARTESIAN_POINT('Ctrl Pts',(-20.6126263109704,51.9525746374723,123.331769641933)) ;
#95616 = CARTESIAN_POINT('Ctrl Pts',(-20.6080629074932,51.9626423170985,123.543345669984)) ;
#95617 = CARTESIAN_POINT('Ctrl Pts',(-20.5678682681263,51.9724831673162,123.746313051267)) ;
#95618 = CARTESIAN_POINT('Ctrl Pts',(-20.4670270183732,51.9858193657922,124.007904980157)) ;
#95619 = CARTESIAN_POINT('Ctrl Pts',(-20.3015603831813,51.9990368896066,124.235140214784)) ;
#95620 = CARTESIAN_POINT('Ctrl Pts',(-20.0837896046647,52.0123718160979,124.411582727351)) ;
#95621 = CARTESIAN_POINT('Ctrl Pts',(-19.9002558485253,52.0223549166925,124.513471552646)) ;
#95622 = CARTESIAN_POINT('Ctrl Pts',(-19.7005524850227,52.0323996925921,124.58204856447)) ;
#95623 = CARTESIAN_POINT('Ctrl Pts',(-19.496714337372,52.042217615778,124.614579101692)) ;
#95624 = CARTESIAN_POINT('Ctrl Pts',(-19.2854774239128,52.0522669297334,124.611577325048)) ;
#95625 = CARTESIAN_POINT('Ctrl Pts',(-19.010863063282,52.0655706703559,124.55854219251)) ;
#95626 = CARTESIAN_POINT('Ctrl Pts',(-18.6949728829699,52.0820608658326,124.40631133582)) ;
#95627 = CARTESIAN_POINT('Ctrl Pts',(-18.4467434896524,52.0987800307572,124.151888767484)) ;
#95628 = CARTESIAN_POINT('Ctrl Pts',(-18.3113738584945,52.1119410244274,123.910570859981)) ;
#95629 = CARTESIAN_POINT('Ctrl Pts',(-18.2412220212376,52.1219372465326,123.712480323946)) ;
#95630 = CARTESIAN_POINT('Ctrl Pts',(-18.2069072492689,52.1319610860664,123.504562137768)) ;
#95631 = CARTESIAN_POINT('Ctrl Pts',(-18.2093339154971,52.1451544080596,123.227174122353)) ;
#95632 = CARTESIAN_POINT('Ctrl Pts',(-18.3035482568181,52.1618135798369,122.885761894292)) ;
#95633 = CARTESIAN_POINT('Ctrl Pts',(-18.549002308558,52.1817237553226,122.540816602252)) ;
#95634 = CARTESIAN_POINT('Ctrl Pts',(-18.8966024948958,52.201613743167,122.299840239529)) ;
#95635 = CARTESIAN_POINT('Ctrl Pts',(-19.3079252637735,52.2216191911818,122.191722536724)) ;
#95636 = CARTESIAN_POINT('Ctrl Pts',(-19.7281008697902,52.2414555852091,122.22971345726)) ;
#95637 = CARTESIAN_POINT('Ctrl Pts',(-20.1132537936542,52.2614633791058,122.410106100044)) ;
#95638 = CARTESIAN_POINT('Ctrl Pts',(-20.4112473017471,52.2812900153998,122.708408638474)) ;
#95639 = CARTESIAN_POINT('Ctrl Pts',(-20.5915866931826,52.3012689583536,123.093018147004)) ;
#95640 = CARTESIAN_POINT('Ctrl Pts',(-20.6290084909863,52.3212007602227,123.515109886166)) ;
#95641 = CARTESIAN_POINT('Ctrl Pts',(-20.5220590647266,52.3410250607202,123.922971194583)) ;
#95642 = CARTESIAN_POINT('Ctrl Pts',(-20.2786176342575,52.3611210620601,124.273924800819)) ;
#95643 = CARTESIAN_POINT('Ctrl Pts',(-19.9358038633672,52.380879478164,124.517203259655)) ;
#95644 = CARTESIAN_POINT('Ctrl Pts',(-19.5241772246425,52.4009731710481,124.630789980782)) ;
#95645 = CARTESIAN_POINT('Ctrl Pts',(-19.2461498309204,52.4140841369548,124.608685679991)) ;
#95646 = CARTESIAN_POINT('Ctrl Pts',(-19.1099523892177,52.4207975117427,124.573829556462)) ;
#95647 = CARTESIAN_POINT('',(-18.2012080090896,13.6718523192586,123.050973081965)) ;
#95648 = CARTESIAN_POINT('Ctrl Pts',(-18.9360879628692,13.6947924667251,122.292840803596)) ;
#95649 = CARTESIAN_POINT('Ctrl Pts',(-18.8235714014898,13.6922154699032,122.334824139467)) ;
#95650 = CARTESIAN_POINT('Ctrl Pts',(-18.717918507247,13.6896773479738,122.393380734364)) ;
#95651 = CARTESIAN_POINT('Ctrl Pts',(-18.5046219362228,13.6839804037588,122.555810931824)) ;
#95652 = CARTESIAN_POINT('Ctrl Pts',(-18.4238036284642,13.6814287159771,122.651100591995)) ;
#95653 = CARTESIAN_POINT('Ctrl Pts',(-18.3231340641736,13.6778224757191,122.790090499525)) ;
#95654 = CARTESIAN_POINT('Ctrl Pts',(-18.2820702591376,13.6761482722924,122.860450448584)) ;
#95655 = CARTESIAN_POINT('Ctrl Pts',(-18.2300500481297,13.6735665071738,122.973308264649)) ;
#95656 = CARTESIAN_POINT('Ctrl Pts',(-18.2145001079492,13.6726943420554,123.012358669986)) ;
#95657 = CARTESIAN_POINT('Ctrl Pts',(-18.2012080090896,13.6718523192586,123.050973081965)) ;
#95658 = CARTESIAN_POINT('Ctrl Pts',(-18.2012080090896,13.6718523192586,123.050973081965)) ;
#95659 = CARTESIAN_POINT('Ctrl Pts',(-18.1581996061038,13.6691278393889,123.175915290792)) ;
#95660 = CARTESIAN_POINT('Ctrl Pts',(-18.1387937958945,13.6666598154068,123.296279415935)) ;
#95661 = CARTESIAN_POINT('Ctrl Pts',(-18.1257612025128,13.661023496104,123.570342737487)) ;
#95662 = CARTESIAN_POINT('Ctrl Pts',(-18.1508137569076,13.6577012237818,123.737417962333)) ;
#95663 = CARTESIAN_POINT('Ctrl Pts',(-18.2352191601102,13.6526511564216,123.974578239407)) ;
#95664 = CARTESIAN_POINT('Ctrl Pts',(-18.2712831463275,13.6509739277543,124.051197325921)) ;
#95665 = CARTESIAN_POINT('Ctrl Pts',(-18.3579770185685,13.6475919378534,124.196910378393)) ;
#95666 = CARTESIAN_POINT('Ctrl Pts',(-18.4086013486671,13.6458822226032,124.265780153595)) ;
#95667 = CARTESIAN_POINT('Ctrl Pts',(-18.5223724110274,13.6425352830893,124.392419038975)) ;
#95668 = CARTESIAN_POINT('Ctrl Pts',(-18.5854306417936,13.6408892425574,124.450124298751)) ;
#95669 = CARTESIAN_POINT('Ctrl Pts',(-18.7230337869855,13.6374586642957,124.554029585411)) ;
#95670 = CARTESIAN_POINT('Ctrl Pts',(-18.7977853498151,13.6357466098985,124.599582194036)) ;
#95671 = CARTESIAN_POINT('Ctrl Pts',(-18.9542303094569,13.6324211081276,124.674756173776)) ;
#95672 = CARTESIAN_POINT('Ctrl Pts',(-19.0352628167113,13.6307370012966,124.704593618465)) ;
#95673 = CARTESIAN_POINT('Ctrl Pts',(-19.203949871872,13.6273270305868,124.748915542086)) ;
#95674 = CARTESIAN_POINT('Ctrl Pts',(-19.2914050956568,13.6256576319658,124.762774348756)) ;
#95675 = CARTESIAN_POINT('Ctrl Pts',(-19.4687754438232,13.62226745034,124.773437732167)) ;
#95676 = CARTESIAN_POINT('Ctrl Pts',(-19.5581411015172,13.6205446496771,124.77006951148)) ;
#95677 = CARTESIAN_POINT('Ctrl Pts',(-19.7354306126231,13.6171441040415,124.745652632289)) ;
#95678 = CARTESIAN_POINT('Ctrl Pts',(-19.822565001308,13.6154427854294,124.724844993805)) ;
#95679 = CARTESIAN_POINT('Ctrl Pts',(-20.0764731495327,13.6103641080683,124.637307284215)) ;
#95680 = CARTESIAN_POINT('Ctrl Pts',(-20.2329408847691,13.6070536493622,124.546357434949)) ;
#95681 = CARTESIAN_POINT('Ctrl Pts',(-20.4370829945165,13.6019893485599,124.367567415324)) ;
#95682 = CARTESIAN_POINT('Ctrl Pts',(-20.4996594996402,13.6002817418393,124.300939997901)) ;
#95683 = CARTESIAN_POINT('Ctrl Pts',(-20.6683074370187,13.5952033913329,124.081669485175)) ;
#95684 = CARTESIAN_POINT('Ctrl Pts',(-20.7512472957358,13.5918390838879,123.913926550694)) ;
#95685 = CARTESIAN_POINT('Ctrl Pts',(-20.8485292133704,13.5850157442221,123.555907247786)) ;
#95686 = CARTESIAN_POINT('Ctrl Pts',(-20.8615435921713,13.5817118196242,123.368766670857)) ;
#95687 = CARTESIAN_POINT('Ctrl Pts',(-20.8277134344081,13.5766954025581,123.091458278734)) ;
#95688 = CARTESIAN_POINT('Ctrl Pts',(-20.8071567516996,13.5750061219952,122.999086539571)) ;
#95689 = CARTESIAN_POINT('Ctrl Pts',(-20.7484711008796,13.5716296807235,122.819618482393)) ;
#95690 = CARTESIAN_POINT('Ctrl Pts',(-20.7104369116122,13.5699752678018,122.733015801732)) ;
#95691 = CARTESIAN_POINT('Ctrl Pts',(-20.5904523188124,13.5656129119562,122.518345024356)) ;
#95692 = CARTESIAN_POINT('Ctrl Pts',(-20.496859833978,13.5629586805197,122.398743249045)) ;
#95693 = CARTESIAN_POINT('Ctrl Pts',(-20.3308891118335,13.5589725221892,122.242960467886)) ;
#95694 = CARTESIAN_POINT('Ctrl Pts',(-20.2714146128716,13.5576281988933,122.195112314727)) ;
#95695 = CARTESIAN_POINT('Ctrl Pts',(-20.1451496366424,13.554975483985,122.10873977592)) ;
#95696 = CARTESIAN_POINT('Ctrl Pts',(-20.0784457854721,13.5536392537494,122.070280759549)) ;
#95697 = CARTESIAN_POINT('Ctrl Pts',(-20.0093941796458,13.5522956097346,122.037202589381)) ;
#95698 = CARTESIAN_POINT('Origin',(-19.4092696390756,14.2022556137854,123.41183365498)) ;
#95699 = CARTESIAN_POINT('',(-18.4466282248614,13.7999200508426,123.124282652847)) ;
#95700 = CARTESIAN_POINT('Origin',(-19.4092696390756,13.7999200508426,123.41183365498)) ;
#95701 = CARTESIAN_POINT('',(-19.217636498755,14.2022556137854,123.354590842934)) ;
#95702 = CARTESIAN_POINT('Origin',(-20.3808792107654,13.7999200508426,126.250138578733)) ;
#95703 = CARTESIAN_POINT('',(-19.5760412740791,13.7999200508426,122.562017662105)) ;
#95704 = CARTESIAN_POINT('',(-18.7566932181948,13.7999200508426,122.84249718599)) ;
#95705 = CARTESIAN_POINT('',(-19.5760412740791,13.7999200508426,122.562017662105)) ;
#95706 = CARTESIAN_POINT('',(-18.5899215831784,13.7999200508426,123.692313178869)) ;
#95707 = CARTESIAN_POINT('',(-18.7566932181948,13.7999200508426,122.84249718599)) ;
#95708 = CARTESIAN_POINT('',(-19.2424980040462,13.7999200508426,124.261649647864)) ;
#95709 = CARTESIAN_POINT('',(-18.5899215831784,13.7999200508426,123.692313178869)) ;
#95710 = CARTESIAN_POINT('',(-20.0618460599304,13.7999200508426,123.981170123979)) ;
#95711 = CARTESIAN_POINT('',(-19.2424980040462,13.7999200508426,124.261649647864)) ;
#95712 = CARTESIAN_POINT('',(-20.2286176949469,13.7999200508426,123.131354131099)) ;
#95713 = CARTESIAN_POINT('',(-20.0618460599304,13.7999200508426,123.981170123979)) ;
#95714 = CARTESIAN_POINT('',(-20.2286176949469,13.7999200508426,123.131354131099)) ;
#95715 = CARTESIAN_POINT('Origin',(-19.5760412740791,15.3022556137854,122.562017662105)) ;
#95716 = CARTESIAN_POINT('',(-19.5760412740791,12.9245228503138,122.562017662105)) ;
#95717 = CARTESIAN_POINT('',(-19.5760412740791,13.7999200508426,122.562017662105)) ;
#95718 = CARTESIAN_POINT('',(-18.7566932181948,12.9245228503138,122.84249718599)) ;
#95719 = CARTESIAN_POINT('',(-19.5760412740791,12.9245228503138,122.562017662105)) ;
#95720 = CARTESIAN_POINT('',(-18.7566932181948,13.7999200508426,122.84249718599)) ;
#95721 = CARTESIAN_POINT('Origin',(-18.7566932181948,15.3022556137854,122.84249718599)) ;
#95722 = CARTESIAN_POINT('',(-18.5899215831784,12.9245228503138,123.692313178869)) ;
#95723 = CARTESIAN_POINT('',(-18.7566932181948,12.9245228503138,122.84249718599)) ;
#95724 = CARTESIAN_POINT('',(-18.5899215831784,13.7999200508426,123.692313178869)) ;
#95725 = CARTESIAN_POINT('Origin',(-18.5899215831784,15.3022556137854,123.692313178869)) ;
#95726 = CARTESIAN_POINT('',(-19.2424980040462,12.9245228503138,124.261649647864)) ;
#95727 = CARTESIAN_POINT('',(-18.5899215831784,12.9245228503138,123.692313178869)) ;
#95728 = CARTESIAN_POINT('',(-19.2424980040462,13.7999200508426,124.261649647864)) ;
#95729 = CARTESIAN_POINT('Origin',(-19.2424980040462,15.3022556137854,124.261649647864)) ;
#95730 = CARTESIAN_POINT('',(-20.0618460599304,12.9245228503138,123.981170123979)) ;
#95731 = CARTESIAN_POINT('',(-19.2424980040462,12.9245228503138,124.261649647864)) ;
#95732 = CARTESIAN_POINT('',(-20.0618460599304,13.7999200508426,123.981170123979)) ;
#95733 = CARTESIAN_POINT('Origin',(-20.0618460599304,15.3022556137854,123.981170123979)) ;
#95734 = CARTESIAN_POINT('',(-20.2286176949469,12.9245228503138,123.131354131099)) ;
#95735 = CARTESIAN_POINT('',(-20.0618460599304,12.9245228503138,123.981170123979)) ;
#95736 = CARTESIAN_POINT('',(-20.2286176949469,13.7999200508426,123.131354131099)) ;
#95737 = CARTESIAN_POINT('Origin',(-20.2286176949469,15.3022556137854,123.131354131099)) ;
#95738 = CARTESIAN_POINT('',(-20.2286176949469,12.9245228503138,123.131354131099)) ;
#95739 = CARTESIAN_POINT('Origin',(-19.5760412740791,12.9245228503138,122.562017662105)) ;
#95740 = CARTESIAN_POINT('Origin',(-19.4092696390481,30.19753203383,123.411833654989)) ;
#95741 = CARTESIAN_POINT('',(-20.5587133983317,-13.5907660201144,123.018355650104)) ;
#95742 = CARTESIAN_POINT('',(-20.5587133983317,-13.6088050314641,123.018355650104)) ;
#95743 = CARTESIAN_POINT('',(-20.5587133983318,30.19753203383,123.018355650104)) ;
#95744 = CARTESIAN_POINT('',(-18.74954501676,-13.6947924674767,122.391633028015)) ;
#95745 = CARTESIAN_POINT('Ctrl Pts',(-18.7495450168639,-13.694792467579,122.391633028167)) ;
#95746 = CARTESIAN_POINT('Ctrl Pts',(-18.7717824791181,-13.693549440697,122.377252914101)) ;
#95747 = CARTESIAN_POINT('Ctrl Pts',(-18.7944799450894,-13.6923110178551,
122.363606189365)) ;
#95748 = CARTESIAN_POINT('Ctrl Pts',(-18.8233797355929,-13.6907571749221,
122.347492278542)) ;
#95749 = CARTESIAN_POINT('Ctrl Pts',(-18.8291762036581,-13.6904466706209,
122.344321992078)) ;
#95750 = CARTESIAN_POINT('Ctrl Pts',(-18.8395619159465,-13.6898921945116,
122.338751260341)) ;
#95751 = CARTESIAN_POINT('Ctrl Pts',(-18.8441411969368,-13.6896483541755,
122.336332581449)) ;
#95752 = CARTESIAN_POINT('Ctrl Pts',(-18.8531963369238,-13.6891673703794,
122.331623649583)) ;
#95753 = CARTESIAN_POINT('Ctrl Pts',(-18.8576712263133,-13.6889302438833,
122.329331754761)) ;
#95754 = CARTESIAN_POINT('Ctrl Pts',(-18.8681991480126,-13.688373645001,122.32402192245)) ;
#95755 = CARTESIAN_POINT('Ctrl Pts',(-18.8742634037827,-13.6880540186235,
122.321026628287)) ;
#95756 = CARTESIAN_POINT('Ctrl Pts',(-18.9018739572431,-13.6866031402668,
122.307674693153)) ;
#95757 = CARTESIAN_POINT('Ctrl Pts',(-18.9236979565235,-13.6854679114251,
122.297904788864)) ;
#95758 = CARTESIAN_POINT('Ctrl Pts',(-18.9576652568446,-13.6837234054745,
122.283886733789)) ;
#95759 = CARTESIAN_POINT('Ctrl Pts',(-18.9696116640058,-13.6831141948193,
122.279176759977)) ;
#95760 = CARTESIAN_POINT('Ctrl Pts',(-18.9905101176454,-13.682056549185,122.271317825666)) ;
#95761 = CARTESIAN_POINT('Ctrl Pts',(-18.9994285486634,-13.681607707848,122.268082731327)) ;
#95762 = CARTESIAN_POINT('Ctrl Pts',(-19.0132752362238,-13.6809146541397,
122.263242702341)) ;
#95763 = CARTESIAN_POINT('Ctrl Pts',(-19.0181773865804,-13.6806700223095,
122.261564297921)) ;
#95764 = CARTESIAN_POINT('Ctrl Pts',(-19.0291710963939,-13.680122983839,122.257878661006)) ;
#95765 = CARTESIAN_POINT('Ctrl Pts',(-19.0352681187225,-13.6798206811171,
122.255888200664)) ;
#95766 = CARTESIAN_POINT('Ctrl Pts',(-19.0520517546084,-13.6789912856685,
122.250555631694)) ;
#95767 = CARTESIAN_POINT('Ctrl Pts',(-19.0627692608448,-13.6784647419291,
122.247312829317)) ;
#95768 = CARTESIAN_POINT('Ctrl Pts',(-19.0881961663465,-13.6772214527088,
122.240001500072)) ;
#95769 = CARTESIAN_POINT('Ctrl Pts',(-19.1029403832171,-13.6765051754162,
122.236061074708)) ;
#95770 = CARTESIAN_POINT('Ctrl Pts',(-19.1255674183077,-13.6754097116266,
122.23046846583)) ;
#95771 = CARTESIAN_POINT('Ctrl Pts',(-19.1333989106632,-13.6750312258273,
122.228615162591)) ;
#95772 = CARTESIAN_POINT('Ctrl Pts',(-19.1445596354868,-13.6744922015034,
122.226090834403)) ;
#95773 = CARTESIAN_POINT('Ctrl Pts',(-19.1478741775764,-13.6743321624252,
122.225355743157)) ;
#95774 = CARTESIAN_POINT('Ctrl Pts',(-19.1561389190288,-13.673933144723,122.223559122057)) ;
#95775 = CARTESIAN_POINT('Ctrl Pts',(-19.1610927431651,-13.6736940269801,
122.222514624969)) ;
#95776 = CARTESIAN_POINT('Ctrl Pts',(-19.1860492098872,-13.6724900155874,
122.21741535287)) ;
#95777 = CARTESIAN_POINT('Ctrl Pts',(-19.2061452432381,-13.6715227053514,
122.213834105627)) ;
#95778 = CARTESIAN_POINT('Ctrl Pts',(-19.23291792797,-13.6702410510381,122.209756084041)) ;
#95779 = CARTESIAN_POINT('Ctrl Pts',(-19.2395220894196,-13.6699254411882,
122.20880573253)) ;
#95780 = CARTESIAN_POINT('Ctrl Pts',(-19.2537750909116,-13.6692455630651,
122.206874401013)) ;
#95781 = CARTESIAN_POINT('Ctrl Pts',(-19.2614261289387,-13.668881388136,122.205911744049)) ;
#95782 = CARTESIAN_POINT('Ctrl Pts',(-19.2746967185821,-13.6682511222357,
122.204370226132)) ;
#95783 = CARTESIAN_POINT('Ctrl Pts',(-19.2803120938844,-13.6679848573333,
122.203757599962)) ;
#95784 = CARTESIAN_POINT('Ctrl Pts',(-19.2935187530765,-13.6673596131917,
122.202409910547)) ;
#95785 = CARTESIAN_POINT('Ctrl Pts',(-19.3011130974726,-13.6670008332143,
122.201707122629)) ;
#95786 = CARTESIAN_POINT('Ctrl Pts',(-19.3329230523149,-13.6655008847925,
122.199065236754)) ;
#95787 = CARTESIAN_POINT('Ctrl Pts',(-19.3571873487778,-13.664364252329,122.197781153088)) ;
#95788 = CARTESIAN_POINT('Ctrl Pts',(-19.3940722173949,-13.6626373173957,
122.196937060716)) ;
#95789 = CARTESIAN_POINT('Ctrl Pts',(-19.4066742116343,-13.6620472278919,
122.196844783129)) ;
#95790 = CARTESIAN_POINT('Ctrl Pts',(-19.4259425468957,-13.661143213185,122.197003475478)) ;
#95791 = CARTESIAN_POINT('Ctrl Pts',(-19.4326091837732,-13.6608301168815,
122.197113268994)) ;
#95792 = CARTESIAN_POINT('Ctrl Pts',(-19.4451526076521,-13.660240218195,122.197423147325)) ;
#95793 = CARTESIAN_POINT('Ctrl Pts',(-19.4510295040133,-13.6599635058396,
122.19761103046)) ;
#95794 = CARTESIAN_POINT('Ctrl Pts',(-19.4610629910378,-13.6594904300927,
122.198004728816)) ;
#95795 = CARTESIAN_POINT('Ctrl Pts',(-19.4652203168081,-13.6592942228917,
122.198189252841)) ;
#95796 = CARTESIAN_POINT('Ctrl Pts',(-19.4749307882136,-13.6588354605347,
122.198670255355)) ;
#95797 = CARTESIAN_POINT('Ctrl Pts',(-19.480483002822,-13.6585727900909,122.198983508737)) ;
#95798 = CARTESIAN_POINT('Ctrl Pts',(-19.4969230193466,-13.6577939246046,
122.200024325125)) ;
#95799 = CARTESIAN_POINT('Ctrl Pts',(-19.5078033495282,-13.6572770059852,
122.200860462429)) ;
#95800 = CARTESIAN_POINT('Ctrl Pts',(-19.5426000601527,-13.6556195588844,
122.20400660586)) ;
#95801 = CARTESIAN_POINT('Ctrl Pts',(-19.5664597389735,-13.6544764879401,
122.206879525702)) ;
#95802 = CARTESIAN_POINT('Ctrl Pts',(-19.5996156476836,-13.6528853024637,
122.211873404616)) ;
#95803 = CARTESIAN_POINT('Ctrl Pts',(-19.6089958730021,-13.6524347890233,
122.213398993468)) ;
#95804 = CARTESIAN_POINT('Ctrl Pts',(-19.6255056712482,-13.6516413299066,
122.216283349095)) ;
#95805 = CARTESIAN_POINT('Ctrl Pts',(-19.6326427659189,-13.6512981446249,
122.217596240465)) ;
#95806 = CARTESIAN_POINT('Ctrl Pts',(-19.6398740641871,-13.65095021773,122.218993553832)) ;
#95807 = CARTESIAN_POINT('Ctrl Pts',(-19.6399804380918,-13.6509450996054,
122.219014123363)) ;
#95808 = CARTESIAN_POINT('Ctrl Pts',(-19.6401944986045,-13.6509348001003,
122.21905554597)) ;
#95809 = CARTESIAN_POINT('Ctrl Pts',(-19.6403021850202,-13.6509296187279,
122.219076399376)) ;
#95810 = CARTESIAN_POINT('Ctrl Pts',(-19.6405196262895,-13.6509191563605,
122.219118537291)) ;
#95811 = CARTESIAN_POINT('Ctrl Pts',(-19.6406293810393,-13.6509138753685,
122.219139822369)) ;
#95812 = CARTESIAN_POINT('Ctrl Pts',(-19.6408517953669,-13.6509031735115,
122.219182987723)) ;
#95813 = CARTESIAN_POINT('Ctrl Pts',(-19.6409644547319,-13.6508977526538,
122.219204868803)) ;
#95814 = CARTESIAN_POINT('Ctrl Pts',(-19.6411936268907,-13.6508867254122,
122.219249413086)) ;
#95815 = CARTESIAN_POINT('Ctrl Pts',(-19.6413101392158,-13.6508811190469,
122.219272077352)) ;
#95816 = CARTESIAN_POINT('Ctrl Pts',(-19.6415481182962,-13.6508696677994,
122.21931840583)) ;
#95817 = CARTESIAN_POINT('Ctrl Pts',(-19.6416695849778,-13.6508638229156,
122.219342071568)) ;
#95818 = CARTESIAN_POINT('Ctrl Pts',(-19.6419187815019,-13.6508518316393,
122.219390662836)) ;
#95819 = CARTESIAN_POINT('Ctrl Pts',(-19.6420465110655,-13.6508456852534,
122.219415590351)) ;
#95820 = CARTESIAN_POINT('Ctrl Pts',(-19.6476098301456,-13.6505779735594,
122.220502247573)) ;
#95821 = CARTESIAN_POINT('Ctrl Pts',(-19.6530381096081,-13.6503166336167,
122.221601113854)) ;
#95822 = CARTESIAN_POINT('Ctrl Pts',(-19.6650703742322,-13.6497369944636,
122.224122615209)) ;
#95823 = CARTESIAN_POINT('Ctrl Pts',(-19.671670393751,-13.6494188088537,122.225563291859)) ;
#95824 = CARTESIAN_POINT('Ctrl Pts',(-19.6969974026277,-13.6481965312817,
122.231313475636)) ;
#95825 = CARTESIAN_POINT('Ctrl Pts',(-19.7156331698654,-13.6472946520805,
122.236012006291)) ;
#95826 = CARTESIAN_POINT('Ctrl Pts',(-19.7430105495079,-13.6459607527317,
122.24360959158)) ;
#95827 = CARTESIAN_POINT('Ctrl Pts',(-19.7518431923233,-13.6455289736605,
122.246169115899)) ;
#95828 = CARTESIAN_POINT('Ctrl Pts',(-19.7661434780406,-13.6448266814585,
122.250489631365)) ;
#95829 = CARTESIAN_POINT('Ctrl Pts',(-19.7716291951974,-13.6445564928947,
122.252189558673)) ;
#95830 = CARTESIAN_POINT('Ctrl Pts',(-19.7798739640202,-13.6441490076473,
122.254808683075)) ;
#95831 = CARTESIAN_POINT('Ctrl Pts',(-19.7826421070064,-13.6440119618968,
122.255698995249)) ;
#95832 = CARTESIAN_POINT('Ctrl Pts',(-19.7886896507559,-13.6437120665695,
122.257668039151)) ;
#95833 = CARTESIAN_POINT('Ctrl Pts',(-19.7919677038318,-13.6435491915586,
122.258750828292)) ;
#95834 = CARTESIAN_POINT('Ctrl Pts',(-19.7989756785177,-13.6432003403116,
122.261098841193)) ;
#95835 = CARTESIAN_POINT('Ctrl Pts',(-19.8027041534928,-13.643014344504,122.262368261136)) ;
#95836 = CARTESIAN_POINT('Ctrl Pts',(-19.8223045893248,-13.6420345896768,
122.269148086418)) ;
#95837 = CARTESIAN_POINT('Ctrl Pts',(-19.8380671453385,-13.6412398806722,
122.274969161328)) ;
#95838 = CARTESIAN_POINT('Ctrl Pts',(-19.8668764918669,-13.6397765946529,
122.286292812165)) ;
#95839 = CARTESIAN_POINT('Ctrl Pts',(-19.8799576410896,-13.6391079725323,
122.291700168665)) ;
#95840 = CARTESIAN_POINT('Ctrl Pts',(-19.9010632608055,-13.6380224992499,
122.300859614311)) ;
#95841 = CARTESIAN_POINT('Ctrl Pts',(-19.9091464149024,-13.6376051463538,
122.30447305652)) ;
#95842 = CARTESIAN_POINT('Ctrl Pts',(-19.9248761743006,-13.636789656279,122.311712116973)) ;
#95843 = CARTESIAN_POINT('Ctrl Pts',(-19.9325258297617,-13.6363915085031,
122.315329912622)) ;
#95844 = CARTESIAN_POINT('Ctrl Pts',(-19.9505456394539,-13.6354496403085,
122.324083641514)) ;
#95845 = CARTESIAN_POINT('Ctrl Pts',(-19.9608814461058,-13.6349062543941,
122.329288406133)) ;
#95846 = CARTESIAN_POINT('Ctrl Pts',(-19.9912063484371,-13.6333012416947,
122.345106086667)) ;
#95847 = CARTESIAN_POINT('Ctrl Pts',(-20.0109749728718,-13.6322406103438,
122.35613070028)) ;
#95848 = CARTESIAN_POINT('Ctrl Pts',(-20.0378294263587,-13.6307720674989,
122.372106413805)) ;
#95849 = CARTESIAN_POINT('Ctrl Pts',(-20.045187635425,-13.6303667541563,122.376590474133)) ;
#95850 = CARTESIAN_POINT('Ctrl Pts',(-20.0581910393609,-13.6296449177419,
122.384705642507)) ;
#95851 = CARTESIAN_POINT('Ctrl Pts',(-20.0638550216281,-13.6293285924206,
122.3883059737)) ;
#95852 = CARTESIAN_POINT('Ctrl Pts',(-20.0719387863185,-13.6288742877062,
122.393538994947)) ;
#95853 = CARTESIAN_POINT('Ctrl Pts',(-20.0743829773879,-13.6287365493352,
122.395133767831)) ;
#95854 = CARTESIAN_POINT('Ctrl Pts',(-20.0772853821822,-13.6285725369608,
122.39704245903)) ;
#95855 = CARTESIAN_POINT('Ctrl Pts',(-20.0777491587394,-13.6285463155674,
122.397347905349)) ;
#95856 = CARTESIAN_POINT('Ctrl Pts',(-20.0786932965544,-13.6284929069781,
122.397970649312)) ;
#95857 = CARTESIAN_POINT('Ctrl Pts',(-20.0791736420482,-13.628465719642,122.398287970635)) ;
#95858 = CARTESIAN_POINT('Ctrl Pts',(-20.0800305219467,-13.6284171940863,
122.39885490983)) ;
#95859 = CARTESIAN_POINT('Ctrl Pts',(-20.0804071430302,-13.6283958566751,
122.399104396539)) ;
#95860 = CARTESIAN_POINT('Ctrl Pts',(-20.0810735810095,-13.6283580834894,
122.399546402917)) ;
#95861 = CARTESIAN_POINT('Ctrl Pts',(-20.0813634545221,-13.6283416482402,
122.399738837127)) ;
#95862 = CARTESIAN_POINT('Ctrl Pts',(-20.0902267068211,-13.627838952855,122.405628245407)) ;
#95863 = CARTESIAN_POINT('Ctrl Pts',(-20.0987273946819,-13.6273520380273,
122.41143380672)) ;
#95864 = CARTESIAN_POINT('Ctrl Pts',(-20.1181352124667,-13.6262291937517,
122.425053289256)) ;
#95865 = CARTESIAN_POINT('Ctrl Pts',(-20.1289887345753,-13.6255929325447,
122.432941263961)) ;
#95866 = CARTESIAN_POINT('Ctrl Pts',(-20.1598411693405,-13.623760865024,122.456154318432)) ;
#95867 = CARTESIAN_POINT('Ctrl Pts',(-20.179497078235,-13.6225650397266,122.471923913381)) ;
#95868 = CARTESIAN_POINT('Ctrl Pts',(-20.2039385071538,-13.6210446163719,
122.492814768438)) ;
#95869 = CARTESIAN_POINT('Ctrl Pts',(-20.2091895374752,-13.6207158727961,
122.49738164405)) ;
#95870 = CARTESIAN_POINT('Ctrl Pts',(-20.2151770886304,-13.62033855872,122.502680118662)) ;
#95871 = CARTESIAN_POINT('Ctrl Pts',(-20.2159522454046,-13.6202896631917,
122.503367836969)) ;
#95872 = CARTESIAN_POINT('Ctrl Pts',(-20.2195445273023,-13.620062844918,122.506563128759)) ;
#95873 = CARTESIAN_POINT('Ctrl Pts',(-20.2223508491543,-13.6198850141316,
122.509082822236)) ;
#95874 = CARTESIAN_POINT('Ctrl Pts',(-20.2304948862323,-13.6193670422278,
122.516463836177)) ;
#95875 = CARTESIAN_POINT('Ctrl Pts',(-20.2358010636348,-13.6190271643956,
122.521359722944)) ;
#95876 = CARTESIAN_POINT('Ctrl Pts',(-20.2444014063974,-13.6184721432654,
122.529438164395)) ;
#95877 = CARTESIAN_POINT('Ctrl Pts',(-20.2477217614171,-13.6182568357673,
122.532592556519)) ;
#95878 = CARTESIAN_POINT('Ctrl Pts',(-20.2610594123415,-13.6173876196673,
122.545407804316)) ;
#95879 = CARTESIAN_POINT('Ctrl Pts',(-20.2709282051993,-13.6167345425856,
122.555221672591)) ;
#95880 = CARTESIAN_POINT('Ctrl Pts',(-20.2882624560896,-13.6155665990756,
122.573062170325)) ;
#95881 = CARTESIAN_POINT('Ctrl Pts',(-20.295791986104,-13.6150519094649,122.581024349182)) ;
#95882 = CARTESIAN_POINT('Ctrl Pts',(-20.3067378673226,-13.6142911215712,
122.59291743706)) ;
#95883 = CARTESIAN_POINT('Ctrl Pts',(-20.3102383230532,-13.6140458522976,
122.596770207866)) ;
#95884 = CARTESIAN_POINT('Ctrl Pts',(-20.3173275677795,-13.6135451515054,
122.604674447381)) ;
#95885 = CARTESIAN_POINT('Ctrl Pts',(-20.320914267111,-13.6132897110777,122.608727646857)) ;
#95886 = CARTESIAN_POINT('Ctrl Pts',(-20.3399498247594,-13.6119228509513,
122.630530886894)) ;
#95887 = CARTESIAN_POINT('Ctrl Pts',(-20.3549076171131,-13.6108091746304,
122.648702973382)) ;
#95888 = CARTESIAN_POINT('Ctrl Pts',(-20.3763191129364,-13.6091577826272,
122.676312515767)) ;
#95889 = CARTESIAN_POINT('Ctrl Pts',(-20.3831827120002,-13.6086189941672,
122.685425120709)) ;
#95890 = CARTESIAN_POINT('Ctrl Pts',(-20.3936665083757,-13.6077812307049,
122.699759892477)) ;
#95891 = CARTESIAN_POINT('Ctrl Pts',(-20.3973757885229,-13.6074818166569,
122.704916066268)) ;
#95892 = CARTESIAN_POINT('Ctrl Pts',(-20.4049850236797,-13.6068612978947,
122.715670374084)) ;
#95893 = CARTESIAN_POINT('Ctrl Pts',(-20.4088786039128,-13.6065402412509,
122.721272753535)) ;
#95894 = CARTESIAN_POINT('Ctrl Pts',(-20.4199606285467,-13.6056160630772,
122.737508543343)) ;
#95895 = CARTESIAN_POINT('Ctrl Pts',(-20.427028049079,-13.6050137921692,122.748223487526)) ;
#95896 = CARTESIAN_POINT('Ctrl Pts',(-20.4439033742141,-13.6035427368904,
122.774712112123)) ;
#95897 = CARTESIAN_POINT('Ctrl Pts',(-20.4535218732508,-13.6026750262393,
122.790602538728)) ;
#95898 = CARTESIAN_POINT('Ctrl Pts',(-20.4688560633354,-13.6012333168085,
122.817298796115)) ;
#95899 = CARTESIAN_POINT('Ctrl Pts',(-20.4747796980336,-13.6006605834102,
122.827981447011)) ;
#95900 = CARTESIAN_POINT('Ctrl Pts',(-20.4829869289623,-13.5998426470645,
122.843323355846)) ;
#95901 = CARTESIAN_POINT('Ctrl Pts',(-20.4854033371946,-13.5995986567211,
122.847910750378)) ;
#95902 = CARTESIAN_POINT('Ctrl Pts',(-20.4895361947,-13.5991757130952,122.85588001783)) ;
#95903 = CARTESIAN_POINT('Ctrl Pts',(-20.4912663127831,-13.5989968945199,
122.859254723209)) ;
#95904 = CARTESIAN_POINT('Ctrl Pts',(-20.4946539149002,-13.5986432183309,
122.865939368197)) ;
#95905 = CARTESIAN_POINT('Ctrl Pts',(-20.4963121284697,-13.5984683700984,
122.869248892297)) ;
#95906 = CARTESIAN_POINT('Ctrl Pts',(-20.4998875432325,-13.5980875532769,
122.876467018383)) ;
#95907 = CARTESIAN_POINT('Ctrl Pts',(-20.5017989117916,-13.5978815284479,
122.880378448463)) ;
#95908 = CARTESIAN_POINT('Ctrl Pts',(-20.5064659021014,-13.5973723467665,
122.890060572172)) ;
#95909 = CARTESIAN_POINT('Ctrl Pts',(-20.5091970583652,-13.597068951058,122.895842897992)) ;
#95910 = CARTESIAN_POINT('Ctrl Pts',(-20.5294985778144,-13.5947719899805,
122.939718394837)) ;
#95911 = CARTESIAN_POINT('Ctrl Pts',(-20.5451271696464,-13.5927564994546,
122.978667012923)) ;
#95912 = CARTESIAN_POINT('Ctrl Pts',(-20.5587133983318,-13.5907660201144,
123.018355650104)) ;
#95913 = CARTESIAN_POINT('',(-19.0974359579283,-13.6947924664111,122.237608099923)) ;
#95914 = CARTESIAN_POINT('Origin',(-19.4092696801845,-13.6947924276734,123.411833722943)) ;
#95915 = CARTESIAN_POINT('Ctrl Pts',(-20.5587133983318,-13.6088050314642,
123.018355650104)) ;
#95916 = CARTESIAN_POINT('Ctrl Pts',(-20.5553438079184,-13.6092962280985,
123.008512267185)) ;
#95917 = CARTESIAN_POINT('Ctrl Pts',(-20.5518513187474,-13.6097873550664,
122.998721991471)) ;
#95918 = CARTESIAN_POINT('Ctrl Pts',(-20.5434236364509,-13.6109330714511,
122.976022567895)) ;
#95919 = CARTESIAN_POINT('Ctrl Pts',(-20.5383968526497,-13.6115880006921,
122.963159692719)) ;
#95920 = CARTESIAN_POINT('Ctrl Pts',(-20.5264139591459,-13.6130861321529,
122.933974707307)) ;
#95921 = CARTESIAN_POINT('Ctrl Pts',(-20.5193173477431,-13.6139290526108,
122.917713533569)) ;
#95922 = CARTESIAN_POINT('Ctrl Pts',(-20.5092688417327,-13.6150630225624,
122.895998477061)) ;
#95923 = CARTESIAN_POINT('Ctrl Pts',(-20.5066276347547,-13.6153559808119,
122.89040330844)) ;
#95924 = CARTESIAN_POINT('Ctrl Pts',(-20.502032354391,-13.615857027939,122.880858173907)) ;
#95925 = CARTESIAN_POINT('Ctrl Pts',(-20.5000993220779,-13.6160652740916,
122.876898223071)) ;
#95926 = CARTESIAN_POINT('Ctrl Pts',(-20.4963104761307,-13.6164686039566,
122.869242448983)) ;
#95927 = CARTESIAN_POINT('Ctrl Pts',(-20.4944572516781,-13.6166637067726,
122.865545412534)) ;
#95928 = CARTESIAN_POINT('Ctrl Pts',(-20.4907451692781,-13.6170502377559,
122.858233532779)) ;
#95929 = CARTESIAN_POINT('Ctrl Pts',(-20.4888869748423,-13.6172416691845,
122.854618412757)) ;
#95930 = CARTESIAN_POINT('Ctrl Pts',(-20.4843780018769,-13.6177013032405,
122.84595342807)) ;
#95931 = CARTESIAN_POINT('Ctrl Pts',(-20.4817097359941,-13.6179693390874,
122.840912765679)) ;
#95932 = CARTESIAN_POINT('Ctrl Pts',(-20.4648271544284,-13.619641074788,122.809555625552)) ;
#95933 = CARTESIAN_POINT('Ctrl Pts',(-20.4496806822719,-13.6210342463968,
122.783752961496)) ;
#95934 = CARTESIAN_POINT('Ctrl Pts',(-20.426967239871,-13.6230045680127,122.748139813375)) ;
#95935 = CARTESIAN_POINT('Ctrl Pts',(-20.4201792919864,-13.6235802564365,
122.737845826057)) ;
#95936 = CARTESIAN_POINT('Ctrl Pts',(-20.4098481622919,-13.6244391662298,
122.722685845324)) ;
#95937 = CARTESIAN_POINT('Ctrl Pts',(-20.4064236014756,-13.6247211671694,
122.717739958489)) ;
#95938 = CARTESIAN_POINT('Ctrl Pts',(-20.4021659205852,-13.6250685925039,
122.711687393957)) ;
#95939 = CARTESIAN_POINT('Ctrl Pts',(-20.4013674482898,-13.6251336119702,
122.710556427625)) ;
#95940 = CARTESIAN_POINT('Ctrl Pts',(-20.4002133048617,-13.6252273999639,
122.708927600363)) ;
#95941 = CARTESIAN_POINT('Ctrl Pts',(-20.3998591875595,-13.6252561500634,
122.708428638781)) ;
#95942 = CARTESIAN_POINT('Ctrl Pts',(-20.3990768664728,-13.6253196076579,
122.70732808802)) ;
#95943 = CARTESIAN_POINT('Ctrl Pts',(-20.3986484909098,-13.6253543171956,
122.706726621383)) ;
#95944 = CARTESIAN_POINT('Ctrl Pts',(-20.3979145115824,-13.6254137239483,
122.705698053348)) ;
#95945 = CARTESIAN_POINT('Ctrl Pts',(-20.3976091786562,-13.6254384178799,
122.705270758751)) ;
#95946 = CARTESIAN_POINT('Ctrl Pts',(-20.397087378809,-13.6254805861973,122.704541532087)) ;
#95947 = CARTESIAN_POINT('Ctrl Pts',(-20.3968710502561,-13.6254980588929,
122.704239501052)) ;
#95948 = CARTESIAN_POINT('Ctrl Pts',(-20.3965013931081,-13.6255278996236,
122.703723897266)) ;
#95949 = CARTESIAN_POINT('Ctrl Pts',(-20.3963481336436,-13.6255402668109,
122.703510274947)) ;
#95950 = CARTESIAN_POINT('Ctrl Pts',(-20.3950831717322,-13.6256423030957,
122.701748302279)) ;
#95951 = CARTESIAN_POINT('Ctrl Pts',(-20.3939678974135,-13.6257320159907,
122.700202522089)) ;
#95952 = CARTESIAN_POINT('Ctrl Pts',(-20.3909646912427,-13.6259729329128,
122.696060629061)) ;
#95953 = CARTESIAN_POINT('Ctrl Pts',(-20.3890701032366,-13.6261242199319,
122.693469366869)) ;
#95954 = CARTESIAN_POINT('Ctrl Pts',(-20.3852803037695,-13.6264254778996,
122.68832887364)) ;
#95955 = CARTESIAN_POINT('Ctrl Pts',(-20.3833853199085,-13.6265754449183,
122.68577950652)) ;
#95956 = CARTESIAN_POINT('Ctrl Pts',(-20.3783021918991,-13.6269759534538,
122.678996774767)) ;
#95957 = CARTESIAN_POINT('Ctrl Pts',(-20.3750963174573,-13.6272267195812,
122.674776799364)) ;
#95958 = CARTESIAN_POINT('Ctrl Pts',(-20.3598879606624,-13.6284078058735,
122.655027255085)) ;
#95959 = CARTESIAN_POINT('Ctrl Pts',(-20.3475380331744,-13.6293425243824,
122.639769197627)) ;
#95960 = CARTESIAN_POINT('Ctrl Pts',(-20.3250865081291,-13.6309963678851,
122.613365548638)) ;
#95961 = CARTESIAN_POINT('Ctrl Pts',(-20.3151372832034,-13.6317144393509,
122.602095631098)) ;
#95962 = CARTESIAN_POINT('Ctrl Pts',(-20.2979451636562,-13.6329274508519,
122.583334907608)) ;
#95963 = CARTESIAN_POINT('Ctrl Pts',(-20.290810372577,-13.6334231389733,122.575747355837)) ;
#95964 = CARTESIAN_POINT('Ctrl Pts',(-20.2797640558079,-13.6341784956345,
122.564298669534)) ;
#95965 = CARTESIAN_POINT('Ctrl Pts',(-20.2759224571499,-13.6344390207193,
122.56037081116)) ;
#95966 = CARTESIAN_POINT('Ctrl Pts',(-20.26942796267,-13.6348758282378,122.5538199778)) ;
#95967 = CARTESIAN_POINT('Ctrl Pts',(-20.2667893980366,-13.6350523041401,
122.551182927339)) ;
#95968 = CARTESIAN_POINT('Ctrl Pts',(-20.2618820867791,-13.6353787046789,
122.546323403066)) ;
#95969 = CARTESIAN_POINT('Ctrl Pts',(-20.259616692343,-13.6355286752513,122.544097594175)) ;
#95970 = CARTESIAN_POINT('Ctrl Pts',(-20.2550017156138,-13.6358327684797,
122.539598687801)) ;
#95971 = CARTESIAN_POINT('Ctrl Pts',(-20.2526516340345,-13.6359868824503,
122.537326139909)) ;
#95972 = CARTESIAN_POINT('Ctrl Pts',(-20.2470915646565,-13.6363497851998,
122.531992766317)) ;
#95973 = CARTESIAN_POINT('Ctrl Pts',(-20.243873929026,-13.6365584629181,122.528939976367)) ;
#95974 = CARTESIAN_POINT('Ctrl Pts',(-20.2335606666722,-13.6372231778913,
122.519261843037)) ;
#95975 = CARTESIAN_POINT('Ctrl Pts',(-20.2264023019244,-13.6376783420438,
122.512703880949)) ;
#95976 = CARTESIAN_POINT('Ctrl Pts',(-20.2036228680529,-13.6391088997394,
122.492331800047)) ;
#95977 = CARTESIAN_POINT('Ctrl Pts',(-20.187724461554,-13.6400811046819,122.478833763101)) ;
#95978 = CARTESIAN_POINT('Ctrl Pts',(-20.1637981168748,-13.6415183580918,
122.459557354291)) ;
#95979 = CARTESIAN_POINT('Ctrl Pts',(-20.1560344913884,-13.6419809828887,
122.453457095166)) ;
#95980 = CARTESIAN_POINT('Ctrl Pts',(-20.1425134171039,-13.6427804358353,
122.443096986235)) ;
#95981 = CARTESIAN_POINT('Ctrl Pts',(-20.1367910486356,-13.6431168898162,
122.438792150456)) ;
#95982 = CARTESIAN_POINT('Ctrl Pts',(-20.1252697522125,-13.6437905745032,
122.430283335715)) ;
#95983 = CARTESIAN_POINT('Ctrl Pts',(-20.1194710335211,-13.644127792214,122.426079542561)) ;
#95984 = CARTESIAN_POINT('Ctrl Pts',(-20.1072784530794,-13.6448330024161,
122.417403936894)) ;
#95985 = CARTESIAN_POINT('Ctrl Pts',(-20.100877997422,-13.6452010358921,122.412941945714)) ;
#95986 = CARTESIAN_POINT('Ctrl Pts',(-20.0757000753169,-13.6466403538196,
122.395747504592)) ;
#95987 = CARTESIAN_POINT('Ctrl Pts',(-20.0566104769855,-13.647713555942,122.383480395732)) ;
#95988 = CARTESIAN_POINT('Ctrl Pts',(-20.0270071279921,-13.6493493626985,
122.365608182793)) ;
#95989 = CARTESIAN_POINT('Ctrl Pts',(-20.0167358434802,-13.6499118660897,
122.359611171347)) ;
#95990 = CARTESIAN_POINT('Ctrl Pts',(-19.9984519859016,-13.6509038972769,
122.34929288374)) ;
#95991 = CARTESIAN_POINT('Ctrl Pts',(-19.9904757963391,-13.6513335568291,
122.344909041075)) ;
#95992 = CARTESIAN_POINT('Ctrl Pts',(-19.9741206758747,-13.6522084660054,
122.336157836637)) ;
#95993 = CARTESIAN_POINT('Ctrl Pts',(-19.9657385482259,-13.6526536996476,
122.331797769637)) ;
#95994 = CARTESIAN_POINT('Ctrl Pts',(-19.9315537336651,-13.6544578782867,
122.314519733796)) ;
#95995 = CARTESIAN_POINT('Ctrl Pts',(-19.9053455279596,-13.6558145092579,
122.302425151038)) ;
#95996 = CARTESIAN_POINT('Ctrl Pts',(-19.8697828320191,-13.6576311507477,
122.287526031283)) ;
#95997 = CARTESIAN_POINT('Ctrl Pts',(-19.8607894324787,-13.6580885406436,
122.283884228326)) ;
#95998 = CARTESIAN_POINT('Ctrl Pts',(-19.8438677556951,-13.6589459487442,
122.2772667481)) ;
#95999 = CARTESIAN_POINT('Ctrl Pts',(-19.8359501118568,-13.6593458338057,
122.274265475625)) ;
#96000 = CARTESIAN_POINT('Ctrl Pts',(-19.8206957756275,-13.6601141598108,
122.268664812271)) ;
#96001 = CARTESIAN_POINT('Ctrl Pts',(-19.81336420219,-13.6604825122226,122.266052675809)) ;
#96002 = CARTESIAN_POINT('Ctrl Pts',(-19.7963573741226,-13.6613351856603,
122.260176920395)) ;
#96003 = CARTESIAN_POINT('Ctrl Pts',(-19.7866650768951,-13.661819882873,122.256964471485)) ;
#96004 = CARTESIAN_POINT('Ctrl Pts',(-19.7582866858297,-13.6632335594711,
122.247954042316)) ;
#96005 = CARTESIAN_POINT('Ctrl Pts',(-19.7394994981533,-13.6641623326195,
122.242484733412)) ;
#96006 = CARTESIAN_POINT('Ctrl Pts',(-19.7148385348169,-13.6653693068274,
122.235947210719)) ;
#96007 = CARTESIAN_POINT('Ctrl Pts',(-19.7090775842078,-13.6656504282528,
122.234465201087)) ;
#96008 = CARTESIAN_POINT('Ctrl Pts',(-19.6990556154707,-13.6661380218234,
122.231965368509)) ;
#96009 = CARTESIAN_POINT('Ctrl Pts',(-19.6947995534492,-13.6663446364545,
122.230928174563)) ;
#96010 = CARTESIAN_POINT('Ctrl Pts',(-19.6890822019901,-13.6666215935146,
122.229567583001)) ;
#96011 = CARTESIAN_POINT('Ctrl Pts',(-19.6876257977677,-13.6666920921007,
122.229223835876)) ;
#96012 = CARTESIAN_POINT('Ctrl Pts',(-19.6856952502208,-13.6667854740914,
122.228771943129)) ;
#96013 = CARTESIAN_POINT('Ctrl Pts',(-19.6852216725895,-13.6668083759741,
122.228661390369)) ;
#96014 = CARTESIAN_POINT('Ctrl Pts',(-19.6843148070425,-13.6668522210348,
122.22845026424)) ;
#96015 = CARTESIAN_POINT('Ctrl Pts',(-19.6838815300983,-13.6668731645632,
122.228349644437)) ;
#96016 = CARTESIAN_POINT('Ctrl Pts',(-19.6830101300092,-13.6669152768387,
122.228147783698)) ;
#96017 = CARTESIAN_POINT('Ctrl Pts',(-19.6825720056838,-13.6669364455442,
122.228046547998)) ;
#96018 = CARTESIAN_POINT('Ctrl Pts',(-19.6816583691911,-13.6669805798771,
122.227835971781)) ;
#96019 = CARTESIAN_POINT('Ctrl Pts',(-19.6811828471333,-13.6670035451713,
122.227726674425)) ;
#96020 = CARTESIAN_POINT('Ctrl Pts',(-19.6801616963258,-13.6670528500514,
122.227492613454)) ;
#96021 = CARTESIAN_POINT('Ctrl Pts',(-19.6796160469497,-13.6670791889406,
122.227367940375)) ;
#96022 = CARTESIAN_POINT('Ctrl Pts',(-19.6784149782977,-13.6671371499622,
122.227094386549)) ;
#96023 = CARTESIAN_POINT('Ctrl Pts',(-19.6777595211324,-13.6671687708248,
122.226945672502)) ;
#96024 = CARTESIAN_POINT('Ctrl Pts',(-19.6762867606039,-13.6672397978627,
122.226612808575)) ;
#96025 = CARTESIAN_POINT('Ctrl Pts',(-19.6754693893873,-13.6672792017538,
122.226428960001)) ;
#96026 = CARTESIAN_POINT('Ctrl Pts',(-19.6691835002928,-13.6675821136324,
122.225021925319)) ;
#96027 = CARTESIAN_POINT('Ctrl Pts',(-19.6637067583777,-13.6678453409614,
122.223835738519)) ;
#96028 = CARTESIAN_POINT('Ctrl Pts',(-19.6490068710556,-13.6685501556025,
122.220758260213)) ;
#96029 = CARTESIAN_POINT('Ctrl Pts',(-19.6397696132971,-13.6689912538379,
122.218936216271)) ;
#96030 = CARTESIAN_POINT('Ctrl Pts',(-19.5984001142658,-13.6709605208545,
122.211274574153)) ;
#96031 = CARTESIAN_POINT('Ctrl Pts',(-19.5660615865026,-13.6724847047256,
122.20662465681)) ;
#96032 = CARTESIAN_POINT('Ctrl Pts',(-19.5265198316265,-13.674352394419,122.202557594951)) ;
#96033 = CARTESIAN_POINT('Ctrl Pts',(-19.5194585358497,-13.6746859995493,
122.201893737659)) ;
#96034 = CARTESIAN_POINT('Ctrl Pts',(-19.5071117962561,-13.6752695688255,
122.200841958224)) ;
#96035 = CARTESIAN_POINT('Ctrl Pts',(-19.5018288674458,-13.6755193482243,
122.200426718249)) ;
#96036 = CARTESIAN_POINT('Ctrl Pts',(-19.4913610746823,-13.6760144633439,
122.199672820738)) ;
#96037 = CARTESIAN_POINT('Ctrl Pts',(-19.4861764172785,-13.6762597854933,
122.199332834716)) ;
#96038 = CARTESIAN_POINT('Ctrl Pts',(-19.4746055714863,-13.6768075002876,
122.198648585738)) ;
#96039 = CARTESIAN_POINT('Ctrl Pts',(-19.4682185271621,-13.6771099843821,
122.198321469393)) ;
#96040 = CARTESIAN_POINT('Ctrl Pts',(-19.4511035463345,-13.6779208911553,
122.197580355277)) ;
#96041 = CARTESIAN_POINT('Ctrl Pts',(-19.4403722228531,-13.6784297275162,
122.197258099531)) ;
#96042 = CARTESIAN_POINT('Ctrl Pts',(-19.4038573081181,-13.6801616749163,
122.196645835341)) ;
#96043 = CARTESIAN_POINT('Ctrl Pts',(-19.3780691337557,-13.6813849840632,
122.197034381386)) ;
#96044 = CARTESIAN_POINT('Ctrl Pts',(-19.3426925684915,-13.6830594541963,
122.198694692533)) ;
#96045 = CARTESIAN_POINT('Ctrl Pts',(-19.3330780383093,-13.6835143184019,
122.199260568802)) ;
#96046 = CARTESIAN_POINT('Ctrl Pts',(-19.3144357599424,-13.6843961940493,
122.200580386497)) ;
#96047 = CARTESIAN_POINT('Ctrl Pts',(-19.3054077083509,-13.6848232259916,
122.201321100333)) ;
#96048 = CARTESIAN_POINT('Ctrl Pts',(-19.2630785486813,-13.6868261288978,
122.205271060711)) ;
#96049 = CARTESIAN_POINT('Ctrl Pts',(-19.2299110143255,-13.6883969627554,
122.209753954854)) ;
#96050 = CARTESIAN_POINT('Ctrl Pts',(-19.1905066978994,-13.6902829323177,
122.216747141867)) ;
#96051 = CARTESIAN_POINT('Ctrl Pts',(-19.1840518985177,-13.690592537616,122.217946739341)) ;
#96052 = CARTESIAN_POINT('Ctrl Pts',(-19.172206799988,-13.6911621852162,122.220247581481)) ;
#96053 = CARTESIAN_POINT('Ctrl Pts',(-19.1668136442431,-13.6914221133092,
122.221333234725)) ;
#96054 = CARTESIAN_POINT('Ctrl Pts',(-19.1399645675824,-13.6927185803384,
122.226928021789)) ;
#96055 = CARTESIAN_POINT('Ctrl Pts',(-19.1186260691845,-13.6937564904465,
122.231980740695)) ;
#96056 = CARTESIAN_POINT('Ctrl Pts',(-19.0974359581966,-13.6947924657248,
122.23760810103)) ;
#96057 = CARTESIAN_POINT('Origin',(-19.4092696390481,30.19753203383,123.411833654989)) ;
#96058 = CARTESIAN_POINT('',(-20.5587133983317,-13.2308616644972,123.018355650104)) ;
#96059 = CARTESIAN_POINT('',(-20.5587133983317,-13.2488777185652,123.018355650104)) ;
#96060 = CARTESIAN_POINT('',(-20.5587133983318,30.19753203383,123.018355650104)) ;
#96061 = CARTESIAN_POINT('Ctrl Pts',(-20.5587133983318,-13.5907660201144,
123.018355650104)) ;
#96062 = CARTESIAN_POINT('Ctrl Pts',(-20.56593732345,-13.5897076635949,123.039458470443)) ;
#96063 = CARTESIAN_POINT('Ctrl Pts',(-20.5726734285229,-13.5886447944098,
123.061046089787)) ;
#96064 = CARTESIAN_POINT('Ctrl Pts',(-20.5788143718832,-13.5875842682099,
123.082879229601)) ;
#96065 = CARTESIAN_POINT('Ctrl Pts',(-20.5844670252955,-13.5866080685136,
123.10297633277)) ;
#96066 = CARTESIAN_POINT('Ctrl Pts',(-20.5896157919086,-13.5856338540164,
123.123280967438)) ;
#96067 = CARTESIAN_POINT('Ctrl Pts',(-20.5942142847724,-13.5846669715988,
123.143594801252)) ;
#96068 = CARTESIAN_POINT('Ctrl Pts',(-20.6024121753676,-13.582943277225,123.179808967961)) ;
#96069 = CARTESIAN_POINT('Ctrl Pts',(-20.6089969640239,-13.581195662089,123.216626237646)) ;
#96070 = CARTESIAN_POINT('Ctrl Pts',(-20.613873868681,-13.5794267489624,123.253800284983)) ;
#96071 = CARTESIAN_POINT('Ctrl Pts',(-20.6181206868664,-13.5778863759261,
123.286171518656)) ;
#96072 = CARTESIAN_POINT('Ctrl Pts',(-20.6210730667175,-13.5763298527071,
123.318812691199)) ;
#96073 = CARTESIAN_POINT('Ctrl Pts',(-20.6226995289543,-13.5747589111888,
123.351552659914)) ;
#96074 = CARTESIAN_POINT('Ctrl Pts',(-20.6262189702516,-13.5713596091144,
123.422397463664)) ;
#96075 = CARTESIAN_POINT('Ctrl Pts',(-20.6235258528076,-13.568019599761,123.493434316554)) ;
#96076 = CARTESIAN_POINT('Ctrl Pts',(-20.6146534922241,-13.5647273358169,
123.563806226816)) ;
#96077 = CARTESIAN_POINT('Ctrl Pts',(-20.6066941938399,-13.561773881565,123.626936103738)) ;
#96078 = CARTESIAN_POINT('Ctrl Pts',(-20.5937805912982,-13.5587726665141,
123.68936523936)) ;
#96079 = CARTESIAN_POINT('Ctrl Pts',(-20.5760569392211,-13.555742631866,123.750438575568)) ;
#96080 = CARTESIAN_POINT('Ctrl Pts',(-20.5742064981929,-13.5554262805629,
123.756814948031)) ;
#96081 = CARTESIAN_POINT('Ctrl Pts',(-20.5723036709229,-13.5551096151135,
123.763176552808)) ;
#96082 = CARTESIAN_POINT('Ctrl Pts',(-20.5703486535344,-13.554792657074,123.769522651472)) ;
#96083 = CARTESIAN_POINT('Ctrl Pts',(-20.5533588564485,-13.5520381788753,
123.824672508053)) ;
#96084 = CARTESIAN_POINT('Ctrl Pts',(-20.5324454793954,-13.5493260681323,
123.878578509422)) ;
#96085 = CARTESIAN_POINT('Ctrl Pts',(-20.5078026319292,-13.5466198502774,
123.930747096362)) ;
#96086 = CARTESIAN_POINT('Ctrl Pts',(-20.5021696792017,-13.5460012530447,
123.942671983877)) ;
#96087 = CARTESIAN_POINT('Ctrl Pts',(-20.4963420590768,-13.5453829637184,
123.954506171273)) ;
#96088 = CARTESIAN_POINT('Ctrl Pts',(-20.4903224440844,-13.5447645466604,
123.966243908149)) ;
#96089 = CARTESIAN_POINT('Ctrl Pts',(-20.4636757803969,-13.54202703747,124.018202634309)) ;
#96090 = CARTESIAN_POINT('Ctrl Pts',(-20.4332959442728,-13.5392673299222,
124.068205889822)) ;
#96091 = CARTESIAN_POINT('Ctrl Pts',(-20.3994679607172,-13.5365087036993,
124.115789036991)) ;
#96092 = CARTESIAN_POINT('Ctrl Pts',(-20.3922732090164,-13.5359219814469,
124.125909324783)) ;
#96093 = CARTESIAN_POINT('Ctrl Pts',(-20.3849226376165,-13.5353353081087,
124.135920237148)) ;
#96094 = CARTESIAN_POINT('Ctrl Pts',(-20.3774192467102,-13.534748907658,124.145817464939)) ;
#96095 = CARTESIAN_POINT('Ctrl Pts',(-20.3386338088895,-13.5317177716687,
124.196976776494)) ;
#96096 = CARTESIAN_POINT('Ctrl Pts',(-20.2958246690734,-13.528693211446,124.245013289959)) ;
#96097 = CARTESIAN_POINT('Ctrl Pts',(-20.249447641988,-13.5256682001997,124.289413747893)) ;
#96098 = CARTESIAN_POINT('Ctrl Pts',(-20.2448685657576,-13.5253695230752,
124.293797665844)) ;
#96099 = CARTESIAN_POINT('Ctrl Pts',(-20.2402547389873,-13.5250708415537,
124.298146163806)) ;
#96100 = CARTESIAN_POINT('Ctrl Pts',(-20.2356066219666,-13.5247721488716,
124.302458765092)) ;
#96101 = CARTESIAN_POINT('Ctrl Pts',(-20.183843586898,-13.5214458040943,124.350485381162)) ;
#96102 = CARTESIAN_POINT('Ctrl Pts',(-20.127976706822,-13.5181307274801,124.393921453457)) ;
#96103 = CARTESIAN_POINT('Ctrl Pts',(-20.0686432308458,-13.5147860917316,
124.432261194075)) ;
#96104 = CARTESIAN_POINT('Ctrl Pts',(-20.0406935936576,-13.5132105670525,
124.450321518749)) ;
#96105 = CARTESIAN_POINT('Ctrl Pts',(-20.0120340287551,-13.5116375405296,
124.467207643775)) ;
#96106 = CARTESIAN_POINT('Ctrl Pts',(-19.9828868068577,-13.5100766230102,
124.482818828033)) ;
#96107 = CARTESIAN_POINT('Ctrl Pts',(-19.9536176487585,-13.5085091754568,
124.498495321037)) ;
#96108 = CARTESIAN_POINT('Ctrl Pts',(-19.9238573504429,-13.5069539384339,
124.51288597522)) ;
#96109 = CARTESIAN_POINT('Ctrl Pts',(-19.8938494319314,-13.5054206439141,
124.525937923186)) ;
#96110 = CARTESIAN_POINT('Ctrl Pts',(-19.8902157103964,-13.5052349740779,
124.527518410829)) ;
#96111 = CARTESIAN_POINT('Ctrl Pts',(-19.886578373474,-13.505049625991,124.529079329428)) ;
#96112 = CARTESIAN_POINT('Ctrl Pts',(-19.8829378650492,-13.5048646169337,
124.530620635501)) ;
#96113 = CARTESIAN_POINT('Ctrl Pts',(-19.8665940013421,-13.5040340288771,
124.53754024492)) ;
#96114 = CARTESIAN_POINT('Ctrl Pts',(-19.8498855391435,-13.5031929130003,
124.544187172173)) ;
#96115 = CARTESIAN_POINT('Ctrl Pts',(-19.8330955607533,-13.5023530749188,
124.550436959119)) ;
#96116 = CARTESIAN_POINT('Ctrl Pts',(-19.8230237579344,-13.5018492813248,
124.554186018249)) ;
#96117 = CARTESIAN_POINT('Ctrl Pts',(-19.8129230379855,-13.5013459475376,
124.557793087623)) ;
#96118 = CARTESIAN_POINT('Ctrl Pts',(-19.8028576452835,-13.500845621912,124.561239752691)) ;
#96119 = CARTESIAN_POINT('Ctrl Pts',(-19.7819722926047,-13.499807462999,124.568391467247)) ;
#96120 = CARTESIAN_POINT('Ctrl Pts',(-19.7606464564749,-13.4987524949004,
124.575053463302)) ;
#96121 = CARTESIAN_POINT('Ctrl Pts',(-19.7391236596882,-13.4976925462973,
124.581124987871)) ;
#96122 = CARTESIAN_POINT('Ctrl Pts',(-19.7213339213807,-13.4968164423014,
124.586143426426)) ;
#96123 = CARTESIAN_POINT('Ctrl Pts',(-19.7034101220554,-13.495936935673,124.590759277656)) ;
#96124 = CARTESIAN_POINT('Ctrl Pts',(-19.6854975315309,-13.4950607059879,
124.594941446993)) ;
#96125 = CARTESIAN_POINT('Ctrl Pts',(-19.6502490847657,-13.4933364587125,
124.603171131751)) ;
#96126 = CARTESIAN_POINT('Ctrl Pts',(-19.6143838979347,-13.4916076553557,
124.609879314588)) ;
#96127 = CARTESIAN_POINT('Ctrl Pts',(-19.5781418159829,-13.4898815149819,
124.614966267772)) ;
#96128 = CARTESIAN_POINT('Ctrl Pts',(-19.5444166377919,-13.4882752498737,
124.619699947334)) ;
#96129 = CARTESIAN_POINT('Ctrl Pts',(-19.5103657241023,-13.4866712907194,
124.623030074038)) ;
#96130 = CARTESIAN_POINT('Ctrl Pts',(-19.4761936044083,-13.4850754545887,
124.624915300612)) ;
#96131 = CARTESIAN_POINT('Ctrl Pts',(-19.4056491671545,-13.4817810332065,
124.628807135503)) ;
#96132 = CARTESIAN_POINT('Ctrl Pts',(-19.3349063087448,-13.4784584750556,
124.626536071471)) ;
#96133 = CARTESIAN_POINT('Ctrl Pts',(-19.2647959442042,-13.475090394799,124.618139274467)) ;
#96134 = CARTESIAN_POINT('Ctrl Pts',(-19.2028468114975,-13.4721143775988,
124.610719910792)) ;
#96135 = CARTESIAN_POINT('Ctrl Pts',(-19.1415300759262,-13.4691715788272,
124.598531445015)) ;
#96136 = CARTESIAN_POINT('Ctrl Pts',(-19.0814715524571,-13.4662550237273,
124.581703011162)) ;
#96137 = CARTESIAN_POINT('Ctrl Pts',(-19.0733112299114,-13.4658587430837,
124.579416483951)) ;
#96138 = CARTESIAN_POINT('Ctrl Pts',(-19.0651741191567,-13.4654629469358,
124.577044373145)) ;
#96139 = CARTESIAN_POINT('Ctrl Pts',(-19.0570617756056,-13.465067617788,124.574587075545)) ;
#96140 = CARTESIAN_POINT('Ctrl Pts',(-19.000751634656,-13.4623235229539,124.557530256719)) ;
#96141 = CARTESIAN_POINT('Ctrl Pts',(-18.9457219239064,-13.4595504723728,
124.536390948226)) ;
#96142 = CARTESIAN_POINT('Ctrl Pts',(-18.89248914347,-13.4567592247754,124.511371655913)) ;
#96143 = CARTESIAN_POINT('Ctrl Pts',(-18.8819780049518,-13.4562080758425,
124.506431443416)) ;
#96144 = CARTESIAN_POINT('Ctrl Pts',(-18.8715368654157,-13.4556562174275,
124.501340105159)) ;
#96145 = CARTESIAN_POINT('Ctrl Pts',(-18.8611696110404,-13.4551037323577,
124.496099422863)) ;
#96146 = CARTESIAN_POINT('Ctrl Pts',(-18.8091740597987,-13.4523328187948,
124.469815495125)) ;
#96147 = CARTESIAN_POINT('Ctrl Pts',(-18.7591032718826,-13.4495960832786,
124.439803819648)) ;
#96148 = CARTESIAN_POINT('Ctrl Pts',(-18.7114210793505,-13.4468582140995,
124.406345235522)) ;
#96149 = CARTESIAN_POINT('Ctrl Pts',(-18.7010771382274,-13.4462642741801,
124.399086894286)) ;
#96150 = CARTESIAN_POINT('Ctrl Pts',(-18.6908455040754,-13.4456702809095,
124.391666504264)) ;
#96151 = CARTESIAN_POINT('Ctrl Pts',(-18.6807307419424,-13.4450758737854,
124.384087208076)) ;
#96152 = CARTESIAN_POINT('Ctrl Pts',(-18.6306582928725,-13.4421333013296,
124.346566412492)) ;
#96153 = CARTESIAN_POINT('Ctrl Pts',(-18.5835300614982,-13.4391667165854,
124.305206222441)) ;
#96154 = CARTESIAN_POINT('Ctrl Pts',(-18.5398291697829,-13.4362229685555,
124.260432009035)) ;
#96155 = CARTESIAN_POINT('Ctrl Pts',(-18.5342276903528,-13.4358456457278,
124.254692953708)) ;
#96156 = CARTESIAN_POINT('Ctrl Pts',(-18.5286824745029,-13.4354686980963,
124.248897860581)) ;
#96157 = CARTESIAN_POINT('Ctrl Pts',(-18.5231944998514,-13.4350922243203,
124.243047673027)) ;
#96158 = CARTESIAN_POINT('Ctrl Pts',(-18.4751530720707,-13.4317965936244,
124.191835453449)) ;
#96159 = CARTESIAN_POINT('Ctrl Pts',(-18.4316218927803,-13.4285013031375,
124.136533143445)) ;
#96160 = CARTESIAN_POINT('Ctrl Pts',(-18.3931030203371,-13.4251593702564,
124.077755046073)) ;
#96161 = CARTESIAN_POINT('Ctrl Pts',(-18.3736529244268,-13.4234718620055,
124.048075059126)) ;
#96162 = CARTESIAN_POINT('Ctrl Pts',(-18.3555348638421,-13.4217961608826,
124.017581885118)) ;
#96163 = CARTESIAN_POINT('Ctrl Pts',(-18.3388642863592,-13.4201356010657,
123.98653207766)) ;
#96164 = CARTESIAN_POINT('Ctrl Pts',(-18.3221937088763,-13.4184750412487,
123.955482270202)) ;
#96165 = CARTESIAN_POINT('Ctrl Pts',(-18.3069708268978,-13.4168296227376,
123.923876598611)) ;
#96166 = CARTESIAN_POINT('Ctrl Pts',(-18.2932530411003,-13.4152026797105,
123.891992846498)) ;
#96167 = CARTESIAN_POINT('Ctrl Pts',(-18.2858775697348,-13.4143279414774,
123.874850305842)) ;
#96168 = CARTESIAN_POINT('Ctrl Pts',(-18.2788149523104,-13.4134404278288,
123.857335977321)) ;
#96169 = CARTESIAN_POINT('Ctrl Pts',(-18.2721864213062,-13.4125540267446,
123.839721084128)) ;
#96170 = CARTESIAN_POINT('Ctrl Pts',(-18.2678851640197,-13.4119788406107,
123.828290770586)) ;
#96171 = CARTESIAN_POINT('Ctrl Pts',(-18.2637657227856,-13.4114041229464,
123.816818573283)) ;
#96172 = CARTESIAN_POINT('Ctrl Pts',(-18.2598502057626,-13.4108336684169,
123.805382714791)) ;
#96173 = CARTESIAN_POINT('Ctrl Pts',(-18.2529164488948,-13.4098234843241,
123.785131631245)) ;
#96174 = CARTESIAN_POINT('Ctrl Pts',(-18.2464401978026,-13.4087998151319,
123.764457090461)) ;
#96175 = CARTESIAN_POINT('Ctrl Pts',(-18.2405218051168,-13.4077755235016,
123.743608272412)) ;
#96176 = CARTESIAN_POINT('Ctrl Pts',(-18.2358570076826,-13.4069681906289,
123.727175514718)) ;
#96177 = CARTESIAN_POINT('Ctrl Pts',(-18.2315378594555,-13.4061604710741,
123.710634973009)) ;
#96178 = CARTESIAN_POINT('Ctrl Pts',(-18.2275915825149,-13.4053586630578,
123.694115193161)) ;
#96179 = CARTESIAN_POINT('Ctrl Pts',(-18.2193649561818,-13.4036871698909,
123.659677149923)) ;
#96180 = CARTESIAN_POINT('Ctrl Pts',(-18.212586452156,-13.4020080189065,123.624621081852)) ;
#96181 = CARTESIAN_POINT('Ctrl Pts',(-18.2073572834588,-13.400320627094,123.589182423146)) ;
#96182 = CARTESIAN_POINT('Ctrl Pts',(-18.2023294815898,-13.3986982140109,
123.555108449864)) ;
#96183 = CARTESIAN_POINT('Ctrl Pts',(-18.1987338885547,-13.3970681825614,
123.520681412362)) ;
#96184 = CARTESIAN_POINT('Ctrl Pts',(-18.1966167882638,-13.3954300145273,
123.486123355283)) ;
#96185 = CARTESIAN_POINT('Ctrl Pts',(-18.1922918737684,-13.3920834859253,
123.415526490959)) ;
#96186 = CARTESIAN_POINT('Ctrl Pts',(-18.1941415226558,-13.388742198361,123.344682672193)) ;
#96187 = CARTESIAN_POINT('Ctrl Pts',(-18.2021385235879,-13.3854302875451,
123.274427810234)) ;
#96188 = CARTESIAN_POINT('Ctrl Pts',(-18.2092990642338,-13.3824647918281,
123.211521378324)) ;
#96189 = CARTESIAN_POINT('Ctrl Pts',(-18.2213731434422,-13.3794885282211,
123.149245864423)) ;
#96190 = CARTESIAN_POINT('Ctrl Pts',(-18.238227509507,-13.3764859557225,123.088250239276)) ;
#96191 = CARTESIAN_POINT('Ctrl Pts',(-18.2401260273587,-13.3761477384637,
123.081379539852)) ;
#96192 = CARTESIAN_POINT('Ctrl Pts',(-18.2420851460551,-13.375809187389,123.074525068168)) ;
#96193 = CARTESIAN_POINT('Ctrl Pts',(-18.2441046345441,-13.3754702802864,
123.067687743544)) ;
#96194 = CARTESIAN_POINT('Ctrl Pts',(-18.2604997135887,-13.3727188861753,
123.01217939167)) ;
#96195 = CARTESIAN_POINT('Ctrl Pts',(-18.2808555539981,-13.3699925972808,
122.957877743366)) ;
#96196 = CARTESIAN_POINT('Ctrl Pts',(-18.3049820365015,-13.3672751518648,
122.905281794913)) ;
#96197 = CARTESIAN_POINT('Ctrl Pts',(-18.3104099938304,-13.3666637831019,
122.893448799206)) ;
#96198 = CARTESIAN_POINT('Ctrl Pts',(-18.3160286105546,-13.3660528619574,
122.881702062166)) ;
#96199 = CARTESIAN_POINT('Ctrl Pts',(-18.3218353836545,-13.3654422032513,
122.870047132195)) ;
#96200 = CARTESIAN_POINT('Ctrl Pts',(-18.3479168374066,-13.3626993947193,
122.817698347116)) ;
#96201 = CARTESIAN_POINT('Ctrl Pts',(-18.3777659981092,-13.3599341452412,
122.767267441824)) ;
#96202 = CARTESIAN_POINT('Ctrl Pts',(-18.4111023296304,-13.357172146824,122.719224155708)) ;
#96203 = CARTESIAN_POINT('Ctrl Pts',(-18.417959821757,-13.3566039864556,122.709341350935)) ;
#96204 = CARTESIAN_POINT('Ctrl Pts',(-18.4249647234089,-13.356035963656,122.699559487071)) ;
#96205 = CARTESIAN_POINT('Ctrl Pts',(-18.4321143587216,-13.3554683020607,
122.689882511064)) ;
#96206 = CARTESIAN_POINT('Ctrl Pts',(-18.4706634727333,-13.35240760727,122.63770658389)) ;
#96207 = CARTESIAN_POINT('Ctrl Pts',(-18.5133604462358,-13.3493587902268,
122.588667559195)) ;
#96208 = CARTESIAN_POINT('Ctrl Pts',(-18.5597444718207,-13.3462943624018,
122.543298747037)) ;
#96209 = CARTESIAN_POINT('Ctrl Pts',(-18.5637142504198,-13.3460320932295,
122.539415855518)) ;
#96210 = CARTESIAN_POINT('Ctrl Pts',(-18.5677110113616,-13.3457697097113,
122.535559827728)) ;
#96211 = CARTESIAN_POINT('Ctrl Pts',(-18.5717344516033,-13.345507194615,122.531730987185)) ;
#96212 = CARTESIAN_POINT('Ctrl Pts',(-18.623082789129,-13.3421568991061,122.482866188715)) ;
#96213 = CARTESIAN_POINT('Ctrl Pts',(-18.6786228698299,-13.338828645327,122.438576979517)) ;
#96214 = CARTESIAN_POINT('Ctrl Pts',(-18.7377100724562,-13.3354839544011,
122.399384325589)) ;
#96215 = CARTESIAN_POINT('Ctrl Pts',(-18.767244422085,-13.333812132639,122.379794135284)) ;
#96216 = CARTESIAN_POINT('Ctrl Pts',(-18.7976016312454,-13.3321383322381,
122.361524896854)) ;
#96217 = CARTESIAN_POINT('Ctrl Pts',(-18.8285361720955,-13.3304754178574,
122.344690489127)) ;
#96218 = CARTESIAN_POINT('Ctrl Pts',(-18.8594707129456,-13.3288125034767,
122.327856081401)) ;
#96219 = CARTESIAN_POINT('Ctrl Pts',(-18.8909818700569,-13.3271604751162,
122.312456715393)) ;
#96220 = CARTESIAN_POINT('Ctrl Pts',(-18.9228035874227,-13.3255321974351,
122.298551715541)) ;
#96221 = CARTESIAN_POINT('Ctrl Pts',(-18.9407277043713,-13.3246150426742,
122.290719490755)) ;
#96222 = CARTESIAN_POINT('Ctrl Pts',(-18.9590307252784,-13.3236891386708,
122.283241963262)) ;
#96223 = CARTESIAN_POINT('Ctrl Pts',(-18.9774515078905,-13.3227643623052,
122.276237336887)) ;
#96224 = CARTESIAN_POINT('Ctrl Pts',(-18.9901971670677,-13.3221244934886,
122.271390714334)) ;
#96225 = CARTESIAN_POINT('Ctrl Pts',(-19.0029987077064,-13.3214851645282,
122.266769512102)) ;
#96226 = CARTESIAN_POINT('Ctrl Pts',(-19.0157644887606,-13.3208496471916,
122.262399188488)) ;
#96227 = CARTESIAN_POINT('Ctrl Pts',(-19.0351967286771,-13.3198822543386,
122.255746624369)) ;
#96228 = CARTESIAN_POINT('Ctrl Pts',(-19.0550311200099,-13.3188995497272,
122.249511485614)) ;
#96229 = CARTESIAN_POINT('Ctrl Pts',(-19.0750103150925,-13.3179143486395,
122.243794015065)) ;
#96230 = CARTESIAN_POINT('Ctrl Pts',(-19.0898815241755,-13.3171810292388,
122.23953830308)) ;
#96231 = CARTESIAN_POINT('Ctrl Pts',(-19.1048325016901,-13.3164463267048,
122.235568416248)) ;
#96232 = CARTESIAN_POINT('Ctrl Pts',(-19.1197517969606,-13.3157155258924,
122.231907676295)) ;
#96233 = CARTESIAN_POINT('Ctrl Pts',(-19.1535484259518,-13.3140600452897,
122.223615014491)) ;
#96234 = CARTESIAN_POINT('Ctrl Pts',(-19.1879779337239,-13.3123990969106,
122.216710989836)) ;
#96235 = CARTESIAN_POINT('Ctrl Pts',(-19.2228067269689,-13.3107371594226,
122.211301490279)) ;
#96236 = CARTESIAN_POINT('Ctrl Pts',(-19.2576355202139,-13.3090752219345,
122.205891990722)) ;
#96237 = CARTESIAN_POINT('Ctrl Pts',(-19.2928629740217,-13.3074122953375,
122.20197725082)) ;
#96238 = CARTESIAN_POINT('Ctrl Pts',(-19.3282401173873,-13.3057528582991,
122.199612506558)) ;
#96239 = CARTESIAN_POINT('Ctrl Pts',(-19.398630865178,-13.3024510367574,122.194907318375)) ;
#96240 = CARTESIAN_POINT('Ctrl Pts',(-19.4692861473342,-13.2991176447074,
122.196343939404)) ;
#96241 = CARTESIAN_POINT('Ctrl Pts',(-19.5393882913664,-13.2957819799608,
122.203895315336)) ;
#96242 = CARTESIAN_POINT('Ctrl Pts',(-19.6019322760329,-13.2928059545104,
122.210632529255)) ;
#96243 = CARTESIAN_POINT('Ctrl Pts',(-19.6638875199564,-13.2898555176066,
122.222224583108)) ;
#96244 = CARTESIAN_POINT('Ctrl Pts',(-19.7246141366804,-13.2868881760099,
122.238546075622)) ;
#96245 = CARTESIAN_POINT('Ctrl Pts',(-19.73207549509,-13.2865235846599,122.240551464889)) ;
#96246 = CARTESIAN_POINT('Ctrl Pts',(-19.7395183186333,-13.2861587381073,
122.242628189198)) ;
#96247 = CARTESIAN_POINT('Ctrl Pts',(-19.7469414304181,-13.2857935575323,
122.244775962586)) ;
#96248 = CARTESIAN_POINT('Ctrl Pts',(-19.8029632309156,-13.2830375605983,
122.260985085625)) ;
#96249 = CARTESIAN_POINT('Ctrl Pts',(-19.857779407027,-13.2802762462415,122.281221360628)) ;
#96250 = CARTESIAN_POINT('Ctrl Pts',(-19.910881366359,-13.2775362339649,122.305293293724)) ;
#96251 = CARTESIAN_POINT('Ctrl Pts',(-19.9221620488068,-13.2769541611226,
122.310407000197)) ;
#96252 = CARTESIAN_POINT('Ctrl Pts',(-19.9333654396209,-13.2763730496086,
122.315693629464)) ;
#96253 = CARTESIAN_POINT('Ctrl Pts',(-19.9444867734003,-13.275793154619,122.32115106359)) ;
#96254 = CARTESIAN_POINT('Ctrl Pts',(-19.9974395521089,-13.2730320603416,
122.347135923622)) ;
#96255 = CARTESIAN_POINT('Ctrl Pts',(-20.0484651131994,-13.2702660520457,
122.376964792411)) ;
#96256 = CARTESIAN_POINT('Ctrl Pts',(-20.0970822215966,-13.2674654035197,
122.410354874698)) ;
#96257 = CARTESIAN_POINT('Ctrl Pts',(-20.10654387841,-13.2669203531027,122.416853111841)) ;
#96258 = CARTESIAN_POINT('Ctrl Pts',(-20.1159143949477,-13.2663739906764,
122.42348609493)) ;
#96259 = CARTESIAN_POINT('Ctrl Pts',(-20.1251903403651,-13.265826097125,122.430251541506)) ;
#96260 = CARTESIAN_POINT('Ctrl Pts',(-20.1753445951763,-13.2628636828859,
122.466831740743)) ;
#96261 = CARTESIAN_POINT('Ctrl Pts',(-20.2226472254636,-13.2599278644311,
122.507226244186)) ;
#96262 = CARTESIAN_POINT('Ctrl Pts',(-20.266620420239,-13.2570325479737,122.55102268034)) ;
#96263 = CARTESIAN_POINT('Ctrl Pts',(-20.2728768835143,-13.2566206051713,
122.557253994571)) ;
#96264 = CARTESIAN_POINT('Ctrl Pts',(-20.2790660044712,-13.2562094822639,
122.563554110306)) ;
#96265 = CARTESIAN_POINT('Ctrl Pts',(-20.2851864621822,-13.255799219304,122.569921774187)) ;
#96266 = CARTESIAN_POINT('Ctrl Pts',(-20.3338878536137,-13.2525346959724,
122.620590221845)) ;
#96267 = CARTESIAN_POINT('Ctrl Pts',(-20.3781259396579,-13.2492233617159,
122.675416282898)) ;
#96268 = CARTESIAN_POINT('Ctrl Pts',(-20.4173808066979,-13.2458562753417,
122.733779254705)) ;
#96269 = CARTESIAN_POINT('Ctrl Pts',(-20.43718409816,-13.244157647939,122.76322220098)) ;
#96270 = CARTESIAN_POINT('Ctrl Pts',(-20.455667001888,-13.24247686509,122.793495317731)) ;
#96271 = CARTESIAN_POINT('Ctrl Pts',(-20.4727206302616,-13.240815458859,122.824366306644)) ;
#96272 = CARTESIAN_POINT('Ctrl Pts',(-20.4897742586351,-13.239154052628,122.855237295557)) ;
#96273 = CARTESIAN_POINT('Ctrl Pts',(-20.5053984145253,-13.237512023015,122.886705511631)) ;
#96274 = CARTESIAN_POINT('Ctrl Pts',(-20.5195341424226,-13.235890902084,122.918519729956)) ;
#96275 = CARTESIAN_POINT('Ctrl Pts',(-20.5278248514833,-13.2349401026566,
122.937179004529)) ;
#96276 = CARTESIAN_POINT('Ctrl Pts',(-20.5357182017675,-13.2339772581505,
122.956222346134)) ;
#96277 = CARTESIAN_POINT('Ctrl Pts',(-20.5430988792399,-13.2330133138736,
122.97539677505)) ;
#96278 = CARTESIAN_POINT('Ctrl Pts',(-20.548597300709,-13.2322951993201,122.989681248529)) ;
#96279 = CARTESIAN_POINT('Ctrl Pts',(-20.5538121555756,-13.2315764744071,
123.004037942814)) ;
#96280 = CARTESIAN_POINT('Ctrl Pts',(-20.5587133983318,-13.2308616644972,
123.018355650104)) ;
#96281 = CARTESIAN_POINT('Ctrl Pts',(-20.5587133983318,-13.2488777185653,
123.018355650104)) ;
#96282 = CARTESIAN_POINT('Ctrl Pts',(-20.5452279189122,-13.2508290942128,
122.978961325726)) ;
#96283 = CARTESIAN_POINT('Ctrl Pts',(-20.5297301971886,-13.2527525899432,
122.940295905666)) ;
#96284 = CARTESIAN_POINT('Ctrl Pts',(-20.5095423363804,-13.2550063846824,
122.896578057874)) ;
#96285 = CARTESIAN_POINT('Ctrl Pts',(-20.5067635720036,-13.2553117377111,
122.890685494264)) ;
#96286 = CARTESIAN_POINT('Ctrl Pts',(-20.5020290479444,-13.2558240965181,
122.88085142619)) ;
#96287 = CARTESIAN_POINT('Ctrl Pts',(-20.5000990252097,-13.2560308412582,
122.876897674573)) ;
#96288 = CARTESIAN_POINT('Ctrl Pts',(-20.496503383061,-13.2564121726585,122.869632195151)) ;
#96289 = CARTESIAN_POINT('Ctrl Pts',(-20.4948439998353,-13.2565866950533,
122.866317436836)) ;
#96290 = CARTESIAN_POINT('Ctrl Pts',(-20.491479949231,-13.2569376014485,122.859673597664)) ;
#96291 = CARTESIAN_POINT('Ctrl Pts',(-20.4897750275258,-13.2571139862273,
122.856344690437)) ;
#96292 = CARTESIAN_POINT('Ctrl Pts',(-20.4857206208597,-13.257530039289,122.848517639968)) ;
#96293 = CARTESIAN_POINT('Ctrl Pts',(-20.4833582732193,-13.2577698252515,
122.8440262451)) ;
#96294 = CARTESIAN_POINT('Ctrl Pts',(-20.4767904248743,-13.2584293153007,
122.831726839407)) ;
#96295 = CARTESIAN_POINT('Ctrl Pts',(-20.4725274737423,-13.2588494982383,
122.823949889647)) ;
#96296 = CARTESIAN_POINT('Ctrl Pts',(-20.4576190442211,-13.2602920980988,
122.797444963399)) ;
#96297 = CARTESIAN_POINT('Ctrl Pts',(-20.4465608370239,-13.2613170415191,
122.778953804338)) ;
#96298 = CARTESIAN_POINT('Ctrl Pts',(-20.4279237797055,-13.2629680183823,
122.749591377065)) ;
#96299 = CARTESIAN_POINT('Ctrl Pts',(-20.4206484766444,-13.2635951307028,
122.738532873673)) ;
#96300 = CARTESIAN_POINT('Ctrl Pts',(-20.4093533352545,-13.264543605474,122.721960479056)) ;
#96301 = CARTESIAN_POINT('Ctrl Pts',(-20.4054653968743,-13.2648657930848,
122.716357982697)) ;
#96302 = CARTESIAN_POINT('Ctrl Pts',(-20.3978360316589,-13.265489960892,122.705559362354)) ;
#96303 = CARTESIAN_POINT('Ctrl Pts',(-20.3941002904594,-13.265791963121,122.700359497099)) ;
#96304 = CARTESIAN_POINT('Ctrl Pts',(-20.3837717953175,-13.2666173422878,
122.686220248648)) ;
#96305 = CARTESIAN_POINT('Ctrl Pts',(-20.3770972736061,-13.2671402774034,
122.67734135497)) ;
#96306 = CARTESIAN_POINT('Ctrl Pts',(-20.3552772496752,-13.2688184635994,
122.64912884871)) ;
#96307 = CARTESIAN_POINT('Ctrl Pts',(-20.339667029652,-13.2699719973207,122.630162552814)) ;
#96308 = CARTESIAN_POINT('Ctrl Pts',(-20.3199874548715,-13.2713795727534,
122.607677399147)) ;
#96309 = CARTESIAN_POINT('Ctrl Pts',(-20.3164558539442,-13.2716304389984,
122.603695427217)) ;
#96310 = CARTESIAN_POINT('Ctrl Pts',(-20.3094084211521,-13.272127815255,122.595853675899)) ;
#96311 = CARTESIAN_POINT('Ctrl Pts',(-20.3058936556296,-13.272374316978,122.591993105779)) ;
#96312 = CARTESIAN_POINT('Ctrl Pts',(-20.2907416573438,-13.2734306446195,
122.575564345389)) ;
#96313 = CARTESIAN_POINT('Ctrl Pts',(-20.2788642600619,-13.2742425074191,
122.563220391595)) ;
#96314 = CARTESIAN_POINT('Ctrl Pts',(-20.2594855277182,-13.2755382049922,
122.543914646525)) ;
#96315 = CARTESIAN_POINT('Ctrl Pts',(-20.2521503411841,-13.2760223642858,
122.536789321623)) ;
#96316 = CARTESIAN_POINT('Ctrl Pts',(-20.2388893579011,-13.2768861789263,
122.524229212362)) ;
#96317 = CARTESIAN_POINT('Ctrl Pts',(-20.2329979123172,-13.2772660253462,
122.518759046178)) ;
#96318 = CARTESIAN_POINT('Ctrl Pts',(-20.2238405185812,-13.2778504294636,
122.510424179245)) ;
#96319 = CARTESIAN_POINT('Ctrl Pts',(-20.2206127837743,-13.2780552885428,
122.507517857075)) ;
#96320 = CARTESIAN_POINT('Ctrl Pts',(-20.2164689059155,-13.2783168677851,
122.50382666473)) ;
#96321 = CARTESIAN_POINT('Ctrl Pts',(-20.2155670885947,-13.2783737087306,
122.503025768994)) ;
#96322 = CARTESIAN_POINT('Ctrl Pts',(-20.2094923989091,-13.2787560187135,
122.49764705165)) ;
#96323 = CARTESIAN_POINT('Ctrl Pts',(-20.2042817487532,-13.2790811536934,
122.493112066599)) ;
#96324 = CARTESIAN_POINT('Ctrl Pts',(-20.1797046034348,-13.2806020335944,
122.472087509413)) ;
#96325 = CARTESIAN_POINT('Ctrl Pts',(-20.1598620635089,-13.2817929044339,
122.456164323999)) ;
#96326 = CARTESIAN_POINT('Ctrl Pts',(-20.1288429091883,-13.2836117877989,
122.432834589954)) ;
#96327 = CARTESIAN_POINT('Ctrl Pts',(-20.1180194730722,-13.2842389932766,
122.424970679845)) ;
#96328 = CARTESIAN_POINT('Ctrl Pts',(-20.098657325909,-13.2853496854727,122.411385712189)) ;
#96329 = CARTESIAN_POINT('Ctrl Pts',(-20.0901717507945,-13.2858327116712,
122.405591247764)) ;
#96330 = CARTESIAN_POINT('Ctrl Pts',(-20.0813198350304,-13.2863330415229,
122.399709870731)) ;
#96331 = CARTESIAN_POINT('Ctrl Pts',(-20.0810258652794,-13.286349653317,122.399514736318)) ;
#96332 = CARTESIAN_POINT('Ctrl Pts',(-20.0803503627475,-13.2863878157348,
122.399066767766)) ;
#96333 = CARTESIAN_POINT('Ctrl Pts',(-20.079968772011,-13.2864093668911,122.398814021112)) ;
#96334 = CARTESIAN_POINT('Ctrl Pts',(-20.0791010724234,-13.2864583567751,
122.398240005412)) ;
#96335 = CARTESIAN_POINT('Ctrl Pts',(-20.0786148751351,-13.2864857963163,
122.397918870341)) ;
#96336 = CARTESIAN_POINT('Ctrl Pts',(-20.0726891438206,-13.2868200946508,
122.394011023188)) ;
#96337 = CARTESIAN_POINT('Ctrl Pts',(-20.0672210839812,-13.2871272164141,
122.390467782787)) ;
#96338 = CARTESIAN_POINT('Ctrl Pts',(-20.0551735473048,-13.2878010061905,
122.382798013752)) ;
#96339 = CARTESIAN_POINT('Ctrl Pts',(-20.0485824729291,-13.2881677743214,
122.378690243093)) ;
#96340 = CARTESIAN_POINT('Ctrl Pts',(-20.0193682636182,-13.2897854037625,
122.360869621958)) ;
#96341 = CARTESIAN_POINT('Ctrl Pts',(-19.9963401826866,-13.291039921831,122.347834643782)) ;
#96342 = CARTESIAN_POINT('Ctrl Pts',(-19.9624213071959,-13.2928542203253,
122.330071582362)) ;
#96343 = CARTESIAN_POINT('Ctrl Pts',(-19.9518578157841,-13.2934145623421,
122.324734753611)) ;
#96344 = CARTESIAN_POINT('Ctrl Pts',(-19.9335664927922,-13.2943768013482,
122.315826749552)) ;
#96345 = CARTESIAN_POINT('Ctrl Pts',(-19.9258760088059,-13.29477897744,122.312180897575)) ;
#96346 = CARTESIAN_POINT('Ctrl Pts',(-19.9100927445774,-13.2955996463423,
122.304900593367)) ;
#96347 = CARTESIAN_POINT('Ctrl Pts',(-19.9019971849016,-13.2960180845677,
122.30127336752)) ;
#96348 = CARTESIAN_POINT('Ctrl Pts',(-19.881591562157,-13.2970669189339,122.292397652228)) ;
#96349 = CARTESIAN_POINT('Ctrl Pts',(-19.8692331466275,-13.2976968097996,
122.287263276402)) ;
#96350 = CARTESIAN_POINT('Ctrl Pts',(-19.8366269253034,-13.2993468908501,
122.274344257024)) ;
#96351 = CARTESIAN_POINT('Ctrl Pts',(-19.816251137838,-13.3003661596876,122.266895911894)) ;
#96352 = CARTESIAN_POINT('Ctrl Pts',(-19.7952093167804,-13.301411994841,122.259836816864)) ;
#96353 = CARTESIAN_POINT('Ctrl Pts',(-19.7947315788093,-13.3014357362769,
122.259676876207)) ;
#96354 = CARTESIAN_POINT('Ctrl Pts',(-19.7939924368489,-13.3014724631405,
122.259429931966)) ;
#96355 = CARTESIAN_POINT('Ctrl Pts',(-19.7937311025063,-13.3014854474539,
122.259342720057)) ;
#96356 = CARTESIAN_POINT('Ctrl Pts',(-19.7929998688994,-13.3015217757983,
122.259098970818)) ;
#96357 = CARTESIAN_POINT('Ctrl Pts',(-19.7925299035945,-13.3015451209055,
122.258942631946)) ;
#96358 = CARTESIAN_POINT('Ctrl Pts',(-19.7874458548361,-13.3017976327867,
122.257254822225)) ;
#96359 = CARTESIAN_POINT('Ctrl Pts',(-19.7828227222355,-13.3020269514942,
122.255750775121)) ;
#96360 = CARTESIAN_POINT('Ctrl Pts',(-19.771971445687,-13.3025646731325,122.252292408037)) ;
#96361 = CARTESIAN_POINT('Ctrl Pts',(-19.7657363510388,-13.3028732777776,
122.250360458378)) ;
#96362 = CARTESIAN_POINT('Ctrl Pts',(-19.7421983407583,-13.3040364103773,
122.243274574793)) ;
#96363 = CARTESIAN_POINT('Ctrl Pts',(-19.7247968162017,-13.3048923275424,
122.238456288084)) ;
#96364 = CARTESIAN_POINT('Ctrl Pts',(-19.7018456831866,-13.3060132415451,
122.232648875728)) ;
#96365 = CARTESIAN_POINT('Ctrl Pts',(-19.6963874756617,-13.3062792426517,
122.231307995256)) ;
#96366 = CARTESIAN_POINT('Ctrl Pts',(-19.6845688350844,-13.3068539114095,
122.228491405647)) ;
#96367 = CARTESIAN_POINT('Ctrl Pts',(-19.6782054068235,-13.3071625137876,
122.227028996179)) ;
#96368 = CARTESIAN_POINT('Ctrl Pts',(-19.6715707489624,-13.3074834043972,
122.225560459392)) ;
#96369 = CARTESIAN_POINT('Ctrl Pts',(-19.671310991166,-13.3074959664199,122.225503053245)) ;
#96370 = CARTESIAN_POINT('Ctrl Pts',(-19.6707892985434,-13.3075211929882,
122.225387939534)) ;
#96371 = CARTESIAN_POINT('Ctrl Pts',(-19.670527363528,-13.3075338575202,122.225330233408)) ;
#96372 = CARTESIAN_POINT('Ctrl Pts',(-19.6699993133407,-13.3075593858785,
122.225214083576)) ;
#96373 = CARTESIAN_POINT('Ctrl Pts',(-19.6697331975372,-13.3075722496909,
122.22515564263)) ;
#96374 = CARTESIAN_POINT('Ctrl Pts',(-19.6691945495914,-13.3075982845586,
122.225037541583)) ;
#96375 = CARTESIAN_POINT('Ctrl Pts',(-19.6689220164501,-13.3076114555924,
122.224977885813)) ;
#96376 = CARTESIAN_POINT('Ctrl Pts',(-19.6662025976113,-13.3077428651083,
122.224383603845)) ;
#96377 = CARTESIAN_POINT('Ctrl Pts',(-19.663754082892,-13.3078610619803,122.223856451074)) ;
#96378 = CARTESIAN_POINT('Ctrl Pts',(-19.6559081312359,-13.3082394196596,
122.22219262743)) ;
#96379 = CARTESIAN_POINT('Ctrl Pts',(-19.6505045697393,-13.3084994073814,
122.221085138835)) ;
#96380 = CARTESIAN_POINT('Ctrl Pts',(-19.6379112359763,-13.3091039860922,
122.218593309143)) ;
#96381 = CARTESIAN_POINT('Ctrl Pts',(-19.6307161124811,-13.3094483945696,
122.21723708596)) ;
#96382 = CARTESIAN_POINT('Ctrl Pts',(-19.5986844749278,-13.3109774797526,
122.211498718937)) ;
#96383 = CARTESIAN_POINT('Ctrl Pts',(-19.5737273767555,-13.3121571060806,
122.207825516802)) ;
#96384 = CARTESIAN_POINT('Ctrl Pts',(-19.5360419008567,-13.3139324223016,
122.203472621454)) ;
#96385 = CARTESIAN_POINT('Ctrl Pts',(-19.5233877516588,-13.3145277690634,
122.202211958503)) ;
#96386 = CARTESIAN_POINT('Ctrl Pts',(-19.5040217264941,-13.3154394067243,
122.200589225338)) ;
#96387 = CARTESIAN_POINT('Ctrl Pts',(-19.4973227542694,-13.3157548402767,
122.200083814917)) ;
#96388 = CARTESIAN_POINT('Ctrl Pts',(-19.4847091544252,-13.3163491412989,
122.199237320485)) ;
#96389 = CARTESIAN_POINT('Ctrl Pts',(-19.4787955523003,-13.3166279166605,
122.198883887691)) ;
#96390 = CARTESIAN_POINT('Ctrl Pts',(-19.4728283087744,-13.316909423253,122.198571031223)) ;
#96391 = CARTESIAN_POINT('Ctrl Pts',(-19.4727770023954,-13.3169118436626,
122.198568344546)) ;
#96392 = CARTESIAN_POINT('Ctrl Pts',(-19.4726731322132,-13.3169167438317,
122.198562911952)) ;
#96393 = CARTESIAN_POINT('Ctrl Pts',(-19.4726205685759,-13.3169192235842,
122.198560166206)) ;
#96394 = CARTESIAN_POINT('Ctrl Pts',(-19.4725141618847,-13.3169242434791,
122.198554614816)) ;
#96395 = CARTESIAN_POINT('Ctrl Pts',(-19.4724603194284,-13.3169267835941,
122.198551809372)) ;
#96396 = CARTESIAN_POINT('Ctrl Pts',(-19.4723513346701,-13.3169319251801,
122.198546138029)) ;
#96397 = CARTESIAN_POINT('Ctrl Pts',(-19.472296192347,-13.316934526653,122.198543272305)) ;
#96398 = CARTESIAN_POINT('Ctrl Pts',(-19.4721845874617,-13.3169397919193,
122.198537479875)) ;
#96399 = CARTESIAN_POINT('Ctrl Pts',(-19.4721281245245,-13.3169424557313,
122.198534553331)) ;
#96400 = CARTESIAN_POINT('Ctrl Pts',(-19.4720138567241,-13.3169478467019,
122.198528638687)) ;
#96401 = CARTESIAN_POINT('Ctrl Pts',(-19.4719560520131,-13.316950573854,122.198525650786)) ;
#96402 = CARTESIAN_POINT('Ctrl Pts',(-19.4718586561757,-13.3169551688971,
122.198520623414)) ;
#96403 = CARTESIAN_POINT('Ctrl Pts',(-19.4718190650736,-13.3169570367767,
122.198518581746)) ;
#96404 = CARTESIAN_POINT('Ctrl Pts',(-19.4717354877619,-13.3169609799128,
122.198514275861)) ;
#96405 = CARTESIAN_POINT('Ctrl Pts',(-19.4716915014395,-13.3169630551768,
122.198512012093)) ;
#96406 = CARTESIAN_POINT('Ctrl Pts',(-19.4715986881943,-13.3169674341067,
122.198507240496)) ;
#96407 = CARTESIAN_POINT('Ctrl Pts',(-19.471549861426,-13.3169697377678,122.198504733231)) ;
#96408 = CARTESIAN_POINT('Ctrl Pts',(-19.4714468875836,-13.3169745961326,
122.198499451734)) ;
#96409 = CARTESIAN_POINT('Ctrl Pts',(-19.4713927402387,-13.3169771508522,
122.198496678168)) ;
#96410 = CARTESIAN_POINT('Ctrl Pts',(-19.4712786087018,-13.3169825357147,
122.198490839716)) ;
#96411 = CARTESIAN_POINT('Ctrl Pts',(-19.4712186244759,-13.3169853658631,
122.198487775655)) ;
#96412 = CARTESIAN_POINT('Ctrl Pts',(-19.4710922661237,-13.3169913276889,
122.198481330525)) ;
#96413 = CARTESIAN_POINT('Ctrl Pts',(-19.4710258922826,-13.3169944593576,
122.198477950471)) ;
#96414 = CARTESIAN_POINT('Ctrl Pts',(-19.4708861672507,-13.317001051956,122.198470846539)) ;
#96415 = CARTESIAN_POINT('Ctrl Pts',(-19.4708128158659,-13.3170045129005,
122.198467123859)) ;
#96416 = CARTESIAN_POINT('Ctrl Pts',(-19.4706585132213,-13.3170117934407,
122.198459306825)) ;
#96417 = CARTESIAN_POINT('Ctrl Pts',(-19.4705775618018,-13.3170156130507,
122.198455213916)) ;
#96418 = CARTESIAN_POINT('Ctrl Pts',(-19.4704074044744,-13.3170236418306,
122.198446627821)) ;
#96419 = CARTESIAN_POINT('Ctrl Pts',(-19.4703181984045,-13.3170278510162,
122.198442136367)) ;
#96420 = CARTESIAN_POINT('Ctrl Pts',(-19.4701308476873,-13.3170366912514,
122.198432724124)) ;
#96421 = CARTESIAN_POINT('Ctrl Pts',(-19.4700327031015,-13.3170413223079,
122.198427805412)) ;
#96422 = CARTESIAN_POINT('Ctrl Pts',(-19.4698267672242,-13.3170510397292,
122.198417509572)) ;
#96423 = CARTESIAN_POINT('Ctrl Pts',(-19.4697189757993,-13.3170561261119,
122.198412134899)) ;
#96424 = CARTESIAN_POINT('Ctrl Pts',(-19.4695332043355,-13.317064892277,122.198402896817)) ;
#96425 = CARTESIAN_POINT('Ctrl Pts',(-19.4694552247481,-13.3170685720056,
122.198399026567)) ;
#96426 = CARTESIAN_POINT('Ctrl Pts',(-19.4692558052216,-13.3170779823768,
122.198389148332)) ;
#96427 = CARTESIAN_POINT('Ctrl Pts',(-19.4691343646939,-13.3170837130981,
122.198383151058)) ;
#96428 = CARTESIAN_POINT('Ctrl Pts',(-19.4643233221868,-13.3173107473774,
122.198146284319)) ;
#96429 = CARTESIAN_POINT('Ctrl Pts',(-19.4596324317274,-13.317532242173,122.197942584631)) ;
#96430 = CARTESIAN_POINT('Ctrl Pts',(-19.4485946518937,-13.3180537602859,
122.197527364937)) ;
#96431 = CARTESIAN_POINT('Ctrl Pts',(-19.4422470599583,-13.318353936158,122.1973384051)) ;
#96432 = CARTESIAN_POINT('Ctrl Pts',(-19.4078742136445,-13.3199808549637,
122.19658484286)) ;
#96433 = CARTESIAN_POINT('Ctrl Pts',(-19.379837413508,-13.3213138766209,122.196940512794)) ;
#96434 = CARTESIAN_POINT('Ctrl Pts',(-19.3441762786893,-13.3230088080406,
122.198628153689)) ;
#96435 = CARTESIAN_POINT('Ctrl Pts',(-19.3365178624542,-13.3233727346108,
122.199063308476)) ;
#96436 = CARTESIAN_POINT('Ctrl Pts',(-19.3181185687875,-13.324246778642,122.200283675759)) ;
#96437 = CARTESIAN_POINT('Ctrl Pts',(-19.3073829902812,-13.3247565195504,
122.201139233532)) ;
#96438 = CARTESIAN_POINT('Ctrl Pts',(-19.293019930862,-13.3254382387744,122.202476277043)) ;
#96439 = CARTESIAN_POINT('Ctrl Pts',(-19.2893812370104,-13.325610922935,122.202831573367)) ;
#96440 = CARTESIAN_POINT('Ctrl Pts',(-19.2856312687237,-13.3257888746649,
122.20321483073)) ;
#96441 = CARTESIAN_POINT('Ctrl Pts',(-19.2855183411218,-13.3257942335413,
122.203226388243)) ;
#96442 = CARTESIAN_POINT('Ctrl Pts',(-19.2852895671704,-13.3258050897764,
122.203249834386)) ;
#96443 = CARTESIAN_POINT('Ctrl Pts',(-19.2851737208131,-13.3258105871349,
122.203261723856)) ;
#96444 = CARTESIAN_POINT('Ctrl Pts',(-19.2844652132305,-13.32584420849,122.203334541899)) ;
#96445 = CARTESIAN_POINT('Ctrl Pts',(-19.2838725950298,-13.3258723301368,
122.203395889775)) ;
#96446 = CARTESIAN_POINT('Ctrl Pts',(-19.2831419096539,-13.3259070031724,
122.203472073655)) ;
#96447 = CARTESIAN_POINT('Ctrl Pts',(-19.2830037998492,-13.3259135568482,
122.203486497415)) ;
#96448 = CARTESIAN_POINT('Ctrl Pts',(-19.282784117217,-13.3259239813473,122.203509478462)) ;
#96449 = CARTESIAN_POINT('Ctrl Pts',(-19.2827025428798,-13.3259278522518,
122.203518020323)) ;
#96450 = CARTESIAN_POINT('Ctrl Pts',(-19.2825241656159,-13.3259363166842,
122.20353671693)) ;
#96451 = CARTESIAN_POINT('Ctrl Pts',(-19.28242736301,-13.3259409101949,122.203546875053)) ;
#96452 = CARTESIAN_POINT('Ctrl Pts',(-19.2822150380999,-13.3259509854947,
122.203569181475)) ;
#96453 = CARTESIAN_POINT('Ctrl Pts',(-19.2820995163652,-13.325956467254,122.203581334704)) ;
#96454 = CARTESIAN_POINT('Ctrl Pts',(-19.2818451881675,-13.3259685356631,
122.203608127662)) ;
#96455 = CARTESIAN_POINT('Ctrl Pts',(-19.2817063826056,-13.325975122266,122.203622774732)) ;
#96456 = CARTESIAN_POINT('Ctrl Pts',(-19.2800546664106,-13.3260534993643,
122.203797355283)) ;
#96457 = CARTESIAN_POINT('Ctrl Pts',(-19.2785420542074,-13.3261252741542,
122.203960106505)) ;
#96458 = CARTESIAN_POINT('Ctrl Pts',(-19.2760351151975,-13.3262442293342,
122.204234607747)) ;
#96459 = CARTESIAN_POINT('Ctrl Pts',(-19.2750406140605,-13.3262914184424,
122.204344745683)) ;
#96460 = CARTESIAN_POINT('Ctrl Pts',(-19.2674370403143,-13.3266522074986,
122.205196327707)) ;
#96461 = CARTESIAN_POINT('Ctrl Pts',(-19.2608340087651,-13.3269655141319,
122.205990800528)) ;
#96462 = CARTESIAN_POINT('Ctrl Pts',(-19.2400189080934,-13.3279534243422,
122.208668824123)) ;
#96463 = CARTESIAN_POINT('Ctrl Pts',(-19.2258334691908,-13.328627019105,122.210749730574)) ;
#96464 = CARTESIAN_POINT('Ctrl Pts',(-19.1950137231925,-13.3300941772889,
122.215829521062)) ;
#96465 = CARTESIAN_POINT('Ctrl Pts',(-19.178398513466,-13.3308874664713,122.218925441671)) ;
#96466 = CARTESIAN_POINT('Ctrl Pts',(-19.1587678187261,-13.3318314596333,
122.223008745008)) ;
#96467 = CARTESIAN_POINT('Ctrl Pts',(-19.1556847898296,-13.3319799165575,
122.223662559242)) ;
#96468 = CARTESIAN_POINT('Ctrl Pts',(-19.1525705677369,-13.3321301057838,
122.2243356617)) ;
#96469 = CARTESIAN_POINT('Ctrl Pts',(-19.1525367913798,-13.3321317347397,
122.22434296357)) ;
#96470 = CARTESIAN_POINT('Ctrl Pts',(-19.1524674805703,-13.3321350774966,
122.224357950477)) ;
#96471 = CARTESIAN_POINT('Ctrl Pts',(-19.1524319467319,-13.332136791271,122.224365635541)) ;
#96472 = CARTESIAN_POINT('Ctrl Pts',(-19.152359031301,-13.3321403079983,122.224381408718)) ;
#96473 = CARTESIAN_POINT('Ctrl Pts',(-19.1523216494517,-13.3321421109668,
122.224389497064)) ;
#96474 = CARTESIAN_POINT('Ctrl Pts',(-19.1522449438167,-13.3321458106347,
122.224406097727)) ;
#96475 = CARTESIAN_POINT('Ctrl Pts',(-19.1522056199779,-13.3321477073404,
122.224414610253)) ;
#96476 = CARTESIAN_POINT('Ctrl Pts',(-19.1521249315099,-13.3321515992617,
122.224432081274)) ;
#96477 = CARTESIAN_POINT('Ctrl Pts',(-19.152083566793,-13.3321535944856,122.224441040007)) ;
#96478 = CARTESIAN_POINT('Ctrl Pts',(-19.1519986934808,-13.3321576884283,
122.224459426435)) ;
#96479 = CARTESIAN_POINT('Ctrl Pts',(-19.1519551843249,-13.3321597871785,
122.224468854493)) ;
#96480 = CARTESIAN_POINT('Ctrl Pts',(-19.1518659128665,-13.3321640934581,
122.224488203983)) ;
#96481 = CARTESIAN_POINT('Ctrl Pts',(-19.1518201519035,-13.3321663009278,
122.224498125391)) ;
#96482 = CARTESIAN_POINT('Ctrl Pts',(-19.151726264357,-13.332170830087,122.224518486779)) ;
#96483 = CARTESIAN_POINT('Ctrl Pts',(-19.1516781373138,-13.3321731518042,
122.224528927152)) ;
#96484 = CARTESIAN_POINT('Ctrl Pts',(-19.1515761616787,-13.3321780713736,
122.224551055587)) ;
#96485 = CARTESIAN_POINT('Ctrl Pts',(-19.1515223133528,-13.3321806692273,
122.224562744364)) ;
#96486 = CARTESIAN_POINT('Ctrl Pts',(-19.1514002517456,-13.3321865581166,
122.224589248791)) ;
#96487 = CARTESIAN_POINT('Ctrl Pts',(-19.1513320388879,-13.3321898491745,
122.22460406667)) ;
#96488 = CARTESIAN_POINT('Ctrl Pts',(-19.1472092463045,-13.3323887679583,
122.225500032993)) ;
#96489 = CARTESIAN_POINT('Ctrl Pts',(-19.1431592231712,-13.3325845907736,
122.226401936822)) ;
#96490 = CARTESIAN_POINT('Ctrl Pts',(-19.1310681853084,-13.3331703460153,
122.229159588206)) ;
#96491 = CARTESIAN_POINT('Ctrl Pts',(-19.1230413803994,-13.3335607030117,
122.231076533285)) ;
#96492 = CARTESIAN_POINT('Ctrl Pts',(-19.0996414403238,-13.3347022274925,
122.236917490937)) ;
#96493 = CARTESIAN_POINT('Ctrl Pts',(-19.0843248493894,-13.3354538525933,
122.241061047384)) ;
#96494 = CARTESIAN_POINT('Ctrl Pts',(-19.059968387753,-13.336654237335,122.248164935341)) ;
#96495 = CARTESIAN_POINT('Ctrl Pts',(-19.0508744979106,-13.3371036033445,
122.250933496963)) ;
#96496 = CARTESIAN_POINT('Ctrl Pts',(-19.041705455486,-13.3375577983117,122.253842946901)) ;
#96497 = CARTESIAN_POINT('Ctrl Pts',(-19.0415969020042,-13.3375631757452,
122.253877409058)) ;
#96498 = CARTESIAN_POINT('Ctrl Pts',(-19.0413792054089,-13.3375739601427,
122.253946554259)) ;
#96499 = CARTESIAN_POINT('Ctrl Pts',(-19.0412700622116,-13.3375793671126,
122.253981237516)) ;
#96500 = CARTESIAN_POINT('Ctrl Pts',(-19.0410510028819,-13.3375902196693,
122.254050883754)) ;
#96501 = CARTESIAN_POINT('Ctrl Pts',(-19.0409410870657,-13.3375956652427,
122.254085846879)) ;
#96502 = CARTESIAN_POINT('Ctrl Pts',(-19.0407202913764,-13.3376066044824,
122.254156114412)) ;
#96503 = CARTESIAN_POINT('Ctrl Pts',(-19.0406094112717,-13.3376120981632,
122.254191419201)) ;
#96504 = CARTESIAN_POINT('Ctrl Pts',(-19.040386485539,-13.3376231436085,122.254262435162)) ;
#96505 = CARTESIAN_POINT('Ctrl Pts',(-19.0402744402681,-13.3376286953589,
122.254298146596)) ;
#96506 = CARTESIAN_POINT('Ctrl Pts',(-19.0400489713282,-13.3376398675024,
122.254370044854)) ;
#96507 = CARTESIAN_POINT('Ctrl Pts',(-19.0399355477223,-13.3376454878967,
122.254406232105)) ;
#96508 = CARTESIAN_POINT('Ctrl Pts',(-19.0397070954834,-13.3376568085709,
122.254479155685)) ;
#96509 = CARTESIAN_POINT('Ctrl Pts',(-19.0395920671335,-13.3376625088419,
122.25451589245)) ;
#96510 = CARTESIAN_POINT('Ctrl Pts',(-19.0393601629524,-13.3376740013,122.254589994114)) ;
#96511 = CARTESIAN_POINT('Ctrl Pts',(-19.0392432871479,-13.3376797934917,
122.254627359621)) ;
#96512 = CARTESIAN_POINT('Ctrl Pts',(-19.0390074267959,-13.3376914827571,
122.25470280419)) ;
#96513 = CARTESIAN_POINT('Ctrl Pts',(-19.0388884425091,-13.3376973798246,
122.254740883885)) ;
#96514 = CARTESIAN_POINT('Ctrl Pts',(-19.0386480823165,-13.3377092928825,
122.254817849559)) ;
#96515 = CARTESIAN_POINT('Ctrl Pts',(-19.0385267065236,-13.3377153088752,
122.254856736329)) ;
#96516 = CARTESIAN_POINT('Ctrl Pts',(-19.0382812550526,-13.3377274750866,
122.254935417458)) ;
#96517 = CARTESIAN_POINT('Ctrl Pts',(-19.0381571797212,-13.3377336252973,
122.254975212657)) ;
#96518 = CARTESIAN_POINT('Ctrl Pts',(-19.0379059914914,-13.3377460767112,
122.255055821876)) ;
#96519 = CARTESIAN_POINT('Ctrl Pts',(-19.0377788789168,-13.3377523779088,
122.255096636888)) ;
#96520 = CARTESIAN_POINT('Ctrl Pts',(-19.0375212441218,-13.3377651497733,
122.255179408574)) ;
#96521 = CARTESIAN_POINT('Ctrl Pts',(-19.0373907223113,-13.3377716204319,
122.255221366377)) ;
#96522 = CARTESIAN_POINT('Ctrl Pts',(-19.0371258568404,-13.3377847516905,
122.255306560034)) ;
#96523 = CARTESIAN_POINT('Ctrl Pts',(-19.0369915133848,-13.3377914122943,
122.255349797274)) ;
#96524 = CARTESIAN_POINT('Ctrl Pts',(-19.0367185448415,-13.3378049462815,
122.255437702254)) ;
#96525 = CARTESIAN_POINT('Ctrl Pts',(-19.0365799202535,-13.3378118196562,
122.255482371511)) ;
#96526 = CARTESIAN_POINT('Ctrl Pts',(-19.0362978736293,-13.3378258048102,
122.255573311902)) ;
#96527 = CARTESIAN_POINT('Ctrl Pts',(-19.0361544524342,-13.3378329165664,
122.255619584709)) ;
#96528 = CARTESIAN_POINT('Ctrl Pts',(-19.0359263483931,-13.3378442278965,
122.255693226093)) ;
#96529 = CARTESIAN_POINT('Ctrl Pts',(-19.0358416595435,-13.337848427585,122.255720577419)) ;
#96530 = CARTESIAN_POINT('Ctrl Pts',(-19.035654423411,-13.337857712772,122.255781070396)) ;
#96531 = CARTESIAN_POINT('Ctrl Pts',(-19.0355518777005,-13.3378627982382,
122.255814216332)) ;
#96532 = CARTESIAN_POINT('Ctrl Pts',(-19.0353240076609,-13.3378740991321,
122.255887904445)) ;
#96533 = CARTESIAN_POINT('Ctrl Pts',(-19.0351986855838,-13.3378803145191,
122.255928453336)) ;
#96534 = CARTESIAN_POINT('Ctrl Pts',(-19.0349184013047,-13.3378942157852,
122.256019191757)) ;
#96535 = CARTESIAN_POINT('Ctrl Pts',(-19.0347634423273,-13.3379019016182,
122.256069392159)) ;
#96536 = CARTESIAN_POINT('Ctrl Pts',(-19.0344139593646,-13.3379192364169,
122.256182688082)) ;
#96537 = CARTESIAN_POINT('Ctrl Pts',(-19.0342194413875,-13.3379288852741,
122.256245801496)) ;
#96538 = CARTESIAN_POINT('Ctrl Pts',(-19.0292278127303,-13.3381765030178,
122.257866781309)) ;
#96539 = CARTESIAN_POINT('Ctrl Pts',(-19.0244404263421,-13.3384143037357,
122.259454458494)) ;
#96540 = CARTESIAN_POINT('Ctrl Pts',(-19.0128982678759,-13.3389884136442,
122.263362218635)) ;
#96541 = CARTESIAN_POINT('Ctrl Pts',(-19.0061537913089,-13.3393245356042,
122.265712144077)) ;
#96542 = CARTESIAN_POINT('Ctrl Pts',(-18.9843478242423,-13.3404135922291,
122.273526120646)) ;
#96543 = CARTESIAN_POINT('Ctrl Pts',(-18.9693735887403,-13.3411649858557,
122.279228666485)) ;
#96544 = CARTESIAN_POINT('Ctrl Pts',(-18.9376910090279,-13.3427656831395,
122.292017280387)) ;
#96545 = CARTESIAN_POINT('Ctrl Pts',(-18.9210198420192,-13.3436147071352,
122.299184899963)) ;
#96546 = CARTESIAN_POINT('Ctrl Pts',(-18.8947114131146,-13.3449711507317,
122.311201155099)) ;
#96547 = CARTESIAN_POINT('Ctrl Pts',(-18.8849674188033,-13.3454772316842,
122.315809363257)) ;
#96548 = CARTESIAN_POINT('Ctrl Pts',(-18.8701187344389,-13.34625481936,122.323075053432)) ;
#96549 = CARTESIAN_POINT('Ctrl Pts',(-18.8649694444918,-13.346525663204,122.325640169307)) ;
#96550 = CARTESIAN_POINT('Ctrl Pts',(-18.8597951056349,-13.346799067657,122.328263797716)) ;
#96551 = CARTESIAN_POINT('Ctrl Pts',(-18.8597516351301,-13.3468013646632,
122.328285842555)) ;
#96552 = CARTESIAN_POINT('Ctrl Pts',(-18.8596627487803,-13.3468060616498,
122.328330925483)) ;
#96553 = CARTESIAN_POINT('Ctrl Pts',(-18.8596173329339,-13.3468084616385,
122.328353963873)) ;
#96554 = CARTESIAN_POINT('Ctrl Pts',(-18.8595244842444,-13.3468133684016,
122.328401071169)) ;
#96555 = CARTESIAN_POINT('Ctrl Pts',(-18.8594770520024,-13.346815875153,122.328425140096)) ;
#96556 = CARTESIAN_POINT('Ctrl Pts',(-18.8593800998114,-13.3468209992053,
122.328474345338)) ;
#96557 = CARTESIAN_POINT('Ctrl Pts',(-18.8593305797524,-13.3468236165215,
122.328499482063)) ;
#96558 = CARTESIAN_POINT('Ctrl Pts',(-18.8592293792541,-13.3468289655735,
122.328550860863)) ;
#96559 = CARTESIAN_POINT('Ctrl Pts',(-18.8591776987793,-13.3468316973215,
122.328577103338)) ;
#96560 = CARTESIAN_POINT('Ctrl Pts',(-18.8590721040616,-13.3468372791475,
122.328630732063)) ;
#96561 = CARTESIAN_POINT('Ctrl Pts',(-18.8590181898945,-13.3468401292326,
122.328658118686)) ;
#96562 = CARTESIAN_POINT('Ctrl Pts',(-18.8589080530362,-13.3468459517185,
122.328714074931)) ;
#96563 = CARTESIAN_POINT('Ctrl Pts',(-18.8588518309071,-13.3468489241016,
122.328742644712)) ;
#96564 = CARTESIAN_POINT('Ctrl Pts',(-18.8587370038692,-13.3468549951459,
122.328801006354)) ;
#96565 = CARTESIAN_POINT('Ctrl Pts',(-18.8586783992932,-13.3468580938023,
122.328830798524)) ;
#96566 = CARTESIAN_POINT('Ctrl Pts',(-18.8585653217553,-13.3468640729723,
122.328888294071)) ;
#96567 = CARTESIAN_POINT('Ctrl Pts',(-18.8585108483696,-13.3468669534864,
122.32891599685)) ;
#96568 = CARTESIAN_POINT('Ctrl Pts',(-18.8583912107376,-13.3468732801468,
122.328976850674)) ;
#96569 = CARTESIAN_POINT('Ctrl Pts',(-18.8583260471173,-13.3468767263203,
122.329010003631)) ;
#96570 = CARTESIAN_POINT('Ctrl Pts',(-18.858183141305,-13.346884284323,122.32908272532)) ;
#96571 = CARTESIAN_POINT('Ctrl Pts',(-18.8581054010911,-13.3468883961325,
122.329122296181)) ;
#96572 = CARTESIAN_POINT('Ctrl Pts',(-18.8553606934422,-13.3470335783592,
122.33051976316)) ;
#96573 = CARTESIAN_POINT('Ctrl Pts',(-18.8526987507822,-13.3471747183719,
122.331887499396)) ;
#96574 = CARTESIAN_POINT('Ctrl Pts',(-18.8444314678514,-13.3476141177699,
122.336174008397)) ;
#96575 = CARTESIAN_POINT('Ctrl Pts',(-18.8388438402901,-13.347912614025,122.339126685355)) ;
#96576 = CARTESIAN_POINT('Ctrl Pts',(-18.8106859244637,-13.3494245921978,
122.354288428899)) ;
#96577 = CARTESIAN_POINT('Ctrl Pts',(-18.7884835330187,-13.3506427517128,
122.367166739877)) ;
#96578 = CARTESIAN_POINT('Ctrl Pts',(-18.7574757470401,-13.3523755912563,
122.386490347429)) ;
#96579 = CARTESIAN_POINT('Ctrl Pts',(-18.7483233303963,-13.3528909208824,
122.392366071302)) ;
#96580 = CARTESIAN_POINT('Ctrl Pts',(-18.7316729966105,-13.3538354859042,
122.403373833332)) ;
#96581 = CARTESIAN_POINT('Ctrl Pts',(-18.7241513963752,-13.3542649095427,
122.408468608713)) ;
#96582 = CARTESIAN_POINT('Ctrl Pts',(-18.7166298709666,-13.3546972031208,
122.413687346727)) ;
#96583 = CARTESIAN_POINT('Ctrl Pts',(-18.7165721195082,-13.3547005225116,
122.413727424446)) ;
#96584 = CARTESIAN_POINT('Ctrl Pts',(-18.7164554172712,-13.3547072305754,
122.413808427183)) ;
#96585 = CARTESIAN_POINT('Ctrl Pts',(-18.7163964666579,-13.3547106192462,
122.413849352399)) ;
#96586 = CARTESIAN_POINT('Ctrl Pts',(-18.7162772962386,-13.3547174699088,
122.41393209959)) ;
#96587 = CARTESIAN_POINT('Ctrl Pts',(-18.7162170757472,-13.354720931948,122.41397392238)) ;
#96588 = CARTESIAN_POINT('Ctrl Pts',(-18.7106701572007,-13.3550398382063,
122.417826970233)) ;
#96589 = CARTESIAN_POINT('Ctrl Pts',(-18.7052149753335,-13.3553550287032,
122.421683385498)) ;
#96590 = CARTESIAN_POINT('Ctrl Pts',(-18.6914622852756,-13.3561537828534,
122.431576655219)) ;
#96591 = CARTESIAN_POINT('Ctrl Pts',(-18.683208931944,-13.3566370130523,122.437674000132)) ;
#96592 = CARTESIAN_POINT('Ctrl Pts',(-18.6590960319231,-13.3580613767778,
122.455964614775)) ;
#96593 = CARTESIAN_POINT('Ctrl Pts',(-18.6434593010741,-13.3590012951512,
122.468445829943)) ;
#96594 = CARTESIAN_POINT('Ctrl Pts',(-18.6219798661478,-13.3603209866614,
122.486476776221)) ;
#96595 = CARTESIAN_POINT('Ctrl Pts',(-18.6158733236602,-13.3606995492345,
122.491707127935)) ;
#96596 = CARTESIAN_POINT('Ctrl Pts',(-18.6097563470408,-13.3610825229733,
122.497052588861)) ;
#96597 = CARTESIAN_POINT('Ctrl Pts',(-18.6096935370172,-13.3610864558094,
122.497107488257)) ;
#96598 = CARTESIAN_POINT('Ctrl Pts',(-18.6095543985491,-13.3610951688325,
122.49722912817)) ;
#96599 = CARTESIAN_POINT('Ctrl Pts',(-18.6094780728025,-13.3610999490441,
122.497295871774)) ;
#96600 = CARTESIAN_POINT('Ctrl Pts',(-18.6093089439101,-13.3611105427603,
122.497443805131)) ;
#96601 = CARTESIAN_POINT('Ctrl Pts',(-18.6092161447712,-13.3611163563012,
122.497524999455)) ;
#96602 = CARTESIAN_POINT('Ctrl Pts',(-18.608961920369,-13.3611322850028,122.497747500662)) ;
#96603 = CARTESIAN_POINT('Ctrl Pts',(-18.6088005201761,-13.3611424003933,
122.497888836172)) ;
#96604 = CARTESIAN_POINT('Ctrl Pts',(-18.6060091022714,-13.3613173928109,
122.500334541848)) ;
#96605 = CARTESIAN_POINT('Ctrl Pts',(-18.6033890112299,-13.3614823611394,
122.502650209892)) ;
#96606 = CARTESIAN_POINT('Ctrl Pts',(-18.5976232261579,-13.3618470431525,
122.507790586009)) ;
#96607 = CARTESIAN_POINT('Ctrl Pts',(-18.594482204895,-13.3620468098679,122.510620468649)) ;
#96608 = CARTESIAN_POINT('Ctrl Pts',(-18.5815761681471,-13.3628723791545,
122.522370703935)) ;
#96609 = CARTESIAN_POINT('Ctrl Pts',(-18.5719423907334,-13.3634997865374,
122.531433802383)) ;
#96610 = CARTESIAN_POINT('Ctrl Pts',(-18.5504874896909,-13.3649193322179,
122.552288529581)) ;
#96611 = CARTESIAN_POINT('Ctrl Pts',(-18.5387575044489,-13.365711325687,122.564170260344)) ;
#96612 = CARTESIAN_POINT('Ctrl Pts',(-18.5237874296271,-13.3667412457248,
122.579972557899)) ;
#96613 = CARTESIAN_POINT('Ctrl Pts',(-18.5203218849068,-13.3669810676662,
122.583676955652)) ;
#96614 = CARTESIAN_POINT('Ctrl Pts',(-18.5168686973641,-13.367221432483,122.587414795655)) ;
#96615 = CARTESIAN_POINT('Ctrl Pts',(-18.5168577595361,-13.3672221938427,
122.58742663558)) ;
#96616 = CARTESIAN_POINT('Ctrl Pts',(-18.5168359036866,-13.3672237152118,
122.587450294936)) ;
#96617 = CARTESIAN_POINT('Ctrl Pts',(-18.5168249857844,-13.3672244752129,
122.587462114235)) ;
#96618 = CARTESIAN_POINT('Ctrl Pts',(-18.5168031693219,-13.3672259938968,
122.587485732837)) ;
#96619 = CARTESIAN_POINT('Ctrl Pts',(-18.5167922704174,-13.3672267526035,
122.58749753251)) ;
#96620 = CARTESIAN_POINT('Ctrl Pts',(-18.5167704912355,-13.3672282687485,
122.587521112627)) ;
#96621 = CARTESIAN_POINT('Ctrl Pts',(-18.5167596110082,-13.3672290261832,
122.587532893016)) ;
#96622 = CARTESIAN_POINT('Ctrl Pts',(-18.5167378688188,-13.3672305398091,
122.587556434952)) ;
#96623 = CARTESIAN_POINT('Ctrl Pts',(-18.5167270063538,-13.3672312960352,
122.587568197042)) ;
#96624 = CARTESIAN_POINT('Ctrl Pts',(-18.5167052985569,-13.3672328073227,
122.587591703604)) ;
#96625 = CARTESIAN_POINT('Ctrl Pts',(-18.516694453782,-13.3672335623452,122.58760344747)) ;
#96626 = CARTESIAN_POINT('Ctrl Pts',(-18.5166727804776,-13.3672350712871,
122.587626918539)) ;
#96627 = CARTESIAN_POINT('Ctrl Pts',(-18.5166619524181,-13.3672358251737,
122.587638645232)) ;
#96628 = CARTESIAN_POINT('Ctrl Pts',(-18.5166403122601,-13.3672373318634,
122.587662082259)) ;
#96629 = CARTESIAN_POINT('Ctrl Pts',(-18.5166295002028,-13.3672380846637,
122.587673792547)) ;
#96630 = CARTESIAN_POINT('Ctrl Pts',(-18.5134149869873,-13.3674619024595,
122.591155494558)) ;
#96631 = CARTESIAN_POINT('Ctrl Pts',(-18.5102315402403,-13.3676847737275,
122.594644143493)) ;
#96632 = CARTESIAN_POINT('Ctrl Pts',(-18.5053006862292,-13.3680318893206,
122.600111414455)) ;
#96633 = CARTESIAN_POINT('Ctrl Pts',(-18.5035392534791,-13.3681562735316,
122.602077313781)) ;
#96634 = CARTESIAN_POINT('Ctrl Pts',(-18.4980969957137,-13.368541784209,122.608191281244)) ;
#96635 = CARTESIAN_POINT('Ctrl Pts',(-18.4944381496269,-13.3688026825386,
122.61235882918)) ;
#96636 = CARTESIAN_POINT('Ctrl Pts',(-18.4831845050064,-13.3696105943536,
122.625355523017)) ;
#96637 = CARTESIAN_POINT('Ctrl Pts',(-18.475688015924,-13.370156575175,122.634268941991)) ;
#96638 = CARTESIAN_POINT('Ctrl Pts',(-18.4544325876435,-13.3717291288739,
122.660292498896)) ;
#96639 = CARTESIAN_POINT('Ctrl Pts',(-18.4410078693402,-13.3727527537507,
122.677669471024)) ;
#96640 = CARTESIAN_POINT('Ctrl Pts',(-18.4221668920765,-13.3742462428024,
122.703473591337)) ;
#96641 = CARTESIAN_POINT('Ctrl Pts',(-18.4163722974893,-13.3747140001268,
122.711618916006)) ;
#96642 = CARTESIAN_POINT('Ctrl Pts',(-18.4075200358554,-13.3754427498945,
122.724393195021)) ;
#96643 = CARTESIAN_POINT('Ctrl Pts',(-18.4043924344706,-13.3757030762256,
122.728973159054)) ;
#96644 = CARTESIAN_POINT('Ctrl Pts',(-18.3997274021304,-13.3760958025304,
122.735905947536)) ;
#96645 = CARTESIAN_POINT('Ctrl Pts',(-18.398166592045,-13.3762279621017,122.738242961674)) ;
#96646 = CARTESIAN_POINT('Ctrl Pts',(-18.3947247016994,-13.3765211120614,
122.743435451624)) ;
#96647 = CARTESIAN_POINT('Ctrl Pts',(-18.3928475407721,-13.3766821417875,
122.746293493754)) ;
#96648 = CARTESIAN_POINT('Ctrl Pts',(-18.3909766913437,-13.3768437985691,
122.749168302905)) ;
#96649 = CARTESIAN_POINT('Ctrl Pts',(-18.3909709092369,-13.3768442982019,
122.749177188136)) ;
#96650 = CARTESIAN_POINT('Ctrl Pts',(-18.3909592951262,-13.3768453018019,
122.749195035785)) ;
#96651 = CARTESIAN_POINT('Ctrl Pts',(-18.3909534623636,-13.3768458058348,
122.749203999373)) ;
#96652 = CARTESIAN_POINT('Ctrl Pts',(-18.3909417461145,-13.3768468183068,
122.74922200502)) ;
#96653 = CARTESIAN_POINT('Ctrl Pts',(-18.3909358623542,-13.3768473267698,
122.749231047504)) ;
#96654 = CARTESIAN_POINT('Ctrl Pts',(-18.3909240431642,-13.3768483481845,
122.749249212411)) ;
#96655 = CARTESIAN_POINT('Ctrl Pts',(-18.3909181079088,-13.3768488611213,
122.749258334569)) ;
#96656 = CARTESIAN_POINT('Ctrl Pts',(-18.3909061853908,-13.3768498915133,
122.749276659357)) ;
#96657 = CARTESIAN_POINT('Ctrl Pts',(-18.3909001982543,-13.3768504089578,
122.749285861798)) ;
#96658 = CARTESIAN_POINT('Ctrl Pts',(-18.3908881718299,-13.3768514483783,
122.749304347385)) ;
#96659 = CARTESIAN_POINT('Ctrl Pts',(-18.3908821324558,-13.376851970362,122.74931363067)) ;
#96660 = CARTESIAN_POINT('Ctrl Pts',(-18.3908700015064,-13.3768530188659,
122.749332278036)) ;
#96661 = CARTESIAN_POINT('Ctrl Pts',(-18.3908639095545,-13.3768535454188,
122.749341642702)) ;
#96662 = CARTESIAN_POINT('Ctrl Pts',(-18.3908516739967,-13.3768546030145,
122.749360452005)) ;
#96663 = CARTESIAN_POINT('Ctrl Pts',(-18.3908455296984,-13.3768551341173,
122.749369897711)) ;
#96664 = CARTESIAN_POINT('Ctrl Pts',(-18.3908331869644,-13.376856201028,122.749388872927)) ;
#96665 = CARTESIAN_POINT('Ctrl Pts',(-18.3908269892115,-13.3768567367771,
122.749398401392)) ;
#96666 = CARTESIAN_POINT('Ctrl Pts',(-18.3908145405507,-13.3768578128963,
122.749417540631)) ;
#96667 = CARTESIAN_POINT('Ctrl Pts',(-18.390808289363,-13.3768583532907,122.74942715184)) ;
#96668 = CARTESIAN_POINT('Ctrl Pts',(-18.3907957335943,-13.3768594387217,
122.749446456948)) ;
#96669 = CARTESIAN_POINT('Ctrl Pts',(-18.3907894288256,-13.3768599837748,
122.749456151141)) ;
#96670 = CARTESIAN_POINT('Ctrl Pts',(-18.39077676444,-13.3768610786495,122.74947562447)) ;
#96671 = CARTESIAN_POINT('Ctrl Pts',(-18.3907704052802,-13.3768616284319,
122.749485402908)) ;
#96672 = CARTESIAN_POINT('Ctrl Pts',(-18.390757633046,-13.3768627326853,122.749505043307)) ;
#96673 = CARTESIAN_POINT('Ctrl Pts',(-18.3907512196331,-13.3768632871858,
122.749514905794)) ;
#96674 = CARTESIAN_POINT('Ctrl Pts',(-18.3907383375213,-13.3768644009946,
122.749534716415)) ;
#96675 = CARTESIAN_POINT('Ctrl Pts',(-18.3907318690915,-13.37686496028,122.749544664142)) ;
#96676 = CARTESIAN_POINT('Ctrl Pts',(-18.3907188777956,-13.3768660835859,
122.749564643952)) ;
#96677 = CARTESIAN_POINT('Ctrl Pts',(-18.3907123545036,-13.3768666476435,
122.749574676696)) ;
#96678 = CARTESIAN_POINT('Ctrl Pts',(-18.3906992518081,-13.3768677806393,
122.749594829135)) ;
#96679 = CARTESIAN_POINT('Ctrl Pts',(-18.3906926727333,-13.3768683495495,
122.74960494833)) ;
#96680 = CARTESIAN_POINT('Ctrl Pts',(-18.3906794599658,-13.376869492122,122.749625271389)) ;
#96681 = CARTESIAN_POINT('Ctrl Pts',(-18.3906728255778,-13.3768700658448,
122.749635476329)) ;
#96682 = CARTESIAN_POINT('Ctrl Pts',(-18.3906594997692,-13.3768712182524,
122.749655974609)) ;
#96683 = CARTESIAN_POINT('Ctrl Pts',(-18.3906528090286,-13.3768717968785,
122.749666266909)) ;
#96684 = CARTESIAN_POINT('Ctrl Pts',(-18.3906393711157,-13.3768729590415,
122.749686939004)) ;
#96685 = CARTESIAN_POINT('Ctrl Pts',(-18.3906326238557,-13.3768735425862,
122.749697318939)) ;
#96686 = CARTESIAN_POINT('Ctrl Pts',(-18.3906190729928,-13.3768747145793,
122.749718166184)) ;
#96687 = CARTESIAN_POINT('Ctrl Pts',(-18.3906122690149,-13.3768753030604,
122.749728634077)) ;
#96688 = CARTESIAN_POINT('Ctrl Pts',(-18.3905986046586,-13.3768764849322,
122.749749657343)) ;
#96689 = CARTESIAN_POINT('Ctrl Pts',(-18.3905917439995,-13.3768770783475,
122.749760213155)) ;
#96690 = CARTESIAN_POINT('Ctrl Pts',(-18.3905779638416,-13.3768782702992,
122.74978141603)) ;
#96691 = CARTESIAN_POINT('Ctrl Pts',(-18.3905710452459,-13.3768788687579,
122.74979206171)) ;
#96692 = CARTESIAN_POINT('Ctrl Pts',(-18.3905571511829,-13.3768800706272,
122.749813441313)) ;
#96693 = CARTESIAN_POINT('Ctrl Pts',(-18.3905501750023,-13.3768806740998,
122.749824176339)) ;
#96694 = CARTESIAN_POINT('Ctrl Pts',(-18.3884479529676,-13.3770625311926,
122.753059211433)) ;
#96695 = CARTESIAN_POINT('Ctrl Pts',(-18.3863680303638,-13.3772439441288,
122.756293434186)) ;
#96696 = CARTESIAN_POINT('Ctrl Pts',(-18.3815271437052,-13.3776696928001,
122.763900016937)) ;
#96697 = CARTESIAN_POINT('Ctrl Pts',(-18.3787786747778,-13.3779141535009,
122.768280231923)) ;
#96698 = CARTESIAN_POINT('Ctrl Pts',(-18.3692901081473,-13.3787677530145,
122.7836187377)) ;
#96699 = CARTESIAN_POINT('Ctrl Pts',(-18.3626962067539,-13.379378281947,122.794666372696)) ;
#96700 = CARTESIAN_POINT('Ctrl Pts',(-18.3454085761085,-13.3810257426399,
122.824704656564)) ;
#96701 = CARTESIAN_POINT('Ctrl Pts',(-18.335048269181,-13.382064149279,122.843881830466)) ;
#96702 = CARTESIAN_POINT('Ctrl Pts',(-18.3211439701148,-13.3835270265698,
122.871362092374)) ;
#96703 = CARTESIAN_POINT('Ctrl Pts',(-18.3171680168704,-13.3839542212821,
122.879441854487)) ;
#96704 = CARTESIAN_POINT('Ctrl Pts',(-18.3099771127772,-13.3847435831836,
122.894474494045)) ;
#96705 = CARTESIAN_POINT('Ctrl Pts',(-18.3067373870593,-13.3851059129165,
122.90141500941)) ;
#96706 = CARTESIAN_POINT('Ctrl Pts',(-18.3025370697126,-13.3855847770263,
122.910640028206)) ;
#96707 = CARTESIAN_POINT('Ctrl Pts',(-18.3015175370548,-13.3857017452631,
122.912897474592)) ;
#96708 = CARTESIAN_POINT('Ctrl Pts',(-18.3004983112666,-13.3858194257373,
122.915172765614)) ;
#96709 = CARTESIAN_POINT('Ctrl Pts',(-18.3004917085975,-13.3858201881176,
122.915187506015)) ;
#96710 = CARTESIAN_POINT('Ctrl Pts',(-18.3004784917221,-13.385821714274,122.91521701415)) ;
#96711 = CARTESIAN_POINT('Ctrl Pts',(-18.3004718773668,-13.3858224780674,
122.915231782221)) ;
#96712 = CARTESIAN_POINT('Ctrl Pts',(-18.3004586367009,-13.3858240070986,
122.915261346638)) ;
#96713 = CARTESIAN_POINT('Ctrl Pts',(-18.3004520107137,-13.3858247722992,
122.915276142265)) ;
#96714 = CARTESIAN_POINT('Ctrl Pts',(-18.3004387472419,-13.3858263040923,
122.915305760783)) ;
#96715 = CARTESIAN_POINT('Ctrl Pts',(-18.3004321089316,-13.3858270707803,
122.91532058552)) ;
#96716 = CARTESIAN_POINT('Ctrl Pts',(-18.2991387725807,-13.3859764502171,
122.918209031724)) ;
#96717 = CARTESIAN_POINT('Ctrl Pts',(-18.2978632483265,-13.3861249809128,
122.921087647275)) ;
#96718 = CARTESIAN_POINT('Ctrl Pts',(-18.2943101519845,-13.3865421748281,
122.929191214444)) ;
#96719 = CARTESIAN_POINT('Ctrl Pts',(-18.29205813526,-13.3868106543641,122.93442728797)) ;
#96720 = CARTESIAN_POINT('Ctrl Pts',(-18.2855436637273,-13.3875995847923,
122.949872382096)) ;
#96721 = CARTESIAN_POINT('Ctrl Pts',(-18.2813837033121,-13.3881193667763,
122.960124010957)) ;
#96722 = CARTESIAN_POINT('Ctrl Pts',(-18.2717940433691,-13.3893585124946,
122.984715136903)) ;
#96723 = CARTESIAN_POINT('Ctrl Pts',(-18.2664946547687,-13.3900773473825,
122.999103363326)) ;
#96724 = CARTESIAN_POINT('Ctrl Pts',(-18.2589628957656,-13.3911563433964,
123.020810965051)) ;
#96725 = CARTESIAN_POINT('Ctrl Pts',(-18.2565250325121,-13.3915156390818,
123.028057393181)) ;
#96726 = CARTESIAN_POINT('Ctrl Pts',(-18.2531078768523,-13.3920347245763,
123.038541130682)) ;
#96727 = CARTESIAN_POINT('Ctrl Pts',(-18.2520734469534,-13.3921940271163,
123.041760281249)) ;
#96728 = CARTESIAN_POINT('Ctrl Pts',(-18.251045879315,-13.3923544785025,123.045004513629)) ;
#96729 = CARTESIAN_POINT('Ctrl Pts',(-18.2510392894921,-13.3923555075745,
123.045025320939)) ;
#96730 = CARTESIAN_POINT('Ctrl Pts',(-18.2510258105944,-13.3923576126387,
123.045067884429)) ;
#96731 = CARTESIAN_POINT('Ctrl Pts',(-18.2510189217492,-13.3923586886037,
123.045089640066)) ;
#96732 = CARTESIAN_POINT('Ctrl Pts',(-18.2510048344239,-13.3923608891018,
123.045134133551)) ;
#96733 = CARTESIAN_POINT('Ctrl Pts',(-18.2509976359677,-13.3923620136405,
123.045156871522)) ;
#96734 = CARTESIAN_POINT('Ctrl Pts',(-18.2509829187618,-13.3923643129795,
123.045203363941)) ;
#96735 = CARTESIAN_POINT('Ctrl Pts',(-18.2509753999949,-13.3923654877924,
123.045227118657)) ;
#96736 = CARTESIAN_POINT('Ctrl Pts',(-18.2509600311132,-13.3923678894378,
123.045275680137)) ;
#96737 = CARTESIAN_POINT('Ctrl Pts',(-18.2509521811117,-13.3923691162633,
123.045300486774)) ;
#96738 = CARTESIAN_POINT('Ctrl Pts',(-18.2509361390098,-13.3923716236471,
123.045351186771)) ;
#96739 = CARTESIAN_POINT('Ctrl Pts',(-18.2509279469193,-13.3923729042155,
123.045377080347)) ;
#96740 = CARTESIAN_POINT('Ctrl Pts',(-18.2509112096252,-13.3923755208424,
123.045429989788)) ;
#96741 = CARTESIAN_POINT('Ctrl Pts',(-18.2509026644943,-13.3923768569022,
123.045457005691)) ;
#96742 = CARTESIAN_POINT('Ctrl Pts',(-18.2508852100857,-13.3923795862754,
123.045512195482)) ;
#96743 = CARTESIAN_POINT('Ctrl Pts',(-18.250876300924,-13.3923809795843,123.045540369291)) ;
#96744 = CARTESIAN_POINT('Ctrl Pts',(-18.2508543419544,-13.3923844141777,
123.045609819858)) ;
#96745 = CARTESIAN_POINT('Ctrl Pts',(-18.2508412932732,-13.3923864554801,
123.045651097152)) ;
#96746 = CARTESIAN_POINT('Ctrl Pts',(-18.2508128248774,-13.3923909097966,
123.045741168853)) ;
#96747 = CARTESIAN_POINT('Ctrl Pts',(-18.2507974060689,-13.3923933228134,
123.045789963444)) ;
#96748 = CARTESIAN_POINT('Ctrl Pts',(-18.2507524594717,-13.3924003583595,
123.0459322334)) ;
#96749 = CARTESIAN_POINT('Ctrl Pts',(-18.2507229399015,-13.3924049809592,
123.046025711403)) ;
#96750 = CARTESIAN_POINT('Ctrl Pts',(-18.2491289933776,-13.3926546848277,
123.051075302574)) ;
#96751 = CARTESIAN_POINT('Ctrl Pts',(-18.2475963756887,-13.3929000250872,
123.056041390375)) ;
#96752 = CARTESIAN_POINT('Ctrl Pts',(-18.2424886668612,-13.393735649858,123.072976608148)) ;
#96753 = CARTESIAN_POINT('Ctrl Pts',(-18.2390663268281,-13.3943267028447,
123.084990967522)) ;
#96754 = CARTESIAN_POINT('Ctrl Pts',(-18.2312177913983,-13.395760092817,123.114249022152)) ;
#96755 = CARTESIAN_POINT('Ctrl Pts',(-18.2269841201169,-13.3966022265531,
123.131541441677)) ;
#96756 = CARTESIAN_POINT('Ctrl Pts',(-18.223119648681,-13.3974454030261,123.148976089644)) ;
#96757 = CARTESIAN_POINT('Ctrl Pts',(-18.2231073691857,-13.3974480830802,
123.14903150724)) ;
#96758 = CARTESIAN_POINT('Ctrl Pts',(-18.2230828406592,-13.3974534382001,
123.149142241687)) ;
#96759 = CARTESIAN_POINT('Ctrl Pts',(-18.2230705916524,-13.3974561132576,
123.149197558361)) ;
#96760 = CARTESIAN_POINT('Ctrl Pts',(-18.2230461193779,-13.3974614594072,
123.149308112105)) ;
#96761 = CARTESIAN_POINT('Ctrl Pts',(-18.2230338960794,-13.3974641305037,
123.149363349261)) ;
#96762 = CARTESIAN_POINT('Ctrl Pts',(-18.2230094704838,-13.3974694697597,
123.149473765226)) ;
#96763 = CARTESIAN_POINT('Ctrl Pts',(-18.2229972681868,-13.3974721379174,
123.149528943995)) ;
#96764 = CARTESIAN_POINT('Ctrl Pts',(-18.2229728798514,-13.3974774723279,
123.14963926452)) ;
#96765 = CARTESIAN_POINT('Ctrl Pts',(-18.2229606938109,-13.39748013858,123.14969440626)) ;
#96766 = CARTESIAN_POINT('Ctrl Pts',(-18.2229363332554,-13.3974854702116,
123.149804674075)) ;
#96767 = CARTESIAN_POINT('Ctrl Pts',(-18.2229241587319,-13.3974881355925,
123.149859800177)) ;
#96768 = CARTESIAN_POINT('Ctrl Pts',(-18.2228998164575,-13.3974934665211,
123.149970058209)) ;
#96769 = CARTESIAN_POINT('Ctrl Pts',(-18.222887648702,-13.3974961320699,123.150025190162)) ;
#96770 = CARTESIAN_POINT('Ctrl Pts',(-18.2228633151988,-13.3975014643787,
123.150135481503)) ;
#96771 = CARTESIAN_POINT('Ctrl Pts',(-18.2228511494338,-13.3975041311434,
123.150190640986)) ;
#96772 = CARTESIAN_POINT('Ctrl Pts',(-18.2228268150796,-13.3975094669457,
123.150301009351)) ;
#96773 = CARTESIAN_POINT('Ctrl Pts',(-18.2228146465259,-13.3975121359772,
123.150356218104)) ;
#96774 = CARTESIAN_POINT('Ctrl Pts',(-18.2227903017722,-13.3975174773753,
123.15046670699)) ;
#96775 = CARTESIAN_POINT('Ctrl Pts',(-18.2227781255604,-13.3975201497468,
123.150521987223)) ;
#96776 = CARTESIAN_POINT('Ctrl Pts',(-18.2227537605896,-13.3975254989073,
123.150632641466)) ;
#96777 = CARTESIAN_POINT('Ctrl Pts',(-18.2227415718718,-13.3975281756901,
123.15068801535)) ;
#96778 = CARTESIAN_POINT('Ctrl Pts',(-18.2227171769687,-13.3975335347626,
123.150798879439)) ;
#96779 = CARTESIAN_POINT('Ctrl Pts',(-18.2227049707799,-13.3975362170565,
123.150854369737)) ;
#96780 = CARTESIAN_POINT('Ctrl Pts',(-18.2226805359322,-13.3975415882611,
123.150965489634)) ;
#96781 = CARTESIAN_POINT('Ctrl Pts',(-18.2226683073037,-13.3975442771694,
123.151021119187)) ;
#96782 = CARTESIAN_POINT('Ctrl Pts',(-18.2226438224996,-13.3975496627319,
123.151132540974)) ;
#96783 = CARTESIAN_POINT('Ctrl Pts',(-18.2226315663567,-13.397552359384,123.151188333168)) ;
#96784 = CARTESIAN_POINT('Ctrl Pts',(-18.2226070214042,-13.3975577615756,
123.151300103875)) ;
#96785 = CARTESIAN_POINT('Ctrl Pts',(-18.2225947325907,-13.3975604671217,
123.151356082531)) ;
#96786 = CARTESIAN_POINT('Ctrl Pts',(-18.2225701170509,-13.3975658882736,
123.151468250441)) ;
#96787 = CARTESIAN_POINT('Ctrl Pts',(-18.2225577903586,-13.3975686038784,
123.151524439682)) ;
#96788 = CARTESIAN_POINT('Ctrl Pts',(-18.2225330937139,-13.3975740463455,
123.15163705357)) ;
#96789 = CARTESIAN_POINT('Ctrl Pts',(-18.2225207238019,-13.397576773206,123.151693478193)) ;
#96790 = CARTESIAN_POINT('Ctrl Pts',(-18.2224959352809,-13.3975822394049,
123.15180658813)) ;
#96791 = CARTESIAN_POINT('Ctrl Pts',(-18.2224835167033,-13.3975849787444,
123.15186327348)) ;
#96792 = CARTESIAN_POINT('Ctrl Pts',(-18.2224586252827,-13.397590471154,123.151976930829)) ;
#96793 = CARTESIAN_POINT('Ctrl Pts',(-18.2224461524868,-13.3975932242226,
123.152033902809)) ;
#96794 = CARTESIAN_POINT('Ctrl Pts',(-18.2224211469388,-13.3975987453735,
123.152148160012)) ;
#96795 = CARTESIAN_POINT('Ctrl Pts',(-18.2224086142233,-13.3976015134575,
123.152205445282)) ;
#96796 = CARTESIAN_POINT('Ctrl Pts',(-18.2223834830007,-13.3976070659576,
123.152320356394)) ;
#96797 = CARTESIAN_POINT('Ctrl Pts',(-18.2223708845329,-13.3976098503758,
123.152377982292)) ;
#96798 = CARTESIAN_POINT('Ctrl Pts',(-18.2223456157714,-13.3976154369106,
123.152493602977)) ;
#96799 = CARTESIAN_POINT('Ctrl Pts',(-18.2223329455753,-13.3976182390172,
123.152551597576)) ;
#96800 = CARTESIAN_POINT('Ctrl Pts',(-18.2223075272283,-13.3976238623195,
123.152667984497)) ;
#96801 = CARTESIAN_POINT('Ctrl Pts',(-18.2222947790929,-13.3976266835244,
123.15272637703)) ;
#96802 = CARTESIAN_POINT('Ctrl Pts',(-18.2222691984953,-13.397632346472,123.152843589857)) ;
#96803 = CARTESIAN_POINT('Ctrl Pts',(-18.2222563661212,-13.3976351882089,
123.152902410052)) ;
#96804 = CARTESIAN_POINT('Ctrl Pts',(-18.2222306104971,-13.3976408937122,
123.153020509143)) ;
#96805 = CARTESIAN_POINT('Ctrl Pts',(-18.2222176872966,-13.3976437574825,
123.153079788141)) ;
#96806 = CARTESIAN_POINT('Ctrl Pts',(-18.2221917432412,-13.3976495085999,
123.153198836928)) ;
#96807 = CARTESIAN_POINT('Ctrl Pts',(-18.2221787224698,-13.3976523959445,
123.153258606688)) ;
#96808 = CARTESIAN_POINT('Ctrl Pts',(-18.222152576269,-13.3976581958119,123.153378670221)) ;
#96809 = CARTESIAN_POINT('Ctrl Pts',(-18.2221394509066,-13.3976611083371,
123.153438964069)) ;
#96810 = CARTESIAN_POINT('Ctrl Pts',(-18.2221130882449,-13.3976669602334,
123.153560110374)) ;
#96811 = CARTESIAN_POINT('Ctrl Pts',(-18.2220998510532,-13.3976698995991,
123.153620962746)) ;
#96812 = CARTESIAN_POINT('Ctrl Pts',(-18.222073257208,-13.3976758069036,123.153743261939)) ;
#96813 = CARTESIAN_POINT('Ctrl Pts',(-18.222059900633,-13.3976787748449,123.153804708839)) ;
#96814 = CARTESIAN_POINT('Ctrl Pts',(-18.2220330601851,-13.3976847411024,
123.153928234476)) ;
#96815 = CARTESIAN_POINT('Ctrl Pts',(-18.2220195764187,-13.3976877394163,
123.153990313196)) ;
#96816 = CARTESIAN_POINT('Ctrl Pts',(-18.2219924734308,-13.3976937682978,
123.154115141468)) ;
#96817 = CARTESIAN_POINT('Ctrl Pts',(-18.2219788543187,-13.3976967988641,
123.154177891024)) ;
#96818 = CARTESIAN_POINT('Ctrl Pts',(-18.2219514721411,-13.3977028942113,
123.154304101667)) ;
#96819 = CARTESIAN_POINT('Ctrl Pts',(-18.2219377091959,-13.3977059589901,
123.154367562746)) ;
#96820 = CARTESIAN_POINT('Ctrl Pts',(-18.2219100304974,-13.3977121248091,
123.154495238921)) ;
#96821 = CARTESIAN_POINT('Ctrl Pts',(-18.2218961148485,-13.3977152258525,
123.154559454122)) ;
#96822 = CARTESIAN_POINT('Ctrl Pts',(-18.2218681214673,-13.3977214663479,
123.154688683122)) ;
#96823 = CARTESIAN_POINT('Ctrl Pts',(-18.2218540438659,-13.3977246057992,
123.154753696945)) ;
#96824 = CARTESIAN_POINT('Ctrl Pts',(-18.2218257168632,-13.3977309253637,
123.154884569971)) ;
#96825 = CARTESIAN_POINT('Ctrl Pts',(-18.2218114676113,-13.3977341054739,
123.154950429158)) ;
#96826 = CARTESIAN_POINT('Ctrl Pts',(-18.2206177464285,-13.3980006174148,
123.160469958468)) ;
#96827 = CARTESIAN_POINT('Ctrl Pts',(-18.2194758516924,-13.3982637760351,
123.165931695837)) ;
#96828 = CARTESIAN_POINT('Ctrl Pts',(-18.2168634397538,-13.3988859271353,
123.178871359441)) ;
#96829 = CARTESIAN_POINT('Ctrl Pts',(-18.215425577729,-13.3992447446782,123.186355644931)) ;
#96830 = CARTESIAN_POINT('Ctrl Pts',(-18.2116012121085,-13.4002473663908,
123.207325051666)) ;
#96831 = CARTESIAN_POINT('Ctrl Pts',(-18.2093721471055,-13.400890302016,123.220837736344)) ;
#96832 = CARTESIAN_POINT('Ctrl Pts',(-18.2066505824798,-13.4017641535182,
123.239271501973)) ;
#96833 = CARTESIAN_POINT('Ctrl Pts',(-18.2059589801352,-13.4019956877779,
123.244162100775)) ;
#96834 = CARTESIAN_POINT('Ctrl Pts',(-18.2030040761728,-13.4030293003968,
123.266017926323)) ;
#96835 = CARTESIAN_POINT('Ctrl Pts',(-18.2010696058717,-13.4038308230221,
123.283025604649)) ;
#96836 = CARTESIAN_POINT('Ctrl Pts',(-18.1987541666902,-13.4050118794439,
123.308088499368)) ;
#96837 = CARTESIAN_POINT('Ctrl Pts',(-18.1980930057755,-13.4053901203964,
123.316115691217)) ;
#96838 = CARTESIAN_POINT('Ctrl Pts',(-18.1970380995953,-13.4060773415519,
123.330693939728)) ;
#96839 = CARTESIAN_POINT('Ctrl Pts',(-18.1966175229341,-13.4063861600578,
123.337242747047)) ;
#96840 = CARTESIAN_POINT('Ctrl Pts',(-18.1959747733166,-13.4069268477794,
123.348701874398)) ;
#96841 = CARTESIAN_POINT('Ctrl Pts',(-18.1957293040146,-13.4071585684706,
123.353610738454)) ;
#96842 = CARTESIAN_POINT('Ctrl Pts',(-18.1952708243686,-13.4076515525697,
123.364048820894)) ;
#96843 = CARTESIAN_POINT('Ctrl Pts',(-18.1950657866747,-13.4079128599884,
123.369578275986)) ;
#96844 = CARTESIAN_POINT('Ctrl Pts',(-18.1945805775629,-13.4086715720514,
123.385622613897)) ;
#96845 = CARTESIAN_POINT('Ctrl Pts',(-18.1943991764936,-13.4091695527317,
123.396139946277)) ;
#96846 = CARTESIAN_POINT('Ctrl Pts',(-18.1942395365168,-13.410946150053,123.433615253431)) ;
#96847 = CARTESIAN_POINT('Ctrl Pts',(-18.1950219323352,-13.4122283415411,
123.460568534753)) ;
#96848 = CARTESIAN_POINT('Ctrl Pts',(-18.197558558744,-13.4141619677531,123.501232840074)) ;
#96849 = CARTESIAN_POINT('Ctrl Pts',(-18.1986510137003,-13.4148153046717,
123.514976776847)) ;
#96850 = CARTESIAN_POINT('Ctrl Pts',(-18.2005727281965,-13.4157600330808,
123.534862149409)) ;
#96851 = CARTESIAN_POINT('Ctrl Pts',(-18.201215418181,-13.4160525381248,123.541020467499)) ;
#96852 = CARTESIAN_POINT('Ctrl Pts',(-18.2019069271142,-13.4163455009711,
123.547189401704)) ;
#96853 = CARTESIAN_POINT('Ctrl Pts',(-18.201908696765,-13.4163462505636,123.54720518592)) ;
#96854 = CARTESIAN_POINT('Ctrl Pts',(-18.2019122422395,-13.4163477520968,
123.54723680381)) ;
#96855 = CARTESIAN_POINT('Ctrl Pts',(-18.2019140180674,-13.4163485040385,
123.547252637503)) ;
#96856 = CARTESIAN_POINT('Ctrl Pts',(-18.2019175759493,-13.41635001029,123.547284354772)) ;
#96857 = CARTESIAN_POINT('Ctrl Pts',(-18.2019193580338,-13.416350764612,123.5473002386)) ;
#96858 = CARTESIAN_POINT('Ctrl Pts',(-18.2019229284918,-13.4163522756482,
123.547332056644)) ;
#96859 = CARTESIAN_POINT('Ctrl Pts',(-18.2019247168908,-13.4163530323724,
123.547347991069)) ;
#96860 = CARTESIAN_POINT('Ctrl Pts',(-18.2019283000676,-13.4163545482484,
123.547379911051)) ;
#96861 = CARTESIAN_POINT('Ctrl Pts',(-18.2019300948428,-13.4163553073984,
123.547395896568)) ;
#96862 = CARTESIAN_POINT('Ctrl Pts',(-18.2019336908081,-13.4163568281386,
123.547427919001)) ;
#96863 = CARTESIAN_POINT('Ctrl Pts',(-18.2019354920599,-13.4163575897541,
123.547443956448)) ;
#96864 = CARTESIAN_POINT('Ctrl Pts',(-18.2019391010789,-13.4163591154654,
123.547476083581)) ;
#96865 = CARTESIAN_POINT('Ctrl Pts',(-18.2019409088315,-13.416359879554,123.547492173117)) ;
#96866 = CARTESIAN_POINT('Ctrl Pts',(-18.2019445309307,-13.416361410242,123.547524405073)) ;
#96867 = CARTESIAN_POINT('Ctrl Pts',(-18.2019463452902,-13.4163621768459,
123.547540547587)) ;
#96868 = CARTESIAN_POINT('Ctrl Pts',(-18.202493599596,-13.4165933610962,123.552408637057)) ;
#96869 = CARTESIAN_POINT('Ctrl Pts',(-18.2030682834334,-13.4168235929693,
123.557257259879)) ;
#96870 = CARTESIAN_POINT('Ctrl Pts',(-18.2045036730148,-13.417370406019,123.568773315569)) ;
#96871 = CARTESIAN_POINT('Ctrl Pts',(-18.2053905226168,-13.4176868180764,
123.575437332814)) ;
#96872 = CARTESIAN_POINT('Ctrl Pts',(-18.2092607774667,-13.4189854456315,
123.602781821159)) ;
#96873 = CARTESIAN_POINT('Ctrl Pts',(-18.2127221227601,-13.4199646702924,
123.623391012255)) ;
#96874 = CARTESIAN_POINT('Ctrl Pts',(-18.2192939490879,-13.4215775104731,
123.657162597942)) ;
#96875 = CARTESIAN_POINT('Ctrl Pts',(-18.2220956859239,-13.4222111225105,
123.670380434125)) ;
#96876 = CARTESIAN_POINT('Ctrl Pts',(-18.2278499909049,-13.4234198097491,
123.695458071278)) ;
#96877 = CARTESIAN_POINT('Ctrl Pts',(-18.2307621869983,-13.4239944701776,
123.707325412048)) ;
#96878 = CARTESIAN_POINT('Ctrl Pts',(-18.2366952325998,-13.4250988625176,
123.730018231974)) ;
#96879 = CARTESIAN_POINT('Ctrl Pts',(-18.2396882629745,-13.4256284403642,
123.740849714526)) ;
#96880 = CARTESIAN_POINT('Ctrl Pts',(-18.2481045233248,-13.4270477868265,
123.769740009157)) ;
#96881 = CARTESIAN_POINT('Ctrl Pts',(-18.2537985945701,-13.4279381849914,
123.787716677618)) ;
#96882 = CARTESIAN_POINT('Ctrl Pts',(-18.2713240649172,-13.4304936774347,
123.838877653668)) ;
#96883 = CARTESIAN_POINT('Ctrl Pts',(-18.2841833571535,-13.4321583972246,
123.871689696396)) ;
#96884 = CARTESIAN_POINT('Ctrl Pts',(-18.3050090129642,-13.4345834722808,
123.918703083063)) ;
#96885 = CARTESIAN_POINT('Ctrl Pts',(-18.3118632856505,-13.4353464774128,
123.933376984394)) ;
#96886 = CARTESIAN_POINT('Ctrl Pts',(-18.3295597723867,-13.437235489409,123.969367760875)) ;
#96887 = CARTESIAN_POINT('Ctrl Pts',(-18.3407418875125,-13.4383607081841,
123.990509830898)) ;
#96888 = CARTESIAN_POINT('Ctrl Pts',(-18.3570015681671,-13.4399142477195,
124.019171732627)) ;
#96889 = CARTESIAN_POINT('Ctrl Pts',(-18.3615501871828,-13.4403407433514,
124.026985329835)) ;
#96890 = CARTESIAN_POINT('Ctrl Pts',(-18.369737453328,-13.4410949238326,124.040695103776)) ;
#96891 = CARTESIAN_POINT('Ctrl Pts',(-18.3733401217708,-13.4414223890476,
124.046612294915)) ;
#96892 = CARTESIAN_POINT('Ctrl Pts',(-18.3807802948143,-13.4420901430436,
124.058600337392)) ;
#96893 = CARTESIAN_POINT('Ctrl Pts',(-18.3846214169675,-13.4424304766152,
124.064668621118)) ;
#96894 = CARTESIAN_POINT('Ctrl Pts',(-18.3992759220869,-13.443711763868,124.087372135911)) ;
#96895 = CARTESIAN_POINT('Ctrl Pts',(-18.4104425147867,-13.4446535682912,
124.103775797351)) ;
#96896 = CARTESIAN_POINT('Ctrl Pts',(-18.426738506524,-13.4459773215147,124.126497501034)) ;
#96897 = CARTESIAN_POINT('Ctrl Pts',(-18.4315372484053,-13.4463613492467,
124.133048749287)) ;
#96898 = CARTESIAN_POINT('Ctrl Pts',(-18.4394708833801,-13.4469868766891,
124.143655034489)) ;
#96899 = CARTESIAN_POINT('Ctrl Pts',(-18.4425663823417,-13.4472286844924,
124.147739200335)) ;
#96900 = CARTESIAN_POINT('Ctrl Pts',(-18.4485403927075,-13.4476910769672,
124.155518500553)) ;
#96901 = CARTESIAN_POINT('Ctrl Pts',(-18.4514146131975,-13.4479116941984,
124.159216812355)) ;
#96902 = CARTESIAN_POINT('Ctrl Pts',(-18.4543308990835,-13.4481337052284,
124.162924794683)) ;
#96903 = CARTESIAN_POINT('Ctrl Pts',(-18.4543516453474,-13.4481352845073,
124.162951170773)) ;
#96904 = CARTESIAN_POINT('Ctrl Pts',(-18.4543843348962,-13.4481377728051,
124.162992727605)) ;
#96905 = CARTESIAN_POINT('Ctrl Pts',(-18.4543962772916,-13.4481386818183,
124.163007908719)) ;
#96906 = CARTESIAN_POINT('Ctrl Pts',(-18.4544203821908,-13.4481405165365,
124.163038549243)) ;
#96907 = CARTESIAN_POINT('Ctrl Pts',(-18.454432544895,-13.4481414422556,124.163054008881)) ;
#96908 = CARTESIAN_POINT('Ctrl Pts',(-18.4544570953238,-13.4481433107562,
124.163085212614)) ;
#96909 = CARTESIAN_POINT('Ctrl Pts',(-18.4544694826408,-13.4481442535054,
124.163100956162)) ;
#96910 = CARTESIAN_POINT('Ctrl Pts',(-18.454494486796,-13.448146156405,124.163132733348)) ;
#96911 = CARTESIAN_POINT('Ctrl Pts',(-18.4545071038768,-13.4481471165727,
124.163148767265)) ;
#96912 = CARTESIAN_POINT('Ctrl Pts',(-18.4545325721937,-13.4481490546581,
124.163181130989)) ;
#96913 = CARTESIAN_POINT('Ctrl Pts',(-18.4545454236522,-13.4481500325916,
124.163197461047)) ;
#96914 = CARTESIAN_POINT('Ctrl Pts',(-18.454571365879,-13.448152006597,124.163230423508)) ;
#96915 = CARTESIAN_POINT('Ctrl Pts',(-18.4545844565788,-13.4481530026625,
124.163247055792)) ;
#96916 = CARTESIAN_POINT('Ctrl Pts',(-18.4546108823239,-13.448155013311,124.163280629006)) ;
#96917 = CARTESIAN_POINT('Ctrl Pts',(-18.4546242175126,-13.4481560279037,
124.163297570085)) ;
#96918 = CARTESIAN_POINT('Ctrl Pts',(-18.4546511375263,-13.448158076005,124.163331767508)) ;
#96919 = CARTESIAN_POINT('Ctrl Pts',(-18.4546647222404,-13.4481591095038,
124.163349023677)) ;
#96920 = CARTESIAN_POINT('Ctrl Pts',(-18.4546921465044,-13.4481611958087,
124.16338385778)) ;
#96921 = CARTESIAN_POINT('Ctrl Pts',(-18.4547059862535,-13.4481622486284,
124.163401435931)) ;
#96922 = CARTESIAN_POINT('Ctrl Pts',(-18.4547339260275,-13.4481643739845,
124.163436920797)) ;
#96923 = CARTESIAN_POINT('Ctrl Pts',(-18.4547480261076,-13.4481654465234,
124.163454827545)) ;
#96924 = CARTESIAN_POINT('Ctrl Pts',(-18.4547764922468,-13.448167611747,124.163490976735)) ;
#96925 = CARTESIAN_POINT('Ctrl Pts',(-18.45479085824,-13.448168704425,124.163509219054)) ;
#96926 = CARTESIAN_POINT('Ctrl Pts',(-18.4548198618314,-13.4481709103497,
124.16354604641)) ;
#96927 = CARTESIAN_POINT('Ctrl Pts',(-18.4548344995653,-13.4481720236051,
124.163564631579)) ;
#96928 = CARTESIAN_POINT('Ctrl Pts',(-18.4548640527607,-13.4481742711451,
124.163602152287)) ;
#96929 = CARTESIAN_POINT('Ctrl Pts',(-18.454878967835,-13.4481754053985,124.163621087291)) ;
#96930 = CARTESIAN_POINT('Ctrl Pts',(-18.454909081508,-13.4481776953702,124.1636593149)) ;
#96931 = CARTESIAN_POINT('Ctrl Pts',(-18.4549242802871,-13.4481788511003,
124.163678607689)) ;
#96932 = CARTESIAN_POINT('Ctrl Pts',(-18.4582459198339,-13.4484314209979,
124.167894715609)) ;
#96933 = CARTESIAN_POINT('Ctrl Pts',(-18.4615800145149,-13.448682588636,124.172069682603)) ;
#96934 = CARTESIAN_POINT('Ctrl Pts',(-18.469942955028,-13.4493068872479,124.18240128202)) ;
#96935 = CARTESIAN_POINT('Ctrl Pts',(-18.4750048947004,-13.4496797235772,
124.188530813012)) ;
#96936 = CARTESIAN_POINT('Ctrl Pts',(-18.4911902337031,-13.4508566868596,
124.207742545554)) ;
#96937 = CARTESIAN_POINT('Ctrl Pts',(-18.5025310157395,-13.4516591195798,
124.22063883992)) ;
#96938 = CARTESIAN_POINT('Ctrl Pts',(-18.5275806219977,-13.4533913520761,
124.247934995264)) ;
#96939 = CARTESIAN_POINT('Ctrl Pts',(-18.5413771755605,-13.4543214285738,
124.262247459655)) ;
#96940 = CARTESIAN_POINT('Ctrl Pts',(-18.5595658342737,-13.4555224978174,
124.280212431811)) ;
#96941 = CARTESIAN_POINT('Ctrl Pts',(-18.5636410836888,-13.4557900253099,
124.28418140786)) ;
#96942 = CARTESIAN_POINT('Ctrl Pts',(-18.5699961422154,-13.456204860294,124.290284361079)) ;
#96943 = CARTESIAN_POINT('Ctrl Pts',(-18.5722565621878,-13.4563519569228,
124.292438421401)) ;
#96944 = CARTESIAN_POINT('Ctrl Pts',(-18.5777752459485,-13.456709993655,124.297656988165)) ;
#96945 = CARTESIAN_POINT('Ctrl Pts',(-18.581042174413,-13.4569210259936,124.300712257513)) ;
#96946 = CARTESIAN_POINT('Ctrl Pts',(-18.587728322913,-13.457351088436,124.306896357689)) ;
#96947 = CARTESIAN_POINT('Ctrl Pts',(-18.5911487235541,-13.4575701283576,
124.31002380376)) ;
#96948 = CARTESIAN_POINT('Ctrl Pts',(-18.5993056857436,-13.4580902188756,
124.317396877365)) ;
#96949 = CARTESIAN_POINT('Ctrl Pts',(-18.6040578538237,-13.4583914226953,
124.321625024442)) ;
#96950 = CARTESIAN_POINT('Ctrl Pts',(-18.6177425552721,-13.4592536229019,
124.333609505238)) ;
#96951 = CARTESIAN_POINT('Ctrl Pts',(-18.6267554478517,-13.4598152893926,
124.34127293834)) ;
#96952 = CARTESIAN_POINT('Ctrl Pts',(-18.6558862676618,-13.4616097768507,
124.365318012487)) ;
#96953 = CARTESIAN_POINT('Ctrl Pts',(-18.6764177550588,-13.4628423650804,
124.381187594996)) ;
#96954 = CARTESIAN_POINT('Ctrl Pts',(-18.703675151774,-13.4644337286175,124.400894564925)) ;
#96955 = CARTESIAN_POINT('Ctrl Pts',(-18.7099513397061,-13.4647972495674,
124.405342075097)) ;
#96956 = CARTESIAN_POINT('Ctrl Pts',(-18.7210834212,-13.4654370641045,124.413072876023)) ;
#96957 = CARTESIAN_POINT('Ctrl Pts',(-18.7259216232483,-13.4657135155103,
124.41638118384)) ;
#96958 = CARTESIAN_POINT('Ctrl Pts',(-18.7360084205432,-13.4662866164862,
124.423171827536)) ;
#96959 = CARTESIAN_POINT('Ctrl Pts',(-18.741260539275,-13.46658322454,124.426648618653)) ;
#96960 = CARTESIAN_POINT('Ctrl Pts',(-18.7466584206567,-13.4668863152612,
124.430161838578)) ;
#96961 = CARTESIAN_POINT('Ctrl Pts',(-18.7467773895922,-13.4668929944967,
124.430239240029)) ;
#96962 = CARTESIAN_POINT('Ctrl Pts',(-18.7543525810557,-13.4673182311975,
124.435165787146)) ;
#96963 = CARTESIAN_POINT('Ctrl Pts',(-18.7618618253275,-13.4677363735785,
124.439932934617)) ;
#96964 = CARTESIAN_POINT('Ctrl Pts',(-18.7878349192858,-13.4691721274749,
124.456024208921)) ;
#96965 = CARTESIAN_POINT('Ctrl Pts',(-18.8065487552903,-13.4701883561081,
124.466936755611)) ;
#96966 = CARTESIAN_POINT('Ctrl Pts',(-18.8284226767592,-13.4713629994707,
124.478920097028)) ;
#96967 = CARTESIAN_POINT('Ctrl Pts',(-18.8313075201354,-13.4715176637053,
124.480485355695)) ;
#96968 = CARTESIAN_POINT('Ctrl Pts',(-18.8375424561477,-13.4718514508138,
124.483835676323)) ;
#96969 = CARTESIAN_POINT('Ctrl Pts',(-18.8408946369089,-13.47203061832,124.485616762594)) ;
#96970 = CARTESIAN_POINT('Ctrl Pts',(-18.8486150408826,-13.4724425281532,
124.489672498521)) ;
#96971 = CARTESIAN_POINT('Ctrl Pts',(-18.8529888612696,-13.4726753493784,
124.491936357139)) ;
#96972 = CARTESIAN_POINT('Ctrl Pts',(-18.8619809682865,-13.4731527803317,
124.496521500682)) ;
#96973 = CARTESIAN_POINT('Ctrl Pts',(-18.8666005510132,-13.473397398353,124.498840036081)) ;
#96974 = CARTESIAN_POINT('Ctrl Pts',(-18.8917829465409,-13.4747269830128,
124.511278358115)) ;
#96975 = CARTESIAN_POINT('Ctrl Pts',(-18.9126142798848,-13.4758124766327,
124.520844292971)) ;
#96976 = CARTESIAN_POINT('Ctrl Pts',(-18.9398469193848,-13.4772099580599,
124.532428485236)) ;
#96977 = CARTESIAN_POINT('Ctrl Pts',(-18.9460115350909,-13.4775249327917,
124.53499098715)) ;
#96978 = CARTESIAN_POINT('Ctrl Pts',(-18.9577436116296,-13.4781217973632,
124.539754742755)) ;
#96979 = CARTESIAN_POINT('Ctrl Pts',(-18.9633068327394,-13.4784037368473,
124.541965908013)) ;
#96980 = CARTESIAN_POINT('Ctrl Pts',(-18.9690054325709,-13.4786914602654,
124.544182250146)) ;
#96981 = CARTESIAN_POINT('Ctrl Pts',(-18.969124692343,-13.4786974812351,124.54422861186)) ;
#96982 = CARTESIAN_POINT('Ctrl Pts',(-18.9756155515057,-13.4790251538126,
124.546750724675)) ;
#96983 = CARTESIAN_POINT('Ctrl Pts',(-18.9820079363085,-13.4793464849441,
124.549172681164)) ;
#96984 = CARTESIAN_POINT('Ctrl Pts',(-18.9984742172146,-13.4801709044593,
124.555253034951)) ;
#96985 = CARTESIAN_POINT('Ctrl Pts',(-19.0085767021514,-13.4806735424703,
124.558832316035)) ;
#96986 = CARTESIAN_POINT('Ctrl Pts',(-19.0460800499892,-13.4825296506793,
124.571563682847)) ;
#96987 = CARTESIAN_POINT('Ctrl Pts',(-19.0737572215603,-13.4838807682486,
124.579871252103)) ;
#96988 = CARTESIAN_POINT('Ctrl Pts',(-19.1083148092527,-13.4855603095389,
124.588914272203)) ;
#96989 = CARTESIAN_POINT('Ctrl Pts',(-19.1149399014898,-13.4858819166606,
124.590588334364)) ;
#96990 = CARTESIAN_POINT('Ctrl Pts',(-19.1253043269892,-13.4863845662226,
124.59311444383)) ;
#96991 = CARTESIAN_POINT('Ctrl Pts',(-19.1290341778102,-13.4865653578815,
124.594004829871)) ;
#96992 = CARTESIAN_POINT('Ctrl Pts',(-19.1379123085385,-13.4869954826592,
124.596079829927)) ;
#96993 = CARTESIAN_POINT('Ctrl Pts',(-19.1430642174333,-13.4872449121367,
124.597248551544)) ;
#96994 = CARTESIAN_POINT('Ctrl Pts',(-19.1544315725255,-13.4877949115265,
124.599749418219)) ;
#96995 = CARTESIAN_POINT('Ctrl Pts',(-19.1606501789442,-13.4880955638614,
124.601066459959)) ;
#96996 = CARTESIAN_POINT('Ctrl Pts',(-19.177091310499,-13.4888898181408,124.604413940863)) ;
#96997 = CARTESIAN_POINT('Ctrl Pts',(-19.1873301056241,-13.4893838145982,
124.606361744655)) ;
#96998 = CARTESIAN_POINT('Ctrl Pts',(-19.2244506232028,-13.4911718042321,
124.612929721153)) ;
#96999 = CARTESIAN_POINT('Ctrl Pts',(-19.2514611964707,-13.492466264447,124.616776119437)) ;
#97000 = CARTESIAN_POINT('Ctrl Pts',(-19.2873013256925,-13.4941707843582,
124.620653991908)) ;
#97001 = CARTESIAN_POINT('Ctrl Pts',(-19.2960342435353,-13.4945852013439,
124.621503288529)) ;
#97002 = CARTESIAN_POINT('Ctrl Pts',(-19.3125239104713,-13.495366194272,124.622926815573)) ;
#97003 = CARTESIAN_POINT('Ctrl Pts',(-19.3202784640329,-13.4957328394796,
124.62352130072)) ;
#97004 = CARTESIAN_POINT('Ctrl Pts',(-19.3282302826886,-13.4961082874633,
124.624054161277)) ;
#97005 = CARTESIAN_POINT('Ctrl Pts',(-19.3284223636885,-13.4961173563258,
124.624066986989)) ;
#97006 = CARTESIAN_POINT('Ctrl Pts',(-19.3288188690456,-13.4961360761891,
124.624093367949)) ;
#97007 = CARTESIAN_POINT('Ctrl Pts',(-19.3290232938787,-13.4961457271714,
124.624106917148)) ;
#97008 = CARTESIAN_POINT('Ctrl Pts',(-19.3294489836675,-13.4961658234418,
124.624135023556)) ;
#97009 = CARTESIAN_POINT('Ctrl Pts',(-19.3296702493529,-13.4961762687049,
124.624149571908)) ;
#97010 = CARTESIAN_POINT('Ctrl Pts',(-19.3301349403587,-13.4961982044705,
124.624179997854)) ;
#97011 = CARTESIAN_POINT('Ctrl Pts',(-19.3303783663683,-13.4962096949208,
124.624195862701)) ;
#97012 = CARTESIAN_POINT('Ctrl Pts',(-19.3308938892488,-13.4962340281482,
124.624229305045)) ;
#97013 = CARTESIAN_POINT('Ctrl Pts',(-19.3311659872356,-13.4962468708573,
124.624246864256)) ;
#97014 = CARTESIAN_POINT('Ctrl Pts',(-19.3317470349285,-13.4962742943557,
124.624284164402)) ;
#97015 = CARTESIAN_POINT('Ctrl Pts',(-19.3320559863537,-13.4962888750531,
124.624303878856)) ;
#97016 = CARTESIAN_POINT('Ctrl Pts',(-19.3327212334083,-13.4963202691753,
124.624346073536)) ;
#97017 = CARTESIAN_POINT('Ctrl Pts',(-19.3330775315159,-13.4963370824656,
124.624368514813)) ;
#97018 = CARTESIAN_POINT('Ctrl Pts',(-19.3338511584282,-13.4963735868428,
124.624416899019)) ;
#97019 = CARTESIAN_POINT('Ctrl Pts',(-19.3342684908802,-13.4963932777302,
124.624442783561)) ;
#97020 = CARTESIAN_POINT('Ctrl Pts',(-19.3351823007901,-13.4964363908314,
124.624498987966)) ;
#97021 = CARTESIAN_POINT('Ctrl Pts',(-19.3356787836563,-13.4964598127409,
124.624529218392)) ;
#97022 = CARTESIAN_POINT('Ctrl Pts',(-19.3367751881016,-13.4965115322254,
124.624595301752)) ;
#97023 = CARTESIAN_POINT('Ctrl Pts',(-19.3373751180179,-13.4965398293348,
124.624631014453)) ;
#97024 = CARTESIAN_POINT('Ctrl Pts',(-19.3387114246526,-13.4966028534743,
124.624709567254)) ;
#97025 = CARTESIAN_POINT('Ctrl Pts',(-19.3394478144212,-13.4966375797755,
124.624752181922)) ;
#97026 = CARTESIAN_POINT('Ctrl Pts',(-19.3411025488181,-13.49671560423,124.624846429001)) ;
#97027 = CARTESIAN_POINT('Ctrl Pts',(-19.3420209142465,-13.4967589012191,
124.62489768921)) ;
#97028 = CARTESIAN_POINT('Ctrl Pts',(-19.3432835284905,-13.4968184201703,
124.624966726058)) ;
#97029 = CARTESIAN_POINT('Ctrl Pts',(-19.3436277278366,-13.4968346447347,
124.624985399166)) ;
#97030 = CARTESIAN_POINT('Ctrl Pts',(-19.344613080972,-13.496881089173,124.625038434836)) ;
#97031 = CARTESIAN_POINT('Ctrl Pts',(-19.3452542541173,-13.4969113080038,
124.625072435624)) ;
#97032 = CARTESIAN_POINT('Ctrl Pts',(-19.3471062634393,-13.4969985865253,
124.625169173664)) ;
#97033 = CARTESIAN_POINT('Ctrl Pts',(-19.3483171671606,-13.497055642592,124.625230606657)) ;
#97034 = CARTESIAN_POINT('Ctrl Pts',(-19.3641171032813,-13.4977999983073,
124.626008476717)) ;
#97035 = CARTESIAN_POINT('Ctrl Pts',(-19.3787178156327,-13.4984865393675,
124.626463572181)) ;
#97036 = CARTESIAN_POINT('Ctrl Pts',(-19.4054261995314,-13.4997425601292,
124.626814161937)) ;
#97037 = CARTESIAN_POINT('Ctrl Pts',(-19.4175308846078,-13.5003118805728,
124.626792154159)) ;
#97038 = CARTESIAN_POINT('Ctrl Pts',(-19.4342371707054,-13.501099167948,124.626512098489)) ;
#97039 = CARTESIAN_POINT('Ctrl Pts',(-19.438840674241,-13.501316272718,124.626408746316)) ;
#97040 = CARTESIAN_POINT('Ctrl Pts',(-19.4477384728886,-13.501736342966,124.626158367149)) ;
#97041 = CARTESIAN_POINT('Ctrl Pts',(-19.4520327913469,-13.5019392898085,
124.626014724822)) ;
#97042 = CARTESIAN_POINT('Ctrl Pts',(-19.4730015931659,-13.5029310925452,
124.625201949896)) ;
#97043 = CARTESIAN_POINT('Ctrl Pts',(-19.4896618335716,-13.5037215440508,
124.624212092281)) ;
#97044 = CARTESIAN_POINT('Ctrl Pts',(-19.5198974968035,-13.5051573036587,
124.621789667075)) ;
#97045 = CARTESIAN_POINT('Ctrl Pts',(-19.5334793329442,-13.5058027182553,
124.620470915758)) ;
#97046 = CARTESIAN_POINT('Ctrl Pts',(-19.5541126298452,-13.5067834606179,
124.618116015626)) ;
#97047 = CARTESIAN_POINT('Ctrl Pts',(-19.5611819268799,-13.5071195312457,
124.617246149856)) ;
#97048 = CARTESIAN_POINT('Ctrl Pts',(-19.5745918239888,-13.5077571664879,
124.615476242574)) ;
#97049 = CARTESIAN_POINT('Ctrl Pts',(-19.5809337541553,-13.508058781177,124.614588133414)) ;
#97050 = CARTESIAN_POINT('Ctrl Pts',(-19.5875457393529,-13.5083733464568,
124.613608844766)) ;
#97051 = CARTESIAN_POINT('Ctrl Pts',(-19.5878230860399,-13.5083865414305,
124.613567669349)) ;
#97052 = CARTESIAN_POINT('Ctrl Pts',(-19.588397602504,-13.5084138749038,124.613482172264)) ;
#97053 = CARTESIAN_POINT('Ctrl Pts',(-19.588694770147,-13.5084280133326,124.613437836361)) ;
#97054 = CARTESIAN_POINT('Ctrl Pts',(-19.5965404944298,-13.508801297996,124.612264318779)) ;
#97055 = CARTESIAN_POINT('Ctrl Pts',(-19.6040782729423,-13.5091600833775,
124.61106413678)) ;
#97056 = CARTESIAN_POINT('Ctrl Pts',(-19.6247587556578,-13.51014522316,124.607571215617)) ;
#97057 = CARTESIAN_POINT('Ctrl Pts',(-19.6378757784219,-13.5107709100776,
124.605132908048)) ;
#97058 = CARTESIAN_POINT('Ctrl Pts',(-19.6534960643099,-13.5115183806056,
124.601962260983)) ;
#97059 = CARTESIAN_POINT('Ctrl Pts',(-19.6560404610727,-13.5116402141508,
124.601437289398)) ;
#97060 = CARTESIAN_POINT('Ctrl Pts',(-19.6592408402569,-13.5117935685159,
124.600766262927)) ;
#97061 = CARTESIAN_POINT('Ctrl Pts',(-19.6598984117627,-13.5118250835864,
124.600627819653)) ;
#97062 = CARTESIAN_POINT('Ctrl Pts',(-19.6614990516764,-13.5119018111709,
124.600289438282)) ;
#97063 = CARTESIAN_POINT('Ctrl Pts',(-19.6624419976112,-13.5119470241558,
124.600088923144)) ;
#97064 = CARTESIAN_POINT('Ctrl Pts',(-19.6823447831539,-13.5129016051274,
124.595831878255)) ;
#97065 = CARTESIAN_POINT('Ctrl Pts',(-19.7012049917796,-13.513811480666,124.591323193894)) ;
#97066 = CARTESIAN_POINT('Ctrl Pts',(-19.7282116696,-13.5151256574852,124.584179560815)) ;
#97067 = CARTESIAN_POINT('Ctrl Pts',(-19.7364508672912,-13.5155280968149,
124.581906894152)) ;
#97068 = CARTESIAN_POINT('Ctrl Pts',(-19.7517889883416,-13.5162803152717,
124.577501413677)) ;
#97069 = CARTESIAN_POINT('Ctrl Pts',(-19.7588937094624,-13.5166299733507,
124.575390201642)) ;
#97070 = CARTESIAN_POINT('Ctrl Pts',(-19.7736932522357,-13.5173609688278,
124.570844636687)) ;
#97071 = CARTESIAN_POINT('Ctrl Pts',(-19.781384035399,-13.5177423424347,124.568398353187)) ;
#97072 = CARTESIAN_POINT('Ctrl Pts',(-19.8016972216982,-13.518753621969,124.561713547474)) ;
#97073 = CARTESIAN_POINT('Ctrl Pts',(-19.8142752895256,-13.5193839350338,
124.557343845585)) ;
#97074 = CARTESIAN_POINT('Ctrl Pts',(-19.8450815710289,-13.5209371465221,
124.546070710902)) ;
#97075 = CARTESIAN_POINT('Ctrl Pts',(-19.8632204367783,-13.5218595909063,
124.53893365864)) ;
#97076 = CARTESIAN_POINT('Ctrl Pts',(-19.8911035099361,-13.5232888436824,
124.52718023569)) ;
#97077 = CARTESIAN_POINT('Ctrl Pts',(-19.9009711721303,-13.5237970143589,
124.522865372571)) ;
#97078 = CARTESIAN_POINT('Ctrl Pts',(-19.9213400607644,-13.5248514722218,
124.513634088004)) ;
#97079 = CARTESIAN_POINT('Ctrl Pts',(-19.9318309107245,-13.5253976440036,
124.508697379023)) ;
#97080 = CARTESIAN_POINT('Ctrl Pts',(-19.9675468860051,-13.527269203917,124.491261689226)) ;
#97081 = CARTESIAN_POINT('Ctrl Pts',(-19.9924073327646,-13.5285926852364,
124.478036632061)) ;
#97082 = CARTESIAN_POINT('Ctrl Pts',(-20.0227563091423,-13.5302455362025,
124.460512601585)) ;
#97083 = CARTESIAN_POINT('Ctrl Pts',(-20.02869730688,-13.5305709343063,124.45701440077)) ;
#97084 = CARTESIAN_POINT('Ctrl Pts',(-20.0414762145855,-13.5312751997801,
124.449342648812)) ;
#97085 = CARTESIAN_POINT('Ctrl Pts',(-20.0483032425237,-13.5316542457621,
124.445151669537)) ;
#97086 = CARTESIAN_POINT('Ctrl Pts',(-20.0656193105432,-13.532622792184,124.4342844294)) ;
#97087 = CARTESIAN_POINT('Ctrl Pts',(-20.0760482175288,-13.5332126838663,
124.427514118614)) ;
#97088 = CARTESIAN_POINT('Ctrl Pts',(-20.0993970556466,-13.5345463400912,
124.411841733607)) ;
#97089 = CARTESIAN_POINT('Ctrl Pts',(-20.1122522298494,-13.5352898039799,
124.402847019914)) ;
#97090 = CARTESIAN_POINT('Ctrl Pts',(-20.129822676762,-13.5363177188711,124.390039093196)) ;
#97091 = CARTESIAN_POINT('Ctrl Pts',(-20.1346889767581,-13.5366037013361,
124.386435801663)) ;
#97092 = CARTESIAN_POINT('Ctrl Pts',(-20.1435271964023,-13.5371254675079,
124.379788599214)) ;
#97093 = CARTESIAN_POINT('Ctrl Pts',(-20.1475076330916,-13.53736134206,124.376756242005)) ;
#97094 = CARTESIAN_POINT('Ctrl Pts',(-20.1515488499621,-13.5376017383622,
124.373637938221)) ;
#97095 = CARTESIAN_POINT('Ctrl Pts',(-20.1516284616327,-13.5376064745179,
124.373576492098)) ;
#97096 = CARTESIAN_POINT('Ctrl Pts',(-20.1517885406491,-13.5376159984709,
124.373452907701)) ;
#97097 = CARTESIAN_POINT('Ctrl Pts',(-20.1518690077677,-13.5376207862629,
124.373390769257)) ;
#97098 = CARTESIAN_POINT('Ctrl Pts',(-20.1520308950442,-13.5376304193068,
124.373265723969)) ;
#97099 = CARTESIAN_POINT('Ctrl Pts',(-20.1521123149319,-13.5376352645518,
124.373202816944)) ;
#97100 = CARTESIAN_POINT('Ctrl Pts',(-20.1522762037894,-13.5376450182451,
124.373076159096)) ;
#97101 = CARTESIAN_POINT('Ctrl Pts',(-20.1523586725455,-13.5376499266909,
124.373012408004)) ;
#97102 = CARTESIAN_POINT('Ctrl Pts',(-20.1525247544395,-13.5376598124891,
124.372883987023)) ;
#97103 = CARTESIAN_POINT('Ctrl Pts',(-20.1526083673882,-13.5376647898415,
124.372819316801)) ;
#97104 = CARTESIAN_POINT('Ctrl Pts',(-20.1565241020009,-13.5378979066095,
124.369789885017)) ;
#97105 = CARTESIAN_POINT('Ctrl Pts',(-20.1603384697342,-13.5381258406053,
124.366802231859)) ;
#97106 = CARTESIAN_POINT('Ctrl Pts',(-20.1691938297751,-13.5386570489025,
124.359780281156)) ;
#97107 = CARTESIAN_POINT('Ctrl Pts',(-20.1742207413676,-13.5389601594828,
124.35572845484)) ;
#97108 = CARTESIAN_POINT('Ctrl Pts',(-20.1878883477874,-13.5397887783108,
124.344531096488)) ;
#97109 = CARTESIAN_POINT('Ctrl Pts',(-20.1964628078282,-13.5403135878407,
124.337305711612)) ;
#97110 = CARTESIAN_POINT('Ctrl Pts',(-20.2207449111832,-13.5418159365084,
124.316262422201)) ;
#97111 = CARTESIAN_POINT('Ctrl Pts',(-20.2361972706496,-13.5427918201599,
124.302156182834)) ;
#97112 = CARTESIAN_POINT('Ctrl Pts',(-20.2604696853981,-13.5443672064874,
124.278820946732)) ;
#97113 = CARTESIAN_POINT('Ctrl Pts',(-20.2695219397479,-13.5449647586521,
124.269839750026)) ;
#97114 = CARTESIAN_POINT('Ctrl Pts',(-20.2821176175632,-13.5458118909743,
124.256943198299)) ;
#97115 = CARTESIAN_POINT('Ctrl Pts',(-20.2857794884998,-13.5460600968923,
124.253144666046)) ;
#97116 = CARTESIAN_POINT('Ctrl Pts',(-20.2917420621039,-13.5464674944649,
124.246878384435)) ;
#97117 = CARTESIAN_POINT('Ctrl Pts',(-20.294057439055,-13.5466265095813,124.244424686955)) ;
#97118 = CARTESIAN_POINT('Ctrl Pts',(-20.2988889636719,-13.5469600630228,
124.239261612456)) ;
#97119 = CARTESIAN_POINT('Ctrl Pts',(-20.3014030224666,-13.5471346244423,
124.236550329751)) ;
#97120 = CARTESIAN_POINT('Ctrl Pts',(-20.3066896946718,-13.5475038393261,
124.230796464982)) ;
#97121 = CARTESIAN_POINT('Ctrl Pts',(-20.3094592997375,-13.5476985263424,
124.227751184542)) ;
#97122 = CARTESIAN_POINT('Ctrl Pts',(-20.3160790568499,-13.5481669238772,
124.220397788963)) ;
#97123 = CARTESIAN_POINT('Ctrl Pts',(-20.3199140513206,-13.5484408076547,
124.216076176231)) ;
#97124 = CARTESIAN_POINT('Ctrl Pts',(-20.3304241427183,-13.5491984705193,
124.204060909508)) ;
#97125 = CARTESIAN_POINT('Ctrl Pts',(-20.3370335144526,-13.5496829536307,
124.196310443725)) ;
#97126 = CARTESIAN_POINT('Ctrl Pts',(-20.362593417188,-13.5515881439498,124.165562800586)) ;
#97127 = CARTESIAN_POINT('Ctrl Pts',(-20.3807926137771,-13.5530159478525,
124.141954852798)) ;
#97128 = CARTESIAN_POINT('Ctrl Pts',(-20.4032415394135,-13.5548539395069,
124.110506613991)) ;
#97129 = CARTESIAN_POINT('Ctrl Pts',(-20.4082989131651,-13.5552735323794,
124.103255778991)) ;
#97130 = CARTESIAN_POINT('Ctrl Pts',(-20.4152402147271,-13.5558570739101,
124.093068750837)) ;
#97131 = CARTESIAN_POINT('Ctrl Pts',(-20.4171912852663,-13.5560219651554,
124.090178707413)) ;
#97132 = CARTESIAN_POINT('Ctrl Pts',(-20.4207076152799,-13.5563207262438,
124.084921442523)) ;
#97133 = CARTESIAN_POINT('Ctrl Pts',(-20.4222770721548,-13.556454655888,124.08255706298)) ;
#97134 = CARTESIAN_POINT('Ctrl Pts',(-20.425284904907,-13.5567124609697,124.077991137257)) ;
#97135 = CARTESIAN_POINT('Ctrl Pts',(-20.4267244445915,-13.5568363527486,
124.075790378253)) ;
#97136 = CARTESIAN_POINT('Ctrl Pts',(-20.4281645332563,-13.5569608068971,
124.073573098306)) ;
#97137 = CARTESIAN_POINT('Ctrl Pts',(-20.4281722358149,-13.5569614725761,
124.073561238355)) ;
#97138 = CARTESIAN_POINT('Ctrl Pts',(-20.4281877571685,-13.5569628140097,
124.073537338565)) ;
#97139 = CARTESIAN_POINT('Ctrl Pts',(-20.4281955763669,-13.5569634897996,
124.073525298091)) ;
#97140 = CARTESIAN_POINT('Ctrl Pts',(-20.4301247688294,-13.5571302279076,
124.070554495734)) ;
#97141 = CARTESIAN_POINT('Ctrl Pts',(-20.4320332501104,-13.557296102685,124.067587372509)) ;
#97142 = CARTESIAN_POINT('Ctrl Pts',(-20.4362705302379,-13.5576664932113,
124.060936159175)) ;
#97143 = CARTESIAN_POINT('Ctrl Pts',(-20.438592484424,-13.5578709102727,124.057247763645)) ;
#97144 = CARTESIAN_POINT('Ctrl Pts',(-20.4450344081987,-13.5584422082349,
124.046891660436)) ;
#97145 = CARTESIAN_POINT('Ctrl Pts',(-20.4491097839389,-13.5588084880854,
124.040196449447)) ;
#97146 = CARTESIAN_POINT('Ctrl Pts',(-20.4640293625576,-13.560168700002,124.015143210974)) ;
#97147 = CARTESIAN_POINT('Ctrl Pts',(-20.4744545086066,-13.561157847172,123.996540154476)) ;
#97148 = CARTESIAN_POINT('Ctrl Pts',(-20.4940481412781,-13.5631139910882,
123.959311509913)) ;
#97149 = CARTESIAN_POINT('Ctrl Pts',(-20.5032395469785,-13.5640809222002,
123.940706255608)) ;
#97150 = CARTESIAN_POINT('Ctrl Pts',(-20.5140840992029,-13.5652926751113,
123.917260947361)) ;
#97151 = CARTESIAN_POINT('Ctrl Pts',(-20.5161892768624,-13.5655314924234,
123.912633669285)) ;
#97152 = CARTESIAN_POINT('Ctrl Pts',(-20.5194407783164,-13.5659061057922,
123.905366046913)) ;
#97153 = CARTESIAN_POINT('Ctrl Pts',(-20.5206068700668,-13.5660416479672,
123.902734601443)) ;
#97154 = CARTESIAN_POINT('Ctrl Pts',(-20.522920382198,-13.5663129777833,123.897463352778)) ;
#97155 = CARTESIAN_POINT('Ctrl Pts',(-20.5240677940841,-13.5664487645478,
123.894823566433)) ;
#97156 = CARTESIAN_POINT('Ctrl Pts',(-20.5263474717599,-13.5667210105193,
123.889527437453)) ;
#97157 = CARTESIAN_POINT('Ctrl Pts',(-20.5274796698494,-13.566857469595,123.886871086242)) ;
#97158 = CARTESIAN_POINT('Ctrl Pts',(-20.5300589287941,-13.567171231901,123.880759339595)) ;
#97159 = CARTESIAN_POINT('Ctrl Pts',(-20.5314994977795,-13.5673486136518,
123.877301241108)) ;
#97160 = CARTESIAN_POINT('Ctrl Pts',(-20.535208837648,-13.567810984029,123.868279617654)) ;
#97161 = CARTESIAN_POINT('Ctrl Pts',(-20.5374523663653,-13.5680962643996,
123.862705842021)) ;
#97162 = CARTESIAN_POINT('Ctrl Pts',(-20.5442882790718,-13.5689831831001,
123.845352318652)) ;
#97163 = CARTESIAN_POINT('Ctrl Pts',(-20.5487381724704,-13.5695862670895,
123.833517425835)) ;
#97164 = CARTESIAN_POINT('Ctrl Pts',(-20.563809263402,-13.5717210352755,123.791452823134)) ;
#97165 = CARTESIAN_POINT('Ctrl Pts',(-20.5734188180678,-13.5732557483291,
123.760874073529)) ;
#97166 = CARTESIAN_POINT('Ctrl Pts',(-20.5832553636488,-13.5750373220317,
123.72461784502)) ;
#97167 = CARTESIAN_POINT('Ctrl Pts',(-20.5846658596313,-13.575298969527,123.719274960244)) ;
#97168 = CARTESIAN_POINT('Ctrl Pts',(-20.5867812686191,-13.575701146792,123.711034505897)) ;
#97169 = CARTESIAN_POINT('Ctrl Pts',(-20.5875120429498,-13.5758419769676,
123.708143669462)) ;
#97170 = CARTESIAN_POINT('Ctrl Pts',(-20.5889492161943,-13.5761227877677,
123.70236903395)) ;
#97171 = CARTESIAN_POINT('Ctrl Pts',(-20.5896557009296,-13.5762627684677,
123.699485277874)) ;
#97172 = CARTESIAN_POINT('Ctrl Pts',(-20.590880934677,-13.5765090090445,123.694403543943)) ;
#97173 = CARTESIAN_POINT('Ctrl Pts',(-20.5914041386817,-13.5766153194584,
123.692206658159)) ;
#97174 = CARTESIAN_POINT('Ctrl Pts',(-20.5919384467653,-13.5767251020549,
123.689935062756)) ;
#97175 = CARTESIAN_POINT('Ctrl Pts',(-20.5919556717079,-13.5767286425319,
123.689861800868)) ;
#97176 = CARTESIAN_POINT('Ctrl Pts',(-20.5919907343717,-13.5767358521328,
123.689712608574)) ;
#97177 = CARTESIAN_POINT('Ctrl Pts',(-20.5920085715905,-13.5767395212516,
123.689636678042)) ;
#97178 = CARTESIAN_POINT('Ctrl Pts',(-20.592044883944,-13.5767469936052,123.68948203457)) ;
#97179 = CARTESIAN_POINT('Ctrl Pts',(-20.5920633585364,-13.5767507968345,
123.68940332149)) ;
#97180 = CARTESIAN_POINT('Ctrl Pts',(-20.5921009717066,-13.5767585430991,
123.689242994402)) ;
#97181 = CARTESIAN_POINT('Ctrl Pts',(-20.5921201097037,-13.5767624861294,
123.689161380221)) ;
#97182 = CARTESIAN_POINT('Ctrl Pts',(-20.5921590767254,-13.5767705179166,
123.688995127553)) ;
#97183 = CARTESIAN_POINT('Ctrl Pts',(-20.5921789051036,-13.5767746066644,
123.688910488958)) ;
#97184 = CARTESIAN_POINT('Ctrl Pts',(-20.5922052732939,-13.576780046324,123.688797880372)) ;
#97185 = CARTESIAN_POINT('Ctrl Pts',(-20.5922118211656,-13.5767813973192,
123.688769912415)) ;
#97186 = CARTESIAN_POINT('Ctrl Pts',(-20.5922256441169,-13.57678424976,123.688710860942)) ;
#97187 = CARTESIAN_POINT('Ctrl Pts',(-20.5922329189778,-13.5767857512061,
123.688679777307)) ;
#97188 = CARTESIAN_POINT('Ctrl Pts',(-20.592248276592,-13.5767889213429,123.68861414646)) ;
#97189 = CARTESIAN_POINT('Ctrl Pts',(-20.5922563590754,-13.5767905900342,
123.688579599102)) ;
#97190 = CARTESIAN_POINT('Ctrl Pts',(-20.5922734215406,-13.5767941133364,
123.688506653759)) ;
#97191 = CARTESIAN_POINT('Ctrl Pts',(-20.5922824011327,-13.5767959679365,
123.688468255835)) ;
#97192 = CARTESIAN_POINT('Ctrl Pts',(-20.592301357184,-13.5767998837959,123.688387179448)) ;
#97193 = CARTESIAN_POINT('Ctrl Pts',(-20.5923113332024,-13.5768019450502,
123.688344500886)) ;
#97194 = CARTESIAN_POINT('Ctrl Pts',(-20.5923323922763,-13.5768062972492,
123.688254385728)) ;
#97195 = CARTESIAN_POINT('Ctrl Pts',(-20.5923434747913,-13.5768085881885,
123.688206948992)) ;
#97196 = CARTESIAN_POINT('Ctrl Pts',(-20.5923668689407,-13.5768134253248,
123.688106787301)) ;
#97197 = CARTESIAN_POINT('Ctrl Pts',(-20.5923791799008,-13.5768159715138,
123.6880540622)) ;
#97198 = CARTESIAN_POINT('Ctrl Pts',(-20.5938377371731,-13.5771177163749,
123.681805499849)) ;
#97199 = CARTESIAN_POINT('Ctrl Pts',(-20.5952352991861,-13.5774163677189,
123.675598379099)) ;
#97200 = CARTESIAN_POINT('Ctrl Pts',(-20.5983891212009,-13.5781136263492,
123.661058974758)) ;
#97201 = CARTESIAN_POINT('Ctrl Pts',(-20.6001066681349,-13.5785118396116,
123.652718635992)) ;
#97202 = CARTESIAN_POINT('Ctrl Pts',(-20.6076278468565,-13.5803470921298,
123.614147862253)) ;
#97203 = CARTESIAN_POINT('Ctrl Pts',(-20.6123688956798,-13.5817785183569,
123.583722085553)) ;
#97204 = CARTESIAN_POINT('Ctrl Pts',(-20.6170455689385,-13.5836633139606,
123.543788256835)) ;
#97205 = CARTESIAN_POINT('Ctrl Pts',(-20.6180328089848,-13.5841058231419,
123.534415511227)) ;
#97206 = CARTESIAN_POINT('Ctrl Pts',(-20.619408736992,-13.5848003846422,123.519712333182)) ;
#97207 = CARTESIAN_POINT('Ctrl Pts',(-20.6198714761203,-13.585051922661,123.514389188381)) ;
#97208 = CARTESIAN_POINT('Ctrl Pts',(-20.6206565654059,-13.5855141605686,
123.504610612477)) ;
#97209 = CARTESIAN_POINT('Ctrl Pts',(-20.6209894875762,-13.5857247890175,
123.50015611956)) ;
#97210 = CARTESIAN_POINT('Ctrl Pts',(-20.6216717351584,-13.5861911479725,
123.490296332517)) ;
#97211 = CARTESIAN_POINT('Ctrl Pts',(-20.6220094939214,-13.5864469424831,
123.484890335814)) ;
#97212 = CARTESIAN_POINT('Ctrl Pts',(-20.622709210363,-13.5870408421842,123.472343367396)) ;
#97213 = CARTESIAN_POINT('Ctrl Pts',(-20.6230443024971,-13.5873790788204,
123.465201102944)) ;
#97214 = CARTESIAN_POINT('Ctrl Pts',(-20.6238130875013,-13.588335719782,123.44500882138)) ;
#97215 = CARTESIAN_POINT('Ctrl Pts',(-20.624099479888,-13.5889546812866,123.431954198421)) ;
#97216 = CARTESIAN_POINT('Ctrl Pts',(-20.6243312103492,-13.5908447731047,
123.392099202608)) ;
#97217 = CARTESIAN_POINT('Ctrl Pts',(-20.6236003082956,-13.5921152280196,
123.3653029068)) ;
#97218 = CARTESIAN_POINT('Ctrl Pts',(-20.6213519582103,-13.5938775473575,
123.32809536005)) ;
#97219 = CARTESIAN_POINT('Ctrl Pts',(-20.6205848168732,-13.5943723779706,
123.317646653178)) ;
#97220 = CARTESIAN_POINT('Ctrl Pts',(-20.6187561124718,-13.5953745536532,
123.296490159051)) ;
#97221 = CARTESIAN_POINT('Ctrl Pts',(-20.6176872478047,-13.5958818317924,
123.285783922206)) ;
#97222 = CARTESIAN_POINT('Ctrl Pts',(-20.6118016941146,-13.5983456768661,
123.233823558094)) ;
#97223 = CARTESIAN_POINT('Ctrl Pts',(-20.6050138650644,-13.600295510766,123.192820658949)) ;
#97224 = CARTESIAN_POINT('Ctrl Pts',(-20.5893956535576,-13.6037363828272,
123.12141206059)) ;
#97225 = CARTESIAN_POINT('Ctrl Pts',(-20.5814527566936,-13.6052222365077,
123.090852587564)) ;
#97226 = CARTESIAN_POINT('Ctrl Pts',(-20.5680475149523,-13.6074078920833,
123.046458366207)) ;
#97227 = CARTESIAN_POINT('Ctrl Pts',(-20.5635102765326,-13.6081057742435,
123.03236848346)) ;
#97228 = CARTESIAN_POINT('Ctrl Pts',(-20.5587133983318,-13.6088050314642,
123.018355650104)) ;
#97229 = CARTESIAN_POINT('Origin',(-19.4092696390481,30.19753203383,123.411833654989)) ;
#97230 = CARTESIAN_POINT('',(-20.5587133983317,-12.870840300276,123.018355650104)) ;
#97231 = CARTESIAN_POINT('',(-20.5587133983317,-12.8888247888664,123.018355650104)) ;
#97232 = CARTESIAN_POINT('',(-20.5587133983318,30.19753203383,123.018355650104)) ;
#97233 = CARTESIAN_POINT('Ctrl Pts',(-20.5587133983318,-13.2308616644972,
123.018355650104)) ;
#97234 = CARTESIAN_POINT('Ctrl Pts',(-20.5651030596262,-13.229929779781,123.037021385437)) ;
#97235 = CARTESIAN_POINT('Ctrl Pts',(-20.571110201071,-13.2289823495695,123.05606688297)) ;
#97236 = CARTESIAN_POINT('Ctrl Pts',(-20.5766346967623,-13.2280348698646,
123.075225992995)) ;
#97237 = CARTESIAN_POINT('Ctrl Pts',(-20.5804556631602,-13.2273795542814,
123.088477214412)) ;
#97238 = CARTESIAN_POINT('Ctrl Pts',(-20.5840467550479,-13.2267242150223,
123.101782361935)) ;
#97239 = CARTESIAN_POINT('Ctrl Pts',(-20.5873888704399,-13.2260739790644,
123.115049267412)) ;
#97240 = CARTESIAN_POINT('Ctrl Pts',(-20.5958751718356,-13.2244228995324,
123.148736601706)) ;
#97241 = CARTESIAN_POINT('Ctrl Pts',(-20.6029877979522,-13.2227693158545,
123.183089803483)) ;
#97242 = CARTESIAN_POINT('Ctrl Pts',(-20.6086118707812,-13.2211109075677,
123.217864308786)) ;
#97243 = CARTESIAN_POINT('Ctrl Pts',(-20.6142359436102,-13.2194524992809,
123.252638814089)) ;
#97244 = CARTESIAN_POINT('Ctrl Pts',(-20.6183711963401,-13.2177892663854,
123.287833939062)) ;
#97245 = CARTESIAN_POINT('Ctrl Pts',(-20.6209576635384,-13.2161188884183,
123.323188139639)) ;
#97246 = CARTESIAN_POINT('Ctrl Pts',(-20.626117181998,-13.2127867966906,123.393713159487)) ;
#97247 = CARTESIAN_POINT('Ctrl Pts',(-20.6251084153611,-13.2094316614767,
123.464545406272)) ;
#97248 = CARTESIAN_POINT('Ctrl Pts',(-20.6179500569869,-13.2061226175737,
123.53486837926)) ;
#97249 = CARTESIAN_POINT('Ctrl Pts',(-20.6114440133148,-13.2031151145932,
123.598783080019)) ;
#97250 = CARTESIAN_POINT('Ctrl Pts',(-20.5998719182444,-13.2001058428465,
123.662103461852)) ;
#97251 = CARTESIAN_POINT('Ctrl Pts',(-20.5833655484139,-13.1970492393283,
123.724155110697)) ;
#97252 = CARTESIAN_POINT('Ctrl Pts',(-20.5818199248864,-13.1967630250753,
123.729965503253)) ;
#97253 = CARTESIAN_POINT('Ctrl Pts',(-20.5802310740959,-13.1964763958136,
123.735764779462)) ;
#97254 = CARTESIAN_POINT('Ctrl Pts',(-20.5785991271999,-13.196189314135,123.74155239001)) ;
#97255 = CARTESIAN_POINT('Ctrl Pts',(-20.5629158502188,-13.1934304121803,
123.797172275376)) ;
#97256 = CARTESIAN_POINT('Ctrl Pts',(-20.5432693640621,-13.1907006475101,
123.851638852534)) ;
#97257 = CARTESIAN_POINT('Ctrl Pts',(-20.5198427099514,-13.1879971448032,
123.904452524167)) ;
#97258 = CARTESIAN_POINT('Ctrl Pts',(-20.5145280138739,-13.1873838137161,
123.916434116251)) ;
#97259 = CARTESIAN_POINT('Ctrl Pts',(-20.5090189587703,-13.1867718342768,
123.928330711781)) ;
#97260 = CARTESIAN_POINT('Ctrl Pts',(-20.5033180308026,-13.1861611729122,
123.940136610295)) ;
#97261 = CARTESIAN_POINT('Ctrl Pts',(-20.4776135363666,-13.1834078068395,
123.993367357002)) ;
#97262 = CARTESIAN_POINT('Ctrl Pts',(-20.4480363827302,-13.1806156356085,
124.044686828789)) ;
#97263 = CARTESIAN_POINT('Ctrl Pts',(-20.4148677357801,-13.1778111404931,
124.093609544805)) ;
#97264 = CARTESIAN_POINT('Ctrl Pts',(-20.4085646074065,-13.1772781946433,
124.102906461857)) ;
#97265 = CARTESIAN_POINT('Ctrl Pts',(-20.4021319119919,-13.176744803748,124.112116902308)) ;
#97266 = CARTESIAN_POINT('Ctrl Pts',(-20.3955717634326,-13.1762111495361,
124.121237641107)) ;
#97267 = CARTESIAN_POINT('Ctrl Pts',(-20.3584318078858,-13.1731898926962,
124.172874251236)) ;
#97268 = CARTESIAN_POINT('Ctrl Pts',(-20.3172676470507,-13.1702142455432,
124.221543946994)) ;
#97269 = CARTESIAN_POINT('Ctrl Pts',(-20.2725129555952,-13.1672162128464,
124.266735329173)) ;
#97270 = CARTESIAN_POINT('Ctrl Pts',(-20.2673412360118,-13.1668697690679,
124.271957511443)) ;
#97271 = CARTESIAN_POINT('Ctrl Pts',(-20.2621216145638,-13.1665230263657,
124.27713328278)) ;
#97272 = CARTESIAN_POINT('Ctrl Pts',(-20.2568547957218,-13.1661758798175,
124.282261881939)) ;
#97273 = CARTESIAN_POINT('Ctrl Pts',(-20.2060103624581,-13.1628246216797,
124.331771980072)) ;
#97274 = CARTESIAN_POINT('Ctrl Pts',(-20.1509030738596,-13.1594555857011,
124.376749628861)) ;
#97275 = CARTESIAN_POINT('Ctrl Pts',(-20.0922049214542,-13.1561418975459,
124.416644729834)) ;
#97276 = CARTESIAN_POINT('Ctrl Pts',(-20.0625828370052,-13.1544696413275,
124.436777834569)) ;
#97277 = CARTESIAN_POINT('Ctrl Pts',(-20.0321001427256,-13.1527935023082,
124.455575601458)) ;
#97278 = CARTESIAN_POINT('Ctrl Pts',(-20.0009853414478,-13.1511142506408,
124.472926687489)) ;
#97279 = CARTESIAN_POINT('Ctrl Pts',(-19.9710941646612,-13.1495010374305,
124.489595422582)) ;
#97280 = CARTESIAN_POINT('Ctrl Pts',(-19.940620277451,-13.147884951575,124.504929131994)) ;
#97281 = CARTESIAN_POINT('Ctrl Pts',(-19.9097829203064,-13.1462666758921,
124.518871301761)) ;
#97282 = CARTESIAN_POINT('Ctrl Pts',(-19.89019337095,-13.14523866006,124.527728118559)) ;
#97283 = CARTESIAN_POINT('Ctrl Pts',(-19.8702108645291,-13.1442031299505,
124.536131563851)) ;
#97284 = CARTESIAN_POINT('Ctrl Pts',(-19.850079646816,-13.1431759272749,124.54396988051)) ;
#97285 = CARTESIAN_POINT('Ctrl Pts',(-19.8343292839389,-13.1423722593042,
124.550102461931)) ;
#97286 = CARTESIAN_POINT('Ctrl Pts',(-19.8184884430473,-13.1415736887748,
124.555890025945)) ;
#97287 = CARTESIAN_POINT('Ctrl Pts',(-19.8026819097733,-13.1407878025743,
124.561299914315)) ;
#97288 = CARTESIAN_POINT('Ctrl Pts',(-19.7848840081771,-13.1399029073845,
124.567391361388)) ;
#97289 = CARTESIAN_POINT('Ctrl Pts',(-19.7667158870795,-13.1390131360211,
124.573143159454)) ;
#97290 = CARTESIAN_POINT('Ctrl Pts',(-19.7484539454112,-13.1381271180561,
124.578452659807)) ;
#97291 = CARTESIAN_POINT('Ctrl Pts',(-19.7364611963144,-13.1375452636541,
124.581939447068)) ;
#97292 = CARTESIAN_POINT('Ctrl Pts',(-19.724428382192,-13.1369650279592,124.58523648351)) ;
#97293 = CARTESIAN_POINT('Ctrl Pts',(-19.7124372447582,-13.1363888549909,
124.588326450944)) ;
#97294 = CARTESIAN_POINT('Ctrl Pts',(-19.6790232593382,-13.1347833162944,
124.596936820673)) ;
#97295 = CARTESIAN_POINT('Ctrl Pts',(-19.644923205786,-13.1331490770808,124.604200845067)) ;
#97296 = CARTESIAN_POINT('Ctrl Pts',(-19.6103888679249,-13.1314967446217,
124.609997647046)) ;
#97297 = CARTESIAN_POINT('Ctrl Pts',(-19.5758545300639,-13.1298444121627,
124.615794449025)) ;
#97298 = CARTESIAN_POINT('Ctrl Pts',(-19.5408866318659,-13.1281739864582,
124.620123739065)) ;
#97299 = CARTESIAN_POINT('Ctrl Pts',(-19.5057550181026,-13.1264960747798,
124.622922614444)) ;
#97300 = CARTESIAN_POINT('Ctrl Pts',(-19.4350404472996,-13.1231186949368,
124.628556322947)) ;
#97301 = CARTESIAN_POINT('Ctrl Pts',(-19.3639599033745,-13.119800985813,124.627984868216)) ;
#97302 = CARTESIAN_POINT('Ctrl Pts',(-19.2933549850892,-13.1164657148701,
124.621217667238)) ;
#97303 = CARTESIAN_POINT('Ctrl Pts',(-19.2283137701815,-13.1133932649695,
124.61498372513)) ;
#97304 = CARTESIAN_POINT('Ctrl Pts',(-19.16385600908,-13.1102924643637,124.603506258005)) ;
#97305 = CARTESIAN_POINT('Ctrl Pts',(-19.1006866708454,-13.1072237698506,
124.586917672335)) ;
#97306 = CARTESIAN_POINT('Ctrl Pts',(-19.0955850924919,-13.1069759409839,
124.585577972222)) ;
#97307 = CARTESIAN_POINT('Ctrl Pts',(-19.0904919120722,-13.1067283215208,
124.584204963757)) ;
#97308 = CARTESIAN_POINT('Ctrl Pts',(-19.0854074984666,-13.106480943306,124.582798731319)) ;
#97309 = CARTESIAN_POINT('Ctrl Pts',(-19.0283917691888,-13.1037068870597,
124.567029485503)) ;
#97310 = CARTESIAN_POINT('Ctrl Pts',(-18.9725714701789,-13.1009347849524,
124.547103588077)) ;
#97311 = CARTESIAN_POINT('Ctrl Pts',(-18.9184743782479,-13.0981286305584,
124.523213836593)) ;
#97312 = CARTESIAN_POINT('Ctrl Pts',(-18.9083633281646,-13.0976041445536,
124.518748707967)) ;
#97313 = CARTESIAN_POINT('Ctrl Pts',(-18.8983124239469,-13.0970784689761,
124.514145243963)) ;
#97314 = CARTESIAN_POINT('Ctrl Pts',(-18.8883250403597,-13.0965513687291,
124.509404892396)) ;
#97315 = CARTESIAN_POINT('Ctrl Pts',(-18.8360528442201,-13.0937926194271,
124.484594732187)) ;
#97316 = CARTESIAN_POINT('Ctrl Pts',(-18.7855858381871,-13.0910584749846,
124.45606112771)) ;
#97317 = CARTESIAN_POINT('Ctrl Pts',(-18.737387336142,-13.0883504306553,124.424068838693)) ;
#97318 = CARTESIAN_POINT('Ctrl Pts',(-18.7265267868874,-13.0877402281059,
124.41686002896)) ;
#97319 = CARTESIAN_POINT('Ctrl Pts',(-18.7157813118055,-13.0871313507488,
124.409475790609)) ;
#97320 = CARTESIAN_POINT('Ctrl Pts',(-18.7051560265558,-13.0865238156907,
124.40191946783)) ;
#97321 = CARTESIAN_POINT('Ctrl Pts',(-18.6535295136305,-13.0835719027972,
124.365204538634)) ;
#97322 = CARTESIAN_POINT('Ctrl Pts',(-18.6048193468118,-13.0805866753734,
124.324478100412)) ;
#97323 = CARTESIAN_POINT('Ctrl Pts',(-18.559536039588,-13.0775726118254,124.280164643745)) ;
#97324 = CARTESIAN_POINT('Ctrl Pts',(-18.5543893100279,-13.0772300447536,
124.275128143734)) ;
#97325 = CARTESIAN_POINT('Ctrl Pts',(-18.5492868133224,-13.0768871051843,
124.27004535092)) ;
#97326 = CARTESIAN_POINT('Ctrl Pts',(-18.5442292731428,-13.0765437996927,
124.264916922578)) ;
#97327 = CARTESIAN_POINT('Ctrl Pts',(-18.4944270647826,-13.0731632290955,
124.21441666993)) ;
#97328 = CARTESIAN_POINT('Ctrl Pts',(-18.449127153017,-13.069833350483,124.159633049982)) ;
#97329 = CARTESIAN_POINT('Ctrl Pts',(-18.4088767576804,-13.0665160349233,
124.101224675379)) ;
#97330 = CARTESIAN_POINT('Ctrl Pts',(-18.3880836527802,-13.0648023302542,
124.071051270869)) ;
#97331 = CARTESIAN_POINT('Ctrl Pts',(-18.3686831483461,-13.0630787969676,
124.039969361738)) ;
#97332 = CARTESIAN_POINT('Ctrl Pts',(-18.350789329446,-13.0613571613528,124.008210490782)) ;
#97333 = CARTESIAN_POINT('Ctrl Pts',(-18.3342661469707,-13.0597674001297,
123.978884295912)) ;
#97334 = CARTESIAN_POINT('Ctrl Pts',(-18.3190273256574,-13.0581792569958,
123.948981553369)) ;
#97335 = CARTESIAN_POINT('Ctrl Pts',(-18.3051259677726,-13.0566019647331,
123.918699168974)) ;
#97336 = CARTESIAN_POINT('Ctrl Pts',(-18.2958227679809,-13.0555463941068,
123.898433301818)) ;
#97337 = CARTESIAN_POINT('Ctrl Pts',(-18.287015690004,-13.0544857440984,123.877766169464)) ;
#97338 = CARTESIAN_POINT('Ctrl Pts',(-18.2788142679726,-13.0534299520535,
123.856936508375)) ;
#97339 = CARTESIAN_POINT('Ctrl Pts',(-18.2720489498095,-13.0525590336846,
123.839754209505)) ;
#97340 = CARTESIAN_POINT('Ctrl Pts',(-18.2656949317367,-13.0516914209316,
123.822461883274)) ;
#97341 = CARTESIAN_POINT('Ctrl Pts',(-18.2597886515046,-13.0508326916541,
123.805202890392)) ;
#97342 = CARTESIAN_POINT('Ctrl Pts',(-18.2540260376267,-13.0499948503975,
123.788363711079)) ;
#97343 = CARTESIAN_POINT('Ctrl Pts',(-18.2485605249512,-13.0491462820869,
123.771171431162)) ;
#97344 = CARTESIAN_POINT('Ctrl Pts',(-18.2434971135028,-13.0482990036882,
123.753915976615)) ;
#97345 = CARTESIAN_POINT('Ctrl Pts',(-18.2404390039636,-13.0477872794919,
123.743494332889)) ;
#97346 = CARTESIAN_POINT('Ctrl Pts',(-18.2375266199112,-13.0472760258174,
123.73304999958)) ;
#97347 = CARTESIAN_POINT('Ctrl Pts',(-18.2347742440617,-13.0467678900933,
123.722649457742)) ;
#97348 = CARTESIAN_POINT('Ctrl Pts',(-18.2264046704784,-13.045222723457,123.691022926708)) ;
#97349 = CARTESIAN_POINT('Ctrl Pts',(-18.2192341431193,-13.0436600419622,
123.658745397244)) ;
#97350 = CARTESIAN_POINT('Ctrl Pts',(-18.2133759357069,-13.0420909675042,
123.626039505502)) ;
#97351 = CARTESIAN_POINT('Ctrl Pts',(-18.2075421751403,-13.0405284409401,
123.593470098496)) ;
#97352 = CARTESIAN_POINT('Ctrl Pts',(-18.2030100267147,-13.0389595746585,
123.560476491226)) ;
#97353 = CARTESIAN_POINT('Ctrl Pts',(-18.1998422604654,-13.0373953518967,
123.52729495595)) ;
#97354 = CARTESIAN_POINT('Ctrl Pts',(-18.1994702427518,-13.0372116519234,
123.523398166252)) ;
#97355 = CARTESIAN_POINT('Ctrl Pts',(-18.1991169845345,-13.0370280159926,
123.519498797244)) ;
#97356 = CARTESIAN_POINT('Ctrl Pts',(-18.1987825410503,-13.0368444618938,
123.515597240442)) ;
#97357 = CARTESIAN_POINT('Ctrl Pts',(-18.1927631009154,-13.0335407859016,
123.445375547651)) ;
#97358 = CARTESIAN_POINT('Ctrl Pts',(-18.1928675682951,-13.0302328466101,
123.374779012882)) ;
#97359 = CARTESIAN_POINT('Ctrl Pts',(-18.1990833786732,-13.0268838791217,
123.304618398216)) ;
#97360 = CARTESIAN_POINT('Ctrl Pts',(-18.204661352787,-13.0238785664076,123.241657324985)) ;
#97361 = CARTESIAN_POINT('Ctrl Pts',(-18.2151513512694,-13.020898497468,123.179196145019)) ;
#97362 = CARTESIAN_POINT('Ctrl Pts',(-18.2304396956473,-13.0179372381882,
123.117884916896)) ;
#97363 = CARTESIAN_POINT('Ctrl Pts',(-18.2322927026136,-13.017578322014,123.110453756921)) ;
#97364 = CARTESIAN_POINT('Ctrl Pts',(-18.2342161373331,-13.0172196821609,
123.103039478988)) ;
#97365 = CARTESIAN_POINT('Ctrl Pts',(-18.2362097459809,-13.0168613071728,
123.095643232361)) ;
#97366 = CARTESIAN_POINT('Ctrl Pts',(-18.2515352549037,-13.0141063637269,
123.038785912937)) ;
#97367 = CARTESIAN_POINT('Ctrl Pts',(-18.27098761908,-13.011330055596,122.983085004515)) ;
#97368 = CARTESIAN_POINT('Ctrl Pts',(-18.2943798093764,-13.0085420966995,
122.929063975142)) ;
#97369 = CARTESIAN_POINT('Ctrl Pts',(-18.2990774697369,-13.0079822139425,
122.918215378021)) ;
#97370 = CARTESIAN_POINT('Ctrl Pts',(-18.3039338633981,-13.0074218613175,
122.90743447064)) ;
#97371 = CARTESIAN_POINT('Ctrl Pts',(-18.3089472378951,-13.0068611174976,
122.896725404613)) ;
#97372 = CARTESIAN_POINT('Ctrl Pts',(-18.3334911262173,-13.0041158939557,
122.84429722061)) ;
#97373 = CARTESIAN_POINT('Ctrl Pts',(-18.36177130619,-13.0013947918626,122.793656640004)) ;
#97374 = CARTESIAN_POINT('Ctrl Pts',(-18.3935250077928,-12.9986707661173,
122.745268774306)) ;
#97375 = CARTESIAN_POINT('Ctrl Pts',(-18.4006875968857,-12.9980563156405,
122.734354065733)) ;
#97376 = CARTESIAN_POINT('Ctrl Pts',(-18.4080267390288,-12.9974417164067,
122.723553871416)) ;
#97377 = CARTESIAN_POINT('Ctrl Pts',(-18.415539101432,-12.9968266580205,122.712873345176)) ;
#97378 = CARTESIAN_POINT('Ctrl Pts',(-18.4508447834905,-12.9939360818386,
122.662678314185)) ;
#97379 = CARTESIAN_POINT('Ctrl Pts',(-18.4899294490682,-12.9910307279178,
122.615200191548)) ;
#97380 = CARTESIAN_POINT('Ctrl Pts',(-18.5324020700621,-12.98814332233,122.570912040006)) ;
#97381 = CARTESIAN_POINT('Ctrl Pts',(-18.5387515083003,-12.9877116700557,
122.564291189295)) ;
#97382 = CARTESIAN_POINT('Ctrl Pts',(-18.5451765897313,-12.9872804189035,
122.557741570101)) ;
#97383 = CARTESIAN_POINT('Ctrl Pts',(-18.5516759296756,-12.9868496782118,
122.551264700326)) ;
#97384 = CARTESIAN_POINT('Ctrl Pts',(-18.6014123332493,-12.9835534215054,
122.501700250435)) ;
#97385 = CARTESIAN_POINT('Ctrl Pts',(-18.6553788032398,-12.9802519555717,
122.456515862803)) ;
#97386 = CARTESIAN_POINT('Ctrl Pts',(-18.712960946223,-12.9769173597984,122.416243327404)) ;
#97387 = CARTESIAN_POINT('Ctrl Pts',(-18.7438881619006,-12.9751263572873,
122.394613055871)) ;
#97388 = CARTESIAN_POINT('Ctrl Pts',(-18.7757829518889,-12.9733486752165,
122.374457367794)) ;
#97389 = CARTESIAN_POINT('Ctrl Pts',(-18.8084081076775,-12.9715813245094,
122.355892692528)) ;
#97390 = CARTESIAN_POINT('Ctrl Pts',(-18.837127721745,-12.970025542506,122.339550385616)) ;
#97391 = CARTESIAN_POINT('Ctrl Pts',(-18.8664126210517,-12.9684777663934,
122.324440405561)) ;
#97392 = CARTESIAN_POINT('Ctrl Pts',(-18.8960887573314,-12.9669359571817,
122.310611025942)) ;
#97393 = CARTESIAN_POINT('Ctrl Pts',(-18.9169673695376,-12.96585121905,122.30088138151)) ;
#97394 = CARTESIAN_POINT('Ctrl Pts',(-18.9382553584935,-12.9647552497427,
122.291688495408)) ;
#97395 = CARTESIAN_POINT('Ctrl Pts',(-18.9597182873768,-12.9636626863374,
122.283139950614)) ;
#97396 = CARTESIAN_POINT('Ctrl Pts',(-18.9783815268816,-12.9627126402082,
122.275706503867)) ;
#97397 = CARTESIAN_POINT('Ctrl Pts',(-18.9971764742932,-12.9617651693813,
122.268759589331)) ;
#97398 = CARTESIAN_POINT('Ctrl Pts',(-19.0159377952944,-12.9608298976992,
122.262339872155)) ;
#97399 = CARTESIAN_POINT('Ctrl Pts',(-19.031969968729,-12.9600306769079,122.256854010091)) ;
#97400 = CARTESIAN_POINT('Ctrl Pts',(-19.0483449489832,-12.9592217466141,
122.251630103386)) ;
#97401 = CARTESIAN_POINT('Ctrl Pts',(-19.0647600599905,-12.9584173094523,
122.246776125928)) ;
#97402 = CARTESIAN_POINT('Ctrl Pts',(-19.0738959072207,-12.9579695991071,
122.244074639688)) ;
#97403 = CARTESIAN_POINT('Ctrl Pts',(-19.0830438689744,-12.9575232805054,
122.241486858984)) ;
#97404 = CARTESIAN_POINT('Ctrl Pts',(-19.0921497777622,-12.9570808020558,
122.239024680918)) ;
#97405 = CARTESIAN_POINT('Ctrl Pts',(-19.1231074167154,-12.9555764944238,
122.230653938207)) ;
#97406 = CARTESIAN_POINT('Ctrl Pts',(-19.1547161144588,-12.95405373186,122.223426935519)) ;
#97407 = CARTESIAN_POINT('Ctrl Pts',(-19.1867552061612,-12.9525179515628,
122.21745799246)) ;
#97408 = CARTESIAN_POINT('Ctrl Pts',(-19.2186512193937,-12.9509890296715,
122.21151570519)) ;
#97409 = CARTESIAN_POINT('Ctrl Pts',(-19.250973204314,-12.9494472060551,122.206820489916)) ;
#97410 = CARTESIAN_POINT('Ctrl Pts',(-19.2834868818629,-12.9478978453932,
122.203436123512)) ;
#97411 = CARTESIAN_POINT('Ctrl Pts',(-19.2881465797159,-12.9476757987626,
122.202951093025)) ;
#97412 = CARTESIAN_POINT('Ctrl Pts',(-19.2928101957978,-12.9474535973271,
122.202492900932)) ;
#97413 = CARTESIAN_POINT('Ctrl Pts',(-19.2974770238049,-12.9472312568782,
122.202061648675)) ;
#97414 = CARTESIAN_POINT('Ctrl Pts',(-19.3681091091339,-12.943866151171,122.195534678719)) ;
#97415 = CARTESIAN_POINT('Ctrl Pts',(-19.4391888785763,-12.9405486009369,
122.195206717904)) ;
#97416 = CARTESIAN_POINT('Ctrl Pts',(-19.5098704045165,-12.9372019724685,
122.201079599835)) ;
#97417 = CARTESIAN_POINT('Ctrl Pts',(-19.5750398193813,-12.9341163314023,
122.206494484049)) ;
#97418 = CARTESIAN_POINT('Ctrl Pts',(-19.6396940363769,-12.9310133340658,
122.217168874093)) ;
#97419 = CARTESIAN_POINT('Ctrl Pts',(-19.7031246513772,-12.9279493121566,
122.232980344431)) ;
#97420 = CARTESIAN_POINT('Ctrl Pts',(-19.7084896913727,-12.9276901533877,
122.23431769818)) ;
#97421 = CARTESIAN_POINT('Ctrl Pts',(-19.7138459830822,-12.9274312734486,
122.235691772185)) ;
#97422 = CARTESIAN_POINT('Ctrl Pts',(-19.7191931003158,-12.927172706425,122.237102475425)) ;
#97423 = CARTESIAN_POINT('Ctrl Pts',(-19.7767824747378,-12.9243878950051,
122.252295992515)) ;
#97424 = CARTESIAN_POINT('Ctrl Pts',(-19.8332074062206,-12.9215938819148,
122.271716377075)) ;
#97425 = CARTESIAN_POINT('Ctrl Pts',(-19.8879296000351,-12.9187651732054,
122.295173215181)) ;
#97426 = CARTESIAN_POINT('Ctrl Pts',(-19.8978131881789,-12.9182542691295,
122.299409845894)) ;
#97427 = CARTESIAN_POINT('Ctrl Pts',(-19.9076412784483,-12.9177422332347,
122.303778022898)) ;
#97428 = CARTESIAN_POINT('Ctrl Pts',(-19.917410761548,-12.917228915314,122.308276454066)) ;
#97429 = CARTESIAN_POINT('Ctrl Pts',(-19.9698458561983,-12.9144738182957,
122.332420583461)) ;
#97430 = CARTESIAN_POINT('Ctrl Pts',(-20.0205275411525,-12.9117487873609,
122.360291612852)) ;
#97431 = CARTESIAN_POINT('Ctrl Pts',(-20.0689919763738,-12.9090471640156,
122.39163155064)) ;
#97432 = CARTESIAN_POINT('Ctrl Pts',(-20.0800508385963,-12.9084306938099,
122.398782857624)) ;
#97433 = CARTESIAN_POINT('Ctrl Pts',(-20.0909943581407,-12.9078154424008,
122.406114599069)) ;
#97434 = CARTESIAN_POINT('Ctrl Pts',(-20.1018172131709,-12.9072013306773,
122.413623379716)) ;
#97435 = CARTESIAN_POINT('Ctrl Pts',(-20.1529268781081,-12.9043012600087,
122.449082716634)) ;
#97436 = CARTESIAN_POINT('Ctrl Pts',(-20.2012709035099,-12.9013695518875,
122.48844329651)) ;
#97437 = CARTESIAN_POINT('Ctrl Pts',(-20.2463568603113,-12.8984127829644,
122.531304904702)) ;
#97438 = CARTESIAN_POINT('Ctrl Pts',(-20.2523609389698,-12.898019031241,122.537012767754)) ;
#97439 = CARTESIAN_POINT('Ctrl Pts',(-20.2583072855055,-12.8976248350859,
122.542782659255)) ;
#97440 = CARTESIAN_POINT('Ctrl Pts',(-20.2641947794291,-12.8972302100307,
122.548613578514)) ;
#97441 = CARTESIAN_POINT('Ctrl Pts',(-20.314383161087,-12.8938661992751,122.598319685223)) ;
#97442 = CARTESIAN_POINT('Ctrl Pts',(-20.3601611471171,-12.8905427332555,
122.6523320438)) ;
#97443 = CARTESIAN_POINT('Ctrl Pts',(-20.4009740199394,-12.8872427554171,
122.710001540445)) ;
#97444 = CARTESIAN_POINT('Ctrl Pts',(-20.4233513650492,-12.8854334061153,
122.741621226575)) ;
#97445 = CARTESIAN_POINT('Ctrl Pts',(-20.4441862691242,-12.8836140272436,
122.774275982503)) ;
#97446 = CARTESIAN_POINT('Ctrl Pts',(-20.4633562400616,-12.8817930848427,
122.807724944864)) ;
#97447 = CARTESIAN_POINT('Ctrl Pts',(-20.4789775775287,-12.880309224703,122.834982029952)) ;
#97448 = CARTESIAN_POINT('Ctrl Pts',(-20.4934941190755,-12.878824326319,122.862765821822)) ;
#97449 = CARTESIAN_POINT('Ctrl Pts',(-20.5068633098144,-12.8773429707999,
122.890936323475)) ;
#97450 = CARTESIAN_POINT('Ctrl Pts',(-20.5168522759644,-12.8762361566011,
122.911984283141)) ;
#97451 = CARTESIAN_POINT('Ctrl Pts',(-20.5262810415717,-12.8751269962437,
122.933425113875)) ;
#97452 = CARTESIAN_POINT('Ctrl Pts',(-20.5350451807603,-12.8740258444861,
122.955023710081)) ;
#97453 = CARTESIAN_POINT('Ctrl Pts',(-20.5435823739876,-12.8729532068744,
122.976063014144)) ;
#97454 = CARTESIAN_POINT('Ctrl Pts',(-20.5514890204704,-12.8718881684698,
122.997251507192)) ;
#97455 = CARTESIAN_POINT('Ctrl Pts',(-20.5587133983318,-12.870840300276,123.018355650104)) ;
#97456 = CARTESIAN_POINT('Ctrl Pts',(-20.5587133983318,-12.8888247888663,
123.018355650104)) ;
#97457 = CARTESIAN_POINT('Ctrl Pts',(-20.5521333479611,-12.8897813285136,
122.99913374255)) ;
#97458 = CARTESIAN_POINT('Ctrl Pts',(-20.544986195852,-12.8907544247006,122.979842107534)) ;
#97459 = CARTESIAN_POINT('Ctrl Pts',(-20.5373508716136,-12.8917312466635,
122.960747600208)) ;
#97460 = CARTESIAN_POINT('Ctrl Pts',(-20.5316648181194,-12.8924586895019,
122.946527851745)) ;
#97461 = CARTESIAN_POINT('Ctrl Pts',(-20.5257090870077,-12.893188198594,122.932417187712)) ;
#97462 = CARTESIAN_POINT('Ctrl Pts',(-20.5195338126948,-12.8939144748306,
122.918518987863)) ;
#97463 = CARTESIAN_POINT('Ctrl Pts',(-20.5053980204641,-12.8955769904473,
122.886704682055)) ;
#97464 = CARTESIAN_POINT('Ctrl Pts',(-20.4897738045878,-12.8972454835374,
122.855236420196)) ;
#97465 = CARTESIAN_POINT('Ctrl Pts',(-20.472720199896,-12.8989103111607,122.824365527584)) ;
#97466 = CARTESIAN_POINT('Ctrl Pts',(-20.4556665952043,-12.900575138784,122.793494634972)) ;
#97467 = CARTESIAN_POINT('Ctrl Pts',(-20.4371837991994,-12.9022363009406,
122.763221757143)) ;
#97468 = CARTESIAN_POINT('Ctrl Pts',(-20.4173808136202,-12.9038841546903,
122.733779264997)) ;
#97469 = CARTESIAN_POINT('Ctrl Pts',(-20.378126552407,-12.9071505955648,122.675417192628)) ;
#97470 = CARTESIAN_POINT('Ctrl Pts',(-20.3338886395771,-12.9104588638225,
122.620591045438)) ;
#97471 = CARTESIAN_POINT('Ctrl Pts',(-20.2851865110284,-12.9138225142835,
122.569921825006)) ;
#97472 = CARTESIAN_POINT('Ctrl Pts',(-20.2421545541131,-12.916794549922,122.525151795944)) ;
#97473 = CARTESIAN_POINT('Ctrl Pts',(-20.1957262083222,-12.919718658498,122.483724696734)) ;
#97474 = CARTESIAN_POINT('Ctrl Pts',(-20.1463750247226,-12.9226187056346,
122.446058553584)) ;
#97475 = CARTESIAN_POINT('Ctrl Pts',(-20.1393717500589,-12.9230302424035,
122.440713467068)) ;
#97476 = CARTESIAN_POINT('Ctrl Pts',(-20.1323096729016,-12.9234412946332,
122.435444052637)) ;
#97477 = CARTESIAN_POINT('Ctrl Pts',(-20.1251902035935,-12.9238519305238,
122.430251441751)) ;
#97478 = CARTESIAN_POINT('Ctrl Pts',(-20.0775529762442,-12.9265995447674,
122.395507056373)) ;
#97479 = CARTESIAN_POINT('Ctrl Pts',(-20.0274189221845,-12.9293831647335,
122.36425951725)) ;
#97480 = CARTESIAN_POINT('Ctrl Pts',(-19.9752633934627,-12.9321792524141,
122.33680018293)) ;
#97481 = CARTESIAN_POINT('Ctrl Pts',(-19.9650803310329,-12.9327251722065,
122.331438908248)) ;
#97482 = CARTESIAN_POINT('Ctrl Pts',(-19.9548202906176,-12.9332715672717,
122.3262219041)) ;
#97483 = CARTESIAN_POINT('Ctrl Pts',(-19.9444869290103,-12.9338182624219,
122.321151139951)) ;
#97484 = CARTESIAN_POINT('Ctrl Pts',(-19.8921031518617,-12.9365896700241,
122.295445489721)) ;
#97485 = CARTESIAN_POINT('Ctrl Pts',(-19.8378976694709,-12.9393311003954,
122.273533346428)) ;
#97486 = CARTESIAN_POINT('Ctrl Pts',(-19.7823758000423,-12.9420751350089,
122.255616681963)) ;
#97487 = CARTESIAN_POINT('Ctrl Pts',(-19.7706215724554,-12.9426560593849,
122.251823644123)) ;
#97488 = CARTESIAN_POINT('Ctrl Pts',(-19.7588084136355,-12.9432371004799,
122.248209505671)) ;
#97489 = CARTESIAN_POINT('Ctrl Pts',(-19.7469412273492,-12.9438185674378,
122.244775903831)) ;
#97490 = CARTESIAN_POINT('Ctrl Pts',(-19.6865738302043,-12.9467764418596,
122.227309454672)) ;
#97491 = CARTESIAN_POINT('Ctrl Pts',(-19.6249018821105,-12.949750672126,122.214546021405)) ;
#97492 = CARTESIAN_POINT('Ctrl Pts',(-19.5625626760622,-12.9527091008562,
122.206617018493)) ;
#97493 = CARTESIAN_POINT('Ctrl Pts',(-19.554847738741,-12.9530752282689,122.205635745802)) ;
#97494 = CARTESIAN_POINT('Ctrl Pts',(-19.5471225956678,-12.9534411136671,
122.204728452756)) ;
#97495 = CARTESIAN_POINT('Ctrl Pts',(-19.5393884676709,-12.9538066960978,
122.203895334328)) ;
#97496 = CARTESIAN_POINT('Ctrl Pts',(-19.4692865579104,-12.9571203245475,
122.19634397328)) ;
#97497 = CARTESIAN_POINT('Ctrl Pts',(-19.3986312606187,-12.9604271439176,
122.194907283884)) ;
#97498 = CARTESIAN_POINT('Ctrl Pts',(-19.3282399792359,-12.9637793859921,
122.199612515792)) ;
#97499 = CARTESIAN_POINT('Ctrl Pts',(-19.2928625679178,-12.965464163487,122.201977282015)) ;
#97500 = CARTESIAN_POINT('Ctrl Pts',(-19.2576349916118,-12.9671409241981,
122.205892055812)) ;
#97501 = CARTESIAN_POINT('Ctrl Pts',(-19.2228061543919,-12.9688031493527,
122.21130157921)) ;
#97502 = CARTESIAN_POINT('Ctrl Pts',(-19.1879773171721,-12.9704653745073,
122.216711102609)) ;
#97503 = CARTESIAN_POINT('Ctrl Pts',(-19.1535478436083,-12.9721130641054,
122.223615141076)) ;
#97504 = CARTESIAN_POINT('Ctrl Pts',(-19.1197512600762,-12.973739699374,122.23190780803)) ;
#97505 = CARTESIAN_POINT('Ctrl Pts',(-19.0997129733655,-12.9747041454949,
122.236824601997)) ;
#97506 = CARTESIAN_POINT('Ctrl Pts',(-19.0796177689363,-12.9756793751788,
122.24230102622)) ;
#97507 = CARTESIAN_POINT('Ctrl Pts',(-19.0597343062078,-12.976654697032,122.248274053086)) ;
#97508 = CARTESIAN_POINT('Ctrl Pts',(-19.0449255259917,-12.977381096008,122.252722636479)) ;
#97509 = CARTESIAN_POINT('Ctrl Pts',(-19.030234031092,-12.9781075461099,122.257445598432)) ;
#97510 = CARTESIAN_POINT('Ctrl Pts',(-19.0157652488497,-12.9788296304523,
122.262398928274)) ;
#97511 = CARTESIAN_POINT('Ctrl Pts',(-18.997310390654,-12.9797506453602,122.268716875306)) ;
#97512 = CARTESIAN_POINT('Ctrl Pts',(-18.9787817776044,-12.9806863048851,
122.275561190029)) ;
#97513 = CARTESIAN_POINT('Ctrl Pts',(-18.9604534337523,-12.9816216662129,
122.282847423918)) ;
#97514 = CARTESIAN_POINT('Ctrl Pts',(-18.9477794349783,-12.9822684659684,
122.287885834378)) ;
#97515 = CARTESIAN_POINT('Ctrl Pts',(-18.9352009150736,-12.9829151231355,
122.293134502465)) ;
#97516 = CARTESIAN_POINT('Ctrl Pts',(-18.9228031507999,-12.9835566968411,
122.298551906331)) ;
#97517 = CARTESIAN_POINT('Ctrl Pts',(-18.8909815562634,-12.9852034371626,
122.312456867373)) ;
#97518 = CARTESIAN_POINT('Ctrl Pts',(-18.8594704563973,-12.9868560446172,
122.327856212618)) ;
#97519 = CARTESIAN_POINT('Ctrl Pts',(-18.8285359486612,-12.9885147179043,
122.344690610719)) ;
#97520 = CARTESIAN_POINT('Ctrl Pts',(-18.7976014409252,-12.9901733911914,
122.36152500882)) ;
#97521 = CARTESIAN_POINT('Ctrl Pts',(-18.7672442409463,-12.9918381303111,
122.379794248709)) ;
#97522 = CARTESIAN_POINT('Ctrl Pts',(-18.7377099123456,-12.9935091339629,
122.39938443179)) ;
#97523 = CARTESIAN_POINT('Ctrl Pts',(-18.6786227542836,-12.9968521880147,
122.438577069614)) ;
#97524 = CARTESIAN_POINT('Ctrl Pts',(-18.6230826776324,-13.000197572698,122.482866292867)) ;
#97525 = CARTESIAN_POINT('Ctrl Pts',(-18.5717344340444,-13.0035326050172,
122.531731003894)) ;
#97526 = CARTESIAN_POINT('Ctrl Pts',(-18.5247437552054,-13.0065846165696,
122.576448910136)) ;
#97527 = CARTESIAN_POINT('Ctrl Pts',(-18.4813955849673,-13.0096473642193,
122.624878003455)) ;
#97528 = CARTESIAN_POINT('Ctrl Pts',(-18.4421536815968,-13.0127043920218,
122.676488415712)) ;
#97529 = CARTESIAN_POINT('Ctrl Pts',(-18.438776795943,-13.0129674586022,122.680929649336)) ;
#97530 = CARTESIAN_POINT('Ctrl Pts',(-18.435430293391,-13.0132304828264,122.685394420443)) ;
#97531 = CARTESIAN_POINT('Ctrl Pts',(-18.4321144560272,-13.0134934542082,
122.689882379362)) ;
#97532 = CARTESIAN_POINT('Ctrl Pts',(-18.3973394741381,-13.0162513774819,
122.736950034672)) ;
#97533 = CARTESIAN_POINT('Ctrl Pts',(-18.3659920401579,-13.0189973645648,
122.786501245856)) ;
#97534 = CARTESIAN_POINT('Ctrl Pts',(-18.3383622492015,-13.0217630898231,
122.838071283918)) ;
#97535 = CARTESIAN_POINT('Ctrl Pts',(-18.3326963269523,-13.0223302451917,
122.848646529548)) ;
#97536 = CARTESIAN_POINT('Ctrl Pts',(-18.3271865893633,-13.0228982305889,
122.859306579928)) ;
#97537 = CARTESIAN_POINT('Ctrl Pts',(-18.3218353067289,-13.0234673191557,
122.870047286594)) ;
#97538 = CARTESIAN_POINT('Ctrl Pts',(-18.2960311604381,-13.0262114920266,
122.921839498857)) ;
#97539 = CARTESIAN_POINT('Ctrl Pts',(-18.273946562433,-13.0289466035877,122.975445942036)) ;
#97540 = CARTESIAN_POINT('Ctrl Pts',(-18.2557823112103,-13.0316624975888,
123.030372148933)) ;
#97541 = CARTESIAN_POINT('Ctrl Pts',(-18.2516903406755,-13.0322743234269,
123.042745707164)) ;
#97542 = CARTESIAN_POINT('Ctrl Pts',(-18.2477971303781,-13.0328851739874,
123.055186165822)) ;
#97543 = CARTESIAN_POINT('Ctrl Pts',(-18.2441046359624,-13.033494933158,123.067687738743)) ;
#97544 = CARTESIAN_POINT('Ctrl Pts',(-18.2261808912318,-13.036454766401,123.128371649544)) ;
#97545 = CARTESIAN_POINT('Ctrl Pts',(-18.2130166903095,-13.0394380498732,
123.190407590526)) ;
#97546 = CARTESIAN_POINT('Ctrl Pts',(-18.2047511162301,-13.042438965811,123.253148355502)) ;
#97547 = CARTESIAN_POINT('Ctrl Pts',(-18.2038177968771,-13.0427778186112,
123.26023282049)) ;
#97548 = CARTESIAN_POINT('Ctrl Pts',(-18.2029468824761,-13.0431168962275,
123.267326259419)) ;
#97549 = CARTESIAN_POINT('Ctrl Pts',(-18.2021385327264,-13.0434561902842,
123.274427729951)) ;
#97550 = CARTESIAN_POINT('Ctrl Pts',(-18.1941414732614,-13.0468128496365,
123.34468306455)) ;
#97551 = CARTESIAN_POINT('Ctrl Pts',(-18.1922918880808,-13.0501297950685,
123.415526871215)) ;
#97552 = CARTESIAN_POINT('Ctrl Pts',(-18.1966167976812,-13.0534545350462,
123.486123509007)) ;
#97553 = CARTESIAN_POINT('Ctrl Pts',(-18.1988186844713,-13.0551472180647,
123.522065486652)) ;
#97554 = CARTESIAN_POINT('Ctrl Pts',(-18.2026201779857,-13.0568444933791,
123.557865731132)) ;
#97555 = CARTESIAN_POINT('Ctrl Pts',(-18.2079682354,-13.0585351659895,123.593274647265)) ;
#97556 = CARTESIAN_POINT('Ctrl Pts',(-18.2131103582355,-13.0601607368395,
123.627320092578)) ;
#97557 = CARTESIAN_POINT('Ctrl Pts',(-18.2196817476484,-13.0617802036885,
123.661003310782)) ;
#97558 = CARTESIAN_POINT('Ctrl Pts',(-18.2275916180223,-13.063383615616,123.694115341802)) ;
#97559 = CARTESIAN_POINT('Ctrl Pts',(-18.2325978992378,-13.0643984402128,
123.71507246639)) ;
#97560 = CARTESIAN_POINT('Ctrl Pts',(-18.238205882646,-13.0654199755197,123.736062655809)) ;
#97561 = CARTESIAN_POINT('Ctrl Pts',(-18.2443545975886,-13.0664387567713,
123.756824730622)) ;
#97562 = CARTESIAN_POINT('Ctrl Pts',(-18.2492019833702,-13.0672419206518,
123.773192668832)) ;
#97563 = CARTESIAN_POINT('Ctrl Pts',(-18.2543843856651,-13.068043372866,123.789418946586)) ;
#97564 = CARTESIAN_POINT('Ctrl Pts',(-18.2598500881022,-13.0688384759608,
123.805382371146)) ;
#97565 = CARTESIAN_POINT('Ctrl Pts',(-18.2658850525413,-13.0697163903658,
123.823008412931)) ;
#97566 = CARTESIAN_POINT('Ctrl Pts',(-18.2724068028398,-13.0706067410412,
123.840719869312)) ;
#97567 = CARTESIAN_POINT('Ctrl Pts',(-18.2793257757553,-13.0714972686474,
123.858233433094)) ;
#97568 = CARTESIAN_POINT('Ctrl Pts',(-18.283813915918,-13.072074928477,123.869593981829)) ;
#97569 = CARTESIAN_POINT('Ctrl Pts',(-18.2884681744065,-13.0726526627545,
123.880871562284)) ;
#97570 = CARTESIAN_POINT('Ctrl Pts',(-18.2932531655623,-13.0732271253608,
123.89199313578)) ;
#97571 = CARTESIAN_POINT('Ctrl Pts',(-18.3069710130514,-13.0748740229544,
123.923877008516)) ;
#97572 = CARTESIAN_POINT('Ctrl Pts',(-18.3221939451645,-13.0765340989596,
123.955482740778)) ;
#97573 = CARTESIAN_POINT('Ctrl Pts',(-18.3388645214529,-13.0781972778934,
123.986532515534)) ;
#97574 = CARTESIAN_POINT('Ctrl Pts',(-18.3555350977413,-13.0798604568272,
124.01758229029)) ;
#97575 = CARTESIAN_POINT('Ctrl Pts',(-18.3736531056248,-13.0815267386897,
124.048075338036)) ;
#97576 = CARTESIAN_POINT('Ctrl Pts',(-18.3931030451195,-13.083186047998,124.07775508389)) ;
#97577 = CARTESIAN_POINT('Ctrl Pts',(-18.4316216073325,-13.0864721357949,
124.136532703092)) ;
#97578 = CARTESIAN_POINT('Ctrl Pts',(-18.4751527090631,-13.089790362517,124.191835046653)) ;
#97579 = CARTESIAN_POINT('Ctrl Pts',(-18.5231943392562,-13.0931166999359,
124.243047501832)) ;
#97580 = CARTESIAN_POINT('Ctrl Pts',(-18.5660543598903,-13.0960842697257,
124.288736352874)) ;
#97581 = CARTESIAN_POINT('Ctrl Pts',(-18.6124082795638,-13.0990174373958,
124.331061368972)) ;
#97582 = CARTESIAN_POINT('Ctrl Pts',(-18.6617760948158,-13.1019732940616,
124.369591086397)) ;
#97583 = CARTESIAN_POINT('Ctrl Pts',(-18.6680461563274,-13.1023487087527,
124.374484632871)) ;
#97584 = CARTESIAN_POINT('Ctrl Pts',(-18.6743647888655,-13.1027244894354,
124.379317009841)) ;
#97585 = CARTESIAN_POINT('Ctrl Pts',(-18.6807309684182,-13.1031007530736,
124.384087377781)) ;
#97586 = CARTESIAN_POINT('Ctrl Pts',(-18.7273268815062,-13.1058547356843,
124.4190030832)) ;
#97587 = CARTESIAN_POINT('Ctrl Pts',(-18.7764051125978,-13.1086131334079,
124.45054289871)) ;
#97588 = CARTESIAN_POINT('Ctrl Pts',(-18.8275084107538,-13.1113469816988,
124.478416876936)) ;
#97589 = CARTESIAN_POINT('Ctrl Pts',(-18.8386345148919,-13.1119421894815,
124.484485541693)) ;
#97590 = CARTESIAN_POINT('Ctrl Pts',(-18.8498565064832,-13.1125362335942,
124.490380608565)) ;
#97591 = CARTESIAN_POINT('Ctrl Pts',(-18.8611694947514,-13.1131288151207,
124.496099364079)) ;
#97592 = CARTESIAN_POINT('Ctrl Pts',(-18.9136880971347,-13.1158797729433,
124.522647703017)) ;
#97593 = CARTESIAN_POINT('Ctrl Pts',(-18.9681047243549,-13.1186438690749,
124.545359825598)) ;
#97594 = CARTESIAN_POINT('Ctrl Pts',(-19.0239064931186,-13.1214376143307,
124.564023371071)) ;
#97595 = CARTESIAN_POINT('Ctrl Pts',(-19.0349058562285,-13.1219883032997,
124.567702234987)) ;
#97596 = CARTESIAN_POINT('Ctrl Pts',(-19.0459589767591,-13.1225401442647,
124.571223944324)) ;
#97597 = CARTESIAN_POINT('Ctrl Pts',(-19.0570618357224,-13.1230932636784,
124.574587093755)) ;
#97598 = CARTESIAN_POINT('Ctrl Pts',(-19.1167680563634,-13.1260676930447,
124.592672610526)) ;
#97599 = CARTESIAN_POINT('Ctrl Pts',(-19.1778160979921,-13.1290113327516,
124.60613932436)) ;
#97600 = CARTESIAN_POINT('Ctrl Pts',(-19.239581589968,-13.1319272155962,124.614851469523)) ;
#97601 = CARTESIAN_POINT('Ctrl Pts',(-19.2479736764787,-13.1323233970286,
124.616035189972)) ;
#97602 = CARTESIAN_POINT('Ctrl Pts',(-19.2563789907143,-13.1327190660501,
124.617131214563)) ;
#97603 = CARTESIAN_POINT('Ctrl Pts',(-19.2647959493122,-13.1331142302675,
124.618139275079)) ;
#97604 = CARTESIAN_POINT('Ctrl Pts',(-19.334905482715,-13.1364057729999,124.62653597224)) ;
#97605 = CARTESIAN_POINT('Ctrl Pts',(-19.4056483658304,-13.139733462171,124.62880718039)) ;
#97606 = CARTESIAN_POINT('Ctrl Pts',(-19.4761936160471,-13.1431024819908,
124.624915299969)) ;
#97607 = CARTESIAN_POINT('Ctrl Pts',(-19.5129227182888,-13.144856548679,124.622889008002)) ;
#97608 = CARTESIAN_POINT('Ctrl Pts',(-19.5495114434135,-13.1465967018408,
124.619192933056)) ;
#97609 = CARTESIAN_POINT('Ctrl Pts',(-19.5857063219984,-13.1483201646471,
124.613880240191)) ;
#97610 = CARTESIAN_POINT('Ctrl Pts',(-19.6193755894895,-13.1499233674345,
124.608938257121)) ;
#97611 = CARTESIAN_POINT('Ctrl Pts',(-19.6527037127881,-13.1515121278449,
124.602598051184)) ;
#97612 = CARTESIAN_POINT('Ctrl Pts',(-19.6854981284202,-13.1530842107175,
124.594941307633)) ;
#97613 = CARTESIAN_POINT('Ctrl Pts',(-19.7071633185249,-13.1541227861468,
124.589882982872)) ;
#97614 = CARTESIAN_POINT('Ctrl Pts',(-19.7288448306834,-13.1551716918062,
124.584188830054)) ;
#97615 = CARTESIAN_POINT('Ctrl Pts',(-19.7502864737702,-13.1562211252396,
124.577918306514)) ;
#97616 = CARTESIAN_POINT('Ctrl Pts',(-19.7680195723214,-13.1570890487667,
124.572732332125)) ;
#97617 = CARTESIAN_POINT('Ctrl Pts',(-19.7855886529758,-13.1579573332887,
124.567153112527)) ;
#97618 = CARTESIAN_POINT('Ctrl Pts',(-19.8028567953322,-13.1588204336388,
124.561240043737)) ;
#97619 = CARTESIAN_POINT('Ctrl Pts',(-19.8196418206451,-13.1596593867193,
124.555492407004)) ;
#97620 = CARTESIAN_POINT('Ctrl Pts',(-19.8365238609528,-13.1605123080096,
124.549296185975)) ;
#97621 = CARTESIAN_POINT('Ctrl Pts',(-19.8532087528451,-13.1613635178667,
124.542746542583)) ;
#97622 = CARTESIAN_POINT('Ctrl Pts',(-19.8632091884824,-13.1618737081301,
124.53882087812)) ;
#97623 = CARTESIAN_POINT('Ctrl Pts',(-19.8731391003765,-13.1623832835692,
124.534769208951)) ;
#97624 = CARTESIAN_POINT('Ctrl Pts',(-19.8829384261627,-13.1628888680262,
124.530620397938)) ;
#97625 = CARTESIAN_POINT('Ctrl Pts',(-19.913003931288,-13.1644400616915,124.517891348871)) ;
#97626 = CARTESIAN_POINT('Ctrl Pts',(-19.9428522050097,-13.1659985862561,
124.503820459197)) ;
#97627 = CARTESIAN_POINT('Ctrl Pts',(-19.9722380350367,-13.1675616636008,
124.488454517319)) ;
#97628 = CARTESIAN_POINT('Ctrl Pts',(-20.0015005423961,-13.1691181812238,
124.473153061247)) ;
#97629 = CARTESIAN_POINT('Ctrl Pts',(-20.0303038741354,-13.1706792134941,
124.4565675882)) ;
#97630 = CARTESIAN_POINT('Ctrl Pts',(-20.0584230059923,-13.1722420171226,
124.438793148967)) ;
#97631 = CARTESIAN_POINT('Ctrl Pts',(-20.0618399940339,-13.1724319263039,
124.436633229997)) ;
#97632 = CARTESIAN_POINT('Ctrl Pts',(-20.0652469059663,-13.1726218616423,
124.434455811017)) ;
#97633 = CARTESIAN_POINT('Ctrl Pts',(-20.0686433618844,-13.1728118182152,
124.432261109401)) ;
#97634 = CARTESIAN_POINT('Ctrl Pts',(-20.1279765818108,-13.1761301993118,
124.393921523435)) ;
#97635 = CARTESIAN_POINT('Ctrl Pts',(-20.1838434763563,-13.1794637724057,
124.350485479794)) ;
#97636 = CARTESIAN_POINT('Ctrl Pts',(-20.2356065856208,-13.1827969618018,
124.302458798815)) ;
#97637 = CARTESIAN_POINT('Ctrl Pts',(-20.2826796101207,-13.18582814189,124.258783657145)) ;
#97638 = CARTESIAN_POINT('Ctrl Pts',(-20.3262323299467,-13.188853915509,124.211424181396)) ;
#97639 = CARTESIAN_POINT('Ctrl Pts',(-20.3658051465989,-13.19187761842,124.160890207514)) ;
#97640 = CARTESIAN_POINT('Ctrl Pts',(-20.3697154679666,-13.1921764005412,
124.155896777817)) ;
#97641 = CARTESIAN_POINT('Ctrl Pts',(-20.3735869608074,-13.1924751624439,
124.150872379739)) ;
#97642 = CARTESIAN_POINT('Ctrl Pts',(-20.3774192020029,-13.1927739073464,
124.14581752391)) ;
#97643 = CARTESIAN_POINT('Ctrl Pts',(-20.4127161983117,-13.1955255080899,
124.09925959124)) ;
#97644 = CARTESIAN_POINT('Ctrl Pts',(-20.4446279969202,-13.198267332075,124.050183676268)) ;
#97645 = CARTESIAN_POINT('Ctrl Pts',(-20.4728597724474,-13.2010292632912,
123.999049053477)) ;
#97646 = CARTESIAN_POINT('Ctrl Pts',(-20.4788469006977,-13.2016149875717,
123.98820490574)) ;
#97647 = CARTESIAN_POINT('Ctrl Pts',(-20.4846686819584,-13.2022016161533,
123.977268268734)) ;
#97648 = CARTESIAN_POINT('Ctrl Pts',(-20.4903225596479,-13.2027894340587,
123.96624368281)) ;
#97649 = CARTESIAN_POINT('Ctrl Pts',(-20.5166408261384,-13.2055256708739,
123.914925276888)) ;
#97650 = CARTESIAN_POINT('Ctrl Pts',(-20.5392851334898,-13.208260517437,123.861761919089)) ;
#97651 = CARTESIAN_POINT('Ctrl Pts',(-20.5580507717644,-13.2109629922143,
123.807242058036)) ;
#97652 = CARTESIAN_POINT('Ctrl Pts',(-20.5623545638074,-13.2115827893815,
123.794738239048)) ;
#97653 = CARTESIAN_POINT('Ctrl Pts',(-20.5664545430273,-13.2122008838315,
123.782163150813)) ;
#97654 = CARTESIAN_POINT('Ctrl Pts',(-20.5703485986545,-13.2128169018266,
123.769522829615)) ;
#97655 = CARTESIAN_POINT('Ctrl Pts',(-20.5890821117237,-13.2157804396565,
123.70871280402)) ;
#97656 = CARTESIAN_POINT('Ctrl Pts',(-20.6030195691534,-13.2187668771431,
123.646477351041)) ;
#97657 = CARTESIAN_POINT('Ctrl Pts',(-20.612010912125,-13.2218051835997,123.583470848285)) ;
#97658 = CARTESIAN_POINT('Ctrl Pts',(-20.6129451788092,-13.2221208859934,
123.576924009109)) ;
#97659 = CARTESIAN_POINT('Ctrl Pts',(-20.6138260884446,-13.2224371484029,
123.57036885689)) ;
#97660 = CARTESIAN_POINT('Ctrl Pts',(-20.6146535038414,-13.2227540033275,
123.563806134672)) ;
#97661 = CARTESIAN_POINT('Ctrl Pts',(-20.6235260013047,-13.2261516854667,
123.493433095389)) ;
#97662 = CARTESIAN_POINT('Ctrl Pts',(-20.6262189115083,-13.2294902857806,
123.422396280088)) ;
#97663 = CARTESIAN_POINT('Ctrl Pts',(-20.622699528908,-13.2327808911029,123.351552658982)) ;
#97664 = CARTESIAN_POINT('Ctrl Pts',(-20.6208323619883,-13.2345266829367,
123.313967411561)) ;
#97665 = CARTESIAN_POINT('Ctrl Pts',(-20.6172167302929,-13.2362874613737,
123.276512223843)) ;
#97666 = CARTESIAN_POINT('Ctrl Pts',(-20.6119035134746,-13.2380562906017,
123.239445545867)) ;
#97667 = CARTESIAN_POINT('Ctrl Pts',(-20.6072736820335,-13.2395976132042,
123.207146380035)) ;
#97668 = CARTESIAN_POINT('Ctrl Pts',(-20.6013557629974,-13.2411450487989,
123.175142388246)) ;
#97669 = CARTESIAN_POINT('Ctrl Pts',(-20.5942145044862,-13.2426940083626,
123.143595771839)) ;
#97670 = CARTESIAN_POINT('Ctrl Pts',(-20.5892178400552,-13.2437777992861,
123.121522931895)) ;
#97671 = CARTESIAN_POINT('Ctrl Pts',(-20.5835709204747,-13.2448654054133,
123.099461510239)) ;
#97672 = CARTESIAN_POINT('Ctrl Pts',(-20.5773352917912,-13.2459424605924,
123.077665243905)) ;
#97673 = CARTESIAN_POINT('Ctrl Pts',(-20.5715973932994,-13.2469335448281,
123.057608763625)) ;
#97674 = CARTESIAN_POINT('Ctrl Pts',(-20.5653617058162,-13.2479156952537,
123.037776953081)) ;
#97675 = CARTESIAN_POINT('Ctrl Pts',(-20.5587133983318,-13.2488777185652,
123.018355650104)) ;
#97676 = CARTESIAN_POINT('Origin',(-19.4092696390481,30.19753203383,123.411833654989)) ;
#97677 = CARTESIAN_POINT('',(-20.5587133983317,-12.510900730771,123.018355650104)) ;
#97678 = CARTESIAN_POINT('',(-20.5587133983317,-12.5288903030032,123.018355650104)) ;
#97679 = CARTESIAN_POINT('',(-20.5587133983318,30.19753203383,123.018355650104)) ;
#97680 = CARTESIAN_POINT('Ctrl Pts',(-20.5587133983318,-12.870840300276,123.018355650104)) ;
#97681 = CARTESIAN_POINT('Ctrl Pts',(-20.564131347186,-12.8700544476548,123.03418278001)) ;
#97682 = CARTESIAN_POINT('Ctrl Pts',(-20.5692731213384,-12.8692618062304,
123.050283437968)) ;
#97683 = CARTESIAN_POINT('Ctrl Pts',(-20.5740378170817,-12.8684744374755,
123.066347059699)) ;
#97684 = CARTESIAN_POINT('Ctrl Pts',(-20.5760823053151,-12.8681365846006,
123.073239815791)) ;
#97685 = CARTESIAN_POINT('Ctrl Pts',(-20.5780579919871,-12.867799702525,123.080125549278)) ;
#97686 = CARTESIAN_POINT('Ctrl Pts',(-20.5799597328274,-12.8674647441515,
123.086978917588)) ;
#97687 = CARTESIAN_POINT('Ctrl Pts',(-20.5884193069586,-12.865974738189,123.117464973332)) ;
#97688 = CARTESIAN_POINT('Ctrl Pts',(-20.5957772602773,-12.8644630347073,
123.148618908581)) ;
#97689 = CARTESIAN_POINT('Ctrl Pts',(-20.601914631413,-12.8629422477991,123.180222303212)) ;
#97690 = CARTESIAN_POINT('Ctrl Pts',(-20.6080212760854,-12.8614290746398,
123.211667476917)) ;
#97691 = CARTESIAN_POINT('Ctrl Pts',(-20.6129192955571,-12.8599069087778,
123.243557042946)) ;
#97692 = CARTESIAN_POINT('Ctrl Pts',(-20.6165402120496,-12.858388175797,123.275658548418)) ;
#97693 = CARTESIAN_POINT('Ctrl Pts',(-20.6172240713776,-12.8581013424172,
123.281721354342)) ;
#97694 = CARTESIAN_POINT('Ctrl Pts',(-20.6178625225035,-12.8578146314863,
123.287791685004)) ;
#97695 = CARTESIAN_POINT('Ctrl Pts',(-20.6184553089328,-12.8575281267115,
123.293867931873)) ;
#97696 = CARTESIAN_POINT('Ctrl Pts',(-20.625308056386,-12.8542160656237,123.364110743096)) ;
#97697 = CARTESIAN_POINT('Ctrl Pts',(-20.6260247358445,-12.8509002845194,
123.434794086066)) ;
#97698 = CARTESIAN_POINT('Ctrl Pts',(-20.6206096506246,-12.8475541933109,
123.505114266259)) ;
#97699 = CARTESIAN_POINT('Ctrl Pts',(-20.615684190146,-12.8445106511807,123.569076190093)) ;
#97700 = CARTESIAN_POINT('Ctrl Pts',(-20.6056936470832,-12.8414987770609,
123.632579414616)) ;
#97701 = CARTESIAN_POINT('Ctrl Pts',(-20.5907484396515,-12.8384804507048,
123.694948013173)) ;
#97702 = CARTESIAN_POINT('Ctrl Pts',(-20.5891615151249,-12.838159956249,123.701570487916)) ;
#97703 = CARTESIAN_POINT('Ctrl Pts',(-20.5875187754993,-12.8378393890454,
123.708180177836)) ;
#97704 = CARTESIAN_POINT('Ctrl Pts',(-20.5858203871939,-12.8375187034571,
123.714776278472)) ;
#97705 = CARTESIAN_POINT('Ctrl Pts',(-20.5710304288031,-12.8347260991438,
123.772216649225)) ;
#97706 = CARTESIAN_POINT('Ctrl Pts',(-20.5520413961415,-12.8319149846305,
123.828527968095)) ;
#97707 = CARTESIAN_POINT('Ctrl Pts',(-20.5290384866588,-12.8291247582725,
123.883176018888)) ;
#97708 = CARTESIAN_POINT('Ctrl Pts',(-20.5246751108182,-12.8285954858216,
123.89354209822)) ;
#97709 = CARTESIAN_POINT('Ctrl Pts',(-20.5201674509584,-12.8280669649586,
123.90384838225)) ;
#97710 = CARTESIAN_POINT('Ctrl Pts',(-20.5155169701899,-12.8275394645878,
123.914091296471)) ;
#97711 = CARTESIAN_POINT('Ctrl Pts',(-20.4911675717112,-12.824777531496,123.967722052596)) ;
#97712 = CARTESIAN_POINT('Ctrl Pts',(-20.4629293195428,-12.8220158289772,
124.019547058866)) ;
#97713 = CARTESIAN_POINT('Ctrl Pts',(-20.4310695730123,-12.8192219391127,
124.069078503608)) ;
#97714 = CARTESIAN_POINT('Ctrl Pts',(-20.4249397087669,-12.8186843904047,
124.078608429775)) ;
#97715 = CARTESIAN_POINT('Ctrl Pts',(-20.418675918171,-12.8181456501741,124.088053526982)) ;
#97716 = CARTESIAN_POINT('Ctrl Pts',(-20.4122802995279,-12.8176054875281,
124.097410427531)) ;
#97717 = CARTESIAN_POINT('Ctrl Pts',(-20.377524398935,-12.8146700655968,124.148258910452)) ;
#97718 = CARTESIAN_POINT('Ctrl Pts',(-20.3389277635664,-12.8117625018628,
124.196418759589)) ;
#97719 = CARTESIAN_POINT('Ctrl Pts',(-20.2968796424746,-12.8088828516116,
124.241408472533)) ;
#97720 = CARTESIAN_POINT('Ctrl Pts',(-20.2905194059579,-12.8084472731314,
124.248213656872)) ;
#97721 = CARTESIAN_POINT('Ctrl Pts',(-20.284080275214,-12.8080123333077,124.254946370142)) ;
#97722 = CARTESIAN_POINT('Ctrl Pts',(-20.2775636789539,-12.8075780323319,
124.261605010325)) ;
#97723 = CARTESIAN_POINT('Ctrl Pts',(-20.228210311426,-12.8042888588397,124.312034145886)) ;
#97724 = CARTESIAN_POINT('Ctrl Pts',(-20.1745274478076,-12.8009600868674,
124.358095285596)) ;
#97725 = CARTESIAN_POINT('Ctrl Pts',(-20.1171473202792,-12.7975966410503,
124.399231793786)) ;
#97726 = CARTESIAN_POINT('Ctrl Pts',(-20.0848738198182,-12.7957048681525,
124.422369057038)) ;
#97727 = CARTESIAN_POINT('Ctrl Pts',(-20.0515069956519,-12.7938301259444,
124.443889257671)) ;
#97728 = CARTESIAN_POINT('Ctrl Pts',(-20.017293716012,-12.7919703264446,124.463666635038)) ;
#97729 = CARTESIAN_POINT('Ctrl Pts',(-19.9903760328249,-12.7905071082365,
124.479226709483)) ;
#97730 = CARTESIAN_POINT('Ctrl Pts',(-19.9629350601289,-12.7890531394645,
124.493708837511)) ;
#97731 = CARTESIAN_POINT('Ctrl Pts',(-19.9350995258085,-12.7876074032817,
124.507072818951)) ;
#97732 = CARTESIAN_POINT('Ctrl Pts',(-19.913035641509,-12.7864614380023,124.517665801894)) ;
#97733 = CARTESIAN_POINT('Ctrl Pts',(-19.8905487205702,-12.7853054287652,
124.527636628228)) ;
#97734 = CARTESIAN_POINT('Ctrl Pts',(-19.8678671660526,-12.7841509014001,
124.536882189191)) ;
#97735 = CARTESIAN_POINT('Ctrl Pts',(-19.8461963974136,-12.7830478246512,
124.545715728905)) ;
#97736 = CARTESIAN_POINT('Ctrl Pts',(-19.824348499549,-12.7819461006402,124.553887424883)) ;
#97737 = CARTESIAN_POINT('Ctrl Pts',(-19.8025379523346,-12.7808557819277,
124.56134917461)) ;
#97738 = CARTESIAN_POINT('Ctrl Pts',(-19.7884497934317,-12.7801515087554,
124.566168967292)) ;
#97739 = CARTESIAN_POINT('Ctrl Pts',(-19.7740409591828,-12.7794353947332,
124.570804577597)) ;
#97740 = CARTESIAN_POINT('Ctrl Pts',(-19.7596521729602,-12.7787251458483,
124.575138419879)) ;
#97741 = CARTESIAN_POINT('Ctrl Pts',(-19.7533117073152,-12.7784121723573,
124.577048141635)) ;
#97742 = CARTESIAN_POINT('Ctrl Pts',(-19.74697535317,-12.7781003377311,124.578899915679)) ;
#97743 = CARTESIAN_POINT('Ctrl Pts',(-19.7406731878155,-12.7777911569645,
124.580686761222)) ;
#97744 = CARTESIAN_POINT('Ctrl Pts',(-19.7107655597112,-12.7763239051763,
124.589166435901)) ;
#97745 = CARTESIAN_POINT('Ctrl Pts',(-19.6801868425886,-12.7748458991295,
124.596591804714)) ;
#97746 = CARTESIAN_POINT('Ctrl Pts',(-19.6491539460698,-12.773356568108,124.602842225626)) ;
#97747 = CARTESIAN_POINT('Ctrl Pts',(-19.6182872600569,-12.7718752138624,
124.609059169623)) ;
#97748 = CARTESIAN_POINT('Ctrl Pts',(-19.5869718168498,-12.7703826556291,
124.614113481114)) ;
#97749 = CARTESIAN_POINT('Ctrl Pts',(-19.5554385968128,-12.7688783318133,
124.617935032101)) ;
#97750 = CARTESIAN_POINT('Ctrl Pts',(-19.5486024681402,-12.7685522074544,
124.618763511218)) ;
#97751 = CARTESIAN_POINT('Ctrl Pts',(-19.5417561512828,-12.7682255301309,
124.619534241395)) ;
#97752 = CARTESIAN_POINT('Ctrl Pts',(-19.5349020671652,-12.767898294121,124.620246824849)) ;
#97753 = CARTESIAN_POINT('Ctrl Pts',(-19.4643349076577,-12.7645291910702,
124.627583325158)) ;
#97754 = CARTESIAN_POINT('Ctrl Pts',(-19.3932654909685,-12.7611694127812,
124.628723974149)) ;
#97755 = CARTESIAN_POINT('Ctrl Pts',(-19.3225080055547,-12.7578667843255,
124.623658029657)) ;
#97756 = CARTESIAN_POINT('Ctrl Pts',(-19.2524440060968,-12.7545965245506,
124.618641735903)) ;
#97757 = CARTESIAN_POINT('Ctrl Pts',(-19.1829222635137,-12.7512924797053,
124.607551627984)) ;
#97758 = CARTESIAN_POINT('Ctrl Pts',(-19.1148106902483,-12.7479375921959,
124.590536256818)) ;
#97759 = CARTESIAN_POINT('Ctrl Pts',(-19.0583882398865,-12.7451584613537,
124.57644101736)) ;
#97760 = CARTESIAN_POINT('Ctrl Pts',(-19.0030139762503,-12.7424180770252,
124.558299071169)) ;
#97761 = CARTESIAN_POINT('Ctrl Pts',(-18.9492001726806,-12.7396961292572,
124.536281066922)) ;
#97762 = CARTESIAN_POINT('Ctrl Pts',(-18.9374084921155,-12.7390996960659,
124.531456481861)) ;
#97763 = CARTESIAN_POINT('Ctrl Pts',(-18.9256916702083,-12.7385041480798,
124.526445981017)) ;
#97764 = CARTESIAN_POINT('Ctrl Pts',(-18.9140549873802,-12.7379092716233,
124.521251675782)) ;
#97765 = CARTESIAN_POINT('Ctrl Pts',(-18.8609346076704,-12.7351937156767,
124.497540153306)) ;
#97766 = CARTESIAN_POINT('Ctrl Pts',(-18.8095515023045,-12.732452168523,124.470023976683)) ;
#97767 = CARTESIAN_POINT('Ctrl Pts',(-18.7603808349887,-12.7296938003854,
124.438960334641)) ;
#97768 = CARTESIAN_POINT('Ctrl Pts',(-18.74982659843,-12.729101730531,124.432292680033)) ;
#97769 = CARTESIAN_POINT('Ctrl Pts',(-18.7393742020045,-12.7285088856924,
124.425461751911)) ;
#97770 = CARTESIAN_POINT('Ctrl Pts',(-18.7290281930024,-12.7279153565559,
124.418470367596)) ;
#97771 = CARTESIAN_POINT('Ctrl Pts',(-18.6786081150779,-12.725022860976,124.384398664977)) ;
#97772 = CARTESIAN_POINT('Ctrl Pts',(-18.6307895240425,-12.7221506683599,
124.346561738427)) ;
#97773 = CARTESIAN_POINT('Ctrl Pts',(-18.5860427072605,-12.719299388302,124.305334250884)) ;
#97774 = CARTESIAN_POINT('Ctrl Pts',(-18.5788824411168,-12.7188431340803,
124.298737138409)) ;
#97775 = CARTESIAN_POINT('Ctrl Pts',(-18.571800761787,-12.7183874153361,124.292053293323)) ;
#97776 = CARTESIAN_POINT('Ctrl Pts',(-18.5647995198402,-12.717932234567,124.285284348417)) ;
#97777 = CARTESIAN_POINT('Ctrl Pts',(-18.514320403513,-12.7146503706968,124.23648009913)) ;
#97778 = CARTESIAN_POINT('Ctrl Pts',(-18.4681382862254,-12.7113409674474,
124.183361047885)) ;
#97779 = CARTESIAN_POINT('Ctrl Pts',(-18.4268046286191,-12.7079998035975,
124.1265422665)) ;
#97780 = CARTESIAN_POINT('Ctrl Pts',(-18.4024700563435,-12.7060327433881,
124.093091059366)) ;
#97781 = CARTESIAN_POINT('Ctrl Pts',(-18.3798823636766,-12.7040831719724,
124.05844254212)) ;
#97782 = CARTESIAN_POINT('Ctrl Pts',(-18.3591746639711,-12.7021457426413,
124.022854472477)) ;
#97783 = CARTESIAN_POINT('Ctrl Pts',(-18.3443843149212,-12.7007619454801,
123.997435909357)) ;
#97784 = CARTESIAN_POINT('Ctrl Pts',(-18.3305521009411,-12.6993843425355,
123.97153864566)) ;
#97785 = CARTESIAN_POINT('Ctrl Pts',(-18.3177114250398,-12.6980109856402,
123.945262714487)) ;
#97786 = CARTESIAN_POINT('Ctrl Pts',(-18.3065669838062,-12.6968190471993,
123.922457795721)) ;
#97787 = CARTESIAN_POINT('Ctrl Pts',(-18.2961005346161,-12.695618357183,123.899218416616)) ;
#97788 = CARTESIAN_POINT('Ctrl Pts',(-18.2864138586514,-12.6944212672785,
123.87577416035)) ;
#97789 = CARTESIAN_POINT('Ctrl Pts',(-18.2767271826868,-12.6932241773741,
123.852329904085)) ;
#97790 = CARTESIAN_POINT('Ctrl Pts',(-18.2678204007533,-12.6920306875816,
123.828681297026)) ;
#97791 = CARTESIAN_POINT('Ctrl Pts',(-18.259745197628,-12.6908531495886,123.805075889067)) ;
#97792 = CARTESIAN_POINT('Ctrl Pts',(-18.2552593151472,-12.6901990116096,
123.791962771742)) ;
#97793 = CARTESIAN_POINT('Ctrl Pts',(-18.2509209660898,-12.6895333106017,
123.778534845474)) ;
#97794 = CARTESIAN_POINT('Ctrl Pts',(-18.2468545478701,-12.6888739164767,
123.765156527001)) ;
#97795 = CARTESIAN_POINT('Ctrl Pts',(-18.2453071343995,-12.6886229940933,
123.760065611827)) ;
#97796 = CARTESIAN_POINT('Ctrl Pts',(-18.2437985845914,-12.6883729849888,
123.754982050513)) ;
#97797 = CARTESIAN_POINT('Ctrl Pts',(-18.242333854468,-12.6881248738665,123.749926498379)) ;
#97798 = CARTESIAN_POINT('Ctrl Pts',(-18.2337910747404,-12.68667780957,123.720440883529)) ;
#97799 = CARTESIAN_POINT('Ctrl Pts',(-18.2262665255178,-12.6852153862968,
123.690273420263)) ;
#97800 = CARTESIAN_POINT('Ctrl Pts',(-18.2198840166692,-12.6837414307203,
123.659639501093)) ;
#97801 = CARTESIAN_POINT('Ctrl Pts',(-18.2135385245717,-12.6822760236703,
123.629183250015)) ;
#97802 = CARTESIAN_POINT('Ctrl Pts',(-18.2083221076355,-12.6807992176973,
123.598266500514)) ;
#97803 = CARTESIAN_POINT('Ctrl Pts',(-18.2043080726945,-12.6793147732788,
123.567118939855)) ;
#97804 = CARTESIAN_POINT('Ctrl Pts',(-18.2033130940989,-12.6789468167352,
123.559398240704)) ;
#97805 = CARTESIAN_POINT('Ctrl Pts',(-18.2023917498007,-12.6785783908704,
123.551663423602)) ;
#97806 = CARTESIAN_POINT('Ctrl Pts',(-18.2015446716631,-12.6782095529563,
123.543918094799)) ;
#97807 = CARTESIAN_POINT('Ctrl Pts',(-18.1938583064652,-12.6748627272252,
123.473637180778)) ;
#97808 = CARTESIAN_POINT('Ctrl Pts',(-18.1923230480661,-12.6715220564939,
123.40284100622)) ;
#97809 = CARTESIAN_POINT('Ctrl Pts',(-18.1969478260541,-12.6682155379078,
123.332324423928)) ;
#97810 = CARTESIAN_POINT('Ctrl Pts',(-18.2012690204717,-12.6651260685984,
123.266436750501)) ;
#97811 = CARTESIAN_POINT('Ctrl Pts',(-18.2109601523505,-12.6620310002457,
123.200988306394)) ;
#97812 = CARTESIAN_POINT('Ctrl Pts',(-18.2259053563382,-12.6588878040942,
123.136706647061)) ;
#97813 = CARTESIAN_POINT('Ctrl Pts',(-18.226906023296,-12.6586773491193,123.132402622001)) ;
#97814 = CARTESIAN_POINT('Ctrl Pts',(-18.2279302255568,-12.6584666783841,
123.128103824411)) ;
#97815 = CARTESIAN_POINT('Ctrl Pts',(-18.2289779200788,-12.6582557791229,
123.123810471517)) ;
#97816 = CARTESIAN_POINT('Ctrl Pts',(-18.2428415843462,-12.6554650452882,
123.066998488773)) ;
#97817 = CARTESIAN_POINT('Ctrl Pts',(-18.260802124165,-12.6526971472817,123.011226189608)) ;
#97818 = CARTESIAN_POINT('Ctrl Pts',(-18.2826888624215,-12.6499642441051,
122.957013196104)) ;
#97819 = CARTESIAN_POINT('Ctrl Pts',(-18.2873385993681,-12.6493836513862,
122.945495894809)) ;
#97820 = CARTESIAN_POINT('Ctrl Pts',(-18.2921653605667,-12.6488046380907,
122.934048909311)) ;
#97821 = CARTESIAN_POINT('Ctrl Pts',(-18.2971672226535,-12.6482273208029,
122.922677124281)) ;
#97822 = CARTESIAN_POINT('Ctrl Pts',(-18.3208525736772,-12.6454935463849,
122.868828234503)) ;
#97823 = CARTESIAN_POINT('Ctrl Pts',(-18.3484380413906,-12.6427273694512,
122.816735382859)) ;
#97824 = CARTESIAN_POINT('Ctrl Pts',(-18.3796624863801,-12.6399265123793,
122.76688791521)) ;
#97825 = CARTESIAN_POINT('Ctrl Pts',(-18.3857548490442,-12.6393800226961,
122.757161918449)) ;
#97826 = CARTESIAN_POINT('Ctrl Pts',(-18.3919856074846,-12.6388322127425,
122.747521327664)) ;
#97827 = CARTESIAN_POINT('Ctrl Pts',(-18.3983526181023,-12.6382830656004,
122.737969668085)) ;
#97828 = CARTESIAN_POINT('Ctrl Pts',(-18.4321759300713,-12.6353658449108,
122.687228624731)) ;
#97829 = CARTESIAN_POINT('Ctrl Pts',(-18.4697955271774,-12.6324929751343,
122.639077908616)) ;
#97830 = CARTESIAN_POINT('Ctrl Pts',(-18.5108371563559,-12.629644765804,122.593992001533)) ;
#97831 = CARTESIAN_POINT('Ctrl Pts',(-18.5175176505436,-12.6291811524861,
122.586653205626)) ;
#97832 = CARTESIAN_POINT('Ctrl Pts',(-18.5242887247866,-12.6287181925529,
122.579395542829)) ;
#97833 = CARTESIAN_POINT('Ctrl Pts',(-18.531148661798,-12.6282558010846,122.572220979169)) ;
#97834 = CARTESIAN_POINT('Ctrl Pts',(-18.5798691064298,-12.6249718178806,
122.521266002328)) ;
#97835 = CARTESIAN_POINT('Ctrl Pts',(-18.6329650099344,-12.6216433959297,
122.474618633894)) ;
#97836 = CARTESIAN_POINT('Ctrl Pts',(-18.6898007287457,-12.6182833583503,
122.43284929189)) ;
#97837 = CARTESIAN_POINT('Ctrl Pts',(-18.7241719282777,-12.6162513875317,
122.407589430338)) ;
#97838 = CARTESIAN_POINT('Ctrl Pts',(-18.759829316988,-12.614235820897,122.384177429425)) ;
#97839 = CARTESIAN_POINT('Ctrl Pts',(-18.7965064276864,-12.612237690103,122.362754466898)) ;
#97840 = CARTESIAN_POINT('Ctrl Pts',(-18.8205874689939,-12.6109257800514,
122.348688821166)) ;
#97841 = CARTESIAN_POINT('Ctrl Pts',(-18.8451075374113,-12.6096213862839,
122.335479687399)) ;
#97842 = CARTESIAN_POINT('Ctrl Pts',(-18.8699865330137,-12.6083248007956,
122.323155728497)) ;
#97843 = CARTESIAN_POINT('Ctrl Pts',(-18.8937408055685,-12.6070868310008,
122.311388907867)) ;
#97844 = CARTESIAN_POINT('Ctrl Pts',(-18.9179531479374,-12.6058411342532,
122.300368835537)) ;
#97845 = CARTESIAN_POINT('Ctrl Pts',(-18.942379754122,-12.6045965813391,122.290201036242)) ;
#97846 = CARTESIAN_POINT('Ctrl Pts',(-18.9668063603067,-12.603352028425,122.280033236946)) ;
#97847 = CARTESIAN_POINT('Ctrl Pts',(-18.9914466315666,-12.6021086193443,
122.270717837563)) ;
#97848 = CARTESIAN_POINT('Ctrl Pts',(-19.0160375804665,-12.6008752248834,
122.262305732671)) ;
#97849 = CARTESIAN_POINT('Ctrl Pts',(-19.0279711155679,-12.6002766812423,
122.258223492925)) ;
#97850 = CARTESIAN_POINT('Ctrl Pts',(-19.0402106989141,-12.599665093615,122.254248724039)) ;
#97851 = CARTESIAN_POINT('Ctrl Pts',(-19.0523573718177,-12.5990611136393,
122.250515641013)) ;
#97852 = CARTESIAN_POINT('Ctrl Pts',(-19.0559238033494,-12.5988837767466,
122.249419556092)) ;
#97853 = CARTESIAN_POINT('Ctrl Pts',(-19.0594821184921,-12.5987070957026,
122.248343979565)) ;
#97854 = CARTESIAN_POINT('Ctrl Pts',(-19.0630219692901,-12.5985315932456,
122.247291492905)) ;
#97855 = CARTESIAN_POINT('Ctrl Pts',(-19.0919445235585,-12.5970976403397,
122.2386920902)) ;
#97856 = CARTESIAN_POINT('Ctrl Pts',(-19.1215582408283,-12.5956536956958,
122.231064351425)) ;
#97857 = CARTESIAN_POINT('Ctrl Pts',(-19.1516492835637,-12.5942025436577,
122.224535188501)) ;
#97858 = CARTESIAN_POINT('Ctrl Pts',(-19.1815504472288,-12.5927605486102,
122.218047225592)) ;
#97859 = CARTESIAN_POINT('Ctrl Pts',(-19.2119223782702,-12.591311436841,122.212644267252)) ;
#97860 = CARTESIAN_POINT('Ctrl Pts',(-19.2425367876188,-12.5898579403164,
122.208402704607)) ;
#97861 = CARTESIAN_POINT('Ctrl Pts',(-19.2513254391689,-12.5894406768527,
122.207185055241)) ;
#97862 = CARTESIAN_POINT('Ctrl Pts',(-19.2601339864558,-12.5890230520307,
122.206062802624)) ;
#97863 = CARTESIAN_POINT('Ctrl Pts',(-19.2689568481623,-12.5886051304848,
122.205036979157)) ;
#97864 = CARTESIAN_POINT('Ctrl Pts',(-19.3394420252231,-12.5852663867599,
122.196841752814)) ;
#97865 = CARTESIAN_POINT('Ctrl Pts',(-19.410490096359,-12.5819070867189,122.1948389208)) ;
#97866 = CARTESIAN_POINT('Ctrl Pts',(-19.4813003313193,-12.5785748167538,
122.199044524326)) ;
#97867 = CARTESIAN_POINT('Ctrl Pts',(-19.5229287891854,-12.576615816619,122.201516946417)) ;
#97868 = CARTESIAN_POINT('Ctrl Pts',(-19.5643931281479,-12.5746631140264,
122.206134835923)) ;
#97869 = CARTESIAN_POINT('Ctrl Pts',(-19.6054057130924,-12.5727088655748,
122.212843856641)) ;
#97870 = CARTESIAN_POINT('Ctrl Pts',(-19.6338055212484,-12.5713556155616,
122.217489623338)) ;
#97871 = CARTESIAN_POINT('Ctrl Pts',(-19.6619888212105,-12.5700016242955,
122.223137005476)) ;
#97872 = CARTESIAN_POINT('Ctrl Pts',(-19.6898640931495,-12.5686442874272,
122.22975385717)) ;
#97873 = CARTESIAN_POINT('Ctrl Pts',(-19.7313957563595,-12.5666219768359,
122.239612374664)) ;
#97874 = CARTESIAN_POINT('Ctrl Pts',(-19.7725387901329,-12.5645976075795,
122.251695198859)) ;
#97875 = CARTESIAN_POINT('Ctrl Pts',(-19.8129943705516,-12.5625726742712,
122.265948740499)) ;
#97876 = CARTESIAN_POINT('Ctrl Pts',(-19.8534157131153,-12.5605494546788,
122.280190219261)) ;
#97877 = CARTESIAN_POINT('Ctrl Pts',(-19.8931501354318,-12.5585256719889,
122.296598589212)) ;
#97878 = CARTESIAN_POINT('Ctrl Pts',(-19.9319122235072,-12.5565028170232,
122.315069949812)) ;
#97879 = CARTESIAN_POINT('Ctrl Pts',(-19.9706765800063,-12.5544798436766,
122.333542391387)) ;
#97880 = CARTESIAN_POINT('Ctrl Pts',(-20.0084678974379,-12.5524577981627,
122.354077794308)) ;
#97881 = CARTESIAN_POINT('Ctrl Pts',(-20.0450225553403,-12.5504381715652,
122.376524944743)) ;
#97882 = CARTESIAN_POINT('Ctrl Pts',(-20.0559527979467,-12.5498342811186,
122.383236888287)) ;
#97883 = CARTESIAN_POINT('Ctrl Pts',(-20.0667726545608,-12.5492306069413,
122.390119451859)) ;
#97884 = CARTESIAN_POINT('Ctrl Pts',(-20.077475574039,-12.5486271888959,122.397167835851)) ;
#97885 = CARTESIAN_POINT('Ctrl Pts',(-20.1186055699818,-12.5463083279707,
122.424253903871)) ;
#97886 = CARTESIAN_POINT('Ctrl Pts',(-20.1581358544575,-12.543969043762,122.453877091541)) ;
#97887 = CARTESIAN_POINT('Ctrl Pts',(-20.1957506463839,-12.5416357742674,
122.485824194355)) ;
#97888 = CARTESIAN_POINT('Ctrl Pts',(-20.2118808139423,-12.5406352097028,
122.499523914464)) ;
#97889 = CARTESIAN_POINT('Ctrl Pts',(-20.2276590811139,-12.5396357511899,
122.513650425928)) ;
#97890 = CARTESIAN_POINT('Ctrl Pts',(-20.243062215745,-12.5386394835516,122.528184496595)) ;
#97891 = CARTESIAN_POINT('Ctrl Pts',(-20.2944479462159,-12.5353158782233,
122.576670980408)) ;
#97892 = CARTESIAN_POINT('Ctrl Pts',(-20.3415329737153,-12.532009642944,122.629576036724)) ;
#97893 = CARTESIAN_POINT('Ctrl Pts',(-20.3837451342896,-12.5286466831811,
122.6862694571)) ;
#97894 = CARTESIAN_POINT('Ctrl Pts',(-20.4101767352934,-12.5265409295443,
122.72176865559)) ;
#97895 = CARTESIAN_POINT('Ctrl Pts',(-20.4346273329003,-12.5244450180581,
122.758664042742)) ;
#97896 = CARTESIAN_POINT('Ctrl Pts',(-20.4569465104085,-12.5223708167657,
122.796675895304)) ;
#97897 = CARTESIAN_POINT('Ctrl Pts',(-20.4704293348034,-12.5211178094909,
122.81963853059)) ;
#97898 = CARTESIAN_POINT('Ctrl Pts',(-20.4831352348093,-12.5198727248409,
122.843008095819)) ;
#97899 = CARTESIAN_POINT('Ctrl Pts',(-20.4950395648443,-12.5186381791135,
122.866719387774)) ;
#97900 = CARTESIAN_POINT('Ctrl Pts',(-20.5064343332851,-12.5174564777787,
122.889415724356)) ;
#97901 = CARTESIAN_POINT('Ctrl Pts',(-20.5171391704667,-12.516268216922,122.912522290061)) ;
#97902 = CARTESIAN_POINT('Ctrl Pts',(-20.5270577879578,-12.5150802068191,
122.935813119464)) ;
#97903 = CARTESIAN_POINT('Ctrl Pts',(-20.5370427795746,-12.5138842467038,
122.959259808132)) ;
#97904 = CARTESIAN_POINT('Ctrl Pts',(-20.5462308378015,-12.5126885407095,
122.982892725681)) ;
#97905 = CARTESIAN_POINT('Ctrl Pts',(-20.5545735719567,-12.5115000367491,
123.006463703773)) ;
#97906 = CARTESIAN_POINT('Ctrl Pts',(-20.5559773620207,-12.5113000531442,
123.010429874123)) ;
#97907 = CARTESIAN_POINT('Ctrl Pts',(-20.5573573342059,-12.5111002734513,
123.014394261087)) ;
#97908 = CARTESIAN_POINT('Ctrl Pts',(-20.5587133983318,-12.510900730771,123.018355650104)) ;
#97909 = CARTESIAN_POINT('Ctrl Pts',(-20.5587133983318,-12.5288903030032,
123.018355650104)) ;
#97910 = CARTESIAN_POINT('Ctrl Pts',(-20.5512973233617,-12.5299743464015,
122.996691513896)) ;
#97911 = CARTESIAN_POINT('Ctrl Pts',(-20.5431621002651,-12.5310699985716,
122.974938614825)) ;
#97912 = CARTESIAN_POINT('Ctrl Pts',(-20.5343643484455,-12.5321671007081,
122.953349423013)) ;
#97913 = CARTESIAN_POINT('Ctrl Pts',(-20.5257935014248,-12.5332359072362,
122.93231704291)) ;
#97914 = CARTESIAN_POINT('Ctrl Pts',(-20.5165941531816,-12.5343060899024,
122.911440402021)) ;
#97915 = CARTESIAN_POINT('Ctrl Pts',(-20.5068634554415,-12.5353682558269,
122.890936630329)) ;
#97916 = CARTESIAN_POINT('Ctrl Pts',(-20.4904550413478,-12.5371593358493,
122.856362092573)) ;
#97917 = CARTESIAN_POINT('Ctrl Pts',(-20.4723169096776,-12.5389655205005,
122.822370467086)) ;
#97918 = CARTESIAN_POINT('Ctrl Pts',(-20.4525322484779,-12.5407863761255,
122.789218987759)) ;
#97919 = CARTESIAN_POINT('Ctrl Pts',(-20.4364149882719,-12.5422697072582,
122.762212661335)) ;
#97920 = CARTESIAN_POINT('Ctrl Pts',(-20.4192060558486,-12.5437627744711,
122.735763811037)) ;
#97921 = CARTESIAN_POINT('Ctrl Pts',(-20.4009740009317,-12.5452653433241,
122.710001513587)) ;
#97922 = CARTESIAN_POINT('Ctrl Pts',(-20.3601607316284,-12.5486289108168,
122.652331460018)) ;
#97923 = CARTESIAN_POINT('Ctrl Pts',(-20.314382633631,-12.5519576978783,122.598319162259)) ;
#97924 = CARTESIAN_POINT('Ctrl Pts',(-20.264194774419,-12.5552556142764,122.548613573552)) ;
#97925 = CARTESIAN_POINT('Ctrl Pts',(-20.2199733821787,-12.5581614655501,
122.50481711821)) ;
#97926 = CARTESIAN_POINT('Ctrl Pts',(-20.1724287468514,-12.5610855672777,
122.46446661033)) ;
#97927 = CARTESIAN_POINT('Ctrl Pts',(-20.1220491099906,-12.5640439274086,
122.427968155092)) ;
#97928 = CARTESIAN_POINT('Ctrl Pts',(-20.1153547340205,-12.564437030182,122.4231182912)) ;
#97929 = CARTESIAN_POINT('Ctrl Pts',(-20.1086103483572,-12.5648307378465,
122.418336383281)) ;
#97930 = CARTESIAN_POINT('Ctrl Pts',(-20.1018171428105,-12.5652250879601,
122.413623330901)) ;
#97931 = CARTESIAN_POINT('Ctrl Pts',(-20.0543887279106,-12.5679783390836,
122.380718010695)) ;
#97932 = CARTESIAN_POINT('Ctrl Pts',(-20.0046414660269,-12.5707060852374,
122.3512164515)) ;
#97933 = CARTESIAN_POINT('Ctrl Pts',(-19.9530333777819,-12.5734075221596,
122.325386743022)) ;
#97934 = CARTESIAN_POINT('Ctrl Pts',(-19.941254108775,-12.5740241106304,122.319491250767)) ;
#97935 = CARTESIAN_POINT('Ctrl Pts',(-19.9293780049681,-12.5746393285057,
122.313786859513)) ;
#97936 = CARTESIAN_POINT('Ctrl Pts',(-19.917410699934,-12.5752531662224,122.308276425695)) ;
#97937 = CARTESIAN_POINT('Ctrl Pts',(-19.8633471850043,-12.5780262403996,
122.283382481727)) ;
#97938 = CARTESIAN_POINT('Ctrl Pts',(-19.8074868691746,-12.5808351609625,
122.262481160964)) ;
#97939 = CARTESIAN_POINT('Ctrl Pts',(-19.7503640578849,-12.5836604667693,
122.245771695433)) ;
#97940 = CARTESIAN_POINT('Ctrl Pts',(-19.740014119503,-12.5841723768162,122.242744149437)) ;
#97941 = CARTESIAN_POINT('Ctrl Pts',(-19.7296227829521,-12.5846848247728,
122.23985408833)) ;
#97942 = CARTESIAN_POINT('Ctrl Pts',(-19.7191932913646,-12.5851976948804,
122.237102525828)) ;
#97943 = CARTESIAN_POINT('Ctrl Pts',(-19.6558874459894,-12.5883107589698,
122.220400849739)) ;
#97944 = CARTESIAN_POINT('Ctrl Pts',(-19.5912954627906,-12.5913740642442,
122.208837801332)) ;
#97945 = CARTESIAN_POINT('Ctrl Pts',(-19.526127439856,-12.5944572798939,122.202540410786)) ;
#97946 = CARTESIAN_POINT('Ctrl Pts',(-19.5207121490837,-12.5947134869799,
122.202017114246)) ;
#97947 = CARTESIAN_POINT('Ctrl Pts',(-19.5152928865667,-12.5949698315505,
122.201530148797)) ;
#97948 = CARTESIAN_POINT('Ctrl Pts',(-19.5098700634689,-12.5952263535819,
122.201079571498)) ;
#97949 = CARTESIAN_POINT('Ctrl Pts',(-19.4391885772369,-12.5985698811328,
122.195206712913)) ;
#97950 = CARTESIAN_POINT('Ctrl Pts',(-19.368108823692,-12.6019299757216,122.195534711353)) ;
#97951 = CARTESIAN_POINT('Ctrl Pts',(-19.2974771300709,-12.6052545103642,
122.202061638855)) ;
#97952 = CARTESIAN_POINT('Ctrl Pts',(-19.264919611918,-12.6067869470287,122.205070211207)) ;
#97953 = CARTESIAN_POINT('Ctrl Pts',(-19.232519142656,-12.6083230835739,122.20939412978)) ;
#97954 = CARTESIAN_POINT('Ctrl Pts',(-19.2005115540717,-12.6098552748236,
122.214976955947)) ;
#97955 = CARTESIAN_POINT('Ctrl Pts',(-19.1683618366306,-12.6113942697283,
122.220584572507)) ;
#97956 = CARTESIAN_POINT('Ctrl Pts',(-19.1366090978605,-12.6129292842218,
122.227462097252)) ;
#97957 = CARTESIAN_POINT('Ctrl Pts',(-19.1054768153904,-12.6144525708304,
122.235502147131)) ;
#97958 = CARTESIAN_POINT('Ctrl Pts',(-19.1010216926892,-12.6146705576984,
122.236652702308)) ;
#97959 = CARTESIAN_POINT('Ctrl Pts',(-19.0965792414712,-12.6148883043974,
122.237826984182)) ;
#97960 = CARTESIAN_POINT('Ctrl Pts',(-19.0921500800229,-12.615105788223,122.239024599188)) ;
#97961 = CARTESIAN_POINT('Ctrl Pts',(-19.0757863316444,-12.6159092925976,
122.243449244994)) ;
#97962 = CARTESIAN_POINT('Ctrl Pts',(-19.0592877183448,-12.6167226885707,
122.248282362629)) ;
#97963 = CARTESIAN_POINT('Ctrl Pts',(-19.0429653896252,-12.6175313828714,
122.253443784117)) ;
#97964 = CARTESIAN_POINT('Ctrl Pts',(-19.0338845974628,-12.6179812932361,
122.256315298139)) ;
#97965 = CARTESIAN_POINT('Ctrl Pts',(-19.0248581373652,-12.6184297483577,
122.2592875218)) ;
#97966 = CARTESIAN_POINT('Ctrl Pts',(-19.015937477921,-12.6188742353227,122.262339980754)) ;
#97967 = CARTESIAN_POINT('Ctrl Pts',(-18.9943633025614,-12.6199492051485,
122.269722202343)) ;
#97968 = CARTESIAN_POINT('Ctrl Pts',(-18.9727448824911,-12.621033427544,122.277802596725)) ;
#97969 = CARTESIAN_POINT('Ctrl Pts',(-18.951332662961,-12.6221207014324,122.286516090025)) ;
#97970 = CARTESIAN_POINT('Ctrl Pts',(-18.932710984903,-12.6230662766579,122.294093999768)) ;
#97971 = CARTESIAN_POINT('Ctrl Pts',(-18.9142452661049,-12.6240141598346,
122.302149910466)) ;
#97972 = CARTESIAN_POINT('Ctrl Pts',(-18.8960888185098,-12.6249602721053,
122.310610997432)) ;
#97973 = CARTESIAN_POINT('Ctrl Pts',(-18.8623769650047,-12.6267169592603,
122.326321059812)) ;
#97974 = CARTESIAN_POINT('Ctrl Pts',(-18.8291703996934,-12.6284881998388,
122.343684588744)) ;
#97975 = CARTESIAN_POINT('Ctrl Pts',(-18.796723314406,-12.630261824987,122.362627814245)) ;
#97976 = CARTESIAN_POINT('Ctrl Pts',(-18.7681602501713,-12.6318231414685,
122.379303474385)) ;
#97977 = CARTESIAN_POINT('Ctrl Pts',(-18.7401858451121,-12.6333863058065,
122.397202430399)) ;
#97978 = CARTESIAN_POINT('Ctrl Pts',(-18.7129609677122,-12.6349430168755,
122.416243312375)) ;
#97979 = CARTESIAN_POINT('Ctrl Pts',(-18.65537916063,-12.6382355289092,122.456515610996)) ;
#97980 = CARTESIAN_POINT('Ctrl Pts',(-18.6014126610834,-12.64154805959,122.501699936648)) ;
#97981 = CARTESIAN_POINT('Ctrl Pts',(-18.5516760417856,-12.6448737795494,
122.551264588604)) ;
#97982 = CARTESIAN_POINT('Ctrl Pts',(-18.5081695754955,-12.6477829101929,
122.594620628679)) ;
#97983 = CARTESIAN_POINT('Ctrl Pts',(-18.4679940640809,-12.6506640612105,
122.641239022823)) ;
#97984 = CARTESIAN_POINT('Ctrl Pts',(-18.4315471870801,-12.6535589646203,
122.69065080508)) ;
#97985 = CARTESIAN_POINT('Ctrl Pts',(-18.4261283549183,-12.6539893717496,
122.697997227515)) ;
#97986 = CARTESIAN_POINT('Ctrl Pts',(-18.420791871952,-12.6544200828757,122.705405338076)) ;
#97987 = CARTESIAN_POINT('Ctrl Pts',(-18.4155389701689,-12.6548512351516,
122.712873531796)) ;
#97988 = CARTESIAN_POINT('Ctrl Pts',(-18.3822506705162,-12.6575835013828,
122.760200415237)) ;
#97989 = CARTESIAN_POINT('Ctrl Pts',(-18.3523671417877,-12.6603208780007,
122.809879007862)) ;
#97990 = CARTESIAN_POINT('Ctrl Pts',(-18.326160980716,-12.6630421379968,122.861450579004)) ;
#97991 = CARTESIAN_POINT('Ctrl Pts',(-18.3202342287031,-12.6636575746918,
122.873113939854)) ;
#97992 = CARTESIAN_POINT('Ctrl Pts',(-18.3144953835249,-12.6642721870576,
122.884874016727)) ;
#97993 = CARTESIAN_POINT('Ctrl Pts',(-18.308947278158,-12.6648857295503,122.896725318607)) ;
#97994 = CARTESIAN_POINT('Ctrl Pts',(-18.2839766277757,-12.6676471326003,
122.950065097914)) ;
#97995 = CARTESIAN_POINT('Ctrl Pts',(-18.2629042147484,-12.6704151369168,
123.005188849325)) ;
#97996 = CARTESIAN_POINT('Ctrl Pts',(-18.2459271204826,-12.6732053908041,
123.06157649149)) ;
#97997 = CARTESIAN_POINT('Ctrl Pts',(-18.2425230455819,-12.6737648642379,
123.072882770079)) ;
#97998 = CARTESIAN_POINT('Ctrl Pts',(-18.2392834628039,-12.674325232198,123.084239803811)) ;
#97999 = CARTESIAN_POINT('Ctrl Pts',(-18.2362097247212,-12.6748866208308,
123.095643311234)) ;
#98000 = CARTESIAN_POINT('Ctrl Pts',(-18.2197606774572,-12.6778908807596,
123.156668950869)) ;
#98001 = CARTESIAN_POINT('Ctrl Pts',(-18.2080932229473,-12.6808711487217,
123.218922344467)) ;
#98002 = CARTESIAN_POINT('Ctrl Pts',(-18.2013270459942,-12.6838320550255,
123.281754494586)) ;
#98003 = CARTESIAN_POINT('Ctrl Pts',(-18.2005072046526,-12.6841908209008,
123.289367714667)) ;
#98004 = CARTESIAN_POINT('Ctrl Pts',(-18.1997592601557,-12.6845493025162,
123.296989420099)) ;
#98005 = CARTESIAN_POINT('Ctrl Pts',(-18.1990833744788,-12.6849075081088,
123.304618445561)) ;
#98006 = CARTESIAN_POINT('Ctrl Pts',(-18.1928676180941,-12.6882017319327,
123.374778482004)) ;
#98007 = CARTESIAN_POINT('Ctrl Pts',(-18.19276306282,-12.6915271808586,123.445375035136)) ;
#98008 = CARTESIAN_POINT('Ctrl Pts',(-18.1987825324872,-12.6948703138278,
123.515597140546)) ;
#98009 = CARTESIAN_POINT('Ctrl Pts',(-18.2016301149524,-12.6964518230551,
123.548816551406)) ;
#98010 = CARTESIAN_POINT('Ctrl Pts',(-18.2058458747109,-12.6980235182476,
123.581876442846)) ;
#98011 = CARTESIAN_POINT('Ctrl Pts',(-18.2113730134147,-12.6995841135068,
123.614539279926)) ;
#98012 = CARTESIAN_POINT('Ctrl Pts',(-18.2169231633016,-12.7011512060054,
123.647338102472)) ;
#98013 = CARTESIAN_POINT('Ctrl Pts',(-18.2237954271965,-12.7027071059535,
123.679735951078)) ;
#98014 = CARTESIAN_POINT('Ctrl Pts',(-18.2318821698856,-12.704250511325,123.711507884019)) ;
#98015 = CARTESIAN_POINT('Ctrl Pts',(-18.2328296452799,-12.7044313429242,
123.715230411845)) ;
#98016 = CARTESIAN_POINT('Ctrl Pts',(-18.2337937384031,-12.7046120030052,
123.718944370924)) ;
#98017 = CARTESIAN_POINT('Ctrl Pts',(-18.2347742338545,-12.7047924894739,
123.722649419171)) ;
#98018 = CARTESIAN_POINT('Ctrl Pts',(-18.2393315788933,-12.705631390982,123.739870491668)) ;
#98019 = CARTESIAN_POINT('Ctrl Pts',(-18.2443302770562,-12.706483268537,123.757210917875)) ;
#98020 = CARTESIAN_POINT('Ctrl Pts',(-18.2496955204389,-12.7073326882528,
123.774371597192)) ;
#98021 = CARTESIAN_POINT('Ctrl Pts',(-18.2529356436212,-12.7078456611631,
123.784735100004)) ;
#98022 = CARTESIAN_POINT('Ctrl Pts',(-18.2563084612474,-12.708357737682,123.795033282245)) ;
#98023 = CARTESIAN_POINT('Ctrl Pts',(-18.259788698278,-12.7088655184933,123.80520302707)) ;
#98024 = CARTESIAN_POINT('Ctrl Pts',(-18.2669483266768,-12.7099101375478,
123.826124473862)) ;
#98025 = CARTESIAN_POINT('Ctrl Pts',(-18.2747672024254,-12.7109660365692,
123.847094489254)) ;
#98026 = CARTESIAN_POINT('Ctrl Pts',(-18.2831760701599,-12.7120216609084,
123.867859060196)) ;
#98027 = CARTESIAN_POINT('Ctrl Pts',(-18.290113361736,-12.7128925479371,123.884989771205)) ;
#98028 = CARTESIAN_POINT('Ctrl Pts',(-18.2974512583823,-12.7137632480116,
123.901980759439)) ;
#98029 = CARTESIAN_POINT('Ctrl Pts',(-18.3051258897595,-12.7146272730841,
123.918698999033)) ;
#98030 = CARTESIAN_POINT('Ctrl Pts',(-18.3201817067025,-12.7163222865232,
123.951496242646)) ;
#98031 = CARTESIAN_POINT('Ctrl Pts',(-18.3368069909225,-12.7180282649194,
123.983848034839)) ;
#98032 = CARTESIAN_POINT('Ctrl Pts',(-18.3549324233468,-12.7197467163026,
124.015504866554)) ;
#98033 = CARTESIAN_POINT('Ctrl Pts',(-18.3716663093501,-12.7213332367715,
124.044731303791)) ;
#98034 = CARTESIAN_POINT('Ctrl Pts',(-18.3896781708207,-12.7229303885638,
124.073365123192)) ;
#98035 = CARTESIAN_POINT('Ctrl Pts',(-18.4088768334324,-12.724539358364,124.101224785305)) ;
#98036 = CARTESIAN_POINT('Ctrl Pts',(-18.4491275723409,-12.7279126257966,
124.159633644737)) ;
#98037 = CARTESIAN_POINT('Ctrl Pts',(-18.4944275965094,-12.7312613121533,
124.214417206875)) ;
#98038 = CARTESIAN_POINT('Ctrl Pts',(-18.5442292542679,-12.7345698810621,
124.264916903438)) ;
#98039 = CARTESIAN_POINT('Ctrl Pts',(-18.5887386598446,-12.7375268596462,
124.310050169619)) ;
#98040 = CARTESIAN_POINT('Ctrl Pts',(-18.6367330228432,-12.7405056930324,
124.351645964647)) ;
#98041 = CARTESIAN_POINT('Ctrl Pts',(-18.6877054107912,-12.7435210083957,
124.389274681643)) ;
#98042 = CARTESIAN_POINT('Ctrl Pts',(-18.6934843042472,-12.7438628637986,
124.393540762852)) ;
#98043 = CARTESIAN_POINT('Ctrl Pts',(-18.6993014407765,-12.7442051881205,
124.397755896102)) ;
#98044 = CARTESIAN_POINT('Ctrl Pts',(-18.7051560542356,-12.7445480026765,
124.401919487515)) ;
#98045 = CARTESIAN_POINT('Ctrl Pts',(-18.7523161220863,-12.7473094416401,
124.435458038763)) ;
#98046 = CARTESIAN_POINT('Ctrl Pts',(-18.8018455593698,-12.7500407281242,
124.46560262868)) ;
#98047 = CARTESIAN_POINT('Ctrl Pts',(-18.8532867392077,-12.7527494963093,
124.492078493519)) ;
#98048 = CARTESIAN_POINT('Ctrl Pts',(-18.8648711673282,-12.753359504292,124.498040793647)) ;
#98049 = CARTESIAN_POINT('Ctrl Pts',(-18.8765524420874,-12.7539683702829,
124.50381721878)) ;
#98050 = CARTESIAN_POINT('Ctrl Pts',(-18.8883251538838,-12.7545761814695,
124.509404946278)) ;
#98051 = CARTESIAN_POINT('Ctrl Pts',(-18.9417239133121,-12.7573330962649,
124.534749804931)) ;
#98052 = CARTESIAN_POINT('Ctrl Pts',(-18.9969404708393,-12.7601272255492,
124.556177860383)) ;
#98053 = CARTESIAN_POINT('Ctrl Pts',(-19.0534514339364,-12.7629283003078,
124.573487347359)) ;
#98054 = CARTESIAN_POINT('Ctrl Pts',(-19.0640589928895,-12.7634540844036,
124.576736476262)) ;
#98055 = CARTESIAN_POINT('Ctrl Pts',(-19.0747121066515,-12.7639801132182,
124.579840628182)) ;
#98056 = CARTESIAN_POINT('Ctrl Pts',(-19.0854072398552,-12.7645061865598,
124.582798659793)) ;
#98057 = CARTESIAN_POINT('Ctrl Pts',(-19.1484560428165,-12.7676074377385,
124.600236530702)) ;
#98058 = CARTESIAN_POINT('Ctrl Pts',(-19.2128533641525,-12.7706663358614,
124.612561216615)) ;
#98059 = CARTESIAN_POINT('Ctrl Pts',(-19.2778924676512,-12.773756334454,124.619635764162)) ;
#98060 = CARTESIAN_POINT('Ctrl Pts',(-19.2830428465134,-12.7740010282241,
124.620195990213)) ;
#98061 = CARTESIAN_POINT('Ctrl Pts',(-19.2881972439497,-12.7742459170218,
124.620723319615)) ;
#98062 = CARTESIAN_POINT('Ctrl Pts',(-19.2933553055049,-12.7744910373231,
124.621217697948)) ;
#98063 = CARTESIAN_POINT('Ctrl Pts',(-19.3639604343561,-12.7778463192005,
124.627984900231)) ;
#98064 = CARTESIAN_POINT('Ctrl Pts',(-19.4350409539448,-12.7812066706123,
124.628556271668)) ;
#98065 = CARTESIAN_POINT('Ctrl Pts',(-19.5057548323387,-12.7845191703928,
124.622922629244)) ;
#98066 = CARTESIAN_POINT('Ctrl Pts',(-19.5408861042798,-12.7861648491936,
124.62012378652)) ;
#98067 = CARTESIAN_POINT('Ctrl Pts',(-19.5758538458867,-12.7878143806419,
124.615794540443)) ;
#98068 = CARTESIAN_POINT('Ctrl Pts',(-19.6103880774634,-12.7894647330416,
124.60999777973)) ;
#98069 = CARTESIAN_POINT('Ctrl Pts',(-19.6449223090401,-12.7911150854413,
124.604201019016)) ;
#98070 = CARTESIAN_POINT('Ctrl Pts',(-19.6790223059611,-12.7927662587925,
124.596937033337)) ;
#98071 = CARTESIAN_POINT('Ctrl Pts',(-19.7124361548751,-12.7944152213992,
124.588326731793)) ;
#98072 = CARTESIAN_POINT('Ctrl Pts',(-19.7307060383748,-12.7953168342243,
124.583618827399)) ;
#98073 = CARTESIAN_POINT('Ctrl Pts',(-19.7490715788918,-12.7962290946323,
124.578427960073)) ;
#98074 = CARTESIAN_POINT('Ctrl Pts',(-19.7672465551424,-12.7971348160649,
124.572823932136)) ;
#98075 = CARTESIAN_POINT('Ctrl Pts',(-19.7791662883019,-12.7977288172698,
124.569148630627)) ;
#98076 = CARTESIAN_POINT('Ctrl Pts',(-19.7910042821239,-12.7983200059584,
124.565296675232)) ;
#98077 = CARTESIAN_POINT('Ctrl Pts',(-19.802683428241,-12.7989035340819,124.561299394608)) ;
#98078 = CARTESIAN_POINT('Ctrl Pts',(-19.8228762261398,-12.7999124319371,
124.554388248967)) ;
#98079 = CARTESIAN_POINT('Ctrl Pts',(-19.8431249000216,-12.8009244496695,
124.546858995403)) ;
#98080 = CARTESIAN_POINT('Ctrl Pts',(-19.8631705724731,-12.8019330346866,
124.538785223922)) ;
#98081 = CARTESIAN_POINT('Ctrl Pts',(-19.8788708148474,-12.8027229822057,
124.532461656109)) ;
#98082 = CARTESIAN_POINT('Ctrl Pts',(-19.8944467130077,-12.8035108239631,
124.525805083938)) ;
#98083 = CARTESIAN_POINT('Ctrl Pts',(-19.9097819710943,-12.8042934117004,
124.518871730917)) ;
#98084 = CARTESIAN_POINT('Ctrl Pts',(-19.94188830032,-12.8059318594787,124.504355867314)) ;
#98085 = CARTESIAN_POINT('Ctrl Pts',(-19.9736004839142,-12.8075974503459,
124.488331287839)) ;
#98086 = CARTESIAN_POINT('Ctrl Pts',(-20.0046715041761,-12.8092799940258,
124.470862698542)) ;
#98087 = CARTESIAN_POINT('Ctrl Pts',(-20.0345082300797,-12.8108956987621,
124.454088047874)) ;
#98088 = CARTESIAN_POINT('Ctrl Pts',(-20.0637532939055,-12.812527036165,124.435982306778)) ;
#98089 = CARTESIAN_POINT('Ctrl Pts',(-20.0922047094035,-12.8141649827786,
124.416644873957)) ;
#98090 = CARTESIAN_POINT('Ctrl Pts',(-20.1509034453611,-12.8175442661676,
124.376749394474)) ;
#98091 = CARTESIAN_POINT('Ctrl Pts',(-20.2060107058325,-12.8208579572261,
124.331771675715)) ;
#98092 = CARTESIAN_POINT('Ctrl Pts',(-20.2568550593904,-12.8242010480661,
124.28226162519)) ;
#98093 = CARTESIAN_POINT('Ctrl Pts',(-20.3023710803736,-12.8271937932222,
124.237940076368)) ;
#98094 = CARTESIAN_POINT('Ctrl Pts',(-20.3443588781256,-12.8302092116877,
124.190092752336)) ;
#98095 = CARTESIAN_POINT('Ctrl Pts',(-20.3823816688422,-12.8331908220597,
124.139225484442)) ;
#98096 = CARTESIAN_POINT('Ctrl Pts',(-20.3868328345476,-12.8335398664509,
124.133270670655)) ;
#98097 = CARTESIAN_POINT('Ctrl Pts',(-20.3912297070035,-12.8338884475229,
124.127274508312)) ;
#98098 = CARTESIAN_POINT('Ctrl Pts',(-20.3955716204218,-12.8342364746619,
124.121237839938)) ;
#98099 = CARTESIAN_POINT('Ctrl Pts',(-20.4301136324034,-12.8370051981363,
124.07321323622)) ;
#98100 = CARTESIAN_POINT('Ctrl Pts',(-20.4611186192062,-12.839777951976,124.022699290936)) ;
#98101 = CARTESIAN_POINT('Ctrl Pts',(-20.4882962820212,-12.8425868853046,
123.97017709754)) ;
#98102 = CARTESIAN_POINT('Ctrl Pts',(-20.4934411728496,-12.8431186328437,
123.960234338557)) ;
#98103 = CARTESIAN_POINT('Ctrl Pts',(-20.4984490345155,-12.8436516769366,
123.950219686188)) ;
#98104 = CARTESIAN_POINT('Ctrl Pts',(-20.50331807879,-12.8441862356861,123.940136510919)) ;
#98105 = CARTESIAN_POINT('Ctrl Pts',(-20.5284481137189,-12.8469451919185,
123.888095384894)) ;
#98106 = CARTESIAN_POINT('Ctrl Pts',(-20.5498457616801,-12.8496745801067,
123.834290984065)) ;
#98107 = CARTESIAN_POINT('Ctrl Pts',(-20.5673171434777,-12.8523779218257,
123.779218839189)) ;
#98108 = CARTESIAN_POINT('Ctrl Pts',(-20.5712802775123,-12.8529911363784,
123.766726507773)) ;
#98109 = CARTESIAN_POINT('Ctrl Pts',(-20.5750415858579,-12.8536030107241,
123.754169020186)) ;
#98110 = CARTESIAN_POINT('Ctrl Pts',(-20.5785991550522,-12.8542135859657,
123.741552291233)) ;
#98111 = CARTESIAN_POINT('Ctrl Pts',(-20.5960109845387,-12.8572019275588,
123.679802168832)) ;
#98112 = CARTESIAN_POINT('Ctrl Pts',(-20.6085129387713,-12.8602368807548,
123.616722534805)) ;
#98113 = CARTESIAN_POINT('Ctrl Pts',(-20.6159685127212,-12.8632832123376,
123.552985078507)) ;
#98114 = CARTESIAN_POINT('Ctrl Pts',(-20.6166742265608,-12.8635715655044,
123.546951954121)) ;
#98115 = CARTESIAN_POINT('Ctrl Pts',(-20.6173347636916,-12.8638600206184,
123.540912944753)) ;
#98116 = CARTESIAN_POINT('Ctrl Pts',(-20.6179500318442,-12.8641485477988,
123.534868626259)) ;
#98117 = CARTESIAN_POINT('Ctrl Pts',(-20.6251084554465,-12.8675054577398,
123.464545155117)) ;
#98118 = CARTESIAN_POINT('Ctrl Pts',(-20.6261171824217,-12.8708059686782,
123.393712914287)) ;
#98119 = CARTESIAN_POINT('Ctrl Pts',(-20.6209576405811,-12.8741441467102,
123.323187825837)) ;
#98120 = CARTESIAN_POINT('Ctrl Pts',(-20.6183711618751,-12.8758175756045,
123.287833593785)) ;
#98121 = CARTESIAN_POINT('Ctrl Pts',(-20.6142358980022,-12.8774935606388,
123.252638459521)) ;
#98122 = CARTESIAN_POINT('Ctrl Pts',(-20.6086118069863,-12.8791574474389,
123.217863914333)) ;
#98123 = CARTESIAN_POINT('Ctrl Pts',(-20.6029877159705,-12.8808213342391,
123.183089369145)) ;
#98124 = CARTESIAN_POINT('Ctrl Pts',(-20.5958750645239,-12.882473122805,123.148736096639)) ;
#98125 = CARTESIAN_POINT('Ctrl Pts',(-20.5873887054029,-12.8840981587624,
123.115048612279)) ;
#98126 = CARTESIAN_POINT('Ctrl Pts',(-20.5825573130237,-12.8850233124389,
123.095869898194)) ;
#98127 = CARTESIAN_POINT('Ctrl Pts',(-20.5772033451909,-12.8859571442745,
123.076611552308)) ;
#98128 = CARTESIAN_POINT('Ctrl Pts',(-20.5713923155841,-12.8868906481699,
123.057550179837)) ;
#98129 = CARTESIAN_POINT('Ctrl Pts',(-20.5673718295211,-12.8875365129573,
123.044362158515)) ;
#98130 = CARTESIAN_POINT('Ctrl Pts',(-20.5631336338023,-12.8881822207643,
123.031268219582)) ;
#98131 = CARTESIAN_POINT('Ctrl Pts',(-20.5587133983318,-12.8888247888663,
123.018355650104)) ;
#98132 = CARTESIAN_POINT('Origin',(-19.4092696390481,30.19753203383,123.411833654989)) ;
#98133 = CARTESIAN_POINT('',(-19.1445267022232,-12.4073898409303,124.597577877357)) ;
#98134 = CARTESIAN_POINT('Ctrl Pts',(-19.1445297491651,-12.4073818757045,
124.597564942756)) ;
#98135 = CARTESIAN_POINT('Ctrl Pts',(-19.1597522610698,-12.408108682073,124.600963694368)) ;
#98136 = CARTESIAN_POINT('Ctrl Pts',(-19.1750386830709,-12.4088372172118,
124.604068961096)) ;
#98137 = CARTESIAN_POINT('Ctrl Pts',(-19.1940988116055,-12.4097464761479,
124.607560087043)) ;
#98138 = CARTESIAN_POINT('Ctrl Pts',(-19.1978202100327,-12.4099240390499,
124.608223777035)) ;
#98139 = CARTESIAN_POINT('Ctrl Pts',(-19.2044726945695,-12.4102415458129,
124.609378200849)) ;
#98140 = CARTESIAN_POINT('Ctrl Pts',(-19.2074026006058,-12.4103814140366,
124.609875568492)) ;
#98141 = CARTESIAN_POINT('Ctrl Pts',(-19.2133565143437,-12.4106657168856,
124.610863816867)) ;
#98142 = CARTESIAN_POINT('Ctrl Pts',(-19.2163806121701,-12.4108101581136,
124.611354019451)) ;
#98143 = CARTESIAN_POINT('Ctrl Pts',(-19.2229214352943,-12.4111226624184,
124.612388904408)) ;
#98144 = CARTESIAN_POINT('Ctrl Pts',(-19.226438762352,-12.4112907692347,124.612929583864)) ;
#98145 = CARTESIAN_POINT('Ctrl Pts',(-19.2361423968796,-12.4117547094832,
124.614377603211)) ;
#98146 = CARTESIAN_POINT('Ctrl Pts',(-19.2423333921115,-12.4120508944275,
124.615252650288)) ;
#98147 = CARTESIAN_POINT('Ctrl Pts',(-19.2767898878628,-12.4137002868897,
124.619851789184)) ;
#98148 = CARTESIAN_POINT('Ctrl Pts',(-19.3051726636459,-12.4150636267818,
124.622627806768)) ;
#98149 = CARTESIAN_POINT('Ctrl Pts',(-19.347032332819,-12.4170652350893,124.625239124705)) ;
#98150 = CARTESIAN_POINT('Ctrl Pts',(-19.3604513412666,-12.417705304266,124.625853051119)) ;
#98151 = CARTESIAN_POINT('Ctrl Pts',(-19.3822928221772,-12.4187433436747,
124.626489581294)) ;
#98152 = CARTESIAN_POINT('Ctrl Pts',(-19.3907101469302,-12.4191424930192,
124.626647350388)) ;
#98153 = CARTESIAN_POINT('Ctrl Pts',(-19.3994233737774,-12.4195547371103,
124.626720083474)) ;
#98154 = CARTESIAN_POINT('Ctrl Pts',(-19.3997182732379,-12.4195686884279,
124.626722437746)) ;
#98155 = CARTESIAN_POINT('Ctrl Pts',(-19.4002595644142,-12.4195942942127,
124.626726561937)) ;
#98156 = CARTESIAN_POINT('Ctrl Pts',(-19.400505955816,-12.4196059489958,124.626728364276)) ;
#98157 = CARTESIAN_POINT('Ctrl Pts',(-19.4009628340174,-12.4196275587905,
124.626731567319)) ;
#98158 = CARTESIAN_POINT('Ctrl Pts',(-19.4011733208026,-12.4196375140076,
124.626732988277)) ;
#98159 = CARTESIAN_POINT('Ctrl Pts',(-19.4015674110765,-12.419656151924,124.626735546288)) ;
#98160 = CARTESIAN_POINT('Ctrl Pts',(-19.4017510142668,-12.4196648347421,
124.62673669642)) ;
#98161 = CARTESIAN_POINT('Ctrl Pts',(-19.4020979562285,-12.4196812412509,
124.626738791093)) ;
#98162 = CARTESIAN_POINT('Ctrl Pts',(-19.4022612950798,-12.4196889650336,
124.626739744315)) ;
#98163 = CARTESIAN_POINT('Ctrl Pts',(-19.4025726986476,-12.4197036896964,
124.626741498819)) ;
#98164 = CARTESIAN_POINT('Ctrl Pts',(-19.4027207631715,-12.4197106906269,
124.626742305972)) ;
#98165 = CARTESIAN_POINT('Ctrl Pts',(-19.4030054970116,-12.4197241531619,
124.626743806107)) ;
#98166 = CARTESIAN_POINT('Ctrl Pts',(-19.4031421662597,-12.4197306148036,
124.626744503093)) ;
#98167 = CARTESIAN_POINT('Ctrl Pts',(-19.4034072340054,-12.4197431465988,
124.626745810159)) ;
#98168 = CARTESIAN_POINT('Ctrl Pts',(-19.4035356326958,-12.4197492167886,
124.626746422945)) ;
#98169 = CARTESIAN_POINT('Ctrl Pts',(-19.4037867866338,-12.4197610899663,
124.626747581769)) ;
#98170 = CARTESIAN_POINT('Ctrl Pts',(-19.4039095417018,-12.4197668929633,
124.626748129556)) ;
#98171 = CARTESIAN_POINT('Ctrl Pts',(-19.4041517346269,-12.4197783417729,
124.626749173618)) ;
#98172 = CARTESIAN_POINT('Ctrl Pts',(-19.4042711724272,-12.4197839875926,
124.626749670886)) ;
#98173 = CARTESIAN_POINT('Ctrl Pts',(-19.4045089208813,-12.4197952255989,
124.626750625669)) ;
#98174 = CARTESIAN_POINT('Ctrl Pts',(-19.4046272316321,-12.4198008177934,
124.626751083515)) ;
#98175 = CARTESIAN_POINT('Ctrl Pts',(-19.4079842736925,-12.4199594901724,
124.626763584428)) ;
#98176 = CARTESIAN_POINT('Ctrl Pts',(-19.4112230458149,-12.4201124419578,
124.626762694024)) ;
#98177 = CARTESIAN_POINT('Ctrl Pts',(-19.4177595895664,-12.4204208801708,
124.626734759013)) ;
#98178 = CARTESIAN_POINT('Ctrl Pts',(-19.4210573317611,-12.4205763606125,
124.626707237795)) ;
#98179 = CARTESIAN_POINT('Ctrl Pts',(-19.4288191601387,-12.4209420287583,
124.626610854626)) ;
#98180 = CARTESIAN_POINT('Ctrl Pts',(-19.4332830628642,-12.4211521073302,
124.62653081239)) ;
#98181 = CARTESIAN_POINT('Ctrl Pts',(-19.4473797140403,-12.4218149193642,
124.626200308583)) ;
#98182 = CARTESIAN_POINT('Ctrl Pts',(-19.4570099979282,-12.422266828784,124.625859851903)) ;
#98183 = CARTESIAN_POINT('Ctrl Pts',(-19.4865873418857,-12.4236534401429,
124.624461728316)) ;
#98184 = CARTESIAN_POINT('Ctrl Pts',(-19.5065130332382,-12.4245854633194,
124.623026699042)) ;
#98185 = CARTESIAN_POINT('Ctrl Pts',(-19.5380419369685,-12.4260679981876,
124.619972940095)) ;
#98186 = CARTESIAN_POINT('Ctrl Pts',(-19.5496725942517,-12.4266169254272,
124.618676578963)) ;
#98187 = CARTESIAN_POINT('Ctrl Pts',(-19.5677801399084,-12.4274748180016,
124.616392996069)) ;
#98188 = CARTESIAN_POINT('Ctrl Pts',(-19.5742708968855,-12.4277829769077,
124.615521060262)) ;
#98189 = CARTESIAN_POINT('Ctrl Pts',(-19.588282887161,-12.4284495607254,124.613523292671)) ;
#98190 = CARTESIAN_POINT('Ctrl Pts',(-19.5958012436992,-12.428808065468,124.612379234439)) ;
#98191 = CARTESIAN_POINT('Ctrl Pts',(-19.6045264049005,-12.429225049911,124.610967598289)) ;
#98192 = CARTESIAN_POINT('Ctrl Pts',(-19.6057441609528,-12.429283268924,124.610768674423)) ;
#98193 = CARTESIAN_POINT('Ctrl Pts',(-19.608599984122,-12.429419850734,124.610297699877)) ;
#98194 = CARTESIAN_POINT('Ctrl Pts',(-19.6102378004946,-12.4294982186121,
124.610024145453)) ;
#98195 = CARTESIAN_POINT('Ctrl Pts',(-19.6142673165483,-12.429691119857,124.609342625707)) ;
#98196 = CARTESIAN_POINT('Ctrl Pts',(-19.6166583643886,-12.429805664886,124.608930852097)) ;
#98197 = CARTESIAN_POINT('Ctrl Pts',(-19.6219524903694,-12.4300594602357,
124.608002788172)) ;
#98198 = CARTESIAN_POINT('Ctrl Pts',(-19.6248549547529,-12.4301987190633,
124.607483086078)) ;
#98199 = CARTESIAN_POINT('Ctrl Pts',(-19.6501893937859,-12.4314152607901,
124.602851567482)) ;
#98200 = CARTESIAN_POINT('Ctrl Pts',(-19.6725033647341,-12.4324936651664,
124.59811945603)) ;
#98201 = CARTESIAN_POINT('Ctrl Pts',(-19.7052318246421,-12.4340841684714,
124.590209795527)) ;
#98202 = CARTESIAN_POINT('Ctrl Pts',(-19.715758073243,-12.4345970713355,124.587515918406)) ;
#98203 = CARTESIAN_POINT('Ctrl Pts',(-19.7339512023946,-12.4354857435635,
124.582598991056)) ;
#98204 = CARTESIAN_POINT('Ctrl Pts',(-19.7416349208939,-12.4358617211333,
124.58044090711)) ;
#98205 = CARTESIAN_POINT('Ctrl Pts',(-19.7620878205968,-12.4368644694892,
124.574478373125)) ;
#98206 = CARTESIAN_POINT('Ctrl Pts',(-19.7748166149887,-12.437490708187,124.570539320529)) ;
#98207 = CARTESIAN_POINT('Ctrl Pts',(-19.801193693259,-12.438795364782,124.561898756198)) ;
#98208 = CARTESIAN_POINT('Ctrl Pts',(-19.8148281605916,-12.4394736846218,
124.557161767809)) ;
#98209 = CARTESIAN_POINT('Ctrl Pts',(-19.8378436867238,-12.4406274615898,
124.548703017981)) ;
#98210 = CARTESIAN_POINT('Ctrl Pts',(-19.8472686691203,-12.4411024651111,
124.545105251598)) ;
#98211 = CARTESIAN_POINT('Ctrl Pts',(-19.8635997788736,-12.4419305084062,
124.538637068485)) ;
#98212 = CARTESIAN_POINT('Ctrl Pts',(-19.870526244468,-12.4422832824072,124.535819487701)) ;
#98213 = CARTESIAN_POINT('Ctrl Pts',(-19.8854161213961,-12.4430452937628,
124.529601696)) ;
#98214 = CARTESIAN_POINT('Ctrl Pts',(-19.8933700818837,-12.4434546271019,
124.526179932695)) ;
#98215 = CARTESIAN_POINT('Ctrl Pts',(-19.9262976802346,-12.4451592348976,
124.511595523311)) ;
#98216 = CARTESIAN_POINT('Ctrl Pts',(-19.9509271478109,-12.4464604754934,
124.499676141103)) ;
#98217 = CARTESIAN_POINT('Ctrl Pts',(-19.9840310259112,-12.4482383263611,
124.482252430348)) ;
#98218 = CARTESIAN_POINT('Ctrl Pts',(-19.9928706730205,-12.4487157753617,
124.477458748955)) ;
#98219 = CARTESIAN_POINT('Ctrl Pts',(-20.0082151069925,-12.4495488284819,
124.468889362496)) ;
#98220 = CARTESIAN_POINT('Ctrl Pts',(-20.0147462304276,-12.4499047838707,
124.465161970561)) ;
#98221 = CARTESIAN_POINT('Ctrl Pts',(-20.0248382506359,-12.4504569044783,
124.459277451686)) ;
#98222 = CARTESIAN_POINT('Ctrl Pts',(-20.0284233574409,-12.4506534567024,
124.457162261673)) ;
#98223 = CARTESIAN_POINT('Ctrl Pts',(-20.0353386881921,-12.4510333989571,
124.453034203911)) ;
#98224 = CARTESIAN_POINT('Ctrl Pts',(-20.0386702505976,-12.4512168095075,
124.451023679802)) ;
#98225 = CARTESIAN_POINT('Ctrl Pts',(-20.0464023046056,-12.451643352577,124.446306733878)) ;
#98226 = CARTESIAN_POINT('Ctrl Pts',(-20.0507953107259,-12.4518863590653,
124.443588178756)) ;
#98227 = CARTESIAN_POINT('Ctrl Pts',(-20.0651770042691,-12.452684195224,124.434560889238)) ;
#98228 = CARTESIAN_POINT('Ctrl Pts',(-20.0750910435288,-12.4532378122893,
124.428134460561)) ;
#98229 = CARTESIAN_POINT('Ctrl Pts',(-20.1074613620315,-12.4550596705293,
124.40647454001)) ;
#98230 = CARTESIAN_POINT('Ctrl Pts',(-20.129501013212,-12.456323174896,124.390633401056)) ;
#98231 = CARTESIAN_POINT('Ctrl Pts',(-20.1585512985233,-12.4580383615936,
124.368240468291)) ;
#98232 = CARTESIAN_POINT('Ctrl Pts',(-20.1660418534896,-12.4584852406522,
124.362324481879)) ;
#98233 = CARTESIAN_POINT('Ctrl Pts',(-20.1777855149808,-12.4591938193923,
124.352822590164)) ;
#98234 = CARTESIAN_POINT('Ctrl Pts',(-20.182085049498,-12.4594549633771,124.349294677514)) ;
#98235 = CARTESIAN_POINT('Ctrl Pts',(-20.1901355608543,-12.4599472966531,
124.342595939478)) ;
#98236 = CARTESIAN_POINT('Ctrl Pts',(-20.1938918302385,-12.4601784139697,
124.339431647082)) ;
#98237 = CARTESIAN_POINT('Ctrl Pts',(-20.1998292076798,-12.4605460130388,
124.334368113853)) ;
#98238 = CARTESIAN_POINT('Ctrl Pts',(-20.2020229042113,-12.460682331019,124.332483707872)) ;
#98239 = CARTESIAN_POINT('Ctrl Pts',(-20.2071287038347,-12.4610007912071,
124.328065998147)) ;
#98240 = CARTESIAN_POINT('Ctrl Pts',(-20.2100355016702,-12.4611829994007,
124.325526616031)) ;
#98241 = CARTESIAN_POINT('Ctrl Pts',(-20.2168999636064,-12.4616154601862,
124.319471895233)) ;
#98242 = CARTESIAN_POINT('Ctrl Pts',(-20.2208468461842,-12.4618658442997,
124.31594446284)) ;
#98243 = CARTESIAN_POINT('Ctrl Pts',(-20.236415767874,-12.4628604591203,124.301846010704)) ;
#98244 = CARTESIAN_POINT('Ctrl Pts',(-20.2478552693966,-12.4636068434076,
124.291075854796)) ;
#98245 = CARTESIAN_POINT('Ctrl Pts',(-20.264603070881,-12.4647227455987,124.274683750025)) ;
#98246 = CARTESIAN_POINT('Ctrl Pts',(-20.2700718553775,-12.4650909426615,
124.269228027516)) ;
#98247 = CARTESIAN_POINT('Ctrl Pts',(-20.2884872485762,-12.4663434971793,
124.250502823113)) ;
#98248 = CARTESIAN_POINT('Ctrl Pts',(-20.3011820969803,-12.4672285862906,
124.236989247802)) ;
#98249 = CARTESIAN_POINT('Ctrl Pts',(-20.3206708080862,-12.468616741868,124.215268214004)) ;
#98250 = CARTESIAN_POINT('Ctrl Pts',(-20.3276744543652,-12.4691219684955,
124.207252902508)) ;
#98251 = CARTESIAN_POINT('Ctrl Pts',(-20.3371826050445,-12.4698164997945,
124.196078293781)) ;
#98252 = CARTESIAN_POINT('Ctrl Pts',(-20.3397780198256,-12.4700069988947,
124.192997069004)) ;
#98253 = CARTESIAN_POINT('Ctrl Pts',(-20.3444715445719,-12.4703531730337,
124.187368427101)) ;
#98254 = CARTESIAN_POINT('Ctrl Pts',(-20.3465746898195,-12.4705089144575,
124.184825264733)) ;
#98255 = CARTESIAN_POINT('Ctrl Pts',(-20.3506837493604,-12.4708144342346,
124.179815086105)) ;
#98256 = CARTESIAN_POINT('Ctrl Pts',(-20.3526903921484,-12.4709642213484,
124.177348702738)) ;
#98257 = CARTESIAN_POINT('Ctrl Pts',(-20.3546999879414,-12.4711148299625,
124.174858786871)) ;
#98258 = CARTESIAN_POINT('Ctrl Pts',(-20.3547126418609,-12.4711157783312,
124.174843107698)) ;
#98259 = CARTESIAN_POINT('Ctrl Pts',(-20.354738020646,-12.4711176804341,124.174811659846)) ;
#98260 = CARTESIAN_POINT('Ctrl Pts',(-20.3547507452693,-12.4711186341505,
124.174795891456)) ;
#98261 = CARTESIAN_POINT('Ctrl Pts',(-20.3547762677684,-12.4711205471224,
124.174764262284)) ;
#98262 = CARTESIAN_POINT('Ctrl Pts',(-20.354789065789,-12.4711215063891,124.174748401312)) ;
#98263 = CARTESIAN_POINT('Ctrl Pts',(-20.3548147377802,-12.4711234306648,
124.174716583602)) ;
#98264 = CARTESIAN_POINT('Ctrl Pts',(-20.3548276113553,-12.4711243956444,
124.174700627345)) ;
#98265 = CARTESIAN_POINT('Ctrl Pts',(-20.3548534365392,-12.471126331503,124.174668616454)) ;
#98266 = CARTESIAN_POINT('Ctrl Pts',(-20.3548663886481,-12.4711273024198,
124.174652561189)) ;
#98267 = CARTESIAN_POINT('Ctrl Pts',(-20.3548923733537,-12.4711292503377,
124.17462034921)) ;
#98268 = CARTESIAN_POINT('Ctrl Pts',(-20.3549054061214,-12.4711302273519,
124.174604192273)) ;
#98269 = CARTESIAN_POINT('Ctrl Pts',(-20.3549315552481,-12.4711321876983,
124.174571773068)) ;
#98270 = CARTESIAN_POINT('Ctrl Pts',(-20.3549446711418,-12.4711331709958,
124.174555511367)) ;
#98271 = CARTESIAN_POINT('Ctrl Pts',(-20.3549709888322,-12.4711351440831,
124.174522879735)) ;
#98272 = CARTESIAN_POINT('Ctrl Pts',(-20.3549841909316,-12.471136133896,124.174506509418)) ;
#98273 = CARTESIAN_POINT('Ctrl Pts',(-20.3550106835919,-12.4711381202066,
124.174473657349)) ;
#98274 = CARTESIAN_POINT('Ctrl Pts',(-20.3550239742008,-12.4711391167085,
124.174457175524)) ;
#98275 = CARTESIAN_POINT('Ctrl Pts',(-20.3550506468494,-12.471141116621,124.174424096722)) ;
#98276 = CARTESIAN_POINT('Ctrl Pts',(-20.3550640286481,-12.4711421200139,
124.17440750003)) ;
#98277 = CARTESIAN_POINT('Ctrl Pts',(-20.3550908864516,-12.4711441339178,
124.174374188014)) ;
#98278 = CARTESIAN_POINT('Ctrl Pts',(-20.3551043622901,-12.4711451444166,
124.174357472883)) ;
#98279 = CARTESIAN_POINT('Ctrl Pts',(-20.3551314107843,-12.4711471727293,
124.174323920711)) ;
#98280 = CARTESIAN_POINT('Ctrl Pts',(-20.3551449834907,-12.4711481905474,
124.174307083594)) ;
#98281 = CARTESIAN_POINT('Ctrl Pts',(-20.3551722284057,-12.471150233701,124.174273284079)) ;
#98282 = CARTESIAN_POINT('Ctrl Pts',(-20.3551859007626,-12.4711512590481,
124.174256321483)) ;
#98283 = CARTESIAN_POINT('Ctrl Pts',(-20.3552133477994,-12.4711533174727,
124.17422226747)) ;
#98284 = CARTESIAN_POINT('Ctrl Pts',(-20.3552271226505,-12.4711543505634,
124.174205175826)) ;
#98285 = CARTESIAN_POINT('Ctrl Pts',(-20.3552547779254,-12.4711564247202,
124.174170859642)) ;
#98286 = CARTESIAN_POINT('Ctrl Pts',(-20.355268658008,-12.4711574657611,124.17415363551)) ;
#98287 = CARTESIAN_POINT('Ctrl Pts',(-20.355296526524,-12.471159556028,124.174119050858)) ;
#98288 = CARTESIAN_POINT('Ctrl Pts',(-20.355310515176,-12.4711606052708,124.174101690051)) ;
#98289 = CARTESIAN_POINT('Ctrl Pts',(-20.3553386041898,-12.471162712195,124.174066827835)) ;
#98290 = CARTESIAN_POINT('Ctrl Pts',(-20.3553527039756,-12.4711637698335,
124.174049327124)) ;
#98291 = CARTESIAN_POINT('Ctrl Pts',(-20.3553810180061,-12.4711658937566,
124.174014181639)) ;
#98292 = CARTESIAN_POINT('Ctrl Pts',(-20.3553952325823,-12.4711669600666,
124.173996536438)) ;
#98293 = CARTESIAN_POINT('Ctrl Pts',(-20.3554237789685,-12.4711691015422,
124.173961098478)) ;
#98294 = CARTESIAN_POINT('Ctrl Pts',(-20.3554381111951,-12.4711701767397,
124.173943305185)) ;
#98295 = CARTESIAN_POINT('Ctrl Pts',(-20.355466896872,-12.4711723362912,124.173907566039)) ;
#98296 = CARTESIAN_POINT('Ctrl Pts',(-20.3554813494987,-12.471173420584,124.17388962119)) ;
#98297 = CARTESIAN_POINT('Ctrl Pts',(-20.35551037858,-12.4711755985232,124.173853575644)) ;
#98298 = CARTESIAN_POINT('Ctrl Pts',(-20.3555249558259,-12.4711766922295,
124.173835473947)) ;
#98299 = CARTESIAN_POINT('Ctrl Pts',(-20.3555542377408,-12.4711788892671,
124.173799110185)) ;
#98300 = CARTESIAN_POINT('Ctrl Pts',(-20.355568941973,-12.4711799925662,124.173780848644)) ;
#98301 = CARTESIAN_POINT('Ctrl Pts',(-20.3555984812218,-12.4711822090433,
124.173744160964)) ;
#98302 = CARTESIAN_POINT('Ctrl Pts',(-20.3556133164591,-12.4711833222384,
124.173725734531)) ;
#98303 = CARTESIAN_POINT('Ctrl Pts',(-20.3556431213415,-12.4711855587814,
124.173688712508)) ;
#98304 = CARTESIAN_POINT('Ctrl Pts',(-20.3556580906243,-12.4711866821026,
124.173670117347)) ;
#98305 = CARTESIAN_POINT('Ctrl Pts',(-20.3556881668883,-12.4711889391464,
124.17363275372)) ;
#98306 = CARTESIAN_POINT('Ctrl Pts',(-20.3557032741525,-12.4711900728909,
124.17361398488)) ;
#98307 = CARTESIAN_POINT('Ctrl Pts',(-20.3557336297761,-12.4711923510381,
124.173576269612)) ;
#98308 = CARTESIAN_POINT('Ctrl Pts',(-20.3557488784024,-12.4711934954615,
124.173557322829)) ;
#98309 = CARTESIAN_POINT('Ctrl Pts',(-20.3557795206565,-12.4711957952616,
124.173519246756)) ;
#98310 = CARTESIAN_POINT('Ctrl Pts',(-20.3557949141969,-12.4711969506325,
124.173500117552)) ;
#98311 = CARTESIAN_POINT('Ctrl Pts',(-20.3558258503679,-12.4711992726366,
124.173461671485)) ;
#98312 = CARTESIAN_POINT('Ctrl Pts',(-20.3558413925835,-12.4712004392394,
124.173442355116)) ;
#98313 = CARTESIAN_POINT('Ctrl Pts',(-20.3558726296969,-12.471202783979,124.173403530186)) ;
#98314 = CARTESIAN_POINT('Ctrl Pts',(-20.3558883247045,-12.4712039621248,
124.173384021464)) ;
#98315 = CARTESIAN_POINT('Ctrl Pts',(-20.3559198712665,-12.4712063302428,
124.173344806953)) ;
#98316 = CARTESIAN_POINT('Ctrl Pts',(-20.355935722734,-12.4712075202093,124.173325101247)) ;
#98317 = CARTESIAN_POINT('Ctrl Pts',(-20.3559675863237,-12.4712099122792,
124.173285487584)) ;
#98318 = CARTESIAN_POINT('Ctrl Pts',(-20.3559835982945,-12.4712111143721,
124.17326557979)) ;
#98319 = CARTESIAN_POINT('Ctrl Pts',(-20.3560157866571,-12.47121353098,124.173225557191)) ;
#98320 = CARTESIAN_POINT('Ctrl Pts',(-20.3560319634087,-12.471214745523,124.173205441913)) ;
#98321 = CARTESIAN_POINT('Ctrl Pts',(-20.3560644858298,-12.471217187371,124.173164998672)) ;
#98322 = CARTESIAN_POINT('Ctrl Pts',(-20.3560808311158,-12.4712184146482,
124.173144671159)) ;
#98323 = CARTESIAN_POINT('Ctrl Pts',(-20.3561136944813,-12.4712208822584,
124.173103798546)) ;
#98324 = CARTESIAN_POINT('Ctrl Pts',(-20.3561302131478,-12.4712221226364,
124.173083252687)) ;
#98325 = CARTESIAN_POINT('Ctrl Pts',(-20.3561634277567,-12.4712246167874,
124.173041937722)) ;
#98326 = CARTESIAN_POINT('Ctrl Pts',(-20.3561801236144,-12.4712258705549,
124.17302116869)) ;
#98327 = CARTESIAN_POINT('Ctrl Pts',(-20.356213697463,-12.4712283918525,124.172979401245)) ;
#98328 = CARTESIAN_POINT('Ctrl Pts',(-20.356230575119,-12.4712296593583,124.172958403218)) ;
#98329 = CARTESIAN_POINT('Ctrl Pts',(-20.3562645168589,-12.4712322084579,
124.172916172347)) ;
#98330 = CARTESIAN_POINT('Ctrl Pts',(-20.3562815811499,-12.4712334900681,
124.172894939213)) ;
#98331 = CARTESIAN_POINT('Ctrl Pts',(-20.3563159011198,-12.471236067752,124.172852231858)) ;
#98332 = CARTESIAN_POINT('Ctrl Pts',(-20.3563331562918,-12.4712373637885,
124.172830758236)) ;
#98333 = CARTESIAN_POINT('Ctrl Pts',(-20.3563678624985,-12.4712399706641,
124.172787564236)) ;
#98334 = CARTESIAN_POINT('Ctrl Pts',(-20.3563853138602,-12.4712412815287,
124.172765843418)) ;
#98335 = CARTESIAN_POINT('Ctrl Pts',(-20.3564204173901,-12.471243918435,124.172722148769)) ;
#98336 = CARTESIAN_POINT('Ctrl Pts',(-20.3564380693811,-12.4712452444645,
124.172700175123)) ;
#98337 = CARTESIAN_POINT('Ctrl Pts',(-20.3564735790337,-12.4712479120691,
124.172655968657)) ;
#98338 = CARTESIAN_POINT('Ctrl Pts',(-20.3564914370027,-12.4712492536684,
124.172633735416)) ;
#98339 = CARTESIAN_POINT('Ctrl Pts',(-20.3565273636917,-12.4712519527979,
124.172589003325)) ;
#98340 = CARTESIAN_POINT('Ctrl Pts',(-20.3565454325433,-12.471253310339,124.172566504271)) ;
#98341 = CARTESIAN_POINT('Ctrl Pts',(-20.3589199807141,-12.4714317204158,
124.16960953792)) ;
#98342 = CARTESIAN_POINT('Ctrl Pts',(-20.3612628174221,-12.4716085949351,
124.166664131738)) ;
#98343 = CARTESIAN_POINT('Ctrl Pts',(-20.3671474532601,-12.4720550570453,
124.15919501124)) ;
#98344 = CARTESIAN_POINT('Ctrl Pts',(-20.3706709242356,-12.4723244160414,
124.154656967092)) ;
#98345 = CARTESIAN_POINT('Ctrl Pts',(-20.3812328702558,-12.4731383198789,
124.140852703057)) ;
#98346 = CARTESIAN_POINT('Ctrl Pts',(-20.3881705460731,-12.4736817661882,
124.131510187451)) ;
#98347 = CARTESIAN_POINT('Ctrl Pts',(-20.4124692744817,-12.4756210993824,
124.09778710743)) ;
#98348 = CARTESIAN_POINT('Ctrl Pts',(-20.4290621858408,-12.4770157746858,
124.072866793059)) ;
#98349 = CARTESIAN_POINT('Ctrl Pts',(-20.4479786742128,-12.47871345024,124.042046547981)) ;
#98350 = CARTESIAN_POINT('Ctrl Pts',(-20.4511983629768,-12.479006421698,124.036709069825)) ;
#98351 = CARTESIAN_POINT('Ctrl Pts',(-20.4566649275737,-12.4795109141869,
124.027487080662)) ;
#98352 = CARTESIAN_POINT('Ctrl Pts',(-20.458931622599,-12.4797222578071,124.02361445814)) ;
#98353 = CARTESIAN_POINT('Ctrl Pts',(-20.4626494813691,-12.4800725258269,
124.017181048319)) ;
#98354 = CARTESIAN_POINT('Ctrl Pts',(-20.464112888515,-12.4802113461607,124.014627382422)) ;
#98355 = CARTESIAN_POINT('Ctrl Pts',(-20.4656712087533,-12.4803601949395,
124.011885039539)) ;
#98356 = CARTESIAN_POINT('Ctrl Pts',(-20.4657753698459,-12.480370149218,124.011701624935)) ;
#98357 = CARTESIAN_POINT('Ctrl Pts',(-20.465961253306,-12.4803879222204,124.011374108909)) ;
#98358 = CARTESIAN_POINT('Ctrl Pts',(-20.4660429940338,-12.4803957408042,
124.011230017775)) ;
#98359 = CARTESIAN_POINT('Ctrl Pts',(-20.4687126631504,-12.4806511971177,
124.006521727889)) ;
#98360 = CARTESIAN_POINT('Ctrl Pts',(-20.4712710217017,-12.4808990667218,
124.001940838803)) ;
#98361 = CARTESIAN_POINT('Ctrl Pts',(-20.4769285645691,-12.4814541312155,
123.991654720221)) ;
#98362 = CARTESIAN_POINT('Ctrl Pts',(-20.4800118496929,-12.4817614308663,
123.98594093322)) ;
#98363 = CARTESIAN_POINT('Ctrl Pts',(-20.4887378614946,-12.4826450168945,
123.969455495226)) ;
#98364 = CARTESIAN_POINT('Ctrl Pts',(-20.4942648579519,-12.4832219168617,
123.958623499026)) ;
#98365 = CARTESIAN_POINT('Ctrl Pts',(-20.5096861701031,-12.4848813326496,
123.927245459585)) ;
#98366 = CARTESIAN_POINT('Ctrl Pts',(-20.5191659592016,-12.4859634098913,
123.90650126362)) ;
#98367 = CARTESIAN_POINT('Ctrl Pts',(-20.5315533902526,-12.4874660051305,
123.877242649079)) ;
#98368 = CARTESIAN_POINT('Ctrl Pts',(-20.5349588417053,-12.4878897223978,
123.868944330591)) ;
#98369 = CARTESIAN_POINT('Ctrl Pts',(-20.5384461543587,-12.4883352844319,
123.860171156653)) ;
#98370 = CARTESIAN_POINT('Ctrl Pts',(-20.5386199588316,-12.4883575222693,
123.859733167528)) ;
#98371 = CARTESIAN_POINT('Ctrl Pts',(-20.5422086846914,-12.4888173420352,
123.850674170893)) ;
#98372 = CARTESIAN_POINT('Ctrl Pts',(-20.5455250585989,-12.4892544793688,
123.84201443296)) ;
#98373 = CARTESIAN_POINT('Ctrl Pts',(-20.5555639371481,-12.4906176754578,
123.814874548874)) ;
#98374 = CARTESIAN_POINT('Ctrl Pts',(-20.5619371309778,-12.4915423965759,
123.796268610423)) ;
#98375 = CARTESIAN_POINT('Ctrl Pts',(-20.5720126702342,-12.4931172498288,
123.76434643516)) ;
#98376 = CARTESIAN_POINT('Ctrl Pts',(-20.575944549847,-12.4937670767884,123.751106801031)) ;
#98377 = CARTESIAN_POINT('Ctrl Pts',(-20.5797816719757,-12.4944411531081,
123.737329765921)) ;
#98378 = CARTESIAN_POINT('Ctrl Pts',(-20.579913202447,-12.4944643111572,123.736856400244)) ;
#98379 = CARTESIAN_POINT('Ctrl Pts',(-20.5801756885541,-12.4945106299561,
123.73590951137)) ;
#98380 = CARTESIAN_POINT('Ctrl Pts',(-20.5803066441599,-12.4945337907003,
123.735435988289)) ;
#98381 = CARTESIAN_POINT('Ctrl Pts',(-20.5805805876458,-12.4945823497407,
123.734443090647)) ;
#98382 = CARTESIAN_POINT('Ctrl Pts',(-20.5807235173836,-12.4946077483214,
123.733923700183)) ;
#98383 = CARTESIAN_POINT('Ctrl Pts',(-20.5810409955255,-12.4946643047998,
123.732767013862)) ;
#98384 = CARTESIAN_POINT('Ctrl Pts',(-20.5812153695489,-12.4946954635898,
123.732129670354)) ;
#98385 = CARTESIAN_POINT('Ctrl Pts',(-20.5817020726261,-12.494782700274,123.730345034078)) ;
#98386 = CARTESIAN_POINT('Ctrl Pts',(-20.582013237394,-12.4948387843878,123.729197424899)) ;
#98387 = CARTESIAN_POINT('Ctrl Pts',(-20.5835709867667,-12.4951211300461,
123.72341870278)) ;
#98388 = CARTESIAN_POINT('Ctrl Pts',(-20.5847918230202,-12.4953475384408,
123.718780706059)) ;
#98389 = CARTESIAN_POINT('Ctrl Pts',(-20.5873079007107,-12.4958253324846,
123.70898683029)) ;
#98390 = CARTESIAN_POINT('Ctrl Pts',(-20.5885968264747,-12.4960767457725,
123.703829443226)) ;
#98391 = CARTESIAN_POINT('Ctrl Pts',(-20.5927162906557,-12.4969024215533,
123.686873880052)) ;
#98392 = CARTESIAN_POINT('Ctrl Pts',(-20.5954039491774,-12.4974771899123,
123.675041748772)) ;
#98393 = CARTESIAN_POINT('Ctrl Pts',(-20.6009471924391,-12.4987460813646,
123.648826245035)) ;
#98394 = CARTESIAN_POINT('Ctrl Pts',(-20.6037205275178,-12.499439984251,123.634427357988)) ;
#98395 = CARTESIAN_POINT('Ctrl Pts',(-20.6074314223375,-12.5004632174386,
123.613087728596)) ;
#98396 = CARTESIAN_POINT('Ctrl Pts',(-20.6085706932937,-12.500793496183,123.606183449859)) ;
#98397 = CARTESIAN_POINT('Ctrl Pts',(-20.6105443747699,-12.5013967436382,
123.593543570532)) ;
#98398 = CARTESIAN_POINT('Ctrl Pts',(-20.6113975110159,-12.5016698042016,
123.587811107432)) ;
#98399 = CARTESIAN_POINT('Ctrl Pts',(-20.6124424792685,-12.5020208908841,
123.580427174408)) ;
#98400 = CARTESIAN_POINT('Ctrl Pts',(-20.6126719828972,-12.5020991155729,
123.578781122948)) ;
#98401 = CARTESIAN_POINT('Ctrl Pts',(-20.6138609855392,-12.5025103404474,
123.570123475)) ;
#98402 = CARTESIAN_POINT('Ctrl Pts',(-20.6147625863996,-12.5028430272626,
123.563104053426)) ;
#98403 = CARTESIAN_POINT('Ctrl Pts',(-20.6182970355689,-12.5042413584114,
123.533544844975)) ;
#98404 = CARTESIAN_POINT('Ctrl Pts',(-20.6203594371846,-12.5053039619827,
123.510941489402)) ;
#98405 = CARTESIAN_POINT('Ctrl Pts',(-20.6228981539913,-12.507195194497,123.470681989344)) ;
#98406 = CARTESIAN_POINT('Ctrl Pts',(-20.6236248774207,-12.5080231963393,
123.453048333042)) ;
#98407 = CARTESIAN_POINT('Ctrl Pts',(-20.6241197122551,-12.5092228192452,
123.427548283734)) ;
#98408 = CARTESIAN_POINT('Ctrl Pts',(-20.6241959434941,-12.5095927908153,
123.419690126285)) ;
#98409 = CARTESIAN_POINT('Ctrl Pts',(-20.6241959212503,-12.51027943733,123.405121050766)) ;
#98410 = CARTESIAN_POINT('Ctrl Pts',(-20.6241403099179,-12.5105959927926,
123.39841043059)) ;
#98411 = CARTESIAN_POINT('Ctrl Pts',(-20.6238886040623,-12.5113131108826,
123.383223341157)) ;
#98412 = CARTESIAN_POINT('Ctrl Pts',(-20.6236593694167,-12.5117138192276,
123.37474777664)) ;
#98413 = CARTESIAN_POINT('Ctrl Pts',(-20.6229189955247,-12.5126478022625,
123.355017749913)) ;
#98414 = CARTESIAN_POINT('Ctrl Pts',(-20.6223399935886,-12.5131813158567,
123.343766618322)) ;
#98415 = CARTESIAN_POINT('Ctrl Pts',(-20.6198047194579,-12.5150216327641,
123.30501159315)) ;
#98416 = CARTESIAN_POINT('Ctrl Pts',(-20.6170687271845,-12.5163287249785,
123.277567089485)) ;
#98417 = CARTESIAN_POINT('Ctrl Pts',(-20.6121680245351,-12.518069963214,123.241049134321)) ;
#98418 = CARTESIAN_POINT('Ctrl Pts',(-20.6108295156638,-12.5185077431266,
123.231873265097)) ;
#98419 = CARTESIAN_POINT('Ctrl Pts',(-20.607848852321,-12.5194109506251,123.212958596754)) ;
#98420 = CARTESIAN_POINT('Ctrl Pts',(-20.6061927285498,-12.5198762910473,
123.203222682517)) ;
#98421 = CARTESIAN_POINT('Ctrl Pts',(-20.6022851852279,-12.5209001904488,
123.181832182804)) ;
#98422 = CARTESIAN_POINT('Ctrl Pts',(-20.5999812966991,-12.521458542291,123.170188213058)) ;
#98423 = CARTESIAN_POINT('Ctrl Pts',(-20.5937088871835,-12.5228738703402,
123.140758792795)) ;
#98424 = CARTESIAN_POINT('Ctrl Pts',(-20.5895101856481,-12.5237305022259,
123.123025480024)) ;
#98425 = CARTESIAN_POINT('Ctrl Pts',(-20.5835836105529,-12.5248379599899,
123.100288436061)) ;
#98426 = CARTESIAN_POINT('Ctrl Pts',(-20.5822197370061,-12.5250867851734,
123.09519222594)) ;
#98427 = CARTESIAN_POINT('Ctrl Pts',(-20.5796584355315,-12.525543455722,123.085865418251)) ;
#98428 = CARTESIAN_POINT('Ctrl Pts',(-20.5784711527048,-12.5257512314965,
123.08163213088)) ;
#98429 = CARTESIAN_POINT('Ctrl Pts',(-20.5715799597673,-12.5269351295508,
123.057564627679)) ;
#98430 = CARTESIAN_POINT('Ctrl Pts',(-20.5653974453407,-12.5279132636579,
123.037881356816)) ;
#98431 = CARTESIAN_POINT('Ctrl Pts',(-20.5587133983317,-12.5288903030033,
123.018355650104)) ;
#98432 = CARTESIAN_POINT('',(-19.5238357170928,-12.4073831970676,124.621346164163)) ;
#98433 = CARTESIAN_POINT('Origin',(-19.4092696390481,-12.4073831970673,123.411833654989)) ;
#98434 = CARTESIAN_POINT('Ctrl Pts',(-20.5587133983317,-12.510900730771,123.018355650104)) ;
#98435 = CARTESIAN_POINT('Ctrl Pts',(-20.5698769460786,-12.5092580324669,
123.050967054375)) ;
#98436 = CARTESIAN_POINT('Ctrl Pts',(-20.5796450054312,-12.5076065202731,
123.084029489636)) ;
#98437 = CARTESIAN_POINT('Ctrl Pts',(-20.5893204251238,-12.5057100112899,
123.122773296104)) ;
#98438 = CARTESIAN_POINT('Ctrl Pts',(-20.5906084555346,-12.5054508741779,
123.128083148678)) ;
#98439 = CARTESIAN_POINT('Ctrl Pts',(-20.5927031491089,-12.50501799702,123.13697998743)) ;
#98440 = CARTESIAN_POINT('Ctrl Pts',(-20.5935294256057,-12.5048440560172,
123.140562260687)) ;
#98441 = CARTESIAN_POINT('Ctrl Pts',(-20.5950192041835,-12.5045244561694,
123.147157657651)) ;
#98442 = CARTESIAN_POINT('Ctrl Pts',(-20.5956875120486,-12.5043787476725,
123.150169661514)) ;
#98443 = CARTESIAN_POINT('Ctrl Pts',(-20.5970019138047,-12.5040874073982,
123.156202123394)) ;
#98444 = CARTESIAN_POINT('Ctrl Pts',(-20.5976479767106,-12.503941776992,123.1592225644)) ;
#98445 = CARTESIAN_POINT('Ctrl Pts',(-20.5991300904758,-12.5036019006435,
123.166283203726)) ;
#98446 = CARTESIAN_POINT('Ctrl Pts',(-20.5999570941839,-12.5034077504466,
123.170325265217)) ;
#98447 = CARTESIAN_POINT('Ctrl Pts',(-20.6024955326435,-12.5027972228567,
123.183062172529)) ;
#98448 = CARTESIAN_POINT('Ctrl Pts',(-20.6041324410203,-12.5023815983093,
123.19177159524)) ;
#98449 = CARTESIAN_POINT('Ctrl Pts',(-20.6068167644363,-12.5016590619771,
123.206967984585)) ;
#98450 = CARTESIAN_POINT('Ctrl Pts',(-20.607907106845,-12.5013518421096,123.213446957826)) ;
#98451 = CARTESIAN_POINT('Ctrl Pts',(-20.6122753319681,-12.5000596648516,
123.240755314618)) ;
#98452 = CARTESIAN_POINT('Ctrl Pts',(-20.6150632124723,-12.499077132396,123.261659231297)) ;
#98453 = CARTESIAN_POINT('Ctrl Pts',(-20.618923089565,-12.4973789315367,123.297747217377)) ;
#98454 = CARTESIAN_POINT('Ctrl Pts',(-20.6202564033931,-12.4966658384734,
123.312898132013)) ;
#98455 = CARTESIAN_POINT('Ctrl Pts',(-20.6217476150328,-12.4956493481685,
123.334475523452)) ;
#98456 = CARTESIAN_POINT('Ctrl Pts',(-20.6221395131171,-12.4953473163249,
123.340884440706)) ;
#98457 = CARTESIAN_POINT('Ctrl Pts',(-20.6226249758822,-12.4949170342135,
123.350010432499)) ;
#98458 = CARTESIAN_POINT('Ctrl Pts',(-20.6227602544121,-12.4947890104071,
123.352725189758)) ;
#98459 = CARTESIAN_POINT('Ctrl Pts',(-20.6231885501644,-12.4943542494303,
123.361942368127)) ;
#98460 = CARTESIAN_POINT('Ctrl Pts',(-20.6234384216131,-12.4940472935097,
123.368446670845)) ;
#98461 = CARTESIAN_POINT('Ctrl Pts',(-20.6238988143281,-12.4933314741698,
123.38360584283)) ;
#98462 = CARTESIAN_POINT('Ctrl Pts',(-20.6240691186891,-12.4929224320628,
123.392261572861)) ;
#98463 = CARTESIAN_POINT('Ctrl Pts',(-20.6243549246725,-12.4914178901105,
123.42407191398)) ;
#98464 = CARTESIAN_POINT('Ctrl Pts',(-20.623901006214,-12.4903201671175,123.447226583789)) ;
#98465 = CARTESIAN_POINT('Ctrl Pts',(-20.6218509528039,-12.488300053935,123.489737826862)) ;
#98466 = CARTESIAN_POINT('Ctrl Pts',(-20.6204518896715,-12.4873783154767,
123.509096497463)) ;
#98467 = CARTESIAN_POINT('Ctrl Pts',(-20.6180870851889,-12.4862099225664,
123.533627402456)) ;
#98468 = CARTESIAN_POINT('Ctrl Pts',(-20.6175507293893,-12.4859617087126,
123.538838150508)) ;
#98469 = CARTESIAN_POINT('Ctrl Pts',(-20.6160644671224,-12.485314946828,123.552414683243)) ;
#98470 = CARTESIAN_POINT('Ctrl Pts',(-20.6150612664878,-12.4849166656924,
123.560774362998)) ;
#98471 = CARTESIAN_POINT('Ctrl Pts',(-20.6139344409102,-12.4845054432692,
123.569404883565)) ;
#98472 = CARTESIAN_POINT('Ctrl Pts',(-20.6138975332878,-12.4844920109284,
123.569686793507)) ;
#98473 = CARTESIAN_POINT('Ctrl Pts',(-20.6137955602058,-12.4844549991568,
123.57046357169)) ;
#98474 = CARTESIAN_POINT('Ctrl Pts',(-20.6137302887326,-12.4844314209153,
123.570958412883)) ;
#98475 = CARTESIAN_POINT('Ctrl Pts',(-20.6135484490314,-12.4843660446729,
123.572330468049)) ;
#98476 = CARTESIAN_POINT('Ctrl Pts',(-20.6134312272799,-12.4843242504778,
123.573207595281)) ;
#98477 = CARTESIAN_POINT('Ctrl Pts',(-20.613251798503,-12.4842608042561,123.574539113222)) ;
#98478 = CARTESIAN_POINT('Ctrl Pts',(-20.6131902923543,-12.4842391481303,
123.57499359789)) ;
#98479 = CARTESIAN_POINT('Ctrl Pts',(-20.6126734314331,-12.4840579339374,
123.578796610598)) ;
#98480 = CARTESIAN_POINT('Ctrl Pts',(-20.612204364305,-12.483898457602,123.582143263928)) ;
#98481 = CARTESIAN_POINT('Ctrl Pts',(-20.6109126507904,-12.4834722083572,
123.591087605764)) ;
#98482 = CARTESIAN_POINT('Ctrl Pts',(-20.6100648546541,-12.4832055931875,
123.596681584301)) ;
#98483 = CARTESIAN_POINT('Ctrl Pts',(-20.6081104497312,-12.4826185553911,
123.608996006905)) ;
#98484 = CARTESIAN_POINT('Ctrl Pts',(-20.6069863408637,-12.4822982505344,
123.615713484789)) ;
#98485 = CARTESIAN_POINT('Ctrl Pts',(-20.6022458286365,-12.4810133551369,
123.642648577744)) ;
#98486 = CARTESIAN_POINT('Ctrl Pts',(-20.5981734990602,-12.4800517565733,
123.662782528416)) ;
#98487 = CARTESIAN_POINT('Ctrl Pts',(-20.5875383784548,-12.477821955531,123.709265232995)) ;
#98488 = CARTESIAN_POINT('Ctrl Pts',(-20.5805988965207,-12.4765547800466,
123.735516421783)) ;
#98489 = CARTESIAN_POINT('Ctrl Pts',(-20.5696935074108,-12.4747805930788,
123.771802798001)) ;
#98490 = CARTESIAN_POINT('Ctrl Pts',(-20.5664647072722,-12.4742769787114,
123.782051038392)) ;
#98491 = CARTESIAN_POINT('Ctrl Pts',(-20.5610722049514,-12.4734684980667,
123.798406676697)) ;
#98492 = CARTESIAN_POINT('Ctrl Pts',(-20.5589948439257,-12.4731641453354,
123.804541949838)) ;
#98493 = CARTESIAN_POINT('Ctrl Pts',(-20.5567786485438,-12.4728465937101,
123.810918914261)) ;
#98494 = CARTESIAN_POINT('Ctrl Pts',(-20.5566886857919,-12.472833715193,123.811177494571)) ;
#98495 = CARTESIAN_POINT('Ctrl Pts',(-20.5565117746751,-12.4728084131445,
123.811685437615)) ;
#98496 = CARTESIAN_POINT('Ctrl Pts',(-20.5564248323812,-12.4727959896512,
123.811934802495)) ;
#98497 = CARTESIAN_POINT('Ctrl Pts',(-20.5562535444701,-12.4727715355344,
123.812425569757)) ;
#98498 = CARTESIAN_POINT('Ctrl Pts',(-20.5561692039284,-12.4727595049443,
123.812666973903)) ;
#98499 = CARTESIAN_POINT('Ctrl Pts',(-20.5560027274649,-12.4727357786899,
123.813142989299)) ;
#98500 = CARTESIAN_POINT('Ctrl Pts',(-20.5559205957442,-12.472724083054,123.813377602001)) ;
#98501 = CARTESIAN_POINT('Ctrl Pts',(-20.5557581652805,-12.4727009721211,
123.813841135212)) ;
#98502 = CARTESIAN_POINT('Ctrl Pts',(-20.5556778699715,-12.4726895568486,
123.814070056883)) ;
#98503 = CARTESIAN_POINT('Ctrl Pts',(-20.5555187561439,-12.4726669546537,
123.814523255246)) ;
#98504 = CARTESIAN_POINT('Ctrl Pts',(-20.5554399403437,-12.4726557677482,
123.814747532915)) ;
#98505 = CARTESIAN_POINT('Ctrl Pts',(-20.5552834397394,-12.4726335721361,
123.815192452374)) ;
#98506 = CARTESIAN_POINT('Ctrl Pts',(-20.5552057570363,-12.4726225634448,
123.815413094868)) ;
#98507 = CARTESIAN_POINT('Ctrl Pts',(-20.5550511823071,-12.47260067522,123.815851729641)) ;
#98508 = CARTESIAN_POINT('Ctrl Pts',(-20.5549742917813,-12.4725897956971,
123.816069722434)) ;
#98509 = CARTESIAN_POINT('Ctrl Pts',(-20.5548209613447,-12.4725681171193,
123.816504035308)) ;
#98510 = CARTESIAN_POINT('Ctrl Pts',(-20.5547445223555,-12.4725573180701,
123.816720355727)) ;
#98511 = CARTESIAN_POINT('Ctrl Pts',(-20.5545917495665,-12.4725357512968,
123.817152309343)) ;
#98512 = CARTESIAN_POINT('Ctrl Pts',(-20.5545154161457,-12.4725249835773,
123.817367942627)) ;
#98513 = CARTESIAN_POINT('Ctrl Pts',(-20.554362497669,-12.4725034290143,123.817799532525)) ;
#98514 = CARTESIAN_POINT('Ctrl Pts',(-20.554285912407,-12.4724926421697,123.818015489062)) ;
#98515 = CARTESIAN_POINT('Ctrl Pts',(-20.5541321149872,-12.4724709966191,
123.818448780714)) ;
#98516 = CARTESIAN_POINT('Ctrl Pts',(-20.554054902028,-12.4724601379084,123.818666115525)) ;
#98517 = CARTESIAN_POINT('Ctrl Pts',(-20.5538994474567,-12.4724382924862,
123.819103285869)) ;
#98518 = CARTESIAN_POINT('Ctrl Pts',(-20.5538212043756,-12.4724273057631,
123.819323120915)) ;
#98519 = CARTESIAN_POINT('Ctrl Pts',(-20.5521461312132,-12.472192276619,123.824025188155)) ;
#98520 = CARTESIAN_POINT('Ctrl Pts',(-20.5505230495355,-12.4719680572778,
123.828498015406)) ;
#98521 = CARTESIAN_POINT('Ctrl Pts',(-20.5470920447227,-12.4715012207749,
123.837782583323)) ;
#98522 = CARTESIAN_POINT('Ctrl Pts',(-20.545279776755,-12.4712585761245,123.842592616834)) ;
#98523 = CARTESIAN_POINT('Ctrl Pts',(-20.5412215841293,-12.4707236865552,
123.85315992767)) ;
#98524 = CARTESIAN_POINT('Ctrl Pts',(-20.5389621481497,-12.4704313438943,
123.858911857777)) ;
#98525 = CARTESIAN_POINT('Ctrl Pts',(-20.5294362088686,-12.4692207609637,
123.882629045141)) ;
#98526 = CARTESIAN_POINT('Ctrl Pts',(-20.5217843414093,-12.4682990128992,
123.900436219727)) ;
#98527 = CARTESIAN_POINT('Ctrl Pts',(-20.501165312954,-12.465940341664,123.945421666798)) ;
#98528 = CARTESIAN_POINT('Ctrl Pts',(-20.4876076525377,-12.4645028407755,
123.972315118446)) ;
#98529 = CARTESIAN_POINT('Ctrl Pts',(-20.4674710325589,-12.4625197033754,
124.008817597608)) ;
#98530 = CARTESIAN_POINT('Ctrl Pts',(-20.4617323304794,-12.461969598235,124.018877559604)) ;
#98531 = CARTESIAN_POINT('Ctrl Pts',(-20.4511654175284,-12.4609830805322,
124.036801005878)) ;
#98532 = CARTESIAN_POINT('Ctrl Pts',(-20.4463897992397,-12.460546332738,124.044694443315)) ;
#98533 = CARTESIAN_POINT('Ctrl Pts',(-20.4396673789375,-12.4599438014973,
124.055525194609)) ;
#98534 = CARTESIAN_POINT('Ctrl Pts',(-20.4377970254292,-12.4597774302075,
124.058509552236)) ;
#98535 = CARTESIAN_POINT('Ctrl Pts',(-20.43586201618,-12.459606596716,124.061567444051)) ;
#98536 = CARTESIAN_POINT('Ctrl Pts',(-20.4358103038864,-12.4596020322031,
124.061649143315)) ;
#98537 = CARTESIAN_POINT('Ctrl Pts',(-20.4357045907878,-12.4595927030947,
124.061816113306)) ;
#98538 = CARTESIAN_POINT('Ctrl Pts',(-20.4356505891068,-12.459587938506,124.061901383483)) ;
#98539 = CARTESIAN_POINT('Ctrl Pts',(-20.4355401935752,-12.4595782003562,
124.062075653092)) ;
#98540 = CARTESIAN_POINT('Ctrl Pts',(-20.4354837988351,-12.4595732268083,
124.06216465182)) ;
#98541 = CARTESIAN_POINT('Ctrl Pts',(-20.4353685091946,-12.4595630614947,
124.062346542538)) ;
#98542 = CARTESIAN_POINT('Ctrl Pts',(-20.4353096131754,-12.4595578697304,
124.062439433995)) ;
#98543 = CARTESIAN_POINT('Ctrl Pts',(-20.4351892083157,-12.4595472583566,
124.062629280868)) ;
#98544 = CARTESIAN_POINT('Ctrl Pts',(-20.4351276983703,-12.4595418387586,
124.062726235522)) ;
#98545 = CARTESIAN_POINT('Ctrl Pts',(-20.4350325013834,-12.4595334530627,
124.062876242143)) ;
#98546 = CARTESIAN_POINT('Ctrl Pts',(-20.4349988240092,-12.4595304868914,
124.062929300155)) ;
#98547 = CARTESIAN_POINT('Ctrl Pts',(-20.4349237604242,-12.4595238764662,
124.063047541014)) ;
#98548 = CARTESIAN_POINT('Ctrl Pts',(-20.4348823721598,-12.4595202322329,
124.06311272246)) ;
#98549 = CARTESIAN_POINT('Ctrl Pts',(-20.434790171371,-12.45951211529,124.063257896824)) ;
#98550 = CARTESIAN_POINT('Ctrl Pts',(-20.4347393556036,-12.4595076425972,
124.063337887895)) ;
#98551 = CARTESIAN_POINT('Ctrl Pts',(-20.4346262278446,-12.459497687339,124.063515920661)) ;
#98552 = CARTESIAN_POINT('Ctrl Pts',(-20.4345639112101,-12.4594922048166,
124.063613959273)) ;
#98553 = CARTESIAN_POINT('Ctrl Pts',(-20.4344252926012,-12.4594800123641,
124.063831969625)) ;
#98554 = CARTESIAN_POINT('Ctrl Pts',(-20.4343489836095,-12.4594733024885,
124.06395193694)) ;
#98555 = CARTESIAN_POINT('Ctrl Pts',(-20.4341794099958,-12.4594583963107,
124.064218424636)) ;
#98556 = CARTESIAN_POINT('Ctrl Pts',(-20.434086134991,-12.4594502000899,124.06436493845)) ;
#98557 = CARTESIAN_POINT('Ctrl Pts',(-20.4338791151946,-12.4594320156182,
124.064689965582)) ;
#98558 = CARTESIAN_POINT('Ctrl Pts',(-20.4337653551914,-12.4594220274922,
124.064868469141)) ;
#98559 = CARTESIAN_POINT('Ctrl Pts',(-20.4335419205685,-12.4594024187099,
124.065218863705)) ;
#98560 = CARTESIAN_POINT('Ctrl Pts',(-20.4334322492732,-12.4593927980233,
124.065390756915)) ;
#98561 = CARTESIAN_POINT('Ctrl Pts',(-20.4330079734983,-12.4593555953291,
124.066055376134)) ;
#98562 = CARTESIAN_POINT('Ctrl Pts',(-20.4326930566002,-12.4593280158204,
124.066547902769)) ;
#98563 = CARTESIAN_POINT('Ctrl Pts',(-20.4315225765269,-12.4592256346694,
124.068375612981)) ;
#98564 = CARTESIAN_POINT('Ctrl Pts',(-20.4306647559242,-12.459150851292,124.069709346894)) ;
#98565 = CARTESIAN_POINT('Ctrl Pts',(-20.4269897725468,-12.4588315326541,
124.075398673278)) ;
#98566 = CARTESIAN_POINT('Ctrl Pts',(-20.4241473359069,-12.4585872025776,
124.079737887864)) ;
#98567 = CARTESIAN_POINT('Ctrl Pts',(-20.4212162085802,-12.4583379011617,
124.084150580735)) ;
#98568 = CARTESIAN_POINT('Ctrl Pts',(-20.4211552135779,-12.4583327145097,
124.084242379123)) ;
#98569 = CARTESIAN_POINT('Ctrl Pts',(-20.4210325073564,-12.4583222826367,
124.084426999308)) ;
#98570 = CARTESIAN_POINT('Ctrl Pts',(-20.4209707958481,-12.4583170374177,
124.084519820923)) ;
#98571 = CARTESIAN_POINT('Ctrl Pts',(-20.4208465901858,-12.4583064828448,
124.084706585596)) ;
#98572 = CARTESIAN_POINT('Ctrl Pts',(-20.4207840957401,-12.4583011734954,
124.084800528408)) ;
#98573 = CARTESIAN_POINT('Ctrl Pts',(-20.4206582561405,-12.4582904849681,
124.084989635702)) ;
#98574 = CARTESIAN_POINT('Ctrl Pts',(-20.4205949106049,-12.4582851057899,
124.085084800005)) ;
#98575 = CARTESIAN_POINT('Ctrl Pts',(-20.4204672988626,-12.4582742717616,
124.085276453088)) ;
#98576 = CARTESIAN_POINT('Ctrl Pts',(-20.4204030322665,-12.4582688169138,
124.085372941627)) ;
#98577 = CARTESIAN_POINT('Ctrl Pts',(-20.4202735063263,-12.4582578255355,
124.085567348878)) ;
#98578 = CARTESIAN_POINT('Ctrl Pts',(-20.4202082465428,-12.4582522890065,
124.085665267344)) ;
#98579 = CARTESIAN_POINT('Ctrl Pts',(-20.4200766597832,-12.4582411280674,
124.085862643393)) ;
#98580 = CARTESIAN_POINT('Ctrl Pts',(-20.4200103323859,-12.4582355036639,
124.085962100619)) ;
#98581 = CARTESIAN_POINT('Ctrl Pts',(-20.4198765334075,-12.458224160575,124.086162666625)) ;
#98582 = CARTESIAN_POINT('Ctrl Pts',(-20.4198090613353,-12.4582184418941,
124.086263775064)) ;
#98583 = CARTESIAN_POINT('Ctrl Pts',(-20.4196728932111,-12.4582069036267,
124.086467759793)) ;
#98584 = CARTESIAN_POINT('Ctrl Pts',(-20.4196041965947,-12.4582010840425,
124.086570635757)) ;
#98585 = CARTESIAN_POINT('Ctrl Pts',(-20.4194654964649,-12.4581893370959,
124.086778276139)) ;
#98586 = CARTESIAN_POINT('Ctrl Pts',(-20.4193954923694,-12.4581834097388,
124.086883040155)) ;
#98587 = CARTESIAN_POINT('Ctrl Pts',(-20.4192540909941,-12.458171440105,124.087094581899)) ;
#98588 = CARTESIAN_POINT('Ctrl Pts',(-20.4191826931035,-12.4581653978358,
124.087201359157)) ;
#98589 = CARTESIAN_POINT('Ctrl Pts',(-20.4190384142349,-12.4581531909485,
124.087417057626)) ;
#98590 = CARTESIAN_POINT('Ctrl Pts',(-20.4189655325758,-12.458147026337,124.087525978354)) ;
#98591 = CARTESIAN_POINT('Ctrl Pts',(-20.4188181923908,-12.4581345670271,
124.087746099347)) ;
#98592 = CARTESIAN_POINT('Ctrl Pts',(-20.4187437330564,-12.4581282723298,
124.087857299192)) ;
#98593 = CARTESIAN_POINT('Ctrl Pts',(-20.4185931393808,-12.4581155447624,
124.088082120028)) ;
#98594 = CARTESIAN_POINT('Ctrl Pts',(-20.4185170042983,-12.4581091119049,
124.08819574036)) ;
#98595 = CARTESIAN_POINT('Ctrl Pts',(-20.4183629565049,-12.4580960995744,
124.088425549945)) ;
#98596 = CARTESIAN_POINT('Ctrl Pts',(-20.4182850428729,-12.4580895201053,
124.088541738656)) ;
#98597 = CARTESIAN_POINT('Ctrl Pts',(-20.4181273304388,-12.4580762057176,
124.088776839544)) ;
#98598 = CARTESIAN_POINT('Ctrl Pts',(-20.4180475306846,-12.4580694708073,
124.088895751062)) ;
#98599 = CARTESIAN_POINT('Ctrl Pts',(-20.4125436192329,-12.4576050873114,
124.09709412774)) ;
#98600 = CARTESIAN_POINT('Ctrl Pts',(-20.4070226345764,-12.4571482136181,
124.105108172067)) ;
#98601 = CARTESIAN_POINT('Ctrl Pts',(-20.393799664974,-12.4560741305029,124.123816939878)) ;
#98602 = CARTESIAN_POINT('Ctrl Pts',(-20.3860187590488,-12.4554575338095,
124.134454391518)) ;
#98603 = CARTESIAN_POINT('Ctrl Pts',(-20.3598565716444,-12.4534313825222,
124.169026508729)) ;
#98604 = CARTESIAN_POINT('Ctrl Pts',(-20.3407566767456,-12.4520259695336,
124.192402950134)) ;
#98605 = CARTESIAN_POINT('Ctrl Pts',(-20.3131223330305,-12.4500710252596,
124.223764250325)) ;
#98606 = CARTESIAN_POINT('Ctrl Pts',(-20.3053136172147,-12.449526590763,124.232373825256)) ;
#98607 = CARTESIAN_POINT('Ctrl Pts',(-20.2938895640292,-12.448739951032,124.244611949627)) ;
#98608 = CARTESIAN_POINT('Ctrl Pts',(-20.2903729134465,-12.4484991161708,
124.248331783656)) ;
#98609 = CARTESIAN_POINT('Ctrl Pts',(-20.2836115492218,-12.4480386297987,
124.255393858855)) ;
#98610 = CARTESIAN_POINT('Ctrl Pts',(-20.2803709128506,-12.4478190269787,
124.25873988595)) ;
#98611 = CARTESIAN_POINT('Ctrl Pts',(-20.2735750321903,-12.44736083512,124.265676506209)) ;
#98612 = CARTESIAN_POINT('Ctrl Pts',(-20.2700164674698,-12.4471222188575,
124.269263724662)) ;
#98613 = CARTESIAN_POINT('Ctrl Pts',(-20.2550484953945,-12.4461241063048,
124.284165131778)) ;
#98614 = CARTESIAN_POINT('Ctrl Pts',(-20.2434376101677,-12.445363224511,124.295274582443)) ;
#98615 = CARTESIAN_POINT('Ctrl Pts',(-20.2075906801642,-12.4430558602535,
124.328236472873)) ;
#98616 = CARTESIAN_POINT('Ctrl Pts',(-20.1826914080235,-12.4415093017599,
124.34934599734)) ;
#98617 = CARTESIAN_POINT('Ctrl Pts',(-20.1495833317207,-12.439524330996,124.375197253257)) ;
#98618 = CARTESIAN_POINT('Ctrl Pts',(-20.1421275219788,-12.4390817377921,
124.380881182336)) ;
#98619 = CARTESIAN_POINT('Ctrl Pts',(-20.122939380754,-12.437953566624,124.395161124986)) ;
#98620 = CARTESIAN_POINT('Ctrl Pts',(-20.1111171125251,-12.4372685533432,
124.40363380578)) ;
#98621 = CARTESIAN_POINT('Ctrl Pts',(-20.0754370279853,-12.4352276206579,
124.428247196113)) ;
#98622 = CARTESIAN_POINT('Ctrl Pts',(-20.0511544275459,-12.4338729410052,
124.443753899228)) ;
#98623 = CARTESIAN_POINT('Ctrl Pts',(-20.017449932026,-12.432028140645,124.463626994151)) ;
#98624 = CARTESIAN_POINT('Ctrl Pts',(-20.0084896013078,-12.4315410008158,
124.468757461644)) ;
#98625 = CARTESIAN_POINT('Ctrl Pts',(-19.9908708607762,-12.4305889549318,
124.478549450139)) ;
#98626 = CARTESIAN_POINT('Ctrl Pts',(-19.9822190922358,-12.4301241322034,
124.483221302814)) ;
#98627 = CARTESIAN_POINT('Ctrl Pts',(-19.9640769871351,-12.429154505061,124.492735219978)) ;
#98628 = CARTESIAN_POINT('Ctrl Pts',(-19.9545777531398,-12.4286495211339,
124.497558503084)) ;
#98629 = CARTESIAN_POINT('Ctrl Pts',(-19.9246493739527,-12.4270680105316,
124.512262922471)) ;
#98630 = CARTESIAN_POINT('Ctrl Pts',(-19.9040059234597,-12.4259914690301,
124.521697098471)) ;
#98631 = CARTESIAN_POINT('Ctrl Pts',(-19.8771487872796,-12.4246125299219,
124.533072663581)) ;
#98632 = CARTESIAN_POINT('Ctrl Pts',(-19.8711671633837,-12.4243067388453,
124.535550028959)) ;
#98633 = CARTESIAN_POINT('Ctrl Pts',(-19.8613224103786,-12.4238056211636,
124.539535469481)) ;
#98634 = CARTESIAN_POINT('Ctrl Pts',(-19.8574708649023,-12.4236101083685,
124.541071783872)) ;
#98635 = CARTESIAN_POINT('Ctrl Pts',(-19.8529605871501,-12.4233817766793,
124.542844144687)) ;
#98636 = CARTESIAN_POINT('Ctrl Pts',(-19.8523094297314,-12.423348827042,124.543099374926)) ;
#98637 = CARTESIAN_POINT('Ctrl Pts',(-19.8474053085878,-12.423100783311,124.545016730012)) ;
#98638 = CARTESIAN_POINT('Ctrl Pts',(-19.8431432185426,-12.4228858520485,
124.546655431128)) ;
#98639 = CARTESIAN_POINT('Ctrl Pts',(-19.8329268764751,-12.422372140158,124.550517472558)) ;
#98640 = CARTESIAN_POINT('Ctrl Pts',(-19.8269642132081,-12.4220735180171,
124.552718195285)) ;
#98641 = CARTESIAN_POINT('Ctrl Pts',(-19.8111239131671,-12.4212831871768,
124.558423767138)) ;
#98642 = CARTESIAN_POINT('Ctrl Pts',(-19.8012177165774,-12.4207919949184,
124.561847762981)) ;
#98643 = CARTESIAN_POINT('Ctrl Pts',(-19.7601338315114,-12.4187654878981,
124.575455553688)) ;
#98644 = CARTESIAN_POINT('Ctrl Pts',(-19.7285945839766,-12.4172340497047,
124.584502908679)) ;
#98645 = CARTESIAN_POINT('Ctrl Pts',(-19.6901537693317,-12.415374745288,124.593864020183)) ;
#98646 = CARTESIAN_POINT('Ctrl Pts',(-19.6835663524498,-12.4150564282802,
124.595410011397)) ;
#98647 = CARTESIAN_POINT('Ctrl Pts',(-19.672063914205,-12.4145010061238,124.598008315653)) ;
#98648 = CARTESIAN_POINT('Ctrl Pts',(-19.6671546330432,-12.4142640765089,
124.599085307476)) ;
#98649 = CARTESIAN_POINT('Ctrl Pts',(-19.6574487837096,-12.413795868214,124.601151523565)) ;
#98650 = CARTESIAN_POINT('Ctrl Pts',(-19.6526526352281,-12.4135646044212,
124.60214226932)) ;
#98651 = CARTESIAN_POINT('Ctrl Pts',(-19.6420636834182,-12.413054222158,124.604262965701)) ;
#98652 = CARTESIAN_POINT('Ctrl Pts',(-19.6362683752166,-12.4127750240252,
124.605379758676)) ;
#98653 = CARTESIAN_POINT('Ctrl Pts',(-19.5951593428287,-12.4107954678892,
124.612991492592)) ;
#98654 = CARTESIAN_POINT('Ctrl Pts',(-19.5595812733024,-12.4090859603097,
124.617960313953)) ;
#98655 = CARTESIAN_POINT('Ctrl Pts',(-19.5238357170927,-12.4073831970678,
124.621346164163)) ;
#98656 = CARTESIAN_POINT('Origin',(-19.4092696390481,-12.3398872919312,123.411833654989)) ;
#98657 = CARTESIAN_POINT('',(-19.7583036208567,-12.0999018514474,122.923846357696)) ;
#98658 = CARTESIAN_POINT('Origin',(-19.4092696390481,-12.0999018514474,123.411833654989)) ;
#98659 = CARTESIAN_POINT('',(-19.4092696390481,-12.3998836520522,123.411833654989)) ;
#98660 = CARTESIAN_POINT('',(-19.4790764354098,-12.3398872919312,123.314236195531)) ;
#98661 = CARTESIAN_POINT('Origin',(-19.4092696390481,-11.9199127710845,123.411833654989)) ;
#98662 = CARTESIAN_POINT('',(-20.1895953175517,-12.4705811104891,122.32085388287)) ;
#98663 = CARTESIAN_POINT('',(-19.5488832317715,-11.9199127710845,123.216638736072)) ;
#98664 = CARTESIAN_POINT('Ctrl Pts',(-19.5238357170906,-12.4073831970675,
124.621346164163)) ;
#98665 = CARTESIAN_POINT('Ctrl Pts',(-19.5962324284842,-12.4089443847789,
124.61762503581)) ;
#98666 = CARTESIAN_POINT('Ctrl Pts',(-19.6679519600925,-12.4104965535015,
124.607473895949)) ;
#98667 = CARTESIAN_POINT('Ctrl Pts',(-19.8093655444423,-12.4135619883255,
124.574339807829)) ;
#98668 = CARTESIAN_POINT('Ctrl Pts',(-19.878741257865,-12.415095859395,124.551406258254)) ;
#98669 = CARTESIAN_POINT('Ctrl Pts',(-20.0813588019352,-12.4197782665645,
124.46400772854)) ;
#98670 = CARTESIAN_POINT('Ctrl Pts',(-20.2057814700574,-12.4228609961199,
124.381074213256)) ;
#98671 = CARTESIAN_POINT('Ctrl Pts',(-20.3710577753689,-12.4276127977452,
124.222765293075)) ;
#98672 = CARTESIAN_POINT('Ctrl Pts',(-20.4243166090151,-12.4292659064182,
124.160569795075)) ;
#98673 = CARTESIAN_POINT('Ctrl Pts',(-20.5181725089382,-12.4326333165008,
124.026919412824)) ;
#98674 = CARTESIAN_POINT('Ctrl Pts',(-20.5587677064569,-12.4343499486542,
123.955322064525)) ;
#98675 = CARTESIAN_POINT('Ctrl Pts',(-20.6259284021624,-12.4377451727854,
123.804205715492)) ;
#98676 = CARTESIAN_POINT('Ctrl Pts',(-20.6521167329554,-12.4394104855471,
123.724954628002)) ;
#98677 = CARTESIAN_POINT('Ctrl Pts',(-20.6887992598423,-12.4427709330836,
123.562622945221)) ;
#98678 = CARTESIAN_POINT('Ctrl Pts',(-20.6992800173493,-12.4444740645654,
123.479692662602)) ;
#98679 = CARTESIAN_POINT('Ctrl Pts',(-20.7040628297017,-12.4478688624783,
123.311618284165)) ;
#98680 = CARTESIAN_POINT('Ctrl Pts',(-20.698059256379,-12.4495305257553,123.227027212024)) ;
#98681 = CARTESIAN_POINT('Ctrl Pts',(-20.6698162203938,-12.452910900607,123.060015655013)) ;
#98682 = CARTESIAN_POINT('Ctrl Pts',(-20.6475775884725,-12.4546483109235,
122.977657011261)) ;
#98683 = CARTESIAN_POINT('Ctrl Pts',(-20.5872478367947,-12.4580007720277,
122.818668580782)) ;
#98684 = CARTESIAN_POINT('Ctrl Pts',(-20.5492675453858,-12.4596416636238,
122.742149856431)) ;
#98685 = CARTESIAN_POINT('Ctrl Pts',(-20.4588032040082,-12.4630480670111,
122.596363457829)) ;
#98686 = CARTESIAN_POINT('Ctrl Pts',(-20.4059643471343,-12.4647476001311,
122.527466647333)) ;
#98687 = CARTESIAN_POINT('Ctrl Pts',(-20.2982554730135,-12.4678125093508,
122.4123130576)) ;
#98688 = CARTESIAN_POINT('Ctrl Pts',(-20.2456600338429,-12.4692000007384,
122.364350348791)) ;
#98689 = CARTESIAN_POINT('Ctrl Pts',(-20.1895953242298,-12.4705811104891,
122.320853887647)) ;
#98690 = CARTESIAN_POINT('',(-18.4227818193872,-12.5498512937297,124.541625342821)) ;
#98691 = CARTESIAN_POINT('Ctrl Pts',(-18.4227818193872,-12.5498512937297,
124.541625342821)) ;
#98692 = CARTESIAN_POINT('Ctrl Pts',(-18.523921374435,-12.5305321283799,124.578641685623)) ;
#98693 = CARTESIAN_POINT('Ctrl Pts',(-18.6455674693221,-12.5080679368029,
124.611133209733)) ;
#98694 = CARTESIAN_POINT('Ctrl Pts',(-18.8434953872101,-12.4694919241786,
124.626965465885)) ;
#98695 = CARTESIAN_POINT('Ctrl Pts',(-18.9055194053882,-12.4570505014027,
124.627023882188)) ;
#98696 = CARTESIAN_POINT('Ctrl Pts',(-19.0259931889205,-12.4324340735925,
124.618609684159)) ;
#98697 = CARTESIAN_POINT('Ctrl Pts',(-19.0864413674558,-12.4199510743861,
124.610350106817)) ;
#98698 = CARTESIAN_POINT('Ctrl Pts',(-19.1445267022232,-12.4073898409303,
124.597577877357)) ;
#98699 = CARTESIAN_POINT('Ctrl Pts',(-20.1895953242298,-12.4705811104891,
122.320853887647)) ;
#98700 = CARTESIAN_POINT('Ctrl Pts',(-20.1773671163109,-12.4708823427136,
122.31136692563)) ;
#98701 = CARTESIAN_POINT('Ctrl Pts',(-20.1649739999333,-12.4711830202549,
122.302092254234)) ;
#98702 = CARTESIAN_POINT('Ctrl Pts',(-20.0815320001337,-12.4731748557987,
122.241884004884)) ;
#98703 = CARTESIAN_POINT('Ctrl Pts',(-20.0056947472065,-12.4748348374862,
122.197775741839)) ;
#98704 = CARTESIAN_POINT('Ctrl Pts',(-19.8462866625701,-12.4782125473853,
122.12455639128)) ;
#98705 = CARTESIAN_POINT('Ctrl Pts',(-19.7626979246505,-12.4799263147623,
122.095588188368)) ;
#98706 = CARTESIAN_POINT('Ctrl Pts',(-19.5904912703646,-12.4833084828718,
122.054218582603)) ;
#98707 = CARTESIAN_POINT('Ctrl Pts',(-19.50223016541,-12.4849766794126,122.042003974107)) ;
#98708 = CARTESIAN_POINT('Ctrl Pts',(-19.3687946089318,-12.4875069623851,
122.036526751585)) ;
#98709 = CARTESIAN_POINT('Ctrl Pts',(-19.3239430277806,-12.4883579509319,
122.036875236449)) ;
#98710 = CARTESIAN_POINT('Ctrl Pts',(-19.1898575173771,-12.4908935345291,
122.044487847896)) ;
#98711 = CARTESIAN_POINT('Ctrl Pts',(-19.1010237275889,-12.4925610112359,
122.058345540396)) ;
#98712 = CARTESIAN_POINT('Ctrl Pts',(-18.927465445027,-12.4959478846101,122.10272424865)) ;
#98713 = CARTESIAN_POINT('Ctrl Pts',(-18.8430397577009,-12.4976141777241,
122.133326264349)) ;
#98714 = CARTESIAN_POINT('Ctrl Pts',(-18.6785559071882,-12.5009671960115,
122.211661837729)) ;
#98715 = CARTESIAN_POINT('Ctrl Pts',(-18.5989299359681,-12.5027045657308,
122.259661569629)) ;
#98716 = CARTESIAN_POINT('Ctrl Pts',(-18.4525004431847,-12.5061073744163,
122.368980228931)) ;
#98717 = CARTESIAN_POINT('Ctrl Pts',(-18.3857906860324,-12.507727171673,122.429696850446)) ;
#98718 = CARTESIAN_POINT('Ctrl Pts',(-18.2617407828677,-12.5110837575642,
122.566225042383)) ;
#98719 = CARTESIAN_POINT('Ctrl Pts',(-18.2049741722999,-12.5128703471317,
122.642533598537)) ;
#98720 = CARTESIAN_POINT('Ctrl Pts',(-18.1094497652685,-12.5162623626902,
122.802392995369)) ;
#98721 = CARTESIAN_POINT('Ctrl Pts',(-18.0702566535678,-12.5178649946102,
122.885427595447)) ;
#98722 = CARTESIAN_POINT('Ctrl Pts',(-18.0069266678437,-12.5212444282736,
123.060192718302)) ;
#98723 = CARTESIAN_POINT('Ctrl Pts',(-17.9834963365382,-12.5229822629239,
123.152105302265)) ;
#98724 = CARTESIAN_POINT('Ctrl Pts',(-17.9551578642983,-12.5263554079533,
123.339243986634)) ;
#98725 = CARTESIAN_POINT('Ctrl Pts',(-17.9501721908057,-12.5280313344139,
123.433934396647)) ;
#98726 = CARTESIAN_POINT('Ctrl Pts',(-17.9626538167798,-12.533138571593,123.71840359676)) ;
#98727 = CARTESIAN_POINT('Ctrl Pts',(-18.0082890864271,-12.5364847742368,
123.905274766927)) ;
#98728 = CARTESIAN_POINT('Ctrl Pts',(-18.1279903364265,-12.5414807225745,
124.164911073218)) ;
#98729 = CARTESIAN_POINT('Ctrl Pts',(-18.176617440371,-12.5431677444753,124.248138628516)) ;
#98730 = CARTESIAN_POINT('Ctrl Pts',(-18.2890126007803,-12.5465526000103,
124.403858752384)) ;
#98731 = CARTESIAN_POINT('Ctrl Pts',(-18.3526450100352,-12.5481950593457,
124.475987264072)) ;
#98732 = CARTESIAN_POINT('Ctrl Pts',(-18.4227818193873,-12.5498512937297,
124.541625342821)) ;
#98733 = CARTESIAN_POINT('Ctrl Pts',(-18.2740165434593,-11.9799091312055,
123.800453906728)) ;
#98734 = CARTESIAN_POINT('Ctrl Pts',(-18.3189584392777,-11.9865359820236,
123.931788685072)) ;
#98735 = CARTESIAN_POINT('Ctrl Pts',(-18.4545056203785,-11.9997666085046,
124.178258720661)) ;
#98736 = CARTESIAN_POINT('Ctrl Pts',(-18.7737315341766,-12.0197422297632,
124.458465138621)) ;
#98737 = CARTESIAN_POINT('Ctrl Pts',(-19.1683573427766,-12.0396595646652,
124.612093184928)) ;
#98738 = CARTESIAN_POINT('Ctrl Pts',(-19.5908277766353,-12.0595328413812,
124.622778366067)) ;
#98739 = CARTESIAN_POINT('Ctrl Pts',(-19.9944642973842,-12.0795573315451,
124.48737361252)) ;
#98740 = CARTESIAN_POINT('Ctrl Pts',(-20.3250783272367,-12.0994251726959,
124.224300972963)) ;
#98741 = CARTESIAN_POINT('Ctrl Pts',(-20.5474460981866,-12.1193708235754,
123.863226295649)) ;
#98742 = CARTESIAN_POINT('Ctrl Pts',(-20.6329261309455,-12.1392762241924,
123.448705492107)) ;
#98743 = CARTESIAN_POINT('Ctrl Pts',(-20.5727438962401,-12.1591504520087,
123.030430647925)) ;
#98744 = CARTESIAN_POINT('Ctrl Pts',(-20.3723428413833,-12.1791362428864,
122.655687392966)) ;
#98745 = CARTESIAN_POINT('Ctrl Pts',(-20.0574084503166,-12.1990304855461,
122.373329473787)) ;
#98746 = CARTESIAN_POINT('Ctrl Pts',(-19.6656738070417,-12.2189092016182,
122.214453028879)) ;
#98747 = CARTESIAN_POINT('Ctrl Pts',(-19.239903745311,-12.2389486514628,122.19917989261)) ;
#98748 = CARTESIAN_POINT('Ctrl Pts',(-18.8378746103373,-12.2588118130006,
122.329001366094)) ;
#98749 = CARTESIAN_POINT('Ctrl Pts',(-18.5023851900328,-12.2787911810149,
122.589387311488)) ;
#98750 = CARTESIAN_POINT('Ctrl Pts',(-18.2772973920916,-12.2986017615377,
122.945534607748)) ;
#98751 = CARTESIAN_POINT('Ctrl Pts',(-18.1859011753708,-12.3185826898233,
123.360352214875)) ;
#98752 = CARTESIAN_POINT('Ctrl Pts',(-18.2415933923227,-12.3384753616927,
123.779690524285)) ;
#98753 = CARTESIAN_POINT('Ctrl Pts',(-18.4366948614835,-12.3584016919798,
124.155782344013)) ;
#98754 = CARTESIAN_POINT('Ctrl Pts',(-18.7493815278539,-12.3783722460721,
124.443073249867)) ;
#98755 = CARTESIAN_POINT('Ctrl Pts',(-19.0736806414741,-12.3949040851597,
124.578622091975)) ;
#98756 = CARTESIAN_POINT('Ctrl Pts',(-19.3515878511827,-12.4082438239873,
124.616550891535)) ;
#98757 = CARTESIAN_POINT('Ctrl Pts',(-19.5623143731514,-12.4182760662059,
124.608028982489)) ;
#98758 = CARTESIAN_POINT('Ctrl Pts',(-19.7648627207614,-12.4281337668493,
124.564138701125)) ;
#98759 = CARTESIAN_POINT('Ctrl Pts',(-19.9594468747988,-12.4381256314886,
124.485041805288)) ;
#98760 = CARTESIAN_POINT('Ctrl Pts',(-20.1360963170606,-12.4480481812487,
124.374088363487)) ;
#98761 = CARTESIAN_POINT('Ctrl Pts',(-20.343597806423,-12.4613259547422,124.187361881646)) ;
#98762 = CARTESIAN_POINT('Ctrl Pts',(-20.4979415790558,-12.4746732936828,
123.949247000731)) ;
#98763 = CARTESIAN_POINT('Ctrl Pts',(-20.5838258599568,-12.487880525476,123.685145402898)) ;
#98764 = CARTESIAN_POINT('Ctrl Pts',(-20.6134813220022,-12.4978676415657,
123.477327143621)) ;
#98765 = CARTESIAN_POINT('Ctrl Pts',(-20.6067609199625,-12.5078185471454,
123.268195479492)) ;
#98766 = CARTESIAN_POINT('Ctrl Pts',(-20.5631573577601,-12.5178736491529,
123.061381748979)) ;
#98767 = CARTESIAN_POINT('Ctrl Pts',(-20.4864536514248,-12.527695322474,122.869648827725)) ;
#98768 = CARTESIAN_POINT('Ctrl Pts',(-20.3753205327506,-12.5377537935489,
122.689772542766)) ;
#98769 = CARTESIAN_POINT('Ctrl Pts',(-20.2362754807728,-12.5476784047254,
122.534182107646)) ;
#98770 = CARTESIAN_POINT('Ctrl Pts',(-20.0174292748724,-12.5609557436258,
122.360945081816)) ;
#98771 = CARTESIAN_POINT('Ctrl Pts',(-19.7578510281524,-12.5742546228634,
122.248867980768)) ;
#98772 = CARTESIAN_POINT('Ctrl Pts',(-19.4824869521696,-12.5874934950341,
122.208104909407)) ;
#98773 = CARTESIAN_POINT('Ctrl Pts',(-19.2721842153981,-12.5975001131707,
122.21353782758)) ;
#98774 = CARTESIAN_POINT('Ctrl Pts',(-19.0656057276748,-12.6075310582322,
122.255904223279)) ;
#98775 = CARTESIAN_POINT('Ctrl Pts',(-18.8727802949704,-12.617387231584,122.331796225653)) ;
#98776 = CARTESIAN_POINT('Ctrl Pts',(-18.6933999328504,-12.6273865025469,
122.441334289296)) ;
#98777 = CARTESIAN_POINT('Ctrl Pts',(-18.5371999064352,-12.6372809543042,
122.578764112647)) ;
#98778 = CARTESIAN_POINT('Ctrl Pts',(-18.4051179275359,-12.6473442701136,
122.743982938966)) ;
#98779 = CARTESIAN_POINT('Ctrl Pts',(-18.3057447547748,-12.6571831268532,
122.925434057123)) ;
#98780 = CARTESIAN_POINT('Ctrl Pts',(-18.2376547087134,-12.6672492486708,
123.125766673325)) ;
#98781 = CARTESIAN_POINT('Ctrl Pts',(-18.206055983078,-12.677132476395,123.331154376031)) ;
#98782 = CARTESIAN_POINT('Ctrl Pts',(-18.2101872557623,-12.6871219376738,
123.541102632634)) ;
#98783 = CARTESIAN_POINT('Ctrl Pts',(-18.2506856928927,-12.6970856481003,
123.74662922549)) ;
#98784 = CARTESIAN_POINT('Ctrl Pts',(-18.3262879795565,-12.7070806508312,
123.942700671826)) ;
#98785 = CARTESIAN_POINT('Ctrl Pts',(-18.4355049039603,-12.7171169818415,
124.123217317546)) ;
#98786 = CARTESIAN_POINT('Ctrl Pts',(-18.5715338638784,-12.7269632111838,
124.27926193741)) ;
#98787 = CARTESIAN_POINT('Ctrl Pts',(-18.7345869209909,-12.736948709459,124.411432149983)) ;
#98788 = CARTESIAN_POINT('Ctrl Pts',(-18.9171714469055,-12.746883612442,124.512934464709)) ;
#98789 = CARTESIAN_POINT('Ctrl Pts',(-19.1170398133317,-12.7569411155372,
124.581832628825)) ;
#98790 = CARTESIAN_POINT('Ctrl Pts',(-19.3209400838913,-12.7667627719077,
124.614524423763)) ;
#98791 = CARTESIAN_POINT('Ctrl Pts',(-19.5323133855585,-12.7768188345729,
124.611634485292)) ;
#98792 = CARTESIAN_POINT('Ctrl Pts',(-19.7375456372687,-12.7867594992761,
124.572166329011)) ;
#98793 = CARTESIAN_POINT('Ctrl Pts',(-19.93232144883,-12.7966639032246,124.498546479799)) ;
#98794 = CARTESIAN_POINT('Ctrl Pts',(-20.1138409022028,-12.8067103882181,
124.390597508332)) ;
#98795 = CARTESIAN_POINT('Ctrl Pts',(-20.2716172669119,-12.8166066160299,
124.2549368052)) ;
#98796 = CARTESIAN_POINT('Ctrl Pts',(-20.4056121615744,-12.8266661995934,
124.091347649612)) ;
#98797 = CARTESIAN_POINT('Ctrl Pts',(-20.5070661434651,-12.8365182092622,
123.910765827753)) ;
#98798 = CARTESIAN_POINT('Ctrl Pts',(-20.5770507746877,-12.8464807407018,
123.713371088349)) ;
#98799 = CARTESIAN_POINT('Ctrl Pts',(-20.6116193303451,-12.8565122889411,
123.505321757984)) ;
#98800 = CARTESIAN_POINT('Ctrl Pts',(-20.6097667692632,-12.8664037001542,
123.297381634971)) ;
#98801 = CARTESIAN_POINT('Ctrl Pts',(-20.5717313898556,-12.8764199538622,
123.090264177676)) ;
#98802 = CARTESIAN_POINT('Ctrl Pts',(-20.4977853648253,-12.8864500567069,
122.89279425975)) ;
#98803 = CARTESIAN_POINT('Ctrl Pts',(-20.3928637151754,-12.8963065056606,
122.714092804995)) ;
#98804 = CARTESIAN_POINT('Ctrl Pts',(-20.2567958143652,-12.9063055164329,
122.553905485734)) ;
#98805 = CARTESIAN_POINT('Ctrl Pts',(-20.0967563316711,-12.9162007333509,
122.420949578462)) ;
#98806 = CARTESIAN_POINT('Ctrl Pts',(-19.9130848769324,-12.9262612487082,
122.316129324988)) ;
#98807 = CARTESIAN_POINT('Ctrl Pts',(-19.7181830252173,-12.9361105420953,
122.246165871294)) ;
#98808 = CARTESIAN_POINT('Ctrl Pts',(-19.5105194500095,-12.9461377177753,
122.209950448507)) ;
#98809 = CARTESIAN_POINT('Ctrl Pts',(-19.299679000414,-12.9561662934024,122.210897337973)) ;
#98810 = CARTESIAN_POINT('Ctrl Pts',(-19.0959517297678,-12.9660113869483,
122.24735852657)) ;
#98811 = CARTESIAN_POINT('Ctrl Pts',(-18.8985634625517,-12.9760026283801,
122.319182831211)) ;
#98812 = CARTESIAN_POINT('Ctrl Pts',(-18.7160505191915,-12.9860384095234,
122.425038812806)) ;
#98813 = CARTESIAN_POINT('Ctrl Pts',(-18.5574736215449,-12.9958906152531,
122.558270842358)) ;
#98814 = CARTESIAN_POINT('Ctrl Pts',(-18.4224851135183,-13.0058527093701,
122.718394045707)) ;
#98815 = CARTESIAN_POINT('Ctrl Pts',(-18.3169324702331,-13.0158752701972,
122.900755197435)) ;
#98816 = CARTESIAN_POINT('Ctrl Pts',(-18.2451304645408,-13.0258030418487,
123.096749192298)) ;
#98817 = CARTESIAN_POINT('Ctrl Pts',(-18.2080549192017,-13.0358454259736,
123.304574979866)) ;
#98818 = CARTESIAN_POINT('Ctrl Pts',(-18.2075488204936,-13.0457346500442,
123.512488897481)) ;
#98819 = CARTESIAN_POINT('Ctrl Pts',(-18.2431194310782,-13.0557238982115,
123.71945288329)) ;
#98820 = CARTESIAN_POINT('Ctrl Pts',(-18.3140184178644,-13.0656824752535,
123.916437204)) ;
#98821 = CARTESIAN_POINT('Ctrl Pts',(-18.4169896551576,-13.0755820443448,
124.097312993024)) ;
#98822 = CARTESIAN_POINT('Ctrl Pts',(-18.5518287332227,-13.0856299564288,
124.259889547526)) ;
#98823 = CARTESIAN_POINT('Ctrl Pts',(-18.7103385128651,-13.095525310736,124.394667774035)) ;
#98824 = CARTESIAN_POINT('Ctrl Pts',(-18.8927954186044,-13.1055869612272,
124.501642284912)) ;
#98825 = CARTESIAN_POINT('Ctrl Pts',(-19.0867950664044,-13.1154315766896,
124.57376207888)) ;
#98826 = CARTESIAN_POINT('Ctrl Pts',(-19.2926111071582,-13.125391655591,124.612276634278)) ;
#98827 = CARTESIAN_POINT('Ctrl Pts',(-19.5036297409115,-13.1354298499494,
124.614075936602)) ;
#98828 = CARTESIAN_POINT('Ctrl Pts',(-19.7084424494727,-13.145303565349,124.580155177337)) ;
#98829 = CARTESIAN_POINT('Ctrl Pts',(-19.9081211365426,-13.1553752748833,
124.509801884541)) ;
#98830 = CARTESIAN_POINT('Ctrl Pts',(-20.0882669718417,-13.1652077153358,
124.408397803474)) ;
#98831 = CARTESIAN_POINT('Ctrl Pts',(-20.251665867001,-13.1752395362612,124.275064613203)) ;
#98832 = CARTESIAN_POINT('Ctrl Pts',(-20.3888240086769,-13.1852599061468,
124.115169869146)) ;
#98833 = CARTESIAN_POINT('Ctrl Pts',(-20.4949634505062,-13.1951266772805,
123.936935074863)) ;
#98834 = CARTESIAN_POINT('Ctrl Pts',(-20.5700454180125,-13.2051974484699,
123.73899843199)) ;
#98835 = CARTESIAN_POINT('Ctrl Pts',(-20.6087537229639,-13.2150406089915,
123.535705448998)) ;
#98836 = CARTESIAN_POINT('Ctrl Pts',(-20.6123036162393,-13.2250208421779,
123.325926400063)) ;
#98837 = CARTESIAN_POINT('Ctrl Pts',(-20.5788478949797,-13.2350393622131,
123.117985154536)) ;
#98838 = CARTESIAN_POINT('Ctrl Pts',(-20.5111351253768,-13.2449226705968,
122.921523560764)) ;
#98839 = CARTESIAN_POINT('Ctrl Pts',(-20.4084000500647,-13.2549909547676,
122.736499705286)) ;
#98840 = CARTESIAN_POINT('Ctrl Pts',(-20.2783984194009,-13.2648210814352,
122.57580630881)) ;
#98841 = CARTESIAN_POINT('Ctrl Pts',(-20.1189511854657,-13.2748876536418,
122.436701963552)) ;
#98842 = CARTESIAN_POINT('Ctrl Pts',(-19.9408318283433,-13.2847778098825,
122.329389675604)) ;
#98843 = CARTESIAN_POINT('Ctrl Pts',(-19.7449774449838,-13.2947703374589,
122.253452034578)) ;
#98844 = CARTESIAN_POINT('Ctrl Pts',(-19.5395052216676,-13.3047318273332,
122.212975244473)) ;
#98845 = CARTESIAN_POINT('Ctrl Pts',(-19.3312252373972,-13.3146410492204,
122.208333178973)) ;
#98846 = CARTESIAN_POINT('Ctrl Pts',(-19.1224390210634,-13.3246896290307,
122.240442168995)) ;
#98847 = CARTESIAN_POINT('Ctrl Pts',(-18.9256507377425,-13.3345726035008,
122.307133961459)) ;
#98848 = CARTESIAN_POINT('Ctrl Pts',(-18.7411652161108,-13.3445675146435,
122.407705197204)) ;
#98849 = CARTESIAN_POINT('Ctrl Pts',(-18.5766905845214,-13.3545879012171,
122.539355445226)) ;
#98850 = CARTESIAN_POINT('Ctrl Pts',(-18.439033782546,-13.3644980050741,122.695723682082)) ;
#98851 = CARTESIAN_POINT('Ctrl Pts',(-18.3299475073302,-13.374425717284,122.873667347378)) ;
#98852 = CARTESIAN_POINT('Ctrl Pts',(-18.2526965192885,-13.3844688270513,
123.070156691491)) ;
#98853 = CARTESIAN_POINT('Ctrl Pts',(-18.2112560671657,-13.3943552475068,
123.273838838563)) ;
#98854 = CARTESIAN_POINT('Ctrl Pts',(-18.2053955777972,-13.4043484251125,
123.483833556912)) ;
#98855 = CARTESIAN_POINT('Ctrl Pts',(-18.2360212352886,-13.4142940880164,
123.690668010788)) ;
#98856 = CARTESIAN_POINT('Ctrl Pts',(-18.3017033574793,-13.4242413842216,
123.889219209894)) ;
#98857 = CARTESIAN_POINT('Ctrl Pts',(-18.4020633929193,-13.4342891497995,
124.075085019888)) ;
#98858 = CARTESIAN_POINT('Ctrl Pts',(-18.5304401602059,-13.4441373630171,
124.237516105273)) ;
#98859 = CARTESIAN_POINT('Ctrl Pts',(-18.6863595573855,-13.4540969358112,
124.377263982517)) ;
#98860 = CARTESIAN_POINT('Ctrl Pts',(-18.8657414612721,-13.4641335568437,
124.488354087654)) ;
#98861 = CARTESIAN_POINT('Ctrl Pts',(-19.0585457397273,-13.474014071654,124.565704241206)) ;
#98862 = CARTESIAN_POINT('Ctrl Pts',(-19.2653263873522,-13.4840667229611,
124.60921364299)) ;
#98863 = CARTESIAN_POINT('Ctrl Pts',(-19.4732795778944,-13.4939621212411,
124.616136489103)) ;
#98864 = CARTESIAN_POINT('Ctrl Pts',(-19.6824477518937,-13.5040122429472,
124.586491924911)) ;
#98865 = CARTESIAN_POINT('Ctrl Pts',(-19.8800329152922,-13.5138965224891,
124.522077673044)) ;
#98866 = CARTESIAN_POINT('Ctrl Pts',(-20.0656316982844,-13.523891303781,124.423608798044)) ;
#98867 = CARTESIAN_POINT('Ctrl Pts',(-20.2305126212361,-13.5338391489678,
124.294932509829)) ;
#98868 = CARTESIAN_POINT('Ctrl Pts',(-20.3705968639577,-13.5437761123552,
124.139979594403)) ;
#98869 = CARTESIAN_POINT('Ctrl Pts',(-20.4824093236999,-13.5537590770924,
123.962339129303)) ;
#98870 = CARTESIAN_POINT('Ctrl Pts',(-20.5617843415041,-13.563802928508,123.766698717051)) ;
#98871 = CARTESIAN_POINT('Ctrl Pts',(-20.6055237200818,-13.5736311298428,
123.564729892149)) ;
#98872 = CARTESIAN_POINT('Ctrl Pts',(-20.6138303765551,-13.5837077024408,
123.353094858894)) ;
#98873 = CARTESIAN_POINT('Ctrl Pts',(-20.5859922059522,-13.5935597824484,
123.147807194047)) ;
#98874 = CARTESIAN_POINT('Ctrl Pts',(-20.5217116554415,-13.6036330674525,
122.946063088482)) ;
#98875 = CARTESIAN_POINT('Ctrl Pts',(-20.4255714123975,-13.613474419163,122.762843201202)) ;
#98876 = CARTESIAN_POINT('Ctrl Pts',(-20.298164414403,-13.6234359185595,122.596651330466)) ;
#98877 = CARTESIAN_POINT('Ctrl Pts',(-20.1424206354466,-13.6334716946895,
122.45430968353)) ;
#98878 = CARTESIAN_POINT('Ctrl Pts',(-19.9670675754912,-13.643360121327,122.342655165949)) ;
#98879 = CARTESIAN_POINT('Ctrl Pts',(-19.7726689839442,-13.6533754434019,
122.261750150218)) ;
#98880 = CARTESIAN_POINT('Ctrl Pts',(-19.5667675333596,-13.6634057923022,
122.216240185601)) ;
#98881 = CARTESIAN_POINT('Ctrl Pts',(-19.3600429921044,-13.6732491679088,
122.206925910413)) ;
#98882 = CARTESIAN_POINT('Ctrl Pts',(-19.1508941700709,-13.683278604806,122.233686851283)) ;
#98883 = CARTESIAN_POINT('Ctrl Pts',(-18.9496884166642,-13.6933104827389,
122.296924048435)) ;
#98884 = CARTESIAN_POINT('Ctrl Pts',(-18.7661167458071,-13.7031401058444,
122.391793602705)) ;
#98885 = CARTESIAN_POINT('Ctrl Pts',(-18.5987378462843,-13.7131295769975,
122.518643646911)) ;
#98886 = CARTESIAN_POINT('Ctrl Pts',(-18.455548298143,-13.7231734257599,122.673826390038)) ;
#98887 = CARTESIAN_POINT('Ctrl Pts',(-18.3436412768283,-13.7329951312916,
122.847354036714)) ;
#98888 = CARTESIAN_POINT('Ctrl Pts',(-18.2613484075715,-13.7430301711194,
123.04160927534)) ;
#98889 = CARTESIAN_POINT('Ctrl Pts',(-18.2146498316411,-13.7530548780108,
123.247129044007)) ;
#98890 = CARTESIAN_POINT('Ctrl Pts',(-18.2040846951332,-13.7629075823516,
123.453993461801)) ;
#98891 = CARTESIAN_POINT('Ctrl Pts',(-18.2295836191585,-13.7728957045593,
123.662406074756)) ;
#98892 = CARTESIAN_POINT('Ctrl Pts',(-18.2905119173105,-13.7828241746666,
123.862048522157)) ;
#98893 = CARTESIAN_POINT('Ctrl Pts',(-18.3854475998117,-13.7928131518338,
124.049375421795)) ;
#98894 = CARTESIAN_POINT('Ctrl Pts',(-18.5123625349059,-13.8028509591135,
124.21796475125)) ;
#98895 = CARTESIAN_POINT('Ctrl Pts',(-18.6634533080055,-13.8126972599768,
124.359461546451)) ;
#98896 = CARTESIAN_POINT('Ctrl Pts',(-18.8397204132495,-13.8227230033561,
124.475030609965)) ;
#98897 = CARTESIAN_POINT('Ctrl Pts',(-19.0336949710759,-13.8327538697951,
124.557776886173)) ;
#98898 = CARTESIAN_POINT('Ctrl Pts',(-19.2350194910075,-13.8425912285939,
124.605064267857)) ;
#98899 = CARTESIAN_POINT('Ctrl Pts',(-19.4447178184432,-13.8525831895276,
124.617421996652)) ;
#98900 = CARTESIAN_POINT('Ctrl Pts',(-19.654179846885,-13.8626155520842,124.592661529572)) ;
#98901 = CARTESIAN_POINT('Ctrl Pts',(-19.8528488201353,-13.8724807126586,
124.533165503572)) ;
#98902 = CARTESIAN_POINT('Ctrl Pts',(-20.0402681711591,-13.8824426172363,
124.439690047989)) ;
#98903 = CARTESIAN_POINT('Ctrl Pts',(-20.2096246615694,-13.892477547312,124.313911734447)) ;
#98904 = CARTESIAN_POINT('Ctrl Pts',(-20.3526856495407,-13.9023624941656,
124.163140613639)) ;
#98905 = CARTESIAN_POINT('Ctrl Pts',(-20.4694160674979,-13.9124281704771,
123.986678419521)) ;
#98906 = CARTESIAN_POINT('Ctrl Pts',(-20.552057237403,-13.922267090112,123.797021962787)) ;
#98907 = CARTESIAN_POINT('Ctrl Pts',(-20.6018696695275,-13.9323305998464,
123.591433823541)) ;
#98908 = CARTESIAN_POINT('Ctrl Pts',(-20.614834799251,-13.9422242130082,123.383819073715)) ;
#98909 = CARTESIAN_POINT('Ctrl Pts',(-20.5919920278635,-13.9521682198216,
123.176044959446)) ;
#98910 = CARTESIAN_POINT('Ctrl Pts',(-20.5331619003157,-13.9621691741759,
122.974158349831)) ;
#98911 = CARTESIAN_POINT('Ctrl Pts',(-20.4395047211157,-13.9722079318682,
122.78505259252)) ;
#98912 = CARTESIAN_POINT('Ctrl Pts',(-20.3174523928716,-13.9820321160382,
122.618417896484)) ;
#98913 = CARTESIAN_POINT('Ctrl Pts',(-20.1650112730294,-13.9920901816376,
122.471905247908)) ;
#98914 = CARTESIAN_POINT('Ctrl Pts',(-19.9915019639787,-14.0020202284123,
122.355797825904)) ;
#98915 = CARTESIAN_POINT('Ctrl Pts',(-19.8002891957764,-14.0119716707494,
122.270899230313)) ;
#98916 = CARTESIAN_POINT('Ctrl Pts',(-19.595229379244,-14.0220184679287,122.220289733673)) ;
#98917 = CARTESIAN_POINT('Ctrl Pts',(-19.388678662098,-14.0318664086088,122.206142772655)) ;
#98918 = CARTESIAN_POINT('Ctrl Pts',(-19.180373152553,-14.0418280399514,122.227680220025)) ;
#98919 = CARTESIAN_POINT('Ctrl Pts',(-18.9776681297152,-14.0518566993273,
122.285706645314)) ;
#98920 = CARTESIAN_POINT('Ctrl Pts',(-18.7903445401508,-14.0617670022155,
122.37688778434)) ;
#98921 = CARTESIAN_POINT('Ctrl Pts',(-18.6209463624142,-14.0717018967777,
122.499078902491)) ;
#98922 = CARTESIAN_POINT('Ctrl Pts',(-18.473930832625,-14.0817429954446,122.650555065368)) ;
#98923 = CARTESIAN_POINT('Ctrl Pts',(-18.3571350752983,-14.091630277949,122.822514916368)) ;
#98924 = CARTESIAN_POINT('Ctrl Pts',(-18.2707571772679,-14.1016220184595,
123.013976692331)) ;
#98925 = CARTESIAN_POINT('Ctrl Pts',(-18.2192126463218,-14.1115725676949,
123.2167295132)) ;
#98926 = CARTESIAN_POINT('Ctrl Pts',(-18.203370025027,-14.1215082453297,123.424994308687)) ;
#98927 = CARTESIAN_POINT('Ctrl Pts',(-18.2238119146221,-14.1314936631225,
123.633937869692)) ;
#98928 = CARTESIAN_POINT('Ctrl Pts',(-18.2807153052305,-14.141522455993,123.836949114812)) ;
#98929 = CARTESIAN_POINT('Ctrl Pts',(-18.3704450265709,-14.1514019672209,
124.024261846326)) ;
#98930 = CARTESIAN_POINT('Ctrl Pts',(-18.4923442488738,-14.1613955038939,
124.195388029186)) ;
#98931 = CARTESIAN_POINT('Ctrl Pts',(-18.6429808625608,-14.1714277721577,
124.342995126531)) ;
#98932 = CARTESIAN_POINT('Ctrl Pts',(-18.8138139946076,-14.1812917341636,
124.46058815223)) ;
#98933 = CARTESIAN_POINT('Ctrl Pts',(-19.0063568696892,-14.1913617955085,
124.548546327195)) ;
#98934 = CARTESIAN_POINT('Ctrl Pts',(-19.2066468946363,-14.2012041598572,
124.600533451144)) ;
#98935 = CARTESIAN_POINT('Ctrl Pts',(-19.4153248327152,-14.2111648323597,
124.617920620162)) ;
#98936 = CARTESIAN_POINT('Ctrl Pts',(-19.6254284051724,-14.2212029034275,
124.598242795069)) ;
#98937 = CARTESIAN_POINT('Ctrl Pts',(-19.8257334158535,-14.2310765183879,
124.543671256272)) ;
#98938 = CARTESIAN_POINT('Ctrl Pts',(-20.0172095444712,-14.2411487529692,
124.453349081076)) ;
#98939 = CARTESIAN_POINT('Ctrl Pts',(-20.1860360912961,-14.250972771418,124.334308802736)) ;
#98940 = CARTESIAN_POINT('Ctrl Pts',(-20.335329758392,-14.261037692394,124.184427656445)) ;
#98941 = CARTESIAN_POINT('Ctrl Pts',(-20.4942349167154,-14.2742479906888,
123.956571109529)) ;
#98942 = CARTESIAN_POINT('Ctrl Pts',(-20.5910379612481,-14.2875634374207,
123.690586230537)) ;
#98943 = CARTESIAN_POINT('Ctrl Pts',(-20.6153297521392,-14.300853682688,123.412198369631)) ;
#98944 = CARTESIAN_POINT('Ctrl Pts',(-20.5967516423446,-14.3109044322951,
123.201753217143)) ;
#98945 = CARTESIAN_POINT('Ctrl Pts',(-20.5435902180751,-14.3207170392773,
123.002398211266)) ;
#98946 = CARTESIAN_POINT('Ctrl Pts',(-20.4546105424166,-14.3307881372716,
122.810305971542)) ;
#98947 = CARTESIAN_POINT('Ctrl Pts',(-20.335614571465,-14.3406777100464,122.639802370613)) ;
#98948 = CARTESIAN_POINT('Ctrl Pts',(-20.1392382690808,-14.3539478168497,
122.441607998033)) ;
#98949 = CARTESIAN_POINT('Ctrl Pts',(-19.8341119395452,-14.3705645037722,
122.263579414853)) ;
#98950 = CARTESIAN_POINT('Ctrl Pts',(-19.4873914594696,-14.3871385470885,
122.200251207052)) ;
#98951 = CARTESIAN_POINT('Ctrl Pts',(-19.2087764898779,-14.4004351145203,
122.222571590345)) ;
#98952 = CARTESIAN_POINT('Ctrl Pts',(-19.0047056321309,-14.4104651780977,
122.275708556322)) ;
#98953 = CARTESIAN_POINT('Ctrl Pts',(-18.8155858732602,-14.4203590699469,
122.362246555155)) ;
#98954 = CARTESIAN_POINT('Ctrl Pts',(-18.5855945168441,-14.4336118257325,
122.519619674998)) ;
#98955 = CARTESIAN_POINT('Ctrl Pts',(-18.354527687707,-14.4503399307249,122.789939082739)) ;
#98956 = CARTESIAN_POINT('Ctrl Pts',(-18.206345083616,-14.4701707672034,123.184783553394)) ;
#98957 = CARTESIAN_POINT('Ctrl Pts',(-18.2007419533952,-14.4900961590936,
123.608319979679)) ;
#98958 = CARTESIAN_POINT('Ctrl Pts',(-18.3401055208104,-14.5100213724456,
124.008477424313)) ;
#98959 = CARTESIAN_POINT('Ctrl Pts',(-18.6074981000841,-14.5299463859307,
124.337030852203)) ;
#98960 = CARTESIAN_POINT('Ctrl Pts',(-18.9698370075057,-14.5498228576307,
124.5546243647)) ;
#98961 = CARTESIAN_POINT('Ctrl Pts',(-19.3867579538621,-14.5698021755395,
124.636106316293)) ;
#98962 = CARTESIAN_POINT('Ctrl Pts',(-19.8054747811673,-14.5897351791155,
124.57025712998)) ;
#98963 = CARTESIAN_POINT('Ctrl Pts',(-20.1760500752782,-14.6096304491432,
124.366285619515)) ;
#98964 = CARTESIAN_POINT('Ctrl Pts',(-20.4554967889345,-14.6295517870491,
124.047938368198)) ;
#98965 = CARTESIAN_POINT('Ctrl Pts',(-20.6097302975389,-14.6495094103152,
123.652583446367)) ;
#98966 = CARTESIAN_POINT('Ctrl Pts',(-20.619847629107,-14.6693892422725,123.230070663472)) ;
#98967 = CARTESIAN_POINT('Ctrl Pts',(-20.4862218718762,-14.6892710935694,
122.828917338771)) ;
#98968 = CARTESIAN_POINT('Ctrl Pts',(-20.2206792833433,-14.7093421106732,
122.494899551931)) ;
#98969 = CARTESIAN_POINT('Ctrl Pts',(-19.8617957888506,-14.7291493344262,
122.274354193157)) ;
#98970 = CARTESIAN_POINT('Ctrl Pts',(-19.4458883521652,-14.749130469995,122.187819073494)) ;
#98971 = CARTESIAN_POINT('Ctrl Pts',(-19.0266632363293,-14.7690579633343,
122.249061061451)) ;
#98972 = CARTESIAN_POINT('Ctrl Pts',(-18.6546849719564,-14.7888786246921,
122.447411954383)) ;
#98973 = CARTESIAN_POINT('Ctrl Pts',(-18.369475358789,-14.8089758139139,122.765411956991)) ;
#98974 = CARTESIAN_POINT('Ctrl Pts',(-18.2121518888613,-14.8287394929222,
123.155302158565)) ;
#98975 = CARTESIAN_POINT('Ctrl Pts',(-18.1966217730203,-14.8487967715953,
123.581303860875)) ;
#98976 = CARTESIAN_POINT('Ctrl Pts',(-18.3260111960601,-14.8685921953427,
123.981947285313)) ;
#98977 = CARTESIAN_POINT('Ctrl Pts',(-18.5854071847529,-14.8885558400703,
124.317888718748)) ;
#98978 = CARTESIAN_POINT('Ctrl Pts',(-18.9448261126294,-14.9085393313444,
124.54452721317)) ;
#98979 = CARTESIAN_POINT('Ctrl Pts',(-19.3562025339838,-14.9283468264937,
124.634965611393)) ;
#98980 = CARTESIAN_POINT('Ctrl Pts',(-19.7773748002404,-14.9483294172138,
124.579603814247)) ;
#98981 = CARTESIAN_POINT('Ctrl Pts',(-20.1526221444267,-14.968212071205,124.384671096737)) ;
#98982 = CARTESIAN_POINT('Ctrl Pts',(-20.4400220578317,-14.9881703160681,
124.072556486003)) ;
#98983 = CARTESIAN_POINT('Ctrl Pts',(-20.603282234311,-15.0080459031097,123.68268711379)) ;
#98984 = CARTESIAN_POINT('Ctrl Pts',(-20.6241041088958,-15.0280267912449,
123.258378276788)) ;
#98985 = CARTESIAN_POINT('Ctrl Pts',(-20.49882428268,-15.0479619323559,122.853380511244)) ;
#98986 = CARTESIAN_POINT('Ctrl Pts',(-20.2434601677931,-15.067873950367,122.515729248997)) ;
#98987 = CARTESIAN_POINT('Ctrl Pts',(-19.8888236566201,-15.0877621686106,
122.285352071396)) ;
#98988 = CARTESIAN_POINT('Ctrl Pts',(-19.5451528945832,-15.1043604724575,
122.205344172208)) ;
#98989 = CARTESIAN_POINT('Ctrl Pts',(-19.2662167875968,-15.1176330623603,
122.214362439723)) ;
#98990 = CARTESIAN_POINT('Ctrl Pts',(-19.0602783940838,-15.1276404773112,
122.257360667435)) ;
#98991 = CARTESIAN_POINT('Ctrl Pts',(-18.8649799937117,-15.1376478240438,
122.335647448858)) ;
#98992 = CARTESIAN_POINT('Ctrl Pts',(-18.6279934373651,-15.1509141838454,
122.482611207681)) ;
#98993 = CARTESIAN_POINT('Ctrl Pts',(-18.3871463208659,-15.1674288414683,
122.738163474856)) ;
#98994 = CARTESIAN_POINT('Ctrl Pts',(-18.2465602699306,-15.184026274711,123.061779254572)) ;
#98995 = CARTESIAN_POINT('Ctrl Pts',(-18.2054858082238,-15.197374271856,123.339439468977)) ;
#98996 = CARTESIAN_POINT('Ctrl Pts',(-18.2109597373831,-15.2072700262076,
123.547401686533)) ;
#98997 = CARTESIAN_POINT('Ctrl Pts',(-18.2525893045886,-15.2172579801389,
123.753197572489)) ;
#98998 = CARTESIAN_POINT('Ctrl Pts',(-18.3290124450646,-15.2272152038437,
123.948107118363)) ;
#98999 = CARTESIAN_POINT('Ctrl Pts',(-18.4390392158842,-15.2372507504003,
124.128107201578)) ;
#99000 = CARTESIAN_POINT('Ctrl Pts',(-18.5764840416179,-15.2471378616764,
124.284054988754)) ;
#99001 = CARTESIAN_POINT('Ctrl Pts',(-18.740404239582,-15.2571292667773,124.41538388385)) ;
#99002 = CARTESIAN_POINT('Ctrl Pts',(-18.9238326069413,-15.2670748879921,
124.515742148504)) ;
#99003 = CARTESIAN_POINT('Ctrl Pts',(-19.1218477074097,-15.2770241362604,
124.583157243385)) ;
#99004 = CARTESIAN_POINT('Ctrl Pts',(-19.3305973669952,-15.287070631429,124.615231792399)) ;
#99005 = CARTESIAN_POINT('Ctrl Pts',(-19.5376679109232,-15.2969219742205,
124.610869425438)) ;
#99006 = CARTESIAN_POINT('Ctrl Pts',(-19.7433876136438,-15.3068937543479,
124.570653912151)) ;
#99007 = CARTESIAN_POINT('Ctrl Pts',(-19.9395051954492,-15.3168889543256,
124.495111000184)) ;
#99008 = CARTESIAN_POINT('Ctrl Pts',(-20.1200485214324,-15.3269229460216,
124.386048038708)) ;
#99009 = CARTESIAN_POINT('Ctrl Pts',(-20.2763298783677,-15.3367783509941,
124.249986100095)) ;
#99010 = CARTESIAN_POINT('Ctrl Pts',(-20.4087021600273,-15.3467776488399,
124.086727016584)) ;
#99011 = CARTESIAN_POINT('Ctrl Pts',(-20.509884017524,-15.3566727614451,123.904925296296)) ;
#99012 = CARTESIAN_POINT('Ctrl Pts',(-20.5790585361454,-15.3667334069801,
123.705079423127)) ;
#99013 = CARTESIAN_POINT('Ctrl Pts',(-20.6119035229336,-15.3765822839693,
123.500630501145)) ;
#99014 = CARTESIAN_POINT('Ctrl Pts',(-20.6092249537974,-15.3866109950629,
123.289815316641)) ;
#99015 = CARTESIAN_POINT('Ctrl Pts',(-20.5694153700517,-15.396640396319,123.082753768917)) ;
#99016 = CARTESIAN_POINT('Ctrl Pts',(-20.4961065231675,-15.406480588115,122.889303094458)) ;
#99017 = CARTESIAN_POINT('Ctrl Pts',(-20.3889142955472,-15.416484017308,122.708392623558)) ;
#99018 = CARTESIAN_POINT('Ctrl Pts',(-20.2520951632143,-15.4264695297742,
122.549129099558)) ;
#99019 = CARTESIAN_POINT('Ctrl Pts',(-20.0887057156194,-15.4365106261582,
122.415501236203)) ;
#99020 = CARTESIAN_POINT('Ctrl Pts',(-19.9083321991845,-15.4463538221092,
122.314037131417)) ;
#99021 = CARTESIAN_POINT('Ctrl Pts',(-19.7104324140253,-15.4563401331636,
122.244058196646)) ;
#99022 = CARTESIAN_POINT('Ctrl Pts',(-19.5044074861997,-15.4662748184213,
122.209531335584)) ;
#99023 = CARTESIAN_POINT('Ctrl Pts',(-19.2930056338594,-15.4763323796383,
122.211509097077)) ;
#99024 = CARTESIAN_POINT('Ctrl Pts',(-19.0899248982787,-15.4861540212469,
122.24895534844)) ;
#99025 = CARTESIAN_POINT('Ctrl Pts',(-18.8917123056531,-15.4962100848379,
122.322431822652)) ;
#99026 = CARTESIAN_POINT('Ctrl Pts',(-18.7115304286449,-15.5061507605997,
122.428321236786)) ;
#99027 = CARTESIAN_POINT('Ctrl Pts',(-18.5526336052968,-15.516055119388,122.562890932367)) ;
#99028 = CARTESIAN_POINT('Ctrl Pts',(-18.4177188485031,-15.5261017739638,
122.725376550476)) ;
#99029 = CARTESIAN_POINT('Ctrl Pts',(-18.3144558854452,-15.5359973686067,
122.906011130178)) ;
#99030 = CARTESIAN_POINT('Ctrl Pts',(-18.2429422386435,-15.5460593152635,
123.105064623054)) ;
#99031 = CARTESIAN_POINT('Ctrl Pts',(-18.2077902932112,-15.5559089391957,
123.309140063898)) ;
#99032 = CARTESIAN_POINT('Ctrl Pts',(-18.2079234694867,-15.5658721782255,
123.518586350037)) ;
#99033 = CARTESIAN_POINT('Ctrl Pts',(-18.2449368009256,-15.5758967530014,
123.726071296126)) ;
#99034 = CARTESIAN_POINT('Ctrl Pts',(-18.316515430472,-15.5858153156891,123.921914355744)) ;
#99035 = CARTESIAN_POINT('Ctrl Pts',(-18.421476153643,-15.5958075024131,124.103894260273)) ;
#99036 = CARTESIAN_POINT('Ctrl Pts',(-18.5572936420594,-15.6058423009973,
124.265311516083)) ;
#99037 = CARTESIAN_POINT('Ctrl Pts',(-18.7159696918427,-15.6156974916709,
124.398559351051)) ;
#99038 = CARTESIAN_POINT('Ctrl Pts',(-18.8978108066733,-15.6256968398239,
124.503966265376)) ;
#99039 = CARTESIAN_POINT('Ctrl Pts',(-19.0931220053763,-15.6355919654991,
124.575680360087)) ;
#99040 = CARTESIAN_POINT('Ctrl Pts',(-19.3012849776767,-15.6456525084472,
124.6129736069)) ;
#99041 = CARTESIAN_POINT('Ctrl Pts',(-19.5083624664889,-15.6555017827141,
124.613661373885)) ;
#99042 = CARTESIAN_POINT('Ctrl Pts',(-19.7161694335848,-15.665529007284,124.578275144617)) ;
#99043 = CARTESIAN_POINT('Ctrl Pts',(-19.9145290551385,-15.6755574064718,
124.50681132013)) ;
#99044 = CARTESIAN_POINT('Ctrl Pts',(-20.0943037788258,-15.6854031568852,
124.404246514876)) ;
#99045 = CARTESIAN_POINT('Ctrl Pts',(-20.2562467072818,-15.695391947286,124.270541635842)) ;
#99046 = CARTESIAN_POINT('Ctrl Pts',(-20.392860442262,-15.7054368756857,124.10951908799)) ;
#99047 = CARTESIAN_POINT('Ctrl Pts',(-20.4975269150596,-15.7152613604747,
123.931448000396)) ;
#99048 = CARTESIAN_POINT('Ctrl Pts',(-20.5716719540745,-15.7253187580159,
123.733454629045)) ;
#99049 = CARTESIAN_POINT('Ctrl Pts',(-20.6095443624206,-15.7352448496021,
123.528227172313)) ;
#99050 = CARTESIAN_POINT('Ctrl Pts',(-20.6117538881597,-15.7451996347466,
123.318960205369)) ;
#99051 = CARTESIAN_POINT('Ctrl Pts',(-20.5770787944233,-15.7552370044043,
123.110812421118)) ;
#99052 = CARTESIAN_POINT('Ctrl Pts',(-20.5079786644666,-15.7651258145259,
122.914732694554)) ;
#99053 = CARTESIAN_POINT('Ctrl Pts',(-20.4051776385121,-15.7751151735769,
122.731611754423)) ;
#99054 = CARTESIAN_POINT('Ctrl Pts',(-20.2724329624827,-15.785073721033,122.569723636666)) ;
#99055 = CARTESIAN_POINT('Ctrl Pts',(-20.1148565490367,-15.7949732975841,
122.433749510485)) ;
#99056 = CARTESIAN_POINT('Ctrl Pts',(-19.9333763926102,-15.8050212094148,
122.325686454382)) ;
#99057 = CARTESIAN_POINT('Ctrl Pts',(-19.738896008294,-15.8149165572753,122.251741274067)) ;
#99058 = CARTESIAN_POINT('Ctrl Pts',(-19.5311562760198,-15.8249782338065,
122.212012298134)) ;
#99059 = CARTESIAN_POINT('Ctrl Pts',(-19.3242083962337,-15.8348227515557,
122.208989216626)) ;
#99060 = CARTESIAN_POINT('Ctrl Pts',(-19.1173679561913,-15.8447831952704,
122.241595187963)) ;
#99061 = CARTESIAN_POINT('Ctrl Pts',(-18.917939291677,-15.8548200280887,122.31051355585)) ;
#99062 = CARTESIAN_POINT('Ctrl Pts',(-18.7362238182825,-15.8646988248355,
122.411112445382)) ;
#99063 = CARTESIAN_POINT('Ctrl Pts',(-18.5717749461407,-15.8747581409638,
122.544043463195)) ;
#99064 = CARTESIAN_POINT('Ctrl Pts',(-18.4354880882042,-15.8846285877171,
122.700537333308)) ;
#99065 = CARTESIAN_POINT('Ctrl Pts',(-18.326637697773,-15.8946212259751,122.880215418249)) ;
#99066 = CARTESIAN_POINT('Ctrl Pts',(-18.2507661793473,-15.904653241523,123.076992696614)) ;
#99067 = CARTESIAN_POINT('Ctrl Pts',(-18.2104378402102,-15.9145190978296,
123.28046630249)) ;
#99068 = CARTESIAN_POINT('Ctrl Pts',(-18.2059425097453,-15.9245883872987,
123.492083430756)) ;
#99069 = CARTESIAN_POINT('Ctrl Pts',(-18.2375158673357,-15.93443194485,123.696615030416)) ;
#99070 = CARTESIAN_POINT('Ctrl Pts',(-18.3043904646456,-15.9444120716378,
123.895478498069)) ;
#99071 = CARTESIAN_POINT('Ctrl Pts',(-18.405520803553,-15.9544306202378,124.080226272213)) ;
#99072 = CARTESIAN_POINT('Ctrl Pts',(-18.5350894076568,-15.964313920761,124.242688884961)) ;
#99073 = CARTESIAN_POINT('Ctrl Pts',(-18.6938314242704,-15.9743822078091,
124.382650655659)) ;
#99074 = CARTESIAN_POINT('Ctrl Pts',(-18.8701229122418,-15.9842123308277,
124.49055863566)) ;
#99075 = CARTESIAN_POINT('Ctrl Pts',(-19.0669348057109,-15.9942789147531,
124.568265960041)) ;
#99076 = CARTESIAN_POINT('Ctrl Pts',(-19.2707000217283,-16.0041690277675,
124.609767421826)) ;
#99077 = CARTESIAN_POINT('Ctrl Pts',(-19.4806745579737,-16.0141617165302,
124.615758779483)) ;
#99078 = CARTESIAN_POINT('Ctrl Pts',(-19.6878442505005,-16.0241226048859,
124.585148629839)) ;
#99079 = CARTESIAN_POINT('Ctrl Pts',(-19.8857864877061,-16.0340405497659,
124.519664690455)) ;
#99080 = CARTESIAN_POINT('Ctrl Pts',(-20.0711599659427,-16.0440483028621,
124.420109851482)) ;
#99081 = CARTESIAN_POINT('Ctrl Pts',(-20.2365270806304,-16.0540793968212,
124.289260675966)) ;
#99082 = CARTESIAN_POINT('Ctrl Pts',(-20.3744685647117,-16.0639273648492,
124.134853388205)) ;
#99083 = CARTESIAN_POINT('Ctrl Pts',(-20.4860139635941,-16.073989320975,123.955138435932)) ;
#99084 = CARTESIAN_POINT('Ctrl Pts',(-20.5632011629455,-16.0838865325762,
123.761905688894)) ;
#99085 = CARTESIAN_POINT('Ctrl Pts',(-20.6064813781661,-16.0938176992408,
123.557660550307)) ;
#99086 = CARTESIAN_POINT('Ctrl Pts',(-20.6134913356324,-16.103859883445,123.346661512795)) ;
#99087 = CARTESIAN_POINT('Ctrl Pts',(-20.5843659339003,-16.1137465516981,
123.14085393464)) ;
#99088 = CARTESIAN_POINT('Ctrl Pts',(-20.5195954479631,-16.1237396636764,
122.941012395821)) ;
#99089 = CARTESIAN_POINT('Ctrl Pts',(-20.4215027237051,-16.1336853412922,
122.756360632577)) ;
#99090 = CARTESIAN_POINT('Ctrl Pts',(-20.2931478547544,-16.1436326442772,
122.591249132135)) ;
#99091 = CARTESIAN_POINT('Ctrl Pts',(-20.1363629667239,-16.1536803680239,
122.449699004815)) ;
#99092 = CARTESIAN_POINT('Ctrl Pts',(-19.9610175606814,-16.1635287417865,
122.339609666204)) ;
#99093 = CARTESIAN_POINT('Ctrl Pts',(-19.7673272141133,-16.1734877142322,
122.260115093733)) ;
#99094 = CARTESIAN_POINT('Ctrl Pts',(-19.5610605978917,-16.1835265761133,
122.21547621593)) ;
#99095 = CARTESIAN_POINT('Ctrl Pts',(-19.3535277384194,-16.1934051802851,
122.207127939738)) ;
#99096 = CARTESIAN_POINT('Ctrl Pts',(-19.1441319995967,-16.2034567214885,
122.235331709229)) ;
#99097 = CARTESIAN_POINT('Ctrl Pts',(-18.9458603435588,-16.2133521194688,
122.298425318921)) ;
#99098 = CARTESIAN_POINT('Ctrl Pts',(-18.7586572676854,-16.2234033520141,
122.396376404111)) ;
#99099 = CARTESIAN_POINT('Ctrl Pts',(-18.5939995467362,-16.2332895426384,
122.523238122634)) ;
#99100 = CARTESIAN_POINT('Ctrl Pts',(-18.452105397037,-16.2432820819541,122.6781235239)) ;
#99101 = CARTESIAN_POINT('Ctrl Pts',(-18.3397979191434,-16.2532305278489,
122.854575575533)) ;
#99102 = CARTESIAN_POINT('Ctrl Pts',(-18.2596650212314,-16.2631673303808,
123.047478366738)) ;
#99103 = CARTESIAN_POINT('Ctrl Pts',(-18.213763833646,-16.2731503378321,123.252299108074)) ;
#99104 = CARTESIAN_POINT('Ctrl Pts',(-18.2044549906042,-16.2831941792469,
123.463222901046)) ;
#99105 = CARTESIAN_POINT('Ctrl Pts',(-18.230844018045,-16.2930223778708,123.668181805345)) ;
#99106 = CARTESIAN_POINT('Ctrl Pts',(-18.293857978941,-16.303098971313,123.870388955193)) ;
#99107 = CARTESIAN_POINT('Ctrl Pts',(-18.3888049572277,-16.3129509706546,
124.054515489403)) ;
#99108 = CARTESIAN_POINT('Ctrl Pts',(-18.51691360887,-16.3230245574784,124.2231066674)) ;
#99109 = CARTESIAN_POINT('Ctrl Pts',(-18.6688148153604,-16.3328647825759,
124.363569501756)) ;
#99110 = CARTESIAN_POINT('Ctrl Pts',(-18.8445860740731,-16.3428304866046,
124.477551496908)) ;
#99111 = CARTESIAN_POINT('Ctrl Pts',(-19.0388043493852,-16.3528571199112,
124.559512214627)) ;
#99112 = CARTESIAN_POINT('Ctrl Pts',(-19.2419523690038,-16.362771415623,124.606112527445)) ;
#99113 = CARTESIAN_POINT('Ctrl Pts',(-19.4516578331547,-16.3727597043154,
124.617191578532)) ;
#99114 = CARTESIAN_POINT('Ctrl Pts',(-19.661089094413,-16.3827984374738,124.591182848114)) ;
#99115 = CARTESIAN_POINT('Ctrl Pts',(-19.859004541584,-16.3926417693013,124.5307445253)) ;
#99116 = CARTESIAN_POINT('Ctrl Pts',(-20.0470963473085,-16.4026694951809,
124.435533956543)) ;
#99117 = CARTESIAN_POINT('Ctrl Pts',(-20.2155368885849,-16.4127018315695,
124.308590596586)) ;
#99118 = CARTESIAN_POINT('Ctrl Pts',(-20.3567606206054,-16.4225313318701,
124.15774756144)) ;
#99119 = CARTESIAN_POINT('Ctrl Pts',(-20.4720239138682,-16.4325208357869,
123.982187719517)) ;
#99120 = CARTESIAN_POINT('Ctrl Pts',(-20.5550085562044,-16.4425646762993,
123.788026903889)) ;
#99121 = CARTESIAN_POINT('Ctrl Pts',(-20.602374888895,-16.4523863820673,123.587050646233)) ;
#99122 = CARTESIAN_POINT('Ctrl Pts',(-20.6148970316239,-16.4624214291997,
123.376455143425)) ;
#99123 = CARTESIAN_POINT('Ctrl Pts',(-20.5901081049944,-16.4724461066366,
123.167160145948)) ;
#99124 = CARTESIAN_POINT('Ctrl Pts',(-20.5308182160957,-16.482298921491,122.968690519958)) ;
#99125 = CARTESIAN_POINT('Ctrl Pts',(-20.4370333022036,-16.4922866310986,
122.780843362128)) ;
#99126 = CARTESIAN_POINT('Ctrl Pts',(-20.31277289343,-16.5022166410927,122.613084096028)) ;
#99127 = CARTESIAN_POINT('Ctrl Pts',(-20.1605853136459,-16.5122063963118,
122.468351964831)) ;
#99128 = CARTESIAN_POINT('Ctrl Pts',(-19.984783451763,-16.5222330049947,122.352041817663)) ;
#99129 = CARTESIAN_POINT('Ctrl Pts',(-19.7942943126666,-16.5321169450166,
122.26903888892)) ;
#99130 = CARTESIAN_POINT('Ctrl Pts',(-19.5902387691111,-16.5421061725551,
122.219375676687)) ;
#99131 = CARTESIAN_POINT('Ctrl Pts',(-19.3795149747174,-16.5521490430788,
122.206262664231)) ;
#99132 = CARTESIAN_POINT('Ctrl Pts',(-19.1740770383601,-16.5619814298342,
122.229113777772)) ;
#99133 = CARTESIAN_POINT('Ctrl Pts',(-18.9723117795397,-16.5719747230058,
122.28765602834)) ;
#99134 = CARTESIAN_POINT('Ctrl Pts',(-18.7832283003811,-16.5820067286542,
122.3811032648)) ;
#99135 = CARTESIAN_POINT('Ctrl Pts',(-18.6159331208007,-16.5918719846232,
122.503667595197)) ;
#99136 = CARTESIAN_POINT('Ctrl Pts',(-18.4706150959863,-16.6018338645307,
122.65448612328)) ;
#99137 = CARTESIAN_POINT('Ctrl Pts',(-18.3531300325997,-16.6118687978926,
122.829697635396)) ;
#99138 = CARTESIAN_POINT('Ctrl Pts',(-18.2687898157938,-16.6217537562719,
123.019658602296)) ;
#99139 = CARTESIAN_POINT('Ctrl Pts',(-18.2178601672243,-16.6318193831945,
123.225013792638)) ;
#99140 = CARTESIAN_POINT('Ctrl Pts',(-18.2034722691943,-16.6416584888589,
123.431395574494)) ;
#99141 = CARTESIAN_POINT('Ctrl Pts',(-18.2253430566944,-16.6517213038642,
123.641785438067)) ;
#99142 = CARTESIAN_POINT('Ctrl Pts',(-18.2826479337508,-16.6616175099129,
123.84180974963)) ;
#99143 = CARTESIAN_POINT('Ctrl Pts',(-18.3736809540544,-16.6715583329382,
124.029901929783)) ;
#99144 = CARTESIAN_POINT('Ctrl Pts',(-18.4967610854605,-16.6815629159168,
124.200486438673)) ;
#99145 = CARTESIAN_POINT('Ctrl Pts',(-18.647994986647,-16.6915838103616,124.347144061911)) ;
#99146 = CARTESIAN_POINT('Ctrl Pts',(-18.8200146036931,-16.701475730951,124.464013888075)) ;
#99147 = CARTESIAN_POINT('Ctrl Pts',(-19.011525631297,-16.7114691632964,124.550383159991)) ;
#99148 = CARTESIAN_POINT('Ctrl Pts',(-19.2141727521891,-16.7214147681962,
124.601876513476)) ;
#99149 = CARTESIAN_POINT('Ctrl Pts',(-19.422697781733,-16.7313620416778,124.617828957646)) ;
#99150 = CARTESIAN_POINT('Ctrl Pts',(-19.6328892633515,-16.7414099561541,
124.596890600958)) ;
#99151 = CARTESIAN_POINT('Ctrl Pts',(-19.8322547940053,-16.7512575965015,
124.541079255269)) ;
#99152 = CARTESIAN_POINT('Ctrl Pts',(-20.0213360328354,-16.7612193118781,
124.451058503508)) ;
#99153 = CARTESIAN_POINT('Ctrl Pts',(-20.1929241016736,-16.7712479354509,
124.328527656308)) ;
#99154 = CARTESIAN_POINT('Ctrl Pts',(-20.3389201808685,-16.7811582975173,
124.179902269364)) ;
#99155 = CARTESIAN_POINT('Ctrl Pts',(-20.457646288526,-16.7910929911697,124.008060926701)) ;
#99156 = CARTESIAN_POINT('Ctrl Pts',(-20.5454725595361,-16.8011348342976,
123.816097312001)) ;
#99157 = CARTESIAN_POINT('Ctrl Pts',(-20.5979872971143,-16.811019339868,123.615017272021)) ;
#99158 = CARTESIAN_POINT('Ctrl Pts',(-20.6152306651984,-16.8210214436532,
123.405480465075)) ;
#99159 = CARTESIAN_POINT('Ctrl Pts',(-20.59615783476,-16.8309397950682,123.197804707673)) ;
#99160 = CARTESIAN_POINT('Ctrl Pts',(-20.540565323971,-16.8409874510891,122.994052134755)) ;
#99161 = CARTESIAN_POINT('Ctrl Pts',(-20.4522004901236,-16.8508586441173,
122.806233806691)) ;
#99162 = CARTESIAN_POINT('Ctrl Pts',(-20.330289879921,-16.8609243572608,122.633325413483)) ;
#99163 = CARTESIAN_POINT('Ctrl Pts',(-20.183485044894,-16.8707768178334,122.48712577747)) ;
#99164 = CARTESIAN_POINT('Ctrl Pts',(-19.9518928688603,-16.884205280556,122.325807060645)) ;
#99165 = CARTESIAN_POINT('Ctrl Pts',(-19.6903721435856,-16.8972862280731,
122.230698865878)) ;
#99166 = CARTESIAN_POINT('Ctrl Pts',(-19.4083019370764,-16.9107607263076,
122.205773135081)) ;
#99167 = CARTESIAN_POINT('Ctrl Pts',(-19.2023529385055,-16.9205928299171,
122.223887098564)) ;
#99168 = CARTESIAN_POINT('Ctrl Pts',(-18.999812486702,-16.9305587330438,122.277379743026)) ;
#99169 = CARTESIAN_POINT('Ctrl Pts',(-18.8085487000268,-16.940586142354,122.366089485371)) ;
#99170 = CARTESIAN_POINT('Ctrl Pts',(-18.6376144826563,-16.9504971737206,
122.485180969732)) ;
#99171 = CARTESIAN_POINT('Ctrl Pts',(-18.4395800103084,-16.9637414813416,
122.681031846871)) ;
#99172 = CARTESIAN_POINT('Ctrl Pts',(-18.2607391510961,-16.9804419640128,
122.987662429286)) ;
#99173 = CARTESIAN_POINT('Ctrl Pts',(-18.1977926141964,-16.9969487931686,
123.333078282104)) ;
#99174 = CARTESIAN_POINT('Ctrl Pts',(-18.21996988737,-17.0102594214062,123.61194498674)) ;
#99175 = CARTESIAN_POINT('Ctrl Pts',(-18.2726905014791,-17.0202519849463,
123.815342190681)) ;
#99176 = CARTESIAN_POINT('Ctrl Pts',(-18.3604559458648,-17.0302820679478,
124.007038137918)) ;
#99177 = CARTESIAN_POINT('Ctrl Pts',(-18.5172872049266,-17.0434556719456,
124.235392789729)) ;
#99178 = CARTESIAN_POINT('Ctrl Pts',(-18.7857688583209,-17.060093377177,124.465519405574)) ;
#99179 = CARTESIAN_POINT('Ctrl Pts',(-19.1813867266289,-17.0799751397444,
124.614927197697)) ;
#99180 = CARTESIAN_POINT('Ctrl Pts',(-19.5363104604699,-17.0966714919609,
124.619236224993)) ;
#99181 = CARTESIAN_POINT('Ctrl Pts',(-19.8044222178332,-17.10982851975,124.551190236168)) ;
#99182 = CARTESIAN_POINT('Ctrl Pts',(-20.0610846479586,-17.1232058743935,
124.436239227628)) ;
#99183 = CARTESIAN_POINT('Ctrl Pts',(-20.3337550798783,-17.1397367086523,
124.214393691027)) ;
#99184 = CARTESIAN_POINT('Ctrl Pts',(-20.552444499908,-17.1597013983954,123.850597149284)) ;
#99185 = CARTESIAN_POINT('Ctrl Pts',(-20.6332803463199,-17.1796178918191,
123.43489710999)) ;
#99186 = CARTESIAN_POINT('Ctrl Pts',(-20.5683255521694,-17.1995076111686,
123.016962706715)) ;
#99187 = CARTESIAN_POINT('Ctrl Pts',(-20.3632006229321,-17.2195143408165,
122.644358719004)) ;
#99188 = CARTESIAN_POINT('Ctrl Pts',(-20.0460339730344,-17.2393523944634,
122.366143379611)) ;
#99189 = CARTESIAN_POINT('Ctrl Pts',(-19.6502010706745,-17.259345732677,122.211319441534)) ;
#99190 = CARTESIAN_POINT('Ctrl Pts',(-19.2274811222759,-17.2792285320836,
122.201182920592)) ;
#99191 = CARTESIAN_POINT('Ctrl Pts',(-18.8264483172778,-17.2991207130023,
122.335224657511)) ;
#99192 = CARTESIAN_POINT('Ctrl Pts',(-18.494427195319,-17.3190228914974,122.59779931291)) ;
#99193 = CARTESIAN_POINT('Ctrl Pts',(-18.2711837063155,-17.3390602027011,
122.960542012371)) ;
#99194 = CARTESIAN_POINT('Ctrl Pts',(-18.1854522373414,-17.358872644242,123.37318298385)) ;
#99195 = CARTESIAN_POINT('Ctrl Pts',(-18.2465250493595,-17.3789378849769,
123.795223719384)) ;
#99196 = CARTESIAN_POINT('Ctrl Pts',(-18.4447588511698,-17.3986950898327,
124.165833746942)) ;
#99197 = CARTESIAN_POINT('Ctrl Pts',(-18.7611993809905,-17.4187283624784,
124.45065900879)) ;
#99198 = CARTESIAN_POINT('Ctrl Pts',(-19.151895539613,-17.4385412709322,124.60874609905)) ;
#99199 = CARTESIAN_POINT('Ctrl Pts',(-19.5765780331308,-17.4585374170597,
124.62471106204)) ;
#99200 = CARTESIAN_POINT('Ctrl Pts',(-19.9789205926903,-17.4783991702822,
124.495756813336)) ;
#99201 = CARTESIAN_POINT('Ctrl Pts',(-20.3161959451289,-17.4984676874103,
124.23451737686)) ;
#99202 = CARTESIAN_POINT('Ctrl Pts',(-20.5412459661709,-17.5182985604071,
123.877828564051)) ;
#99203 = CARTESIAN_POINT('Ctrl Pts',(-20.6325581559788,-17.5382204712238,
123.46429428522)) ;
#99204 = CARTESIAN_POINT('Ctrl Pts',(-20.5771055766192,-17.5581499146591,
123.04411437641)) ;
#99205 = CARTESIAN_POINT('Ctrl Pts',(-20.3819898078724,-17.5780595847755,
122.668498755483)) ;
#99206 = CARTESIAN_POINT('Ctrl Pts',(-20.0714043072489,-17.5979329420383,
122.381902372699)) ;
#99207 = CARTESIAN_POINT('Ctrl Pts',(-19.6794131872028,-17.6179244766563,
122.217639354158)) ;
#99208 = CARTESIAN_POINT('Ctrl Pts',(-19.2574583116907,-17.637790094067,122.19695164849)) ;
#99209 = CARTESIAN_POINT('Ctrl Pts',(-18.8513811749437,-17.6577710238952,
122.321792132921)) ;
#99210 = CARTESIAN_POINT('Ctrl Pts',(-18.5132668411587,-17.6777094859784,
122.577558538929)) ;
#99211 = CARTESIAN_POINT('Ctrl Pts',(-18.2826875965841,-17.6976016792001,
122.932201622898)) ;
#99212 = CARTESIAN_POINT('Ctrl Pts',(-18.1868226140581,-17.7175723942355,
123.345774506082)) ;
#99213 = CARTESIAN_POINT('Ctrl Pts',(-18.2367369836848,-17.7373820659016,
123.764115286737)) ;
#99214 = CARTESIAN_POINT('Ctrl Pts',(-18.4277722418755,-17.7573752825927,
124.143707962254)) ;
#99215 = CARTESIAN_POINT('Ctrl Pts',(-18.7346736477837,-17.7772261947891,
124.43373031469)) ;
#99216 = CARTESIAN_POINT('Ctrl Pts',(-19.1263241450421,-17.7973008011081,
124.603166605669)) ;
#99217 = CARTESIAN_POINT('Ctrl Pts',(-19.4769996748503,-17.8138174329915,
124.624023086089)) ;
#99218 = CARTESIAN_POINT('Ctrl Pts',(-19.7517471364402,-17.8271561406856,
124.568109834498)) ;
#99219 = CARTESIAN_POINT('Ctrl Pts',(-19.9444114057768,-17.8369985149939,
124.492567968026)) ;
#99220 = CARTESIAN_POINT('Ctrl Pts',(-20.1249105700444,-17.8470535349766,
124.382584090348)) ;
#99221 = CARTESIAN_POINT('Ctrl Pts',(-20.3337149262914,-17.8602856916342,
124.198802243698)) ;
#99222 = CARTESIAN_POINT('Ctrl Pts',(-20.5299811761327,-17.8769006589793,
123.905006598856)) ;
#99223 = CARTESIAN_POINT('Ctrl Pts',(-20.613922053345,-17.8934952459905,123.562354881372)) ;
#99224 = CARTESIAN_POINT('Ctrl Pts',(-20.6085090197538,-17.9067288143459,
123.284145316307)) ;
#99225 = CARTESIAN_POINT('Ctrl Pts',(-20.5678477375611,-17.9167724321545,
123.076973084474)) ;
#99226 = CARTESIAN_POINT('Ctrl Pts',(-20.4930714664377,-17.9266593563894,
122.883014220121)) ;
#99227 = CARTESIAN_POINT('Ctrl Pts',(-20.3849668276119,-17.9366500108362,
122.702955355308)) ;
#99228 = CARTESIAN_POINT('Ctrl Pts',(-20.2475870495674,-17.9466117692902,
122.544870576556)) ;
#99229 = CARTESIAN_POINT('Ctrl Pts',(-20.0298560619442,-17.9599516343574,
122.368099017691)) ;
#99230 = CARTESIAN_POINT('Ctrl Pts',(-19.7713313632374,-17.9732604172707,
122.253061487403)) ;
#99231 = CARTESIAN_POINT('Ctrl Pts',(-19.4973910422953,-17.9864561747147,
122.2091658422)) ;
#99232 = CARTESIAN_POINT('Ctrl Pts',(-19.2879780352631,-17.9964180583912,
122.211856716464)) ;
#99233 = CARTESIAN_POINT('Ctrl Pts',(-19.0806023133034,-18.0064611679059,
122.251524998746)) ;
#99234 = CARTESIAN_POINT('Ctrl Pts',(-18.886918893878,-18.0163134179051,122.324944160845)) ;
#99235 = CARTESIAN_POINT('Ctrl Pts',(-18.7065327708684,-18.0262849548556,
122.431701962759)) ;
#99236 = CARTESIAN_POINT('Ctrl Pts',(-18.5470138459245,-18.0362802203331,
122.568533539152)) ;
#99237 = CARTESIAN_POINT('Ctrl Pts',(-18.4133926489539,-18.0463141932067,
122.731738687311)) ;
#99238 = CARTESIAN_POINT('Ctrl Pts',(-18.3116707861614,-18.0561696079691,
122.912264137183)) ;
#99239 = CARTESIAN_POINT('Ctrl Pts',(-18.2415826974838,-18.0661688854779,
123.11041408596)) ;
#99240 = CARTESIAN_POINT('Ctrl Pts',(-18.2070923144644,-18.0760640696409,
123.315598951689)) ;
#99241 = CARTESIAN_POINT('Ctrl Pts',(-18.2088036917932,-18.0861244492817,
123.527064316189)) ;
#99242 = CARTESIAN_POINT('Ctrl Pts',(-18.246286472234,-18.0959743182898,123.730739665361)) ;
#99243 = CARTESIAN_POINT('Ctrl Pts',(-18.3194342400498,-18.1060058794977,
123.928528739854)) ;
#99244 = CARTESIAN_POINT('Ctrl Pts',(-18.4259724173369,-18.11601632838,124.110043073467)) ;
#99245 = CARTESIAN_POINT('Ctrl Pts',(-18.5608034636279,-18.125923067797,124.268770670719)) ;
#99246 = CARTESIAN_POINT('Ctrl Pts',(-18.7213893093871,-18.1358610838654,
124.402405362414)) ;
#99247 = CARTESIAN_POINT('Ctrl Pts',(-18.9039272660046,-18.1458663303166,
124.506966401756)) ;
#99248 = CARTESIAN_POINT('Ctrl Pts',(-19.1025083237275,-18.1559003913728,
124.578100104448)) ;
#99249 = CARTESIAN_POINT('Ctrl Pts',(-19.3064701251401,-18.165745472431,124.61335951133)) ;
#99250 = CARTESIAN_POINT('Ctrl Pts',(-19.5163698498164,-18.1757312783845,
124.613051491713)) ;
#99251 = CARTESIAN_POINT('Ctrl Pts',(-19.7220693078652,-18.1856660989387,
124.576625319767)) ;
#99252 = CARTESIAN_POINT('Ctrl Pts',(-19.9206135170437,-18.1957236240709,
124.503998225256)) ;
#99253 = CARTESIAN_POINT('Ctrl Pts',(-20.0994449004582,-18.2055452747222,
124.400734678168)) ;
#99254 = CARTESIAN_POINT('Ctrl Pts',(-20.2616284109122,-18.215601338227,124.265148635079)) ;
#99255 = CARTESIAN_POINT('Ctrl Pts',(-20.395971358036,-18.2255420052909,124.105055283385)) ;
#99256 = CARTESIAN_POINT('Ctrl Pts',(-20.5006583410874,-18.2354463989569,
123.925059619228)) ;
#99257 = CARTESIAN_POINT('Ctrl Pts',(-20.5733969612198,-18.2454929227199,
123.72679071817)) ;
#99258 = CARTESIAN_POINT('Ctrl Pts',(-20.6102547691903,-18.2553890057363,
123.521996954159)) ;
#99259 = CARTESIAN_POINT('Ctrl Pts',(-20.6109546878675,-18.2654557049663,
123.310402216948)) ;
#99260 = CARTESIAN_POINT('Ctrl Pts',(-20.5759989895683,-18.2752793153674,
123.106826891601)) ;
#99261 = CARTESIAN_POINT('Ctrl Pts',(-20.5049472997739,-18.2853351755449,
122.907747144791)) ;
#99262 = CARTESIAN_POINT('Ctrl Pts',(-20.4014240713101,-18.2952683218498,
122.726358495049)) ;
#99263 = CARTESIAN_POINT('Ctrl Pts',(-20.2681766211451,-18.3052135776204,
122.565269677507)) ;
#99264 = CARTESIAN_POINT('Ctrl Pts',(-20.108444651531,-18.3151968760589,122.429084130783)) ;
#99265 = CARTESIAN_POINT('Ctrl Pts',(-19.9264068256941,-18.3252340562055,
122.322397283645)) ;
#99266 = CARTESIAN_POINT('Ctrl Pts',(-19.7322883054911,-18.335088608915,122.249961685163)) ;
#99267 = CARTESIAN_POINT('Ctrl Pts',(-19.5256522325447,-18.3450881273623,
122.211500200816)) ;
#99268 = CARTESIAN_POINT('Ctrl Pts',(-19.3176033221378,-18.3549832098244,
122.20930081902)) ;
#99269 = CARTESIAN_POINT('Ctrl Pts',(-19.108965237349,-18.3650437553305,122.243837245453)) ;
#99270 = CARTESIAN_POINT('Ctrl Pts',(-18.9136030140935,-18.3748930625785,
122.312505387756)) ;
#99271 = CARTESIAN_POINT('Ctrl Pts',(-18.7296291359286,-18.3849201526658,
122.415407130194)) ;
#99272 = CARTESIAN_POINT('Ctrl Pts',(-18.5666314561259,-18.3949490568028,
122.549156082067)) ;
#99273 = CARTESIAN_POINT('Ctrl Pts',(-18.4315663670725,-18.4047929219021,
122.705941999935)) ;
#99274 = CARTESIAN_POINT('Ctrl Pts',(-18.3236932626047,-18.4147887486105,
122.886285416158)) ;
#99275 = CARTESIAN_POINT('Ctrl Pts',(-18.2489130638018,-18.4248139652595,
123.083339173562)) ;
#99276 = CARTESIAN_POINT('Ctrl Pts',(-18.2097414858544,-18.4347037974171,
123.287534573888)) ;
#99277 = CARTESIAN_POINT('Ctrl Pts',(-18.2063008121488,-18.4446946535018,
123.497538646126)) ;
#99278 = CARTESIAN_POINT('Ctrl Pts',(-18.2392644708854,-18.4546397480947,
123.704000419562)) ;
#99279 = CARTESIAN_POINT('Ctrl Pts',(-18.3072547511552,-18.4645916518628,
123.901873676827)) ;
#99280 = CARTESIAN_POINT('Ctrl Pts',(-18.409584917856,-18.4746280513322,124.086389083374)) ;
#99281 = CARTESIAN_POINT('Ctrl Pts',(-18.5403379402418,-18.4845171214209,
124.248032499882)) ;
#99282 = CARTESIAN_POINT('Ctrl Pts',(-18.6985038225338,-18.4945064107918,
124.386177736897)) ;
#99283 = CARTESIAN_POINT('Ctrl Pts',(-18.8777803735944,-18.5044649770015,
124.494293558998)) ;
#99284 = CARTESIAN_POINT('Ctrl Pts',(-19.0717815244749,-18.5143645482183,
124.569677874931)) ;
#99285 = CARTESIAN_POINT('Ctrl Pts',(-19.2789648666435,-18.5244124626325,
124.610759941002)) ;
#99286 = CARTESIAN_POINT('Ctrl Pts',(-19.4869782090201,-18.5343078054931,
124.61534083382)) ;
#99287 = CARTESIAN_POINT('Ctrl Pts',(-19.6960324588586,-18.5443694994405,
124.58324034386)) ;
#99288 = CARTESIAN_POINT('Ctrl Pts',(-19.8920550551004,-18.5542139525247,
124.516818977732)) ;
#99289 = CARTESIAN_POINT('Ctrl Pts',(-20.0760459244368,-18.5641746374831,
124.416850418007)) ;
#99290 = CARTESIAN_POINT('Ctrl Pts',(-20.2409137352254,-18.5742105699917,
124.285180323825)) ;
#99291 = CARTESIAN_POINT('Ctrl Pts',(-20.3785155808731,-18.5840991856797,
124.129353391566)) ;
#99292 = CARTESIAN_POINT('Ctrl Pts',(-20.48871764755,-18.5941135948222,123.949947980869)) ;
#99293 = CARTESIAN_POINT('Ctrl Pts',(-20.5657248006156,-18.60414740378,123.753577893086)) ;
#99294 = CARTESIAN_POINT('Ctrl Pts',(-20.6071923975581,-18.6139778580362,
123.55108919975)) ;
#99295 = CARTESIAN_POINT('Ctrl Pts',(-20.6130809578818,-18.6240555256144,
123.339347401)) ;
#99296 = CARTESIAN_POINT('Ctrl Pts',(-20.582902760328,-18.6339073937366,123.134395538266)) ;
#99297 = CARTESIAN_POINT('Ctrl Pts',(-20.5163228115591,-18.643980431302,122.933405256778)) ;
#99298 = CARTESIAN_POINT('Ctrl Pts',(-20.4181024696244,-18.6538229846528,
122.751261329554)) ;
#99299 = CARTESIAN_POINT('Ctrl Pts',(-20.2885210753734,-18.6638033801463,
122.586249219186)) ;
#99300 = CARTESIAN_POINT('Ctrl Pts',(-20.1313832431075,-18.6738218581241,
122.446011934941)) ;
#99301 = CARTESIAN_POINT('Ctrl Pts',(-19.9549077903807,-18.6837051724301,
122.336291516789)) ;
#99302 = CARTESIAN_POINT('Ctrl Pts',(-19.7584730123952,-18.6937734749689,
122.25754001902)) ;
#99303 = CARTESIAN_POINT('Ctrl Pts',(-19.556232273998,-18.7036035222423,122.214866321465)) ;
#99304 = CARTESIAN_POINT('Ctrl Pts',(-19.3447577100388,-18.7136703936578,
122.207524272249)) ;
#99305 = CARTESIAN_POINT('Ctrl Pts',(-19.1388736488503,-18.7235594324569,
122.236610948676)) ;
#99306 = CARTESIAN_POINT('Ctrl Pts',(-18.9389372923617,-18.733556130591,122.301297571124)) ;
#99307 = CARTESIAN_POINT('Ctrl Pts',(-18.7541016123129,-18.7435085563029,
122.399376155892)) ;
#99308 = CARTESIAN_POINT('Ctrl Pts',(-18.5891329718093,-18.7534498585359,
122.527667437495)) ;
#99309 = CARTESIAN_POINT('Ctrl Pts',(-18.4481604174868,-18.7634330976198,
122.683186439299)) ;
#99310 = CARTESIAN_POINT('Ctrl Pts',(-18.3360106457652,-18.7734718991884,
122.861948263678)) ;
#99311 = CARTESIAN_POINT('Ctrl Pts',(-18.2577237712713,-18.78332000531,123.05363441793)) ;
#99312 = CARTESIAN_POINT('Ctrl Pts',(-18.2127797984057,-18.7933802008854,
123.26028308256)) ;
#99313 = CARTESIAN_POINT('Ctrl Pts',(-18.2047236232763,-18.8032778841968,
123.468215807643)) ;
#99314 = CARTESIAN_POINT('Ctrl Pts',(-18.232308200635,-18.8132089245708,123.675163356788)) ;
#99315 = CARTESIAN_POINT('Ctrl Pts',(-18.2963305132176,-18.8232511422274,
123.876337750937)) ;
#99316 = CARTESIAN_POINT('Ctrl Pts',(-18.3926662074323,-18.8331378029614,
124.060523596312)) ;
#99317 = CARTESIAN_POINT('Ctrl Pts',(-18.5205935024228,-18.8431309115638,
124.227156296495)) ;
#99318 = CARTESIAN_POINT('Ctrl Pts',(-18.6748368622049,-18.8530766102021,
124.368321248557)) ;
#99319 = CARTESIAN_POINT('Ctrl Pts',(-18.8510538196153,-18.8630238324731,
124.48094398264)) ;
#99320 = CARTESIAN_POINT('Ctrl Pts',(-19.046181766046,-18.8730718580533,124.561846138917)) ;
#99321 = CARTESIAN_POINT('Ctrl Pts',(-19.2482397187317,-18.8829191051962,
124.606896824179)) ;
#99322 = CARTESIAN_POINT('Ctrl Pts',(-19.4574511334665,-18.8928822822869,
124.616949965162)) ;
#99323 = CARTESIAN_POINT('Ctrl Pts',(-19.6665802279663,-18.9029120033203,
124.590031806156)) ;
#99324 = CARTESIAN_POINT('Ctrl Pts',(-19.8654407164327,-18.9128164708532,
124.528232706635)) ;
#99325 = CARTESIAN_POINT('Ctrl Pts',(-20.0527877669274,-18.922840956683,124.431771226548)) ;
#99326 = CARTESIAN_POINT('Ctrl Pts',(-20.2186677554441,-18.9327447918069,
124.305885683981)) ;
#99327 = CARTESIAN_POINT('Ctrl Pts',(-20.3622739072169,-18.9427959825169,
124.150907456591)) ;
#99328 = CARTESIAN_POINT('Ctrl Pts',(-20.4749461011622,-18.9526804251752,
123.976278851929)) ;
#99329 = CARTESIAN_POINT('Ctrl Pts',(-20.5568157650928,-18.962673433027,123.78282343957)) ;
#99330 = CARTESIAN_POINT('Ctrl Pts',(-20.6035788977904,-18.9726217527433,
123.578959645628)) ;
#99331 = CARTESIAN_POINT('Ctrl Pts',(-20.6145188710685,-18.9825585914528,
123.37036111914)) ;
#99332 = CARTESIAN_POINT('Ctrl Pts',(-20.589212232289,-18.9925415803724,123.161991377442)) ;
#99333 = CARTESIAN_POINT('Ctrl Pts',(-20.5273804622031,-19.0025854597365,
122.96011896677)) ;
#99334 = CARTESIAN_POINT('Ctrl Pts',(-20.4339101946007,-19.0124135250949,
122.77581699888)) ;
#99335 = CARTESIAN_POINT('Ctrl Pts',(-20.3068358614909,-19.0224906136498,
122.606366147601)) ;
#99336 = CARTESIAN_POINT('Ctrl Pts',(-20.1557713245553,-19.0323407658061,
122.464647188933)) ;
#99337 = CARTESIAN_POINT('Ctrl Pts',(-19.9784770787633,-19.0424212462584,
122.348647952787)) ;
#99338 = CARTESIAN_POINT('Ctrl Pts',(-19.788854482648,-19.0522357440273,122.267192152771)) ;
#99339 = CARTESIAN_POINT('Ctrl Pts',(-19.5829445361139,-19.0623040400474,
122.218373125658)) ;
#99340 = CARTESIAN_POINT('Ctrl Pts',(-19.3751375053277,-19.0722028725302,
122.206308011531)) ;
#99341 = CARTESIAN_POINT('Ctrl Pts',(-19.1652616283384,-19.0822557525447,
122.230802022399)) ;
#99342 = CARTESIAN_POINT('Ctrl Pts',(-18.9663763468156,-19.0921255680409,
122.290099668272)) ;
#99343 = CARTESIAN_POINT('Ctrl Pts',(-18.7770383310176,-19.1021982491237,
122.38485181426)) ;
#99344 = CARTESIAN_POINT('Ctrl Pts',(-18.6109895737395,-19.1120307276946,
122.507998067796)) ;
#99345 = CARTESIAN_POINT('Ctrl Pts',(-18.4655594712225,-19.1220613616807,
122.660691104319)) ;
#99346 = CARTESIAN_POINT('Ctrl Pts',(-18.349343398378,-19.1320929188999,122.836690060582)) ;
#99347 = CARTESIAN_POINT('Ctrl Pts',(-18.2667541318604,-19.1419226277716,
123.026104598747)) ;
#99348 = CARTESIAN_POINT('Ctrl Pts',(-18.2169065980263,-19.1519120765737,
123.230119020484)) ;
#99349 = CARTESIAN_POINT('Ctrl Pts',(-18.2037005085259,-19.1619559289737,
123.440857004451)) ;
#99350 = CARTESIAN_POINT('Ctrl Pts',(-18.2263400159674,-19.1717776423058,
123.64609476695)) ;
#99351 = CARTESIAN_POINT('Ctrl Pts',(-18.2850324786468,-19.1818126472945,
123.848732790107)) ;
#99352 = CARTESIAN_POINT('Ctrl Pts',(-18.3784519437941,-19.1918374857421,
124.037658539047)) ;
#99353 = CARTESIAN_POINT('Ctrl Pts',(-18.5007451863381,-19.2016896986973,
124.204825795845)) ;
#99354 = CARTESIAN_POINT('Ctrl Pts',(-18.6520376571185,-19.2116796548911,
124.350470474927)) ;
#99355 = CARTESIAN_POINT('Ctrl Pts',(-18.8252508954375,-19.2216077651743,
124.466935243607)) ;
#99356 = CARTESIAN_POINT('Ctrl Pts',(-19.0170807390467,-19.2315963652539,
124.552376207305)) ;
#99357 = CARTESIAN_POINT('Ctrl Pts',(-19.2216757118603,-19.2416229571814,
124.603121646828)) ;
#99358 = CARTESIAN_POINT('Ctrl Pts',(-19.4289827253932,-19.2515080852456,
124.617585297945)) ;
#99359 = CARTESIAN_POINT('Ctrl Pts',(-19.6379309811041,-19.2614992027191,
124.596074975299)) ;
#99360 = CARTESIAN_POINT('Ctrl Pts',(-19.8408408717167,-19.2715398185709,
124.537900611631)) ;
#99361 = CARTESIAN_POINT('Ctrl Pts',(-20.0267914789812,-19.2813728094246,
124.447599731047)) ;
#99362 = CARTESIAN_POINT('Ctrl Pts',(-20.1973182354438,-19.2913659408749,
124.32489768278)) ;
#99363 = CARTESIAN_POINT('Ctrl Pts',(-20.344215288086,-19.3013979893103,124.173548746077)) ;
#99364 = CARTESIAN_POINT('Ctrl Pts',(-20.4608333198919,-19.3112632358527,
124.002055700407)) ;
#99365 = CARTESIAN_POINT('Ctrl Pts',(-20.547284865377,-19.3212251106795,123.81129491968)) ;
#99366 = CARTESIAN_POINT('Ctrl Pts',(-20.5993432776528,-19.3312600737908,
123.60686431608)) ;
#99367 = CARTESIAN_POINT('Ctrl Pts',(-20.6152338875009,-19.3411449182532,
123.399631879616)) ;
#99368 = CARTESIAN_POINT('Ctrl Pts',(-20.5944804099078,-19.3512109710939,
123.189068844725)) ;
#99369 = CARTESIAN_POINT('Ctrl Pts',(-20.5389790680612,-19.3610484870029,
122.989799972099)) ;
#99370 = CARTESIAN_POINT('Ctrl Pts',(-20.4478587685214,-19.3711172351118,
122.798779782253)) ;
#99371 = CARTESIAN_POINT('Ctrl Pts',(-20.3271508539874,-19.3809977521428,
122.629693362415)) ;
#99372 = CARTESIAN_POINT('Ctrl Pts',(-20.1776005275586,-19.3909889390772,
122.482244406539)) ;
#99373 = CARTESIAN_POINT('Ctrl Pts',(-20.0053468870928,-19.4009420053522,
122.363394242763)) ;
#99374 = CARTESIAN_POINT('Ctrl Pts',(-19.8135070670267,-19.4109778428848,
122.275616759111)) ;
#99375 = CARTESIAN_POINT('Ctrl Pts',(-19.6123108253215,-19.4208679690962,
122.223108779778)) ;
#99376 = CARTESIAN_POINT('Ctrl Pts',(-19.4029666689472,-19.4308601510042,
122.205825287568)) ;
#99377 = CARTESIAN_POINT('Ctrl Pts',(-19.1947651157361,-19.4408060909428,
122.225135232897)) ;
#99378 = CARTESIAN_POINT('Ctrl Pts',(-18.9929315302296,-19.4507532747068,
122.279902900179)) ;
#99379 = CARTESIAN_POINT('Ctrl Pts',(-18.8018734361418,-19.4608012130143,
122.369991201364)) ;
#99380 = CARTESIAN_POINT('Ctrl Pts',(-18.6326906138696,-19.4706488477546,
122.489316984808)) ;
#99381 = CARTESIAN_POINT('Ctrl Pts',(-18.4846495795059,-19.4806105617284,
122.637436199205)) ;
#99382 = CARTESIAN_POINT('Ctrl Pts',(-18.3639748906232,-19.4906391965192,
122.810334890515)) ;
#99383 = CARTESIAN_POINT('Ctrl Pts',(-18.2761502384956,-19.5005495151164,
122.999255239059)) ;
#99384 = CARTESIAN_POINT('Ctrl Pts',(-18.2217946833003,-19.5104843714279,
123.20092836226)) ;
#99385 = CARTESIAN_POINT('Ctrl Pts',(-18.2032878692115,-19.5205256073886,
123.4112041524)) ;
#99386 = CARTESIAN_POINT('Ctrl Pts',(-18.2211226486538,-19.5304123789686,
123.618309023476)) ;
#99387 = CARTESIAN_POINT('Ctrl Pts',(-18.275002195084,-19.5404125576748,123.821490956925)) ;
#99388 = CARTESIAN_POINT('Ctrl Pts',(-18.3624737997359,-19.5503298358844,
124.010785275748)) ;
#99389 = CARTESIAN_POINT('Ctrl Pts',(-18.483060444576,-19.560377082298,124.184170472808)) ;
#99390 = CARTESIAN_POINT('Ctrl Pts',(-18.6292379697869,-19.5702509712793,
124.331599090875)) ;
#99391 = CARTESIAN_POINT('Ctrl Pts',(-18.8019088757238,-19.5803129888599,
124.453750363811)) ;
#99392 = CARTESIAN_POINT('Ctrl Pts',(-18.9895857136376,-19.5901840505942,
124.542341706941)) ;
#99393 = CARTESIAN_POINT('Ctrl Pts',(-19.1921191318972,-19.6001781139545,
124.598242963255)) ;
#99394 = CARTESIAN_POINT('Ctrl Pts',(-19.4021178235081,-19.6102102719879,
124.617737810741)) ;
#99395 = CARTESIAN_POINT('Ctrl Pts',(-19.60885022585,-19.620074148228,124.601214016186)) ;
#99396 = CARTESIAN_POINT('Ctrl Pts',(-19.8137388217969,-19.6301446628663,
124.547988032572)) ;
#99397 = CARTESIAN_POINT('Ctrl Pts',(-20.0019235290395,-19.6399852998073,
124.462005162133)) ;
#99398 = CARTESIAN_POINT('Ctrl Pts',(-20.1748742226983,-19.6499524286475,
124.343734642557)) ;
#99399 = CARTESIAN_POINT('Ctrl Pts',(-20.3252319606434,-19.659966401772,124.196364097471)) ;
#99400 = CARTESIAN_POINT('Ctrl Pts',(-20.4877985891898,-19.6732511356353,
123.969234284442)) ;
#99401 = CARTESIAN_POINT('Ctrl Pts',(-20.5871267471998,-19.68647640035,123.706173989786)) ;
#99402 = CARTESIAN_POINT('Ctrl Pts',(-20.6152290402165,-19.6997869229049,
123.427775442869)) ;
#99403 = CARTESIAN_POINT('Ctrl Pts',(-20.5994928169475,-19.7098155678071,
123.217527900628)) ;
#99404 = CARTESIAN_POINT('Ctrl Pts',(-20.5484314466191,-19.719696600161,123.016168192722)) ;
#99405 = CARTESIAN_POINT('Ctrl Pts',(-20.4627206601069,-19.7296775728411,
122.824640804872)) ;
#99406 = CARTESIAN_POINT('Ctrl Pts',(-20.3449158860642,-19.7396587004271,
122.651015512196)) ;
#99407 = CARTESIAN_POINT('Ctrl Pts',(-20.1513346859303,-19.7529018906885,
122.450805211649)) ;
#99408 = CARTESIAN_POINT('Ctrl Pts',(-19.8474852356226,-19.7695698860493,
122.268618426649)) ;
#99409 = CARTESIAN_POINT('Ctrl Pts',(-19.5025941864014,-19.7860903860613,
122.201353738697)) ;
#99410 = CARTESIAN_POINT('Ctrl Pts',(-19.2234378604732,-19.7994034023773,
122.220278401907)) ;
#99411 = CARTESIAN_POINT('Ctrl Pts',(-19.0209391211837,-19.8093199606103,
122.270033891639)) ;
#99412 = CARTESIAN_POINT('Ctrl Pts',(-18.8281393510094,-19.8193476289132,
122.355168877401)) ;
#99413 = CARTESIAN_POINT('Ctrl Pts',(-18.5974709403945,-19.8325282186578,
122.508922361254)) ;
#99414 = CARTESIAN_POINT('Ctrl Pts',(-18.3626797203254,-19.8492763577772,
122.776419833526)) ;
#99415 = CARTESIAN_POINT('Ctrl Pts',(-18.2093485760041,-19.8690711002878,
123.168602453068)) ;
#99416 = CARTESIAN_POINT('Ctrl Pts',(-18.1985006752077,-19.8891154930966,
123.594513754046)) ;
#99417 = CARTESIAN_POINT('Ctrl Pts',(-18.3326934538561,-19.9089546753953,
123.994555115207)) ;
#99418 = CARTESIAN_POINT('Ctrl Pts',(-18.5955320180039,-19.9288799990882,
124.326702902685)) ;
#99419 = CARTESIAN_POINT('Ctrl Pts',(-18.956082418232,-19.9488036371397,124.549244784898)) ;
#99420 = CARTESIAN_POINT('Ctrl Pts',(-19.3708156632894,-19.9687285106052,
124.635502195262)) ;
#99421 = CARTESIAN_POINT('Ctrl Pts',(-19.7892668039668,-19.9886071176841,
124.57573076847)) ;
#99422 = CARTESIAN_POINT('Ctrl Pts',(-20.1641243491407,-20.0085845605161,
124.375961483469)) ;
#99423 = CARTESIAN_POINT('Ctrl Pts',(-20.4474718656203,-20.0285164086008,
124.060750203232)) ;
#99424 = CARTESIAN_POINT('Ctrl Pts',(-20.6063139039005,-20.0484116769434,
123.668704752711)) ;
#99425 = CARTESIAN_POINT('Ctrl Pts',(-20.6223315894437,-20.0683341753555,
123.245390722407)) ;
#99426 = CARTESIAN_POINT('Ctrl Pts',(-20.4925827338842,-20.0882936572315,
122.841292761768)) ;
#99427 = CARTESIAN_POINT('Ctrl Pts',(-20.2339043814148,-20.1081714096908,
122.507125870931)) ;
#99428 = CARTESIAN_POINT('Ctrl Pts',(-19.8771666497164,-20.1280532004254,
122.280149017489)) ;
#99429 = CARTESIAN_POINT('Ctrl Pts',(-19.4603683816316,-20.1481265392764,
122.188512156608)) ;
#99430 = CARTESIAN_POINT('Ctrl Pts',(-19.0428240144052,-20.1679310065122,
122.243764222499)) ;
#99431 = CARTESIAN_POINT('Ctrl Pts',(-18.6655193205356,-20.18791434692,122.439036366789)) ;
#99432 = CARTESIAN_POINT('Ctrl Pts',(-18.378944103388,-20.207829311518,122.750776767031)) ;
#99433 = CARTESIAN_POINT('Ctrl Pts',(-18.2152095070376,-20.2276978462343,
123.14030325011)) ;
#99434 = CARTESIAN_POINT('Ctrl Pts',(-18.194735718625,-20.2477502304461,123.566054362886)) ;
#99435 = CARTESIAN_POINT('Ctrl Pts',(-18.3185727849557,-20.2675241942353,
123.968029304062)) ;
#99436 = CARTESIAN_POINT('Ctrl Pts',(-18.5752735116453,-20.2875785732566,
124.308301037845)) ;
#99437 = CARTESIAN_POINT('Ctrl Pts',(-18.9284268704818,-20.3073753108299,
124.537586373438)) ;
#99438 = CARTESIAN_POINT('Ctrl Pts',(-19.3416860056703,-20.3273431231813,
124.634515293149)) ;
#99439 = CARTESIAN_POINT('Ctrl Pts',(-19.7631262365245,-20.3473020992464,
124.583944380649)) ;
#99440 = CARTESIAN_POINT('Ctrl Pts',(-20.1408299891448,-20.3671970175238,
124.393492184598)) ;
#99441 = CARTESIAN_POINT('Ctrl Pts',(-20.4312553316077,-20.3870933299741,
124.08593537269)) ;
#99442 = CARTESIAN_POINT('Ctrl Pts',(-20.5998518999724,-20.4070012633482,
123.697630560032)) ;
#99443 = CARTESIAN_POINT('Ctrl Pts',(-20.6258245093442,-20.4269511536367,
123.274274473307)) ;
#99444 = CARTESIAN_POINT('Ctrl Pts',(-20.5065978280721,-20.446828384138,122.868753359327)) ;
#99445 = CARTESIAN_POINT('Ctrl Pts',(-20.2550275405402,-20.466811053009,122.526376016071)) ;
#99446 = CARTESIAN_POINT('Ctrl Pts',(-19.9023835176968,-20.4867439395894,
122.291183316406)) ;
#99447 = CARTESIAN_POINT('Ctrl Pts',(-19.4912070240972,-20.5066566856073,
122.190296734046)) ;
#99448 = CARTESIAN_POINT('Ctrl Pts',(-19.1409158279758,-20.5232264069491,
122.227731110961)) ;
#99449 = CARTESIAN_POINT('Ctrl Pts',(-18.8799588153574,-20.5365264182541,
122.328242534721)) ;
#99450 = CARTESIAN_POINT('Ctrl Pts',(-18.6408172004457,-20.549796606004,122.47183213169)) ;
#99451 = CARTESIAN_POINT('Ctrl Pts',(-18.394934203615,-20.5664239883694,122.725969038816)) ;
#99452 = CARTESIAN_POINT('Ctrl Pts',(-18.2507664374242,-20.5830462781146,
123.04861816816)) ;
#99453 = CARTESIAN_POINT('Ctrl Pts',(-18.2066181220842,-20.5962914925091,
123.323576700989)) ;
#99454 = CARTESIAN_POINT('Ctrl Pts',(-18.209201949241,-20.6062034574698,123.531950135799)) ;
#99455 = CARTESIAN_POINT('Ctrl Pts',(-18.2487326234934,-20.6162620806342,
123.739663863355)) ;
#99456 = CARTESIAN_POINT('Ctrl Pts',(-18.321833023747,-20.62610219475,123.933220836106)) ;
#99457 = CARTESIAN_POINT('Ctrl Pts',(-18.4296380816943,-20.6361679797077,
124.115280083265)) ;
#99458 = CARTESIAN_POINT('Ctrl Pts',(-18.565025394748,-20.6460512974956,124.272929877172)) ;
#99459 = CARTESIAN_POINT('Ctrl Pts',(-18.7271272469446,-20.6560407353541,
124.406415176552)) ;
#99460 = CARTESIAN_POINT('Ctrl Pts',(-18.9095372660013,-20.6660044494069,
124.509410291724)) ;
#99461 = CARTESIAN_POINT('Ctrl Pts',(-19.1076118068024,-20.6759994610661,
124.57959779033)) ;
#99462 = CARTESIAN_POINT('Ctrl Pts',(-19.3157493336726,-20.6860357527603,
124.614140462832)) ;
#99463 = CARTESIAN_POINT('Ctrl Pts',(-19.5227562056662,-20.6958821304538,
124.612396672406)) ;
#99464 = CARTESIAN_POINT('Ctrl Pts',(-19.7292111708807,-20.7058670746045,
124.574608760862)) ;
#99465 = CARTESIAN_POINT('Ctrl Pts',(-19.9251254485163,-20.7158040457344,
124.501991071344)) ;
#99466 = CARTESIAN_POINT('Ctrl Pts',(-20.1073988536891,-20.7258538303662,
124.395191797424)) ;
#99467 = CARTESIAN_POINT('Ctrl Pts',(-20.2652964301104,-20.7357042924436,
124.261177002087)) ;
#99468 = CARTESIAN_POINT('Ctrl Pts',(-20.3995514510502,-20.7456763059641,
124.100196464847)) ;
#99469 = CARTESIAN_POINT('Ctrl Pts',(-20.5040635942811,-20.7556714530835,
123.917862077342)) ;
#99470 = CARTESIAN_POINT('Ctrl Pts',(-20.5753478626825,-20.7657054228196,
123.719345015492)) ;
#99471 = CARTESIAN_POINT('Ctrl Pts',(-20.6107721846466,-20.7755609684902,
123.51518156139)) ;
#99472 = CARTESIAN_POINT('Ctrl Pts',(-20.6104965949966,-20.7855597255034,
123.30501028613)) ;
#99473 = CARTESIAN_POINT('Ctrl Pts',(-20.5742911195978,-20.7954568607406,
123.100083967225)) ;
#99474 = CARTESIAN_POINT('Ctrl Pts',(-20.5019849733934,-20.8055099565802,
122.901512715217)) ;
#99475 = CARTESIAN_POINT('Ctrl Pts',(-20.3980814652501,-20.8153934653108,
122.721558488357)) ;
#99476 = CARTESIAN_POINT('Ctrl Pts',(-20.263395591003,-20.8253883379569,122.56028534315)) ;
#99477 = CARTESIAN_POINT('Ctrl Pts',(-20.1021248524995,-20.8354082995926,
122.424747058563)) ;
#99478 = CARTESIAN_POINT('Ctrl Pts',(-19.921956015776,-20.8453136633924,122.320331601474)) ;
#99479 = CARTESIAN_POINT('Ctrl Pts',(-19.725855765747,-20.855254251,122.248133909939)) ;
#99480 = CARTESIAN_POINT('Ctrl Pts',(-19.518894597609,-20.8652570691006,122.210725271242)) ;
#99481 = CARTESIAN_POINT('Ctrl Pts',(-19.3079457697242,-20.8752917808248,
122.210161245103)) ;
#99482 = CARTESIAN_POINT('Ctrl Pts',(-19.1039507333,-20.8851366875621,122.245209735339)) ;
#99483 = CARTESIAN_POINT('Ctrl Pts',(-18.9062616113821,-20.8951225401311,
122.31575973506)) ;
#99484 = CARTESIAN_POINT('Ctrl Pts',(-18.7246214892623,-20.9050573485441,
122.418938875796)) ;
#99485 = CARTESIAN_POINT('Ctrl Pts',(-18.561841162844,-20.9151148756252,122.553835370837)) ;
#99486 = CARTESIAN_POINT('Ctrl Pts',(-18.427891530097,-20.9249365306223,122.711002696304)) ;
#99487 = CARTESIAN_POINT('Ctrl Pts',(-18.3204489264364,-20.9349925747953,
122.893054738965)) ;
#99488 = CARTESIAN_POINT('Ctrl Pts',(-18.2474436154527,-20.9449333148405,
123.088883548636)) ;
#99489 = CARTESIAN_POINT('Ctrl Pts',(-18.2090477920976,-20.9548374359133,
123.29353111196)) ;
#99490 = CARTESIAN_POINT('Ctrl Pts',(-18.2068652482952,-20.9648849770676,
123.504735999368)) ;
#99491 = CARTESIAN_POINT('Ctrl Pts',(-18.2407324436048,-20.974783728668,123.710092331499)) ;
#99492 = CARTESIAN_POINT('Ctrl Pts',(-18.3106819819032,-20.9848322076338,
123.909401519179)) ;
#99493 = CARTESIAN_POINT('Ctrl Pts',(-18.4125254527133,-20.9947197047175,
124.090634271952)) ;
#99494 = CARTESIAN_POINT('Ctrl Pts',(-18.5453697794472,-21.0047127950156,
124.253363731307)) ;
#99495 = CARTESIAN_POINT('Ctrl Pts',(-18.7038706520059,-21.0146649650759,
124.389958775153)) ;
#99496 = CARTESIAN_POINT('Ctrl Pts',(-18.8832629433911,-21.0246033849904,
124.497042472193)) ;
#99497 = CARTESIAN_POINT('Ctrl Pts',(-19.0793903123972,-21.034588515076,124.571934115704)) ;
#99498 = CARTESIAN_POINT('Ctrl Pts',(-19.2866320145112,-21.0446252044901,
124.611524785214)) ;
#99499 = CARTESIAN_POINT('Ctrl Pts',(-19.4938007367227,-21.0544798884826,
124.614806296443)) ;
#99500 = CARTESIAN_POINT('Ctrl Pts',(-19.7013905047255,-21.0644793725304,
124.58188080799)) ;
#99501 = CARTESIAN_POINT('Ctrl Pts',(-19.8981741001193,-21.0743744613073,
124.514312934719)) ;
#99502 = CARTESIAN_POINT('Ctrl Pts',(-20.0832161414479,-21.0844350159535,
124.411930701688)) ;
#99503 = CARTESIAN_POINT('Ctrl Pts',(-20.2443229986613,-21.0942842803264,
124.281830742076)) ;
#99504 = CARTESIAN_POINT('Ctrl Pts',(-20.3832402412749,-21.1043115327742,
124.123279767756)) ;
#99505 = CARTESIAN_POINT('Ctrl Pts',(-20.4920625671697,-21.1143398303444,
123.942698364555)) ;
#99506 = CARTESIAN_POINT('Ctrl Pts',(-20.5668644588155,-21.1241859593504,
123.749699487049)) ;
#99507 = CARTESIAN_POINT('Ctrl Pts',(-20.6081396038319,-21.1341798647124,
123.543691058258)) ;
#99508 = CARTESIAN_POINT('Ctrl Pts',(-20.6126551695877,-21.1442039623955,
123.332995679603)) ;
#99509 = CARTESIAN_POINT('Ctrl Pts',(-20.5812076422708,-21.1540937902495,
123.127469067177)) ;
#99510 = CARTESIAN_POINT('Ctrl Pts',(-20.5141570119894,-21.1640857716799,
122.928403453829)) ;
#99511 = CARTESIAN_POINT('Ctrl Pts',(-20.4139656530443,-21.1740327764458,
122.744850138733)) ;
#99512 = CARTESIAN_POINT('Ctrl Pts',(-20.2836858888149,-21.1839824278356,
122.581191682877)) ;
#99513 = CARTESIAN_POINT('Ctrl Pts',(-20.1254894870367,-21.194019430813,122.441562342392)) ;
#99514 = CARTESIAN_POINT('Ctrl Pts',(-19.9481736001043,-21.203908339248,122.33301377474)) ;
#99515 = CARTESIAN_POINT('Ctrl Pts',(-19.7528897175657,-21.2138976717255,
122.255780017016)) ;
#99516 = CARTESIAN_POINT('Ctrl Pts',(-19.5477653161879,-21.2238562271626,
122.213910828471)) ;
#99517 = CARTESIAN_POINT('Ctrl Pts',(-19.3397218993329,-21.2337557983631,
122.207813426892)) ;
#99518 = CARTESIAN_POINT('Ctrl Pts',(-19.130738656835,-21.2438037236151,122.238452332836)) ;
#99519 = CARTESIAN_POINT('Ctrl Pts',(-18.9331920064937,-21.2536990231411,
122.303763604084)) ;
#99520 = CARTESIAN_POINT('Ctrl Pts',(-18.7469406192402,-21.263760879589,122.403992352658)) ;
#99521 = CARTESIAN_POINT('Ctrl Pts',(-18.5844660296623,-21.2736047260057,
122.53218624934)) ;
#99522 = CARTESIAN_POINT('Ctrl Pts',(-18.4445262947739,-21.2835676751337,
122.688016080046)) ;
#99523 = CARTESIAN_POINT('Ctrl Pts',(-18.333265179863,-21.2936017115617,122.867242963847)) ;
#99524 = CARTESIAN_POINT('Ctrl Pts',(-18.2557608886967,-21.3034891385198,
123.060114884469)) ;
#99525 = CARTESIAN_POINT('Ctrl Pts',(-18.2119773200861,-21.3135035728562,
123.266061490478)) ;
#99526 = CARTESIAN_POINT('Ctrl Pts',(-18.2051328159796,-21.3235385174911,
123.476902517083)) ;
#99527 = CARTESIAN_POINT('Ctrl Pts',(-18.2338429477955,-21.3333708675221,
123.681630907638)) ;
#99528 = CARTESIAN_POINT('Ctrl Pts',(-18.2991641208712,-21.3434463066393,
123.883082579957)) ;
#99529 = CARTESIAN_POINT('Ctrl Pts',(-18.3962071485922,-21.3532987718739,
124.066122341709)) ;
#99530 = CARTESIAN_POINT('Ctrl Pts',(-18.5262236980694,-21.3633716494508,
124.233228409853)) ;
#99531 = CARTESIAN_POINT('Ctrl Pts',(-18.6797475455815,-21.3732142456433,
124.371988495187)) ;
#99532 = CARTESIAN_POINT('Ctrl Pts',(-18.8570886147005,-21.3831946297586,
124.48410636434)) ;
#99533 = CARTESIAN_POINT('Ctrl Pts',(-19.0521035724344,-21.3932131104074,
124.563654855738)) ;
#99534 = CARTESIAN_POINT('Ctrl Pts',(-19.2551257739416,-21.4030964254077,
124.607973945122)) ;
#99535 = CARTESIAN_POINT('Ctrl Pts',(-19.4665891744947,-21.4131647224982,
124.616429420007)) ;
#99536 = CARTESIAN_POINT('Ctrl Pts',(-19.6714489368059,-21.4229947908705,
124.588945544384)) ;
#99537 = CARTESIAN_POINT('Ctrl Pts',(-19.8731768207665,-21.4330615833389,
124.525074750821)) ;
#99538 = CARTESIAN_POINT('Ctrl Pts',(-20.0574667598914,-21.4429509168274,
124.428757618369)) ;
#99539 = CARTESIAN_POINT('Ctrl Pts',(-20.2242553472925,-21.4529530482435,
124.300765564857)) ;
#99540 = CARTESIAN_POINT('Ctrl Pts',(-20.3653246670734,-21.4628769178645,
124.147006881623)) ;
#99541 = CARTESIAN_POINT('Ctrl Pts',(-20.4788172016488,-21.4729204333817,
123.968992935367)) ;
#99542 = CARTESIAN_POINT('Ctrl Pts',(-20.5586276546259,-21.48280264627,123.777137744705)) ;
#99543 = CARTESIAN_POINT('Ctrl Pts',(-20.6047443187928,-21.4928707234894,
123.570599790388)) ;
#99544 = CARTESIAN_POINT('Ctrl Pts',(-20.6142702682855,-21.5027092282236,
123.363949181152)) ;
#99545 = CARTESIAN_POINT('Ctrl Pts',(-20.5874714843295,-21.512771996653,123.154128174873)) ;
#99546 = CARTESIAN_POINT('Ctrl Pts',(-20.5254553914185,-21.5226689899357,
122.955506847117)) ;
#99547 = CARTESIAN_POINT('Ctrl Pts',(-20.4301916539881,-21.5326002175705,
122.769727332739)) ;
#99548 = CARTESIAN_POINT('Ctrl Pts',(-20.3025228537875,-21.5426423762126,
122.601589170386)) ;
#99549 = CARTESIAN_POINT('Ctrl Pts',(-20.1500910021351,-21.5525290857437,
122.460275050097)) ;
#99550 = CARTESIAN_POINT('Ctrl Pts',(-19.973768618933,-21.5625220581723,122.346075103576)) ;
#99551 = CARTESIAN_POINT('Ctrl Pts',(-19.7811612033928,-21.5724682527089,
122.264687819142)) ;
#99552 = CARTESIAN_POINT('Ctrl Pts',(-19.5774463713409,-21.5824136275604,
122.217531674259)) ;
#99553 = CARTESIAN_POINT('Ctrl Pts',(-19.3663628261567,-21.5924685469203,
122.206670484406)) ;
#99554 = CARTESIAN_POINT('Ctrl Pts',(-19.1613711508948,-21.6022900663638,
122.231635675794)) ;
#99555 = CARTESIAN_POINT('Ctrl Pts',(-18.9589018263288,-21.6123558351307,
122.293046547694)) ;
#99556 = CARTESIAN_POINT('Ctrl Pts',(-18.7732093967951,-21.6222577567857,
122.387219902228)) ;
#99557 = CARTESIAN_POINT('Ctrl Pts',(-18.6042493045324,-21.6323008156068,
122.513803005883)) ;
#99558 = CARTESIAN_POINT('Ctrl Pts',(-18.4618697995582,-21.6422068096495,
122.665791835697)) ;
#99559 = CARTESIAN_POINT('Ctrl Pts',(-18.3471676674249,-21.6521445827313,
122.840411207979)) ;
#99560 = CARTESIAN_POINT('Ctrl Pts',(-18.2638835645742,-21.6621849464636,
123.034362297601)) ;
#99561 = CARTESIAN_POINT('Ctrl Pts',(-18.2161214585187,-21.6720722901871,
123.236674089419)) ;
#99562 = CARTESIAN_POINT('Ctrl Pts',(-18.2037418784335,-21.6820645207558,
123.446362867399)) ;
#99563 = CARTESIAN_POINT('Ctrl Pts',(-18.2279129398473,-21.6920130485394,
123.654122577843)) ;
#99564 = CARTESIAN_POINT('Ctrl Pts',(-18.2874294786073,-21.7019498322627,
123.854348921147)) ;
#99565 = CARTESIAN_POINT('Ctrl Pts',(-18.3810239655157,-21.7119328330596,
124.042227799406)) ;
#99566 = CARTESIAN_POINT('Ctrl Pts',(-18.5068623001527,-21.7219767199004,
124.21175777701)) ;
#99567 = CARTESIAN_POINT('Ctrl Pts',(-18.6566314086409,-21.7318047434749,
124.354140474258)) ;
#99568 = CARTESIAN_POINT('Ctrl Pts',(-18.8330992281218,-21.7418819916886,
124.471280680952)) ;
#99569 = CARTESIAN_POINT('Ctrl Pts',(-19.0228746479121,-21.7517315469939,
124.554257402682)) ;
#99570 = CARTESIAN_POINT('Ctrl Pts',(-19.2288169451705,-21.7618142551916,
124.604222158295)) ;
#99571 = CARTESIAN_POINT('Ctrl Pts',(-19.434726136211,-21.771626848118,124.617503247817)) ;
#99572 = CARTESIAN_POINT('Ctrl Pts',(-19.645078520801,-21.781694040376,124.59459379872)) ;
#99573 = CARTESIAN_POINT('Ctrl Pts',(-19.8449338785876,-21.7915928698386,
124.536394647074)) ;
#99574 = CARTESIAN_POINT('Ctrl Pts',(-20.0345279392192,-21.8016468610288,
124.44306072579)) ;
#99575 = CARTESIAN_POINT('Ctrl Pts',(-20.2021240600792,-21.811518585812,124.320586090869)) ;
#99576 = CARTESIAN_POINT('Ctrl Pts',(-20.3487851741388,-21.8215890279422,
124.167950383326)) ;
#99577 = CARTESIAN_POINT('Ctrl Pts',(-20.4640443777313,-21.8314221063725,
123.996318711555)) ;
#99578 = CARTESIAN_POINT('Ctrl Pts',(-20.5499711530946,-21.8414525798739,
123.803755933391)) ;
#99579 = CARTESIAN_POINT('Ctrl Pts',(-20.6005714144959,-21.8514841791725,
123.599007999502)) ;
#99580 = CARTESIAN_POINT('Ctrl Pts',(-20.6149930379093,-21.8613138802107,
123.392875006616)) ;
#99581 = CARTESIAN_POINT('Ctrl Pts',(-20.5936752467639,-21.8713033182672,
123.183943946455)) ;
#99582 = CARTESIAN_POINT('Ctrl Pts',(-20.5355777419372,-21.8813472214833,
122.98094198863)) ;
#99583 = CARTESIAN_POINT('Ctrl Pts',(-20.445548537231,-21.8911687422968,122.795122741373)) ;
#99584 = CARTESIAN_POINT('Ctrl Pts',(-20.322397811083,-21.9012044665439,122.62381712929)) ;
#99585 = CARTESIAN_POINT('Ctrl Pts',(-20.171182524821,-21.9112266204764,122.477072722608)) ;
#99586 = CARTESIAN_POINT('Ctrl Pts',(-19.9997840023455,-21.9210888522337,
122.360437968865)) ;
#99587 = CARTESIAN_POINT('Ctrl Pts',(-19.8091030321403,-21.9310479226916,
122.273953551051)) ;
#99588 = CARTESIAN_POINT('Ctrl Pts',(-19.6046853178578,-21.9410830950677,
122.221814064061)) ;
#99589 = CARTESIAN_POINT('Ctrl Pts',(-19.3975576664443,-21.950963480226,122.205891559508)) ;
#99590 = CARTESIAN_POINT('Ctrl Pts',(-19.1871564974738,-21.9610201948199,
122.226451141237)) ;
#99591 = CARTESIAN_POINT('Ctrl Pts',(-18.9870882748877,-21.970899463392,122.282251999282)) ;
#99592 = CARTESIAN_POINT('Ctrl Pts',(-18.7973962258328,-21.9808904208777,
122.372443190088)) ;
#99593 = CARTESIAN_POINT('Ctrl Pts',(-18.6256636516401,-21.9909310795129,
122.495187411846)) ;
#99594 = CARTESIAN_POINT('Ctrl Pts',(-18.4806666654856,-22.0007640592209,
122.642521309246)) ;
#99595 = CARTESIAN_POINT('Ctrl Pts',(-18.3610492272004,-22.0107571924706,
122.815226202152)) ;
#99596 = CARTESIAN_POINT('Ctrl Pts',(-18.2732875695345,-22.0207892448539,
123.007015410382)) ;
#99597 = CARTESIAN_POINT('Ctrl Pts',(-18.2208007012517,-22.0306544738052,
123.207651206206)) ;
#99598 = CARTESIAN_POINT('Ctrl Pts',(-18.2031911282992,-22.0406164150485,
123.416346476884)) ;
#99599 = CARTESIAN_POINT('Ctrl Pts',(-18.2225608620644,-22.0506511300852,
123.626406998495)) ;
#99600 = CARTESIAN_POINT('Ctrl Pts',(-18.2769704965142,-22.0605369004293,
123.827014413738)) ;
#99601 = CARTESIAN_POINT('Ctrl Pts',(-18.366948204184,-22.070599497818,124.018445065004)) ;
#99602 = CARTESIAN_POINT('Ctrl Pts',(-18.4861761411031,-22.0804499096533,
124.187785807338)) ;
#99603 = CARTESIAN_POINT('Ctrl Pts',(-18.6352320965058,-22.0904770789392,
124.336841757389)) ;
#99604 = CARTESIAN_POINT('Ctrl Pts',(-18.808239143253,-22.1005045596534,124.457313557774)) ;
#99605 = CARTESIAN_POINT('Ctrl Pts',(-18.9958335692752,-22.1103476122327,
124.544640097376)) ;
#99606 = CARTESIAN_POINT('Ctrl Pts',(-19.1986730989959,-22.1203415156713,
124.599405997316)) ;
#99607 = CARTESIAN_POINT('Ctrl Pts',(-19.4086761315926,-22.1303686384477,
124.617796950224)) ;
#99608 = CARTESIAN_POINT('Ctrl Pts',(-19.6158461251628,-22.1402593433397,
124.599954847377)) ;
#99609 = CARTESIAN_POINT('Ctrl Pts',(-19.8188982021993,-22.1502513701901,
124.546160266747)) ;
#99610 = CARTESIAN_POINT('Ctrl Pts',(-20.0086259529036,-22.1601973516786,
124.45827440018)) ;
#99611 = CARTESIAN_POINT('Ctrl Pts',(-20.1804838887985,-22.1701445243005,
124.339105469021)) ;
#99612 = CARTESIAN_POINT('Ctrl Pts',(-20.3303650977474,-22.1801924656267,
124.190260950407)) ;
#99613 = CARTESIAN_POINT('Ctrl Pts',(-20.4498461742952,-22.1900400994344,
124.021187769906)) ;
#99614 = CARTESIAN_POINT('Ctrl Pts',(-20.5397670914778,-22.2000018141195,
123.832058923698)) ;
#99615 = CARTESIAN_POINT('Ctrl Pts',(-20.5956054686817,-22.210030446998,123.628740807769)) ;
#99616 = CARTESIAN_POINT('Ctrl Pts',(-20.6151272869738,-22.2199407725331,
123.421319776094)) ;
#99617 = CARTESIAN_POINT('Ctrl Pts',(-20.598836628483,-22.2298756030049,123.213090217045)) ;
#99618 = CARTESIAN_POINT('Ctrl Pts',(-20.5459055531694,-22.2399169353868,
123.00873376961)) ;
#99619 = CARTESIAN_POINT('Ctrl Pts',(-20.4596600398954,-22.2498098088257,
122.819481768458)) ;
#99620 = CARTESIAN_POINT('Ctrl Pts',(-20.3413884622513,-22.2597789746436,
122.646447117661)) ;
#99621 = CARTESIAN_POINT('Ctrl Pts',(-20.1937643881,-22.2698077083601,122.495947000572)) ;
#99622 = CARTESIAN_POINT('Ctrl Pts',(-19.9684090306471,-22.2830002271312,
122.334150743361)) ;
#99623 = CARTESIAN_POINT('Ctrl Pts',(-19.7027956010466,-22.2963600951739,
122.233654614918)) ;
#99624 = CARTESIAN_POINT('Ctrl Pts',(-19.42611363998,-22.3095854323228,122.206049791513)) ;
#99625 = CARTESIAN_POINT('Ctrl Pts',(-19.2168214700513,-22.3195666581634,
122.221179694036)) ;
#99626 = CARTESIAN_POINT('Ctrl Pts',(-19.012339181645,-22.3296022251463,122.273098828801)) ;
#99627 = CARTESIAN_POINT('Ctrl Pts',(-18.8230824090921,-22.3394653031084,
122.357872761559)) ;
#99628 = CARTESIAN_POINT('Ctrl Pts',(-18.6478261042922,-22.3495356019095,
122.476601242485)) ;
#99629 = CARTESIAN_POINT('Ctrl Pts',(-18.4992732806358,-22.3593779004773,
122.620651320733)) ;
#99630 = CARTESIAN_POINT('Ctrl Pts',(-18.3759121078464,-22.3693385986471,
122.78985774388)) ;
#99631 = CARTESIAN_POINT('Ctrl Pts',(-18.283467953693,-22.3793766328265,122.979554985667)) ;
#99632 = CARTESIAN_POINT('Ctrl Pts',(-18.2259320470836,-22.389250369673,123.179027442661)) ;
#99633 = CARTESIAN_POINT('Ctrl Pts',(-18.2034947869199,-22.3993221535983,
123.389545854405)) ;
#99634 = CARTESIAN_POINT('Ctrl Pts',(-18.217484779639,-22.4091542747995,123.595794462009)) ;
#99635 = CARTESIAN_POINT('Ctrl Pts',(-18.2675292104201,-22.4191872988249,
123.800687076778)) ;
#99636 = CARTESIAN_POINT('Ctrl Pts',(-18.3527474459772,-22.4292031790216,
123.993252190823)) ;
#99637 = CARTESIAN_POINT('Ctrl Pts',(-18.4682277000465,-22.4390866981158,
124.165989253353)) ;
#99638 = CARTESIAN_POINT('Ctrl Pts',(-18.6132948326488,-22.4490771104794,
124.317850133931)) ;
#99639 = CARTESIAN_POINT('Ctrl Pts',(-18.8379447971246,-22.4623402736829,
124.483061847326)) ;
#99640 = CARTESIAN_POINT('Ctrl Pts',(-19.1007521920215,-22.4756178439341,
124.586210065187)) ;
#99641 = CARTESIAN_POINT('Ctrl Pts',(-19.3792361220402,-22.4889481464407,
124.617408839646)) ;
#99642 = CARTESIAN_POINT('Ctrl Pts',(-19.5869520039068,-22.4988468282571,
124.604630774508)) ;
#99643 = CARTESIAN_POINT('Ctrl Pts',(-19.791192680303,-22.5088363433046,124.55577826563)) ;
#99644 = CARTESIAN_POINT('Ctrl Pts',(-19.9830639045614,-22.5187843950796,
124.472536061326)) ;
#99645 = CARTESIAN_POINT('Ctrl Pts',(-20.1575731810792,-22.5287257983581,
124.357556144055)) ;
#99646 = CARTESIAN_POINT('Ctrl Pts',(-20.3608542077614,-22.5420124631391,
124.165920176529)) ;
#99647 = CARTESIAN_POINT('Ctrl Pts',(-20.5464539922117,-22.5586228847939,
123.86548937341)) ;
#99648 = CARTESIAN_POINT('Ctrl Pts',(-20.6330198333904,-22.5785341470447,
123.451045864646)) ;
#99649 = CARTESIAN_POINT('Ctrl Pts',(-20.573021398025,-22.5984782762096,123.031223501012)) ;
#99650 = CARTESIAN_POINT('Ctrl Pts',(-20.3735530276952,-22.6184014388147,
122.65754803355)) ;
#99651 = CARTESIAN_POINT('Ctrl Pts',(-20.0594593277888,-22.6382915612213,
122.374246029825)) ;
#99652 = CARTESIAN_POINT('Ctrl Pts',(-19.6652814296702,-22.6582965148214,
122.214565908822)) ;
#99653 = CARTESIAN_POINT('Ctrl Pts',(-19.2436812894664,-22.678134771837,122.198771677157)) ;
#99654 = CARTESIAN_POINT('Ctrl Pts',(-18.8388333057128,-22.6981290726235,
122.328355766307)) ;
#99655 = CARTESIAN_POINT('Ctrl Pts',(-18.5045252190836,-22.718014314668,122.58723585018)) ;
#99656 = CARTESIAN_POINT('Ctrl Pts',(-18.2777439716951,-22.7378892611439,
122.943826458795)) ;
#99657 = CARTESIAN_POINT('Ctrl Pts',(-18.1858522089115,-22.757922331085,123.359795276024)) ;
#99658 = CARTESIAN_POINT('Ctrl Pts',(-18.2415379304341,-22.7778108379854,
123.778960090008)) ;
#99659 = CARTESIAN_POINT('Ctrl Pts',(-18.4353339908866,-22.7976656977667,
124.154091731349)) ;
#99660 = CARTESIAN_POINT('Ctrl Pts',(-18.7489215265165,-22.8177165315544,
124.442775246828)) ;
#99661 = CARTESIAN_POINT('Ctrl Pts',(-19.1366296538309,-22.8374824734436,
124.605298710016)) ;
#99662 = CARTESIAN_POINT('Ctrl Pts',(-19.5614833894531,-22.857495204903,124.626852845355)) ;
#99663 = CARTESIAN_POINT('Ctrl Pts',(-19.9658127034173,-22.8773880398465,
124.502264667132)) ;
#99664 = CARTESIAN_POINT('Ctrl Pts',(-20.3038468327672,-22.8972950631861,
124.24768908528)) ;
#99665 = CARTESIAN_POINT('Ctrl Pts',(-20.5353241050734,-22.9172103280868,
123.892984638816)) ;
#99666 = CARTESIAN_POINT('Ctrl Pts',(-20.6318705158806,-22.9372420202465,
123.478179039821)) ;
#99667 = CARTESIAN_POINT('Ctrl Pts',(-20.5815656326253,-22.9570850668195,
123.059226614385)) ;
#99668 = CARTESIAN_POINT('Ctrl Pts',(-20.3915264865765,-22.9770016147193,
122.68085169778)) ;
#99669 = CARTESIAN_POINT('Ctrl Pts',(-20.0834094997949,-22.9969338577106,
122.389795997805)) ;
#99670 = CARTESIAN_POINT('Ctrl Pts',(-19.6951658363259,-23.0168376925199,
122.221411064852)) ;
#99671 = CARTESIAN_POINT('Ctrl Pts',(-19.2728523173506,-23.0367380927074,
122.195093370532)) ;
#99672 = CARTESIAN_POINT('Ctrl Pts',(-18.8658349068545,-23.0566877690867,
122.314600203806)) ;
#99673 = CARTESIAN_POINT('Ctrl Pts',(-18.5243859747012,-23.0766202933071,
122.565678716369)) ;
#99674 = CARTESIAN_POINT('Ctrl Pts',(-18.2889454953529,-23.0965403022933,
122.917803081957)) ;
#99675 = CARTESIAN_POINT('Ctrl Pts',(-18.1876928509677,-23.1164972084694,
123.329839785219)) ;
#99676 = CARTESIAN_POINT('Ctrl Pts',(-18.2325925918576,-23.1363830479709,
123.750356666916)) ;
#99677 = CARTESIAN_POINT('Ctrl Pts',(-18.4190643793805,-23.1563542201068,
124.131759948009)) ;
#99678 = CARTESIAN_POINT('Ctrl Pts',(-18.7218015414099,-23.1761684170912,
124.424850296392)) ;
#99679 = CARTESIAN_POINT('Ctrl Pts',(-19.109263632571,-23.1961496030594,124.598954222863)) ;
#99680 = CARTESIAN_POINT('Ctrl Pts',(-19.4607814242309,-23.2127251084487,
124.624835889428)) ;
#99681 = CARTESIAN_POINT('Ctrl Pts',(-19.7357494890693,-23.2260345563123,
124.572863177493)) ;
#99682 = CARTESIAN_POINT('Ctrl Pts',(-19.9985287654106,-23.2394022540889,
124.473365747983)) ;
#99683 = CARTESIAN_POINT('Ctrl Pts',(-20.2833778592426,-23.2558928257548,
124.268814816624)) ;
#99684 = CARTESIAN_POINT('Ctrl Pts',(-20.5233279583611,-23.2758130980876,
123.919863291029)) ;
#99685 = CARTESIAN_POINT('Ctrl Pts',(-20.6120068823226,-23.2924301338086,
123.57784929497)) ;
#99686 = CARTESIAN_POINT('Ctrl Pts',(-20.6099216759324,-23.3057209840897,
123.298396665178)) ;
#99687 = CARTESIAN_POINT('Ctrl Pts',(-20.5720876025759,-23.3156900292442,
123.09228660163)) ;
#99688 = CARTESIAN_POINT('Ctrl Pts',(-20.499891105304,-23.3255934198777,122.896976536602)) ;
#99689 = CARTESIAN_POINT('Ctrl Pts',(-20.3931696064655,-23.3356512059904,
122.714468598616)) ;
#99690 = CARTESIAN_POINT('Ctrl Pts',(-20.2592801823281,-23.3455032426402,
122.556402888274)) ;
#99691 = CARTESIAN_POINT('Ctrl Pts',(-20.0435486666867,-23.3588683667834,
122.376463034861)) ;
#99692 = CARTESIAN_POINT('Ctrl Pts',(-19.7882387144785,-23.3720944297464,
122.258444267232)) ;
#99693 = CARTESIAN_POINT('Ctrl Pts',(-19.512736487098,-23.3853980780287,122.210272548135)) ;
#99694 = CARTESIAN_POINT('Ctrl Pts',(-19.3026597055276,-23.3953896091917,
122.210467156068)) ;
#99695 = CARTESIAN_POINT('Ctrl Pts',(-19.0949025299818,-23.405429056991,122.247583991713)) ;
#99696 = CARTESIAN_POINT('Ctrl Pts',(-18.9004743382743,-23.4152728325048,
122.318513397229)) ;
#99697 = CARTESIAN_POINT('Ctrl Pts',(-18.7185635461914,-23.4252584738925,
122.423230002888)) ;
#99698 = CARTESIAN_POINT('Ctrl Pts',(-18.5582621854961,-23.4351952582543,
122.55723697556)) ;
#99699 = CARTESIAN_POINT('Ctrl Pts',(-18.422251596558,-23.4452450927216,122.718888183334)) ;
#99700 = CARTESIAN_POINT('Ctrl Pts',(-18.3183218984366,-23.4550955422248,
122.898025457034)) ;
#99701 = CARTESIAN_POINT('Ctrl Pts',(-18.2456967878488,-23.4650675562069,
123.094658966622)) ;
#99702 = CARTESIAN_POINT('Ctrl Pts',(-18.2082468961159,-23.475062714054,123.301458839307)) ;
#99703 = CARTESIAN_POINT('Ctrl Pts',(-18.2075241676291,-23.4850966404177,
123.512384535685)) ;
#99704 = CARTESIAN_POINT('Ctrl Pts',(-18.2424855463861,-23.4949523488501,
123.716630802841)) ;
#99705 = CARTESIAN_POINT('Ctrl Pts',(-18.3130881217928,-23.5049504981887,
123.914575858876)) ;
#99706 = CARTESIAN_POINT('Ctrl Pts',(-18.4158307592758,-23.5148499013623,
124.095598535347)) ;
#99707 = CARTESIAN_POINT('Ctrl Pts',(-18.5504085106914,-23.5249010982508,
124.258480093894)) ;
#99708 = CARTESIAN_POINT('Ctrl Pts',(-18.7085302744954,-23.5347834220636,
124.393265853387)) ;
#99709 = CARTESIAN_POINT('Ctrl Pts',(-18.8894347314212,-23.5447783177202,
124.500144668724)) ;
#99710 = CARTESIAN_POINT('Ctrl Pts',(-19.0867888297495,-23.5547994171028,
124.573899100679)) ;
#99711 = CARTESIAN_POINT('Ctrl Pts',(-19.2915556219176,-23.5647066849648,
124.611989874118)) ;
#99712 = CARTESIAN_POINT('Ctrl Pts',(-19.5004638116768,-23.5746450287901,
124.614373204255)) ;
#99713 = CARTESIAN_POINT('Ctrl Pts',(-19.7080204412908,-23.5846484480906,
124.58034965562)) ;
#99714 = CARTESIAN_POINT('Ctrl Pts',(-19.9069858061592,-23.5946829987977,
124.510269239607)) ;
#99715 = CARTESIAN_POINT('Ctrl Pts',(-20.0874821198447,-23.6045279484033,
124.408959109667)) ;
#99716 = CARTESIAN_POINT('Ctrl Pts',(-20.2501516504676,-23.6145137905162,
124.276305987844)) ;
#99717 = CARTESIAN_POINT('Ctrl Pts',(-20.3867763334216,-23.6244485978853,
124.118278250785)) ;
#99718 = CARTESIAN_POINT('Ctrl Pts',(-20.4950121057334,-23.6345061395986,
123.936675429295)) ;
#99719 = CARTESIAN_POINT('Ctrl Pts',(-20.5686262719049,-23.6443277371107,
123.743738386367)) ;
#99720 = CARTESIAN_POINT('Ctrl Pts',(-20.6089302652042,-23.6543839965912,
123.536219939472)) ;
#99721 = CARTESIAN_POINT('Ctrl Pts',(-20.6121814570915,-23.6643239328916,
123.327265180955)) ;
#99722 = CARTESIAN_POINT('Ctrl Pts',(-20.579832504684,-23.674231053636,123.121516390031)) ;
#99723 = CARTESIAN_POINT('Ctrl Pts',(-20.5112510751062,-23.6842739595613,
122.921836997899)) ;
#99724 = CARTESIAN_POINT('Ctrl Pts',(-20.4104455684858,-23.6941817406604,
122.739552942359)) ;
#99725 = CARTESIAN_POINT('Ctrl Pts',(-20.278453914512,-23.7041921096629,122.575631897472)) ;
#99726 = CARTESIAN_POINT('Ctrl Pts',(-20.1194051413348,-23.7142229482317,
122.437164824762)) ;
#99727 = CARTESIAN_POINT('Ctrl Pts',(-19.9421231339364,-23.7240757878714,
122.330025519522)) ;
#99728 = CARTESIAN_POINT('Ctrl Pts',(-19.7464393999496,-23.7340637890363,
122.2539194637)) ;
#99729 = CARTESIAN_POINT('Ctrl Pts',(-19.5417130247443,-23.7439926080155,
122.213180878514)) ;
#99730 = CARTESIAN_POINT('Ctrl Pts',(-19.3317876230183,-23.7539803107378,
122.208227535199)) ;
#99731 = CARTESIAN_POINT('Ctrl Pts',(-19.1232603369714,-23.7640163105405,
122.240299689007)) ;
#99732 = CARTESIAN_POINT('Ctrl Pts',(-18.9269409345926,-23.7738711803419,
122.306551170466)) ;
#99733 = CARTESIAN_POINT('Ctrl Pts',(-18.7423483430796,-23.7838706107654,
122.407064740461)) ;
#99734 = CARTESIAN_POINT('Ctrl Pts',(-18.5795334533094,-23.7937657282307,
122.536604738157)) ;
#99735 = CARTESIAN_POINT('Ctrl Pts',(-18.4394363684529,-23.8038262217477,
122.695019238229)) ;
#99736 = CARTESIAN_POINT('Ctrl Pts',(-18.3311723211826,-23.8136757019489,
122.871546097844)) ;
#99737 = CARTESIAN_POINT('Ctrl Pts',(-18.253338855321,-23.8237021522127,123.067434654631)) ;
#99738 = CARTESIAN_POINT('Ctrl Pts',(-18.2112477379437,-23.8337334426908,
123.274085631047)) ;
#99739 = CARTESIAN_POINT('Ctrl Pts',(-18.2053327713523,-23.8435748303426,
123.480899314551)) ;
#99740 = CARTESIAN_POINT('Ctrl Pts',(-18.235505136608,-23.8535782312338,123.689005387988)) ;
#99741 = CARTESIAN_POINT('Ctrl Pts',(-18.30132892869,-23.863562614025,123.888359327412)) ;
#99742 = CARTESIAN_POINT('Ctrl Pts',(-18.4014615932584,-23.8736017040384,
124.074123182308)) ;
#99743 = CARTESIAN_POINT('Ctrl Pts',(-18.5296028651953,-23.8834475129475,
124.236698639084)) ;
#99744 = CARTESIAN_POINT('Ctrl Pts',(-18.6858817741305,-23.8934319357665,
124.376783940283)) ;
#99745 = CARTESIAN_POINT('Ctrl Pts',(-18.8633136681397,-23.9033715610077,
124.487216459625)) ;
#99746 = CARTESIAN_POINT('Ctrl Pts',(-19.0591532422952,-23.9134112505264,
124.565884912864)) ;
#99747 = CARTESIAN_POINT('Ctrl Pts',(-19.2625668465691,-23.923299438945,124.608805758651)) ;
#99748 = CARTESIAN_POINT('Ctrl Pts',(-19.4724402725626,-23.933288964947,124.61621980791)) ;
#99749 = CARTESIAN_POINT('Ctrl Pts',(-19.6797460859704,-23.9432474663022,
124.587011172538)) ;
#99750 = CARTESIAN_POINT('Ctrl Pts',(-19.8778294389247,-23.9531470603059,
124.523118150235)) ;
#99751 = CARTESIAN_POINT('Ctrl Pts',(-20.0645009332798,-23.9631949484272,
124.4242939218)) ;
#99752 = CARTESIAN_POINT('Ctrl Pts',(-20.2287913861833,-23.9730903736727,
124.296622717768)) ;
#99753 = CARTESIAN_POINT('Ctrl Pts',(-20.370743794107,-23.9831517643733,124.139840419593)) ;
#99754 = CARTESIAN_POINT('Ctrl Pts',(-20.4809539229722,-23.9929973480599,
123.964623054228)) ;
#99755 = CARTESIAN_POINT('Ctrl Pts',(-20.5606419837737,-24.0029603213691,
123.770937309358)) ;
#99756 = CARTESIAN_POINT('Ctrl Pts',(-20.605503776578,-24.0129859881949,123.564982234247)) ;
#99757 = CARTESIAN_POINT('Ctrl Pts',(-20.6139419341047,-24.0229004660612,
123.356726781891)) ;
#99758 = CARTESIAN_POINT('Ctrl Pts',(-20.5862956152923,-24.0328889807362,
123.148547424027)) ;
#99759 = CARTESIAN_POINT('Ctrl Pts',(-20.5221502732614,-24.0429330916517,
122.947387425594)) ;
#99760 = CARTESIAN_POINT('Ctrl Pts',(-20.4265837470673,-24.0527612292462,
122.764165552609)) ;
#99761 = CARTESIAN_POINT('Ctrl Pts',(-20.2975940053477,-24.0628377973052,
122.596176910307)) ;
#99762 = CARTESIAN_POINT('Ctrl Pts',(-20.1448810173156,-24.0726899592093,
122.456185655466)) ;
#99763 = CARTESIAN_POINT('Ctrl Pts',(-19.9664285931066,-24.0827629211662,
122.342238441325)) ;
#99764 = CARTESIAN_POINT('Ctrl Pts',(-19.7753138348531,-24.0926054831691,
122.262872509652)) ;
#99765 = CARTESIAN_POINT('Ctrl Pts',(-19.5706729258633,-24.1025859196629,
122.216584695469)) ;
#99766 = CARTESIAN_POINT('Ctrl Pts',(-19.3602825235142,-24.1126042249873,
122.206899948226)) ;
#99767 = CARTESIAN_POINT('Ctrl Pts',(-19.1541286885826,-24.1224881889067,
122.233106235559)) ;
#99768 = CARTESIAN_POINT('Ctrl Pts',(-18.9520644608838,-24.1325540656453,
122.295881868237)) ;
#99769 = CARTESIAN_POINT('Ctrl Pts',(-18.7681068047576,-24.1423931665062,
122.390503401333)) ;
#99770 = CARTESIAN_POINT('Ctrl Pts',(-18.5998257348978,-24.1524262493719,
122.517654569981)) ;
#99771 = CARTESIAN_POINT('Ctrl Pts',(-18.4567081290935,-24.1624479346474,
122.672293738054)) ;
#99772 = CARTESIAN_POINT('Ctrl Pts',(-18.3441156101075,-24.1723146297458,
122.84648676252)) ;
#99773 = CARTESIAN_POINT('Ctrl Pts',(-18.2621969152009,-24.1822745194804,
123.039195156159)) ;
#99774 = CARTESIAN_POINT('Ctrl Pts',(-18.214947672382,-24.1923095073059,123.244789453802)) ;
#99775 = CARTESIAN_POINT('Ctrl Pts',(-18.2039263449336,-24.2021962113802,
123.452375721964)) ;
#99776 = CARTESIAN_POINT('Ctrl Pts',(-18.2296161017623,-24.2122613556131,
123.662377249699)) ;
#99777 = CARTESIAN_POINT('Ctrl Pts',(-18.2898091933398,-24.2221006463416,
123.860311252195)) ;
#99778 = CARTESIAN_POINT('Ctrl Pts',(-18.3852966236733,-24.2321632037801,
124.049053788078)) ;
#99779 = CARTESIAN_POINT('Ctrl Pts',(-18.5102199159403,-24.2420602550322,
124.215459681128)) ;
#99780 = CARTESIAN_POINT('Ctrl Pts',(-18.6621744914154,-24.2519914617804,
124.35863416579)) ;
#99781 = CARTESIAN_POINT('Ctrl Pts',(-18.8387600799693,-24.2620336459993,
124.474338039765)) ;
#99782 = CARTESIAN_POINT('Ctrl Pts',(-19.0296995778466,-24.2719202741102,
124.556477311075)) ;
#99783 = CARTESIAN_POINT('Ctrl Pts',(-19.2340821973349,-24.2819135466426,
124.605065394513)) ;
#99784 = CARTESIAN_POINT('Ctrl Pts',(-19.4428018406446,-24.291858622184,124.617298377036)) ;
#99785 = CARTESIAN_POINT('Ctrl Pts',(-19.6506237184402,-24.3018081729123,
124.593497787053)) ;
#99786 = CARTESIAN_POINT('Ctrl Pts',(-19.8528900152254,-24.3118475077603,
124.533250017202)) ;
#99787 = CARTESIAN_POINT('Ctrl Pts',(-20.0388518383807,-24.3217336467042,
124.440397820434)) ;
#99788 = CARTESIAN_POINT('Ctrl Pts',(-20.2078844550551,-24.3317317596779,
124.315505594781)) ;
#99789 = CARTESIAN_POINT('Ctrl Pts',(-20.3516543996633,-24.3416515220303,
124.16440628031)) ;
#99790 = CARTESIAN_POINT('Ctrl Pts',(-20.4684314575446,-24.351690917643,123.988608388882)) ;
#99791 = CARTESIAN_POINT('Ctrl Pts',(-20.5517608831207,-24.3616001034313,
123.797676720109)) ;
#99792 = CARTESIAN_POINT('Ctrl Pts',(-20.6013705993745,-24.3715352875888,
123.594783317596)) ;
#99793 = CARTESIAN_POINT('Ctrl Pts',(-20.6149354131608,-24.3815763449747,
123.384130104099)) ;
#99794 = CARTESIAN_POINT('Ctrl Pts',(-20.5922202889144,-24.391463503008,123.17750488108)) ;
#99795 = CARTESIAN_POINT('Ctrl Pts',(-20.5336967147129,-24.4014557826839,
122.975767578548)) ;
#99796 = CARTESIAN_POINT('Ctrl Pts',(-20.4413760253052,-24.4114042997289,
122.788083897258)) ;
#99797 = CARTESIAN_POINT('Ctrl Pts',(-20.3182708865033,-24.4213410772993,
122.619329886735)) ;
#99798 = CARTESIAN_POINT('Ctrl Pts',(-20.1671857634462,-24.4313241134463,
122.473618379241)) ;
#99799 = CARTESIAN_POINT('Ctrl Pts',(-19.991862245573,-24.44136786504,122.355989324319)) ;
#99800 = CARTESIAN_POINT('Ctrl Pts',(-19.8030626471356,-24.4511963942526,
122.271955584886)) ;
#99801 = CARTESIAN_POINT('Ctrl Pts',(-19.5976019088052,-24.4612717551613,
122.220631391633)) ;
#99802 = CARTESIAN_POINT('Ctrl Pts',(-19.3908579044476,-24.4711283540485,
122.206005511955)) ;
#99803 = CARTESIAN_POINT('Ctrl Pts',(-19.1804601864088,-24.4811913480664,
122.22772220342)) ;
#99804 = CARTESIAN_POINT('Ctrl Pts',(-18.980700794913,-24.4910692823558,122.284611098396)) ;
#99805 = CARTESIAN_POINT('Ctrl Pts',(-18.7914582896388,-24.5010699299139,
122.376122908358)) ;
#99806 = CARTESIAN_POINT('Ctrl Pts',(-18.6222389333094,-24.5109877763519,
122.498001109228)) ;
#99807 = CARTESIAN_POINT('Ctrl Pts',(-18.4748893105009,-24.5210388933576,
122.64940803406)) ;
#99808 = CARTESIAN_POINT('Ctrl Pts',(-18.3579656286676,-24.5309096286682,
122.820892408784)) ;
#99809 = CARTESIAN_POINT('Ctrl Pts',(-18.270854719681,-24.5409803359112,123.013821897144)) ;
#99810 = CARTESIAN_POINT('Ctrl Pts',(-18.2196956047641,-24.5508133433631,
123.214131866147)) ;
#99811 = CARTESIAN_POINT('Ctrl Pts',(-18.2031823833649,-24.5608438356654,
123.424349262952)) ;
#99812 = CARTESIAN_POINT('Ctrl Pts',(-18.2240367933666,-24.5708754307388,
123.634223384466)) ;
#99813 = CARTESIAN_POINT('Ctrl Pts',(-18.2794463048253,-24.580705129877,123.833292666262)) ;
#99814 = CARTESIAN_POINT('Ctrl Pts',(-18.3694704776268,-24.5906945797586,
124.023035513074)) ;
#99815 = CARTESIAN_POINT('Ctrl Pts',(-18.492166830848,-24.6007384375743,124.194879685867)) ;
#99816 = CARTESIAN_POINT('Ctrl Pts',(-18.6392056361206,-24.6105601281645,
124.339844812056)) ;
#99817 = CARTESIAN_POINT('Ctrl Pts',(-18.8125807649403,-24.6205952187049,
124.460042939287)) ;
#99818 = CARTESIAN_POINT('Ctrl Pts',(-19.0042411232664,-24.6306197376876,
124.547716711439)) ;
#99819 = CARTESIAN_POINT('Ctrl Pts',(-19.2047449312854,-24.6404795830978,
124.600243465133)) ;
#99820 = CARTESIAN_POINT('Ctrl Pts',(-19.4133882116478,-24.6504393594134,
124.617906639743)) ;
#99821 = CARTESIAN_POINT('Ctrl Pts',(-19.6233285409857,-24.6604675567281,
124.598654709041)) ;
#99822 = CARTESIAN_POINT('Ctrl Pts',(-19.8243735433467,-24.6703750990184,
124.544142548399)) ;
#99823 = CARTESIAN_POINT('Ctrl Pts',(-20.0152813474859,-24.6804077495822,
124.454510612115)) ;
#99824 = CARTESIAN_POINT('Ctrl Pts',(-20.1852235327726,-24.6902917060089,
124.334929778442)) ;
#99825 = CARTESIAN_POINT('Ctrl Pts',(-20.3337579691757,-24.7002814073707,
124.186453403808)) ;
#99826 = CARTESIAN_POINT('Ctrl Pts',(-20.4545041927332,-24.7103224026468,
124.01330337814)) ;
#99827 = CARTESIAN_POINT('Ctrl Pts',(-20.5418176556216,-24.7201552919151,
123.825934133809)) ;
#99828 = CARTESIAN_POINT('Ctrl Pts',(-20.5967254098362,-24.7301484502826,
123.623152064914)) ;
#99829 = CARTESIAN_POINT('Ctrl Pts',(-20.6152263745381,-24.7401804926347,
123.413049976285)) ;
#99830 = CARTESIAN_POINT('Ctrl Pts',(-20.5975260632416,-24.7500457365931,
123.206418993902)) ;
#99831 = CARTESIAN_POINT('Ctrl Pts',(-20.5442637123543,-24.7600076278391,
123.003868684083)) ;
#99832 = CARTESIAN_POINT('Ctrl Pts',(-20.4556941376338,-24.7700425278576,
122.812407534119)) ;
#99833 = CARTESIAN_POINT('Ctrl Pts',(-20.3372857181747,-24.7799276082722,
122.641592452716)) ;
#99834 = CARTESIAN_POINT('Ctrl Pts',(-20.1883750420845,-24.789992780397,122.491295789291)) ;
#99835 = CARTESIAN_POINT('Ctrl Pts',(-20.0194007977466,-24.7998400151205,
122.371657221972)) ;
#99836 = CARTESIAN_POINT('Ctrl Pts',(-19.828974180935,-24.8098708264382,122.281093234429)) ;
#99837 = CARTESIAN_POINT('Ctrl Pts',(-19.6259933683602,-24.8198804423517,
122.225493675427)) ;
#99838 = CARTESIAN_POINT('Ctrl Pts',(-19.4185734016865,-24.8297912217554,
122.205975379391)) ;
#99839 = CARTESIAN_POINT('Ctrl Pts',(-19.2104563591448,-24.8397204875445,
122.222280279329)) ;
#99840 = CARTESIAN_POINT('Ctrl Pts',(-19.0060857009913,-24.8497631808571,
122.275238154598)) ;
#99841 = CARTESIAN_POINT('Ctrl Pts',(-18.8169262905509,-24.8596497135518,
122.361399220781)) ;
#99842 = CARTESIAN_POINT('Ctrl Pts',(-18.6435709558657,-24.8696428586551,
122.480058091758)) ;
#99843 = CARTESIAN_POINT('Ctrl Pts',(-18.4942123999932,-24.8795885393292,
122.626382157185)) ;
#99844 = CARTESIAN_POINT('Ctrl Pts',(-18.3721563886052,-24.8895357969559,
122.796202999615)) ;
#99845 = CARTESIAN_POINT('Ctrl Pts',(-18.280744498605,-24.8995836990774,122.986630955136)) ;
#99846 = CARTESIAN_POINT('Ctrl Pts',(-18.2247509300353,-24.9094314046991,
123.185945959147)) ;
#99847 = CARTESIAN_POINT('Ctrl Pts',(-18.203321009763,-24.9193928713332,123.394260433957)) ;
#99848 = CARTESIAN_POINT('Ctrl Pts',(-18.2187746609672,-24.9294224246014,
123.604554035953)) ;
#99849 = CARTESIAN_POINT('Ctrl Pts',(-18.2697576823691,-24.9393293166288,
123.806494488261)) ;
#99850 = CARTESIAN_POINT('Ctrl Pts',(-18.3550027344737,-24.9492769607418,
123.997444643296)) ;
#99851 = CARTESIAN_POINT('Ctrl Pts',(-18.4726412612924,-24.9592770037707,
124.171715727158)) ;
#99852 = CARTESIAN_POINT('Ctrl Pts',(-18.6195572124782,-24.9693157697647,
124.323206658727)) ;
#99853 = CARTESIAN_POINT('Ctrl Pts',(-18.7866725649534,-24.9791408317869,
124.444626460245)) ;
#99854 = CARTESIAN_POINT('Ctrl Pts',(-18.9764902280137,-24.9891953791133,
124.537602574558)) ;
#99855 = CARTESIAN_POINT('Ctrl Pts',(-19.1774391582938,-24.9991386225625,
124.595216985197)) ;
#99856 = CARTESIAN_POINT('Ctrl Pts',(-19.3844082231206,-25.0090407941704,
124.61761785114)) ;
#99857 = CARTESIAN_POINT('Ctrl Pts',(-19.5952631757004,-25.0190936297806,
124.603401294433)) ;
#99858 = CARTESIAN_POINT('Ctrl Pts',(-19.796813720619,-25.0289666874661,124.553771103334)) ;
#99859 = CARTESIAN_POINT('Ctrl Pts',(-19.9892347634904,-25.0389619489918,
124.469341017337)) ;
#99860 = CARTESIAN_POINT('Ctrl Pts',(-20.1643959113906,-25.0489873184123,
124.352113852972)) ;
#99861 = CARTESIAN_POINT('Ctrl Pts',(-20.3146769667768,-25.0588771509389,
124.208421514089)) ;
#99862 = CARTESIAN_POINT('Ctrl Pts',(-20.4803794436835,-25.0721751217483,
123.983283965632)) ;
#99863 = CARTESIAN_POINT('Ctrl Pts',(-20.5831727929034,-25.0853735168574,
123.722088148301)) ;
#99864 = CARTESIAN_POINT('Ctrl Pts',(-20.6148627623827,-25.0987689591369,
123.442321770748)) ;
#99865 = CARTESIAN_POINT('Ctrl Pts',(-20.602237789699,-25.1086447973759,123.23504372945)) ;
#99866 = CARTESIAN_POINT('Ctrl Pts',(-20.5530157124887,-25.1187061999736,
123.029364586797)) ;
#99867 = CARTESIAN_POINT('Ctrl Pts',(-20.4705008425079,-25.1285712569087,
122.839056366478)) ;
#99868 = CARTESIAN_POINT('Ctrl Pts',(-20.3548424221102,-25.1385833528575,
122.663232365539)) ;
#99869 = CARTESIAN_POINT('Ctrl Pts',(-20.1632024292778,-25.151860662003,122.460204392433)) ;
#99870 = CARTESIAN_POINT('Ctrl Pts',(-19.8630433647334,-25.1684596875103,
122.274649384483)) ;
#99871 = CARTESIAN_POINT('Ctrl Pts',(-19.517493075074,-25.1850587355433,122.202608397509)) ;
#99872 = CARTESIAN_POINT('Ctrl Pts',(-19.2395187631259,-25.1983021475742,
122.217832437561)) ;
#99873 = CARTESIAN_POINT('Ctrl Pts',(-19.0339973143478,-25.2083395752627,
122.265684096635)) ;
#99874 = CARTESIAN_POINT('Ctrl Pts',(-18.8424969423371,-25.2182438772183,
122.347427278303)) ;
#99875 = CARTESIAN_POINT('Ctrl Pts',(-18.6084659217411,-25.2315107171934,
122.499206248496)) ;
#99876 = CARTESIAN_POINT('Ctrl Pts',(-18.3717402338248,-25.2481369152834,
122.761724059668)) ;
#99877 = CARTESIAN_POINT('Ctrl Pts',(-18.2123622019135,-25.2680560306668,
123.154130925056)) ;
#99878 = CARTESIAN_POINT('Ctrl Pts',(-18.1988264631865,-25.284662453801,123.507013423043)) ;
#99879 = CARTESIAN_POINT('Ctrl Pts',(-18.2607644903236,-25.2979586742967,
123.779547222944)) ;
#99880 = CARTESIAN_POINT('Ctrl Pts',(-18.368329512262,-25.3112275066382,124.037014016904)) ;
#99881 = CARTESIAN_POINT('Ctrl Pts',(-18.585521594005,-25.3279187546713,124.317571743072)) ;
#99882 = CARTESIAN_POINT('Ctrl Pts',(-18.9413374202487,-25.3477284863441,
124.543094056415)) ;
#99883 = CARTESIAN_POINT('Ctrl Pts',(-19.3559852920937,-25.3677060936726,
124.635224997939)) ;
#99884 = CARTESIAN_POINT('Ctrl Pts',(-19.7759664400881,-25.3876324027305,
124.579702360081)) ;
#99885 = CARTESIAN_POINT('Ctrl Pts',(-20.1505528780592,-25.4074492628952,
124.386507917779)) ;
#99886 = CARTESIAN_POINT('Ctrl Pts',(-20.440148489352,-25.4275490784892,124.072406676841)) ;
#99887 = CARTESIAN_POINT('Ctrl Pts',(-20.6026714249817,-25.4473060423717,
123.684842342551)) ;
#99888 = CARTESIAN_POINT('Ctrl Pts',(-20.6242932438096,-25.4673429684412,
123.259498157525)) ;
#99889 = CARTESIAN_POINT('Ctrl Pts',(-20.4998013402423,-25.4872125508227,
122.855661548304)) ;
#99890 = CARTESIAN_POINT('Ctrl Pts',(-20.2454922051924,-25.5071171225759,
122.517464791175)) ;
#99891 = CARTESIAN_POINT('Ctrl Pts',(-19.8900327537312,-25.5270697247744,
122.28574435269)) ;
#99892 = CARTESIAN_POINT('Ctrl Pts',(-19.4778521106647,-25.5469792157446,
122.189613361865)) ;
#99893 = CARTESIAN_POINT('Ctrl Pts',(-19.0585078223892,-25.5668305844441,
122.238603638374)) ;
#99894 = CARTESIAN_POINT('Ctrl Pts',(-18.6771572364457,-25.5869107805801,
122.430408218222)) ;
#99895 = CARTESIAN_POINT('Ctrl Pts',(-18.3880842706593,-25.6067117241555,
122.736659387425)) ;
#99896 = CARTESIAN_POINT('Ctrl Pts',(-18.2185195127077,-25.626695700665,123.12620002553)) ;
#99897 = CARTESIAN_POINT('Ctrl Pts',(-18.1928057080986,-25.6466116636406,
123.548884545342)) ;
#99898 = CARTESIAN_POINT('Ctrl Pts',(-18.3115038307547,-25.6664820984625,
123.954453885361)) ;
#99899 = CARTESIAN_POINT('Ctrl Pts',(-18.5641908089213,-25.6865323836956,
124.29766701825)) ;
#99900 = CARTESIAN_POINT('Ctrl Pts',(-18.9138515897493,-25.7063063524549,
124.531454917921)) ;
#99901 = CARTESIAN_POINT('Ctrl Pts',(-19.327733745075,-25.7263628105744,124.633528224485)) ;
#99902 = CARTESIAN_POINT('Ctrl Pts',(-19.7463496929672,-25.7461576935654,
124.588652959728)) ;
#99903 = CARTESIAN_POINT('Ctrl Pts',(-20.128140092954,-25.7661243488678,124.4031845523)) ;
#99904 = CARTESIAN_POINT('Ctrl Pts',(-20.4232241870294,-25.7860833189443,
124.098070503408)) ;
#99905 = CARTESIAN_POINT('Ctrl Pts',(-20.5961678392642,-25.8059794065344,
123.712015137049)) ;
#99906 = CARTESIAN_POINT('Ctrl Pts',(-20.6274946198202,-25.825877576446,123.290123236047)) ;
#99907 = CARTESIAN_POINT('Ctrl Pts',(-20.513343401748,-25.8457834118131,122.882523035985)) ;
#99908 = CARTESIAN_POINT('Ctrl Pts',(-20.2664373158449,-25.865733336751,122.537643549283)) ;
#99909 = CARTESIAN_POINT('Ctrl Pts',(-19.9180604761659,-25.8856125266614,
122.298197938678)) ;
#99910 = CARTESIAN_POINT('Ctrl Pts',(-19.5069178890842,-25.905593850942,122.191266266653)) ;
#99911 = CARTESIAN_POINT('Ctrl Pts',(-19.0849510940192,-25.9255236351503,
122.231183035918)) ;
#99912 = CARTESIAN_POINT('Ctrl Pts',(-18.702256540964,-25.9454436245411,122.41244877012)) ;
#99913 = CARTESIAN_POINT('Ctrl Pts',(-18.4045387668294,-25.9652988198951,
122.71191648706)) ;
#99914 = CARTESIAN_POINT('Ctrl Pts',(-18.225635640486,-25.9853448215545,123.098678084913)) ;
#99915 = CARTESIAN_POINT('Ctrl Pts',(-18.1956897254653,-26.0018445687643,
123.448307175656)) ;
#99916 = CARTESIAN_POINT('Ctrl Pts',(-18.2447567373269,-26.0152331732124,
123.725454226179)) ;
#99917 = CARTESIAN_POINT('Ctrl Pts',(-18.3158066591231,-26.0250950015473,
123.920229387462)) ;
#99918 = CARTESIAN_POINT('Ctrl Pts',(-18.4201303183734,-26.0350611443048,
124.101948753799)) ;
#99919 = CARTESIAN_POINT('Ctrl Pts',(-18.600485338267,-26.0484228904298,124.317180388579)) ;
#99920 = CARTESIAN_POINT('Ctrl Pts',(-18.8864936249585,-26.0648772193849,
124.519010362641)) ;
#99921 = CARTESIAN_POINT('Ctrl Pts',(-19.2302506733949,-26.0816444644332,
124.612811063999)) ;
#99922 = CARTESIAN_POINT('Ctrl Pts',(-19.5076063317897,-26.0948310297072,
124.613710718939)) ;
#99923 = CARTESIAN_POINT('Ctrl Pts',(-19.7145916347529,-26.1048204884518,
124.578551190262)) ;
#99924 = CARTESIAN_POINT('Ctrl Pts',(-19.9117339058093,-26.1147742609329,
124.508243101983)) ;
#99925 = CARTESIAN_POINT('Ctrl Pts',(-20.0952486246525,-26.1248220774656,
124.403684638952)) ;
#99926 = CARTESIAN_POINT('Ctrl Pts',(-20.2546739661923,-26.1346636105881,
124.271776270735)) ;
#99927 = CARTESIAN_POINT('Ctrl Pts',(-20.3910509208298,-26.1446498528078,
124.112206211367)) ;
#99928 = CARTESIAN_POINT('Ctrl Pts',(-20.497245436602,-26.1545864762327,123.932272438433)) ;
#99929 = CARTESIAN_POINT('Ctrl Pts',(-20.5713010983377,-26.1646363536156,
123.734419048362)) ;
#99930 = CARTESIAN_POINT('Ctrl Pts',(-20.6092722364872,-26.1744867923932,
123.53082708576)) ;
#99931 = CARTESIAN_POINT('Ctrl Pts',(-20.6118885271186,-26.1844588063619,
123.32122666188)) ;
#99932 = CARTESIAN_POINT('Ctrl Pts',(-20.5779551257686,-26.1944539749881,
123.113820981451)) ;
#99933 = CARTESIAN_POINT('Ctrl Pts',(-20.5080341701387,-26.2044878582493,
122.914819888608)) ;
#99934 = CARTESIAN_POINT('Ctrl Pts',(-20.4067160676002,-26.2143437283126,
122.734062520319)) ;
#99935 = CARTESIAN_POINT('Ctrl Pts',(-20.2739494194638,-26.2243412742298,
122.571154450775)) ;
#99936 = CARTESIAN_POINT('Ctrl Pts',(-20.1163559699603,-26.234249401129,122.434931534787)) ;
#99937 = CARTESIAN_POINT('Ctrl Pts',(-19.9358437933286,-26.2442597726512,
122.326724430963)) ;
#99938 = CARTESIAN_POINT('Ctrl Pts',(-19.7387398429276,-26.2542902153986,
122.251799646237)) ;
#99939 = CARTESIAN_POINT('Ctrl Pts',(-19.5354578042761,-26.2641381679519,
122.212477683951)) ;
#99940 = CARTESIAN_POINT('Ctrl Pts',(-19.3239608031358,-26.2742008369729,
122.208810514693)) ;
#99941 = CARTESIAN_POINT('Ctrl Pts',(-19.1185179571218,-26.2840952124368,
122.241520751434)) ;
#99942 = CARTESIAN_POINT('Ctrl Pts',(-18.9207930277153,-26.2940370107549,
122.309186595827)) ;
#99943 = CARTESIAN_POINT('Ctrl Pts',(-18.7366171954101,-26.3040395044822,
122.41072768971)) ;
#99944 = CARTESIAN_POINT('Ctrl Pts',(-18.5725825693357,-26.3140743029892,
122.5433642602)) ;
#99945 = CARTESIAN_POINT('Ctrl Pts',(-18.4364115557814,-26.3239191869685,
122.699248354577)) ;
#99946 = CARTESIAN_POINT('Ctrl Pts',(-18.3275287061022,-26.3339050437866,
122.878699702378)) ;
#99947 = CARTESIAN_POINT('Ctrl Pts',(-18.2516825636088,-26.3438398579613,
123.073344231258)) ;
#99948 = CARTESIAN_POINT('Ctrl Pts',(-18.2104783325537,-26.3538973577467,
123.280700159749)) ;
#99949 = CARTESIAN_POINT('Ctrl Pts',(-18.2056945121997,-26.363719116165,123.487151327135)) ;
#99950 = CARTESIAN_POINT('Ctrl Pts',(-18.2371725207322,-26.373774773949,123.696178600479)) ;
#99951 = CARTESIAN_POINT('Ctrl Pts',(-18.3040751970282,-26.383716956129,123.894209455763)) ;
#99952 = CARTESIAN_POINT('Ctrl Pts',(-18.4034096187346,-26.3936221648237,
124.077224976992)) ;
#99953 = CARTESIAN_POINT('Ctrl Pts',(-18.5348523656912,-26.4036639557861,
124.242418104865)) ;
#99954 = CARTESIAN_POINT('Ctrl Pts',(-18.6908648201985,-26.4135717302584,
124.380437267069)) ;
#99955 = CARTESIAN_POINT('Ctrl Pts',(-18.8701258394266,-26.423583230486,124.490740559058)) ;
#99956 = CARTESIAN_POINT('Ctrl Pts',(-19.0663873139031,-26.4336159908787,
124.56799590819)) ;
#99957 = CARTESIAN_POINT('Ctrl Pts',(-19.2692608516365,-26.4434665600136,
124.609595332654)) ;
#99958 = CARTESIAN_POINT('Ctrl Pts',(-19.4791433366216,-26.4534551695435,
124.615814186761)) ;
#99959 = CARTESIAN_POINT('Ctrl Pts',(-19.685693046642,-26.4633838255676,124.585673009685)) ;
#99960 = CARTESIAN_POINT('Ctrl Pts',(-19.8851674712078,-26.4733715717454,
124.520072233219)) ;
#99961 = CARTESIAN_POINT('Ctrl Pts',(-20.0709297279972,-26.4834075606811,
124.420049379939)) ;
#99962 = CARTESIAN_POINT('Ctrl Pts',(-20.2337477254927,-26.4932624304947,
124.291905451778)) ;
#99963 = CARTESIAN_POINT('Ctrl Pts',(-20.3740466585876,-26.5032618717365,
124.135400895266)) ;
#99964 = CARTESIAN_POINT('Ctrl Pts',(-20.4841082810196,-26.5131569459166,
123.958835198187)) ;
#99965 = CARTESIAN_POINT('Ctrl Pts',(-20.5630967962793,-26.5232176017563,
123.762660736772)) ;
#99966 = CARTESIAN_POINT('Ctrl Pts',(-20.6060280452835,-26.5330664759519,
123.560090350489)) ;
#99967 = CARTESIAN_POINT('Ctrl Pts',(-20.6137949071109,-26.5430951879151,
123.349401316088)) ;
#99968 = CARTESIAN_POINT('Ctrl Pts',(-20.5842903223688,-26.5531245884982,
123.140622164131)) ;
#99969 = CARTESIAN_POINT('Ctrl Pts',(-20.5206537010445,-26.5629647821151,
122.943778426524)) ;
#99970 = CARTESIAN_POINT('Ctrl Pts',(-20.4225541797564,-26.5729682046903,
122.757780626066)) ;
#99971 = CARTESIAN_POINT('Ctrl Pts',(-20.2937913048424,-26.5829537417834,
122.591935887428)) ;
#99972 = CARTESIAN_POINT('Ctrl Pts',(-20.1372231985941,-26.5929947462702,
122.450378632273)) ;
#99973 = CARTESIAN_POINT('Ctrl Pts',(-19.9620903895731,-26.6028382852114,
122.340106587294)) ;
#99974 = CARTESIAN_POINT('Ctrl Pts',(-19.7679261204485,-26.6128233162022,
122.26040527404)) ;
#99975 = CARTESIAN_POINT('Ctrl Pts',(-19.5637669403558,-26.6227627787242,
122.215737639999)) ;
#99976 = CARTESIAN_POINT('Ctrl Pts',(-19.352891158656,-26.632802510948,122.20716040797)) ;
#99977 = CARTESIAN_POINT('Ctrl Pts',(-19.1468449982947,-26.6426906912652,
122.234804771329)) ;
#99978 = CARTESIAN_POINT('Ctrl Pts',(-18.9465966844002,-26.6526802069677,
122.298069410787)) ;
#99979 = CARTESIAN_POINT('Ctrl Pts',(-18.761026707116,-26.6626387576224,122.394986011761)) ;
#99980 = CARTESIAN_POINT('Ctrl Pts',(-18.5957571329193,-26.6725381647274,
122.521494184071)) ;
#99981 = CARTESIAN_POINT('Ctrl Pts',(-18.4529336890425,-26.6825867511437,
122.677116975308)) ;
#99982 = CARTESIAN_POINT('Ctrl Pts',(-18.3408562350871,-26.6924795701081,
122.852362403782)) ;
#99983 = CARTESIAN_POINT('Ctrl Pts',(-18.2595725055753,-26.7025506876379,
123.047818395146)) ;
#99984 = CARTESIAN_POINT('Ctrl Pts',(-18.2143416825562,-26.712366381604,123.249196814553)) ;
#99985 = CARTESIAN_POINT('Ctrl Pts',(-18.2042182881577,-26.7224327591013,
123.4605366458)) ;
#99986 = CARTESIAN_POINT('Ctrl Pts',(-18.2305738252082,-26.7323317451832,
123.667021003824)) ;
#99987 = CARTESIAN_POINT('Ctrl Pts',(-18.2932434079137,-26.7423859251767,
123.868839194969)) ;
#99988 = CARTESIAN_POINT('Ctrl Pts',(-18.3880999685253,-26.7522567381094,
124.053460808556)) ;
#99989 = CARTESIAN_POINT('Ctrl Pts',(-18.5160984696686,-26.7623306389632,
124.222127178265)) ;
#99990 = CARTESIAN_POINT('Ctrl Pts',(-18.6674236528396,-26.7721507943498,
124.36263447732)) ;
#99991 = CARTESIAN_POINT('Ctrl Pts',(-18.8452192789956,-26.7822295013021,
124.477797245628)) ;
#99992 = CARTESIAN_POINT('Ctrl Pts',(-19.0359780972258,-26.7920810898409,
124.558583789374)) ;
#99993 = CARTESIAN_POINT('Ctrl Pts',(-19.2422791116803,-26.8021542063659,
124.606227050416)) ;
#99994 = CARTESIAN_POINT('Ctrl Pts',(-19.4489350806192,-26.8119967234617,
124.61704170027)) ;
#99995 = CARTESIAN_POINT('Ctrl Pts',(-19.657265177764,-26.8219771850156,124.592159458951)) ;
#99996 = CARTESIAN_POINT('Ctrl Pts',(-19.8587601458989,-26.8319954350064,
124.530862050043)) ;
#99997 = CARTESIAN_POINT('Ctrl Pts',(-20.0442514782667,-26.8418795952002,
124.437157726054)) ;
#99998 = CARTESIAN_POINT('Ctrl Pts',(-20.2136392911617,-26.8519447421752,
124.310379308639)) ;
#99999 = CARTESIAN_POINT('Ctrl Pts',(-20.3553384021326,-26.861786565816,124.159590264565)) ;
#100000 = CARTESIAN_POINT('Ctrl Pts',(-20.4713284113808,-26.8718160382768,
123.983514397752)) ;
#100001 = CARTESIAN_POINT('Ctrl Pts',(-20.5544240075123,-26.8818428935388,
123.789782297594)) ;
#100002 = CARTESIAN_POINT('Ctrl Pts',(-20.6022185711977,-26.8916861436494,
123.588438540082)) ;
#100003 = CARTESIAN_POINT('Ctrl Pts',(-20.6148661807325,-26.9017345832325,
123.377573493786)) ;
#100004 = CARTESIAN_POINT('Ctrl Pts',(-20.59061659497,-26.9116840774804,123.169813387432)) ;
#100005 = CARTESIAN_POINT('Ctrl Pts',(-20.5315083892542,-26.9215919332064,
122.970069920506)) ;
#100006 = CARTESIAN_POINT('Ctrl Pts',(-20.4370085337872,-26.9316514098564,
122.78090053012)) ;
#100007 = CARTESIAN_POINT('Ctrl Pts',(-20.3140323838183,-26.9414922192651,
122.614501406131)) ;
#100008 = CARTESIAN_POINT('Ctrl Pts',(-20.160875315783,-26.9515543695659,
122.468617984252)) ;
#100009 = CARTESIAN_POINT('Ctrl Pts',(-19.9874570121337,-26.9614515306884,
122.353625009764)) ;
#100010 = CARTESIAN_POINT('Ctrl Pts',(-19.7963431799956,-26.9713827050925,
122.2695743807)) ;
#100011 = CARTESIAN_POINT('Ctrl Pts',(-19.5912142351178,-26.9814249088175,
122.219653869201)) ;
#100012 = CARTESIAN_POINT('Ctrl Pts',(-19.383795497965,-26.9913114912479,
122.206165967071)) ;
#100013 = CARTESIAN_POINT('Ctrl Pts',(-19.1749362550269,-27.0013049269963,
122.228796140549)) ;
#100014 = CARTESIAN_POINT('Ctrl Pts',(-18.9741725316196,-27.0112493953544,
122.287126430853)) ;
#100015 = CARTESIAN_POINT('Ctrl Pts',(-18.7862673123072,-27.0212012116,122.379146720648)) ;
#100016 = CARTESIAN_POINT('Ctrl Pts',(-18.6158690070823,-27.0312386477145,
122.503600494927)) ;
#100017 = CARTESIAN_POINT('Ctrl Pts',(-18.4717243417291,-27.0411236068908,
122.65331996426)) ;
#100018 = CARTESIAN_POINT('Ctrl Pts',(-18.3542552366748,-27.0511217251028,
122.827593163894)) ;
#100019 = CARTESIAN_POINT('Ctrl Pts',(-18.2693381131155,-27.0610426576147,
123.018117585554)) ;
#100020 = CARTESIAN_POINT('Ctrl Pts',(-18.2181333214578,-27.0710839578368,
123.222902911602)) ;
#100021 = CARTESIAN_POINT('Ctrl Pts',(-18.2035332635739,-27.0809908762268,
123.43066695104)) ;
#100022 = CARTESIAN_POINT('Ctrl Pts',(-18.2246971739963,-27.0909266679358,
123.638474525358)) ;
#100023 = CARTESIAN_POINT('Ctrl Pts',(-18.2824280316472,-27.1009675625137,
123.841513117119)) ;
#100024 = CARTESIAN_POINT('Ctrl Pts',(-18.3729966212527,-27.1108547642276,
124.028616253587)) ;
#100025 = CARTESIAN_POINT('Ctrl Pts',(-18.4956721309728,-27.1208470319892,
124.199126087472)) ;
#100026 = CARTESIAN_POINT('Ctrl Pts',(-18.6454908462206,-27.130795553011,
124.345080292146)) ;
#100027 = CARTESIAN_POINT('Ctrl Pts',(-18.8179818182383,-27.1407323265887,
124.462892368018)) ;
#100028 = CARTESIAN_POINT('Ctrl Pts',(-19.0091256377102,-27.1507153747297,
124.54962477497)) ;
#100029 = CARTESIAN_POINT('Ctrl Pts',(-19.2137095401017,-27.1607590823398,
124.601783725474)) ;
#100030 = CARTESIAN_POINT('Ctrl Pts',(-19.4197466813637,-27.1705877754931,
124.617765589446)) ;
#100031 = CARTESIAN_POINT('Ctrl Pts',(-19.6305350239936,-27.1806625246225,
124.59738100197)) ;
#100032 = CARTESIAN_POINT('Ctrl Pts',(-19.8303786228286,-27.1905278504181,
124.541825331327)) ;
#100033 = CARTESIAN_POINT('Ctrl Pts',(-20.0207211667131,-27.200550024775,
124.451492552319)) ;
#100034 = CARTESIAN_POINT('Ctrl Pts',(-20.1922715461115,-27.2105760779819,
124.328999938793)) ;
#100035 = CARTESIAN_POINT('Ctrl Pts',(-20.3376266287696,-27.2204297748282,
124.181424461619)) ;
#100036 = CARTESIAN_POINT('Ctrl Pts',(-20.4569429249731,-27.2303891795812,
124.009361438835)) ;
#100037 = CARTESIAN_POINT('Ctrl Pts',(-20.5449154196545,-27.2404274252861,
123.817549450005)) ;
#100038 = CARTESIAN_POINT('Ctrl Pts',(-20.597745493795,-27.2503016094481,
123.616770199216)) ;
#100039 = CARTESIAN_POINT('Ctrl Pts',(-20.6152375325855,-27.260371392586,
123.405824523873)) ;
#100040 = CARTESIAN_POINT('Ctrl Pts',(-20.5963991040706,-27.2702046476068,
123.199941639478)) ;
#100041 = CARTESIAN_POINT('Ctrl Pts',(-20.5415922589756,-27.2802350737385,
122.996324402692)) ;
#100042 = CARTESIAN_POINT('Ctrl Pts',(-20.4516896032714,-27.2902666859255,
122.805537606304)) ;
#100043 = CARTESIAN_POINT('Ctrl Pts',(-20.3328415106183,-27.3000963827801,
122.636499258909)) ;
#100044 = CARTESIAN_POINT('Ctrl Pts',(-20.1844978081138,-27.3100858246826,
122.487836293675)) ;
#100045 = CARTESIAN_POINT('Ctrl Pts',(-20.0113567716327,-27.3201297166982,
122.366974388097)) ;
#100046 = CARTESIAN_POINT('Ctrl Pts',(-19.8242790181535,-27.3299512784675,
122.279594917877)) ;
#100047 = CARTESIAN_POINT('Ctrl Pts',(-19.6206587361092,-27.3399868500917,
122.224347830702)) ;
#100048 = CARTESIAN_POINT('Ctrl Pts',(-19.4106165955193,-27.3500161243735,
122.205937744427)) ;
#100049 = CARTESIAN_POINT('Ctrl Pts',(-19.204608702603,-27.3598499614921,
122.223368192372)) ;
#100050 = CARTESIAN_POINT('Ctrl Pts',(-19.0002654608499,-27.3699023575803,
122.277228790485)) ;
#100051 = CARTESIAN_POINT('Ctrl Pts',(-18.8106801280658,-27.3798391245308,
122.364987702527)) ;
#100052 = CARTESIAN_POINT('Ctrl Pts',(-18.6389579111016,-27.3897733595101,
122.48385080553)) ;
#100053 = CARTESIAN_POINT('Ctrl Pts',(-18.4892353562071,-27.3997971228369,
122.632140885794)) ;
#100054 = CARTESIAN_POINT('Ctrl Pts',(-18.3690785905819,-27.4096834642215,
122.801728546963)) ;
#100055 = CARTESIAN_POINT('Ctrl Pts',(-18.2788245114621,-27.4196725129885,
122.991353358483)) ;
#100056 = CARTESIAN_POINT('Ctrl Pts',(-18.2229994622623,-27.4297137336859,
123.194935290467)) ;
#100057 = CARTESIAN_POINT('Ctrl Pts',(-18.2034414900543,-27.4395463738638,
123.400717191931)) ;
#100058 = CARTESIAN_POINT('Ctrl Pts',(-18.2195809986131,-27.4495403031717,
123.610199098896)) ;
#100059 = CARTESIAN_POINT('Ctrl Pts',(-18.2724661121885,-27.4595695108523,
123.81430616005)) ;
#100060 = CARTESIAN_POINT('Ctrl Pts',(-18.358345281803,-27.4694453225564,
124.00334546028)) ;
#100061 = CARTESIAN_POINT('Ctrl Pts',(-18.4769975640081,-27.4794445495278,
124.176839726728)) ;
#100062 = CARTESIAN_POINT('Ctrl Pts',(-18.6225510048668,-27.4893540306835,
124.325929137091)) ;
#100063 = CARTESIAN_POINT('Ctrl Pts',(-18.7942080256267,-27.4994072609844,
124.449191144084)) ;
#100064 = CARTESIAN_POINT('Ctrl Pts',(-18.9811891233098,-27.5092778775354,
124.53921795475)) ;
#100065 = CARTESIAN_POINT('Ctrl Pts',(-19.1838754168697,-27.5192995392675,
124.596716113866)) ;
#100066 = CARTESIAN_POINT('Ctrl Pts',(-19.3935528071799,-27.5293223524486,
124.61767126676)) ;
#100067 = CARTESIAN_POINT('Ctrl Pts',(-19.6004260321875,-27.5391895169085,
124.602494376512)) ;
#100068 = CARTESIAN_POINT('Ctrl Pts',(-19.804228166654,-27.5491829591284,
124.551440544961)) ;
#100069 = CARTESIAN_POINT('Ctrl Pts',(-19.9966297488941,-27.5592146327288,
124.465075198791)) ;
#100070 = CARTESIAN_POINT('Ctrl Pts',(-20.1684257246606,-27.5690810678418,
124.348824220153)) ;
#100071 = CARTESIAN_POINT('Ctrl Pts',(-20.3194676940511,-27.5790685183749,
124.203009064734)) ;
#100072 = CARTESIAN_POINT('Ctrl Pts',(-20.4424950208796,-27.5890134482028,
124.033926313766)) ;
#100073 = CARTESIAN_POINT('Ctrl Pts',(-20.5350890829591,-27.5990583432579,
123.844155131381)) ;
#100074 = CARTESIAN_POINT('Ctrl Pts',(-20.5924512077816,-27.6089204049438,
123.644900800642)) ;
#100075 = CARTESIAN_POINT('Ctrl Pts',(-20.6150474430418,-27.6189121277306,
123.436078878761)) ;
#100076 = CARTESIAN_POINT('Ctrl Pts',(-20.6010482085292,-27.6288443419706,
123.227739743253)) ;
#100077 = CARTESIAN_POINT('Ctrl Pts',(-20.5515184561338,-27.6387836605363,
123.024732987733)) ;
#100078 = CARTESIAN_POINT('Ctrl Pts',(-20.4664320950726,-27.6488278353122,
122.831477511435)) ;
#100079 = CARTESIAN_POINT('Ctrl Pts',(-20.3512034263352,-27.6586983893772,
122.658901145543)) ;
#100080 = CARTESIAN_POINT('Ctrl Pts',(-20.2068262036804,-27.6686633717313,
122.50709968518)) ;
#100081 = CARTESIAN_POINT('Ctrl Pts',(-20.0369860087491,-27.6786940746212,
122.38211606819)) ;
#100082 = CARTESIAN_POINT('Ctrl Pts',(-19.8507376570184,-27.6885864146464,
122.28952717991)) ;
#100083 = CARTESIAN_POINT('Ctrl Pts',(-19.6480564370335,-27.6986396478063,
122.22972032493)) ;
#100084 = CARTESIAN_POINT('Ctrl Pts',(-19.4416112920202,-27.7085208922831,
122.206286393227)) ;
#100085 = CARTESIAN_POINT('Ctrl Pts',(-19.2311109415465,-27.7185540131541,
122.219090238787)) ;
#100086 = CARTESIAN_POINT('Ctrl Pts',(-19.0290181074154,-27.7284352234292,
122.26734253057)) ;
#100087 = CARTESIAN_POINT('Ctrl Pts',(-18.8349279540132,-27.7384972991985,
122.351381952076)) ;
#100088 = CARTESIAN_POINT('Ctrl Pts',(-18.6618829771477,-27.7483543575803,
122.465445371045)) ;
#100089 = CARTESIAN_POINT('Ctrl Pts',(-18.5089263241519,-27.7583489128693,
122.609456648845)) ;
#100090 = CARTESIAN_POINT('Ctrl Pts',(-18.3840648483023,-27.7682748004048,
122.776687428184)) ;
#100091 = CARTESIAN_POINT('Ctrl Pts',(-18.2891643530214,-27.7782998204,122.964852230341)) ;
#100092 = CARTESIAN_POINT('Ctrl Pts',(-18.2290739310952,-27.7881971975037,
123.164066850917)) ;
#100093 = CARTESIAN_POINT('Ctrl Pts',(-18.2038003185173,-27.7981874345846,
123.372572740902)) ;
#100094 = CARTESIAN_POINT('Ctrl Pts',(-18.2155715258891,-27.8082240473934,
123.58324239782)) ;
#100095 = CARTESIAN_POINT('Ctrl Pts',(-18.2625214255283,-27.8180739308114,
123.784933374561)) ;
#100096 = CARTESIAN_POINT('Ctrl Pts',(-18.3446460998548,-27.8280775477138,
123.978520570021)) ;
#100097 = CARTESIAN_POINT('Ctrl Pts',(-18.4591002632966,-27.838066959479,
124.154640787521)) ;
#100098 = CARTESIAN_POINT('Ctrl Pts',(-18.6028741455423,-27.8480857208238,
124.308533544381)) ;
#100099 = CARTESIAN_POINT('Ctrl Pts',(-18.8247600869896,-27.8613043962049,
124.475933926476)) ;
#100100 = CARTESIAN_POINT('Ctrl Pts',(-19.0869287704517,-27.8746147034496,
124.582416075969)) ;
#100101 = CARTESIAN_POINT('Ctrl Pts',(-19.3630784368199,-27.8878523696756,
124.616824795393)) ;
#100102 = CARTESIAN_POINT('Ctrl Pts',(-19.5713974536242,-27.8977720650863,
124.606952016333)) ;
#100103 = CARTESIAN_POINT('Ctrl Pts',(-19.7774918180567,-27.9078249320848,
124.560209617729)) ;
#100104 = CARTESIAN_POINT('Ctrl Pts',(-19.9686337853255,-27.9176803404141,
124.480202520899)) ;
#100105 = CARTESIAN_POINT('Ctrl Pts',(-20.1463794166959,-27.9277189720907,
124.366454990498)) ;
#100106 = CARTESIAN_POINT('Ctrl Pts',(-20.3519682549476,-27.9410211543577,
124.176828853793)) ;
#100107 = CARTESIAN_POINT('Ctrl Pts',(-20.5406264177097,-27.9575661674406,
123.879925196376)) ;
#100108 = CARTESIAN_POINT('Ctrl Pts',(-20.6172144425616,-27.9742181835168,
123.53423124174)) ;
#100109 = CARTESIAN_POINT('Ctrl Pts',(-20.6051273432698,-27.987441274422,
123.256523048381)) ;
#100110 = CARTESIAN_POINT('Ctrl Pts',(-20.5603980657828,-27.9974022339814,
123.051937942582)) ;
#100111 = CARTESIAN_POINT('Ctrl Pts',(-20.4800782065703,-28.0074270307325,
122.857100319193)) ;
#100112 = CARTESIAN_POINT('Ctrl Pts',(-20.3314043560015,-28.0206514781283,
122.622123870872)) ;
#100113 = CARTESIAN_POINT('Ctrl Pts',(-20.0717197146929,-28.0372852628274,
122.38210218691)) ;
#100114 = CARTESIAN_POINT('Ctrl Pts',(-19.6815155671731,-28.0571879295523,
122.218215393749)) ;
#100115 = CARTESIAN_POINT('Ctrl Pts',(-19.2589567092024,-28.0770881573342,
122.196772520774)) ;
#100116 = CARTESIAN_POINT('Ctrl Pts',(-18.8539833937904,-28.0970056448657,
122.320648397727)) ;
#100117 = CARTESIAN_POINT('Ctrl Pts',(-18.5152101161384,-28.1169351706826,
122.575243944621)) ;
#100118 = CARTESIAN_POINT('Ctrl Pts',(-18.2833376739866,-28.1368974385688,
122.930790621778)) ;
#100119 = CARTESIAN_POINT('Ctrl Pts',(-18.187048784328,-28.156787633521,123.34254491407)) ;
#100120 = CARTESIAN_POINT('Ctrl Pts',(-18.2360061965885,-28.1766778782673,
123.762715938737)) ;
#100121 = CARTESIAN_POINT('Ctrl Pts',(-18.4278813289792,-28.1967522508298,
124.14392922402)) ;
#100122 = CARTESIAN_POINT('Ctrl Pts',(-18.7338457185242,-28.2165376281901,
124.432743552464)) ;
#100123 = CARTESIAN_POINT('Ctrl Pts',(-19.1228314191686,-28.2364995022572,
124.602478423279)) ;
#100124 = CARTESIAN_POINT('Ctrl Pts',(-19.5468861640183,-28.2564794777477,
124.628297018886)) ;
#100125 = CARTESIAN_POINT('Ctrl Pts',(-19.9511281034896,-28.2762919076256,
124.509652729328)) ;
#100126 = CARTESIAN_POINT('Ctrl Pts',(-20.2937311768697,-28.2962720157159,
124.258579189441)) ;
#100127 = CARTESIAN_POINT('Ctrl Pts',(-20.5290187234776,-28.3161663993132,
123.906931333395)) ;
#100128 = CARTESIAN_POINT('Ctrl Pts',(-20.6306760277728,-28.3360933272904,
123.495704244006)) ;
#100129 = CARTESIAN_POINT('Ctrl Pts',(-20.5865144757859,-28.3559881845916,
123.074899434242)) ;
#100130 = CARTESIAN_POINT('Ctrl Pts',(-20.39973706112,-28.3760273781953,122.691977747606)) ;
#100131 = CARTESIAN_POINT('Ctrl Pts',(-20.0964200253337,-28.395867346106,
122.398729979472)) ;
#100132 = CARTESIAN_POINT('Ctrl Pts',(-19.7103074107296,-28.4157821630701,
122.22497327621)) ;
#100133 = CARTESIAN_POINT('Ctrl Pts',(-19.287471657815,-28.4357244084664,
122.193656982197)) ;
#100134 = CARTESIAN_POINT('Ctrl Pts',(-18.8804519656904,-28.4555964565809,
122.307451305372)) ;
#100135 = CARTESIAN_POINT('Ctrl Pts',(-18.5346617341029,-28.475607521535,
122.555147103181)) ;
#100136 = CARTESIAN_POINT('Ctrl Pts',(-18.295817531735,-28.4954190458386,
122.902370164939)) ;
#100137 = CARTESIAN_POINT('Ctrl Pts',(-18.1886236820666,-28.515514257802,
123.315810225157)) ;
#100138 = CARTESIAN_POINT('Ctrl Pts',(-18.2284238585173,-28.5352949817218,
123.734683495509)) ;
#100139 = CARTESIAN_POINT('Ctrl Pts',(-18.4096666532636,-28.5552860573646,
124.118996095771)) ;
#100140 = CARTESIAN_POINT('Ctrl Pts',(-18.709929841296,-28.5751679964076,
124.416746661381)) ;
#100141 = CARTESIAN_POINT('Ctrl Pts',(-19.0947697271538,-28.5951206009108,
124.595141703348)) ;
#100142 = CARTESIAN_POINT('Ctrl Pts',(-19.516360218223,-28.6150194696415,
124.631410649851)) ;
#100143 = CARTESIAN_POINT('Ctrl Pts',(-19.9249280278527,-28.6349128694511,
124.522202046666)) ;
#100144 = CARTESIAN_POINT('Ctrl Pts',(-20.2724837191931,-28.6548220002911,
124.280378884932)) ;
#100145 = CARTESIAN_POINT('Ctrl Pts',(-20.5176133707104,-28.6748541000547,
123.932100986152)) ;
#100146 = CARTESIAN_POINT('Ctrl Pts',(-20.6098155277601,-28.6913861732241,
123.592842898703)) ;
#100147 = CARTESIAN_POINT('Ctrl Pts',(-20.6110967779903,-28.7047215138301,
123.312512369001)) ;
#100148 = CARTESIAN_POINT('Ctrl Pts',(-20.5764613161187,-28.7145640723698,
123.108490737186)) ;
#100149 = CARTESIAN_POINT('Ctrl Pts',(-20.505664464291,-28.7246159792197,
122.909398070917)) ;
#100150 = CARTESIAN_POINT('Ctrl Pts',(-20.3681581178591,-28.7378644936106,
122.667197655362)) ;
#100151 = CARTESIAN_POINT('Ctrl Pts',(-20.1207677449184,-28.7544636685583,
122.415435813106)) ;
#100152 = CARTESIAN_POINT('Ctrl Pts',(-19.8026289126005,-28.7710524543534,
122.263225996982)) ;
#100153 = CARTESIAN_POINT('Ctrl Pts',(-19.5282808762314,-28.7843282706954,
122.211756040343)) ;
#100154 = CARTESIAN_POINT('Ctrl Pts',(-19.3186094838099,-28.7943021214892,
122.209171003004)) ;
#100155 = CARTESIAN_POINT('Ctrl Pts',(-19.1105750903237,-28.8043311535816,
122.243437364695)) ;
#100156 = CARTESIAN_POINT('Ctrl Pts',(-18.9143171416394,-28.8142212790835,
122.312136720202)) ;
#100157 = CARTESIAN_POINT('Ctrl Pts',(-18.7309861960739,-28.824213757355,
122.414657328646)) ;
#100158 = CARTESIAN_POINT('Ctrl Pts',(-18.5687975393856,-28.8341649724524,
122.546853392667)) ;
#100159 = CARTESIAN_POINT('Ctrl Pts',(-18.4308556654562,-28.8442134742074,
122.706820780171)) ;
#100160 = CARTESIAN_POINT('Ctrl Pts',(-18.32478432042,-28.8540548238242,122.884481245149)) ;
#100161 = CARTESIAN_POINT('Ctrl Pts',(-18.2496867593688,-28.8640411148444,
123.080496845909)) ;
#100162 = CARTESIAN_POINT('Ctrl Pts',(-18.2098480762746,-28.873977726573,
123.28559731834)) ;
#100163 = CARTESIAN_POINT('Ctrl Pts',(-18.2062920944329,-28.8840276019406,
123.496826027308)) ;
#100164 = CARTESIAN_POINT('Ctrl Pts',(-18.2386605052024,-28.893878060476,
123.70138378029)) ;
#100165 = CARTESIAN_POINT('Ctrl Pts',(-18.3063536110036,-28.9038499974288,
123.89976815632)) ;
#100166 = CARTESIAN_POINT('Ctrl Pts',(-18.407760255829,-28.9138454543609,
124.083853248681)) ;
#100167 = CARTESIAN_POINT('Ctrl Pts',(-18.5402393517923,-28.923878261414,
124.247960447026)) ;
#100168 = CARTESIAN_POINT('Ctrl Pts',(-18.6962940053379,-28.9337381480039,
124.38441134542)) ;
#100169 = CARTESIAN_POINT('Ctrl Pts',(-18.8757659217663,-28.9437272285692,
124.493420411958)) ;
#100170 = CARTESIAN_POINT('Ctrl Pts',(-19.0703341933737,-28.9536587077783,
124.569178765791)) ;
#100171 = CARTESIAN_POINT('Ctrl Pts',(-19.2761626232485,-28.9636445672243,
124.610567523004)) ;
#100172 = CARTESIAN_POINT('Ctrl Pts',(-19.487130367864,-28.9736827178714,
124.615242556672)) ;
#100173 = CARTESIAN_POINT('Ctrl Pts',(-19.6918527231933,-28.9835308083759,
124.58423421785)) ;
#100174 = CARTESIAN_POINT('Ctrl Pts',(-19.8923396300978,-28.9935917168938,
124.516905030779)) ;
#100175 = CARTESIAN_POINT('Ctrl Pts',(-20.0749919579206,-29.0034865640518,
124.417310799269)) ;
#100176 = CARTESIAN_POINT('Ctrl Pts',(-20.2386582356923,-29.0134282360969,
124.287364248186)) ;
#100177 = CARTESIAN_POINT('Ctrl Pts',(-20.3782212765855,-29.0234307632223,
124.130031009464)) ;
#100178 = CARTESIAN_POINT('Ctrl Pts',(-20.4883954034686,-29.0334655544098,
123.950138201724)) ;
#100179 = CARTESIAN_POINT('Ctrl Pts',(-20.564531957428,-29.0433104342689,
123.757665827761)) ;
#100180 = CARTESIAN_POINT('Ctrl Pts',(-20.6070652567906,-29.0532963148874,
123.552119523767)) ;
#100181 = CARTESIAN_POINT('Ctrl Pts',(-20.613383776334,-29.0632310379806,
123.343316504364)) ;
#100182 = CARTESIAN_POINT('Ctrl Pts',(-20.5827972106513,-29.0732888782918,
123.13412518274)) ;
#100183 = CARTESIAN_POINT('Ctrl Pts',(-20.5182188079825,-29.0831093656883,
122.937999640139)) ;
#100184 = CARTESIAN_POINT('Ctrl Pts',(-20.4185157191678,-29.0931697670334,
122.75150196269)) ;
#100185 = CARTESIAN_POINT('Ctrl Pts',(-20.289372730469,-29.1031007325863,
122.587425312778)) ;
#100186 = CARTESIAN_POINT('Ctrl Pts',(-20.1339227573325,-29.1130395949228,
122.447837729937)) ;
#100187 = CARTESIAN_POINT('Ctrl Pts',(-19.9557965520162,-29.123025325849,
122.336697470279)) ;
#100188 = CARTESIAN_POINT('Ctrl Pts',(-19.7602776862953,-29.1330497112764,
122.258091852478)) ;
#100189 = CARTESIAN_POINT('Ctrl Pts',(-19.556595626797,-29.1429529956297,
122.214833769334)) ;
#100190 = CARTESIAN_POINT('Ctrl Pts',(-19.3452532261386,-29.1530130002077,
122.207556053046)) ;
#100191 = CARTESIAN_POINT('Ctrl Pts',(-19.1403035461361,-29.1628562692768,
122.236311196594)) ;
#100192 = CARTESIAN_POINT('Ctrl Pts',(-18.940407846898,-29.1728468348845,
122.300692953073)) ;
#100193 = CARTESIAN_POINT('Ctrl Pts',(-18.7558729360837,-29.1827749666633,
122.398237499095)) ;
#100194 = CARTESIAN_POINT('Ctrl Pts',(-18.5898613802247,-29.1927628537442,
122.526823549317)) ;
#100195 = CARTESIAN_POINT('Ctrl Pts',(-18.4482966960436,-29.2027988033129,
122.683257170632)) ;
#100196 = CARTESIAN_POINT('Ctrl Pts',(-18.3377647682607,-29.2126536896917,
122.858509371114)) ;
#100197 = CARTESIAN_POINT('Ctrl Pts',(-18.2579463028601,-29.2226531040396,
123.052947689743)) ;
#100198 = CARTESIAN_POINT('Ctrl Pts',(-18.2133359503066,-29.2325482692301,
123.256171150015)) ;
#100199 = CARTESIAN_POINT('Ctrl Pts',(-18.2045696961319,-29.242608587922,
123.467461085334)) ;
#100200 = CARTESIAN_POINT('Ctrl Pts',(-18.2319223637869,-29.2524587196981,
123.672745692546)) ;
#100201 = CARTESIAN_POINT('Ctrl Pts',(-18.2951669463727,-29.2624892901484,
123.873902441532)) ;
#100202 = CARTESIAN_POINT('Ctrl Pts',(-18.3926450082299,-29.2725034408212,
124.060518212084)) ;
#100203 = CARTESIAN_POINT('Ctrl Pts',(-18.5192189833344,-29.2823963743666,
124.225552599469)) ;
#100204 = CARTESIAN_POINT('Ctrl Pts',(-18.6738430227356,-29.2923858883568,
124.367635544127)) ;
#100205 = CARTESIAN_POINT('Ctrl Pts',(-18.8501232113123,-29.3023396590093,
124.480451237584)) ;
#100206 = CARTESIAN_POINT('Ctrl Pts',(-19.0451644894484,-29.3123874276698,
124.56151112699)) ;
#100207 = CARTESIAN_POINT('Ctrl Pts',(-19.2470735425308,-29.3222291541096,
124.606778815765)) ;
#100208 = CARTESIAN_POINT('Ctrl Pts',(-19.4567244182723,-29.3322146709324,
124.616894986264)) ;
#100209 = CARTESIAN_POINT('Ctrl Pts',(-19.6640557016373,-29.342154002628,
124.590645851419)) ;
#100210 = CARTESIAN_POINT('Ctrl Pts',(-19.8656384728452,-29.3521937723255,
124.528141793772)) ;
#100211 = CARTESIAN_POINT('Ctrl Pts',(-20.050544943579,-29.3620819335743,
124.433122021013)) ;
#100212 = CARTESIAN_POINT('Ctrl Pts',(-20.2180648805147,-29.3720714880767,
124.306476690643)) ;
#100213 = CARTESIAN_POINT('Ctrl Pts',(-20.360489219065,-29.3820299026003,
124.153037488567)) ;
#100214 = CARTESIAN_POINT('Ctrl Pts',(-20.4738773634079,-29.3919298154297,
123.978495694279)) ;
#100215 = CARTESIAN_POINT('Ctrl Pts',(-20.5563746904274,-29.4019765150796,
123.78408171757)) ;
#100216 = CARTESIAN_POINT('Ctrl Pts',(-20.6033086955046,-29.4118763753852,
123.581284061447)) ;
#100217 = CARTESIAN_POINT('Ctrl Pts',(-20.6145520873745,-29.4219277795906,
123.370300742644)) ;
#100218 = CARTESIAN_POINT('Ctrl Pts',(-20.5894921806618,-29.4318088165118,
123.164057071259)) ;
#100219 = CARTESIAN_POINT('Ctrl Pts',(-20.5285675602562,-29.4418086486893,
122.962886999942)) ;
#100220 = CARTESIAN_POINT('Ctrl Pts',(-20.434537058349,-29.4517266516742,
122.776744976066)) ;
#100221 = CARTESIAN_POINT('Ctrl Pts',(-20.307923453941,-29.4617779575487,
122.60761220453)) ;
#100222 = CARTESIAN_POINT('Ctrl Pts',(-20.1567634033174,-29.4716477809403,
122.46540429658)) ;
#100223 = CARTESIAN_POINT('Ctrl Pts',(-19.9796844490929,-29.4817219469906,
122.349309672311)) ;
#100224 = CARTESIAN_POINT('Ctrl Pts',(-19.7900581030322,-29.4915420311322,
122.267561975256)) ;
#100225 = CARTESIAN_POINT('Ctrl Pts',(-19.5839697980926,-29.5016207578681,
122.21855619622)) ;
#100226 = CARTESIAN_POINT('Ctrl Pts',(-19.3771735122787,-29.5114723385176,
122.20628301053)) ;
#100227 = CARTESIAN_POINT('Ctrl Pts',(-19.1668254789416,-29.521545466816,
122.230443838208)) ;
#100228 = CARTESIAN_POINT('Ctrl Pts',(-18.968471044131,-29.5313879447074,
122.289426612653)) ;
#100229 = CARTESIAN_POINT('Ctrl Pts',(-18.7804867116248,-29.5413685513055,
122.382611095653)) ;
#100230 = CARTESIAN_POINT('Ctrl Pts',(-18.6111370847585,-29.5513862603243,
122.507808447672)) ;
#100231 = CARTESIAN_POINT('Ctrl Pts',(-18.467698534916,-29.5612724393617,
122.658237466472)) ;
#100232 = CARTESIAN_POINT('Ctrl Pts',(-18.3505689068955,-29.571330051934,
122.834251493888)) ;
#100233 = CARTESIAN_POINT('Ctrl Pts',(-18.2672767957085,-29.5812064453062,
123.024459052734)) ;
#100234 = CARTESIAN_POINT('Ctrl Pts',(-18.2171823110383,-29.5912014734566,
123.22852120628)) ;
#100235 = CARTESIAN_POINT('Ctrl Pts',(-18.203603812341,-29.6012222203026,
123.438760173548)) ;
#100236 = CARTESIAN_POINT('Ctrl Pts',(-18.2262184939456,-29.611124288969,
123.645698374029)) ;
#100237 = CARTESIAN_POINT('Ctrl Pts',(-18.28464557159,-29.6211150287887,123.847446278539)) ;
#100238 = CARTESIAN_POINT('Ctrl Pts',(-18.377093753919,-29.631078224999,124.035386742877)) ;
#100239 = CARTESIAN_POINT('Ctrl Pts',(-18.499638362414,-29.6409824092991,
124.20374661496)) ;
#100240 = CARTESIAN_POINT('Ctrl Pts',(-18.652011710057,-29.65104286969,124.350391637579)) ;
#100241 = CARTESIAN_POINT('Ctrl Pts',(-18.8235918424603,-29.6608834155608,
124.466022295427)) ;
#100242 = CARTESIAN_POINT('Ctrl Pts',(-19.0167459125996,-29.6709456362725,
124.552225117033)) ;
#100243 = CARTESIAN_POINT('Ctrl Pts',(-19.2186520266094,-29.6808427792891,
124.602535489346)) ;
#100244 = CARTESIAN_POINT('Ctrl Pts',(-19.4268756683955,-29.6907739557063,
124.617765857914)) ;
#100245 = CARTESIAN_POINT('Ctrl Pts',(-19.6368811457771,-29.7008161694849,
124.596142976197)) ;
#100246 = CARTESIAN_POINT('Ctrl Pts',(-19.8368504110296,-29.7107027096876,
124.539424761433)) ;
#100247 = CARTESIAN_POINT('Ctrl Pts',(-20.0260826067739,-29.720696304293,
124.448182212986)) ;
#100248 = CARTESIAN_POINT('Ctrl Pts',(-20.1957535071456,-29.7306401794506,
124.326037135567)) ;
#100249 = CARTESIAN_POINT('Ctrl Pts',(-20.3420619715564,-29.7406007155654,
124.176246066117)) ;
#100250 = CARTESIAN_POINT('Ctrl Pts',(-20.4606917552971,-29.7505973188881,
124.002742680431)) ;
#100251 = CARTESIAN_POINT('Ctrl Pts',(-20.5474262529817,-29.7606304018426,
123.81047883451)) ;
#100252 = CARTESIAN_POINT('Ctrl Pts',(-20.5987706274766,-29.7704815705442,
123.609845833871)) ;
#100253 = CARTESIAN_POINT('Ctrl Pts',(-20.6152927534898,-29.7804440612431,
123.401063287717)) ;
#100254 = CARTESIAN_POINT('Ctrl Pts',(-20.5949181650061,-29.7904724896608,
123.191208734176)) ;
#100255 = CARTESIAN_POINT('Ctrl Pts',(-20.539151487676,-29.8003828570254,
122.990473847779)) ;
#100256 = CARTESIAN_POINT('Ctrl Pts',(-20.449643079689,-29.8103177246405,
122.801756688701)) ;
#100257 = CARTESIAN_POINT('Ctrl Pts',(-20.3272805265275,-29.8203588666195,
122.629750103717)) ;
#100258 = CARTESIAN_POINT('Ctrl Pts',(-20.1793067343655,-29.8302460028227,
122.48375783229)) ;
#100259 = CARTESIAN_POINT('Ctrl Pts',(-20.0066330492026,-29.8402382852261,
122.364147144543)) ;
#100260 = CARTESIAN_POINT('Ctrl Pts',(-19.8166010888056,-29.8501868131913,
122.276761833727)) ;
#100261 = CARTESIAN_POINT('Ctrl Pts',(-19.6146259199445,-29.8601235443534,
122.223483742301)) ;
#100262 = CARTESIAN_POINT('Ctrl Pts',(-19.4054733113164,-29.8701067552134,
122.205738011186)) ;
#100263 = CARTESIAN_POINT('Ctrl Pts',(-19.1952435383892,-29.8801498543633,
122.225063273149)) ;
#100264 = CARTESIAN_POINT('Ctrl Pts',(-18.995698872157,-29.8899808186382,
122.27899071721)) ;
#100265 = CARTESIAN_POINT('Ctrl Pts',(-18.8039305084368,-29.9000536710241,
122.368740289525)) ;
#100266 = CARTESIAN_POINT('Ctrl Pts',(-18.6342252081658,-29.9099177987359,
122.48796337269)) ;
#100267 = CARTESIAN_POINT('Ctrl Pts',(-18.4851060056802,-29.9199400008708,
122.636805533423)) ;
#100268 = CARTESIAN_POINT('Ctrl Pts',(-18.3644327027992,-29.9299671938392,
122.809667978915)) ;
#100269 = CARTESIAN_POINT('Ctrl Pts',(-18.2768442246411,-29.9398227878062,
122.997422288897)) ;
#100270 = CARTESIAN_POINT('Ctrl Pts',(-18.2220256383135,-29.9497799596715,
123.199455787164)) ;
#100271 = CARTESIAN_POINT('Ctrl Pts',(-18.2033282561519,-29.9598188036699,
123.40966145316)) ;
#100272 = CARTESIAN_POINT('Ctrl Pts',(-18.2207544000821,-29.9696928275454,
123.616539274817)) ;
#100273 = CARTESIAN_POINT('Ctrl Pts',(-18.2748812707176,-29.9797626535358,
123.821172180483)) ;
#100274 = CARTESIAN_POINT('Ctrl Pts',(-18.3615486455234,-29.9895958974331,
124.008872346803)) ;
#100275 = CARTESIAN_POINT('Ctrl Pts',(-18.4813509838406,-29.9996263252062,
124.182398051882)) ;
#100276 = CARTESIAN_POINT('Ctrl Pts',(-18.6299300191435,-30.0096579419513,
124.332085759338)) ;
#100277 = CARTESIAN_POINT('Ctrl Pts',(-18.798504200778,-30.019487618932,124.45159045083)) ;
#100278 = CARTESIAN_POINT('Ctrl Pts',(-18.9880545166337,-30.0294771357719,
124.542022845038)) ;
#100279 = CARTESIAN_POINT('Ctrl Pts',(-19.1916571634689,-30.0395207479117,
124.597954395009)) ;
#100280 = CARTESIAN_POINT('Ctrl Pts',(-19.3972171314723,-30.049343354247,
124.617681414691)) ;
#100281 = CARTESIAN_POINT('Ctrl Pts',(-19.6076268635285,-30.0593815841462,
124.601538954227)) ;
#100282 = CARTESIAN_POINT('Ctrl Pts',(-19.8113833290408,-30.0693926189382,
124.548770180719)) ;
#100283 = CARTESIAN_POINT('Ctrl Pts',(-20.0008354917922,-30.0792903499053,
124.462723134788)) ;
#100284 = CARTESIAN_POINT('Ctrl Pts',(-20.1742196235901,-30.0892799777558,
124.34422161032)) ;
#100285 = CARTESIAN_POINT('Ctrl Pts',(-20.3238339741852,-30.0992357682018,
124.197860233592)) ;
#100286 = CARTESIAN_POINT('Ctrl Pts',(-20.4457452944911,-30.1091631667638,
124.028453476288)) ;
#100287 = CARTESIAN_POINT('Ctrl Pts',(-20.5372249558593,-30.1191887618737,
123.838579282323)) ;
#100288 = CARTESIAN_POINT('Ctrl Pts',(-20.5936754538382,-30.1290746125433,
123.638560030747)) ;
#100289 = CARTESIAN_POINT('Ctrl Pts',(-20.6152518902951,-30.1390637923875,
123.429661564444)) ;
#100290 = CARTESIAN_POINT('Ctrl Pts',(-20.5997105862796,-30.149104979491,
123.219137564455)) ;
#100291 = CARTESIAN_POINT('Ctrl Pts',(-20.549258857753,-30.158937622967,123.018679749049)) ;
#100292 = CARTESIAN_POINT('Ctrl Pts',(-20.4639295996875,-30.1689315726765,
122.82668449948)) ;
#100293 = CARTESIAN_POINT('Ctrl Pts',(-20.3457758863087,-30.178960695453,
122.652054277009)) ;
#100294 = CARTESIAN_POINT('Ctrl Pts',(-20.2015667374452,-30.1888368263717,
122.50266546943)) ;
#100295 = CARTESIAN_POINT('Ctrl Pts',(-20.0317095857763,-30.1988348613887,
122.378900047192)) ;
#100296 = CARTESIAN_POINT('Ctrl Pts',(-19.8445560545185,-30.2087487911474,
122.287118076493)) ;
#100297 = CARTESIAN_POINT('Ctrl Pts',(-19.6417509926831,-30.2187919788852,
122.228441088149)) ;
#100298 = CARTESIAN_POINT('Ctrl Pts',(-19.4348089198405,-30.2286918210256,
122.206175419555)) ;
#100299 = CARTESIAN_POINT('Ctrl Pts',(-19.2252055891739,-30.2386830878336,
122.219861948835)) ;
#100300 = CARTESIAN_POINT('Ctrl Pts',(-19.0204144352866,-30.2487151899655,
122.270293253069)) ;
#100301 = CARTESIAN_POINT('Ctrl Pts',(-18.8305639825601,-30.2585820709203,
122.353859503755)) ;
#100302 = CARTESIAN_POINT('Ctrl Pts',(-18.655638716602,-30.2685738622084,
122.470167887467)) ;
#100303 = CARTESIAN_POINT('Ctrl Pts',(-18.5032370808643,-30.27860597812,122.615959246412)) ;
#100304 = CARTESIAN_POINT('Ctrl Pts',(-18.380266553391,-30.28847229492,122.78300829887)) ;
#100305 = CARTESIAN_POINT('Ctrl Pts',(-18.2867460459699,-30.2984597763936,
122.970970801034)) ;
#100306 = CARTESIAN_POINT('Ctrl Pts',(-18.2274133436767,-30.3084047007725,
123.171480839467)) ;
#100307 = CARTESIAN_POINT('Ctrl Pts',(-18.2036829184807,-30.3184495866832,
123.381298877807)) ;
#100308 = CARTESIAN_POINT('Ctrl Pts',(-18.2163274014686,-30.3283116903958,
123.588260215081)) ;
#100309 = CARTESIAN_POINT('Ctrl Pts',(-18.2649310241986,-30.3383032542202,
123.792598164554)) ;
#100310 = CARTESIAN_POINT('Ctrl Pts',(-18.3478715849791,-30.3482360622831,
123.984238282877)) ;
#100311 = CARTESIAN_POINT('Ctrl Pts',(-18.462455355806,-30.3581731645195,
124.158935141286)) ;
#100312 = CARTESIAN_POINT('Ctrl Pts',(-18.6074774185911,-30.3682256107899,
124.312635696934)) ;
#100313 = CARTESIAN_POINT('Ctrl Pts',(-18.7733545831817,-30.3780717263715,
124.436489094269)) ;
#100314 = CARTESIAN_POINT('Ctrl Pts',(-18.9618306176264,-30.3881197460864,
124.531848059648)) ;
#100315 = CARTESIAN_POINT('Ctrl Pts',(-19.1619768274087,-30.3980616977153,
124.592115865803)) ;
#100316 = CARTESIAN_POINT('Ctrl Pts',(-19.3694102207659,-30.4080004787144,
124.61722092168)) ;
#100317 = CARTESIAN_POINT('Ctrl Pts',(-19.579859127954,-30.4180265274405,
124.605669432039)) ;
#100318 = CARTESIAN_POINT('Ctrl Pts',(-19.7823544284692,-30.4279133878487,
124.558666010419)) ;
#100319 = CARTESIAN_POINT('Ctrl Pts',(-19.9763868979473,-30.4379446629805,
124.476138593555)) ;
#100320 = CARTESIAN_POINT('Ctrl Pts',(-20.150710848517,-30.4478276402809,
124.363008702625)) ;
#100321 = CARTESIAN_POINT('Ctrl Pts',(-20.3053499579185,-30.4578844936881,
124.218906879609)) ;
#100322 = CARTESIAN_POINT('Ctrl Pts',(-20.4724661045215,-30.471052734764,
123.998074625091)) ;
#100323 = CARTESIAN_POINT('Ctrl Pts',(-20.5799187744265,-30.4844537639905,
123.734274660572)) ;
#100324 = CARTESIAN_POINT('Ctrl Pts',(-20.614229275413,-30.4976666807214,
123.458583483364)) ;
#100325 = CARTESIAN_POINT('Ctrl Pts',(-20.6043586056399,-30.5075950751746,
123.250125848871)) ;
#100326 = CARTESIAN_POINT('Ctrl Pts',(-20.5583338965781,-30.5175765753027,
123.045363393394)) ;
#100327 = CARTESIAN_POINT('Ctrl Pts',(-20.4767223293854,-30.5276171185728,
122.850706285029)) ;
#100328 = CARTESIAN_POINT('Ctrl Pts',(-20.3649484415365,-30.5374664503559,
122.676398462393)) ;
#100329 = CARTESIAN_POINT('Ctrl Pts',(-20.2229259385212,-30.5474618548276,
122.521525763836)) ;
#100330 = CARTESIAN_POINT('Ctrl Pts',(-20.055590612675,-30.5574781822762,
122.393695527064)) ;
#100331 = CARTESIAN_POINT('Ctrl Pts',(-19.8088968704393,-30.5707018394427,
122.265445396)) ;
#100332 = CARTESIAN_POINT('Ctrl Pts',(-19.5330272759911,-30.5839961308321,
122.203984398556)) ;
#100333 = CARTESIAN_POINT('Ctrl Pts',(-19.2539915535658,-30.5972804817636,
122.215885118148)) ;
#100334 = CARTESIAN_POINT('Ctrl Pts',(-19.0492501530024,-30.6072528628254,
122.260890607378)) ;
#100335 = CARTESIAN_POINT('Ctrl Pts',(-18.8564975573062,-30.617161242451,
122.339933470816)) ;
#100336 = CARTESIAN_POINT('Ctrl Pts',(-18.6778988120738,-30.627215241199,
122.452935135198)) ;
#100337 = CARTESIAN_POINT('Ctrl Pts',(-18.5244773338489,-30.6370774383153,
122.592422295361)) ;
#100338 = CARTESIAN_POINT('Ctrl Pts',(-18.3524363986144,-30.6504245646895,
122.814098624358)) ;
#100339 = CARTESIAN_POINT('Ctrl Pts',(-18.2159932726627,-30.6669615303309,
123.138166506218)) ;
#100340 = CARTESIAN_POINT('Ctrl Pts',(-18.1976709541361,-30.6835961345048,
123.491378907598)) ;
#100341 = CARTESIAN_POINT('Ctrl Pts',(-18.2560581551633,-30.6968859277475,
123.764606668898)) ;
#100342 = CARTESIAN_POINT('Ctrl Pts',(-18.3343798010391,-30.7068385590069,
123.958616577234)) ;
#100343 = CARTESIAN_POINT('Ctrl Pts',(-18.4450022346153,-30.7167905263116,
124.136223864481)) ;
#100344 = CARTESIAN_POINT('Ctrl Pts',(-18.6328487890167,-30.7301577847754,
124.345213848635)) ;
#100345 = CARTESIAN_POINT('Ctrl Pts',(-18.9269898158892,-30.7466745967245,
124.537244024158)) ;
#100346 = CARTESIAN_POINT('Ctrl Pts',(-19.3414672375764,-30.7667004917309,
124.634317542057)) ;
#100347 = CARTESIAN_POINT('Ctrl Pts',(-19.7598558729639,-30.7865112218611,
124.584765800214)) ;
#100348 = CARTESIAN_POINT('Ctrl Pts',(-20.1396861267888,-30.8064884379909,
124.394694836617)) ;
#100349 = CARTESIAN_POINT('Ctrl Pts',(-20.4305654395463,-30.8264153133862,
124.086654808637)) ;
#100350 = CARTESIAN_POINT('Ctrl Pts',(-20.5992560862809,-30.8462367748625,
123.700365845776)) ;
#100351 = CARTESIAN_POINT('Ctrl Pts',(-20.6260517237309,-30.8663110926718,
123.274438587329)) ;
#100352 = CARTESIAN_POINT('Ctrl Pts',(-20.5068007041979,-30.8861590616797,
122.869494454809)) ;
#100353 = CARTESIAN_POINT('Ctrl Pts',(-20.256100091772,-30.9061060957429,
122.527507021218)) ;
#100354 = CARTESIAN_POINT('Ctrl Pts',(-19.9044847264426,-30.926002046715,
122.292221832877)) ;
#100355 = CARTESIAN_POINT('Ctrl Pts',(-19.4939183858099,-30.9458975263333,
122.190385255119)) ;
#100356 = CARTESIAN_POINT('Ctrl Pts',(-19.0718958798579,-30.9658536372981,
122.234812006906)) ;
#100357 = CARTESIAN_POINT('Ctrl Pts',(-18.6914880022372,-30.9857581853381,
122.420176892331)) ;
#100358 = CARTESIAN_POINT('Ctrl Pts',(-18.3967602146309,-31.0056323096572,
122.723120461639)) ;
#100359 = CARTESIAN_POINT('Ctrl Pts',(-18.2221440715187,-31.0256868396562,
123.112068315082)) ;
#100360 = CARTESIAN_POINT('Ctrl Pts',(-18.1909870001939,-31.0454943534162,
123.532166264538)) ;
#100361 = CARTESIAN_POINT('Ctrl Pts',(-18.3051668991644,-31.0654777091839,
123.941375976223)) ;
#100362 = CARTESIAN_POINT('Ctrl Pts',(-18.551882465487,-31.0853960117678,
124.285605612131)) ;
#100363 = CARTESIAN_POINT('Ctrl Pts',(-18.8998089612952,-31.1052642272136,
124.525367364196)) ;
#100364 = CARTESIAN_POINT('Ctrl Pts',(-19.3123806313165,-31.1253145440099,
124.632280073311)) ;
#100365 = CARTESIAN_POINT('Ctrl Pts',(-19.7312117429744,-31.1450906058923,
124.59307290429)) ;
#100366 = CARTESIAN_POINT('Ctrl Pts',(-20.1167006281038,-31.1651452115848,
124.411195916949)) ;
#100367 = CARTESIAN_POINT('Ctrl Pts',(-20.4131994881279,-31.1849389007407,
124.112322500088)) ;
#100368 = CARTESIAN_POINT('Ctrl Pts',(-20.5924160483251,-31.2049055923351,
123.727557898885)) ;
#100369 = CARTESIAN_POINT('Ctrl Pts',(-20.6289177402634,-31.224865638086,
123.304647462231)) ;
#100370 = CARTESIAN_POINT('Ctrl Pts',(-20.5195485176998,-31.2447638982363,
122.895963140412)) ;
#100371 = CARTESIAN_POINT('Ctrl Pts',(-20.2777396586892,-31.2646588137855,
122.548891970213)) ;
#100372 = CARTESIAN_POINT('Ctrl Pts',(-19.9319582487345,-31.2845689941991,
122.304652435842)) ;
#100373 = CARTESIAN_POINT('Ctrl Pts',(-19.5230956618841,-31.3045047933133,
122.19273763541)) ;
#100374 = CARTESIAN_POINT('Ctrl Pts',(-19.1005559531157,-31.3244426549675,
122.227039031077)) ;
#100375 = CARTESIAN_POINT('Ctrl Pts',(-18.7153142184441,-31.3443617016051,
122.403079243365)) ;
#100376 = CARTESIAN_POINT('Ctrl Pts',(-18.4127971254137,-31.3643105996593,
122.70039658677)) ;
#100377 = CARTESIAN_POINT('Ctrl Pts',(-18.2301812697165,-31.3842164271023,
123.082254222056)) ;
#100378 = CARTESIAN_POINT('Ctrl Pts',(-18.1953741335306,-31.4007991224676,
123.433044629)) ;
#100379 = CARTESIAN_POINT('Ctrl Pts',(-18.2402816501959,-31.4140733361913,
123.708538677941)) ;
#100380 = CARTESIAN_POINT('Ctrl Pts',(-18.3100454084838,-31.4241200553906,
123.907868173339)) ;
#100381 = CARTESIAN_POINT('Ctrl Pts',(-18.4111023052277,-31.4339640900363,
124.088497852001)) ;
#100382 = CARTESIAN_POINT('Ctrl Pts',(-18.5878427013648,-31.4472984749408,
124.306014534584)) ;
#100383 = CARTESIAN_POINT('Ctrl Pts',(-18.8736728375836,-31.4638856922406,
124.512815831529)) ;
#100384 = CARTESIAN_POINT('Ctrl Pts',(-19.2135918164247,-31.4805189042785,
124.610143193857)) ;
#100385 = CARTESIAN_POINT('Ctrl Pts',(-19.4928519996131,-31.4938013465506,
124.614857715672)) ;
#100386 = CARTESIAN_POINT('Ctrl Pts',(-19.6985677489002,-31.5037072344649,
124.582580227291)) ;
#100387 = CARTESIAN_POINT('Ctrl Pts',(-19.8973118043881,-31.51369565257,124.514752480647)) ;
#100388 = CARTESIAN_POINT('Ctrl Pts',(-20.0817894730488,-31.5237190798087,
124.412897180446)) ;
#100389 = CARTESIAN_POINT('Ctrl Pts',(-20.2438978628984,-31.5336235109258,
124.282224230493)) ;
#100390 = CARTESIAN_POINT('Ctrl Pts',(-20.4278529675942,-31.5468866635362,
124.072693777294)) ;
#100391 = CARTESIAN_POINT('Ctrl Pts',(-20.5532324035977,-31.5602115614401,
123.818652228743)) ;
#100392 = CARTESIAN_POINT('Ctrl Pts',(-20.6078115713069,-31.5734673050557,
123.545311894165)) ;
#100393 = CARTESIAN_POINT('Ctrl Pts',(-20.6128436230812,-31.583426678503,
123.33602567504)) ;
#100394 = CARTESIAN_POINT('Ctrl Pts',(-20.5817628387508,-31.5933705024299,
123.12927158967)) ;
#100395 = CARTESIAN_POINT('Ctrl Pts',(-20.5144000298639,-31.6034184465772,
122.929077707166)) ;
#100396 = CARTESIAN_POINT('Ctrl Pts',(-20.4154292200081,-31.6132694177954,
122.747144547416)) ;
#100397 = CARTESIAN_POINT('Ctrl Pts',(-20.2852347142134,-31.6232412352375,
122.582864786111)) ;
#100398 = CARTESIAN_POINT('Ctrl Pts',(-20.128059609092,-31.6332366575296,
122.443347506794)) ;
#100399 = CARTESIAN_POINT('Ctrl Pts',(-19.9482881599933,-31.6432697226533,
122.333032443774)) ;
#100400 = CARTESIAN_POINT('Ctrl Pts',(-19.755445311698,-31.6531350553185,
122.256713486872)) ;
#100401 = CARTESIAN_POINT('Ctrl Pts',(-19.5504347572408,-31.6630955979161,
122.214029834224)) ;
#100402 = CARTESIAN_POINT('Ctrl Pts',(-19.3395941838846,-31.6731292834178,
122.207900611084)) ;
#100403 = CARTESIAN_POINT('Ctrl Pts',(-19.1338978695012,-31.683014115408,
122.237668442094)) ;
#100404 = CARTESIAN_POINT('Ctrl Pts',(-18.9329243923959,-31.6930815421679,
122.303926593615)) ;
#100405 = CARTESIAN_POINT('Ctrl Pts',(-18.7505899929617,-31.7029200313267,
122.401649380632)) ;
#100406 = CARTESIAN_POINT('Ctrl Pts',(-18.5841524594655,-31.7129835125168,
122.532210329718)) ;
#100407 = CARTESIAN_POINT('Ctrl Pts',(-18.4453883499579,-31.722877670332,
122.68719714899)) ;
#100408 = CARTESIAN_POINT('Ctrl Pts',(-18.3346568467247,-31.7328195270763,
122.864432302257)) ;
#100409 = CARTESIAN_POINT('Ctrl Pts',(-18.2558101880134,-31.7428220047477,
123.059405604086)) ;
#100410 = CARTESIAN_POINT('Ctrl Pts',(-18.2122072187586,-31.752856809052,
123.265799808077)) ;
#100411 = CARTESIAN_POINT('Ctrl Pts',(-18.2048893887999,-31.7627016858976,
123.472654527569)) ;
#100412 = CARTESIAN_POINT('Ctrl Pts',(-18.2336127187798,-31.7726875654532,
123.680580459055)) ;
#100413 = CARTESIAN_POINT('Ctrl Pts',(-18.2975511472833,-31.7826222958117,
123.879454707953)) ;
#100414 = CARTESIAN_POINT('Ctrl Pts',(-18.3963984127662,-31.7926801081246,
124.066335155318)) ;
#100415 = CARTESIAN_POINT('Ctrl Pts',(-18.5228930003451,-31.8025007002489,
124.229549267524)) ;
#100416 = CARTESIAN_POINT('Ctrl Pts',(-18.6794032618757,-31.8125672858587,
124.37193746429)) ;
#100417 = CARTESIAN_POINT('Ctrl Pts',(-18.8553890883581,-31.8224668664405,
124.483128111799)) ;
#100418 = CARTESIAN_POINT('Ctrl Pts',(-19.0508535790771,-31.8325184661188,
124.563325264758)) ;
#100419 = CARTESIAN_POINT('Ctrl Pts',(-19.2536732818215,-31.8423926525358,
124.607740482791)) ;
#100420 = CARTESIAN_POINT('Ctrl Pts',(-19.4648693837268,-31.8524491284167,
124.616554888055)) ;
#100421 = CARTESIAN_POINT('Ctrl Pts',(-19.6710721056032,-31.8623420597193,
124.589086356455)) ;
#100422 = CARTESIAN_POINT('Ctrl Pts',(-19.8727150982132,-31.8724048384319,
124.525215234063)) ;
#100423 = CARTESIAN_POINT('Ctrl Pts',(-20.0562016324184,-31.8822473640131,
124.429511936175)) ;
#100424 = CARTESIAN_POINT('Ctrl Pts',(-20.2230194312061,-31.8922381294379,
124.301933679984)) ;
#100425 = CARTESIAN_POINT('Ctrl Pts',(-20.364256834272,-31.902166205436,124.148246206785)) ;
#100426 = CARTESIAN_POINT('Ctrl Pts',(-20.4776500969338,-31.912154115823,
123.971508397341)) ;
#100427 = CARTESIAN_POINT('Ctrl Pts',(-20.5586853685384,-31.9221900279479,
123.776713283369)) ;
#100428 = CARTESIAN_POINT('Ctrl Pts',(-20.604177260201,-31.9320450407956,
123.574569933392)) ;
#100429 = CARTESIAN_POINT('Ctrl Pts',(-20.6143116224708,-31.9420439867119,
123.364638885295)) ;
#100430 = CARTESIAN_POINT('Ctrl Pts',(-20.5883043264661,-31.9519408991599,
123.158174187975)) ;
#100431 = CARTESIAN_POINT('Ctrl Pts',(-20.5259098227866,-31.9619946972534,
122.956257916759)) ;
#100432 = CARTESIAN_POINT('Ctrl Pts',(-20.4310950389888,-31.97187561808,122.771404879888)) ;
#100433 = CARTESIAN_POINT('Ctrl Pts',(-20.3043855938224,-31.9818801440778,
122.603560415283)) ;
#100434 = CARTESIAN_POINT('Ctrl Pts',(-20.1506871926404,-31.9918641076953,
122.460566435689)) ;
#100435 = CARTESIAN_POINT('Ctrl Pts',(-19.9734467608701,-32.0019037482466,
122.345990369024)) ;
#100436 = CARTESIAN_POINT('Ctrl Pts',(-19.7828774514739,-32.0117477738613,
122.265288194632)) ;
#100437 = CARTESIAN_POINT('Ctrl Pts',(-19.5783150429323,-32.0217387796786,
122.217619083654)) ;
#100438 = CARTESIAN_POINT('Ctrl Pts',(-19.3675761082951,-32.0317765712108,
122.206620385606)) ;
#100439 = CARTESIAN_POINT('Ctrl Pts',(-19.1621125477951,-32.0416209709992,
122.231523007649)) ;
#100440 = CARTESIAN_POINT('Ctrl Pts',(-18.9611827513556,-32.0516057715559,
122.292174309689)) ;
#100441 = CARTESIAN_POINT('Ctrl Pts',(-18.7745945644555,-32.0615452949671,
122.386307708238)) ;
#100442 = CARTESIAN_POINT('Ctrl Pts',(-18.6055634986924,-32.0715850140681,
122.512682808748)) ;
#100443 = CARTESIAN_POINT('Ctrl Pts',(-18.4631294058523,-32.0814731859874,
122.66411514573)) ;
#100444 = CARTESIAN_POINT('Ctrl Pts',(-18.3476659128775,-32.0914627484044,
122.839529109284)) ;
#100445 = CARTESIAN_POINT('Ctrl Pts',(-18.2648166590679,-32.1014211205991,
123.031790607799)) ;
#100446 = CARTESIAN_POINT('Ctrl Pts',(-18.2164011258627,-32.1113211948298,
123.234219332721)) ;
#100447 = CARTESIAN_POINT('Ctrl Pts',(-18.2037134582026,-32.1213672912034,
123.445028896827)) ;
#100448 = CARTESIAN_POINT('Ctrl Pts',(-18.227481855042,-32.1312758752005,
123.651987585625)) ;
#100449 = CARTESIAN_POINT('Ctrl Pts',(-18.2870598166171,-32.1412864537914,
123.853835596916)) ;
#100450 = CARTESIAN_POINT('Ctrl Pts',(-18.3813381611172,-32.1513156119042,
124.042436332284)) ;
#100451 = CARTESIAN_POINT('Ctrl Pts',(-18.5044722983298,-32.1611684937423,
124.208985919632)) ;
#100452 = CARTESIAN_POINT('Ctrl Pts',(-18.6558495541519,-32.1711280548933,
124.353651377035)) ;
#100453 = CARTESIAN_POINT('Ctrl Pts',(-18.8316228024852,-32.1811664894824,
124.470423361386)) ;
#100454 = CARTESIAN_POINT('Ctrl Pts',(-19.0217048104845,-32.1910397617095,
124.553889314401)) ;
#100455 = CARTESIAN_POINT('Ctrl Pts',(-19.2274184440204,-32.201113003703,
124.603996895421)) ;
#100456 = CARTESIAN_POINT('Ctrl Pts',(-19.4334723489275,-32.2109333352361,
124.617559154313)) ;
#100457 = CARTESIAN_POINT('Ctrl Pts',(-19.644075148336,-32.2210119964629,
124.59475247348)) ;
#100458 = CARTESIAN_POINT('Ctrl Pts',(-19.8430504821136,-32.2308635917571,
124.537096728571)) ;
#100459 = CARTESIAN_POINT('Ctrl Pts',(-20.033176863817,-32.2409367269859,
124.443919147938)) ;
#100460 = CARTESIAN_POINT('Ctrl Pts',(-20.2003452849219,-32.2507791625109,
124.321944254892)) ;
#100461 = CARTESIAN_POINT('Ctrl Pts',(-20.3462944726336,-32.2607599316443,
124.171207585303)) ;
#100462 = CARTESIAN_POINT('Ctrl Pts',(-20.4639641991799,-32.2707770328882,
123.9965581573)) ;
#100463 = CARTESIAN_POINT('Ctrl Pts',(-20.5487866768042,-32.2806654804901,
123.806747032011)) ;
#100464 = CARTESIAN_POINT('Ctrl Pts',(-20.6002315928406,-32.2907211946709,
123.601718844625)) ;
#100465 = CARTESIAN_POINT('Ctrl Pts',(-20.615058530721,-32.3005964010847,
123.394627386315)) ;
#100466 = CARTESIAN_POINT('Ctrl Pts',(-20.5939482888607,-32.3105914535575,
123.185569069474)) ;
#100467 = CARTESIAN_POINT('Ctrl Pts',(-20.5363733977679,-32.3206133375196,
122.982888521019)) ;
#100468 = CARTESIAN_POINT('Ctrl Pts',(-20.4457762989598,-32.3305173100489,
122.795421324377)) ;
#100469 = CARTESIAN_POINT('Ctrl Pts',(-20.3232089518915,-32.3405058067098,
122.624911528634)) ;
#100470 = CARTESIAN_POINT('Ctrl Pts',(-20.1731785765745,-32.3504696039577,
122.478746653934)) ;
#100471 = CARTESIAN_POINT('Ctrl Pts',(-20.0013492222596,-32.3603736272658,
122.361121527079)) ;
#100472 = CARTESIAN_POINT('Ctrl Pts',(-19.8086786154125,-32.3704341305874,
122.273939344262)) ;
#100473 = CARTESIAN_POINT('Ctrl Pts',(-19.6082911860057,-32.3802746657273,
122.222412592703)) ;
#100474 = CARTESIAN_POINT('Ctrl Pts',(-19.3974246917064,-32.3903368864319,
122.205837224052)) ;
#100475 = CARTESIAN_POINT('Ctrl Pts',(-19.1903252340285,-32.4002340402081,
122.226013708964)) ;
#100476 = CARTESIAN_POINT('Ctrl Pts',(-18.9890157317782,-32.4101651735936,
122.281360260561)) ;
#100477 = CARTESIAN_POINT('Ctrl Pts',(-18.7983606716983,-32.4202075487393,
122.372034110711)) ;
#100478 = CARTESIAN_POINT('Ctrl Pts',(-18.6289196108017,-32.4300934865054,
122.492406097849)) ;
#100479 = CARTESIAN_POINT('Ctrl Pts',(-18.4811182320896,-32.4400893294903,
122.641766146003)) ;
#100480 = CARTESIAN_POINT('Ctrl Pts',(-18.3621444461765,-32.4500313073689,
122.81362632524)) ;
#100481 = CARTESIAN_POINT('Ctrl Pts',(-18.2744163696933,-32.4599906818499,
123.003725450565)) ;
#100482 = CARTESIAN_POINT('Ctrl Pts',(-18.2207156394496,-32.4699872976837,
123.206931718435)) ;
#100483 = CARTESIAN_POINT('Ctrl Pts',(-18.2033294206092,-32.4800215162572,
123.417158861802)) ;
#100484 = CARTESIAN_POINT('Ctrl Pts',(-18.2221093879091,-32.4898745834678,
123.623444987911)) ;
#100485 = CARTESIAN_POINT('Ctrl Pts',(-18.2764221226504,-32.4998348413454,
123.825667154955)) ;
#100486 = CARTESIAN_POINT('Ctrl Pts',(-18.3658675567127,-32.509863868051,
124.016608463273)) ;
#100487 = CARTESIAN_POINT('Ctrl Pts',(-18.4856092891188,-32.5197740750854,
124.187093390626)) ;
#100488 = CARTESIAN_POINT('Ctrl Pts',(-18.6331239919438,-32.529708985733,
124.334963687184)) ;
#100489 = CARTESIAN_POINT('Ctrl Pts',(-18.8060039309029,-32.5397501159122,
124.456088925357)) ;
#100490 = CARTESIAN_POINT('Ctrl Pts',(-18.9943098816388,-32.5496372562822,
124.54412788712)) ;
#100491 = CARTESIAN_POINT('Ctrl Pts',(-19.197060153654,-32.5596295338181,
124.599039387056)) ;
#100492 = CARTESIAN_POINT('Ctrl Pts',(-19.4053803366227,-32.5695780770865,
124.617773458058)) ;
#100493 = CARTESIAN_POINT('Ctrl Pts',(-19.613538614218,-32.5795147519037,
124.600372590852)) ;
#100494 = CARTESIAN_POINT('Ctrl Pts',(-19.8165641546301,-32.58949817284,124.547077143003)) ;
#100495 = CARTESIAN_POINT('Ctrl Pts',(-20.0082045463583,-32.5995404880293,
124.45852388632)) ;
#100496 = CARTESIAN_POINT('Ctrl Pts',(-20.1782725030157,-32.6093808054685,
124.340732692807)) ;
#100497 = CARTESIAN_POINT('Ctrl Pts',(-20.328482319879,-32.619410509526,124.192751770375)) ;
#100498 = CARTESIAN_POINT('Ctrl Pts',(-20.4501448384363,-32.6294314662485,
124.020761080749)) ;
#100499 = CARTESIAN_POINT('Ctrl Pts',(-20.5391965579339,-32.6392980085521,
123.83340769811)) ;
#100500 = CARTESIAN_POINT('Ctrl Pts',(-20.5955014934989,-32.6493691084972,
123.629325462091)) ;
#100501 = CARTESIAN_POINT('Ctrl Pts',(-20.6150581382055,-32.6592111826748,
123.423332919864)) ;
#100502 = CARTESIAN_POINT('Ctrl Pts',(-20.5991226958927,-32.6691719772618,
123.21453765823)) ;
#100503 = CARTESIAN_POINT('Ctrl Pts',(-20.5463695031869,-32.6792098501627,
123.01021734002)) ;
#100504 = CARTESIAN_POINT('Ctrl Pts',(-20.4607025214654,-32.6890841357068,
122.82110188756)) ;
#100505 = CARTESIAN_POINT('Ctrl Pts',(-20.341200331264,-32.6991538861207,
122.646392788484)) ;
#100506 = CARTESIAN_POINT('Ctrl Pts',(-20.1967030192959,-32.7089871706553,
122.498530535037)) ;
#100507 = CARTESIAN_POINT('Ctrl Pts',(-20.0257286765649,-32.7190175114554,
122.375116138515)) ;
#100508 = CARTESIAN_POINT('Ctrl Pts',(-19.8356093124618,-32.729049435455,
122.28379955299)) ;
#100509 = CARTESIAN_POINT('Ctrl Pts',(-19.6367803866029,-32.7388779703909,
122.227608221759)) ;
#100510 = CARTESIAN_POINT('Ctrl Pts',(-19.4278088178352,-32.7488717481556,
122.205869494664)) ;
#100511 = CARTESIAN_POINT('Ctrl Pts',(-19.2175470603561,-32.7588994586411,
122.221210726533)) ;
#100512 = CARTESIAN_POINT('Ctrl Pts',(-19.0159240629217,-32.7687878694751,
122.271857874026)) ;
#100513 = CARTESIAN_POINT('Ctrl Pts',(-18.8243268121207,-32.7787647200106,
122.357161579746)) ;
#100514 = CARTESIAN_POINT('Ctrl Pts',(-18.6501429000993,-32.7887565165611,
122.474623956198)) ;
#100515 = CARTESIAN_POINT('Ctrl Pts',(-18.4985442927205,-32.7987925226548,
122.621344332583)) ;
#100516 = CARTESIAN_POINT('Ctrl Pts',(-18.376732340572,-32.8086432569176,
122.788842667667)) ;
#100517 = CARTESIAN_POINT('Ctrl Pts',(-18.2842520196366,-32.8186345154458,
122.977402621832)) ;
#100518 = CARTESIAN_POINT('Ctrl Pts',(-18.2262100834321,-32.828552410349,
123.177694172297)) ;
#100519 = CARTESIAN_POINT('Ctrl Pts',(-18.2035294380957,-32.838580552012,
123.387276606826)) ;
#100520 = CARTESIAN_POINT('Ctrl Pts',(-18.2172975843264,-32.8484657201279,
123.594642419645)) ;
#100521 = CARTESIAN_POINT('Ctrl Pts',(-18.2668882885097,-32.8584550836339,
123.798715462742)) ;
#100522 = CARTESIAN_POINT('Ctrl Pts',(-18.3520027661696,-32.8684962186439,
123.991892101773)) ;
#100523 = CARTESIAN_POINT('Ctrl Pts',(-18.4666437851278,-32.878328886832,
124.163898627534)) ;
#100524 = CARTESIAN_POINT('Ctrl Pts',(-18.6113167582633,-32.8883227897865,
124.316255745442)) ;
#100525 = CARTESIAN_POINT('Ctrl Pts',(-18.7811122551078,-32.898352074871,
124.441262749385)) ;
#100526 = CARTESIAN_POINT('Ctrl Pts',(-18.9669950464183,-32.9082276033129,
124.533760943854)) ;
#100527 = CARTESIAN_POINT('Ctrl Pts',(-19.1685290514312,-32.9182278859289,
124.593535704841)) ;
#100528 = CARTESIAN_POINT('Ctrl Pts',(-19.3755681265112,-32.928139901986,
124.617371731269)) ;
#100529 = CARTESIAN_POINT('Ctrl Pts',(-19.5862937526173,-32.938181977325,
124.604789768717)) ;
#100530 = CARTESIAN_POINT('Ctrl Pts',(-19.7887488413775,-32.9480818099811,
124.556492319768)) ;
#100531 = CARTESIAN_POINT('Ctrl Pts',(-19.981704049744,-32.9580742105591,
124.473434535639)) ;
#100532 = CARTESIAN_POINT('Ctrl Pts',(-20.1578345437307,-32.9681082323185,
124.357339413663)) ;
#100533 = CARTESIAN_POINT('Ctrl Pts',(-20.3087209559343,-32.9779728431597,
124.215071271798)) ;
#100534 = CARTESIAN_POINT('Ctrl Pts',(-20.4346339630023,-32.9879652426208,
124.046912175101)) ;
#100535 = CARTESIAN_POINT('Ctrl Pts',(-20.5294401830774,-32.9979971959537,
123.858519235765)) ;
#100536 = CARTESIAN_POINT('Ctrl Pts',(-20.5894011220292,-33.0078635548954,
123.659944017947)) ;
#100537 = CARTESIAN_POINT('Ctrl Pts',(-20.6146093934876,-33.0178510303812,
123.451520243129)) ;
#100538 = CARTESIAN_POINT('Ctrl Pts',(-20.6034027849544,-33.0277959365697,
123.242716471382)) ;
#100539 = CARTESIAN_POINT('Ctrl Pts',(-20.5555298783513,-33.0378409012299,
123.037058384703)) ;
#100540 = CARTESIAN_POINT('Ctrl Pts',(-20.4743442703196,-33.0477027081348,
122.846269990063)) ;
#100541 = CARTESIAN_POINT('Ctrl Pts',(-20.3601235882669,-33.0576953804405,
122.669983020818)) ;
#100542 = CARTESIAN_POINT('Ctrl Pts',(-20.2179031848982,-33.0676240513859,
122.517182301792)) ;
#100543 = CARTESIAN_POINT('Ctrl Pts',(-20.0511405631475,-33.0775765936112,
122.390837745583)) ;
#100544 = CARTESIAN_POINT('Ctrl Pts',(-19.8640787935611,-33.0875779496071,
122.294783722179)) ;
#100545 = CARTESIAN_POINT('Ctrl Pts',(-19.6625777832729,-33.0976065618818,
122.232784383341)) ;
#100546 = CARTESIAN_POINT('Ctrl Pts',(-19.4568140261569,-33.1074708964313,
122.206836473322)) ;
#100547 = CARTESIAN_POINT('Ctrl Pts',(-19.2470090701828,-33.1174632205079,
122.216814036558)) ;
#100548 = CARTESIAN_POINT('Ctrl Pts',(-19.0433688365547,-33.1273907128737,
122.262659363872)) ;
#100549 = CARTESIAN_POINT('Ctrl Pts',(-18.8489001207062,-33.1374180714246,
122.343962774089)) ;
#100550 = CARTESIAN_POINT('Ctrl Pts',(-18.6738284353751,-33.1473044894757,
122.456041526039)) ;
#100551 = CARTESIAN_POINT('Ctrl Pts',(-18.5186048794929,-33.1573362242111,
122.598762054007)) ;
#100552 = CARTESIAN_POINT('Ctrl Pts',(-18.3922312893721,-33.1672178054543,
122.763692528812)) ;
#100553 = CARTESIAN_POINT('Ctrl Pts',(-18.2946528400721,-33.1772797834867,
122.951339734788)) ;
#100554 = CARTESIAN_POINT('Ctrl Pts',(-18.232341305045,-33.1871368618484,
123.149007121717)) ;
#100555 = CARTESIAN_POINT('Ctrl Pts',(-18.2045100982945,-33.1971314349544,
123.357239008032)) ;
#100556 = CARTESIAN_POINT('Ctrl Pts',(-18.2131241345853,-33.207057231242,
123.565761734761)) ;
#100557 = CARTESIAN_POINT('Ctrl Pts',(-18.2581979616527,-33.2170825984117,
123.771633113741)) ;
#100558 = CARTESIAN_POINT('Ctrl Pts',(-18.3372272228421,-33.2269786780656,
123.964094189038)) ;
#100559 = CARTESIAN_POINT('Ctrl Pts',(-18.4492247973474,-33.2369737577711,
124.141890816736)) ;
#100560 = CARTESIAN_POINT('Ctrl Pts',(-18.591079046203,-33.246998845587,124.297761351088)) ;
#100561 = CARTESIAN_POINT('Ctrl Pts',(-18.8100940618361,-33.2601826679542,
124.467641813623)) ;
#100562 = CARTESIAN_POINT('Ctrl Pts',(-19.070920940811,-33.2735047861002,
124.57815484791)) ;
#100563 = CARTESIAN_POINT('Ctrl Pts',(-19.3495997768078,-33.2868839957278,
124.616255035302)) ;
#100564 = CARTESIAN_POINT('Ctrl Pts',(-19.5563150954162,-33.296722232972,
124.608827325648)) ;
#100565 = CARTESIAN_POINT('Ctrl Pts',(-19.7634008047829,-33.3067951562307,
124.564684849008)) ;
#100566 = CARTESIAN_POINT('Ctrl Pts',(-19.9554964751113,-33.3166517976858,
124.486920812469)) ;
#100567 = CARTESIAN_POINT('Ctrl Pts',(-20.1337364235445,-33.3266371731919,
124.376044377868)) ;
#100568 = CARTESIAN_POINT('Ctrl Pts',(-20.3414692158328,-33.3399212046523,
124.189421639535)) ;
#100569 = CARTESIAN_POINT('Ctrl Pts',(-20.534241339007,-33.3564399965226,
123.895712267581)) ;
#100570 = CARTESIAN_POINT('Ctrl Pts',(-20.6157082391679,-33.3732257135293,
123.548262740302)) ;
#100571 = CARTESIAN_POINT('Ctrl Pts',(-20.6070708730679,-33.3863388620383,
123.272702652615)) ;
#100572 = CARTESIAN_POINT('Ctrl Pts',(-20.5647832319966,-33.3963744111184,
123.066024942899)) ;
#100573 = CARTESIAN_POINT('Ctrl Pts',(-20.4868195413994,-33.4063904672979,
122.870399132686)) ;
#100574 = CARTESIAN_POINT('Ctrl Pts',(-20.3416448755985,-33.4195685031639,
122.634464646137)) ;
#100575 = CARTESIAN_POINT('Ctrl Pts',(-20.0859212774212,-33.436170380351,
122.391058471702)) ;
#100576 = CARTESIAN_POINT('Ctrl Pts',(-19.6946142735966,-33.4562335249669,
122.22119315259)) ;
#100577 = CARTESIAN_POINT('Ctrl Pts',(-19.2743515627867,-33.4760344150506,
122.195138698631)) ;
#100578 = CARTESIAN_POINT('Ctrl Pts',(-18.8673400378178,-33.4959775403293,
122.313861132111)) ;
#100579 = CARTESIAN_POINT('Ctrl Pts',(-18.5261644006187,-33.5158755854489,
122.564047591661)) ;
#100580 = CARTESIAN_POINT('Ctrl Pts',(-18.2900746521247,-33.5357613450756,
122.91489298829)) ;
#100581 = CARTESIAN_POINT('Ctrl Pts',(-18.1876300296397,-33.5558265202555,
123.329014515711)) ;
#100582 = CARTESIAN_POINT('Ctrl Pts',(-18.2322759073076,-33.5756531633583,
123.748284653681)) ;
#100583 = CARTESIAN_POINT('Ctrl Pts',(-18.4169536392296,-33.5955618728067,
124.129064799869)) ;
#100584 = CARTESIAN_POINT('Ctrl Pts',(-18.7212368069191,-33.6155137098385,
124.424840772145)) ;
#100585 = CARTESIAN_POINT('Ctrl Pts',(-19.1094163331839,-33.6355221845416,
124.598830097462)) ;
#100586 = CARTESIAN_POINT('Ctrl Pts',(-19.5292986318833,-33.6553236433031,
124.630091374334)) ;
#100587 = CARTESIAN_POINT('Ctrl Pts',(-19.9381108332418,-33.675280531539,
124.516363414137)) ;
#100588 = CARTESIAN_POINT('Ctrl Pts',(-20.2834683895912,-33.6952643689531,
124.2688490976)) ;
#100589 = CARTESIAN_POINT('Ctrl Pts',(-20.5222687544957,-33.7150728081741,
123.921840104974)) ;
#100590 = CARTESIAN_POINT('Ctrl Pts',(-20.6296447988038,-33.7350585175543,
123.51081065447)) ;
#100591 = CARTESIAN_POINT('Ctrl Pts',(-20.5906528622527,-33.7549280405696,
123.089960084968)) ;
#100592 = CARTESIAN_POINT('Ctrl Pts',(-20.4090011369013,-33.7749487796868,
122.705145554708)) ;
#100593 = CARTESIAN_POINT('Ctrl Pts',(-20.1103611716389,-33.7947528446637,
122.408052004709)) ;
#100594 = CARTESIAN_POINT('Ctrl Pts',(-19.7236070361393,-33.8148148083945,
122.228379447766)) ;
#100595 = CARTESIAN_POINT('Ctrl Pts',(-19.3033477933744,-33.834647988683,
122.192286171219)) ;
#100596 = CARTESIAN_POINT('Ctrl Pts',(-18.8940896865763,-33.854567186009,
122.30105373335)) ;
#100597 = CARTESIAN_POINT('Ctrl Pts',(-18.5462824085301,-33.8745052111223,
122.543443913127)) ;
#100598 = CARTESIAN_POINT('Ctrl Pts',(-18.3022893086473,-33.8943832571784,
122.888617834666)) ;
#100599 = CARTESIAN_POINT('Ctrl Pts',(-18.1901238419675,-33.9143679914665,
123.298419694959)) ;
#100600 = CARTESIAN_POINT('Ctrl Pts',(-18.2243456478135,-33.934278808145,
123.720514931603)) ;
#100601 = CARTESIAN_POINT('Ctrl Pts',(-18.40148950432,-33.9542777836637,124.106981507315)) ;
#100602 = CARTESIAN_POINT('Ctrl Pts',(-18.6967361614438,-33.9740827043089,
124.407368109872)) ;
#100603 = CARTESIAN_POINT('Ctrl Pts',(-19.0797619953671,-33.9940666646001,
124.591098001132)) ;
#100604 = CARTESIAN_POINT('Ctrl Pts',(-19.5006265471779,-34.0139528683241,
124.632722200999)) ;
#100605 = CARTESIAN_POINT('Ctrl Pts',(-19.9117318890759,-34.0339020466473,
124.528393120983)) ;
#100606 = CARTESIAN_POINT('Ctrl Pts',(-20.2616903492735,-34.0538038458868,
124.290509110893)) ;
#100607 = CARTESIAN_POINT('Ctrl Pts',(-20.5099189356302,-34.0736824509392,
123.948379858816)) ;
#100608 = CARTESIAN_POINT('Ctrl Pts',(-20.627208709469,-34.0937148106649,
123.538874272135)) ;
#100609 = CARTESIAN_POINT('Ctrl Pts',(-20.6022470568823,-34.110296536621,
123.187197784009)) ;
#100610 = CARTESIAN_POINT('Ctrl Pts',(-20.5124584982992,-34.1234907069189,
122.924736892487)) ;
#100611 = CARTESIAN_POINT('Ctrl Pts',(-20.3777000722358,-34.1368028850121,
122.679516476114)) ;
#100612 = CARTESIAN_POINT('Ctrl Pts',(-20.1339984517837,-34.1533690646054,
122.425063732099)) ;
#100613 = CARTESIAN_POINT('Ctrl Pts',(-19.817224699958,-34.1699972594656,
122.268242004181)) ;
#100614 = CARTESIAN_POINT('Ctrl Pts',(-19.5432355839473,-34.1832858411753,
122.213312684796)) ;
#100615 = CARTESIAN_POINT('Ctrl Pts',(-19.3337565097566,-34.1932540892789,
122.208248778895)) ;
#100616 = CARTESIAN_POINT('Ctrl Pts',(-19.1276245927567,-34.2031688455351,
122.239209955623)) ;
#100617 = CARTESIAN_POINT('Ctrl Pts',(-18.927961344161,-34.2131819961863,
122.305930168428)) ;
#100618 = CARTESIAN_POINT('Ctrl Pts',(-18.743089846786,-34.2231947033883,
122.406594868567)) ;
#100619 = CARTESIAN_POINT('Ctrl Pts',(-18.5254733951057,-34.2364139920796,
122.579427002215)) ;
#100620 = CARTESIAN_POINT('Ctrl Pts',(-18.3148416874587,-34.2530326730776,
122.863105200925)) ;
#100621 = CARTESIAN_POINT('Ctrl Pts',(-18.2135484106384,-34.2695975808511,
123.200460756211)) ;
#100622 = CARTESIAN_POINT('Ctrl Pts',(-18.2053484487877,-34.2829960524619,
123.482045088967)) ;
#100623 = CARTESIAN_POINT('Ctrl Pts',(-18.2351320308585,-34.2928373079489,
123.686795103262)) ;
#100624 = CARTESIAN_POINT('Ctrl Pts',(-18.300516067415,-34.3028236235371,
123.886263741776)) ;
#100625 = CARTESIAN_POINT('Ctrl Pts',(-18.3989921090451,-34.3127602311235,
124.070534239829)) ;
#100626 = CARTESIAN_POINT('Ctrl Pts',(-18.5294851215082,-34.3228100984918,
124.236671800716)) ;
#100627 = CARTESIAN_POINT('Ctrl Pts',(-18.6836449874935,-34.3326605931666,
124.374971475593)) ;
#100628 = CARTESIAN_POINT('Ctrl Pts',(-18.861315743535,-34.3426323935611,
124.486192399696)) ;
#100629 = CARTESIAN_POINT('Ctrl Pts',(-19.0561370853563,-34.3526283605869,
124.565066999234)) ;
#100630 = CARTESIAN_POINT('Ctrl Pts',(-19.2625528551092,-34.3626658199681,
124.608805119111)) ;
#100631 = CARTESIAN_POINT('Ctrl Pts',(-19.4693150635243,-34.3725065208688,
124.616289160971)) ;
#100632 = CARTESIAN_POINT('Ctrl Pts',(-19.6785718666333,-34.3825545421362,
124.587470380198)) ;
#100633 = CARTESIAN_POINT('Ctrl Pts',(-19.8775406745658,-34.3925019352189,
124.523081366889)) ;
#100634 = CARTESIAN_POINT('Ctrl Pts',(-20.0619206026871,-34.4024120812653,
124.426049043357)) ;
#100635 = CARTESIAN_POINT('Ctrl Pts',(-20.2289520503902,-34.4124709951149,
124.296392288548)) ;
#100636 = CARTESIAN_POINT('Ctrl Pts',(-20.3681027803716,-34.4223117654042,
124.143259885666)) ;
#100637 = CARTESIAN_POINT('Ctrl Pts',(-20.4812240073115,-34.4323746349828,
123.964522302239)) ;
#100638 = CARTESIAN_POINT('Ctrl Pts',(-20.5601075037197,-34.4422689581133,
123.772026370823)) ;
#100639 = CARTESIAN_POINT('Ctrl Pts',(-20.6051242664344,-34.4522107652078,
123.567950265463)) ;
#100640 = CARTESIAN_POINT('Ctrl Pts',(-20.6141585895728,-34.4622132761631,
123.357831542534)) ;
#100641 = CARTESIAN_POINT('Ctrl Pts',(-20.5861609748622,-34.4722479969815,
123.148748992767)) ;
#100642 = CARTESIAN_POINT('Ctrl Pts',(-20.5238102222659,-34.4820931744872,
122.951374651742)) ;
#100643 = CARTESIAN_POINT('Ctrl Pts',(-20.4271652880716,-34.4920779348883,
122.765068493332)) ;
#100644 = CARTESIAN_POINT('Ctrl Pts',(-20.3002677713746,-34.5020168412047,
122.599029202079)) ;
#100645 = CARTESIAN_POINT('Ctrl Pts',(-20.1448586763245,-34.5120590688404,
122.45616453495)) ;
#100646 = CARTESIAN_POINT('Ctrl Pts',(-19.9698283798703,-34.5219442804248,
122.34408205666)) ;
#100647 = CARTESIAN_POINT('Ctrl Pts',(-19.7759430957663,-34.5319432106267,
122.262943912525)) ;
#100648 = CARTESIAN_POINT('Ctrl Pts',(-19.5725573411088,-34.5418606335371,
122.216910572658)) ;
#100649 = CARTESIAN_POINT('Ctrl Pts',(-19.3615911423824,-34.5519085656159,
122.206803418974)) ;
#100650 = CARTESIAN_POINT('Ctrl Pts',(-19.155540078122,-34.5617859414253,
122.23283367753)) ;
#100651 = CARTESIAN_POINT('Ctrl Pts',(-18.9536299339585,-34.5718398345932,
122.295219099932)) ;
#100652 = CARTESIAN_POINT('Ctrl Pts',(-18.7685026669244,-34.5817334578465,
122.390126409473)) ;
#100653 = CARTESIAN_POINT('Ctrl Pts',(-18.5998752953312,-34.5917960514695,
122.517809168213)) ;
#100654 = CARTESIAN_POINT('Ctrl Pts',(-18.4590073691217,-34.6016386254585,
122.669410492578)) ;
#100655 = CARTESIAN_POINT('Ctrl Pts',(-18.344517573857,-34.6116293823415,
122.845468478048)) ;
#100656 = CARTESIAN_POINT('Ctrl Pts',(-18.2628714117122,-34.6215574440994,
123.037566664615)) ;
#100657 = CARTESIAN_POINT('Ctrl Pts',(-18.2151802594571,-34.6315454199886,
123.242066320146)) ;
#100658 = CARTESIAN_POINT('Ctrl Pts',(-18.2040198516931,-34.641581084345,
123.45274606339)) ;
#100659 = CARTESIAN_POINT('Ctrl Pts',(-18.2288306349782,-34.6514370227647,
123.658468707891)) ;
#100660 = CARTESIAN_POINT('Ctrl Pts',(-18.2894970696974,-34.6614325141616,
123.859634570927)) ;
#100661 = CARTESIAN_POINT('Ctrl Pts',(-18.3833175326401,-34.671342319115,
124.045659990043)) ;
#100662 = CARTESIAN_POINT('Ctrl Pts',(-18.5090245422639,-34.6813545413818,
124.214494792325)) ;
#100663 = CARTESIAN_POINT('Ctrl Pts',(-18.6626570674728,-34.6913824220746,
124.358861999384)) ;
#100664 = CARTESIAN_POINT('Ctrl Pts',(-18.8358100583168,-34.7012388180572,
124.472679102379)) ;
#100665 = CARTESIAN_POINT('Ctrl Pts',(-19.0291759620761,-34.7112636152372,
124.556510085388)) ;
#100666 = CARTESIAN_POINT('Ctrl Pts',(-19.2344095399434,-34.721294545221,
124.605019586066)) ;
#100667 = CARTESIAN_POINT('Ctrl Pts',(-19.4409993015958,-34.7311391477296,
124.617302775574)) ;
#100668 = CARTESIAN_POINT('Ctrl Pts',(-19.649717533329,-34.7411299989537,
124.593741480784)) ;
#100669 = CARTESIAN_POINT('Ctrl Pts',(-19.8519812854984,-34.751167831965,
124.533566537728)) ;
#100670 = CARTESIAN_POINT('Ctrl Pts',(-20.0372566539474,-34.7610122204304,
124.44132476754)) ;
#100671 = CARTESIAN_POINT('Ctrl Pts',(-20.2062935713949,-34.7709970248,124.316914745808)) ;
#100672 = CARTESIAN_POINT('Ctrl Pts',(-20.3506086954577,-34.7809365442828,
124.165754598844)) ;
#100673 = CARTESIAN_POINT('Ctrl Pts',(-20.4675870983985,-34.7909762752842,
123.990089336034)) ;
#100674 = CARTESIAN_POINT('Ctrl Pts',(-20.5511156818666,-34.8008644035305,
123.799716266804)) ;
#100675 = CARTESIAN_POINT('Ctrl Pts',(-20.6012008971059,-34.810854128739,
123.595768723546)) ;
#100676 = CARTESIAN_POINT('Ctrl Pts',(-20.6149183327468,-34.8208118934405,
123.38687817394)) ;
#100677 = CARTESIAN_POINT('Ctrl Pts',(-20.5927684630614,-34.8307142348525,
123.179874648657)) ;
#100678 = CARTESIAN_POINT('Ctrl Pts',(-20.5341702900792,-34.8407584305589,
122.97701817319)) ;
#100679 = CARTESIAN_POINT('Ctrl Pts',(-20.4425166184617,-34.8506658313181,
122.789970952297)) ;
#100680 = CARTESIAN_POINT('Ctrl Pts',(-20.3188031025353,-34.8606764311925,
122.619714394045)) ;
#100681 = CARTESIAN_POINT('Ctrl Pts',(-20.1668235239592,-34.8707067271047,
122.473528427061)) ;
#100682 = CARTESIAN_POINT('Ctrl Pts',(-19.9950091797691,-34.8805615067544,
122.357781217345)) ;
#100683 = CARTESIAN_POINT('Ctrl Pts',(-19.8039793821543,-34.8905188349719,
122.272158010813)) ;
#100684 = CARTESIAN_POINT('Ctrl Pts',(-19.5992480957468,-34.9005578678788,
122.220952085724)) ;
#100685 = CARTESIAN_POINT('Ctrl Pts',(-19.3921953658923,-34.9104309797681,
122.205929381801)) ;
#100686 = CARTESIAN_POINT('Ctrl Pts',(-19.1815752935626,-34.9205042647952,
122.227570738365)) ;
#100687 = CARTESIAN_POINT('Ctrl Pts',(-18.9828684053808,-34.9303245845319,
122.283763775771)) ;
#100688 = CARTESIAN_POINT('Ctrl Pts',(-18.7920486648443,-34.9404032499104,
122.375750262933)) ;
#100689 = CARTESIAN_POINT('Ctrl Pts',(-18.6238506323388,-34.9502548403942,
122.496683375048)) ;
#100690 = CARTESIAN_POINT('Ctrl Pts',(-18.4758819893934,-34.9603279907131,
122.648127444973)) ;
#100691 = CARTESIAN_POINT('Ctrl Pts',(-18.3591839658888,-34.9701703706881,
122.819021755702)) ;
#100692 = CARTESIAN_POINT('Ctrl Pts',(-18.2721173911497,-34.9801513469312,
123.009920010026)) ;
#100693 = CARTESIAN_POINT('Ctrl Pts',(-18.2196704566526,-34.9901676752865,
123.21387027846)) ;
#100694 = CARTESIAN_POINT('Ctrl Pts',(-18.2033629297156,-35.0000654722776,
123.421305049384)) ;
#100695 = CARTESIAN_POINT('Ctrl Pts',(-18.2231956719439,-35.0100780290097,
123.630879706018)) ;
#100696 = CARTESIAN_POINT('Ctrl Pts',(-18.2796995619994,-35.0201100638562,
123.834064469006)) ;
#100697 = CARTESIAN_POINT('Ctrl Pts',(-18.3684247473299,-35.0299494646716,
124.020942975181)) ;
#100698 = CARTESIAN_POINT('Ctrl Pts',(-18.4908530567065,-35.0400152503232,
124.193516835971)) ;
#100699 = CARTESIAN_POINT('Ctrl Pts',(-18.6388650791382,-35.0499057054378,
124.339584161571)) ;
#100700 = CARTESIAN_POINT('Ctrl Pts',(-18.8114664915511,-35.0598978240735,
124.459300247681)) ;
#100701 = CARTESIAN_POINT('Ctrl Pts',(-19.0017602643688,-35.0698606508366,
124.546794772724)) ;
#100702 = CARTESIAN_POINT('Ctrl Pts',(-19.2030523637477,-35.0797649341095,
124.600122749678)) ;
#100703 = CARTESIAN_POINT('Ctrl Pts',(-19.4137905563915,-35.0898253680566,
124.617781357557)) ;
#100704 = CARTESIAN_POINT('Ctrl Pts',(-19.6198660899427,-35.0996659207298,
124.599260028459)) ;
#100705 = CARTESIAN_POINT('Ctrl Pts',(-19.8241167855346,-35.1097281406755,
124.544295325278)) ;
#100706 = CARTESIAN_POINT('Ctrl Pts',(-20.0125152931457,-35.119625279954,
124.455960243587)) ;
#100707 = CARTESIAN_POINT('Ctrl Pts',(-20.1836871378451,-35.1295564720891,
124.336420801444)) ;
#100708 = CARTESIAN_POINT('Ctrl Pts',(-20.3329871037858,-35.1395986267342,
124.18716278176)) ;
#100709 = CARTESIAN_POINT('Ctrl Pts',(-20.4523816208933,-35.1494853877535,
124.017004311627)) ;
#100710 = CARTESIAN_POINT('Ctrl Pts',(-20.5416439348355,-35.1594846894707,
123.826710764807)) ;
#100711 = CARTESIAN_POINT('Ctrl Pts',(-20.5962295808139,-35.1694054876375,
123.625384496779)) ;
#100712 = CARTESIAN_POINT('Ctrl Pts',(-20.6152613605229,-35.1794395412342,
123.415320795738)) ;
#100713 = CARTESIAN_POINT('Ctrl Pts',(-20.5978472470063,-35.1893626588006,
123.207401865937)) ;
#100714 = CARTESIAN_POINT('Ctrl Pts',(-20.543851324903,-35.1994187822997,
123.003024054546)) ;
#100715 = CARTESIAN_POINT('Ctrl Pts',(-20.4571161579045,-35.2092642239545,
122.815082594222)) ;
#100716 = CARTESIAN_POINT('Ctrl Pts',(-20.3382431270051,-35.2192265250787,
122.642663671508)) ;
#100717 = CARTESIAN_POINT('Ctrl Pts',(-20.1900442155833,-35.2292550043538,
122.492688728247)) ;
#100718 = CARTESIAN_POINT('Ctrl Pts',(-20.0201430110837,-35.2391653578635,
122.372116812809)) ;
#100719 = CARTESIAN_POINT('Ctrl Pts',(-19.8316410773168,-35.2491002300407,
122.282155346529)) ;
#100720 = CARTESIAN_POINT('Ctrl Pts',(-19.6281895456799,-35.2591413676264,
122.22588556621)) ;
#100721 = CARTESIAN_POINT('Ctrl Pts',(-19.4212767037568,-35.2690285168409,
122.205957500751)) ;
#100722 = CARTESIAN_POINT('Ctrl Pts',(-19.2118424307616,-35.279020751592,
122.222079975748)) ;
#100723 = CARTESIAN_POINT('Ctrl Pts',(-19.0092661763632,-35.288969457155,
122.274160402898)) ;
#100724 = CARTESIAN_POINT('Ctrl Pts',(-18.8189496417732,-35.2989055255787,
122.360225763757)) ;
#100725 = CARTESIAN_POINT('Ctrl Pts',(-18.6454413736411,-35.3088912097945,
122.478439165317)) ;
#100726 = CARTESIAN_POINT('Ctrl Pts',(-18.4945269441583,-35.3189316363631,
122.626004450651)) ;
#100727 = CARTESIAN_POINT('Ctrl Pts',(-18.3737039626246,-35.3287707498269,
122.793902602721)) ;
#100728 = CARTESIAN_POINT('Ctrl Pts',(-18.2817008818559,-35.3388004840027,
122.983631428976)) ;
#100729 = CARTESIAN_POINT('Ctrl Pts',(-18.2246114551291,-35.3488225835086,
123.186443865571)) ;
#100730 = CARTESIAN_POINT('Ctrl Pts',(-18.2034063940511,-35.358691023402,
123.392838329371)) ;
#100731 = CARTESIAN_POINT('Ctrl Pts',(-18.2186669911939,-35.3687598880876,
123.603947872075)) ;
#100732 = CARTESIAN_POINT('Ctrl Pts',(-18.2691895164447,-35.3786025611862,
123.80461622)) ;
#100733 = CARTESIAN_POINT('Ctrl Pts',(-18.354096458775,-35.3885631953487,
123.996029326651)) ;
#100734 = CARTESIAN_POINT('Ctrl Pts',(-18.4721989248819,-35.3986011110268,
124.170905836083)) ;
#100735 = CARTESIAN_POINT('Ctrl Pts',(-18.6162270777124,-35.4084753858862,
124.320436148826)) ;
#100736 = CARTESIAN_POINT('Ctrl Pts',(-18.787316229107,-35.4185451362614,
124.445065779618)) ;
#100737 = CARTESIAN_POINT('Ctrl Pts',(-18.9729724191923,-35.4283784316359,
124.536030397053)) ;
#100738 = CARTESIAN_POINT('Ctrl Pts',(-19.1753937241975,-35.4384087291155,
124.595095252712)) ;
#100739 = CARTESIAN_POINT('Ctrl Pts',(-19.3851154662139,-35.4484408155569,
124.617503718592)) ;
#100740 = CARTESIAN_POINT('Ctrl Pts',(-19.5912719292869,-35.4582687440459,
124.603904303236)) ;
#100741 = CARTESIAN_POINT('Ctrl Pts',(-19.7955090685265,-35.4682647851566,
124.554420473631)) ;
#100742 = CARTESIAN_POINT('Ctrl Pts',(-19.9884689899732,-35.4782905972579,
124.469598734734)) ;
#100743 = CARTESIAN_POINT('Ctrl Pts',(-20.1614939117616,-35.4881778321527,
124.354404792167)) ;
#100744 = CARTESIAN_POINT('Ctrl Pts',(-20.3134788862916,-35.4981546983637,
124.209881671069)) ;
#100745 = CARTESIAN_POINT('Ctrl Pts',(-20.4383178117718,-35.5081476422355,
124.040878041078)) ;
#100746 = CARTESIAN_POINT('Ctrl Pts',(-20.5320770090576,-35.5181855649069,
123.851839687454)) ;
#100747 = CARTESIAN_POINT('Ctrl Pts',(-20.590773848519,-35.5280340291686,
123.653272380796)) ;
#100748 = CARTESIAN_POINT('Ctrl Pts',(-20.6148079465354,-35.5380258959126,
123.444622183721)) ;
#100749 = CARTESIAN_POINT('Ctrl Pts',(-20.6024561580354,-35.5479436279538,
123.236459367569)) ;
#100750 = CARTESIAN_POINT('Ctrl Pts',(-20.5536749339709,-35.557971812849,
123.031374263346)) ;
#100751 = CARTESIAN_POINT('Ctrl Pts',(-20.4712889404072,-35.5678569708979,
122.840579540661)) ;
#100752 = CARTESIAN_POINT('Ctrl Pts',(-20.3562493576704,-35.5778463314396,
122.664878273543)) ;
#100753 = CARTESIAN_POINT('Ctrl Pts',(-20.2113820052844,-35.5878874883739,
122.511335982088)) ;
#100754 = CARTESIAN_POINT('Ctrl Pts',(-20.04577987322,-35.5977200718291,122.387625525792)) ;
#100755 = CARTESIAN_POINT('Ctrl Pts',(-19.8584474638155,-35.6077142917911,
122.292485495043)) ;
#100756 = CARTESIAN_POINT('Ctrl Pts',(-19.6566267381721,-35.6177423935784,
122.231520180872)) ;
#100757 = CARTESIAN_POINT('Ctrl Pts',(-19.4504164365776,-35.6276223382014,
122.206599298328)) ;
#100758 = CARTESIAN_POINT('Ctrl Pts',(-19.2406925017737,-35.6376126647585,
122.217663247742)) ;
#100759 = CARTESIAN_POINT('Ctrl Pts',(-19.0370700422423,-35.6475535964128,
122.264742809365)) ;
#100760 = CARTESIAN_POINT('Ctrl Pts',(-18.8436947842426,-35.6575407149157,
122.34657040198)) ;
#100761 = CARTESIAN_POINT('Ctrl Pts',(-18.6668553030641,-35.6675740478129,
122.461522490179)) ;
#100762 = CARTESIAN_POINT('Ctrl Pts',(-18.514926508641,-35.6774401522576,
122.602763662125)) ;
#100763 = CARTESIAN_POINT('Ctrl Pts',(-18.3872831462186,-35.6875062661379,
122.771525487333)) ;
#100764 = CARTESIAN_POINT('Ctrl Pts',(-18.2928656096915,-35.6973622779064,
122.955984007006)) ;
#100765 = CARTESIAN_POINT('Ctrl Pts',(-18.2304659629802,-35.7073569815377,
123.156618921704)) ;
#100766 = CARTESIAN_POINT('Ctrl Pts',(-18.2042001748318,-35.7173883172625,
123.365870940972)) ;
#100767 = CARTESIAN_POINT('Ctrl Pts',(-18.2141648920665,-35.7272548424662,
123.573063975471)) ;
#100768 = CARTESIAN_POINT('Ctrl Pts',(-18.26017755081,-35.737242270512,123.777901924918)) ;
#100769 = CARTESIAN_POINT('Ctrl Pts',(-18.3406309976314,-35.7471872001984,
123.970909538176)) ;
#100770 = CARTESIAN_POINT('Ctrl Pts',(-18.4545817743853,-35.7572321183069,
124.148679008596)) ;
#100771 = CARTESIAN_POINT('Ctrl Pts',(-18.5949502521215,-35.7670940879208,
124.301287113237)) ;
#100772 = CARTESIAN_POINT('Ctrl Pts',(-18.7615786690674,-35.7770861559421,
124.429167514652)) ;
#100773 = CARTESIAN_POINT('Ctrl Pts',(-18.9467874102319,-35.7870170813166,
124.525562437317)) ;
#100774 = CARTESIAN_POINT('Ctrl Pts',(-19.1461828688177,-35.7969677095401,
124.588785204681)) ;
#100775 = CARTESIAN_POINT('Ctrl Pts',(-19.3545824888073,-35.8069679485992,
124.61668903321)) ;
#100776 = CARTESIAN_POINT('Ctrl Pts',(-19.5652103835343,-35.8169964039684,
124.607656604503)) ;
#100777 = CARTESIAN_POINT('Ctrl Pts',(-19.7678210258412,-35.8268624385517,
124.563227774421)) ;
#100778 = CARTESIAN_POINT('Ctrl Pts',(-19.9621986241707,-35.8368547602991,
124.483614794114)) ;
#100779 = CARTESIAN_POINT('Ctrl Pts',(-20.1387827375136,-35.8467870499761,
124.372143296753)) ;
#100780 = CARTESIAN_POINT('Ctrl Pts',(-20.2945277295481,-35.8567886949468,
124.230893556733)) ;
#100781 = CARTESIAN_POINT('Ctrl Pts',(-20.4659698414278,-35.8701013283629,
124.009636039517)) ;
#100782 = CARTESIAN_POINT('Ctrl Pts',(-20.5752600036039,-35.8833330777444,
123.750378219113)) ;
#100783 = CARTESIAN_POINT('Ctrl Pts',(-20.6136582791691,-35.8966563425615,
123.472967021619)) ;
#100784 = CARTESIAN_POINT('Ctrl Pts',(-20.6063007088463,-35.9065320487792,
123.265462367037)) ;
#100785 = CARTESIAN_POINT('Ctrl Pts',(-20.5627998443653,-35.9165216398792,
123.06002944447)) ;
#100786 = CARTESIAN_POINT('Ctrl Pts',(-20.4848914753812,-35.9264487363346,
122.866390358098)) ;
#100787 = CARTESIAN_POINT('Ctrl Pts',(-20.3734990272047,-35.9364738848392,
122.687494727026)) ;
#100788 = CARTESIAN_POINT('Ctrl Pts',(-20.2346261607065,-35.9463695389859,
122.532570049574)) ;
#100789 = CARTESIAN_POINT('Ctrl Pts',(-20.0693930135044,-35.9563730733641,
122.402500547701)) ;
#100790 = CARTESIAN_POINT('Ctrl Pts',(-19.8843702091483,-35.9663582118041,
122.303273461179)) ;
#100791 = CARTESIAN_POINT('Ctrl Pts',(-19.6838894201038,-35.9763941363995,
122.237560814507)) ;
#100792 = CARTESIAN_POINT('Ctrl Pts',(-19.4789119617871,-35.9862454118272,
122.207961793095)) ;
#100793 = CARTESIAN_POINT('Ctrl Pts',(-19.2689199410369,-35.9962376729885,
122.21389590013)) ;
#100794 = CARTESIAN_POINT('Ctrl Pts',(-19.0622933736264,-36.0062775570061,
122.256922543288)) ;
#100795 = CARTESIAN_POINT('Ctrl Pts',(-18.8700530733333,-36.0161123315086,
122.333100079052)) ;
#100796 = CARTESIAN_POINT('Ctrl Pts',(-18.689643846233,-36.0261887125289,
122.444065441217)) ;
#100797 = CARTESIAN_POINT('Ctrl Pts',(-18.5347774955406,-36.0360349856795,
122.581455449752)) ;
#100798 = CARTESIAN_POINT('Ctrl Pts',(-18.3597507534994,-36.0493995069647,
122.801250538127)) ;
#100799 = CARTESIAN_POINT('Ctrl Pts',(-18.2477903091155,-36.0626057513992,
123.058796388371)) ;
#100800 = CARTESIAN_POINT('Ctrl Pts',(-18.205714641578,-36.0758707060764,
123.334416861352)) ;
#100801 = CARTESIAN_POINT('Ctrl Pts',(-18.2106623069333,-36.0859029866281,
123.545283476093)) ;
#100802 = CARTESIAN_POINT('Ctrl Pts',(-18.2516205745853,-36.095811720146,
123.7495235163)) ;
#100803 = CARTESIAN_POINT('Ctrl Pts',(-18.3271374343042,-36.1057492710135,
123.944325431398)) ;
#100804 = CARTESIAN_POINT('Ctrl Pts',(-18.4364697612003,-36.1157791186074,
124.124598444556)) ;
#100805 = CARTESIAN_POINT('Ctrl Pts',(-18.6196410476078,-36.1290142585278,
124.33415566645)) ;
#100806 = CARTESIAN_POINT('Ctrl Pts',(-18.9138912238764,-36.145682722899,
124.53148526373)) ;
#100807 = CARTESIAN_POINT('Ctrl Pts',(-19.3240838284352,-36.1655537347729,
124.633322937475)) ;
#100808 = CARTESIAN_POINT('Ctrl Pts',(-19.6773100015567,-36.1822608191559,
124.596016924406)) ;
#100809 = CARTESIAN_POINT('Ctrl Pts',(-19.9358938823132,-36.1954381004665,
124.496620615535)) ;
#100810 = CARTESIAN_POINT('Ctrl Pts',(-20.1754329120152,-36.2087055609806,
124.35371536447)) ;
#100811 = CARTESIAN_POINT('Ctrl Pts',(-20.4216852100986,-36.2253194516678,
124.100451119342)) ;
#100812 = CARTESIAN_POINT('Ctrl Pts',(-20.5958971043548,-36.2452682510952,
123.713663631291)) ;
#100813 = CARTESIAN_POINT('Ctrl Pts',(-20.62753388448,-36.265189362626,123.291329360729)) ;
#100814 = CARTESIAN_POINT('Ctrl Pts',(-20.5142790125661,-36.2850558107989,
122.884311763888)) ;
#100815 = CARTESIAN_POINT('Ctrl Pts',(-20.266811237073,-36.305082157416,122.53784739008)) ;
#100816 = CARTESIAN_POINT('Ctrl Pts',(-19.9187012601791,-36.3249442018056,
122.298606139668)) ;
#100817 = CARTESIAN_POINT('Ctrl Pts',(-19.5084302667686,-36.3448895044867,
122.191459293807)) ;
#100818 = CARTESIAN_POINT('Ctrl Pts',(-19.0872181553148,-36.3647848115456,
122.230722799833)) ;
#100819 = CARTESIAN_POINT('Ctrl Pts',(-18.7044045852222,-36.3846780817132,
122.410659154903)) ;
#100820 = CARTESIAN_POINT('Ctrl Pts',(-18.4049752396743,-36.4046436743936,
122.711557273194)) ;
#100821 = CARTESIAN_POINT('Ctrl Pts',(-18.2267181674138,-36.4245189980784,
123.094752887157)) ;
#100822 = CARTESIAN_POINT('Ctrl Pts',(-18.1893125772977,-36.4444940606534,
123.517845506069)) ;
#100823 = CARTESIAN_POINT('Ctrl Pts',(-18.2990250302679,-36.4644464702845,
123.927655271407)) ;
#100824 = CARTESIAN_POINT('Ctrl Pts',(-18.5399108663696,-36.4842825245207,
124.273866185745)) ;
#100825 = CARTESIAN_POINT('Ctrl Pts',(-18.8866731555792,-36.5042604359382,
124.519217465692)) ;
#100826 = CARTESIAN_POINT('Ctrl Pts',(-19.2952238613191,-36.5241784854417,
124.63068223934)) ;
#100827 = CARTESIAN_POINT('Ctrl Pts',(-19.7164353919228,-36.5440466292098,
124.597224203483)) ;
#100828 = CARTESIAN_POINT('Ctrl Pts',(-20.1040334065352,-36.5640974857971,
124.419912357957)) ;
#100829 = CARTESIAN_POINT('Ctrl Pts',(-20.4042347444789,-36.583877922253,
124.125172411809)) ;
#100830 = CARTESIAN_POINT('Ctrl Pts',(-20.5886490037227,-36.6039079779308,
123.741383131109)) ;
#100831 = CARTESIAN_POINT('Ctrl Pts',(-20.6300092385519,-36.6237890831056,
123.320612341033)) ;
#100832 = CARTESIAN_POINT('Ctrl Pts',(-20.5264875248147,-36.6436695454733,
122.910815530542)) ;
#100833 = CARTESIAN_POINT('Ctrl Pts',(-20.2879611417274,-36.6636546926177,
122.559120609772)) ;
#100834 = CARTESIAN_POINT('Ctrl Pts',(-19.9453096168618,-36.6835452711541,
122.31119801954)) ;
#100835 = CARTESIAN_POINT('Ctrl Pts',(-19.5387739429105,-36.7034392910285,
122.194351448937)) ;
#100836 = CARTESIAN_POINT('Ctrl Pts',(-19.1162403085951,-36.7233607357549,
122.223172514364)) ;
#100837 = CARTESIAN_POINT('Ctrl Pts',(-18.7288845209874,-36.7432588738103,
122.393638288624)) ;
#100838 = CARTESIAN_POINT('Ctrl Pts',(-18.4210042480154,-36.7633296290264,
122.689049260052)) ;
#100839 = CARTESIAN_POINT('Ctrl Pts',(-18.234838684788,-36.7831151790776,
123.066415062849)) ;
#100840 = CARTESIAN_POINT('Ctrl Pts',(-18.1871546906861,-36.803098253955,
123.488546689358)) ;
#100841 = CARTESIAN_POINT('Ctrl Pts',(-18.2866782022465,-36.8230073366009,
123.900007540057)) ;
#100842 = CARTESIAN_POINT('Ctrl Pts',(-18.5190543067703,-36.8428658957237,
124.252624907996)) ;
#100843 = CARTESIAN_POINT('Ctrl Pts',(-18.8611587762036,-36.8629093395624,
124.50664228398)) ;
#100844 = CARTESIAN_POINT('Ctrl Pts',(-19.1973161978392,-36.8794094042916,
124.607325441852)) ;
#100845 = CARTESIAN_POINT('Ctrl Pts',(-19.4786626925985,-36.8927991441405,
124.615826935614)) ;
#100846 = CARTESIAN_POINT('Ctrl Pts',(-19.6837652519606,-36.9026560453489,
124.586090946552)) ;
#100847 = CARTESIAN_POINT('Ctrl Pts',(-19.8833582560379,-36.9126475711954,
124.520735574864)) ;
#100848 = CARTESIAN_POINT('Ctrl Pts',(-20.067423289702,-36.9225722516463,
124.422418074701)) ;
#100849 = CARTESIAN_POINT('Ctrl Pts',(-20.2330492727635,-36.9325828416907,
124.292613088508)) ;
#100850 = CARTESIAN_POINT('Ctrl Pts',(-20.4195221640316,-36.9458421023944,
124.085379899227)) ;
#100851 = CARTESIAN_POINT('Ctrl Pts',(-20.5482092913646,-36.9591931775447,
123.832415322028)) ;
#100852 = CARTESIAN_POINT('Ctrl Pts',(-20.6059663652822,-36.9723994867795,
123.56077910723)) ;
#100853 = CARTESIAN_POINT('Ctrl Pts',(-20.6137317498353,-36.9823863203698,
123.351006776767)) ;
#100854 = CARTESIAN_POINT('Ctrl Pts',(-20.5851472785443,-36.9923390478658,
123.143693415833)) ;
#100855 = CARTESIAN_POINT('Ctrl Pts',(-20.5202354273777,-37.0023871447074,
122.942695746541)) ;
#100856 = CARTESIAN_POINT('Ctrl Pts',(-20.4236378237333,-37.0122286015793,
122.759708784362)) ;
#100857 = CARTESIAN_POINT('Ctrl Pts',(-20.2952558105265,-37.0222148684928,
122.593637640325)) ;
#100858 = CARTESIAN_POINT('Ctrl Pts',(-20.1407800961841,-37.0321514693932,
122.452959086462)) ;
#100859 = CARTESIAN_POINT('Ctrl Pts',(-19.9622013494077,-37.0422014121802,
122.340085120913)) ;
#100860 = CARTESIAN_POINT('Ctrl Pts',(-19.7706479291959,-37.052051611866,
122.261368675457)) ;
#100861 = CARTESIAN_POINT('Ctrl Pts',(-19.5659719122388,-37.0620245167981,
122.216024338998)) ;
#100862 = CARTESIAN_POINT('Ctrl Pts',(-19.3559444965047,-37.0720228912777,
122.206949462052)) ;
#100863 = CARTESIAN_POINT('Ctrl Pts',(-19.147129183692,-37.0820430651477,
122.234686367879)) ;
#100864 = CARTESIAN_POINT('Ctrl Pts',(-18.9486238419902,-37.0919441090897,
122.297335146715)) ;
#100865 = CARTESIAN_POINT('Ctrl Pts',(-18.7622286581804,-37.101932912814,
122.394055158786)) ;
#100866 = CARTESIAN_POINT('Ctrl Pts',(-18.5959457412124,-37.1118983796458,
122.52148546394)) ;
#100867 = CARTESIAN_POINT('Ctrl Pts',(-18.4548033521353,-37.1218019419188,
122.674574492923)) ;
#100868 = CARTESIAN_POINT('Ctrl Pts',(-18.3407750697206,-37.1318626197968,
122.852679598472)) ;
#100869 = CARTESIAN_POINT('Ctrl Pts',(-18.2609184913322,-37.1417029177462,
123.043551929027)) ;
#100870 = CARTESIAN_POINT('Ctrl Pts',(-18.2141496389797,-37.1517659126557,
123.249845250982)) ;
#100871 = CARTESIAN_POINT('Ctrl Pts',(-18.2042519090553,-37.1616602068028,
123.457641259485)) ;
#100872 = CARTESIAN_POINT('Ctrl Pts',(-18.2301422352711,-37.1716020044997,
123.665013478792)) ;
#100873 = CARTESIAN_POINT('Ctrl Pts',(-18.2919639605262,-37.1816045820288,
123.866035471627)) ;
#100874 = CARTESIAN_POINT('Ctrl Pts',(-18.3883277857359,-37.1916390459499,
124.053684153228)) ;
#100875 = CARTESIAN_POINT('Ctrl Pts',(-18.5131689247711,-37.2014851844709,
124.218805309266)) ;
#100876 = CARTESIAN_POINT('Ctrl Pts',(-18.6665278050143,-37.2114663577079,
124.362001090757)) ;
#100877 = CARTESIAN_POINT('Ctrl Pts',(-18.8419581451818,-37.2214186516652,
124.476033552335)) ;
#100878 = CARTESIAN_POINT('Ctrl Pts',(-19.0353255527134,-37.2314174467998,
124.558511019165)) ;
#100879 = CARTESIAN_POINT('Ctrl Pts',(-19.2409658787007,-37.2414565550606,
124.605951228054)) ;
#100880 = CARTESIAN_POINT('Ctrl Pts',(-19.4472244337061,-37.2512814964997,
124.61717441126)) ;
#100881 = CARTESIAN_POINT('Ctrl Pts',(-19.6571102883794,-37.2613361835741,
124.592183127392)) ;
#100882 = CARTESIAN_POINT('Ctrl Pts',(-19.8571315557716,-37.2712789885143,
124.53146005105)) ;
#100883 = CARTESIAN_POINT('Ctrl Pts',(-20.0431259858872,-37.2811827745108,
124.437871105948)) ;
#100884 = CARTESIAN_POINT('Ctrl Pts',(-20.2123607666547,-37.2912295910756,
124.311522422952)) ;
#100885 = CARTESIAN_POINT('Ctrl Pts',(-20.355079153522,-37.3011251105543,
124.160115648401)) ;
#100886 = CARTESIAN_POINT('Ctrl Pts',(-20.471229061887,-37.3111871958787,
123.983355222886)) ;
#100887 = CARTESIAN_POINT('Ctrl Pts',(-20.5532277933068,-37.3210299068366,
123.793345810117)) ;
#100888 = CARTESIAN_POINT('Ctrl Pts',(-20.6021801457562,-37.3310206241427,
123.589120793377)) ;
#100889 = CARTESIAN_POINT('Ctrl Pts',(-20.6148150633087,-37.3409487072392,
123.380774320727)) ;
#100890 = CARTESIAN_POINT('Ctrl Pts',(-20.5913031305091,-37.350936637351,
123.172108442484)) ;
#100891 = CARTESIAN_POINT('Ctrl Pts',(-20.5312960752613,-37.3609724634783,
122.969843990903)) ;
#100892 = CARTESIAN_POINT('Ctrl Pts',(-20.439063762221,-37.3708278005919,
122.784302531812)) ;
#100893 = CARTESIAN_POINT('Ctrl Pts',(-20.3145262087417,-37.3808255354421,
122.615015421706)) ;
#100894 = CARTESIAN_POINT('Ctrl Pts',(-20.1638782950492,-37.3907334394265,
122.471154334386)) ;
#100895 = CARTESIAN_POINT('Ctrl Pts',(-19.9889330323923,-37.400744513975,
122.354141337136)) ;
#100896 = CARTESIAN_POINT('Ctrl Pts',(-19.7958356435216,-37.4107723695106,
122.269536200538)) ;
#100897 = CARTESIAN_POINT('Ctrl Pts',(-19.5945523247512,-37.4206299634158,
122.220229265376)) ;
#100898 = CARTESIAN_POINT('Ctrl Pts',(-19.3842398023815,-37.4306566502539,
122.205957811399)) ;
#100899 = CARTESIAN_POINT('Ctrl Pts',(-19.1746553810469,-37.4406853194077,
122.228947939233)) ;
#100900 = CARTESIAN_POINT('Ctrl Pts',(-18.9758587439458,-37.4505305276891,
122.28652467685)) ;
#100901 = CARTESIAN_POINT('Ctrl Pts',(-18.7870708871759,-37.4605212166522,
122.378591662848)) ;
#100902 = CARTESIAN_POINT('Ctrl Pts',(-18.6166165908333,-37.4705590929345,
122.502999376711)) ;
#100903 = CARTESIAN_POINT('Ctrl Pts',(-18.4729056358467,-37.4804034705767,
122.651937633883)) ;
#100904 = CARTESIAN_POINT('Ctrl Pts',(-18.3552637827284,-37.4903882749681,
122.82575284458)) ;
#100905 = CARTESIAN_POINT('Ctrl Pts',(-18.2698719431135,-37.5003278051867,
123.016500170408)) ;
#100906 = CARTESIAN_POINT('Ctrl Pts',(-18.2184419853709,-37.5103674932236,
123.221187480338)) ;
#100907 = CARTESIAN_POINT('Ctrl Pts',(-18.2034572768443,-37.5202557825919,
123.428541325561)) ;
#100908 = CARTESIAN_POINT('Ctrl Pts',(-18.2245235759724,-37.5302449062767,
123.637477495693)) ;
#100909 = CARTESIAN_POINT('Ctrl Pts',(-18.2815401834899,-37.5402049159513,
123.838952275133)) ;
#100910 = CARTESIAN_POINT('Ctrl Pts',(-18.3716856840116,-37.5501053456555,
124.026563212702)) ;
#100911 = CARTESIAN_POINT('Ctrl Pts',(-18.494785119563,-37.5601484270623,
124.198090824749)) ;
#100912 = CARTESIAN_POINT('Ctrl Pts',(-18.6437683872977,-37.5700558209699,
124.3436620814)) ;
#100913 = CARTESIAN_POINT('Ctrl Pts',(-18.8173484897518,-37.5800675519591,
124.462707035098)) ;
#100914 = CARTESIAN_POINT('Ctrl Pts',(-19.0095315531602,-37.5900997696738,
124.549604169209)) ;
#100915 = CARTESIAN_POINT('Ctrl Pts',(-19.2101350992192,-37.59995227892,124.601142946947)) ;
#100916 = CARTESIAN_POINT('Ctrl Pts',(-19.4188175642895,-37.609910215463,
124.617888348165)) ;
#100917 = CARTESIAN_POINT('Ctrl Pts',(-19.6288757201125,-37.6199490854713,
124.597608883713)) ;
#100918 = CARTESIAN_POINT('Ctrl Pts',(-19.8290137065175,-37.6298222406296,
124.542458221507)) ;
#100919 = CARTESIAN_POINT('Ctrl Pts',(-20.0202395446897,-37.6398955154793,
124.451563901292)) ;
#100920 = CARTESIAN_POINT('Ctrl Pts',(-20.1886741975902,-37.6497158326567,
124.332099066441)) ;
#100921 = CARTESIAN_POINT('Ctrl Pts',(-20.3376952868541,-37.6597945184502,
124.181545078313)) ;
#100922 = CARTESIAN_POINT('Ctrl Pts',(-20.4557107265369,-37.6696460298333,
124.011288566076)) ;
#100923 = CARTESIAN_POINT('Ctrl Pts',(-20.5444491544677,-37.6797194761399,
123.819044922932)) ;
#100924 = CARTESIAN_POINT('Ctrl Pts',(-20.5972161838608,-37.6895607512646,
123.618968933781)) ;
#100925 = CARTESIAN_POINT('Ctrl Pts',(-20.6153429770732,-37.6995458509214,
123.409854798316)) ;
#100926 = CARTESIAN_POINT('Ctrl Pts',(-20.5965487455393,-37.7095533270557,
123.200291391966)) ;
#100927 = CARTESIAN_POINT('Ctrl Pts',(-20.5423098898942,-37.7194759147646,
122.998872991443)) ;
#100928 = CARTESIAN_POINT('Ctrl Pts',(-20.4536480360329,-37.729462519038,
122.808541266526)) ;
#100929 = CARTESIAN_POINT('Ctrl Pts',(-20.332336766577,-37.7395026473721,
122.635829993168)) ;
#100930 = CARTESIAN_POINT('Ctrl Pts',(-20.1861599736761,-37.7493420819055,
122.489439390282)) ;
#100931 = CARTESIAN_POINT('Ctrl Pts',(-20.0130579461668,-37.7594061363965,
122.36782475606)) ;
#100932 = CARTESIAN_POINT('Ctrl Pts',(-19.8246828637868,-37.7692970556336,
122.279721634696)) ;
#100933 = CARTESIAN_POINT('Ctrl Pts',(-19.6219675903709,-37.7792890489397,
122.224688407359)) ;
#100934 = CARTESIAN_POINT('Ctrl Pts',(-19.4133634234643,-37.789251912899,
122.205938159688)) ;
#100935 = CARTESIAN_POINT('Ctrl Pts',(-19.2058328063247,-37.7991561727167,
122.223065189466)) ;
#100936 = CARTESIAN_POINT('Ctrl Pts',(-19.0013402560776,-37.8092166632881,
122.276967117826)) ;
#100937 = CARTESIAN_POINT('Ctrl Pts',(-18.8133528873735,-37.8190570129192,
122.363395895489)) ;
#100938 = CARTESIAN_POINT('Ctrl Pts',(-18.6392806009119,-37.8291199884092,
122.483574659019)) ;
#100939 = CARTESIAN_POINT('Ctrl Pts',(-18.4913282354017,-37.8390143085526,
122.629818849561)) ;
#100940 = CARTESIAN_POINT('Ctrl Pts',(-18.3700088729256,-37.8489560216842,
122.799976063624)) ;
#100941 = CARTESIAN_POINT('Ctrl Pts',(-18.279415391288,-37.8589589114783,
122.989789779582)) ;
#100942 = CARTESIAN_POINT('Ctrl Pts',(-18.2233347923612,-37.8689987686388,
123.193251803437)) ;
#100943 = CARTESIAN_POINT('Ctrl Pts',(-18.2033890402735,-37.8788229494764,
123.398837819712)) ;
#100944 = CARTESIAN_POINT('Ctrl Pts',(-18.2195295979396,-37.8888799229796,
123.609633003241)) ;
#100945 = CARTESIAN_POINT('Ctrl Pts',(-18.2716173896669,-37.8988080471667,
123.811761427347)) ;
#100946 = CARTESIAN_POINT('Ctrl Pts',(-18.3577187178275,-37.9087617422401,
124.002486489303)) ;
#100947 = CARTESIAN_POINT('Ctrl Pts',(-18.4769711397454,-37.9188079358154,
124.176798392997)) ;
#100948 = CARTESIAN_POINT('Ctrl Pts',(-18.6216236764101,-37.9286560381753,
124.324919228687)) ;
#100949 = CARTESIAN_POINT('Ctrl Pts',(-18.7913505328632,-37.9386176264029,
124.447586807908)) ;
#100950 = CARTESIAN_POINT('Ctrl Pts',(-18.9812025221382,-37.9486462965591,
124.539307200151)) ;
#100951 = CARTESIAN_POINT('Ctrl Pts',(-19.181661769281,-37.9585565994409,
124.596051340258)) ;
#100952 = CARTESIAN_POINT('Ctrl Pts',(-19.389402661016,-37.9684914832488,
124.61772594654)) ;
#100953 = CARTESIAN_POINT('Ctrl Pts',(-19.5999531728707,-37.9785326249394,
124.602647814423)) ;
#100954 = CARTESIAN_POINT('Ctrl Pts',(-19.8015999988339,-37.9884197461034,
124.552166441477)) ;
#100955 = CARTESIAN_POINT('Ctrl Pts',(-19.9935578270306,-37.9984120889519,
124.466868038177)) ;
#100956 = CARTESIAN_POINT('Ctrl Pts',(-20.1670084234208,-38.0083603901759,
124.349989391042)) ;
#100957 = CARTESIAN_POINT('Ctrl Pts',(-20.3175626208799,-38.018297967858,
124.205160842868)) ;
#100958 = CARTESIAN_POINT('Ctrl Pts',(-20.4414789275655,-38.0282845423085,
124.035663138194)) ;
#100959 = CARTESIAN_POINT('Ctrl Pts',(-20.5342491134349,-38.038313352217,
123.84633445262)) ;
#100960 = CARTESIAN_POINT('Ctrl Pts',(-20.5920528166999,-38.0481916735238,
123.646870313856)) ;
#100961 = CARTESIAN_POINT('Ctrl Pts',(-20.6150924690392,-38.0581833208712,
123.438074641308)) ;
#100962 = CARTESIAN_POINT('Ctrl Pts',(-20.6010405372188,-38.068217844309,
123.227595379122)) ;
#100963 = CARTESIAN_POINT('Ctrl Pts',(-20.5519273735408,-38.0780812011876,
123.026114679386)) ;
#100964 = CARTESIAN_POINT('Ctrl Pts',(-20.466884210456,-38.0881514278679,
122.832263240811)) ;
#100965 = CARTESIAN_POINT('Ctrl Pts',(-20.3521054816637,-38.0979937360026,
122.660089841333)) ;
#100966 = CARTESIAN_POINT('Ctrl Pts',(-20.2080246243361,-38.107954468026,
122.508137731308)) ;
#100967 = CARTESIAN_POINT('Ctrl Pts',(-20.038198302605,-38.1179923572241,
122.382882440475)) ;
#100968 = CARTESIAN_POINT('Ctrl Pts',(-19.8524261029089,-38.1278666401429,
122.290188722475)) ;
#100969 = CARTESIAN_POINT('Ctrl Pts',(-19.6494889540396,-38.1379363847604,
122.230017433712)) ;
#100970 = CARTESIAN_POINT('Ctrl Pts',(-19.4440940097249,-38.147769695106,
122.206445815597)) ;
#100971 = CARTESIAN_POINT('Ctrl Pts',(-19.2335783239654,-38.1577999384587,
122.218543085627)) ;
#100972 = CARTESIAN_POINT('Ctrl Pts',(-19.0284556912781,-38.1678322264371,
122.267635241908)) ;
#100973 = CARTESIAN_POINT('Ctrl Pts',(-18.8387371022189,-38.1776594029052,
122.349429641812)) ;
#100974 = CARTESIAN_POINT('Ctrl Pts',(-18.662755742526,-38.187664785772,122.464602000894)) ;
#100975 = CARTESIAN_POINT('Ctrl Pts',(-18.5097931669411,-38.1976474247647,
122.608349415091)) ;
#100976 = CARTESIAN_POINT('Ctrl Pts',(-18.3835843429591,-38.2076914919014,
122.777612783637)) ;
#100977 = CARTESIAN_POINT('Ctrl Pts',(-18.2904551402133,-38.2175127107054,
122.961897235804)) ;
#100978 = CARTESIAN_POINT('Ctrl Pts',(-18.228913755761,-38.2275495496434,
123.163725886586)) ;
#100979 = CARTESIAN_POINT('Ctrl Pts',(-18.2039782973916,-38.2375739617412,
123.372997474066)) ;
#100980 = CARTESIAN_POINT('Ctrl Pts',(-18.2150973209029,-38.2474260461465,
123.579823724448)) ;
#100981 = CARTESIAN_POINT('Ctrl Pts',(-18.2623014384473,-38.2574169428896,
123.784464923673)) ;
#100982 = CARTESIAN_POINT('Ctrl Pts',(-18.3436167643364,-38.2673349347906,
123.97648973343)) ;
#100983 = CARTESIAN_POINT('Ctrl Pts',(-18.458233201214,-38.2773630502476,
124.153414286625)) ;
#100984 = CARTESIAN_POINT('Ctrl Pts',(-18.5997314842118,-38.2872482261897,
124.305625822735)) ;
#100985 = CARTESIAN_POINT('Ctrl Pts',(-18.766947782583,-38.2972375845966,
124.432684039446)) ;
#100986 = CARTESIAN_POINT('Ctrl Pts',(-18.9548533656769,-38.3072787321768,
124.528877092213)) ;
#100987 = CARTESIAN_POINT('Ctrl Pts',(-19.1523136162172,-38.3171113551833,
124.590019608854)) ;
#100988 = CARTESIAN_POINT('Ctrl Pts',(-19.3606809885288,-38.3271054262941,
124.616962197993)) ;
#100989 = CARTESIAN_POINT('Ctrl Pts',(-19.5712845728842,-38.3371340839349,
124.606866062334)) ;
#100990 = CARTESIAN_POINT('Ctrl Pts',(-19.7740057105557,-38.3470184101277,
124.56125238547)) ;
#100991 = CARTESIAN_POINT('Ctrl Pts',(-19.9675216939867,-38.3569841536184,
124.480942711022)) ;
#100992 = CARTESIAN_POINT('Ctrl Pts',(-20.1450861014841,-38.3670125327496,
124.367295867582)) ;
#100993 = CARTESIAN_POINT('Ctrl Pts',(-20.2984877659855,-38.3769133789565,
124.226568088124)) ;
#100994 = CARTESIAN_POINT('Ctrl Pts',(-20.4270610601774,-38.3869720363736,
124.058721674151)) ;
#100995 = CARTESIAN_POINT('Ctrl Pts',(-20.5228145355135,-38.3968295991555,
123.874891014623)) ;
#100996 = CARTESIAN_POINT('Ctrl Pts',(-20.5866403088742,-38.4068980017087,
123.673106510751)) ;
#100997 = CARTESIAN_POINT('Ctrl Pts',(-20.6138575143591,-38.4167534004483,
123.467692701392)) ;
#100998 = CARTESIAN_POINT('Ctrl Pts',(-20.6055012221125,-38.4267482675222,
123.257742303916)) ;
#100999 = CARTESIAN_POINT('Ctrl Pts',(-20.5602077559239,-38.4367795625056,
123.051769934571)) ;
#101000 = CARTESIAN_POINT('Ctrl Pts',(-20.4814642001907,-38.4466460872322,
122.859864487918)) ;
#101001 = CARTESIAN_POINT('Ctrl Pts',(-20.3695390650992,-38.4566335579279,
122.682244937718)) ;
#101002 = CARTESIAN_POINT('Ctrl Pts',(-20.2291244780373,-38.4665783174918,
122.527301395614)) ;
#101003 = CARTESIAN_POINT('Ctrl Pts',(-20.0622287430392,-38.4766238734406,
122.397930530599)) ;
#101004 = CARTESIAN_POINT('Ctrl Pts',(-19.8789244142222,-38.4864834618157,
122.301108920624)) ;
#101005 = CARTESIAN_POINT('Ctrl Pts',(-19.6789175989075,-38.4964844169518,
122.236391582832)) ;
#101006 = CARTESIAN_POINT('Ctrl Pts',(-19.4726821039492,-38.5063886442293,
122.207495520675)) ;
#101007 = CARTESIAN_POINT('Ctrl Pts',(-19.2617238875487,-38.5164307211245,
122.214889174686)) ;
#101008 = CARTESIAN_POINT('Ctrl Pts',(-19.0579327918669,-38.5263383338106,
122.258125125702)) ;
#101009 = CARTESIAN_POINT('Ctrl Pts',(-18.8619377810463,-38.5363928644264,
122.337205356046)) ;
#101010 = CARTESIAN_POINT('Ctrl Pts',(-18.6859931942783,-38.5462536509752,
122.446886128224)) ;
#101011 = CARTESIAN_POINT('Ctrl Pts',(-18.5294712202615,-38.5562474060463,
122.586988957842)) ;
#101012 = CARTESIAN_POINT('Ctrl Pts',(-18.400420712983,-38.5661727662863,
122.750999772463)) ;
#101013 = CARTESIAN_POINT('Ctrl Pts',(-18.3008112095922,-38.5762006956816,
122.936770436318)) ;
#101014 = CARTESIAN_POINT('Ctrl Pts',(-18.2356782752846,-38.5860869624809,
123.134174522919)) ;
#101015 = CARTESIAN_POINT('Ctrl Pts',(-18.2052725853413,-38.5961187313791,
123.342835096657)) ;
#101016 = CARTESIAN_POINT('Ctrl Pts',(-18.2112643039306,-38.6060003272227,
123.550528308194)) ;
#101017 = CARTESIAN_POINT('Ctrl Pts',(-18.2539267473392,-38.6160622126907,
123.757681711865)) ;
#101018 = CARTESIAN_POINT('Ctrl Pts',(-18.3302825292228,-38.6259196467096,
123.950365011094)) ;
#101019 = CARTESIAN_POINT('Ctrl Pts',(-18.4400259339117,-38.6359128897515,
124.129481984297)) ;
#101020 = CARTESIAN_POINT('Ctrl Pts',(-18.5783449252527,-38.6458436506379,
124.285876999745)) ;
#101021 = CARTESIAN_POINT('Ctrl Pts',(-18.7978001477443,-38.6591926428351,
124.460861913959)) ;
#101022 = CARTESIAN_POINT('Ctrl Pts',(-19.0564632288545,-38.6724610156515,
124.573503641403)) ;
#101023 = CARTESIAN_POINT('Ctrl Pts',(-19.332523789923,-38.6857439570358,
124.615449417568)) ;
#101024 = CARTESIAN_POINT('Ctrl Pts',(-19.5435860555807,-38.6957867428781,
124.610291160415)) ;
#101025 = CARTESIAN_POINT('Ctrl Pts',(-19.7466277101908,-38.7056366854302,
124.569582991316)) ;
#101026 = CARTESIAN_POINT('Ctrl Pts',(-19.9425809703638,-38.7156339183491,
124.493607039836)) ;
#101027 = CARTESIAN_POINT('Ctrl Pts',(-20.1225268488081,-38.7256488136837,
124.384284378479)) ;
#101028 = CARTESIAN_POINT('Ctrl Pts',(-20.3318937272993,-38.7388884903219,
124.200838265263)) ;
#101029 = CARTESIAN_POINT('Ctrl Pts',(-20.5281688622949,-38.7554357147272,
123.908916031402)) ;
#101030 = CARTESIAN_POINT('Ctrl Pts',(-20.6137584771506,-38.7720831518583,
123.565384334872)) ;
#101031 = CARTESIAN_POINT('Ctrl Pts',(-20.6085739438225,-38.7853726493365,
123.286078455824)) ;
#101032 = CARTESIAN_POINT('Ctrl Pts',(-20.5693616566855,-38.7952460571589,
123.08223428913)) ;
#101033 = CARTESIAN_POINT('Ctrl Pts',(-20.4940484790816,-38.8052984347516,
122.884789857526)) ;
#101034 = CARTESIAN_POINT('Ctrl Pts',(-20.3871103436895,-38.8152020882925,
122.706124751837)) ;
#101035 = CARTESIAN_POINT('Ctrl Pts',(-20.250629247519,-38.8251463572878,
122.54780095501)) ;
#101036 = CARTESIAN_POINT('Ctrl Pts',(-20.0335844078658,-38.8384773656205,
122.370371670262)) ;
#101037 = CARTESIAN_POINT('Ctrl Pts',(-19.7113360013197,-38.8550989461448,
122.225466434777)) ;
#101038 = CARTESIAN_POINT('Ctrl Pts',(-19.3605438346263,-38.8716416168431,
122.198641643267)) ;
#101039 = CARTESIAN_POINT('Ctrl Pts',(-19.084761921183,-38.8849907764061,
122.250343327836)) ;
#101040 = CARTESIAN_POINT('Ctrl Pts',(-18.8243062404823,-38.8982189265656,
122.347966412132)) ;
#101041 = CARTESIAN_POINT('Ctrl Pts',(-18.5364156813843,-38.9148496037031,
122.553181914486)) ;
#101042 = CARTESIAN_POINT('Ctrl Pts',(-18.296306237545,-38.9347525429912,
122.901730636663)) ;
#101043 = CARTESIAN_POINT('Ctrl Pts',(-18.1891638956512,-38.9546554095944,
123.31104797171)) ;
#101044 = CARTESIAN_POINT('Ctrl Pts',(-18.227521324619,-38.9745685746993,
123.732809828716)) ;
#101045 = CARTESIAN_POINT('Ctrl Pts',(-18.409146223315,-38.9946044038406,
124.118102822698)) ;
#101046 = CARTESIAN_POINT('Ctrl Pts',(-18.7080073088718,-39.0144229787187,
124.415329588812)) ;
#101047 = CARTESIAN_POINT('Ctrl Pts',(-19.0927775117943,-39.0343932797607,
124.594594850276)) ;
#101048 = CARTESIAN_POINT('Ctrl Pts',(-19.5142395770282,-39.0542848121252,
124.631812031699)) ;
#101049 = CARTESIAN_POINT('Ctrl Pts',(-19.9254823216977,-39.0743079099418,
124.522010290735)) ;
#101050 = CARTESIAN_POINT('Ctrl Pts',(-20.2709166656606,-39.0941046628617,
124.281378877761)) ;
#101051 = CARTESIAN_POINT('Ctrl Pts',(-20.5163914412422,-39.1140657513505,
123.93518732308)) ;
#101052 = CARTESIAN_POINT('Ctrl Pts',(-20.628254947306,-39.1340440202826,
123.525352683612)) ;
#101053 = CARTESIAN_POINT('Ctrl Pts',(-20.5944405134673,-39.1538640350736,
123.105323024553)) ;
#101054 = CARTESIAN_POINT('Ctrl Pts',(-20.419247264824,-39.1738024443255,
122.719247022655)) ;
#101055 = CARTESIAN_POINT('Ctrl Pts',(-20.1204990497881,-39.1938495617179,
122.415126584749)) ;
#101056 = CARTESIAN_POINT('Ctrl Pts',(-19.7397607153773,-39.2136958075517,
122.233270712555)) ;
#101057 = CARTESIAN_POINT('Ctrl Pts',(-19.3198592895501,-39.2335447760638,
122.190591110322)) ;
#101058 = CARTESIAN_POINT('Ctrl Pts',(-18.9066442625955,-39.2535950783751,
122.295321814495)) ;
#101059 = CARTESIAN_POINT('Ctrl Pts',(-18.5576899822953,-39.2734300008063,
122.532358340522)) ;
#101060 = CARTESIAN_POINT('Ctrl Pts',(-18.3088686002448,-39.2933604020322,
122.875190487512)) ;
#101061 = CARTESIAN_POINT('Ctrl Pts',(-18.1916327971399,-39.313245347391,
123.281589035791)) ;
#101062 = CARTESIAN_POINT('Ctrl Pts',(-18.2210632496403,-39.3333179555424,
123.707289589619)) ;
#101063 = CARTESIAN_POINT('Ctrl Pts',(-18.3915669320377,-39.3531092718706,
124.092087397356)) ;
#101064 = CARTESIAN_POINT('Ctrl Pts',(-18.6846874615748,-39.3730740616378,
124.399097325358)) ;
#101065 = CARTESIAN_POINT('Ctrl Pts',(-19.0658342984923,-39.3930570173881,
124.586888425602)) ;
#101066 = CARTESIAN_POINT('Ctrl Pts',(-19.4844337905414,-39.4128655393642,
124.633801868885)) ;
#101067 = CARTESIAN_POINT('Ctrl Pts',(-19.8975626358599,-39.4328511141001,
124.534669422863)) ;
#101068 = CARTESIAN_POINT('Ctrl Pts',(-20.2503490487348,-39.4527337541685,
124.301535666755)) ;
#101069 = CARTESIAN_POINT('Ctrl Pts',(-20.5034830816029,-39.4726890663004,
123.961117049262)) ;
#101070 = CARTESIAN_POINT('Ctrl Pts',(-20.6250650986416,-39.4925634229082,
123.556327248378)) ;
#101071 = CARTESIAN_POINT('Ctrl Pts',(-20.601367918286,-39.5125456297692,
123.132160606297)) ;
#101072 = CARTESIAN_POINT('Ctrl Pts',(-20.4345121162113,-39.5324767077192,
122.742504639541)) ;
#101073 = CARTESIAN_POINT('Ctrl Pts',(-20.1449274720632,-39.5524036825742,
122.433328955836)) ;
#101074 = CARTESIAN_POINT('Ctrl Pts',(-19.769254896543,-39.5722361415231,
122.241636665334)) ;
#101075 = CARTESIAN_POINT('Ctrl Pts',(-19.417918476949,-39.5888938256983,
122.1977088759)) ;
#101076 = CARTESIAN_POINT('Ctrl Pts',(-19.1419056561803,-39.6021430496054,
122.235828467844)) ;
#101077 = CARTESIAN_POINT('Ctrl Pts',(-18.9408305883037,-39.6121920710566,
122.300533202526)) ;
#101078 = CARTESIAN_POINT('Ctrl Pts',(-18.7574950441059,-39.6220520792871,
122.397289626952)) ;
#101079 = CARTESIAN_POINT('Ctrl Pts',(-18.5363511197484,-39.6353355925117,
122.567786722781)) ;
#101080 = CARTESIAN_POINT('Ctrl Pts',(-18.3218450210094,-39.6519815115125,
122.849347598179)) ;
#101081 = CARTESIAN_POINT('Ctrl Pts',(-18.2164382084699,-39.6685354893286,
123.185154945585)) ;
#101082 = CARTESIAN_POINT('Ctrl Pts',(-18.2044962111491,-39.6818952183002,
123.465792838375)) ;
#101083 = CARTESIAN_POINT('Ctrl Pts',(-18.231716827372,-39.6917882700969,
123.671995353011)) ;
#101084 = CARTESIAN_POINT('Ctrl Pts',(-18.2946582960229,-39.7017782353779,
123.872338877242)) ;
#101085 = CARTESIAN_POINT('Ctrl Pts',(-18.3909769611807,-39.7117301162387,
124.058105400204)) ;
#101086 = CARTESIAN_POINT('Ctrl Pts',(-18.5194281831487,-39.7217784679306,
124.225785244661)) ;
#101087 = CARTESIAN_POINT('Ctrl Pts',(-18.6717018535489,-39.7316197520368,
124.36588109939)) ;
#101088 = CARTESIAN_POINT('Ctrl Pts',(-18.848276110562,-39.7416064551624,
124.479397195753)) ;
#101089 = CARTESIAN_POINT('Ctrl Pts',(-19.0408979117356,-39.7515414839799,
124.560259154936)) ;
#101090 = CARTESIAN_POINT('Ctrl Pts',(-19.2470780361926,-39.7615972788868,
124.606820788974)) ;
#101091 = CARTESIAN_POINT('Ctrl Pts',(-19.4534807768855,-39.771425642176,
124.616970805183)) ;
#101092 = CARTESIAN_POINT('Ctrl Pts',(-19.6633426209056,-39.781486612074,
124.590821806707)) ;
#101093 = CARTESIAN_POINT('Ctrl Pts',(-19.8625270132295,-39.7914008909638,
124.529358170323)) ;
#101094 = CARTESIAN_POINT('Ctrl Pts',(-20.0499564510726,-39.801409885432,
124.433712289956)) ;
#101095 = CARTESIAN_POINT('Ctrl Pts',(-20.2180166291829,-39.8114397199958,
124.306370914915)) ;
#101096 = CARTESIAN_POINT('Ctrl Pts',(-20.3592599577295,-39.821297950068,
124.154683609805)) ;
#101097 = CARTESIAN_POINT('Ctrl Pts',(-20.4738128783536,-39.8312966558104,
123.978476459926)) ;
#101098 = CARTESIAN_POINT('Ctrl Pts',(-20.5554308678287,-39.8411913117292,
123.787099072571)) ;
#101099 = CARTESIAN_POINT('Ctrl Pts',(-20.6033009346245,-39.8512543761131,
123.581065764927)) ;
#101100 = CARTESIAN_POINT('Ctrl Pts',(-20.6146498647158,-39.861094034393,
123.374482663538)) ;
#101101 = CARTESIAN_POINT('Ctrl Pts',(-20.5896704855374,-39.8711572014749,
123.164432257728)) ;
#101102 = CARTESIAN_POINT('Ctrl Pts',(-20.5294406556673,-39.881051446602,
122.965310865691)) ;
#101103 = CARTESIAN_POINT('Ctrl Pts',(-20.4356297199915,-39.8909932682066,
122.778567325915)) ;
#101104 = CARTESIAN_POINT('Ctrl Pts',(-20.3100866513311,-39.9009957991247,
122.60983556651)) ;
#101105 = CARTESIAN_POINT('Ctrl Pts',(-20.1564664331311,-39.9110304255822,
122.465266919416)) ;
#101106 = CARTESIAN_POINT('Ctrl Pts',(-19.9835680100836,-39.9208759605686,
122.351462351068)) ;
#101107 = CARTESIAN_POINT('Ctrl Pts',(-19.7910775169311,-39.9308593854076,
122.267849933268)) ;
#101108 = CARTESIAN_POINT('Ctrl Pts',(-19.5876362958034,-39.9408097757727,
122.219127757311)) ;
#101109 = CARTESIAN_POINT('Ctrl Pts',(-19.3778391871509,-39.9508074160698,
122.20612563894)) ;
#101110 = CARTESIAN_POINT('Ctrl Pts',(-19.1681833577415,-39.960846496633,
122.230265155625)) ;
#101111 = CARTESIAN_POINT('Ctrl Pts',(-18.9700405365513,-39.9706726474021,
122.288727946231)) ;
#101112 = CARTESIAN_POINT('Ctrl Pts',(-18.780591774925,-39.9807292223312,
122.382551513146)) ;
#101113 = CARTESIAN_POINT('Ctrl Pts',(-18.6124777629719,-39.9906697617115,
122.506703807935)) ;
#101114 = CARTESIAN_POINT('Ctrl Pts',(-18.4685284555379,-40.0005741546879,
122.657157911358)) ;
#101115 = CARTESIAN_POINT('Ctrl Pts',(-18.3513522549896,-40.0106208088928,
122.832864711475)) ;
#101116 = CARTESIAN_POINT('Ctrl Pts',(-18.2675466290961,-40.0205163708312,
123.023310139659)) ;
#101117 = CARTESIAN_POINT('Ctrl Pts',(-18.2172646577187,-40.0305784486768,
123.228752858168)) ;
#101118 = CARTESIAN_POINT('Ctrl Pts',(-18.2035979933319,-40.0404211470905,
123.435248771795)) ;
#101119 = CARTESIAN_POINT('Ctrl Pts',(-18.2258312988387,-40.050411922052,
123.644079110156)) ;
#101120 = CARTESIAN_POINT('Ctrl Pts',(-18.2836612249602,-40.0603397870711,
123.844634382298)) ;
#101121 = CARTESIAN_POINT('Ctrl Pts',(-18.3756796939924,-40.0703285318373,
124.033399255151)) ;
#101122 = CARTESIAN_POINT('Ctrl Pts',(-18.4998707520777,-40.0803613174242,
124.20388557405)) ;
#101123 = CARTESIAN_POINT('Ctrl Pts',(-18.6491083926149,-40.0902280020449,
124.347939944601)) ;
#101124 = CARTESIAN_POINT('Ctrl Pts',(-18.8224225122483,-40.100189894208,
124.465518464563)) ;
#101125 = CARTESIAN_POINT('Ctrl Pts',(-19.0150180752083,-40.1102233711206,
124.551524100041)) ;
#101126 = CARTESIAN_POINT('Ctrl Pts',(-19.2165333231762,-40.1201077123689,
124.602348216435)) ;
#101127 = CARTESIAN_POINT('Ctrl Pts',(-19.4275052057325,-40.13017065449,124.617681843025)) ;
#101128 = CARTESIAN_POINT('Ctrl Pts',(-19.6335421802486,-40.1400210561096,
124.596701422637)) ;
#101129 = CARTESIAN_POINT('Ctrl Pts',(-19.8365009244841,-40.1500479448992,
124.539772935942)) ;
#101130 = CARTESIAN_POINT('Ctrl Pts',(-20.0262992571282,-40.1600765598555,
124.447948653394)) ;
#101131 = CARTESIAN_POINT('Ctrl Pts',(-20.1943553181818,-40.1699217829755,
124.32715130238)) ;
#101132 = CARTESIAN_POINT('Ctrl Pts',(-20.3414348912541,-40.1799124667815,
124.177201638012)) ;
#101133 = CARTESIAN_POINT('Ctrl Pts',(-20.4604129709586,-40.1899503488539,
124.002914142887)) ;
#101134 = CARTESIAN_POINT('Ctrl Pts',(-20.545979628229,-40.1997947084927,
123.814463204431)) ;
#101135 = CARTESIAN_POINT('Ctrl Pts',(-20.5986526084436,-40.2097795791075,
123.61129541818)) ;
#101136 = CARTESIAN_POINT('Ctrl Pts',(-20.6152731232736,-40.2197188624361,
123.402971688009)) ;
#101137 = CARTESIAN_POINT('Ctrl Pts',(-20.5952065539716,-40.2297594718093,
123.192864132009)) ;
#101138 = CARTESIAN_POINT('Ctrl Pts',(-20.5399724504445,-40.2396443227225,
122.992503402502)) ;
#101139 = CARTESIAN_POINT('Ctrl Pts',(-20.4499839838021,-40.2496462788913,
122.802494552139)) ;
#101140 = CARTESIAN_POINT('Ctrl Pts',(-20.3294834698505,-40.2595648756118,
122.632277031866)) ;
#101141 = CARTESIAN_POINT('Ctrl Pts',(-20.1793573778973,-40.2696116976876,
122.483744845768)) ;
#101142 = CARTESIAN_POINT('Ctrl Pts',(-20.0087618788735,-40.2794859788003,
122.365403091064)) ;
#101143 = CARTESIAN_POINT('Ctrl Pts',(-19.8168930839442,-40.2895401788449,
122.276810358682)) ;
#101144 = CARTESIAN_POINT('Ctrl Pts',(-19.6157324060965,-40.2994356084801,
122.223627804589)) ;
#101145 = CARTESIAN_POINT('Ctrl Pts',(-19.4049800444106,-40.3094972367975,
122.205843630002)) ;
#101146 = CARTESIAN_POINT('Ctrl Pts',(-19.1988492745419,-40.3193418656274,
122.224487876728)) ;
#101147 = CARTESIAN_POINT('Ctrl Pts',(-18.9965589509404,-40.329301913233,
122.278544631675)) ;
#101148 = CARTESIAN_POINT('Ctrl Pts',(-18.8054174650425,-40.339340219407,
122.367971854401)) ;
#101149 = CARTESIAN_POINT('Ctrl Pts',(-18.6352824491559,-40.3492135188397,
122.486932297712)) ;
#101150 = CARTESIAN_POINT('Ctrl Pts',(-18.4855140010523,-40.359286780426,
122.636593459226)) ;
#101151 = CARTESIAN_POINT('Ctrl Pts',(-18.3667834334485,-40.3691070063827,
122.805545167445)) ;
#101152 = CARTESIAN_POINT('Ctrl Pts',(-18.2767571497258,-40.3791860703222,
122.99730368283)) ;
#101153 = CARTESIAN_POINT('Ctrl Pts',(-18.2225286191733,-40.389036160342,
123.197214794248)) ;
#101154 = CARTESIAN_POINT('Ctrl Pts',(-18.2033013064807,-40.3991149139558,
123.40817442046)) ;
#101155 = CARTESIAN_POINT('Ctrl Pts',(-18.2203931956037,-40.4089363812152,
123.613989798521)) ;
#101156 = CARTESIAN_POINT('Ctrl Pts',(-18.273929526605,-40.4190019795729,
123.818666747158)) ;
#101157 = CARTESIAN_POINT('Ctrl Pts',(-18.3608545822701,-40.4289046353476,
124.007892489207)) ;
#101158 = CARTESIAN_POINT('Ctrl Pts',(-18.4809798613875,-40.4389554611772,
124.18167274559)) ;
#101159 = CARTESIAN_POINT('Ctrl Pts',(-18.6267630610463,-40.4488296655161,
124.329518269347)) ;
#101160 = CARTESIAN_POINT('Ctrl Pts',(-18.7993190281747,-40.4589021155552,
124.452178869669)) ;
#101161 = CARTESIAN_POINT('Ctrl Pts',(-18.9859194321063,-40.4687311323287,
124.541034176296)) ;
#101162 = CARTESIAN_POINT('Ctrl Pts',(-19.1897830873164,-40.4787979782435,
124.597733520708)) ;
#101163 = CARTESIAN_POINT('Ctrl Pts',(-19.3967719275083,-40.4886881495453,
124.617687610617)) ;
#101164 = CARTESIAN_POINT('Ctrl Pts',(-19.6062174234657,-40.4986803431691,
124.601693990151)) ;
#101165 = CARTESIAN_POINT('Ctrl Pts',(-19.8090634899629,-40.5086431537925,
124.549535305381)) ;
#101166 = CARTESIAN_POINT('Ctrl Pts',(-19.9988895957124,-40.518547426636,
124.463929419697)) ;
#101167 = CARTESIAN_POINT('Ctrl Pts',(-20.1735429954922,-40.5286079184406,
124.344686564957)) ;
#101168 = CARTESIAN_POINT('Ctrl Pts',(-20.3217553007367,-40.5384482501129,
124.20031865067)) ;
#101169 = CARTESIAN_POINT('Ctrl Pts',(-20.4455592782769,-40.5485112962047,
124.028803450596)) ;
#101170 = CARTESIAN_POINT('Ctrl Pts',(-20.5360204974215,-40.5584053518998,
123.841477170554)) ;
#101171 = CARTESIAN_POINT('Ctrl Pts',(-20.5933981036872,-40.5683480522227,
123.640504075308)) ;
#101172 = CARTESIAN_POINT('Ctrl Pts',(-20.6151916590627,-40.5783537931503,
123.431261768905)) ;
#101173 = CARTESIAN_POINT('Ctrl Pts',(-20.6000648886758,-40.5883747036659,
123.2211393517)) ;
#101174 = CARTESIAN_POINT('Ctrl Pts',(-20.5495814744401,-40.5982654391158,
123.019420105902)) ;
#101175 = CARTESIAN_POINT('Ctrl Pts',(-20.4642659195488,-40.6082569798447,
122.827481900596)) ;
#101176 = CARTESIAN_POINT('Ctrl Pts',(-20.347379365736,-40.6182048402663,
122.654062293566)) ;
#101177 = CARTESIAN_POINT('Ctrl Pts',(-20.2024623808449,-40.6281515094527,
122.503294270521)) ;
#101178 = CARTESIAN_POINT('Ctrl Pts',(-20.0317256124835,-40.6381995855883,
122.378919527723)) ;
#101179 = CARTESIAN_POINT('Ctrl Pts',(-19.8458410740601,-40.6480471835939,
122.287772703259)) ;
#101180 = CARTESIAN_POINT('Ctrl Pts',(-19.6448432958164,-40.6580089066784,
122.228991799962)) ;
#101181 = CARTESIAN_POINT('Ctrl Pts',(-19.4352417793941,-40.6680375417614,
122.206112663733)) ;
#101182 = CARTESIAN_POINT('Ctrl Pts',(-19.2273522130901,-40.6779478500794,
122.219741726485)) ;
#101183 = CARTESIAN_POINT('Ctrl Pts',(-19.0243399263925,-40.6878827472153,
122.268855305552)) ;
#101184 = CARTESIAN_POINT('Ctrl Pts',(-18.8309828392154,-40.6979238301579,
122.35354043074)) ;
#101185 = CARTESIAN_POINT('Ctrl Pts',(-18.6578647059456,-40.7078111729861,
122.468611619995)) ;
#101186 = CARTESIAN_POINT('Ctrl Pts',(-18.5055373892302,-40.7178026879254,
122.613227820866)) ;
#101187 = CARTESIAN_POINT('Ctrl Pts',(-18.3811968009084,-40.7277540791219,
122.78148339611)) ;
#101188 = CARTESIAN_POINT('Ctrl Pts',(-18.2878153423615,-40.7376866124545,
122.968251315835)) ;
#101189 = CARTESIAN_POINT('Ctrl Pts',(-18.2278162912962,-40.747683770354,
123.169668517702)) ;
#101190 = CARTESIAN_POINT('Ctrl Pts',(-18.2036472734239,-40.7576687805175,
123.378221810927)) ;
#101191 = CARTESIAN_POINT('Ctrl Pts',(-18.216434819811,-40.7677116070873,
123.588937437878)) ;
#101192 = CARTESIAN_POINT('Ctrl Pts',(-18.2641263294702,-40.7775418413922,
123.790054955095)) ;
#101193 = CARTESIAN_POINT('Ctrl Pts',(-18.3479442221864,-40.7876178666269,
123.984549413725)) ;
#101194 = CARTESIAN_POINT('Ctrl Pts',(-18.4616334114474,-40.7974701031178,
124.157737029947)) ;
#101195 = CARTESIAN_POINT('Ctrl Pts',(-18.6066677695521,-40.8075433095519,
124.312000978312)) ;
#101196 = CARTESIAN_POINT('Ctrl Pts',(-18.7724548681492,-40.8173848190591,
124.435805633127)) ;
#101197 = CARTESIAN_POINT('Ctrl Pts',(-18.9590880493065,-40.8273457658389,
124.530768118377)) ;
#101198 = CARTESIAN_POINT('Ctrl Pts',(-19.1610443905616,-40.8373835946389,
124.591950436125)) ;
#101199 = CARTESIAN_POINT('Ctrl Pts',(-19.3671277911772,-40.8472579043934,
124.617113252493)) ;
#101200 = CARTESIAN_POINT('Ctrl Pts',(-19.5784987611481,-40.8573276020665,
124.605884465264)) ;
#101201 = CARTESIAN_POINT('Ctrl Pts',(-19.7799378276875,-40.8671610733539,
124.559341822632)) ;
#101202 = CARTESIAN_POINT('Ctrl Pts',(-19.9742509902703,-40.8771907198839,
124.477484627646)) ;
#101203 = CARTESIAN_POINT('Ctrl Pts',(-20.151142618583,-40.8872252342113,
124.362531493512)) ;
#101204 = CARTESIAN_POINT('Ctrl Pts',(-20.3025078132816,-40.8970505196821,
124.221977771566)) ;
#101205 = CARTESIAN_POINT('Ctrl Pts',(-20.4297799542184,-40.9070547612307,
124.054566863832)) ;
#101206 = CARTESIAN_POINT('Ctrl Pts',(-20.5257938311325,-40.9170374063098,
123.867906059799)) ;
#101207 = CARTESIAN_POINT('Ctrl Pts',(-20.5880805640029,-40.9270826034013,
123.666142451919)) ;
#101208 = CARTESIAN_POINT('Ctrl Pts',(-20.6141561796031,-40.9369057191614,
123.461275147051)) ;
#101209 = CARTESIAN_POINT('Ctrl Pts',(-20.6045831798159,-40.9469403309617,
123.250536080358)) ;
#101210 = CARTESIAN_POINT('Ctrl Pts',(-20.5580318847412,-40.9569653397348,
123.044977463719)) ;
#101211 = CARTESIAN_POINT('Ctrl Pts',(-20.4783225237379,-40.9668172645764,
122.853807555761)) ;
#101212 = CARTESIAN_POINT('Ctrl Pts',(-20.3653416559623,-40.9768082028991,
122.676771216726)) ;
#101213 = CARTESIAN_POINT('Ctrl Pts',(-20.2244402001406,-40.9867261880456,
122.523042785601)) ;
#101214 = CARTESIAN_POINT('Ctrl Pts',(-20.0572136257415,-40.9967542889411,
122.39468990882)) ;
#101215 = CARTESIAN_POINT('Ctrl Pts',(-19.8729266931194,-41.0066395298837,
122.298623693847)) ;
#101216 = CARTESIAN_POINT('Ctrl Pts',(-19.6728303893407,-41.0166286428503,
122.234864815255)) ;
#101217 = CARTESIAN_POINT('Ctrl Pts',(-19.4635495452488,-41.0266707071911,
122.207129365831)) ;
#101218 = CARTESIAN_POINT('Ctrl Pts',(-19.2570735104498,-41.0364999085956,
122.215570738549)) ;
#101219 = CARTESIAN_POINT('Ctrl Pts',(-19.0514845775134,-41.0465067493538,
122.260076795053)) ;
#101220 = CARTESIAN_POINT('Ctrl Pts',(-18.8571148508699,-41.0564942735457,
122.339588737422)) ;
#101221 = CARTESIAN_POINT('Ctrl Pts',(-18.6788780340058,-41.0665239193543,
122.452209536483)) ;
#101222 = CARTESIAN_POINT('Ctrl Pts',(-18.5251259197854,-41.076397950093,
122.591708322044)) ;
#101223 = CARTESIAN_POINT('Ctrl Pts',(-18.3961453376715,-41.0863972729571,
122.757663550958)) ;
#101224 = CARTESIAN_POINT('Ctrl Pts',(-18.2985943354105,-41.0963081085327,
122.941814170034)) ;
#101225 = CARTESIAN_POINT('Ctrl Pts',(-18.233666624653,-41.1063623565068,
123.142931894614)) ;
#101226 = CARTESIAN_POINT('Ctrl Pts',(-18.2049587347325,-41.1162211007695,
123.348232180008)) ;
#101227 = CARTESIAN_POINT('Ctrl Pts',(-18.2123617920147,-41.1262891868425,
123.559734930369)) ;
#101228 = CARTESIAN_POINT('Ctrl Pts',(-18.2554723235152,-41.136144670022,
123.762411198644)) ;
#101229 = CARTESIAN_POINT('Ctrl Pts',(-18.3336239177919,-41.1461395158162,
123.957452723125)) ;
#101230 = CARTESIAN_POINT('Ctrl Pts',(-18.4452498976815,-41.1561708114787,
124.13638221669)) ;
#101231 = CARTESIAN_POINT('Ctrl Pts',(-18.5836883068814,-41.1660373547686,
124.290859230364)) ;
#101232 = CARTESIAN_POINT('Ctrl Pts',(-18.7486102234299,-41.176024750532,
124.420767830943)) ;
#101233 = CARTESIAN_POINT('Ctrl Pts',(-18.9327951254557,-41.185969791262,
124.519771175335)) ;
#101234 = CARTESIAN_POINT('Ctrl Pts',(-19.1333460759953,-41.1960142974787,
124.585816738068)) ;
#101235 = CARTESIAN_POINT('Ctrl Pts',(-19.3385664298237,-41.205877803616,
124.615684128487)) ;
#101236 = CARTESIAN_POINT('Ctrl Pts',(-19.5485335350719,-41.2158706644521,
124.609757101276)) ;
#101237 = CARTESIAN_POINT('Ctrl Pts',(-19.7529882230433,-41.225796858171,
124.567828907933)) ;
#101238 = CARTESIAN_POINT('Ctrl Pts',(-19.9488341034307,-41.2358157842036,
124.490377466574)) ;
#101239 = CARTESIAN_POINT('Ctrl Pts',(-20.1265464889539,-41.2457307835712,
124.381379470427)) ;
#101240 = CARTESIAN_POINT('Ctrl Pts',(-20.2847612620487,-41.2557855551285,
124.241237890879)) ;
#101241 = CARTESIAN_POINT('Ctrl Pts',(-20.4138157488799,-41.265644517426,
124.079019167484)) ;
#101242 = CARTESIAN_POINT('Ctrl Pts',(-20.5144188110289,-41.2756387612639,
123.894597676821)) ;
#101243 = CARTESIAN_POINT('Ctrl Pts',(-20.5811232639661,-41.2855639906881,
123.696852864862)) ;
#101244 = CARTESIAN_POINT('Ctrl Pts',(-20.6128038064126,-41.2955919545796,
123.48845564233)) ;
#101245 = CARTESIAN_POINT('Ctrl Pts',(-20.608101821923,-41.30547821421,123.280637193688)) ;
#101246 = CARTESIAN_POINT('Ctrl Pts',(-20.5669083907062,-41.3155099772878,
123.073835781524)) ;
#101247 = CARTESIAN_POINT('Ctrl Pts',(-20.4917400895137,-41.3253916035819,
122.880129159094)) ;
#101248 = CARTESIAN_POINT('Ctrl Pts',(-20.3822003976352,-41.3354533730681,
122.699206766562)) ;
#101249 = CARTESIAN_POINT('Ctrl Pts',(-20.2457425972421,-41.3453112405636,
122.543195313791)) ;
#101250 = CARTESIAN_POINT('Ctrl Pts',(-20.0824091516552,-41.3553028656809,
122.411153460934)) ;
#101251 = CARTESIAN_POINT('Ctrl Pts',(-19.8995868245728,-41.3652396647892,
122.310050768588)) ;
#101252 = CARTESIAN_POINT('Ctrl Pts',(-19.7010211447952,-41.3752304943465,
122.241575162717)) ;
#101253 = CARTESIAN_POINT('Ctrl Pts',(-19.4928678909679,-41.3852537300597,
122.208751643948)) ;
#101254 = CARTESIAN_POINT('Ctrl Pts',(-19.2848503987295,-41.3951500780889,
122.212345027075)) ;
#101255 = CARTESIAN_POINT('Ctrl Pts',(-19.0785930235021,-41.4051396405914,
122.25193889369)) ;
#101256 = CARTESIAN_POINT('Ctrl Pts',(-18.8815182789459,-41.4151799482759,
122.32751453515)) ;
#101257 = CARTESIAN_POINT('Ctrl Pts',(-18.7039001527536,-41.4250222516231,
122.433692955489)) ;
#101258 = CARTESIAN_POINT('Ctrl Pts',(-18.5443879687289,-41.4350459599022,
122.571346680599)) ;
#101259 = CARTESIAN_POINT('Ctrl Pts',(-18.3685498378474,-41.4482681373699,
122.786707611366)) ;
#101260 = CARTESIAN_POINT('Ctrl Pts',(-18.2520956910167,-41.4615607224292,
123.044183153437)) ;
#101261 = CARTESIAN_POINT('Ctrl Pts',(-18.2068004013946,-41.4748455783508,
123.319789054625)) ;
#101262 = CARTESIAN_POINT('Ctrl Pts',(-18.2090769291731,-41.4848178055236,
123.529402754101)) ;
#101263 = CARTESIAN_POINT('Ctrl Pts',(-18.247124572802,-41.4947264219626,
123.73423306043)) ;
#101264 = CARTESIAN_POINT('Ctrl Pts',(-18.3212891788336,-41.5047796273463,
123.932122506308)) ;
#101265 = CARTESIAN_POINT('Ctrl Pts',(-18.4265787826922,-41.5146447611066,
124.110821634425)) ;
#101266 = CARTESIAN_POINT('Ctrl Pts',(-18.6083393836921,-41.5279838187329,
124.324380294906)) ;
#101267 = CARTESIAN_POINT('Ctrl Pts',(-18.8983223753606,-41.544553006066,
124.524474927529)) ;
#101268 = CARTESIAN_POINT('Ctrl Pts',(-19.2406726094886,-41.5611981459171,
124.614254626123)) ;
#101269 = CARTESIAN_POINT('Ctrl Pts',(-19.5196923545578,-41.5744704483905,
124.612735692632)) ;
#101270 = CARTESIAN_POINT('Ctrl Pts',(-19.7261709828644,-41.5844514118381,
124.575442073789)) ;
#101271 = CARTESIAN_POINT('Ctrl Pts',(-19.9223348541255,-41.5943932439074,
124.503254265008)) ;
#101272 = CARTESIAN_POINT('Ctrl Pts',(-20.1643780464931,-41.6077128131228,
124.362490991219)) ;
#101273 = CARTESIAN_POINT('Ctrl Pts',(-20.4126433730669,-41.6242429680556,
124.113592083793)) ;
#101274 = CARTESIAN_POINT('Ctrl Pts',(-20.5921670637875,-41.6442646935477,
123.727694403627)) ;
#101275 = CARTESIAN_POINT('Ctrl Pts',(-20.6290956659059,-41.6640760901545,
123.307969401579)) ;
#101276 = CARTESIAN_POINT('Ctrl Pts',(-20.520362522497,-41.6840613388633,
122.897277594779)) ;
#101277 = CARTESIAN_POINT('Ctrl Pts',(-20.2787818073189,-41.7039554014993,
122.549964049023)) ;
#101278 = CARTESIAN_POINT('Ctrl Pts',(-19.9329550815322,-41.7238870806729,
122.3050047685)) ;
#101279 = CARTESIAN_POINT('Ctrl Pts',(-19.5235495259994,-41.7438511351449,
122.192845312316)) ;
#101280 = CARTESIAN_POINT('Ctrl Pts',(-19.1021635775986,-41.7637320369078,
122.226667842613)) ;
#101281 = CARTESIAN_POINT('Ctrl Pts',(-18.7163705659198,-41.7836706985162,
122.402389669507)) ;
#101282 = CARTESIAN_POINT('Ctrl Pts',(-18.4142829913877,-41.8035672237715,
122.698551018439)) ;
#101283 = CARTESIAN_POINT('Ctrl Pts',(-18.2307709082302,-41.8234622622258,
123.079712248742)) ;
#101284 = CARTESIAN_POINT('Ctrl Pts',(-18.1882630419212,-41.8434260855319,
123.502031891265)) ;
#101285 = CARTESIAN_POINT('Ctrl Pts',(-18.2916654938259,-41.8633002096609,
123.911795841578)) ;
#101286 = CARTESIAN_POINT('Ctrl Pts',(-18.5295625163035,-41.8832752853882,
124.263664488095)) ;
#101287 = CARTESIAN_POINT('Ctrl Pts',(-18.873219444132,-41.9032288547448,
124.512455073523)) ;
#101288 = CARTESIAN_POINT('Ctrl Pts',(-19.2785711741301,-41.9230667649326,
124.62913406062)) ;
#101289 = CARTESIAN_POINT('Ctrl Pts',(-19.7023607638137,-41.9430425935036,
124.600734820372)) ;
#101290 = CARTESIAN_POINT('Ctrl Pts',(-20.0896826076553,-41.9629606382138,
124.429504601507)) ;
#101291 = CARTESIAN_POINT('Ctrl Pts',(-20.3954160704905,-41.9828308840015,
124.137780541128)) ;
#101292 = CARTESIAN_POINT('Ctrl Pts',(-20.5842821717011,-42.0028798871011,
123.755726965566)) ;
#101293 = CARTESIAN_POINT('Ctrl Pts',(-20.6312932293781,-42.0226591283419,
123.337676726068)) ;
#101294 = CARTESIAN_POINT('Ctrl Pts',(-20.5322532579379,-42.0426891920508,
122.923558264065)) ;
#101295 = CARTESIAN_POINT('Ctrl Pts',(-20.2989102097368,-42.0625714769527,
122.57095992708)) ;
#101296 = CARTESIAN_POINT('Ctrl Pts',(-19.9600336133139,-42.0824537778457,
122.318274230275)) ;
#101297 = CARTESIAN_POINT('Ctrl Pts',(-19.5531344393446,-42.1024368874641,
122.195898486587)) ;
#101298 = CARTESIAN_POINT('Ctrl Pts',(-19.1308511111101,-42.122327282842,
122.21966427291)) ;
#101299 = CARTESIAN_POINT('Ctrl Pts',(-18.7417287536698,-42.1422240728762,
122.385543026012)) ;
#101300 = CARTESIAN_POINT('Ctrl Pts',(-18.4318799171412,-42.1621411268179,
122.674260711236)) ;
#101301 = CARTESIAN_POINT('Ctrl Pts',(-18.2384283651542,-42.1821446750214,
123.053114066317)) ;
#101302 = CARTESIAN_POINT('Ctrl Pts',(-18.1866755979221,-42.202082968674,
123.473865099148)) ;
#101303 = CARTESIAN_POINT('Ctrl Pts',(-18.2800552694069,-42.2219044561069,
123.884855024677)) ;
#101304 = CARTESIAN_POINT('Ctrl Pts',(-18.5094895023282,-42.2418828490978,
124.242301803889)) ;
#101305 = CARTESIAN_POINT('Ctrl Pts',(-18.8460303591808,-42.2617812307115,
124.498833941423)) ;
#101306 = CARTESIAN_POINT('Ctrl Pts',(-19.1823089291523,-42.2783641614414,
124.604517413265)) ;
#101307 = CARTESIAN_POINT('Ctrl Pts',(-19.4611777277375,-42.2916383970302,
124.616769084087)) ;
#101308 = CARTESIAN_POINT('Ctrl Pts',(-19.6705412325652,-42.3016848144864,
124.589154104494)) ;
#101309 = CARTESIAN_POINT('Ctrl Pts',(-19.8680187765509,-42.3115300397057,
124.527075376806)) ;
#101310 = CARTESIAN_POINT('Ctrl Pts',(-20.1170180200422,-42.3248650107451,
124.398426185164)) ;
#101311 = CARTESIAN_POINT('Ctrl Pts',(-20.377792967121,-42.3414478675377,
124.160899138389)) ;
#101312 = CARTESIAN_POINT('Ctrl Pts',(-20.5424084728688,-42.3580908698871,
123.847785440929)) ;
#101313 = CARTESIAN_POINT('Ctrl Pts',(-20.6040494518553,-42.3713346009188,
123.576174969666)) ;
#101314 = CARTESIAN_POINT('Ctrl Pts',(-20.6143195456336,-42.3813889955934,
123.365096000372)) ;
#101315 = CARTESIAN_POINT('Ctrl Pts',(-20.5886046568097,-42.3912300569819,
123.159770541388)) ;
#101316 = CARTESIAN_POINT('Ctrl Pts',(-20.5264528337274,-42.4012962813384,
122.957516958445)) ;
#101317 = CARTESIAN_POINT('Ctrl Pts',(-20.4318168341843,-42.4111768942581,
122.772567402647)) ;
#101318 = CARTESIAN_POINT('Ctrl Pts',(-20.3054350952454,-42.4211701874177,
122.604783505865)) ;
#101319 = CARTESIAN_POINT('Ctrl Pts',(-20.1524930059633,-42.4311211956413,
122.461991985409)) ;
#101320 = CARTESIAN_POINT('Ctrl Pts',(-19.9753246827111,-42.4411697100033,
122.346976382411)) ;
#101321 = CARTESIAN_POINT('Ctrl Pts',(-19.7849352703812,-42.451011216066,
122.26593658494)) ;
#101322 = CARTESIAN_POINT('Ctrl Pts',(-19.5805701272462,-42.4609968686957,
122.218064985876)) ;
#101323 = CARTESIAN_POINT('Ctrl Pts',(-19.3719158783282,-42.4709358775406,
122.206376313551)) ;
#101324 = CARTESIAN_POINT('Ctrl Pts',(-19.1623315818401,-42.4809768028336,
122.231396662643)) ;
#101325 = CARTESIAN_POINT('Ctrl Pts',(-18.9632343406315,-42.4908671245885,
122.291405161718)) ;
#101326 = CARTESIAN_POINT('Ctrl Pts',(-18.7754899005803,-42.5008630979219,
122.385779465836)) ;
#101327 = CARTESIAN_POINT('Ctrl Pts',(-18.6080417409368,-42.510794497504,
122.510510577482)) ;
#101328 = CARTESIAN_POINT('Ctrl Pts',(-18.4635068962713,-42.520800037981,
122.663351585111)) ;
#101329 = CARTESIAN_POINT('Ctrl Pts',(-18.3477206660267,-42.5308330219123,
122.839646199405)) ;
#101330 = CARTESIAN_POINT('Ctrl Pts',(-18.2654323586817,-42.5406886527391,
123.029819179037)) ;
#101331 = CARTESIAN_POINT('Ctrl Pts',(-18.2164610131023,-42.5506880549323,
123.234217479617)) ;
#101332 = CARTESIAN_POINT('Ctrl Pts',(-18.2036137356792,-42.5605825242934,
123.441872039684)) ;
#101333 = CARTESIAN_POINT('Ctrl Pts',(-18.2274704080538,-42.5706456384576,
123.65204444723)) ;
#101334 = CARTESIAN_POINT('Ctrl Pts',(-18.2859262888241,-42.580485284174,
123.850509106412)) ;
#101335 = CARTESIAN_POINT('Ctrl Pts',(-18.3797751440215,-42.5905484517297,
124.040081083598)) ;
#101336 = CARTESIAN_POINT('Ctrl Pts',(-18.5031830504766,-42.6004427075246,
124.207555003253)) ;
#101337 = CARTESIAN_POINT('Ctrl Pts',(-18.6540904487499,-42.6103844859843,
124.352124377964)) ;
#101338 = CARTESIAN_POINT('Ctrl Pts',(-18.828874671857,-42.6203871788145,
124.469099558466)) ;
#101339 = CARTESIAN_POINT('Ctrl Pts',(-19.0220120735841,-42.6304212007683,
124.55390604498)) ;
#101340 = CARTESIAN_POINT('Ctrl Pts',(-19.2230780744629,-42.6402689918573,
124.6032744046)) ;
#101341 = CARTESIAN_POINT('Ctrl Pts',(-19.4324117143736,-42.6502505164063,
124.617627506494)) ;
#101342 = CARTESIAN_POINT('Ctrl Pts',(-19.6404040401297,-42.6601997398973,
124.595453201123)) ;
#101343 = CARTESIAN_POINT('Ctrl Pts',(-19.842448721353,-42.6701973961138,
124.537470809679)) ;
#101344 = CARTESIAN_POINT('Ctrl Pts',(-20.0319545510749,-42.6802376091689,
124.444544632507)) ;
#101345 = CARTESIAN_POINT('Ctrl Pts',(-20.1991303061263,-42.6900656564452,
124.323105381424)) ;
#101346 = CARTESIAN_POINT('Ctrl Pts',(-20.3462067267429,-42.7001200034775,
124.171307391296)) ;
#101347 = CARTESIAN_POINT('Ctrl Pts',(-20.4630752591194,-42.7100611398061,
123.998036466924)) ;
#101348 = CARTESIAN_POINT('Ctrl Pts',(-20.548356116802,-42.7199653728858,
123.808079119308)) ;
#101349 = CARTESIAN_POINT('Ctrl Pts',(-20.5999588950503,-42.7300120697294,
123.603285104442)) ;
#101350 = CARTESIAN_POINT('Ctrl Pts',(-20.6151816987034,-42.7399076210097,
123.395773544516)) ;
#101351 = CARTESIAN_POINT('Ctrl Pts',(-20.593794965009,-42.7499696988492,
123.185351124598)) ;
#101352 = CARTESIAN_POINT('Ctrl Pts',(-20.5375522517553,-42.7598124079452,
122.986192494632)) ;
#101353 = CARTESIAN_POINT('Ctrl Pts',(-20.4467001710193,-42.7698031401837,
122.796851434156)) ;
#101354 = CARTESIAN_POINT('Ctrl Pts',(-20.3250709421059,-42.7797311654124,
122.627221618873)) ;
#101355 = CARTESIAN_POINT('Ctrl Pts',(-20.1751865622208,-42.789719312063,
122.480152717807)) ;
#101356 = CARTESIAN_POINT('Ctrl Pts',(-20.0010496382006,-42.799754329903,
122.361052243801)) ;
#101357 = CARTESIAN_POINT('Ctrl Pts',(-19.8122379060998,-42.8096191270081,
122.275279706189)) ;
#101358 = CARTESIAN_POINT('Ctrl Pts',(-19.6095891946961,-42.8195798593643,
122.222493574637)) ;
#101359 = CARTESIAN_POINT('Ctrl Pts',(-19.3993145661506,-42.8296133217613,
122.20592601638)) ;
#101360 = CARTESIAN_POINT('Ctrl Pts',(-19.1923870950452,-42.8394988559727,
122.225479644873)) ;
#101361 = CARTESIAN_POINT('Ctrl Pts',(-18.9884138375484,-42.8495636966527,
122.281660892028)) ;
#101362 = CARTESIAN_POINT('Ctrl Pts',(-18.8013313790315,-42.8594118283815,
122.370385298187)) ;
#101363 = CARTESIAN_POINT('Ctrl Pts',(-18.6291240463363,-42.8694393253717,
122.491969978467)) ;
#101364 = CARTESIAN_POINT('Ctrl Pts',(-18.4810143551981,-42.8794677774167,
122.642027857309)) ;
#101365 = CARTESIAN_POINT('Ctrl Pts',(-18.3630867033842,-42.8893130439808,
122.812110783413)) ;
#101366 = CARTESIAN_POINT('Ctrl Pts',(-18.2746848266607,-42.8993037169218,
123.002642529112)) ;
#101367 = CARTESIAN_POINT('Ctrl Pts',(-18.2209096512844,-42.9093415990102,
123.206701699249)) ;
#101368 = CARTESIAN_POINT('Ctrl Pts',(-18.2033597632723,-42.9191859694499,
123.412923603604)) ;
#101369 = CARTESIAN_POINT('Ctrl Pts',(-18.2217313870291,-42.9291707968453,
123.622002009766)) ;
#101370 = CARTESIAN_POINT('Ctrl Pts',(-18.275804649098,-42.9391102422506,
123.823874103542)) ;
#101371 = CARTESIAN_POINT('Ctrl Pts',(-18.3650343553044,-42.9491502465365,
124.015135280682)) ;
#101372 = CARTESIAN_POINT('Ctrl Pts',(-18.4841828341972,-42.9590373557221,
124.185483133562)) ;
#101373 = CARTESIAN_POINT('Ctrl Pts',(-18.6325539890873,-42.9690374156246,
124.334379898025)) ;
#101374 = CARTESIAN_POINT('Ctrl Pts',(-18.8030555432684,-42.9789548315393,
124.454437551852)) ;
#101375 = CARTESIAN_POINT('Ctrl Pts',(-18.9942434246226,-42.9890016462801,
124.544141433821)) ;
#101376 = CARTESIAN_POINT('Ctrl Pts',(-19.1946308818379,-42.9988771234767,
124.598568577232)) ;
#101377 = CARTESIAN_POINT('Ctrl Pts',(-19.4051266336012,-43.008933219198,
124.617829207835)) ;
#101378 = CARTESIAN_POINT('Ctrl Pts',(-19.6124372769649,-43.018826381213,
124.600604753597)) ;
#101379 = CARTESIAN_POINT('Ctrl Pts',(-19.8169977549622,-43.0288886172357,
124.546818615759)) ;
#101380 = CARTESIAN_POINT('Ctrl Pts',(-20.0049933054048,-43.0387330828646,
124.4602510627)) ;
#101381 = CARTESIAN_POINT('Ctrl Pts',(-20.1775205762832,-43.0486931755687,
124.341599696211)) ;
#101382 = CARTESIAN_POINT('Ctrl Pts',(-20.3277014361496,-43.0587314645498,
124.193350158281)) ;
#101383 = CARTESIAN_POINT('Ctrl Pts',(-20.4482019462463,-43.068604787656,
124.024302160045)) ;
#101384 = CARTESIAN_POINT('Ctrl Pts',(-20.5392351931087,-43.0786779717411,
123.833143556949)) ;
#101385 = CARTESIAN_POINT('Ctrl Pts',(-20.594560088588,-43.088498484029,123.634190004681)) ;
#101386 = CARTESIAN_POINT('Ctrl Pts',(-20.6152165701404,-43.0985764801448,
123.423378076302)) ;
#101387 = CARTESIAN_POINT('Ctrl Pts',(-20.5993584627975,-43.1084305551281,
123.216774885685)) ;
#101388 = CARTESIAN_POINT('Ctrl Pts',(-20.5470175733516,-43.1184944367118,
123.011818446741)) ;
#101389 = CARTESIAN_POINT('Ctrl Pts',(-20.4613810725473,-43.1283778626855,
122.82246705492)) ;
#101390 = CARTESIAN_POINT('Ctrl Pts',(-20.3430959724629,-43.1383784666066,
122.648697702157)) ;
#101391 = CARTESIAN_POINT('Ctrl Pts',(-20.1976636032341,-43.1482982509444,
122.499177532182)) ;
#101392 = CARTESIAN_POINT('Ctrl Pts',(-20.0263331256241,-43.1583456013013,
122.375694704454)) ;
#101393 = CARTESIAN_POINT('Ctrl Pts',(-19.8394215696688,-43.1682229435356,
122.285136337893)) ;
#101394 = CARTESIAN_POINT('Ctrl Pts',(-19.6358073187035,-43.1782928246102,
122.22733809939)) ;
#101395 = CARTESIAN_POINT('Ctrl Pts',(-19.4302162364731,-43.1881225298119,
122.206062547646)) ;
#101396 = CARTESIAN_POINT('Ctrl Pts',(-19.2191370000731,-43.1981891909783,
122.220875550628)) ;
#101397 = CARTESIAN_POINT('Ctrl Pts',(-19.0174084879043,-43.2080794128456,
122.271357815421)) ;
#101398 = CARTESIAN_POINT('Ctrl Pts',(-18.8253989818481,-43.2180715889558,
122.356536946084)) ;
#101399 = CARTESIAN_POINT('Ctrl Pts',(-18.6517135764016,-43.2280344190684,
122.473586106999)) ;
#101400 = CARTESIAN_POINT('Ctrl Pts',(-18.5014927134878,-43.2379386314687,
122.617793307873)) ;
#101401 = CARTESIAN_POINT('Ctrl Pts',(-18.3768296284871,-43.2479993455566,
122.788624087561)) ;
#101402 = CARTESIAN_POINT('Ctrl Pts',(-18.2854888105193,-43.2578388485394,
122.974258184958)) ;
#101403 = CARTESIAN_POINT('Ctrl Pts',(-18.2262491361792,-43.2679049871058,
123.177384236377)) ;
#101404 = CARTESIAN_POINT('Ctrl Pts',(-18.2036698015768,-43.2777875015918,
123.38394629601)) ;
#101405 = CARTESIAN_POINT('Ctrl Pts',(-18.217034409601,-43.2877798009473,
123.593558164446)) ;
#101406 = CARTESIAN_POINT('Ctrl Pts',(-18.2663606242069,-43.2977328679007,
123.796938078468)) ;
#101407 = CARTESIAN_POINT('Ctrl Pts',(-18.3510009441216,-43.307767576106,
123.990158103154)) ;
#101408 = CARTESIAN_POINT('Ctrl Pts',(-18.4660870165131,-43.3176557970101,
124.163290942232)) ;
#101409 = CARTESIAN_POINT('Ctrl Pts',(-18.6107602261149,-43.3276502200406,
124.315648485529)) ;
#101410 = CARTESIAN_POINT('Ctrl Pts',(-18.778919336589,-43.3375955594868,
124.439898554788)) ;
#101411 = CARTESIAN_POINT('Ctrl Pts',(-18.9659524526579,-43.3475429040981,
124.533471648758)) ;
#101412 = CARTESIAN_POINT('Ctrl Pts',(-19.1684697685578,-43.3575907995091,
124.593517733059)) ;
#101413 = CARTESIAN_POINT('Ctrl Pts',(-19.3741416564516,-43.3674384449884,
124.617185922135)) ;
#101414 = CARTESIAN_POINT('Ctrl Pts',(-19.5832202350008,-43.3774001589024,
124.605295312467)) ;
#101415 = CARTESIAN_POINT('Ctrl Pts',(-19.788388952215,-43.3874287831934,
124.556694677284)) ;
#101416 = CARTESIAN_POINT('Ctrl Pts',(-19.9797240892769,-43.3973391438501,
124.474263447552)) ;
#101417 = CARTESIAN_POINT('Ctrl Pts',(-20.1545850346626,-43.4072738424234,
124.360032517299)) ;
#101418 = CARTESIAN_POINT('Ctrl Pts',(-20.308442626863,-43.4173156672776,
124.21549439868)) ;
#101419 = CARTESIAN_POINT('Ctrl Pts',(-20.4330508635004,-43.427200241022,
124.049170635153)) ;
#101420 = CARTESIAN_POINT('Ctrl Pts',(-20.5282031141221,-43.4372020903851,
123.861693390623)) ;
#101421 = CARTESIAN_POINT('Ctrl Pts',(-20.5890161547966,-43.4471213919592,
123.662193934249)) ;
#101422 = CARTESIAN_POINT('Ctrl Pts',(-20.6145826712421,-43.4571655003045,
123.452605899371)) ;
#101423 = CARTESIAN_POINT('Ctrl Pts',(-20.6036090436324,-43.4670499237467,
123.245085013458)) ;
#101424 = CARTESIAN_POINT('Ctrl Pts',(-20.556600935761,-43.4770662856562,
123.039815548646)) ;
#101425 = CARTESIAN_POINT('Ctrl Pts',(-20.4739955072434,-43.4871029411616,
122.84566761688)) ;
#101426 = CARTESIAN_POINT('Ctrl Pts',(-20.361755152185,-43.4969330713509,
122.672114426095)) ;
#101427 = CARTESIAN_POINT('Ctrl Pts',(-20.2176634615263,-43.5070091244408,
122.516896559099)) ;
#101428 = CARTESIAN_POINT('Ctrl Pts',(-20.0525626661233,-43.5168613536266,
122.391754844818)) ;
#101429 = CARTESIAN_POINT('Ctrl Pts',(-19.864257399952,-43.5269345614259,
122.294937488847)) ;
#101430 = CARTESIAN_POINT('Ctrl Pts',(-19.6665927108449,-43.5367760727773,
122.23376896009)) ;
#101431 = CARTESIAN_POINT('Ctrl Pts',(-19.458938854123,-43.5467370108148,
122.206756445944)) ;
#101432 = CARTESIAN_POINT('Ctrl Pts',(-19.2481526770492,-43.5567748727398,
122.216705351052)) ;
#101433 = CARTESIAN_POINT('Ctrl Pts',(-19.0455360039206,-43.5666490587369,
122.261974513877)) ;
#101434 = CARTESIAN_POINT('Ctrl Pts',(-18.8501121593131,-43.5767192183147,
122.343316567473)) ;
#101435 = CARTESIAN_POINT('Ctrl Pts',(-18.6758905511319,-43.5865509657406,
122.454570971373)) ;
#101436 = CARTESIAN_POINT('Ctrl Pts',(-18.5201203431998,-43.5965870458119,
122.59686618946)) ;
#101437 = CARTESIAN_POINT('Ctrl Pts',(-18.3920760739767,-43.6066040926644,
122.764070852916)) ;
#101438 = CARTESIAN_POINT('Ctrl Pts',(-18.295971375366,-43.616486350831,122.948265806103)) ;
#101439 = CARTESIAN_POINT('Ctrl Pts',(-18.232417764736,-43.6264740336273,
123.148366425561)) ;
#101440 = CARTESIAN_POINT('Ctrl Pts',(-18.2045129710883,-43.6364206903441,
123.355638686235)) ;
#101441 = CARTESIAN_POINT('Ctrl Pts',(-18.2133309405117,-43.6464777484242,
123.566862574915)) ;
#101442 = CARTESIAN_POINT('Ctrl Pts',(-18.2573403317098,-43.6562959279737,
123.768536219661)) ;
#101443 = CARTESIAN_POINT('Ctrl Pts',(-18.3369007875818,-43.6663318624127,
123.963941924547)) ;
#101444 = CARTESIAN_POINT('Ctrl Pts',(-18.4495740874589,-43.6763565168417,
124.142052906167)) ;
#101445 = CARTESIAN_POINT('Ctrl Pts',(-18.5886758420393,-43.6862085364212,
124.295515615773)) ;
#101446 = CARTESIAN_POINT('Ctrl Pts',(-18.7543989737947,-43.6961994501361,
124.424520494289)) ;
#101447 = CARTESIAN_POINT('Ctrl Pts',(-18.9386300461711,-43.7061174389757,
124.522216831096)) ;
#101448 = CARTESIAN_POINT('Ctrl Pts',(-19.1391738996227,-43.7161455497065,
124.587189241237)) ;
#101449 = CARTESIAN_POINT('Ctrl Pts',(-19.3449855893368,-43.7260307476149,
124.616027510244)) ;
#101450 = CARTESIAN_POINT('Ctrl Pts',(-19.554884068964,-43.7360200228829,
124.609127951976)) ;
#101451 = CARTESIAN_POINT('Ctrl Pts',(-19.7613652618478,-43.7460614810524,
124.5652171775)) ;
#101452 = CARTESIAN_POINT('Ctrl Pts',(-19.9531454614378,-43.7558929448407,
124.488123636082)) ;
#101453 = CARTESIAN_POINT('Ctrl Pts',(-20.1319421287636,-43.7658978771446,
124.37738885238)) ;
#101454 = CARTESIAN_POINT('Ctrl Pts',(-20.2884737443949,-43.7758842410393,
124.237424747763)) ;
#101455 = CARTESIAN_POINT('Ctrl Pts',(-20.4187237694993,-43.7859138699252,
124.071633938485)) ;
#101456 = CARTESIAN_POINT('Ctrl Pts',(-20.5169317589502,-43.7957890920336,
123.888700540743)) ;
#101457 = CARTESIAN_POINT('Ctrl Pts',(-20.5829335070661,-43.8057903044307,
123.689106263425)) ;
#101458 = CARTESIAN_POINT('Ctrl Pts',(-20.61320125235,-43.8156988836662,123.482970484591)) ;
#101459 = CARTESIAN_POINT('Ctrl Pts',(-20.6070669616977,-43.8257537362222,
123.271709055885)) ;
#101460 = CARTESIAN_POINT('Ctrl Pts',(-20.5653971841227,-43.835612318497,
123.06864564445)) ;
#101461 = CARTESIAN_POINT('Ctrl Pts',(-20.4876247624856,-43.8456804479396,
122.871820933791)) ;
#101462 = CARTESIAN_POINT('Ctrl Pts',(-20.3791588454062,-43.8555359196287,
122.695267061936)) ;
#101463 = CARTESIAN_POINT('Ctrl Pts',(-20.2402289792593,-43.865530768015,
122.537636599982)) ;
#101464 = CARTESIAN_POINT('Ctrl Pts',(-20.0751488368937,-43.8755620647995,
122.406393652979)) ;
#101465 = CARTESIAN_POINT('Ctrl Pts',(-19.8929883767883,-43.8854286010096,
122.307167896333)) ;
#101466 = CARTESIAN_POINT('Ctrl Pts',(-19.6940946243766,-43.8954160239704,
122.239956904999)) ;
#101467 = CARTESIAN_POINT('Ctrl Pts',(-19.4873991386008,-43.9053609629902,
122.208320984455)) ;
#101468 = CARTESIAN_POINT('Ctrl Pts',(-19.276294832243,-43.9154058488502,
122.213202322377)) ;
#101469 = CARTESIAN_POINT('Ctrl Pts',(-19.0728380877924,-43.9252743839364,
122.25382983133)) ;
#101470 = CARTESIAN_POINT('Ctrl Pts',(-18.877421866711,-43.9352402519431,
122.329360626703)) ;
#101471 = CARTESIAN_POINT('Ctrl Pts',(-18.6971695759809,-43.9452628993956,
122.438507166562)) ;
#101472 = CARTESIAN_POINT('Ctrl Pts',(-18.5401540064754,-43.9551865384032,
122.575862283478)) ;
#101473 = CARTESIAN_POINT('Ctrl Pts',(-18.4087164928429,-43.9651292634089,
122.738409603941)) ;
#101474 = CARTESIAN_POINT('Ctrl Pts',(-18.3066850944512,-43.9751748694608,
122.923303955363)) ;
#101475 = CARTESIAN_POINT('Ctrl Pts',(-18.239335869185,-43.9850362919819,
123.119396349214)) ;
#101476 = CARTESIAN_POINT('Ctrl Pts',(-18.2062782408327,-43.9950298604311,
123.326845245392)) ;
#101477 = CARTESIAN_POINT('Ctrl Pts',(-18.2096114898177,-44.0049553311864,
123.535514072462)) ;
#101478 = CARTESIAN_POINT('Ctrl Pts',(-18.2495123854255,-44.0149830051423,
123.742490533073)) ;
#101479 = CARTESIAN_POINT('Ctrl Pts',(-18.3235214895332,-44.0248701831839,
123.936757715858)) ;
#101480 = CARTESIAN_POINT('Ctrl Pts',(-18.4315052983995,-44.0348985625521,
124.117800342499)) ;
#101481 = CARTESIAN_POINT('Ctrl Pts',(-18.5673876041931,-44.0447928052736,
124.275321960372)) ;
#101482 = CARTESIAN_POINT('Ctrl Pts',(-18.7847153693869,-44.0581457219245,
124.452998723631)) ;
#101483 = CARTESIAN_POINT('Ctrl Pts',(-19.0405841604005,-44.0713482396712,
124.568621998419)) ;
#101484 = CARTESIAN_POINT('Ctrl Pts',(-19.3175541949895,-44.0847041449522,
124.614316024361)) ;
#101485 = CARTESIAN_POINT('Ctrl Pts',(-19.5256380102988,-44.09460079359,124.612215853843)) ;
#101486 = CARTESIAN_POINT('Ctrl Pts',(-19.7332848983947,-44.1046489316425,
124.573507791128)) ;
#101487 = CARTESIAN_POINT('Ctrl Pts',(-19.9279877050675,-44.1145398918202,
124.500478296984)) ;
#101488 = CARTESIAN_POINT('Ctrl Pts',(-20.1091624018296,-44.124532727697,
124.394118416426)) ;
#101489 = CARTESIAN_POINT('Ctrl Pts',(-20.2695300676021,-44.1345718226986,
124.256926550126)) ;
#101490 = CARTESIAN_POINT('Ctrl Pts',(-20.4013372357258,-44.1444091785497,
124.097532277109)) ;
#101491 = CARTESIAN_POINT('Ctrl Pts',(-20.5404948760595,-44.1578021264805,
123.852796117279)) ;
#101492 = CARTESIAN_POINT('Ctrl Pts',(-20.6114146822472,-44.1709688029074,
123.581864138819)) ;
#101493 = CARTESIAN_POINT('Ctrl Pts',(-20.6101144909671,-44.1843535843142,
123.300568294989)) ;
#101494 = CARTESIAN_POINT('Ctrl Pts',(-20.5732481523805,-44.194215366958,
123.096503125407)) ;
#101495 = CARTESIAN_POINT('Ctrl Pts',(-20.5008589113301,-44.2042145149111,
122.899193683565)) ;
#101496 = CARTESIAN_POINT('Ctrl Pts',(-20.396449056212,-44.2141173075282,
122.719027239465)) ;
#101497 = CARTESIAN_POINT('Ctrl Pts',(-20.2603777954349,-44.2241668874191,
122.557479701202)) ;
#101498 = CARTESIAN_POINT('Ctrl Pts',(-20.0479296377058,-44.2373539612286,
122.379174613278)) ;
#101499 = CARTESIAN_POINT('Ctrl Pts',(-19.7251921408927,-44.2541067511998,
122.228850637469)) ;
#101500 = CARTESIAN_POINT('Ctrl Pts',(-19.3757306114418,-44.2705954032945,
122.198236067247)) ;
#101501 = CARTESIAN_POINT('Ctrl Pts',(-19.0992071105754,-44.2839522294779,
122.246385612878)) ;
#101502 = CARTESIAN_POINT('Ctrl Pts',(-18.903461552723,-44.2938486143558,
122.317045129646)) ;
#101503 = CARTESIAN_POINT('Ctrl Pts',(-18.7209977481743,-44.3038551288763,
122.421622159282)) ;
#101504 = CARTESIAN_POINT('Ctrl Pts',(-18.50748350798,-44.3170452523927,122.598733415765)) ;
#101505 = CARTESIAN_POINT('Ctrl Pts',(-18.3017387192024,-44.3338118135422,
122.889701096753)) ;
#101506 = CARTESIAN_POINT('Ctrl Pts',(-18.1906974855845,-44.3535963022503,
123.295581127979)) ;
#101507 = CARTESIAN_POINT('Ctrl Pts',(-18.2237801123301,-44.3735417498468,
123.718275709203)) ;
#101508 = CARTESIAN_POINT('Ctrl Pts',(-18.3992375725797,-44.3934534120027,
124.1035934683)) ;
#101509 = CARTESIAN_POINT('Ctrl Pts',(-18.6947326457953,-44.4133456040216,
124.406305792813)) ;
#101510 = CARTESIAN_POINT('Ctrl Pts',(-19.0788065290729,-44.4333867345762,
124.590755911003)) ;
#101511 = CARTESIAN_POINT('Ctrl Pts',(-19.4981950361923,-44.4532050691918,
124.63283913726)) ;
#101512 = CARTESIAN_POINT('Ctrl Pts',(-19.9098770739331,-44.4731776344114,
124.529198613639)) ;
#101513 = CARTESIAN_POINT('Ctrl Pts',(-20.260324726777,-44.493066850583,124.292206941175)) ;
#101514 = CARTESIAN_POINT('Ctrl Pts',(-20.5101502059356,-44.5130904249057,
123.947585173963)) ;
#101515 = CARTESIAN_POINT('Ctrl Pts',(-20.6263965337571,-44.5328875879939,
123.542934630654)) ;
#101516 = CARTESIAN_POINT('Ctrl Pts',(-20.5983673710328,-44.5528530818177,
123.119430015915)) ;
#101517 = CARTESIAN_POINT('Ctrl Pts',(-20.4270411722174,-44.5728067895591,
122.731166665459)) ;
#101518 = CARTESIAN_POINT('Ctrl Pts',(-20.1343452039405,-44.5927141662857,
122.425521895148)) ;
#101519 = CARTESIAN_POINT('Ctrl Pts',(-19.7563216296652,-44.6125663778343,
122.237539802008)) ;
#101520 = CARTESIAN_POINT('Ctrl Pts',(-19.332230289126,-44.63263876478,122.189737949116)) ;
#101521 = CARTESIAN_POINT('Ctrl Pts',(-18.9222423968957,-44.6524766344203,
122.288907530951)) ;
#101522 = CARTESIAN_POINT('Ctrl Pts',(-18.5694752445574,-44.6723272889734,
122.520649900601)) ;
#101523 = CARTESIAN_POINT('Ctrl Pts',(-18.3149237858139,-44.6923792233138,
122.862638202691)) ;
#101524 = CARTESIAN_POINT('Ctrl Pts',(-18.19370989295,-44.7122124108799,123.26665041854)) ;
#101525 = CARTESIAN_POINT('Ctrl Pts',(-18.2169009913594,-44.7321416231106,
123.689607385254)) ;
#101526 = CARTESIAN_POINT('Ctrl Pts',(-18.3823273711519,-44.752026588325,
124.078886422621)) ;
#101527 = CARTESIAN_POINT('Ctrl Pts',(-18.6737118515768,-44.7721003294696,
124.390652078349)) ;
#101528 = CARTESIAN_POINT('Ctrl Pts',(-19.0487927727222,-44.79189351125,124.581678914029)) ;
#101529 = CARTESIAN_POINT('Ctrl Pts',(-19.4698622335801,-44.8118562192527,
124.634952561121)) ;
#101530 = CARTESIAN_POINT('Ctrl Pts',(-19.8840681821259,-44.8318391709951,
124.540233175461)) ;
#101531 = CARTESIAN_POINT('Ctrl Pts',(-20.2384850227702,-44.8516497907673,
124.312522302886)) ;
#101532 = CARTESIAN_POINT('Ctrl Pts',(-20.4964727377313,-44.8716335068002,
123.975018736943)) ;
#101533 = CARTESIAN_POINT('Ctrl Pts',(-20.623144683974,-44.8915149706975,
123.571598663289)) ;
#101534 = CARTESIAN_POINT('Ctrl Pts',(-20.6047845721142,-44.9114703005419,
123.147777281056)) ;
#101535 = CARTESIAN_POINT('Ctrl Pts',(-20.4437733265851,-44.9313457613473,
122.756972727048)) ;
#101536 = CARTESIAN_POINT('Ctrl Pts',(-20.1577714535255,-44.9513300813989,
122.44277538795)) ;
#101537 = CARTESIAN_POINT('Ctrl Pts',(-19.7825365441427,-44.9712581141885,
122.245734881039)) ;
#101538 = CARTESIAN_POINT('Ctrl Pts',(-19.4327218144103,-44.9878668761283,
122.198048978152)) ;
#101539 = CARTESIAN_POINT('Ctrl Pts',(-19.1575807895706,-45.0010545148184,
122.232475347837)) ;
#101540 = CARTESIAN_POINT('Ctrl Pts',(-18.9568221140581,-45.0110409491785,
122.293848063992)) ;
#101541 = CARTESIAN_POINT('Ctrl Pts',(-18.7694045437532,-45.0210503231378,
122.389576682981)) ;
#101542 = CARTESIAN_POINT('Ctrl Pts',(-18.5463500655104,-45.0343403567031,
122.557757572776)) ;
#101543 = CARTESIAN_POINT('Ctrl Pts',(-18.3288732235893,-45.0509343443656,
122.83570039441)) ;
#101544 = CARTESIAN_POINT('Ctrl Pts',(-18.2191010454071,-45.0675665996411,
123.171813138053)) ;
#101545 = CARTESIAN_POINT('Ctrl Pts',(-18.2039892476202,-45.080808983309,
123.449835817539)) ;
#101546 = CARTESIAN_POINT('Ctrl Pts',(-18.228353888803,-45.0907231915364,
123.656837027737)) ;
#101547 = CARTESIAN_POINT('Ctrl Pts',(-18.2893746717869,-45.1007798308081,
123.859247365512)) ;
#101548 = CARTESIAN_POINT('Ctrl Pts',(-18.3824077852439,-45.1106256372282,
124.044169153839)) ;
#101549 = CARTESIAN_POINT('Ctrl Pts',(-18.5083407942708,-45.1206706368614,
124.213687382027)) ;
#101550 = CARTESIAN_POINT('Ctrl Pts',(-18.7114733830071,-45.1339516592341,
124.405166972011)) ;
#101551 = CARTESIAN_POINT('Ctrl Pts',(-18.9580691583972,-45.1471491057588,
124.539151464056)) ;
#101552 = CARTESIAN_POINT('Ctrl Pts',(-19.2323658927779,-45.1605634035657,
124.604770439272)) ;
#101553 = CARTESIAN_POINT('Ctrl Pts',(-19.4388388395577,-45.1704024689685,
124.617358316742)) ;
#101554 = CARTESIAN_POINT('Ctrl Pts',(-19.6474045446388,-45.1803856752462,
124.594113920996)) ;
#101555 = CARTESIAN_POINT('Ctrl Pts',(-19.8481328145844,-45.190336910159,
124.535120393601)) ;
#101556 = CARTESIAN_POINT('Ctrl Pts',(-20.0366173779202,-45.2003379098606,
124.441933687023)) ;
#101557 = CARTESIAN_POINT('Ctrl Pts',(-20.2063667529885,-45.2103692556479,
124.316798072063)) ;
#101558 = CARTESIAN_POINT('Ctrl Pts',(-20.3494471671813,-45.220223020353,
124.166984017508)) ;
#101559 = CARTESIAN_POINT('Ctrl Pts',(-20.4661047074202,-45.2301936740213,
123.992857716921)) ;
#101560 = CARTESIAN_POINT('Ctrl Pts',(-20.5509965521289,-45.2401909176785,
123.800556778841)) ;
#101561 = CARTESIAN_POINT('Ctrl Pts',(-20.6011158907681,-45.2502243736227,
123.595680569379)) ;
#101562 = CARTESIAN_POINT('Ctrl Pts',(-20.6149939259179,-45.2600798779231,
123.38893191624)) ;
#101563 = CARTESIAN_POINT('Ctrl Pts',(-20.592723368005,-45.2700793142092,
123.179932810256)) ;
#101564 = CARTESIAN_POINT('Ctrl Pts',(-20.5353204911659,-45.2799737737251,
122.979956620306)) ;
#101565 = CARTESIAN_POINT('Ctrl Pts',(-20.4424886941461,-45.2900368931767,
122.789893973153)) ;
#101566 = CARTESIAN_POINT('Ctrl Pts',(-20.3209726732534,-45.2998765275887,
122.622445042168)) ;
#101567 = CARTESIAN_POINT('Ctrl Pts',(-20.1690810600226,-45.3099397350745,
122.475223235141)) ;
#101568 = CARTESIAN_POINT('Ctrl Pts',(-19.996736286996,-45.3198338424537,
122.358718091964)) ;
#101569 = CARTESIAN_POINT('Ctrl Pts',(-19.8061310069513,-45.3297761746461,
122.273004843829)) ;
#101570 = CARTESIAN_POINT('Ctrl Pts',(-19.6023161130054,-45.3397768009611,
122.221272581274)) ;
#101571 = CARTESIAN_POINT('Ctrl Pts',(-19.391776175051,-45.349818535243,122.206047936607)) ;
#101572 = CARTESIAN_POINT('Ctrl Pts',(-19.1862337808466,-45.3596439611921,
122.226693352974)) ;
#101573 = CARTESIAN_POINT('Ctrl Pts',(-18.9826608086489,-45.3697007877197,
122.283722631723)) ;
#101574 = CARTESIAN_POINT('Ctrl Pts',(-18.7946377034752,-45.3796282208413,
122.374331131619)) ;
#101575 = CARTESIAN_POINT('Ctrl Pts',(-18.6244717487693,-45.3895782132475,
122.495999084926)) ;
#101576 = CARTESIAN_POINT('Ctrl Pts',(-18.4767502078557,-45.3996334143215,
122.64719008305)) ;
#101577 = CARTESIAN_POINT('Ctrl Pts',(-18.3599614373723,-45.4094556883738,
122.817505156019)) ;
#101578 = CARTESIAN_POINT('Ctrl Pts',(-18.2721558939033,-45.4195115823331,
123.009798452416)) ;
#101579 = CARTESIAN_POINT('Ctrl Pts',(-18.2200351253211,-45.4294523041782,
123.212188004326)) ;
#101580 = CARTESIAN_POINT('Ctrl Pts',(-18.2032568015075,-45.4393566482648,
123.419735077374)) ;
#101581 = CARTESIAN_POINT('Ctrl Pts',(-18.2231823776908,-45.4494033155643,
123.629987925787)) ;
#101582 = CARTESIAN_POINT('Ctrl Pts',(-18.2782983093062,-45.4592988740142,
123.830624493296)) ;
#101583 = CARTESIAN_POINT('Ctrl Pts',(-18.3688864957149,-45.4693609527189,
124.021749609544)) ;
#101584 = CARTESIAN_POINT('Ctrl Pts',(-18.4885492669216,-45.4792036511847,
124.190592884242)) ;
#101585 = CARTESIAN_POINT('Ctrl Pts',(-18.637539710938,-45.4891944250792,
124.338601747034)) ;
#101586 = CARTESIAN_POINT('Ctrl Pts',(-18.8089299984805,-45.4991222943141,
124.457728068309)) ;
#101587 = CARTESIAN_POINT('Ctrl Pts',(-18.9994081616876,-45.5091110232839,
124.546160479983)) ;
#101588 = CARTESIAN_POINT('Ctrl Pts',(-19.2034569753931,-45.5191504252677,
124.600067490616)) ;
#101589 = CARTESIAN_POINT('Ctrl Pts',(-19.4095796971761,-45.5289905930044,
124.61778415032)) ;
#101590 = CARTESIAN_POINT('Ctrl Pts',(-19.6200112689302,-45.5390388033789,
124.599364490398)) ;
#101591 = CARTESIAN_POINT('Ctrl Pts',(-19.8219223595933,-45.5489859736667,
124.544913463033)) ;
#101592 = CARTESIAN_POINT('Ctrl Pts',(-20.0108872609062,-45.5588968219218,
124.457119595475)) ;
#101593 = CARTESIAN_POINT('Ctrl Pts',(-20.1841161416152,-45.5689531495995,
124.335945853187)) ;
#101594 = CARTESIAN_POINT('Ctrl Pts',(-20.3307537109057,-45.5788035623681,
124.189705688813)) ;
#101595 = CARTESIAN_POINT('Ctrl Pts',(-20.4523163621318,-45.5888304482018,
124.017494615837)) ;
#101596 = CARTESIAN_POINT('Ctrl Pts',(-20.5416562762477,-45.5988590638326,
123.826515207453)) ;
#101597 = CARTESIAN_POINT('Ctrl Pts',(-20.5958480133212,-45.6087042872101,
123.62676985352)) ;
#101598 = CARTESIAN_POINT('Ctrl Pts',(-20.615373524796,-45.6186949693117,
123.417638284898)) ;
#101599 = CARTESIAN_POINT('Ctrl Pts',(-20.5977412666181,-45.6287328579441,
123.207350206846)) ;
#101600 = CARTESIAN_POINT('Ctrl Pts',(-20.5452503353904,-45.6385771930473,
123.007150530596)) ;
#101601 = CARTESIAN_POINT('Ctrl Pts',(-20.4579510736212,-45.6485621552448,
122.81628083334)) ;
#101602 = CARTESIAN_POINT('Ctrl Pts',(-20.339432406419,-45.6585010967782,
122.644161099599)) ;
#101603 = CARTESIAN_POINT('Ctrl Pts',(-20.1912978264243,-45.6685429817496,
122.493774999575)) ;
#101604 = CARTESIAN_POINT('Ctrl Pts',(-20.0220069616758,-45.6784295296579,
122.373155532441)) ;
#101605 = CARTESIAN_POINT('Ctrl Pts',(-19.8324818823404,-45.6884234551579,
122.282532585649)) ;
#101606 = CARTESIAN_POINT('Ctrl Pts',(-19.6312418898765,-45.6983595462843,
122.22640961651)) ;
#101607 = CARTESIAN_POINT('Ctrl Pts',(-19.4214195398771,-45.7083888152643,
122.205936892233)) ;
#101608 = CARTESIAN_POINT('Ctrl Pts',(-19.2142297342417,-45.7182711978236,
122.22170984425)) ;
#101609 = CARTESIAN_POINT('Ctrl Pts',(-19.009504307263,-45.7283237149114,
122.274021366341)) ;
#101610 = CARTESIAN_POINT('Ctrl Pts',(-18.8198982639339,-45.7382178357354,
122.35964528953)) ;
#101611 = CARTESIAN_POINT('Ctrl Pts',(-18.645147480968,-45.7482798151558,
122.47880170515)) ;
#101612 = CARTESIAN_POINT('Ctrl Pts',(-18.4969722121152,-45.7581243483847,
122.62330352564)) ;
#101613 = CARTESIAN_POINT('Ctrl Pts',(-18.3741142958036,-45.768084427291,
122.792860748407)) ;
#101614 = CARTESIAN_POINT('Ctrl Pts',(-18.2822203335632,-45.7781227038636,
122.982828343236)) ;
#101615 = CARTESIAN_POINT('Ctrl Pts',(-18.2252578386607,-45.7879960904014,
123.182460834267)) ;
#101616 = CARTESIAN_POINT('Ctrl Pts',(-18.2034592120958,-45.7980690331685,
123.39306039462)) ;
#101617 = CARTESIAN_POINT('Ctrl Pts',(-18.2179355062058,-45.8078904472968,
123.59906900645)) ;
#101618 = CARTESIAN_POINT('Ctrl Pts',(-18.2689853650501,-45.8179650773691,
123.804585766185)) ;
#101619 = CARTESIAN_POINT('Ctrl Pts',(-18.353274661512,-45.827831714686,123.994143637568)) ;
#101620 = CARTESIAN_POINT('Ctrl Pts',(-18.4705716953183,-45.8378552600578,
124.169195047555)) ;
#101621 = CARTESIAN_POINT('Ctrl Pts',(-18.6168958229205,-45.847881011575,
124.320918073927)) ;
#101622 = CARTESIAN_POINT('Ctrl Pts',(-18.7841910613387,-45.8577345985843,
124.44306586001)) ;
#101623 = CARTESIAN_POINT('Ctrl Pts',(-18.9722503411076,-45.8677115588123,
124.535960012033)) ;
#101624 = CARTESIAN_POINT('Ctrl Pts',(-19.1745594962506,-45.8777327018408,
124.594704103338)) ;
#101625 = CARTESIAN_POINT('Ctrl Pts',(-19.3810923793622,-45.8876153078607,
124.61753407363)) ;
#101626 = CARTESIAN_POINT('Ctrl Pts',(-19.5922833907373,-45.8976837784934,
124.603825647717)) ;
#101627 = CARTESIAN_POINT('Ctrl Pts',(-19.7931427540884,-45.9075138616771,
124.555060369971)) ;
#101628 = CARTESIAN_POINT('Ctrl Pts',(-19.9870854212737,-45.9175804213574,
124.47044576833)) ;
#101629 = CARTESIAN_POINT('Ctrl Pts',(-20.1602793483263,-45.9274706711867,
124.355350990646)) ;
#101630 = CARTESIAN_POINT('Ctrl Pts',(-20.3127002043108,-45.9374628369355,
124.210813834225)) ;
#101631 = CARTESIAN_POINT('Ctrl Pts',(-20.4371861889498,-45.9474256805316,
124.042378586664)) ;
#101632 = CARTESIAN_POINT('Ctrl Pts',(-20.5304707785403,-45.9573298493593,
123.856207376528)) ;
#101633 = CARTESIAN_POINT('Ctrl Pts',(-20.5907592046951,-45.9673907242537,
123.653499234199)) ;
#101634 = CARTESIAN_POINT('Ctrl Pts',(-20.6146961155578,-45.977229627583,
123.448011373335)) ;
#101635 = CARTESIAN_POINT('Ctrl Pts',(-20.6025149554058,-45.9872980039569,
123.236727574524)) ;
#101636 = CARTESIAN_POINT('Ctrl Pts',(-20.5546576917717,-45.9971786205896,
123.03456293301)) ;
#101637 = CARTESIAN_POINT('Ctrl Pts',(-20.471918396597,-46.0071697808186,
122.841533187963)) ;
#101638 = CARTESIAN_POINT('Ctrl Pts',(-20.3573523340051,-46.0171228542507,
122.666401412184)) ;
#101639 = CARTESIAN_POINT('Ctrl Pts',(-20.21290978771,-46.0271586898633,122.512636265793)) ;
#101640 = CARTESIAN_POINT('Ctrl Pts',(-20.0464766766351,-46.0370488165935,
122.387989822038)) ;
#101641 = CARTESIAN_POINT('Ctrl Pts',(-19.8591881806302,-46.0470409983628,
122.29287624258)) ;
#101642 = CARTESIAN_POINT('Ctrl Pts',(-19.6591289734033,-46.0569869383372,
122.232074376026)) ;
#101643 = CARTESIAN_POINT('Ctrl Pts',(-19.4515659859272,-46.0669341220967,
122.206507164421)) ;
#101644 = CARTESIAN_POINT('Ctrl Pts',(-19.2406311344762,-46.076982060387,
122.217713381224)) ;
#101645 = CARTESIAN_POINT('Ctrl Pts',(-19.0389014507755,-46.0868296952006,
122.264255625121)) ;
#101646 = CARTESIAN_POINT('Ctrl Pts',(-18.845864019977,-46.0967914088986,
122.345445458359)) ;
#101647 = CARTESIAN_POINT('Ctrl Pts',(-18.6687989532534,-46.1068200447197,
122.459919261407)) ;
#101648 = CARTESIAN_POINT('Ctrl Pts',(-18.5160937341406,-46.1167303594715,
122.601640319186)) ;
#101649 = CARTESIAN_POINT('Ctrl Pts',(-18.3895562982381,-46.1266652301342,
122.767816764546)) ;
#101650 = CARTESIAN_POINT('Ctrl Pts',(-18.2929570491633,-46.1367064125359,
122.955504659103)) ;
#101651 = CARTESIAN_POINT('Ctrl Pts',(-18.231205995606,-46.1465933840007,
123.15399394817)) ;
#101652 = CARTESIAN_POINT('Ctrl Pts',(-18.2042980741008,-46.1565928162633,
123.362456961711)) ;
#101653 = CARTESIAN_POINT('Ctrl Pts',(-18.2137796717895,-46.1665128815199,
123.570817245202)) ;
#101654 = CARTESIAN_POINT('Ctrl Pts',(-18.2597821350326,-46.1765497341041,
123.776736067537)) ;
#101655 = CARTESIAN_POINT('Ctrl Pts',(-18.3398482939461,-46.186462393444,
123.969140656716)) ;
#101656 = CARTESIAN_POINT('Ctrl Pts',(-18.4526152165977,-46.1964536053589,
124.146365147496)) ;
#101657 = CARTESIAN_POINT('Ctrl Pts',(-18.5954873608087,-46.2064952467621,
124.301757135188)) ;
#101658 = CARTESIAN_POINT('Ctrl Pts',(-18.7593348263988,-46.2163240409691,
124.427702905897)) ;
#101659 = CARTESIAN_POINT('Ctrl Pts',(-18.9470739163007,-46.2264004520904,
124.525741487184)) ;
#101660 = CARTESIAN_POINT('Ctrl Pts',(-19.144538672568,-46.2362525851328,
124.588397896251)) ;
#101661 = CARTESIAN_POINT('Ctrl Pts',(-19.3543893428707,-46.2463258194742,
124.616598890944)) ;
#101662 = CARTESIAN_POINT('Ctrl Pts',(-19.561126394964,-46.2561673208008,
124.608074076936)) ;
#101663 = CARTESIAN_POINT('Ctrl Pts',(-19.7658434933763,-46.2661282723956,
124.564019788485)) ;
#101664 = CARTESIAN_POINT('Ctrl Pts',(-19.9611394824393,-46.2761660901162,
124.484088757775)) ;
#101665 = CARTESIAN_POINT('Ctrl Pts',(-20.1369164873677,-46.2860404393733,
124.373605731644)) ;
#101666 = CARTESIAN_POINT('Ctrl Pts',(-20.2938331627906,-46.2961099901155,
124.231552761225)) ;
#101667 = CARTESIAN_POINT('Ctrl Pts',(-20.4207867457128,-46.3059440096241,
124.0683564569)) ;
#101668 = CARTESIAN_POINT('Ctrl Pts',(-20.5199207099598,-46.3159781642036,
123.882164631584)) ;
#101669 = CARTESIAN_POINT('Ctrl Pts',(-20.5846123031297,-46.3259940900261,
123.681769042482)) ;
#101670 = CARTESIAN_POINT('Ctrl Pts',(-20.6135083851793,-46.3358763452203,
123.476029208701)) ;
#101671 = CARTESIAN_POINT('Ctrl Pts',(-20.6064248612792,-46.3458651517313,
123.266175723513)) ;
#101672 = CARTESIAN_POINT('Ctrl Pts',(-20.5633304475385,-46.355813718994,
123.061479829175)) ;
#101673 = CARTESIAN_POINT('Ctrl Pts',(-20.4843277046656,-46.365868524296,
122.865438871177)) ;
#101674 = CARTESIAN_POINT('Ctrl Pts',(-20.3753478147443,-46.3756873075596,
122.690117977442)) ;
#101675 = CARTESIAN_POINT('Ctrl Pts',(-20.2349691323031,-46.3857230799201,
122.532619310703)) ;
#101676 = CARTESIAN_POINT('Ctrl Pts',(-20.0691759408736,-46.3957477789488,
122.402497408529)) ;
#101677 = CARTESIAN_POINT('Ctrl Pts',(-19.8867297553205,-46.4055997822079,
122.304449395899)) ;
#101678 = CARTESIAN_POINT('Ctrl Pts',(-19.6873843033137,-46.4155907166051,
122.238359372171)) ;
#101679 = CARTESIAN_POINT('Ctrl Pts',(-19.4810798069849,-46.4255086390362,
122.207965864558)) ;
#101680 = CARTESIAN_POINT('Ctrl Pts',(-19.2703526177087,-46.4355369947185,
122.213873497214)) ;
#101681 = CARTESIAN_POINT('Ctrl Pts',(-19.0667741771753,-46.4454212792291,
122.255577118943)) ;
#101682 = CARTESIAN_POINT('Ctrl Pts',(-18.871242155571,-46.455413963137,122.332388455199)) ;
#101683 = CARTESIAN_POINT('Ctrl Pts',(-18.6915622014373,-46.4654427001447,
122.442695086588)) ;
#101684 = CARTESIAN_POINT('Ctrl Pts',(-18.5358336185271,-46.4753280967736,
122.580323771168)) ;
#101685 = CARTESIAN_POINT('Ctrl Pts',(-18.404808719555,-46.4853159821875,
122.744378203183)) ;
#101686 = CARTESIAN_POINT('Ctrl Pts',(-18.3045250810069,-46.4952666848481,
122.928003706336)) ;
#101687 = CARTESIAN_POINT('Ctrl Pts',(-18.2371710355697,-46.5053070029455,
123.128025654843)) ;
#101688 = CARTESIAN_POINT('Ctrl Pts',(-18.2058821671558,-46.5151815682787,
123.333272137054)) ;
#101689 = CARTESIAN_POINT('Ctrl Pts',(-18.2104984625047,-46.5251812283398,
123.543411466236)) ;
#101690 = CARTESIAN_POINT('Ctrl Pts',(-18.2509769529767,-46.5350902235075,
123.747796646256)) ;
#101691 = CARTESIAN_POINT('Ctrl Pts',(-18.3274733127971,-46.5451449646707,
123.944815347617)) ;
#101692 = CARTESIAN_POINT('Ctrl Pts',(-18.4347110897703,-46.5550035765845,
124.122217178348)) ;
#101693 = CARTESIAN_POINT('Ctrl Pts',(-18.5738806035724,-46.5650716988639,
124.281654657208)) ;
#101694 = CARTESIAN_POINT('Ctrl Pts',(-18.7351876359307,-46.5749271695671,
124.411716813316)) ;
#101695 = CARTESIAN_POINT('Ctrl Pts',(-18.9188672807812,-46.5849220290604,
124.513749762234)) ;
#101696 = CARTESIAN_POINT('Ctrl Pts',(-19.118354849174,-46.5949532824024,
124.582164499542)) ;
#101697 = CARTESIAN_POINT('Ctrl Pts',(-19.3232243282629,-46.6048199812755,
124.614690138812)) ;
#101698 = CARTESIAN_POINT('Ctrl Pts',(-19.5331302566651,-46.6148067970267,
124.611452414342)) ;
#101699 = CARTESIAN_POINT('Ctrl Pts',(-19.738536461996,-46.6247540022221,
124.572058896777)) ;
#101700 = CARTESIAN_POINT('Ctrl Pts',(-19.9357908708862,-46.6347969903484,
124.496809758944)) ;
#101701 = CARTESIAN_POINT('Ctrl Pts',(-20.1138965112704,-46.6446643449699,
124.390442932952)) ;
#101702 = CARTESIAN_POINT('Ctrl Pts',(-20.2727519161392,-46.654630238268,
124.253850206082)) ;
#101703 = CARTESIAN_POINT('Ctrl Pts',(-20.4060931489075,-46.6646540156441,
124.090652823056)) ;
#101704 = CARTESIAN_POINT('Ctrl Pts',(-20.5080934114854,-46.6745795635758,
123.908627324114)) ;
#101705 = CARTESIAN_POINT('Ctrl Pts',(-20.5775159071975,-46.6845200399968,
123.711501929534)) ;
#101706 = CARTESIAN_POINT('Ctrl Pts',(-20.6117775949785,-46.6945662496597,
123.503109228125)) ;
#101707 = CARTESIAN_POINT('Ctrl Pts',(-20.609601734088,-46.7044275063215,
123.295787805518)) ;
#101708 = CARTESIAN_POINT('Ctrl Pts',(-20.5713127454808,-46.7144211345968,
123.089239585452)) ;
#101709 = CARTESIAN_POINT('Ctrl Pts',(-20.4983247752456,-46.724346531907,
122.893724488115)) ;
#101710 = CARTESIAN_POINT('Ctrl Pts',(-20.391439501188,-46.7343744398172,
122.712042412419)) ;
#101711 = CARTESIAN_POINT('Ctrl Pts',(-20.2566892583958,-46.7442607554864,
122.553760365843)) ;
#101712 = CARTESIAN_POINT('Ctrl Pts',(-20.0942706686031,-46.7542923503902,
122.419287277191)) ;
#101713 = CARTESIAN_POINT('Ctrl Pts',(-19.91373555509,-46.7641745933419,122.31641060303)) ;
#101714 = CARTESIAN_POINT('Ctrl Pts',(-19.7146556710455,-46.7742340643717,
122.245124210862)) ;
#101715 = CARTESIAN_POINT('Ctrl Pts',(-19.5101828248972,-46.7841005090349,
122.210192914009)) ;
#101716 = CARTESIAN_POINT('Ctrl Pts',(-19.3006692712857,-46.7940666334836,
122.210645331334)) ;
#101717 = CARTESIAN_POINT('Ctrl Pts',(-19.0931463132773,-46.8040968768747,
122.248040108204)) ;
#101718 = CARTESIAN_POINT('Ctrl Pts',(-18.8978525704914,-46.8139899118278,
122.319631934848)) ;
#101719 = CARTESIAN_POINT('Ctrl Pts',(-18.7150886638094,-46.8240408260646,
122.425644012943)) ;
#101720 = CARTESIAN_POINT('Ctrl Pts',(-18.5560646983535,-46.8339306522892,
122.559594386453)) ;
#101721 = CARTESIAN_POINT('Ctrl Pts',(-18.3758141169603,-46.8472654673361,
122.774360902659)) ;
#101722 = CARTESIAN_POINT('Ctrl Pts',(-18.2567587048321,-46.8605425585076,
123.030322963352)) ;
#101723 = CARTESIAN_POINT('Ctrl Pts',(-18.2080003363345,-46.8737908471059,
123.30452785206)) ;
#101724 = CARTESIAN_POINT('Ctrl Pts',(-18.2078269534675,-46.8838456885999,
123.515888892915)) ;
#101725 = CARTESIAN_POINT('Ctrl Pts',(-18.2432089840298,-46.8936766779075,
123.719550756996)) ;
#101726 = CARTESIAN_POINT('Ctrl Pts',(-18.3149991815687,-46.9037532422307,
123.918820167405)) ;
#101727 = CARTESIAN_POINT('Ctrl Pts',(-18.4179520069313,-46.9136025673647,
124.098495475079)) ;
#101728 = CARTESIAN_POINT('Ctrl Pts',(-18.5971287291252,-46.9269505670019,
124.314512778421)) ;
#101729 = CARTESIAN_POINT('Ctrl Pts',(-18.8850045547426,-46.9435353265385,
124.518066871965)) ;
#101730 = CARTESIAN_POINT('Ctrl Pts',(-19.224607589912,-46.9601038778866,
124.61194925975)) ;
#101731 = CARTESIAN_POINT('Ctrl Pts',(-19.5054384121167,-46.9734637027056,
124.613976516196)) ;
#101732 = CARTESIAN_POINT('Ctrl Pts',(-19.7108170540139,-46.9833691115362,
124.579464056229)) ;
#101733 = CARTESIAN_POINT('Ctrl Pts',(-19.9082274832212,-46.9933291381203,
124.509731303906)) ;
#101734 = CARTESIAN_POINT('Ctrl Pts',(-20.1511343904,-47.0065867223056,124.372969212261)) ;
#101735 = CARTESIAN_POINT('Ctrl Pts',(-20.4042796267339,-47.0232379338003,
124.125469276833)) ;
#101736 = CARTESIAN_POINT('Ctrl Pts',(-20.5876345912551,-47.0431561479106,
123.743721511354)) ;
#101737 = CARTESIAN_POINT('Ctrl Pts',(-20.6305357829739,-47.0630339111314,
123.323189265987)) ;
#101738 = CARTESIAN_POINT('Ctrl Pts',(-20.5263194941184,-47.0830465789186,
122.910705188635)) ;
#101739 = CARTESIAN_POINT('Ctrl Pts',(-20.2902264559902,-47.1028591015852,
122.561714858554)) ;
#101740 = CARTESIAN_POINT('Ctrl Pts',(-19.9468003241497,-47.1228424015851,
122.311660429223)) ;
#101741 = CARTESIAN_POINT('Ctrl Pts',(-19.5402507461604,-47.1427366786864,
122.194589335901)) ;
#101742 = CARTESIAN_POINT('Ctrl Pts',(-19.1173687635124,-47.1626694404441,
122.222669014583)) ;
#101743 = CARTESIAN_POINT('Ctrl Pts',(-18.7289139893824,-47.1826354462089,
122.393931867359)) ;
#101744 = CARTESIAN_POINT('Ctrl Pts',(-18.4233338107071,-47.2025139783737,
122.685985372906)) ;
#101745 = CARTESIAN_POINT('Ctrl Pts',(-18.2348504644111,-47.2224536450341,
123.065707037665)) ;
#101746 = CARTESIAN_POINT('Ctrl Pts',(-18.1872341856347,-47.2423485196794,
123.486082300912)) ;
#101747 = CARTESIAN_POINT('Ctrl Pts',(-18.285549521776,-47.2622556589728,
123.897686321295)) ;
#101748 = CARTESIAN_POINT('Ctrl Pts',(-18.5179844304115,-47.2821662070513,
124.251688353831)) ;
#101749 = CARTESIAN_POINT('Ctrl Pts',(-18.8603588404336,-47.3022347924084,
124.506213290609)) ;
#101750 = CARTESIAN_POINT('Ctrl Pts',(-19.2632972916502,-47.3220165897232,
124.627349301295)) ;
#101751 = CARTESIAN_POINT('Ctrl Pts',(-19.687908123278,-47.3420241366677,
124.604082024254)) ;
#101752 = CARTESIAN_POINT('Ctrl Pts',(-20.0757232293884,-47.3618458749706,
124.438770205697)) ;
#101753 = CARTESIAN_POINT('Ctrl Pts',(-20.3867048359403,-47.3818258948748,
124.149429992821)) ;
#101754 = CARTESIAN_POINT('Ctrl Pts',(-20.5792195365929,-47.401743346137,
123.772199508014)) ;
#101755 = CARTESIAN_POINT('Ctrl Pts',(-20.6323196628595,-47.4216182673097,
123.352926357512)) ;
#101756 = CARTESIAN_POINT('Ctrl Pts',(-20.5382000473738,-47.4416426358605,
122.937716092165)) ;
#101757 = CARTESIAN_POINT('Ctrl Pts',(-20.3096969857281,-47.461509320234,
122.58235343421)) ;
#101758 = CARTESIAN_POINT('Ctrl Pts',(-19.9728434974952,-47.4814531420802,
122.324834861708)) ;
#101759 = CARTESIAN_POINT('Ctrl Pts',(-19.5689827186034,-47.5013605113317,
122.198075400464)) ;
#101760 = CARTESIAN_POINT('Ctrl Pts',(-19.1467741470147,-47.5212352090784,
122.215922859615)) ;
#101761 = CARTESIAN_POINT('Ctrl Pts',(-18.7538248582443,-47.5412171516001,
122.37755972853)) ;
#101762 = CARTESIAN_POINT('Ctrl Pts',(-18.4411591865432,-47.561119818511,
122.662668187137)) ;
#101763 = CARTESIAN_POINT('Ctrl Pts',(-18.2438659827883,-47.5809751760497,
123.035980794577)) ;
#101764 = CARTESIAN_POINT('Ctrl Pts',(-18.1856871425068,-47.6010392147657,
123.458543716843)) ;
#101765 = CARTESIAN_POINT('Ctrl Pts',(-18.2744811769928,-47.6208943944907,
123.871435728534)) ;
#101766 = CARTESIAN_POINT('Ctrl Pts',(-18.4997986396538,-47.6408744991552,
124.231400086488)) ;
#101767 = CARTESIAN_POINT('Ctrl Pts',(-18.8314729486818,-47.660683604325,
124.491205559772)) ;
#101768 = CARTESIAN_POINT('Ctrl Pts',(-19.2352355800395,-47.6806762246657,
124.623773316177)) ;
#101769 = CARTESIAN_POINT('Ctrl Pts',(-19.5868212685849,-47.6972157071698,
124.612937916128)) ;
#101770 = CARTESIAN_POINT('Ctrl Pts',(-19.8558774739996,-47.710580025234,
124.532060996429)) ;
#101771 = CARTESIAN_POINT('Ctrl Pts',(-20.1042150648437,-47.7237976277355,
124.407379094287)) ;
#101772 = CARTESIAN_POINT('Ctrl Pts',(-20.3689671152009,-47.7404552220133,
124.172152307496)) ;
#101773 = CARTESIAN_POINT('Ctrl Pts',(-20.5701609183017,-47.760320924055,
123.800669110087)) ;
#101774 = CARTESIAN_POINT('Ctrl Pts',(-20.6228296467221,-47.776950650745,
123.451116951742)) ;
#101775 = CARTESIAN_POINT('Ctrl Pts',(-20.591441756801,-47.7902397658829,
123.173432269653)) ;
#101776 = CARTESIAN_POINT('Ctrl Pts',(-20.5323650846127,-47.80020411286,122.972473509771)) ;
#101777 = CARTESIAN_POINT('Ctrl Pts',(-20.4397431352178,-47.8101324808615,
122.78542115287)) ;
#101778 = CARTESIAN_POINT('Ctrl Pts',(-20.2747113866372,-47.8234159139502,
122.560165381715)) ;
#101779 = CARTESIAN_POINT('Ctrl Pts',(-19.9984876257808,-47.8400679916905,
122.338584408129)) ;
#101780 = CARTESIAN_POINT('Ctrl Pts',(-19.6654139408128,-47.8566193609914,
122.225127763266)) ;
#101781 = CARTESIAN_POINT('Ctrl Pts',(-19.3866766014648,-47.8699067891403,
122.2059729197)) ;
#101782 = CARTESIAN_POINT('Ctrl Pts',(-19.1767345904945,-47.8799513288404,
122.228509743706)) ;
#101783 = CARTESIAN_POINT('Ctrl Pts',(-18.9778647772016,-47.8897941706643,
122.285740743263)) ;
#101784 = CARTESIAN_POINT('Ctrl Pts',(-18.7891005548347,-47.8997784549112,
122.377489056293)) ;
#101785 = CARTESIAN_POINT('Ctrl Pts',(-18.6197244084275,-47.9097281003104,
122.500245233564)) ;
#101786 = CARTESIAN_POINT('Ctrl Pts',(-18.4733160568554,-47.9197278619988,
122.651124906538)) ;
#101787 = CARTESIAN_POINT('Ctrl Pts',(-18.355252870552,-47.9297592079577,
122.825866915352)) ;
#101788 = CARTESIAN_POINT('Ctrl Pts',(-18.2705550986385,-47.9396141624348,
123.014949860887)) ;
#101789 = CARTESIAN_POINT('Ctrl Pts',(-18.2189034040451,-47.9495867004353,
123.218119554331)) ;
#101790 = CARTESIAN_POINT('Ctrl Pts',(-18.2032894716293,-47.9595816941703,
123.427697273078)) ;
#101791 = CARTESIAN_POINT('Ctrl Pts',(-18.2246368460306,-47.9696157529644,
123.637543751043)) ;
#101792 = CARTESIAN_POINT('Ctrl Pts',(-18.2807655769302,-47.9794710957874,
123.837007896534)) ;
#101793 = CARTESIAN_POINT('Ctrl Pts',(-18.3717098539372,-47.989470575133,
124.026496781304)) ;
#101794 = CARTESIAN_POINT('Ctrl Pts',(-18.4927398324183,-47.9993650238883,
124.195722216039)) ;
#101795 = CARTESIAN_POINT('Ctrl Pts',(-18.6438364232748,-48.0094281433228,
124.343747121093)) ;
#101796 = CARTESIAN_POINT('Ctrl Pts',(-18.8143933334818,-48.019267788564,
124.460861131954)) ;
#101797 = CARTESIAN_POINT('Ctrl Pts',(-19.0068017803678,-48.0293309527501,
124.54874750127)) ;
#101798 = CARTESIAN_POINT('Ctrl Pts',(-19.2082058632802,-48.0392252224989,
124.600841675692)) ;
#101799 = CARTESIAN_POINT('Ctrl Pts',(-19.416494388745,-48.0491669485127,
124.617812118277)) ;
#101800 = CARTESIAN_POINT('Ctrl Pts',(-19.6259143985709,-48.0591698371721,
124.598324259586)) ;
#101801 = CARTESIAN_POINT('Ctrl Pts',(-19.8293661589921,-48.0692096859661,
124.54220631974)) ;
#101802 = CARTESIAN_POINT('Ctrl Pts',(-20.0161233829794,-48.0790339014269,
124.45396960631)) ;
#101803 = CARTESIAN_POINT('Ctrl Pts',(-20.1888586186341,-48.0890907449205,
124.332080418983)) ;
#101804 = CARTESIAN_POINT('Ctrl Pts',(-20.3357293798026,-48.0990193543165,
124.183752079466)) ;
#101805 = CARTESIAN_POINT('Ctrl Pts',(-20.4553755185566,-48.1089712383544,
124.012109238348)) ;
#101806 = CARTESIAN_POINT('Ctrl Pts',(-20.5439400707271,-48.119024191162,
123.820231845081)) ;
#101807 = CARTESIAN_POINT('Ctrl Pts',(-20.5969890504903,-48.1288470676282,
123.620638289231)) ;
#101808 = CARTESIAN_POINT('Ctrl Pts',(-20.6153607624487,-48.1389028001983,
123.410049223762)) ;
#101809 = CARTESIAN_POINT('Ctrl Pts',(-20.5967291543706,-48.148843565186,
123.201887601555)) ;
#101810 = CARTESIAN_POINT('Ctrl Pts',(-20.5430668295236,-48.1587478980916,
123.00069716578)) ;
#101811 = CARTESIAN_POINT('Ctrl Pts',(-20.4539124374532,-48.1687945669723,
122.80924277324)) ;
#101812 = CARTESIAN_POINT('Ctrl Pts',(-20.3348163682477,-48.1786901302781,
122.638629249431)) ;
#101813 = CARTESIAN_POINT('Ctrl Pts',(-20.1854787168421,-48.1887521879784,
122.488852479023)) ;
#101814 = CARTESIAN_POINT('Ctrl Pts',(-20.0161998887154,-48.1985949656059,
122.369803224795)) ;
#101815 = CARTESIAN_POINT('Ctrl Pts',(-19.8262675174626,-48.2085854438577,
122.280207738523)) ;
#101816 = CARTESIAN_POINT('Ctrl Pts',(-19.6248641256518,-48.2185144165013,
122.225310488959)) ;
#101817 = CARTESIAN_POINT('Ctrl Pts',(-19.4157282410988,-48.2285055533808,
122.20577320944)) ;
#101818 = CARTESIAN_POINT('Ctrl Pts',(-19.2057461435763,-48.2385276708698,
122.223152219165)) ;
#101819 = CARTESIAN_POINT('Ctrl Pts',(-19.0043951283758,-48.248428181272,
122.275886365891)) ;
#101820 = CARTESIAN_POINT('Ctrl Pts',(-18.8134346587529,-48.2584171740181,
122.3632575331)) ;
#101821 = CARTESIAN_POINT('Ctrl Pts',(-18.641045347287,-48.2683824180687,
122.482290762175)) ;
#101822 = CARTESIAN_POINT('Ctrl Pts',(-18.4924930895202,-48.2782866825819,
122.628215096512)) ;
#101823 = CARTESIAN_POINT('Ctrl Pts',(-18.3697845395044,-48.2883447742801,
122.800399391867)) ;
#101824 = CARTESIAN_POINT('Ctrl Pts',(-18.2805661767758,-48.2981947147085,
122.987283594755)) ;
#101825 = CARTESIAN_POINT('Ctrl Pts',(-18.2236581684677,-48.308221725882,
123.190252393371)) ;
#101826 = CARTESIAN_POINT('Ctrl Pts',(-18.2033996010484,-48.3182503124941,
123.400119494456)) ;
#101827 = CARTESIAN_POINT('Ctrl Pts',(-18.219194587614,-48.3280955266068,
123.606481917187)) ;
#101828 = CARTESIAN_POINT('Ctrl Pts',(-18.2707998702963,-48.3380862747864,
123.81008550983)) ;
#101829 = CARTESIAN_POINT('Ctrl Pts',(-18.3577998993099,-48.3481239083719,
124.002339524846)) ;
#101830 = CARTESIAN_POINT('Ctrl Pts',(-18.4742953902907,-48.3579691975847,
124.173424423083)) ;
#101831 = CARTESIAN_POINT('Ctrl Pts',(-18.6203765330069,-48.3679505983906,
124.32404507133)) ;
#101832 = CARTESIAN_POINT('Ctrl Pts',(-18.7899420114135,-48.3779028313805,
124.446625734282)) ;
#101833 = CARTESIAN_POINT('Ctrl Pts',(-18.9789868413194,-48.3879016428371,
124.538580257866)) ;
#101834 = CARTESIAN_POINT('Ctrl Pts',(-19.1820248011104,-48.3979407467678,
124.596148015558)) ;
#101835 = CARTESIAN_POINT('Ctrl Pts',(-19.3874736668821,-48.4077656891871,
124.61757403462)) ;
#101836 = CARTESIAN_POINT('Ctrl Pts',(-19.5983397624482,-48.4178203766631,
124.603009670107)) ;
#101837 = CARTESIAN_POINT('Ctrl Pts',(-19.8011230753386,-48.4277631790199,
124.552268924027)) ;
#101838 = CARTESIAN_POINT('Ctrl Pts',(-19.9915243843805,-48.4376669749596,
124.468007687713)) ;
#101839 = CARTESIAN_POINT('Ctrl Pts',(-20.1668107922239,-48.4477137543347,
124.35019781342)) ;
#101840 = CARTESIAN_POINT('Ctrl Pts',(-20.3168498829081,-48.4576094126293,
124.206042816972)) ;
#101841 = CARTESIAN_POINT('Ctrl Pts',(-20.4416259189288,-48.4676709798799,
124.035266345646)) ;
#101842 = CARTESIAN_POINT('Ctrl Pts',(-20.5328863746272,-48.4775156243172,
123.849501112895)) ;
#101843 = CARTESIAN_POINT('Ctrl Pts',(-20.5919002673706,-48.4874756705599,
123.648600717732)) ;
#101844 = CARTESIAN_POINT('Ctrl Pts',(-20.6149049736359,-48.4975139665783,
123.438831673452)) ;
#101845 = CARTESIAN_POINT('Ctrl Pts',(-20.601758722452,-48.5073873079966,
123.231648800502)) ;
#101846 = CARTESIAN_POINT('Ctrl Pts',(-20.5518031671284,-48.5174604117959,
123.025898849127)) ;
#101847 = CARTESIAN_POINT('Ctrl Pts',(-20.4692129884371,-48.5272812269148,
122.836629037996)) ;
#101848 = CARTESIAN_POINT('Ctrl Pts',(-20.3522826405625,-48.5373580919928,
122.660021545699)) ;
#101849 = CARTESIAN_POINT('Ctrl Pts',(-20.2094321696114,-48.547222831648,
122.509642735645)) ;
#101850 = CARTESIAN_POINT('Ctrl Pts',(-20.040330543343,-48.5572452348894,
122.383957764548)) ;
#101851 = CARTESIAN_POINT('Ctrl Pts',(-19.8516573443551,-48.5672709591779,
122.289974671412)) ;
#101852 = CARTESIAN_POINT('Ctrl Pts',(-19.653106142021,-48.5771257421992,
122.230855831632)) ;
#101853 = CARTESIAN_POINT('Ctrl Pts',(-19.4447606745036,-48.5871045859224,
122.206265761505)) ;
#101854 = CARTESIAN_POINT('Ctrl Pts',(-19.2345057126181,-48.5971234781591,
122.218635134644)) ;
#101855 = CARTESIAN_POINT('Ctrl Pts',(-19.0322324411975,-48.6070066872001,
122.266253833423)) ;
#101856 = CARTESIAN_POINT('Ctrl Pts',(-18.8378163548145,-48.6170749965403,
122.349864218783)) ;
#101857 = CARTESIAN_POINT('Ctrl Pts',(-18.664866251198,-48.626905121873,122.4630502975)) ;
#101858 = CARTESIAN_POINT('Ctrl Pts',(-18.5104349683193,-48.63697167425,122.607702663307)) ;
#101859 = CARTESIAN_POINT('Ctrl Pts',(-18.3857576424288,-48.6468619111437,
122.774131254858)) ;
#101860 = CARTESIAN_POINT('Ctrl Pts',(-18.2905113283134,-48.6568541359377,
122.961351716176)) ;
#101861 = CARTESIAN_POINT('Ctrl Pts',(-18.2295845515422,-48.6668167562886,
123.16173604874)) ;
#101862 = CARTESIAN_POINT('Ctrl Pts',(-18.2040083705147,-48.6767217590518,
123.368407504756)) ;
#101863 = CARTESIAN_POINT('Ctrl Pts',(-18.215014431292,-48.6867795214499,
123.579548442088)) ;
#101864 = CARTESIAN_POINT('Ctrl Pts',(-18.2613768578479,-48.6966300408287,
123.781396846566)) ;
#101865 = CARTESIAN_POINT('Ctrl Pts',(-18.3431276950445,-48.7066616178269,
123.975788123339)) ;
#101866 = CARTESIAN_POINT('Ctrl Pts',(-18.4575011822007,-48.7166713529318,
124.152456894868)) ;
#101867 = CARTESIAN_POINT('Ctrl Pts',(-18.5992160663724,-48.7265809295581,
124.30513577047)) ;
#101868 = CARTESIAN_POINT('Ctrl Pts',(-18.7652852836129,-48.7365083154147,
124.431557772479)) ;
#101869 = CARTESIAN_POINT('Ctrl Pts',(-18.9530419153149,-48.746553249905,
124.528196399134)) ;
#101870 = CARTESIAN_POINT('Ctrl Pts',(-19.1515171122009,-48.756439182093,
124.589900087723)) ;
#101871 = CARTESIAN_POINT('Ctrl Pts',(-19.3598605805788,-48.766432488046,
124.616846677336)) ;
#101872 = CARTESIAN_POINT('Ctrl Pts',(-19.5687256311403,-48.7763781258279,
124.607171918899)) ;
#101873 = CARTESIAN_POINT('Ctrl Pts',(-19.7728747092377,-48.7863253941738,
124.561787027165)) ;
#101874 = CARTESIAN_POINT('Ctrl Pts',(-19.9678900052988,-48.7963732963109,
124.480620729469)) ;
#101875 = CARTESIAN_POINT('Ctrl Pts',(-20.1424033659662,-48.8062209911511,
124.369236934699)) ;
#101876 = CARTESIAN_POINT('Ctrl Pts',(-20.2971288989409,-48.8161825008955,
124.228119055015)) ;
#101877 = CARTESIAN_POINT('Ctrl Pts',(-20.4256593397481,-48.8262118925043,
124.060963931451)) ;
#101878 = CARTESIAN_POINT('Ctrl Pts',(-20.5221256513388,-48.8361193880591,
123.876361226826)) ;
#101879 = CARTESIAN_POINT('Ctrl Pts',(-20.5857066016989,-48.8460647797221,
123.677197420647)) ;
#101880 = CARTESIAN_POINT('Ctrl Pts',(-20.6140292659733,-48.8560666973195,
123.468813104556)) ;
#101881 = CARTESIAN_POINT('Ctrl Pts',(-20.6053201133228,-48.8661067648717,
123.257938194825)) ;
#101882 = CARTESIAN_POINT('Ctrl Pts',(-20.5615508370496,-48.8759310763115,
123.056073986905)) ;
#101883 = CARTESIAN_POINT('Ctrl Pts',(-20.481835057426,-48.8859873174676,
122.86028723673)) ;
#101884 = CARTESIAN_POINT('Ctrl Pts',(-20.3705060078886,-48.8959182392032,
122.683639620524)) ;
#101885 = CARTESIAN_POINT('Ctrl Pts',(-20.2303723647411,-48.9058614752794,
122.528564544329)) ;
#101886 = CARTESIAN_POINT('Ctrl Pts',(-20.0648880113729,-48.9158427592919,
122.399490072293)) ;
#101887 = CARTESIAN_POINT('Ctrl Pts',(-19.878216198548,-48.9258870609176,
122.300837780774)) ;
#101888 = CARTESIAN_POINT('Ctrl Pts',(-19.6816696601747,-48.935715142137,
122.237015265823)) ;
#101889 = CARTESIAN_POINT('Ctrl Pts',(-19.4719420297821,-48.9457917449862,
122.207471003049)) ;
#101890 = CARTESIAN_POINT('Ctrl Pts',(-19.2648957747696,-48.9556438241047,
122.214527642256)) ;
#101891 = CARTESIAN_POINT('Ctrl Pts',(-19.057710705254,-48.9657170824136,
122.258197132153)) ;
#101892 = CARTESIAN_POINT('Ctrl Pts',(-18.8657533812735,-48.9755585417939,
122.335430936369)) ;
#101893 = CARTESIAN_POINT('Ctrl Pts',(-18.6875912864788,-48.9855196372063,
122.445472131089)) ;
#101894 = CARTESIAN_POINT('Ctrl Pts',(-18.5303196629414,-48.995556921603,
122.586153066523)) ;
#101895 = CARTESIAN_POINT('Ctrl Pts',(-18.4016538330767,-49.0054332603383,
122.749141697711)) ;
#101896 = CARTESIAN_POINT('Ctrl Pts',(-18.3013797981998,-49.0154953864916,
122.935372743408)) ;
#101897 = CARTESIAN_POINT('Ctrl Pts',(-18.2361811326668,-49.0253635604681,
123.132347585677)) ;
#101898 = CARTESIAN_POINT('Ctrl Pts',(-18.2053436817769,-49.0353691089719,
123.340394845935)) ;
#101899 = CARTESIAN_POINT('Ctrl Pts',(-18.2111591508451,-49.0453517408675,
123.550218995619)) ;
#101900 = CARTESIAN_POINT('Ctrl Pts',(-18.253781537553,-49.0553956832892,
123.757009941247)) ;
#101901 = CARTESIAN_POINT('Ctrl Pts',(-18.3297375526098,-49.0652238313164,
123.949160213562)) ;
#101902 = CARTESIAN_POINT('Ctrl Pts',(-18.4391089482061,-49.0752136986908,
124.128453147214)) ;
#101903 = CARTESIAN_POINT('Ctrl Pts',(-18.5791098749347,-49.0852574376463,
124.286517956109)) ;
#101904 = CARTESIAN_POINT('Ctrl Pts',(-18.7405061461657,-49.0950791861842,
124.41530576025)) ;
#101905 = CARTESIAN_POINT('Ctrl Pts',(-18.9255019726475,-49.105114163794,
124.516713681621)) ;
#101906 = CARTESIAN_POINT('Ctrl Pts',(-19.1252883403302,-49.1151390765517,
124.583837300899)) ;
#101907 = CARTESIAN_POINT('Ctrl Pts',(-19.3300292432667,-49.1249910196455,
124.615157613773)) ;
#101908 = CARTESIAN_POINT('Ctrl Pts',(-19.5399978202591,-49.1349819809746,
124.610707974412)) ;
#101909 = CARTESIAN_POINT('Ctrl Pts',(-19.7445743881936,-49.1448998558431,
124.570292127389)) ;
#101910 = CARTESIAN_POINT('Ctrl Pts',(-19.9411701416523,-49.1549283748443,
124.494185550306)) ;
#101911 = CARTESIAN_POINT('Ctrl Pts',(-20.1190372422758,-49.1648120536421,
124.386753382207)) ;
#101912 = CARTESIAN_POINT('Ctrl Pts',(-20.2776085862395,-49.1748069970819,
124.248885254077)) ;
#101913 = CARTESIAN_POINT('Ctrl Pts',(-20.4099744135466,-49.1848338509043,
124.084828086989)) ;
#101914 = CARTESIAN_POINT('Ctrl Pts',(-20.510648075039,-49.1947180152432,
123.903037977322)) ;
#101915 = CARTESIAN_POINT('Ctrl Pts',(-20.5791926577248,-49.2047061132856,
123.704581130644)) ;
#101916 = CARTESIAN_POINT('Ctrl Pts',(-20.6122374715943,-49.2146572197427,
123.497977351744)) ;
#101917 = CARTESIAN_POINT('Ctrl Pts',(-20.6087584530303,-49.2247022709108,
123.286839556566)) ;
#101918 = CARTESIAN_POINT('Ctrl Pts',(-20.5695137034863,-49.2345640312691,
123.08326163448)) ;
#101919 = CARTESIAN_POINT('Ctrl Pts',(-20.4953630084069,-49.2445268480995,
122.887375704082)) ;
#101920 = CARTESIAN_POINT('Ctrl Pts',(-20.3872484323953,-49.2545615293803,
122.70623567795)) ;
#101921 = CARTESIAN_POINT('Ctrl Pts',(-20.2516257021423,-49.2644465591611,
122.54873912026)) ;
#101922 = CARTESIAN_POINT('Ctrl Pts',(-20.0877956193133,-49.274512152559,
122.414857498311)) ;
#101923 = CARTESIAN_POINT('Ctrl Pts',(-19.9074048645772,-49.2843513209205,
122.313567887635)) ;
#101924 = CARTESIAN_POINT('Ctrl Pts',(-19.7078843684938,-49.294413918662,
122.243329293584)) ;
#101925 = CARTESIAN_POINT('Ctrl Pts',(-19.5025604294177,-49.304310931069,
122.209583344608)) ;
#101926 = CARTESIAN_POINT('Ctrl Pts',(-19.2937846335833,-49.3142422528946,
122.211313962899)) ;
#101927 = CARTESIAN_POINT('Ctrl Pts',(-19.0862373034361,-49.3242840156491,
122.249916128646)) ;
#101928 = CARTESIAN_POINT('Ctrl Pts',(-18.8915024927384,-49.3341722145398,
122.322702651391)) ;
#101929 = CARTESIAN_POINT('Ctrl Pts',(-18.710304164379,-49.3441661531396,
122.429022282141)) ;
#101930 = CARTESIAN_POINT('Ctrl Pts',(-18.5511551207045,-49.3541069741765,
122.564495146748)) ;
#101931 = CARTESIAN_POINT('Ctrl Pts',(-18.4175080465138,-49.3640663564647,
122.725655347758)) ;
#101932 = CARTESIAN_POINT('Ctrl Pts',(-18.3133483467872,-49.3740641161171,
122.908239413942)) ;
#101933 = CARTESIAN_POINT('Ctrl Pts',(-18.242483951838,-49.3841002523194,
123.106968601329)) ;
#101934 = CARTESIAN_POINT('Ctrl Pts',(-18.2076123181363,-49.3939510498103,
123.311104555216)) ;
#101935 = CARTESIAN_POINT('Ctrl Pts',(-18.2081039999634,-49.4039119148866,
123.520505395636)) ;
#101936 = CARTESIAN_POINT('Ctrl Pts',(-18.2454532381414,-49.413940782517,
123.728021411846)) ;
#101937 = CARTESIAN_POINT('Ctrl Pts',(-18.3173380044574,-49.4238510186534,
123.923562578282)) ;
#101938 = CARTESIAN_POINT('Ctrl Pts',(-18.4218783908615,-49.4337859719679,
124.104388358142)) ;
#101939 = CARTESIAN_POINT('Ctrl Pts',(-18.5578017692251,-49.4438269023775,
124.265889289418)) ;
#101940 = CARTESIAN_POINT('Ctrl Pts',(-18.717159569688,-49.4537147991591,
124.399382341823)) ;
#101941 = CARTESIAN_POINT('Ctrl Pts',(-18.8989187332831,-49.4637042508178,
124.50457582267)) ;
#101942 = CARTESIAN_POINT('Ctrl Pts',(-19.0956385064663,-49.4736633411831,
124.576235301042)) ;
#101943 = CARTESIAN_POINT('Ctrl Pts',(-19.3004600938995,-49.4835606534894,
124.612950415189)) ;
#101944 = CARTESIAN_POINT('Ctrl Pts',(-19.5118599213886,-49.4936170793897,
124.613452940956)) ;
#101945 = CARTESIAN_POINT('Ctrl Pts',(-19.7163289030881,-49.5034870819794,
124.578011255348)) ;
#101946 = CARTESIAN_POINT('Ctrl Pts',(-19.9142897101432,-49.5134910151567,
124.507058739221)) ;
#101947 = CARTESIAN_POINT('Ctrl Pts',(-20.0966121318838,-49.5234782756206,
124.402861453915)) ;
#101948 = CARTESIAN_POINT('Ctrl Pts',(-20.2586003670791,-49.5335053272063,
124.267990605406)) ;
#101949 = CARTESIAN_POINT('Ctrl Pts',(-20.3930406244089,-49.5433964170324,
124.109334043346)) ;
#101950 = CARTESIAN_POINT('Ctrl Pts',(-20.5342780283524,-49.5566941718134,
123.868104695058)) ;
#101951 = CARTESIAN_POINT('Ctrl Pts',(-20.6091907968106,-49.5698922314216,
123.597594165935)) ;
#101952 = CARTESIAN_POINT('Ctrl Pts',(-20.6114275578106,-49.5832889719908,
123.316024746317)) ;
#101953 = CARTESIAN_POINT('Ctrl Pts',(-20.5772402703446,-49.5931598840642,
123.111292549066)) ;
#101954 = CARTESIAN_POINT('Ctrl Pts',(-20.5066258357299,-49.6032334458323,
122.911686124555)) ;
#101955 = CARTESIAN_POINT('Ctrl Pts',(-20.4052041629203,-49.6130548584207,
122.73177779847)) ;
#101956 = CARTESIAN_POINT('Ctrl Pts',(-20.2709333113176,-49.6231288756517,
122.568063111328)) ;
#101957 = CARTESIAN_POINT('Ctrl Pts',(-20.0611117353507,-49.6362876626163,
122.387673752344)) ;
#101958 = CARTESIAN_POINT('Ctrl Pts',(-19.8053481405709,-49.6496537657104,
122.263890183305)) ;
#101959 = CARTESIAN_POINT('Ctrl Pts',(-19.5302618913783,-49.6629677005995,
122.21199823279)) ;
#101960 = CARTESIAN_POINT('Ctrl Pts',(-19.3221733074671,-49.672867740047,
122.209045191843)) ;
#101961 = CARTESIAN_POINT('Ctrl Pts',(-19.1153107424769,-49.6828321431815,
122.242142756618)) ;
#101962 = CARTESIAN_POINT('Ctrl Pts',(-18.9161025033483,-49.6928621103026,
122.311283131249)) ;
#101963 = CARTESIAN_POINT('Ctrl Pts',(-18.7342401966072,-49.7027643869117,
122.412568271953)) ;
#101964 = CARTESIAN_POINT('Ctrl Pts',(-18.5173661172651,-49.7160303160808,
122.587991118352)) ;
#101965 = CARTESIAN_POINT('Ctrl Pts',(-18.30957148046,-49.7326518471873,122.873770663409)) ;
#101966 = CARTESIAN_POINT('Ctrl Pts',(-18.1920158054967,-49.7525266758319,
123.279733785891)) ;
#101967 = CARTESIAN_POINT('Ctrl Pts',(-18.2154654244898,-49.7691998839338,
123.633488361271)) ;
#101968 = CARTESIAN_POINT('Ctrl Pts',(-18.3053671060185,-49.7824510089151,
123.897133186416)) ;
#101969 = CARTESIAN_POINT('Ctrl Pts',(-18.4387434972553,-49.7956933277359,
124.141576526697)) ;
#101970 = CARTESIAN_POINT('Ctrl Pts',(-18.6845183791827,-49.8124265680754,
124.398729995882)) ;
#101971 = CARTESIAN_POINT('Ctrl Pts',(-19.0624383745878,-49.8322557162633,
124.585847075868)) ;
#101972 = CARTESIAN_POINT('Ctrl Pts',(-19.4832532299204,-49.852180411364,
124.633993539731)) ;
#101973 = CARTESIAN_POINT('Ctrl Pts',(-19.8953522894153,-49.8721036399474,
124.535577527173)) ;
#101974 = CARTESIAN_POINT('Ctrl Pts',(-20.2491737271437,-49.8920307790735,
124.302567370318)) ;
#101975 = CARTESIAN_POINT('Ctrl Pts',(-20.5020828033969,-49.9119072416892,
123.96393264596)) ;
#101976 = CARTESIAN_POINT('Ctrl Pts',(-20.6250775068884,-49.9318844702945,
123.557364931666)) ;
#101977 = CARTESIAN_POINT('Ctrl Pts',(-20.6016593654049,-49.9518193282682,
123.134106375554)) ;
#101978 = CARTESIAN_POINT('Ctrl Pts',(-20.4359559608619,-49.971715777199,
122.744890981338)) ;
#101979 = CARTESIAN_POINT('Ctrl Pts',(-20.1473323587114,-49.9916370612656,
122.434838855941)) ;
#101980 = CARTESIAN_POINT('Ctrl Pts',(-19.769495662519,-50.0115937109365,
122.24166530792)) ;
#101981 = CARTESIAN_POINT('Ctrl Pts',(-19.3501857546235,-50.0314710040481,
122.189109041307)) ;
#101982 = CARTESIAN_POINT('Ctrl Pts',(-18.9375748048692,-50.0513574762766,
122.281767024943)) ;
#101983 = CARTESIAN_POINT('Ctrl Pts',(-18.5785889176961,-50.0714190422006,
122.512196226664)) ;
#101984 = CARTESIAN_POINT('Ctrl Pts',(-18.3229781414478,-50.0912594497413,
122.84777694806)) ;
#101985 = CARTESIAN_POINT('Ctrl Pts',(-18.1954623195406,-50.1111107737143,
123.250164011553)) ;
#101986 = CARTESIAN_POINT('Ctrl Pts',(-18.2137349038756,-50.1311640436657,
123.676102904834)) ;
#101987 = CARTESIAN_POINT('Ctrl Pts',(-18.3743579080065,-50.150984701049,
124.065860297065)) ;
#101988 = CARTESIAN_POINT('Ctrl Pts',(-18.6598219701115,-50.1709561223796,
124.380051948799)) ;
#101989 = CARTESIAN_POINT('Ctrl Pts',(-19.0341107542293,-50.1908496147432,
124.577425404113)) ;
#101990 = CARTESIAN_POINT('Ctrl Pts',(-19.4558354264791,-50.2108737009843,
124.635288471546)) ;
#101991 = CARTESIAN_POINT('Ctrl Pts',(-19.8676147876328,-50.2306785800972,
124.546941076533)) ;
#101992 = CARTESIAN_POINT('Ctrl Pts',(-20.2278651214723,-50.2506375957951,
124.322644958648)) ;
#101993 = CARTESIAN_POINT('Ctrl Pts',(-20.4895305931583,-50.2706236194241,
123.987809674307)) ;
#101994 = CARTESIAN_POINT('Ctrl Pts',(-20.6208573380819,-50.2904321151846,
123.587584399104)) ;
#101995 = CARTESIAN_POINT('Ctrl Pts',(-20.6081416123269,-50.3104147542902,
123.162980355193)) ;
#101996 = CARTESIAN_POINT('Ctrl Pts',(-20.4519151805266,-50.3302962020842,
122.770059283655)) ;
#101997 = CARTESIAN_POINT('Ctrl Pts',(-20.1703063924428,-50.3502526688217,
122.452767715121)) ;
#101998 = CARTESIAN_POINT('Ctrl Pts',(-19.7988013184218,-50.3701300657773,
122.251091794787)) ;
#101999 = CARTESIAN_POINT('Ctrl Pts',(-19.3787230745867,-50.3901120119526,
122.18774884429)) ;
#102000 = CARTESIAN_POINT('Ctrl Pts',(-18.963260532602,-50.4100411109893,
122.271572679674)) ;
#102001 = CARTESIAN_POINT('Ctrl Pts',(-18.6014589160847,-50.429969734202,
122.491986589679)) ;
#102002 = CARTESIAN_POINT('Ctrl Pts',(-18.3371530683495,-50.4498040583084,
122.820679049951)) ;
#102003 = CARTESIAN_POINT('Ctrl Pts',(-18.2224316258116,-50.4664563456918,
123.155550447963)) ;
#102004 = CARTESIAN_POINT('Ctrl Pts',(-18.2035149014984,-50.479716846714,
123.433758221571)) ;
#102005 = CARTESIAN_POINT('Ctrl Pts',(-18.2255027679537,-50.4897183239153,
123.642859688652)) ;
#102006 = CARTESIAN_POINT('Ctrl Pts',(-18.2839836386085,-50.4997503447748,
123.845501820851)) ;
#102007 = CARTESIAN_POINT('Ctrl Pts',(-18.3749684273573,-50.5096138885003,
124.031828626232)) ;
#102008 = CARTESIAN_POINT('Ctrl Pts',(-18.4977894936302,-50.5195826021705,
124.20165651461)) ;
#102009 = CARTESIAN_POINT('Ctrl Pts',(-18.6994117871218,-50.5329283495742,
124.396673257993)) ;
#102010 = CARTESIAN_POINT('Ctrl Pts',(-18.9435599678376,-50.5460789046468,
124.53307891713)) ;
#102011 = CARTESIAN_POINT('Ctrl Pts',(-19.2163065693772,-50.5594642851967,
124.602308367246)) ;
#102012 = CARTESIAN_POINT('Ctrl Pts',(-19.4236344332824,-50.5693522211896,
124.617685595469)) ;
#102013 = CARTESIAN_POINT('Ctrl Pts',(-19.6326291072843,-50.5793434110022,
124.596970031062)) ;
#102014 = CARTESIAN_POINT('Ctrl Pts',(-19.8341418602987,-50.5892955095405,
124.540573362922)) ;
#102015 = CARTESIAN_POINT('Ctrl Pts',(-20.0244847379365,-50.599341765991,
124.449083602029)) ;
#102016 = CARTESIAN_POINT('Ctrl Pts',(-20.1927929130173,-50.6091912133851,
124.328458293378)) ;
#102017 = CARTESIAN_POINT('Ctrl Pts',(-20.3397272912523,-50.6191538658803,
124.179209308823)) ;
#102018 = CARTESIAN_POINT('Ctrl Pts',(-20.4590067251318,-50.6291769515224,
124.005502955567)) ;
#102019 = CARTESIAN_POINT('Ctrl Pts',(-20.5456866388958,-50.6391020672793,
123.815676391373)) ;
#102020 = CARTESIAN_POINT('Ctrl Pts',(-20.5986692436396,-50.6491545456791,
123.611111447688)) ;
#102021 = CARTESIAN_POINT('Ctrl Pts',(-20.6151364585024,-50.6590060443818,
123.404642114603)) ;
#102022 = CARTESIAN_POINT('Ctrl Pts',(-20.5958123645779,-50.6689777835844,
123.195923961633)) ;
#102023 = CARTESIAN_POINT('Ctrl Pts',(-20.5403702466921,-50.6789729913501,
122.993203998571)) ;
#102024 = CARTESIAN_POINT('Ctrl Pts',(-20.4500128315109,-50.6890069928191,
122.80260998835)) ;
#102025 = CARTESIAN_POINT('Ctrl Pts',(-20.3303547593317,-50.6988623509115,
122.633439919841)) ;
#102026 = CARTESIAN_POINT('Ctrl Pts',(-20.1812288288997,-50.7088618265048,
122.485324053884)) ;
#102027 = CARTESIAN_POINT('Ctrl Pts',(-20.0105355329586,-50.7187562749999,
122.366373216032)) ;
#102028 = CARTESIAN_POINT('Ctrl Pts',(-19.8186064059258,-50.7288193992276,
122.277464208325)) ;
#102029 = CARTESIAN_POINT('Ctrl Pts',(-19.6186870520123,-50.7386590255562,
122.224196940968)) ;
#102030 = CARTESIAN_POINT('Ctrl Pts',(-19.4079577461664,-50.7487222605992,
122.205785639971)) ;
#102031 = CARTESIAN_POINT('Ctrl Pts',(-19.2007413999684,-50.7586162658332,
122.224113081246)) ;
#102032 = CARTESIAN_POINT('Ctrl Pts',(-18.9987616391661,-50.768558979049,
122.277841963926)) ;
#102033 = CARTESIAN_POINT('Ctrl Pts',(-18.807918462245,-50.7785647188472,
122.366364665763)) ;
#102034 = CARTESIAN_POINT('Ctrl Pts',(-18.6352410465518,-50.7885856209936,
122.487041094652)) ;
#102035 = CARTESIAN_POINT('Ctrl Pts',(-18.4878996354826,-50.7984763910424,
122.633772704868)) ;
#102036 = CARTESIAN_POINT('Ctrl Pts',(-18.3668077090979,-50.8084678018222,
122.805397863477)) ;
#102037 = CARTESIAN_POINT('Ctrl Pts',(-18.2778017586643,-50.8184161474867,
122.994654354273)) ;
#102038 = CARTESIAN_POINT('Ctrl Pts',(-18.2225965537156,-50.8283610055478,
123.196325632193)) ;
#102039 = CARTESIAN_POINT('Ctrl Pts',(-18.2033457854986,-50.8384158409408,
123.406811658352)) ;
#102040 = CARTESIAN_POINT('Ctrl Pts',(-18.2201734183687,-50.8482382130423,
123.612639952035)) ;
#102041 = CARTESIAN_POINT('Ctrl Pts',(-18.2733507417294,-50.858294080486,
123.817232751486)) ;
#102042 = CARTESIAN_POINT('Ctrl Pts',(-18.3605863395091,-50.8682348103439,
124.007149029114)) ;
#102043 = CARTESIAN_POINT('Ctrl Pts',(-18.478497718122,-50.878139148895,124.178771170214)) ;
#102044 = CARTESIAN_POINT('Ctrl Pts',(-18.6265953149911,-50.8881858303235,
124.329338290249)) ;
#102045 = CARTESIAN_POINT('Ctrl Pts',(-18.7959297863534,-50.8980813377928,
124.450244709797)) ;
#102046 = CARTESIAN_POINT('Ctrl Pts',(-18.9867919194371,-50.9081436062914,
124.541392395806)) ;
#102047 = CARTESIAN_POINT('Ctrl Pts',(-19.1861395279081,-50.917985596562,
124.596914462037)) ;
#102048 = CARTESIAN_POINT('Ctrl Pts',(-19.3951643337285,-50.9279790134429,
124.617752496104)) ;
#102049 = CARTESIAN_POINT('Ctrl Pts',(-19.6032428232147,-50.9379035012951,
124.602103510427)) ;
#102050 = CARTESIAN_POINT('Ctrl Pts',(-19.8069911079487,-50.9479031352036,
124.550396917399)) ;
#102051 = CARTESIAN_POINT('Ctrl Pts',(-19.998454678653,-50.9578892454603,
124.464201494283)) ;
#102052 = CARTESIAN_POINT('Ctrl Pts',(-20.1727426665322,-50.9679251966475,
124.34532767104)) ;
#102053 = CARTESIAN_POINT('Ctrl Pts',(-20.3212911797634,-50.9777818349823,
124.200825586121)) ;
#102054 = CARTESIAN_POINT('Ctrl Pts',(-20.4444414948792,-50.9877807950603,
124.030511604769)) ;
#102055 = CARTESIAN_POINT('Ctrl Pts',(-20.5354314494611,-50.9976760253741,
123.84339872265)) ;
#102056 = CARTESIAN_POINT('Ctrl Pts',(-20.5934652650774,-51.0077365378427,
123.640040870586)) ;
#102057 = CARTESIAN_POINT('Ctrl Pts',(-20.614970259188,-51.0175858293889,
123.434081676763)) ;
#102058 = CARTESIAN_POINT('Ctrl Pts',(-20.6006581317941,-51.0276130153211,
123.223770241738)) ;
#102059 = CARTESIAN_POINT('Ctrl Pts',(-20.5494981611977,-51.0376415517804,
123.019229095173)) ;
#102060 = CARTESIAN_POINT('Ctrl Pts',(-20.4655381907311,-51.0474867917454,
122.830057877665)) ;
#102061 = CARTESIAN_POINT('Ctrl Pts',(-20.3487581853815,-51.0574774866686,
122.655473670631)) ;
#102062 = CARTESIAN_POINT('Ctrl Pts',(-20.2024196020518,-51.0675153074272,
122.503430996951)) ;
#102063 = CARTESIAN_POINT('Ctrl Pts',(-20.0353908014291,-51.0773599012041,
122.381213155737)) ;
#102064 = CARTESIAN_POINT('Ctrl Pts',(-19.8472666799473,-51.0873438965802,
122.28816811123)) ;
#102065 = CARTESIAN_POINT('Ctrl Pts',(-19.6465155323506,-51.0972929451416,
122.229421088796)) ;
#102066 = CARTESIAN_POINT('Ctrl Pts',(-19.4375248061682,-51.1072953841161,
122.206074791073)) ;
#102067 = CARTESIAN_POINT('Ctrl Pts',(-19.2272849531938,-51.1173166254125,
122.219680945119)) ;
#102068 = CARTESIAN_POINT('Ctrl Pts',(-19.0251689378841,-51.127209303852,
122.268701080517)) ;
#102069 = CARTESIAN_POINT('Ctrl Pts',(-18.8326264136303,-51.1371993577996,
122.352581654393)) ;
#102070 = CARTESIAN_POINT('Ctrl Pts',(-18.6582153237759,-51.1471577189481,
122.468373093087)) ;
#102071 = CARTESIAN_POINT('Ctrl Pts',(-18.5070856494194,-51.1570573458329,
122.611480249763)) ;
#102072 = CARTESIAN_POINT('Ctrl Pts',(-18.3813233676906,-51.1671052426363,
122.781175182277)) ;
#102073 = CARTESIAN_POINT('Ctrl Pts',(-18.288198729716,-51.1770006002723,
122.967235303232)) ;
#102074 = CARTESIAN_POINT('Ctrl Pts',(-18.2277834168476,-51.1870622527289,
123.169927335517)) ;
#102075 = CARTESIAN_POINT('Ctrl Pts',(-18.2039690787718,-51.1969068570009,
123.375523889867)) ;
#102076 = CARTESIAN_POINT('Ctrl Pts',(-18.2156084659759,-51.2068669786989,
123.584589498698)) ;
#102077 = CARTESIAN_POINT('Ctrl Pts',(-18.2641422937408,-51.2169050130614,
123.789955831444)) ;
#102078 = CARTESIAN_POINT('Ctrl Pts',(-18.3458993190265,-51.2267793256479,
123.980794969641)) ;
#102079 = CARTESIAN_POINT('Ctrl Pts',(-18.4617753637743,-51.2368488064306,
124.157922836002)) ;
#102080 = CARTESIAN_POINT('Ctrl Pts',(-18.6032126349684,-51.2466831424477,
124.308745786788)) ;
#102081 = CARTESIAN_POINT('Ctrl Pts',(-18.7716654500986,-51.2567161001759,
124.435671225097)) ;
#102082 = CARTESIAN_POINT('Ctrl Pts',(-18.9596341645194,-51.2667364987511,
124.530785280125)) ;
#102083 = CARTESIAN_POINT('Ctrl Pts',(-19.1580068644862,-51.2766020725223,
124.591379294679)) ;
#102084 = CARTESIAN_POINT('Ctrl Pts',(-19.3680927362869,-51.2866709471784,
124.617127792661)) ;
#102085 = CARTESIAN_POINT('Ctrl Pts',(-19.5748010403265,-51.2965163780839,
124.606284088444)) ;
#102086 = CARTESIAN_POINT('Ctrl Pts',(-19.7793703686397,-51.3064960029546,
124.559741980477)) ;
#102087 = CARTESIAN_POINT('Ctrl Pts',(-19.9733529321733,-51.3165146858687,
124.477700100303)) ;
#102088 = CARTESIAN_POINT('Ctrl Pts',(-20.1480190819141,-51.3263979510525,
124.365122934608)) ;
#102089 = CARTESIAN_POINT('Ctrl Pts',(-20.303232691421,-51.3364662451439,
124.221257989239)) ;
#102090 = CARTESIAN_POINT('Ctrl Pts',(-20.4283189597381,-51.3462963753292,
124.056709439705)) ;
#102091 = CARTESIAN_POINT('Ctrl Pts',(-20.5254218949366,-51.3563629235443,
123.868708523117)) ;
#102092 = CARTESIAN_POINT('Ctrl Pts',(-20.5871979362944,-51.366253172233,
123.670146959543)) ;
#102093 = CARTESIAN_POINT('Ctrl Pts',(-20.6142816479036,-51.376245354009,
123.461845393936)) ;
#102094 = CARTESIAN_POINT('Ctrl Pts',(-20.6046169410662,-51.3862081346368,
123.252623557076)) ;
#102095 = CARTESIAN_POINT('Ctrl Pts',(-20.5595449470191,-51.3961125393105,
123.049323775001)) ;
#102096 = CARTESIAN_POINT('Ctrl Pts',(-20.4784730118799,-51.4061725337896,
122.854007102506)) ;
#102097 = CARTESIAN_POINT('Ctrl Pts',(-20.3672413014276,-51.4160211557594,
122.679356127338)) ;
#102098 = CARTESIAN_POINT('Ctrl Pts',(-20.2251601330051,-51.4260515951712,
122.523552975167)) ;
#102099 = CARTESIAN_POINT('Ctrl Pts',(-20.0582426570691,-51.436061310806,
122.395367401154)) ;
#102100 = CARTESIAN_POINT('Ctrl Pts',(-19.8735803225241,-51.4459720634986,
122.298912809156)) ;
#102101 = CARTESIAN_POINT('Ctrl Pts',(-19.6747349994522,-51.455901336445,
122.235360610812)) ;
#102102 = CARTESIAN_POINT('Ctrl Pts',(-19.4655065157872,-51.4659440278377,
122.207159118173)) ;
#102103 = CARTESIAN_POINT('Ctrl Pts',(-19.2578143892482,-51.4758305610552,
122.2154470542)) ;
#102104 = CARTESIAN_POINT('Ctrl Pts',(-19.0524729011174,-51.4858237059872,
122.259795140594)) ;
#102105 = CARTESIAN_POINT('Ctrl Pts',(-18.8588941425312,-51.4957693868237,
122.338825303902)) ;
#102106 = CARTESIAN_POINT('Ctrl Pts',(-18.6817137252205,-51.5057166439722,
122.449927378614)) ;
#102107 = CARTESIAN_POINT('Ctrl Pts',(-18.5251170857329,-51.5157645478442,
122.591689247072)) ;
#102108 = CARTESIAN_POINT('Ctrl Pts',(-18.3979544915207,-51.5256122469422,
122.755063008501)) ;
#102109 = CARTESIAN_POINT('Ctrl Pts',(-18.2993913118745,-51.5355737379209,
122.939831355835)) ;
#102110 = CARTESIAN_POINT('Ctrl Pts',(-18.2342270421431,-51.5456032003348,
123.14036892592)) ;
#102111 = CARTESIAN_POINT('Ctrl Pts',(-18.2051196470328,-51.5555104314347,
123.346606085303)) ;
#102112 = CARTESIAN_POINT('Ctrl Pts',(-18.2118665891129,-51.5654568101121,
123.555588738738)) ;
#102113 = CARTESIAN_POINT('Ctrl Pts',(-18.2549824721114,-51.575461578921,
123.761472421174)) ;
#102114 = CARTESIAN_POINT('Ctrl Pts',(-18.3335348311947,-51.5854826999412,
123.956951382704)) ;
#102115 = CARTESIAN_POINT('Ctrl Pts',(-18.4431917309961,-51.5953735657938,
124.133632047018)) ;
#102116 = CARTESIAN_POINT('Ctrl Pts',(-18.5830178539678,-51.6053643745531,
124.290347294295)) ;
#102117 = CARTESIAN_POINT('Ctrl Pts',(-18.7473101565169,-51.6153150327334,
124.419863418094)) ;
#102118 = CARTESIAN_POINT('Ctrl Pts',(-18.9311712702313,-51.6252512423755,
124.51897610134)) ;
#102119 = CARTESIAN_POINT('Ctrl Pts',(-19.1303407973497,-51.6352344091004,
124.585241151628)) ;
#102120 = CARTESIAN_POINT('Ctrl Pts',(-19.3392592333053,-51.6452782063107,
124.615709669033)) ;
#102121 = CARTESIAN_POINT('Ctrl Pts',(-19.5458329737632,-51.655106422479,
124.610062204838)) ;
#102122 = CARTESIAN_POINT('Ctrl Pts',(-19.7533510421833,-51.6651829899482,
124.56769906022)) ;
#102123 = CARTESIAN_POINT('Ctrl Pts',(-19.9460915495877,-51.6750350756376,
124.491744734315)) ;
#102124 = CARTESIAN_POINT('Ctrl Pts',(-20.126707254599,-51.685108343043,124.381242661317)) ;
#102125 = CARTESIAN_POINT('Ctrl Pts',(-20.2817384700001,-51.6949497594666,
124.244210900931)) ;
#102126 = CARTESIAN_POINT('Ctrl Pts',(-20.4127892408676,-51.7049110176093,
124.080877679363)) ;
#102127 = CARTESIAN_POINT('Ctrl Pts',(-20.5138960237252,-51.7149476940412,
123.89568099744)) ;
#102128 = CARTESIAN_POINT('Ctrl Pts',(-20.5805895006266,-51.7248263019051,
123.698978774304)) ;
#102129 = CARTESIAN_POINT('Ctrl Pts',(-20.6127348924034,-51.7348865305439,
123.489965838378)) ;
#102130 = CARTESIAN_POINT('Ctrl Pts',(-20.6082491346055,-51.7447535147047,
123.282553117729)) ;
#102131 = CARTESIAN_POINT('Ctrl Pts',(-20.5676589598846,-51.7547590809574,
123.076186453255)) ;
#102132 = CARTESIAN_POINT('Ctrl Pts',(-20.4919451996094,-51.764742869372,
122.880388015478)) ;
#102133 = CARTESIAN_POINT('Ctrl Pts',(-20.3825404235404,-51.7747887261746,
122.699758465771)) ;
#102134 = CARTESIAN_POINT('Ctrl Pts',(-20.2466721692149,-51.7846146033906,
122.544158497217)) ;
#102135 = CARTESIAN_POINT('Ctrl Pts',(-20.083588298045,-51.7946050792319,
122.411807486237)) ;
#102136 = CARTESIAN_POINT('Ctrl Pts',(-19.8987560089923,-51.8046486551307,
122.309726601717)) ;
#102137 = CARTESIAN_POINT('Ctrl Pts',(-19.7035602780868,-51.8144704474287,
122.242391813111)) ;
#102138 = CARTESIAN_POINT('Ctrl Pts',(-19.4952918878439,-51.8245054130546,
122.20875796636)) ;
#102139 = CARTESIAN_POINT('Ctrl Pts',(-19.2845620898213,-51.8345303299877,
122.212381313062)) ;
#102140 = CARTESIAN_POINT('Ctrl Pts',(-19.0811479953115,-51.8443822683638,
122.251400968217)) ;
#102141 = CARTESIAN_POINT('Ctrl Pts',(-18.8847815800089,-51.8543732443885,
122.325877502438)) ;
#102142 = CARTESIAN_POINT('Ctrl Pts',(-18.7055334640367,-51.8642910651922,
122.432438652557)) ;
#102143 = CARTESIAN_POINT('Ctrl Pts',(-18.5457589506594,-51.8743197857568,
122.5699675086)) ;
#102144 = CARTESIAN_POINT('Ctrl Pts',(-18.4140946707182,-51.8842027123659,
122.730718621091)) ;
#102145 = CARTESIAN_POINT('Ctrl Pts',(-18.3108219248006,-51.8942069974854,
122.913912181594)) ;
#102146 = CARTESIAN_POINT('Ctrl Pts',(-18.241073010289,-51.9041906786933,
123.111910056774)) ;
#102147 = CARTESIAN_POINT('Ctrl Pts',(-18.2068130643359,-51.9142316774232,
123.320189019648)) ;
#102148 = CARTESIAN_POINT('Ctrl Pts',(-18.2088961340705,-51.9240641222903,
123.526889580222)) ;
#102149 = CARTESIAN_POINT('Ctrl Pts',(-18.2468544333764,-51.9340591207207,
123.733553097656)) ;
#102150 = CARTESIAN_POINT('Ctrl Pts',(-18.3208167264393,-51.9440906694703,
123.931064859094)) ;
#102151 = CARTESIAN_POINT('Ctrl Pts',(-18.4259390709663,-51.9539560477758,
124.109838075707)) ;
#102152 = CARTESIAN_POINT('Ctrl Pts',(-18.5613822040534,-51.9639178952361,
124.269583193252)) ;
#102153 = CARTESIAN_POINT('Ctrl Pts',(-18.7238931720494,-51.9739528360503,
124.404089900933)) ;
#102154 = CARTESIAN_POINT('Ctrl Pts',(-18.9044114673504,-51.9838377970674,
124.507102309934)) ;
#102155 = CARTESIAN_POINT('Ctrl Pts',(-19.103605135228,-51.9939034059863,
124.578422044445)) ;
#102156 = CARTESIAN_POINT('Ctrl Pts',(-19.3074948086145,-52.003742581028,
124.613485807135)) ;
#102157 = CARTESIAN_POINT('Ctrl Pts',(-19.5190160672945,-52.0138051365279,
124.612887341402)) ;
#102158 = CARTESIAN_POINT('Ctrl Pts',(-19.7237939408024,-52.0237023112208,
124.575955886498)) ;
#102159 = CARTESIAN_POINT('Ctrl Pts',(-19.9199374574091,-52.0336330261442,
124.504449575194)) ;
#102160 = CARTESIAN_POINT('Ctrl Pts',(-20.1026258926737,-52.0436770542218,
124.398570256907)) ;
#102161 = CARTESIAN_POINT('Ctrl Pts',(-20.2617358029847,-52.0535632560751,
124.264827964775)) ;
#102162 = CARTESIAN_POINT('Ctrl Pts',(-20.3968709393118,-52.0635564225419,
124.103998749421)) ;
#102163 = CARTESIAN_POINT('Ctrl Pts',(-20.5015409355508,-52.0734958935291,
123.923114785567)) ;
#102164 = CARTESIAN_POINT('Ctrl Pts',(-20.5737915722018,-52.0835124078833,
123.72534197188)) ;
#102165 = CARTESIAN_POINT('Ctrl Pts',(-20.6104698817285,-52.0934424343601,
123.519799387467)) ;
#102166 = CARTESIAN_POINT('Ctrl Pts',(-20.6108142900536,-52.1034949698696,
123.308481580809)) ;
#102167 = CARTESIAN_POINT('Ctrl Pts',(-20.5753196661961,-52.1133413730892,
123.104537857884)) ;
#102168 = CARTESIAN_POINT('Ctrl Pts',(-20.5047695948295,-52.1233034159433,
122.907357380255)) ;
#102169 = CARTESIAN_POINT('Ctrl Pts',(-20.4001109988085,-52.133331966734,
122.724320605523)) ;
#102170 = CARTESIAN_POINT('Ctrl Pts',(-20.2669195312031,-52.1432422924516,
122.56412000491)) ;
#102171 = CARTESIAN_POINT('Ctrl Pts',(-20.1078817823875,-52.1531772042812,
122.428718692706)) ;
#102172 = CARTESIAN_POINT('Ctrl Pts',(-19.9257386476305,-52.1632182110493,
122.322032737042)) ;
#102173 = CARTESIAN_POINT('Ctrl Pts',(-19.7308938872218,-52.1731058438815,
122.249579702083)) ;
#102174 = CARTESIAN_POINT('Ctrl Pts',(-19.5243909407752,-52.1830962749795,
122.211305885879)) ;
#102175 = CARTESIAN_POINT('Ctrl Pts',(-19.3150968897901,-52.1930517115367,
122.209588118598)) ;
#102176 = CARTESIAN_POINT('Ctrl Pts',(-19.1095609115323,-52.2029626596361,
122.243702264415)) ;
#102177 = CARTESIAN_POINT('Ctrl Pts',(-18.9109542558379,-52.2129747357338,
122.313473083761)) ;
#102178 = CARTESIAN_POINT('Ctrl Pts',(-18.7274412402899,-52.2230020578087,
122.417177689973)) ;
#102179 = CARTESIAN_POINT('Ctrl Pts',(-18.5670835694196,-52.2328608327629,
122.548549354065)) ;
#102180 = CARTESIAN_POINT('Ctrl Pts',(-18.3833390570059,-52.2462870255753,
122.762733894525)) ;
#102181 = CARTESIAN_POINT('Ctrl Pts',(-18.2623738099514,-52.2593710413567,
123.013407906189)) ;
#102182 = CARTESIAN_POINT('Ctrl Pts',(-18.2092235991671,-52.272844490112,
123.291528344292)) ;
#102183 = CARTESIAN_POINT('Ctrl Pts',(-18.2065462370895,-52.2826774479178,
123.498266675928)) ;
#102184 = CARTESIAN_POINT('Ctrl Pts',(-18.239364408563,-52.2926407213685,
123.70512299166)) ;
#102185 = CARTESIAN_POINT('Ctrl Pts',(-18.3085412102281,-52.3026777951864,
123.90447006399)) ;
#102186 = CARTESIAN_POINT('Ctrl Pts',(-18.4092917220299,-52.3125527981981,
124.086015895857)) ;
#102187 = CARTESIAN_POINT('Ctrl Pts',(-18.5425574341044,-52.3226204778243,
124.250410221525)) ;
#102188 = CARTESIAN_POINT('Ctrl Pts',(-18.6987038841185,-52.332461328042,
124.386166026734)) ;
#102189 = CARTESIAN_POINT('Ctrl Pts',(-18.938701212114,-52.345797526518,124.531082088924)) ;
#102190 = CARTESIAN_POINT('Ctrl Pts',(-19.2087115734884,-52.3590150503324,
124.609244570226)) ;
#102191 = CARTESIAN_POINT('Ctrl Pts',(-19.4889265342999,-52.3723499768236,
124.615216461179)) ;
#102192 = CARTESIAN_POINT('Ctrl Pts',(-19.6963982415141,-52.3823330774182,
124.583256156928)) ;
#102193 = CARTESIAN_POINT('Ctrl Pts',(-19.8962330506336,-52.3923778533179,
124.515063127718)) ;
#102194 = CARTESIAN_POINT('Ctrl Pts',(-20.0772449601357,-52.4021957765038,
124.415851656627)) ;
#102195 = CARTESIAN_POINT('Ctrl Pts',(-20.2423282994893,-52.4122450904591,
124.284027825347)) ;
#102196 = CARTESIAN_POINT('Ctrl Pts',(-20.4268318377913,-52.4255488310817,
124.073827185627)) ;
#102197 = CARTESIAN_POINT('Ctrl Pts',(-20.5831621499422,-52.4420390265583,
123.759945797716)) ;
#102198 = CARTESIAN_POINT('Ctrl Pts',(-20.6234000199876,-52.458758191483,
123.406774910232)) ;
#102199 = CARTESIAN_POINT('Ctrl Pts',(-20.5824850850059,-52.4719191851531,
123.133123312395)) ;
#102200 = CARTESIAN_POINT('Ctrl Pts',(-20.516524888799,-52.4819154072584,
122.933597870408)) ;
#102201 = CARTESIAN_POINT('Ctrl Pts',(-20.4162230211807,-52.4919392467921,
122.748268444864)) ;
#102202 = CARTESIAN_POINT('Ctrl Pts',(-20.244314280652,-52.5051325687854,
122.530558822818)) ;
#102203 = CARTESIAN_POINT('Ctrl Pts',(-19.9606378567155,-52.5217917405627,
122.318506473547)) ;
#102204 = CARTESIAN_POINT('Ctrl Pts',(-19.5552839467014,-52.5417019160484,
122.196345922876)) ;
#102205 = CARTESIAN_POINT('Ctrl Pts',(-19.1329275440602,-52.5615919038928,
122.218941373271)) ;
#102206 = CARTESIAN_POINT('Ctrl Pts',(-18.7416359261934,-52.5815973519076,
122.385574891021)) ;
#102207 = CARTESIAN_POINT('Ctrl Pts',(-18.4328880468011,-52.6014337459349,
122.673091141756)) ;
#102208 = CARTESIAN_POINT('Ctrl Pts',(-18.2390833714217,-52.6214415398316,
123.051672742097)) ;
#102209 = CARTESIAN_POINT('Ctrl Pts',(-18.186411953331,-52.6412681761255,
123.470015012187)) ;
#102210 = CARTESIAN_POINT('Ctrl Pts',(-18.279604067918,-52.6612471190794,
123.884456805157)) ;
#102211 = CARTESIAN_POINT('Ctrl Pts',(-18.5087021907737,-52.6811789209484,
124.240933840254)) ;
#102212 = CARTESIAN_POINT('Ctrl Pts',(-18.8431640592749,-52.701003221446,
124.497691087513)) ;
#102213 = CARTESIAN_POINT('Ctrl Pts',(-19.2506095800152,-52.7210992227858,
124.625832857422)) ;
#102214 = CARTESIAN_POINT('Ctrl Pts',(-19.6705944786595,-52.7408576388898,
124.60798982828)) ;
#102215 = CARTESIAN_POINT('Ctrl Pts',(-20.0654778238001,-52.7609513317739,
124.445491769014)) ;
#102216 = CARTESIAN_POINT('Ctrl Pts',(-20.2716335532994,-52.7740622976805,
124.257641744654)) ;
#102217 = CARTESIAN_POINT('Ctrl Pts',(-20.3578982754669,-52.7807756724684,
124.146632267721)) ;
#102218 = CARTESIAN_POINT('Ctrl Pts',(-17.9902032695621,-11.7999200508426,
123.897608969663)) ;
#102219 = CARTESIAN_POINT('Ctrl Pts',(-18.0463644113343,-11.8065469016607,
124.06174960631)) ;
#102220 = CARTESIAN_POINT('Ctrl Pts',(-18.215825846161,-11.8197775281417,
124.369882260699)) ;
#102221 = CARTESIAN_POINT('Ctrl Pts',(-18.6148423423544,-11.8397531494004,
124.720117056252)) ;
#102222 = CARTESIAN_POINT('Ctrl Pts',(-19.1081264048667,-11.8596704843023,
124.912158369366)) ;
#102223 = CARTESIAN_POINT('Ctrl Pts',(-19.63621175278,-11.8795437610183,124.925514984982)) ;
#102224 = CARTESIAN_POINT('Ctrl Pts',(-20.1407585698648,-11.8995682511823,
124.756261059837)) ;
#102225 = CARTESIAN_POINT('Ctrl Pts',(-20.5540259374414,-11.919436092333,
124.427422694935)) ;
#102226 = CARTESIAN_POINT('Ctrl Pts',(-20.8319874786041,-11.9393817432125,
123.976081276933)) ;
#102227 = CARTESIAN_POINT('Ctrl Pts',(-20.9388398779409,-11.9592871438295,
123.457931852337)) ;
#102228 = CARTESIAN_POINT('Ctrl Pts',(-20.863615478076,-11.9791613716459,
122.93508911423)) ;
#102229 = CARTESIAN_POINT('Ctrl Pts',(-20.613117221254,-11.9991471625235,
122.466658528729)) ;
#102230 = CARTESIAN_POINT('Ctrl Pts',(-20.2194522950349,-12.0190414051832,
122.113709218852)) ;
#102231 = CARTESIAN_POINT('Ctrl Pts',(-19.7297864118389,-12.0389201212553,
121.91511024488)) ;
#102232 = CARTESIAN_POINT('Ctrl Pts',(-19.1975736063229,-12.0589595710999,
121.896014807318)) ;
#102233 = CARTESIAN_POINT('Ctrl Pts',(-18.6950368718382,-12.0788227326378,
122.05828741974)) ;
#102234 = CARTESIAN_POINT('Ctrl Pts',(-18.2756725670237,-12.098802100652,
122.383766305065)) ;
#102235 = CARTESIAN_POINT('Ctrl Pts',(-17.9943094984244,-12.1186126811748,
122.828946957063)) ;
#102236 = CARTESIAN_POINT('Ctrl Pts',(-17.8800596440357,-12.1385936094604,
123.347467939146)) ;
#102237 = CARTESIAN_POINT('Ctrl Pts',(-17.9496692515209,-12.1584862813298,
123.871640709025)) ;
#102238 = CARTESIAN_POINT('Ctrl Pts',(-18.1935441283311,-12.1784126116169,
124.341758564742)) ;
#102239 = CARTESIAN_POINT('Ctrl Pts',(-18.5843886944494,-12.1983831657092,
124.700872483781)) ;
#102240 = CARTESIAN_POINT('Ctrl Pts',(-18.9897923054451,-12.2149150047968,
124.870323217842)) ;
#102241 = CARTESIAN_POINT('Ctrl Pts',(-19.3371476852066,-12.2282547436244,
124.917728259279)) ;
#102242 = CARTESIAN_POINT('Ctrl Pts',(-19.600561904579,-12.238286985843,124.907080238284)) ;
#102243 = CARTESIAN_POINT('Ctrl Pts',(-19.8537454249195,-12.2481446864865,
124.852220196248)) ;
#102244 = CARTESIAN_POINT('Ctrl Pts',(-20.0969791918245,-12.2581365511257,
124.753349389585)) ;
#102245 = CARTESIAN_POINT('Ctrl Pts',(-20.3177843724854,-12.2680591008858,
124.614668652868)) ;
#102246 = CARTESIAN_POINT('Ctrl Pts',(-20.5772027359822,-12.2813368743793,
124.381219928393)) ;
#102247 = CARTESIAN_POINT('Ctrl Pts',(-20.7701060086633,-12.2946842133199,
124.083600779959)) ;
#102248 = CARTESIAN_POINT('Ctrl Pts',(-20.8774610072183,-12.3078914451131,
123.753491686556)) ;
#102249 = CARTESIAN_POINT('Ctrl Pts',(-20.9145338769675,-12.3178785612028,
123.493715853778)) ;
#102250 = CARTESIAN_POINT('Ctrl Pts',(-20.9061360148182,-12.3278294667826,
123.23230208977)) ;
#102251 = CARTESIAN_POINT('Ctrl Pts',(-20.8516341650625,-12.33788456879,122.973783899849)) ;
#102252 = CARTESIAN_POINT('Ctrl Pts',(-20.7557577833189,-12.3477062421111,
122.734117231834)) ;
#102253 = CARTESIAN_POINT('Ctrl Pts',(-20.6168413508988,-12.357764713186,
122.509268747216)) ;
#102254 = CARTESIAN_POINT('Ctrl Pts',(-20.4430459892397,-12.3676893243625,
122.314784540958)) ;
#102255 = CARTESIAN_POINT('Ctrl Pts',(-20.1694463091453,-12.3809666632629,
122.098206721406)) ;
#102256 = CARTESIAN_POINT('Ctrl Pts',(-19.8449906513278,-12.3942655425005,
121.958127734837)) ;
#102257 = CARTESIAN_POINT('Ctrl Pts',(-19.5008114094801,-12.4075044146712,
121.90717382515)) ;
#102258 = CARTESIAN_POINT('Ctrl Pts',(-19.2379277204331,-12.4175110328078,
121.913961440906)) ;
#102259 = CARTESIAN_POINT('Ctrl Pts',(-18.9797053775943,-12.4275419778693,
121.966916880926)) ;
#102260 = CARTESIAN_POINT('Ctrl Pts',(-18.7386719801883,-12.4373981512211,
122.061779312103)) ;
#102261 = CARTESIAN_POINT('Ctrl Pts',(-18.5144450957222,-12.447397422184,
122.198699572919)) ;
#102262 = CARTESIAN_POINT('Ctrl Pts',(-18.3191930175226,-12.4572918739413,
122.370484946934)) ;
#102263 = CARTESIAN_POINT('Ctrl Pts',(-18.1540884055978,-12.4673551897507,
122.577006721768)) ;
#102264 = CARTESIAN_POINT('Ctrl Pts',(-18.0298693325494,-12.4771940464903,
122.803819660122)) ;
#102265 = CARTESIAN_POINT('Ctrl Pts',(-17.9447542096665,-12.4872601683079,
123.054234502604)) ;
#102266 = CARTESIAN_POINT('Ctrl Pts',(-17.9052530449946,-12.4971433960322,
123.310969073969)) ;
#102267 = CARTESIAN_POINT('Ctrl Pts',(-17.9104144562362,-12.5071328573109,
123.573404577314)) ;
#102268 = CARTESIAN_POINT('Ctrl Pts',(-17.9610348989325,-12.5170965677374,
123.830313519484)) ;
#102269 = CARTESIAN_POINT('Ctrl Pts',(-18.055535313053,-12.5270915704683,
124.075403882281)) ;
#102270 = CARTESIAN_POINT('Ctrl Pts',(-18.1920541401854,-12.5371279014786,
124.301051073442)) ;
#102271 = CARTESIAN_POINT('Ctrl Pts',(-18.3620887052775,-12.5469741308209,
124.496109020729)) ;
#102272 = CARTESIAN_POINT('Ctrl Pts',(-18.5659035124381,-12.5569596290961,
124.661323909438)) ;
#102273 = CARTESIAN_POINT('Ctrl Pts',(-18.794133205315,-12.5668945320791,
124.78820420773)) ;
#102274 = CARTESIAN_POINT('Ctrl Pts',(-19.0439677038418,-12.5769520351743,
124.874329341901)) ;
#102275 = CARTESIAN_POINT('Ctrl Pts',(-19.2988434093258,-12.5867736915449,
124.91519672569)) ;
#102276 = CARTESIAN_POINT('Ctrl Pts',(-19.5630599609083,-12.59682975421,124.911586781273)) ;
#102277 = CARTESIAN_POINT('Ctrl Pts',(-19.8196010841879,-12.6067704189132,
124.862254027796)) ;
#102278 = CARTESIAN_POINT('Ctrl Pts',(-20.0630721998832,-12.6166748228617,
124.770231291142)) ;
#102279 = CARTESIAN_POINT('Ctrl Pts',(-20.2899726794303,-12.6267213078553,
124.63529723127)) ;
#102280 = CARTESIAN_POINT('Ctrl Pts',(-20.4871951419804,-12.636617535667,
124.46572279971)) ;
#102281 = CARTESIAN_POINT('Ctrl Pts',(-20.6546905094441,-12.6466771192305,
124.261238010029)) ;
#102282 = CARTESIAN_POINT('Ctrl Pts',(-20.7815104793504,-12.6565291288993,
124.035511186315)) ;
#102283 = CARTESIAN_POINT('Ctrl Pts',(-20.8689934761397,-12.6664916603389,
123.788768205197)) ;
#102284 = CARTESIAN_POINT('Ctrl Pts',(-20.9122064367509,-12.6765232085783,
123.528706986233)) ;
#102285 = CARTESIAN_POINT('Ctrl Pts',(-20.9098929873906,-12.6864146197913,
123.268781131544)) ;
#102286 = CARTESIAN_POINT('Ctrl Pts',(-20.8623508858351,-12.6964308734993,
123.009883889903)) ;
#102287 = CARTESIAN_POINT('Ctrl Pts',(-20.769920509206,-12.706460976344,122.763045735835)) ;
#102288 = CARTESIAN_POINT('Ctrl Pts',(-20.6387698639911,-12.7163174252977,
122.539667034596)) ;
#102289 = CARTESIAN_POINT('Ctrl Pts',(-20.468686507231,-12.72631643607,122.339431415899)) ;
#102290 = CARTESIAN_POINT('Ctrl Pts',(-20.2686378940791,-12.736211652988,
122.173234495552)) ;
#102291 = CARTESIAN_POINT('Ctrl Pts',(-20.0390498000103,-12.7462721683453,
122.042207516489)) ;
#102292 = CARTESIAN_POINT('Ctrl Pts',(-19.7954221880598,-12.7561214617324,
121.954750952006)) ;
#102293 = CARTESIAN_POINT('Ctrl Pts',(-19.5358430756164,-12.7661486374124,
121.909479848498)) ;
#102294 = CARTESIAN_POINT('Ctrl Pts',(-19.2722925736252,-12.7761772130396,
121.910661435614)) ;
#102295 = CARTESIAN_POINT('Ctrl Pts',(-19.0176320504801,-12.7860223065854,
121.956236242395)) ;
#102296 = CARTESIAN_POINT('Ctrl Pts',(-18.7708959417052,-12.7960135480172,
122.046015059974)) ;
#102297 = CARTESIAN_POINT('Ctrl Pts',(-18.5427539301237,-12.8060493291605,
122.178333355514)) ;
#102298 = CARTESIAN_POINT('Ctrl Pts',(-18.344530793837,-12.8159015348902,
122.344872755127)) ;
#102299 = CARTESIAN_POINT('Ctrl Pts',(-18.1757936891155,-12.8258636290072,
122.545026044335)) ;
#102300 = CARTESIAN_POINT('Ctrl Pts',(-18.0438514585141,-12.8358861898343,
122.772976611802)) ;
#102301 = CARTESIAN_POINT('Ctrl Pts',(-17.9540972344567,-12.8458139614859,
123.017969138429)) ;
#102302 = CARTESIAN_POINT('Ctrl Pts',(-17.9077512439174,-12.8558563456107,
123.27775092553)) ;
#102303 = CARTESIAN_POINT('Ctrl Pts',(-17.9071170334874,-12.8657455696813,
123.537644244839)) ;
#102304 = CARTESIAN_POINT('Ctrl Pts',(-17.951578905651,-12.8757348178486,
123.796349682054)) ;
#102305 = CARTESIAN_POINT('Ctrl Pts',(-18.0402013685863,-12.8856933948906,
124.042581000348)) ;
#102306 = CARTESIAN_POINT('Ctrl Pts',(-18.1689146990719,-12.8955929639819,
124.268677154619)) ;
#102307 = CARTESIAN_POINT('Ctrl Pts',(-18.3374623673469,-12.9056408760659,
124.471898543285)) ;
#102308 = CARTESIAN_POINT('Ctrl Pts',(-18.5355994492501,-12.9155362303731,
124.640372901657)) ;
#102309 = CARTESIAN_POINT('Ctrl Pts',(-18.7636696514608,-12.9255978808643,
124.774091983327)) ;
#102310 = CARTESIAN_POINT('Ctrl Pts',(-19.0061700042819,-12.9354424963268,
124.864243378729)) ;
#102311 = CARTESIAN_POINT('Ctrl Pts',(-19.263440320499,-12.9454025752282,
124.912387637213)) ;
#102312 = CARTESIAN_POINT('Ctrl Pts',(-19.527213442044,-12.9554407695865,
124.914637912278)) ;
#102313 = CARTESIAN_POINT('Ctrl Pts',(-19.7832305957041,-12.9653144849861,
124.872237771651)) ;
#102314 = CARTESIAN_POINT('Ctrl Pts',(-20.0328289090505,-12.9753861945204,
124.784297245069)) ;
#102315 = CARTESIAN_POINT('Ctrl Pts',(-20.2580129538926,-12.9852186349729,
124.65754226709)) ;
#102316 = CARTESIAN_POINT('Ctrl Pts',(-20.4622619532301,-12.9952504558983,
124.49087643455)) ;
#102317 = CARTESIAN_POINT('Ctrl Pts',(-20.6337103450931,-13.0052708257839,
124.291008668358)) ;
#102318 = CARTESIAN_POINT('Ctrl Pts',(-20.7663859266914,-13.0151375969176,
124.068214529218)) ;
#102319 = CARTESIAN_POINT('Ctrl Pts',(-20.860238962856,-13.025208368107,123.82079438421)) ;
#102320 = CARTESIAN_POINT('Ctrl Pts',(-20.9086253549924,-13.0350515286286,
123.566676912894)) ;
#102321 = CARTESIAN_POINT('Ctrl Pts',(-20.913063221591,-13.045031761815,123.304452798709)) ;
#102322 = CARTESIAN_POINT('Ctrl Pts',(-20.871244216678,-13.0550502818502,
123.044526148757)) ;
#102323 = CARTESIAN_POINT('Ctrl Pts',(-20.7866033496793,-13.0649335902339,
122.798947963481)) ;
#102324 = CARTESIAN_POINT('Ctrl Pts',(-20.6581851562813,-13.0750018744047,
122.567668252138)) ;
#102325 = CARTESIAN_POINT('Ctrl Pts',(-20.4956824752415,-13.0848320010723,
122.366800045795)) ;
#102326 = CARTESIAN_POINT('Ctrl Pts',(-20.2963739380565,-13.0948985732789,
122.192919639631)) ;
#102327 = CARTESIAN_POINT('Ctrl Pts',(-20.0737240319191,-13.1047887295196,
122.058778426284)) ;
#102328 = CARTESIAN_POINT('Ctrl Pts',(-19.8289059210494,-13.114781257096,
121.963856125823)) ;
#102329 = CARTESIAN_POINT('Ctrl Pts',(-19.5720652391397,-13.1247427469703,
121.913259794537)) ;
#102330 = CARTESIAN_POINT('Ctrl Pts',(-19.3117143442224,-13.1346519688575,
121.907457127883)) ;
#102331 = CARTESIAN_POINT('Ctrl Pts',(-19.0507318169299,-13.1447005486678,
121.947593231427)) ;
#102332 = CARTESIAN_POINT('Ctrl Pts',(-18.8047453884644,-13.1545835231379,
122.030958261685)) ;
#102333 = CARTESIAN_POINT('Ctrl Pts',(-18.5741383843272,-13.1645784342806,
122.156672491579)) ;
#102334 = CARTESIAN_POINT('Ctrl Pts',(-18.3685451174446,-13.1745988208542,
122.321235274363)) ;
#102335 = CARTESIAN_POINT('Ctrl Pts',(-18.1964735381612,-13.1845089247113,
122.516696286049)) ;
#102336 = CARTESIAN_POINT('Ctrl Pts',(-18.0601155303138,-13.1944366369212,
122.739126636729)) ;
#102337 = CARTESIAN_POINT('Ctrl Pts',(-17.9635520490142,-13.2044797466884,
122.984738187644)) ;
#102338 = CARTESIAN_POINT('Ctrl Pts',(-17.9117515043607,-13.214366167144,
123.23934198587)) ;
#102339 = CARTESIAN_POINT('Ctrl Pts',(-17.9044262701095,-13.2243593447496,
123.501835598151)) ;
#102340 = CARTESIAN_POINT('Ctrl Pts',(-17.9427087756384,-13.2343050076535,
123.760379203083)) ;
#102341 = CARTESIAN_POINT('Ctrl Pts',(-18.0248121016097,-13.2442523038587,
124.008568584514)) ;
#102342 = CARTESIAN_POINT('Ctrl Pts',(-18.1502624018748,-13.2543000694366,
124.240900424645)) ;
#102343 = CARTESIAN_POINT('Ctrl Pts',(-18.3107346122859,-13.2641482826542,
124.443940073215)) ;
#102344 = CARTESIAN_POINT('Ctrl Pts',(-18.505634717484,-13.2741078554483,
124.618624665501)) ;
#102345 = CARTESIAN_POINT('Ctrl Pts',(-18.7298622874998,-13.2841444764808,
124.757486690818)) ;
#102346 = CARTESIAN_POINT('Ctrl Pts',(-18.9708689515076,-13.2940249912912,
124.854174107934)) ;
#102347 = CARTESIAN_POINT('Ctrl Pts',(-19.2293446499912,-13.3040776425982,
124.908560044492)) ;
#102348 = CARTESIAN_POINT('Ctrl Pts',(-19.4892871259414,-13.3139730408782,
124.917212832017)) ;
#102349 = CARTESIAN_POINT('Ctrl Pts',(-19.7507469643642,-13.3240231625843,
124.88015632989)) ;
#102350 = CARTESIAN_POINT('Ctrl Pts',(-19.9977291617165,-13.3339074421262,
124.799637378817)) ;
#102351 = CARTESIAN_POINT('Ctrl Pts',(-20.2297273479885,-13.3439022234181,
124.676550308236)) ;
#102352 = CARTESIAN_POINT('Ctrl Pts',(-20.4358283328775,-13.3538500686049,
124.515703848554)) ;
#102353 = CARTESIAN_POINT('Ctrl Pts',(-20.6109332605582,-13.3637870319923,
124.322011504396)) ;
#102354 = CARTESIAN_POINT('Ctrl Pts',(-20.750697973779,-13.3737699967295,
124.099960077421)) ;
#102355 = CARTESIAN_POINT('Ctrl Pts',(-20.8499157138425,-13.3838138481452,
123.855409348359)) ;
#102356 = CARTESIAN_POINT('Ctrl Pts',(-20.9045890531855,-13.3936420494799,
123.602946647312)) ;
#102357 = CARTESIAN_POINT('Ctrl Pts',(-20.9149711028211,-13.403718622078,
123.338403239339)) ;
#102358 = CARTESIAN_POINT('Ctrl Pts',(-20.8801719456267,-13.4135707020855,
123.081792606934)) ;
#102359 = CARTESIAN_POINT('Ctrl Pts',(-20.7998200890708,-13.4236439870896,
122.829613269708)) ;
#102360 = CARTESIAN_POINT('Ctrl Pts',(-20.6796429969365,-13.4334853388001,
122.600587873272)) ;
#102361 = CARTESIAN_POINT('Ctrl Pts',(-20.5203827330306,-13.4434468381966,
122.392848692112)) ;
#102362 = CARTESIAN_POINT('Ctrl Pts',(-20.3257020959426,-13.4534826143266,
122.214922798792)) ;
#102363 = CARTESIAN_POINT('Ctrl Pts',(-20.106509157136,-13.4633710409642,
122.075355463823)) ;
#102364 = CARTESIAN_POINT('Ctrl Pts',(-19.8635102674347,-13.4733863630391,
121.974225744482)) ;
#102365 = CARTESIAN_POINT('Ctrl Pts',(-19.6061332113171,-13.4834167119393,
121.917339791102)) ;
#102366 = CARTESIAN_POINT('Ctrl Pts',(-19.34772624537,-13.493260087546,121.905698547325)) ;
#102367 = CARTESIAN_POINT('Ctrl Pts',(-19.0862905181186,-13.5032895244431,
121.939151509404)) ;
#102368 = CARTESIAN_POINT('Ctrl Pts',(-18.834783896269,-13.513321402376,122.018199528681)) ;
#102369 = CARTESIAN_POINT('Ctrl Pts',(-18.6053189853568,-13.5231510254815,
122.136788620459)) ;
#102370 = CARTESIAN_POINT('Ctrl Pts',(-18.3960964023697,-13.5331404966346,
122.295352843074)) ;
#102371 = CARTESIAN_POINT('Ctrl Pts',(-18.2171108841806,-13.543184345397,
122.489332377545)) ;
#102372 = CARTESIAN_POINT('Ctrl Pts',(-18.0772280467266,-13.5530060509287,
122.706244029415)) ;
#102373 = CARTESIAN_POINT('Ctrl Pts',(-17.974363913469,-13.5630410907565,
122.949063789534)) ;
#102374 = CARTESIAN_POINT('Ctrl Pts',(-17.9159925554736,-13.573065797648,
123.205963898225)) ;
#102375 = CARTESIAN_POINT('Ctrl Pts',(-17.9027881139224,-13.5829185019887,
123.464545531986)) ;
#102376 = CARTESIAN_POINT('Ctrl Pts',(-17.934663913364,-13.5929066241964,
123.725061221392)) ;
#102377 = CARTESIAN_POINT('Ctrl Pts',(-18.0108264809125,-13.6028350943037,
123.974614154487)) ;
#102378 = CARTESIAN_POINT('Ctrl Pts',(-18.1294981550369,-13.6128240714709,
124.208771928652)) ;
#102379 = CARTESIAN_POINT('Ctrl Pts',(-18.2881434789744,-13.6228618787506,
124.419507237109)) ;
#102380 = CARTESIAN_POINT('Ctrl Pts',(-18.4770091475431,-13.6327081796139,
124.596377248716)) ;
#102381 = CARTESIAN_POINT('Ctrl Pts',(-18.6973442789797,-13.6427339229932,
124.740836596543)) ;
#102382 = CARTESIAN_POINT('Ctrl Pts',(-18.9398133035653,-13.6527647894322,
124.844267400033)) ;
#102383 = CARTESIAN_POINT('Ctrl Pts',(-19.1914704015603,-13.662602148231,
124.903374596811)) ;
#102384 = CARTESIAN_POINT('Ctrl Pts',(-19.4535935830303,-13.6725941091647,
124.918819329345)) ;
#102385 = CARTESIAN_POINT('Ctrl Pts',(-19.7154208059744,-13.6826264717213,
124.887866426181)) ;
#102386 = CARTESIAN_POINT('Ctrl Pts',(-19.9637570360245,-13.6924916322957,
124.813493884598)) ;
#102387 = CARTESIAN_POINT('Ctrl Pts',(-20.1980303243043,-13.7024535368734,
124.69664719285)) ;
#102388 = CARTESIAN_POINT('Ctrl Pts',(-20.4097244466647,-13.7124884669491,
124.539422352633)) ;
#102389 = CARTESIAN_POINT('Ctrl Pts',(-20.5885492429424,-13.7223734138028,
124.350956304226)) ;
#102390 = CARTESIAN_POINT('Ctrl Pts',(-20.7344600840413,-13.7324390901142,
124.130377299098)) ;
#102391 = CARTESIAN_POINT('Ctrl Pts',(-20.837759491418,-13.7422780097491,
123.893305056922)) ;
#102392 = CARTESIAN_POINT('Ctrl Pts',(-20.9000224691976,-13.7523415194835,
123.636319401091)) ;
#102393 = CARTESIAN_POINT('Ctrl Pts',(-20.9162263459812,-13.7622351326453,
123.376800328538)) ;
#102394 = CARTESIAN_POINT('Ctrl Pts',(-20.8876702021662,-13.7721791394587,
123.117082703603)) ;
#102395 = CARTESIAN_POINT('Ctrl Pts',(-20.8141299534446,-13.782180093813,
122.864725111302)) ;
#102396 = CARTESIAN_POINT('Ctrl Pts',(-20.697056137545,-13.7922188515053,
122.628344090505)) ;
#102397 = CARTESIAN_POINT('Ctrl Pts',(-20.5444882130351,-13.8020430356753,
122.420051830506)) ;
#102398 = CARTESIAN_POINT('Ctrl Pts',(-20.3539349773995,-13.8121011012747,
122.236913035828)) ;
#102399 = CARTESIAN_POINT('Ctrl Pts',(-20.1370466125606,-13.8220311480494,
122.091780837515)) ;
#102400 = CARTESIAN_POINT('Ctrl Pts',(-19.8980293610127,-13.8319825903865,
121.9856600342)) ;
#102401 = CARTESIAN_POINT('Ctrl Pts',(-19.6417039464166,-13.8420293875658,
121.922400808479)) ;
#102402 = CARTESIAN_POINT('Ctrl Pts',(-19.3835149611134,-13.8518773282459,
121.904719817845)) ;
#102403 = CARTESIAN_POINT('Ctrl Pts',(-19.1231332375772,-13.8618389595885,
121.931644427789)) ;
#102404 = CARTESIAN_POINT('Ctrl Pts',(-18.8697526821085,-13.8718676189644,
122.004180140349)) ;
#102405 = CARTESIAN_POINT('Ctrl Pts',(-18.6355992228795,-13.8817779218526,
122.118159162644)) ;
#102406 = CARTESIAN_POINT('Ctrl Pts',(-18.4238530398286,-13.8917128164148,
122.270900422556)) ;
#102407 = CARTESIAN_POINT('Ctrl Pts',(-18.2400856096355,-13.9017539150817,
122.460247612701)) ;
#102408 = CARTESIAN_POINT('Ctrl Pts',(-18.0940931471758,-13.9116411975861,
122.675199141709)) ;
#102409 = CARTESIAN_POINT('Ctrl Pts',(-17.9861233201671,-13.9216329380966,
122.914527586321)) ;
#102410 = CARTESIAN_POINT('Ctrl Pts',(-17.9216953674469,-13.931583487332,
123.167969398232)) ;
#102411 = CARTESIAN_POINT('Ctrl Pts',(-17.9018949026966,-13.9415191649668,
123.42830067272)) ;
#102412 = CARTESIAN_POINT('Ctrl Pts',(-17.9274500776535,-13.9515045827596,
123.689479910381)) ;
#102413 = CARTESIAN_POINT('Ctrl Pts',(-17.9985820584167,-13.9615333756301,
123.943243286239)) ;
#102414 = CARTESIAN_POINT('Ctrl Pts',(-18.1107467629068,-13.9714128868581,
124.17738299688)) ;
#102415 = CARTESIAN_POINT('Ctrl Pts',(-18.2631231043819,-13.981406423531,
124.391289132976)) ;
#102416 = CARTESIAN_POINT('Ctrl Pts',(-18.4514209232036,-13.9914386917948,
124.575796061507)) ;
#102417 = CARTESIAN_POINT('Ctrl Pts',(-18.6649638633447,-14.0013026538007,
124.722784990796)) ;
#102418 = CARTESIAN_POINT('Ctrl Pts',(-18.9056437592007,-14.0113727151456,
124.832730221074)) ;
#102419 = CARTESIAN_POINT('Ctrl Pts',(-19.1560068384201,-14.0212150794943,
124.897711370076)) ;
#102420 = CARTESIAN_POINT('Ctrl Pts',(-19.4168544379476,-14.0311757519968,
124.919442596206)) ;
#102421 = CARTESIAN_POINT('Ctrl Pts',(-19.6794838048793,-14.0412138230646,
124.894842525918)) ;
#102422 = CARTESIAN_POINT('Ctrl Pts',(-19.9298640848764,-14.051087438025,
124.826625554233)) ;
#102423 = CARTESIAN_POINT('Ctrl Pts',(-20.1692084064,-14.0611596726063,124.713720144365)) ;
#102424 = CARTESIAN_POINT('Ctrl Pts',(-20.3802392463019,-14.0709836910551,
124.564918211062)) ;
#102425 = CARTESIAN_POINT('Ctrl Pts',(-20.5668561717494,-14.0810486120311,
124.377563316902)) ;
#102426 = CARTESIAN_POINT('Ctrl Pts',(-20.7654766766846,-14.0942589103259,
124.0927478502)) ;
#102427 = CARTESIAN_POINT('Ctrl Pts',(-20.8864738113405,-14.1075743570578,
123.760309528833)) ;
#102428 = CARTESIAN_POINT('Ctrl Pts',(-20.9168468780944,-14.1208646023251,
123.412265267831)) ;
#102429 = CARTESIAN_POINT('Ctrl Pts',(-20.8936192942763,-14.1309153519322,
123.149220731085)) ;
#102430 = CARTESIAN_POINT('Ctrl Pts',(-20.8271655478931,-14.1407279589144,
122.900025043608)) ;
#102431 = CARTESIAN_POINT('Ctrl Pts',(-20.7159396250951,-14.1507990569087,
122.659911955936)) ;
#102432 = CARTESIAN_POINT('Ctrl Pts',(-20.56718818496,-14.1606886296836,122.446781682834)) ;
#102433 = CARTESIAN_POINT('Ctrl Pts',(-20.3217392336305,-14.1739587364869,
122.199053239677)) ;
#102434 = CARTESIAN_POINT('Ctrl Pts',(-19.9402855601747,-14.1905754234094,
121.976506432685)) ;
#102435 = CARTESIAN_POINT('Ctrl Pts',(-19.5069617032543,-14.2071494667256,
121.897358315389)) ;
#102436 = CARTESIAN_POINT('Ctrl Pts',(-19.1586307174601,-14.2204460341574,
121.925257438203)) ;
#102437 = CARTESIAN_POINT('Ctrl Pts',(-18.9035554294054,-14.2304760977348,
121.991681270408)) ;
#102438 = CARTESIAN_POINT('Ctrl Pts',(-18.6671524907511,-14.240369989584,
122.099857115475)) ;
#102439 = CARTESIAN_POINT('Ctrl Pts',(-18.379673843965,-14.2536227453696,
122.296566106968)) ;
#102440 = CARTESIAN_POINT('Ctrl Pts',(-18.0908336692114,-14.270350850362,
122.63447857022)) ;
#102441 = CARTESIAN_POINT('Ctrl Pts',(-17.9056126156248,-14.2901816868405,
123.128030955025)) ;
#102442 = CARTESIAN_POINT('Ctrl Pts',(-17.8986114852488,-14.3101070787307,
123.657451709172)) ;
#102443 = CARTESIAN_POINT('Ctrl Pts',(-18.0728191190956,-14.3300322920827,
124.157646493931)) ;
#102444 = CARTESIAN_POINT('Ctrl Pts',(-18.4070617662362,-14.3499573055678,
124.56833572685)) ;
#102445 = CARTESIAN_POINT('Ctrl Pts',(-18.8599856109715,-14.3698337772678,
124.840324566468)) ;
#102446 = CARTESIAN_POINT('Ctrl Pts',(-19.3811370011753,-14.3898130951767,
124.942174609197)) ;
#102447 = CARTESIAN_POINT('Ctrl Pts',(-19.9045318981702,-14.4097460987527,
124.859860883971)) ;
#102448 = CARTESIAN_POINT('Ctrl Pts',(-20.3677488802651,-14.4296413687804,
124.604895458802)) ;
#102449 = CARTESIAN_POINT('Ctrl Pts',(-20.7170554974423,-14.4495627066862,
124.206961263789)) ;
#102450 = CARTESIAN_POINT('Ctrl Pts',(-20.9098459944052,-14.4695203299524,
123.712767673844)) ;
#102451 = CARTESIAN_POINT('Ctrl Pts',(-20.922491622849,-14.4894001619096,
123.184628566672)) ;
#102452 = CARTESIAN_POINT('Ctrl Pts',(-20.755460182351,-14.5092820132065,
122.683188642338)) ;
#102453 = CARTESIAN_POINT('Ctrl Pts',(-20.423531062275,-14.5293530303103,
122.265665610548)) ;
#102454 = CARTESIAN_POINT('Ctrl Pts',(-19.974929403366,-14.5491602540634,
121.989985430984)) ;
#102455 = CARTESIAN_POINT('Ctrl Pts',(-19.4550455765242,-14.5691413896322,
121.881815479055)) ;
#102456 = CARTESIAN_POINT('Ctrl Pts',(-18.9310151634136,-14.5890688829714,
121.958367056807)) ;
#102457 = CARTESIAN_POINT('Ctrl Pts',(-18.4660434814142,-14.6088895443292,
122.206302838715)) ;
#102458 = CARTESIAN_POINT('Ctrl Pts',(-18.1095293436928,-14.628986733551,
122.603802596907)) ;
#102459 = CARTESIAN_POINT('Ctrl Pts',(-17.9128741620564,-14.6487504125593,
123.091161865379)) ;
#102460 = CARTESIAN_POINT('Ctrl Pts',(-17.8934588628578,-14.6688076912324,
123.623664539736)) ;
#102461 = CARTESIAN_POINT('Ctrl Pts',(-18.0551924437206,-14.6886031149798,
124.124467473723)) ;
#102462 = CARTESIAN_POINT('Ctrl Pts',(-18.3794344442589,-14.7085667597074,
124.544396149328)) ;
#102463 = CARTESIAN_POINT('Ctrl Pts',(-18.8287062890011,-14.7285502509815,
124.827696849197)) ;
#102464 = CARTESIAN_POINT('Ctrl Pts',(-19.3429243244761,-14.7483577461308,
124.940748089482)) ;
#102465 = CARTESIAN_POINT('Ctrl Pts',(-19.8693900875644,-14.7683403368509,
124.871549887896)) ;
#102466 = CARTESIAN_POINT('Ctrl Pts',(-20.338450413313,-14.7882229908422,
124.627888050851)) ;
#102467 = CARTESIAN_POINT('Ctrl Pts',(-20.6977033226581,-14.8081812357052,
124.237747977146)) ;
#102468 = CARTESIAN_POINT('Ctrl Pts',(-20.9017825247716,-14.8280568227468,
123.750413738946)) ;
#102469 = CARTESIAN_POINT('Ctrl Pts',(-20.9278144322441,-14.8480377108821,
123.220027941428)) ;
#102470 = CARTESIAN_POINT('Ctrl Pts',(-20.7712200432278,-14.8679728519931,
122.71377974773)) ;
#102471 = CARTESIAN_POINT('Ctrl Pts',(-20.4520163194474,-14.8878848700041,
122.291712583774)) ;
#102472 = CARTESIAN_POINT('Ctrl Pts',(-20.0087342255776,-14.9077730882477,
122.003738662211)) ;
#102473 = CARTESIAN_POINT('Ctrl Pts',(-19.5791146983023,-14.9243713920946,
121.903719525723)) ;
#102474 = CARTESIAN_POINT('Ctrl Pts',(-19.2304737179914,-14.9376439819974,
121.914992836126)) ;
#102475 = CARTESIAN_POINT('Ctrl Pts',(-18.9730417117785,-14.9476513969483,
121.968739479905)) ;
#102476 = CARTESIAN_POINT('Ctrl Pts',(-18.7289294126291,-14.9576587436809,
122.066586725819)) ;
#102477 = CARTESIAN_POINT('Ctrl Pts',(-18.4326429910154,-14.9709251034825,
122.250333383344)) ;
#102478 = CARTESIAN_POINT('Ctrl Pts',(-18.1316429666294,-14.9874397611055,
122.569709091786)) ;
#102479 = CARTESIAN_POINT('Ctrl Pts',(-17.9558737385504,-15.0040371943481,
122.974282100994)) ;
#102480 = CARTESIAN_POINT('Ctrl Pts',(-17.904543027528,-15.0173851914931,
123.321319034395)) ;
#102481 = CARTESIAN_POINT('Ctrl Pts',(-17.9113794336415,-15.0272809458447,
123.581279394884)) ;
#102482 = CARTESIAN_POINT('Ctrl Pts',(-17.9634145199472,-15.0372688997761,
123.838522822041)) ;
#102483 = CARTESIAN_POINT('Ctrl Pts',(-18.0589406118144,-15.0472261234808,
124.082161343153)) ;
#102484 = CARTESIAN_POINT('Ctrl Pts',(-18.1964717964565,-15.0572616700375,
124.307162841967)) ;
#102485 = CARTESIAN_POINT('Ctrl Pts',(-18.3682756912085,-15.0671487813136,
124.502099452208)) ;
#102486 = CARTESIAN_POINT('Ctrl Pts',(-18.5731742379269,-15.0771401864144,
124.666262805335)) ;
#102487 = CARTESIAN_POINT('Ctrl Pts',(-18.8024583865383,-15.0870858076292,
124.791713131631)) ;
#102488 = CARTESIAN_POINT('Ctrl Pts',(-19.0499764287922,-15.0970350558975,
124.875984692672)) ;
#102489 = CARTESIAN_POINT('Ctrl Pts',(-19.3109131330844,-15.1070815510661,
124.916080673972)) ;
#102490 = CARTESIAN_POINT('Ctrl Pts',(-19.5697514855712,-15.1169328938577,
124.910630529631)) ;
#102491 = CARTESIAN_POINT('Ctrl Pts',(-19.8269017656823,-15.126904673985,
124.860363871182)) ;
#102492 = CARTESIAN_POINT('Ctrl Pts',(-20.0720498237182,-15.1368998739627,
124.765937816148)) ;
#102493 = CARTESIAN_POINT('Ctrl Pts',(-20.2977304710566,-15.1469338656587,
124.62961150485)) ;
#102494 = CARTESIAN_POINT('Ctrl Pts',(-20.4930841782723,-15.1567892706313,
124.459536040626)) ;
#102495 = CARTESIAN_POINT('Ctrl Pts',(-20.6585517530445,-15.166788568477,
124.255463871845)) ;
#102496 = CARTESIAN_POINT('Ctrl Pts',(-20.7850316142127,-15.1766836810822,
124.028212839193)) ;
#102497 = CARTESIAN_POINT('Ctrl Pts',(-20.8715023711015,-15.1867443266172,
123.778406430621)) ;
#102498 = CARTESIAN_POINT('Ctrl Pts',(-20.9125613873073,-15.1965932036064,
123.522845334443)) ;
#102499 = CARTESIAN_POINT('Ctrl Pts',(-20.9092158790002,-15.2066219147,123.259326277466)) ;
#102500 = CARTESIAN_POINT('Ctrl Pts',(-20.8594566128838,-15.2166513159561,
123.000498815782)) ;
#102501 = CARTESIAN_POINT('Ctrl Pts',(-20.7678229214068,-15.2264915077521,
122.758684061677)) ;
#102502 = CARTESIAN_POINT('Ctrl Pts',(-20.6338348815506,-15.2364949369451,
122.532544532535)) ;
#102503 = CARTESIAN_POINT('Ctrl Pts',(-20.4628129096101,-15.2464804494113,
122.33346329065)) ;
#102504 = CARTESIAN_POINT('Ctrl Pts',(-20.2585778330809,-15.2565215457953,
122.166426384082)) ;
#102505 = CARTESIAN_POINT('Ctrl Pts',(-20.0331117499585,-15.2663647417463,
122.039593657452)) ;
#102506 = CARTESIAN_POINT('Ctrl Pts',(-19.7857377349932,-15.2763510528007,
121.952117481947)) ;
#102507 = CARTESIAN_POINT('Ctrl Pts',(-19.5282066790328,-15.2862857380584,
121.908956316518)) ;
#102508 = CARTESIAN_POINT('Ctrl Pts',(-19.2639544547073,-15.2963432992754,
121.911425908328)) ;
#102509 = CARTESIAN_POINT('Ctrl Pts',(-19.0101023053987,-15.306164940884,
121.958231357651)) ;
#102510 = CARTESIAN_POINT('Ctrl Pts',(-18.7623358060744,-15.316221004475,
122.050074589458)) ;
#102511 = CARTESIAN_POINT('Ctrl Pts',(-18.5371068804422,-15.3261616802368,
122.18243432679)) ;
#102512 = CARTESIAN_POINT('Ctrl Pts',(-18.3384838834569,-15.3360660390251,
122.350644943413)) ;
#102513 = CARTESIAN_POINT('Ctrl Pts',(-18.1698386204844,-15.3461126936009,
122.553750325067)) ;
#102514 = CARTESIAN_POINT('Ctrl Pts',(-18.0407575415116,-15.3560082882438,
122.779542857678)) ;
#102515 = CARTESIAN_POINT('Ctrl Pts',(-17.951363279996,-15.3660702349007,
123.028358749357)) ;
#102516 = CARTESIAN_POINT('Ctrl Pts',(-17.9074208492035,-15.3759198588328,
123.283453459673)) ;
#102517 = CARTESIAN_POINT('Ctrl Pts',(-17.907585086851,-15.3858830978627,
123.54526162962)) ;
#102518 = CARTESIAN_POINT('Ctrl Pts',(-17.9538494830513,-15.3959076726385,
123.804618186356)) ;
#102519 = CARTESIAN_POINT('Ctrl Pts',(-18.0433208232661,-15.4058262353262,
124.049423298802)) ;
#102520 = CARTESIAN_POINT('Ctrl Pts',(-18.174519926167,-15.4158184220502,
124.276899412306)) ;
#102521 = CARTESIAN_POINT('Ctrl Pts',(-18.3442899942266,-15.4258532206344,
124.478672382218)) ;
#102522 = CARTESIAN_POINT('Ctrl Pts',(-18.5426343556928,-15.4357084113081,
124.645234433512)) ;
#102523 = CARTESIAN_POINT('Ctrl Pts',(-18.7699348084434,-15.4457077594611,
124.776994967355)) ;
#102524 = CARTESIAN_POINT('Ctrl Pts',(-19.0140737912038,-15.4556028851362,
124.866639752962)) ;
#102525 = CARTESIAN_POINT('Ctrl Pts',(-19.2742769091682,-15.4656634280843,
124.913258287484)) ;
#102526 = CARTESIAN_POINT('Ctrl Pts',(-19.5331248026427,-15.4755127023512,
124.914120014404)) ;
#102527 = CARTESIAN_POINT('Ctrl Pts',(-19.79288378634,-15.4855399269211,124.869889067141)) ;
#102528 = CARTESIAN_POINT('Ctrl Pts',(-20.0408339347153,-15.4955683261089,
124.780561213655)) ;
#102529 = CARTESIAN_POINT('Ctrl Pts',(-20.265554252512,-15.5054140765224,
124.652356312208)) ;
#102530 = CARTESIAN_POINT('Ctrl Pts',(-20.4679841696938,-15.5154028669231,
124.485226414823)) ;
#102531 = CARTESIAN_POINT('Ctrl Pts',(-20.6387526733419,-15.5254477953228,
124.283949581756)) ;
#102532 = CARTESIAN_POINT('Ctrl Pts',(-20.769587922937,-15.5352722801118,
124.061360477081)) ;
#102533 = CARTESIAN_POINT('Ctrl Pts',(-20.8622706680033,-15.545329677653,
123.813869585061)) ;
#102534 = CARTESIAN_POINT('Ctrl Pts',(-20.9096129923147,-15.5552557692392,
123.557334968006)) ;
#102535 = CARTESIAN_POINT('Ctrl Pts',(-20.9123764589189,-15.5652105543838,
123.295750825225)) ;
#102536 = CARTESIAN_POINT('Ctrl Pts',(-20.8690342234856,-15.5752479240414,
123.035565948603)) ;
#102537 = CARTESIAN_POINT('Ctrl Pts',(-20.7826602440331,-15.585136734163,
122.790464902437)) ;
#102538 = CARTESIAN_POINT('Ctrl Pts',(-20.6541601211365,-15.5951260932141,
122.561562829618)) ;
#102539 = CARTESIAN_POINT('Ctrl Pts',(-20.4882301659971,-15.6050846406702,
122.35920139353)) ;
#102540 = CARTESIAN_POINT('Ctrl Pts',(-20.2912598494344,-15.6149842172212,
122.189232159666)) ;
#102541 = CARTESIAN_POINT('Ctrl Pts',(-20.064410532344,-15.6250321290519,
122.054152289427)) ;
#102542 = CARTESIAN_POINT('Ctrl Pts',(-19.8213096590749,-15.6349274769125,
121.961719281926)) ;
#102543 = CARTESIAN_POINT('Ctrl Pts',(-19.5616355544387,-15.6449891534437,
121.912056861961)) ;
#102544 = CARTESIAN_POINT('Ctrl Pts',(-19.3029494038399,-15.6548336711928,
121.908276718303)) ;
#102545 = CARTESIAN_POINT('Ctrl Pts',(-19.0443982485231,-15.6647941149076,
121.949033267111)) ;
#102546 = CARTESIAN_POINT('Ctrl Pts',(-18.7951121911755,-15.6748309477258,
122.035180093776)) ;
#102547 = CARTESIAN_POINT('Ctrl Pts',(-18.5679663971267,-15.6847097444726,
122.160928349971)) ;
#102548 = CARTESIAN_POINT('Ctrl Pts',(-18.3624049359324,-15.694769060601,
122.327091148207)) ;
#102549 = CARTESIAN_POINT('Ctrl Pts',(-18.1920448569954,-15.7046395073542,
122.522708702974)) ;
#102550 = CARTESIAN_POINT('Ctrl Pts',(-18.0559811065904,-15.7146321456122,
122.747306071798)) ;
#102551 = CARTESIAN_POINT('Ctrl Pts',(-17.9611408622094,-15.7246641611601,
122.993277215718)) ;
#102552 = CARTESIAN_POINT('Ctrl Pts',(-17.9107294356664,-15.7345300174667,
123.24762027853)) ;
#102553 = CARTESIAN_POINT('Ctrl Pts',(-17.9051095124023,-15.7445993069358,
123.51214125627)) ;
#102554 = CARTESIAN_POINT('Ctrl Pts',(-17.9445756716794,-15.7544428644871,
123.767807266494)) ;
#102555 = CARTESIAN_POINT('Ctrl Pts',(-18.0281685488562,-15.764422991275,
124.0163870536)) ;
#102556 = CARTESIAN_POINT('Ctrl Pts',(-18.1545808942031,-15.7744415398749,
124.247322075514)) ;
#102557 = CARTESIAN_POINT('Ctrl Pts',(-18.3165419591898,-15.7843248403981,
124.450401497455)) ;
#102558 = CARTESIAN_POINT('Ctrl Pts',(-18.5149688305721,-15.7943931274462,
124.625353826907)) ;
#102559 = CARTESIAN_POINT('Ctrl Pts',(-18.7353342852211,-15.8042232504649,
124.76023996317)) ;
#102560 = CARTESIAN_POINT('Ctrl Pts',(-18.9813486671262,-15.8142898343902,
124.857374264135)) ;
#102561 = CARTESIAN_POINT('Ctrl Pts',(-19.2360561428616,-15.8241799474047,
124.909251656804)) ;
#102562 = CARTESIAN_POINT('Ctrl Pts',(-19.4985245159601,-15.8341726361673,
124.916741048985)) ;
#102563 = CARTESIAN_POINT('Ctrl Pts',(-19.7574871436884,-15.8441335245231,
124.878478534596)) ;
#102564 = CARTESIAN_POINT('Ctrl Pts',(-20.004915765595,-15.8540514694031,
124.796623445015)) ;
#102565 = CARTESIAN_POINT('Ctrl Pts',(-20.2366326706973,-15.8640592224993,
124.672179876595)) ;
#102566 = CARTESIAN_POINT('Ctrl Pts',(-20.4433415773837,-15.8740903164583,
124.508618623269)) ;
#102567 = CARTESIAN_POINT('Ctrl Pts',(-20.6157693686603,-15.8839382844863,
124.31560845638)) ;
#102568 = CARTESIAN_POINT('Ctrl Pts',(-20.7552008635607,-15.8940002406122,
124.090965026465)) ;
#102569 = CARTESIAN_POINT('Ctrl Pts',(-20.8516852314679,-15.9038974522133,
123.849423164374)) ;
#102570 = CARTESIAN_POINT('Ctrl Pts',(-20.905785380101,-15.9138286188779,
123.59411597792)) ;
#102571 = CARTESIAN_POINT('Ctrl Pts',(-20.9145476357222,-15.9238708030821,
123.330367383369)) ;
#102572 = CARTESIAN_POINT('Ctrl Pts',(-20.8781404899739,-15.9337574713353,
123.073106868608)) ;
#102573 = CARTESIAN_POINT('Ctrl Pts',(-20.7971769554529,-15.9437505833135,
122.823304869138)) ;
#102574 = CARTESIAN_POINT('Ctrl Pts',(-20.6745604614457,-15.9536962609293,
122.592489803753)) ;
#102575 = CARTESIAN_POINT('Ctrl Pts',(-20.5141161128324,-15.9636435639143,
122.386100293049)) ;
#102576 = CARTESIAN_POINT('Ctrl Pts',(-20.3181349029705,-15.9736912876611,
122.20916311758)) ;
#102577 = CARTESIAN_POINT('Ctrl Pts',(-20.0989517012309,-15.9835396614236,
122.071551117016)) ;
#102578 = CARTESIAN_POINT('Ctrl Pts',(-19.8568380440018,-15.9934986338693,
121.97218342843)) ;
#102579 = CARTESIAN_POINT('Ctrl Pts',(-19.5990047972081,-16.0035374957505,
121.916385466121)) ;
#102580 = CARTESIAN_POINT('Ctrl Pts',(-19.3395875748729,-16.0134160999223,
121.905950820223)) ;
#102581 = CARTESIAN_POINT('Ctrl Pts',(-19.0778432793215,-16.0234676411256,
121.941206263373)) ;
#102582 = CARTESIAN_POINT('Ctrl Pts',(-18.8300030362905,-16.0333630391059,
122.020074331794)) ;
#102583 = CARTESIAN_POINT('Ctrl Pts',(-18.5959998150771,-16.0434142716512,
122.142513812537)) ;
#102584 = CARTESIAN_POINT('Ctrl Pts',(-18.3901773440873,-16.0533004622755,
122.301092280295)) ;
#102585 = CARTESIAN_POINT('Ctrl Pts',(-18.2128102595661,-16.0632930015913,
122.494699854183)) ;
#102586 = CARTESIAN_POINT('Ctrl Pts',(-18.0724264392633,-16.073241447486,
122.715265898288)) ;
#102587 = CARTESIAN_POINT('Ctrl Pts',(-17.9722610725586,-16.0831782500179,
122.956395392167)) ;
#102588 = CARTESIAN_POINT('Ctrl Pts',(-17.9148856828891,-16.0931612574692,
123.212421827305)) ;
#102589 = CARTESIAN_POINT('Ctrl Pts',(-17.9032506732785,-16.103205098884,
123.476076424428)) ;
#102590 = CARTESIAN_POINT('Ctrl Pts',(-17.9362383494643,-16.1130332975079,
123.732276332531)) ;
#102591 = CARTESIAN_POINT('Ctrl Pts',(-18.0150068697524,-16.1231098909501,
123.985034482931)) ;
#102592 = CARTESIAN_POINT('Ctrl Pts',(-18.1336923054321,-16.1329618902917,
124.215193158101)) ;
#102593 = CARTESIAN_POINT('Ctrl Pts',(-18.293828954018,-16.1430354771156,
124.425930990448)) ;
#102594 = CARTESIAN_POINT('Ctrl Pts',(-18.4837073307471,-16.152875702213,
124.601509441711)) ;
#102595 = CARTESIAN_POINT('Ctrl Pts',(-18.703422599687,-16.1628414062417,
124.743985806514)) ;
#102596 = CARTESIAN_POINT('Ctrl Pts',(-18.94619596473,-16.1728680395483,124.846435307099)) ;
#102597 = CARTESIAN_POINT('Ctrl Pts',(-19.2001320498308,-16.1827823352601,
124.904684366609)) ;
#102598 = CARTESIAN_POINT('Ctrl Pts',(-19.4622641622427,-16.1927706239526,
124.918531528286)) ;
#102599 = CARTESIAN_POINT('Ctrl Pts',(-19.7240529144461,-16.2028093571109,
124.886019110933)) ;
#102600 = CARTESIAN_POINT('Ctrl Pts',(-19.971447916316,-16.2126526889385,
124.810469269486)) ;
#102601 = CARTESIAN_POINT('Ctrl Pts',(-20.2065617889263,-16.2226804148181,
124.691454476011)) ;
#102602 = CARTESIAN_POINT('Ctrl Pts',(-20.4171114197521,-16.2327127512066,
124.532774031864)) ;
#102603 = CARTESIAN_POINT('Ctrl Pts',(-20.5936406689353,-16.2425422515072,
124.344218105052)) ;
#102604 = CARTESIAN_POINT('Ctrl Pts',(-20.7377182461283,-16.252531755424,
124.124767080073)) ;
#102605 = CARTESIAN_POINT('Ctrl Pts',(-20.8414473437141,-16.2625755959364,
123.882065493061)) ;
#102606 = CARTESIAN_POINT('Ctrl Pts',(-20.900653673808,-16.2723973017045,
123.630843512612)) ;
#102607 = CARTESIAN_POINT('Ctrl Pts',(-20.9163042732894,-16.2824323488368,
123.36759911716)) ;
#102608 = CARTESIAN_POINT('Ctrl Pts',(-20.8853162273939,-16.2924570262737,
123.105980618669)) ;
#102609 = CARTESIAN_POINT('Ctrl Pts',(-20.8112016290082,-16.3023098411282,
122.857893201183)) ;
#102610 = CARTESIAN_POINT('Ctrl Pts',(-20.6939684927004,-16.3122975507357,
122.623085044289)) ;
#102611 = CARTESIAN_POINT('Ctrl Pts',(-20.5386409517621,-16.3222275607298,
122.413386814365)) ;
#102612 = CARTESIAN_POINT('Ctrl Pts',(-20.3484048238338,-16.332217315949,
122.232473149134)) ;
#102613 = CARTESIAN_POINT('Ctrl Pts',(-20.1286513400148,-16.3422439246319,
122.087087277406)) ;
#102614 = CARTESIAN_POINT('Ctrl Pts',(-19.8905383570704,-16.3521278646537,
121.983335342418)) ;
#102615 = CARTESIAN_POINT('Ctrl Pts',(-19.6354682256549,-16.3621170921922,
121.921258549847)) ;
#102616 = CARTESIAN_POINT('Ctrl Pts',(-19.3720634366755,-16.3721599627159,
121.904869502532)) ;
#102617 = CARTESIAN_POINT('Ctrl Pts',(-19.115265317879,-16.3819923494713,
121.933435787349)) ;
#102618 = CARTESIAN_POINT('Ctrl Pts',(-18.8630593043573,-16.3919856426429,
122.006615981384)) ;
#102619 = CARTESIAN_POINT('Ctrl Pts',(-18.6267060253685,-16.4020176482913,
122.123427107478)) ;
#102620 = CARTESIAN_POINT('Ctrl Pts',(-18.4175878783122,-16.4118829042603,
122.276634889428)) ;
#102621 = CARTESIAN_POINT('Ctrl Pts',(-18.235941989852,-16.4218447841678,
122.465159983501)) ;
#102622 = CARTESIAN_POINT('Ctrl Pts',(-18.0890877174542,-16.4318797175297,
122.684175710584)) ;
#102623 = CARTESIAN_POINT('Ctrl Pts',(-17.9836645209362,-16.441764675909,
122.92162846115)) ;
#102624 = CARTESIAN_POINT('Ctrl Pts',(-17.9200049383359,-16.4518303028317,
123.178322908577)) ;
#102625 = CARTESIAN_POINT('Ctrl Pts',(-17.9020225616626,-16.461669408496,
123.436301022822)) ;
#102626 = CARTESIAN_POINT('Ctrl Pts',(-17.9293636219284,-16.4717322235013,
123.699287948739)) ;
#102627 = CARTESIAN_POINT('Ctrl Pts',(-18.0009973197692,-16.48162842955,123.949318087485)) ;
#102628 = CARTESIAN_POINT('Ctrl Pts',(-18.1147911167,-16.4915692525753,124.184432400747)) ;
#102629 = CARTESIAN_POINT('Ctrl Pts',(-18.2686434852337,-16.501573835554,
124.397661532984)) ;
#102630 = CARTESIAN_POINT('Ctrl Pts',(-18.4576877170773,-16.5115947299987,
124.580981693684)) ;
#102631 = CARTESIAN_POINT('Ctrl Pts',(-18.6727140788603,-16.5214866505881,
124.727067000492)) ;
#102632 = CARTESIAN_POINT('Ctrl Pts',(-18.9121040759921,-16.5314800829335,
124.835026163748)) ;
#102633 = CARTESIAN_POINT('Ctrl Pts',(-19.1654138675533,-16.5414256878334,
124.899390294724)) ;
#102634 = CARTESIAN_POINT('Ctrl Pts',(-19.4260705655085,-16.5513729613149,
124.91932812352)) ;
#102635 = CARTESIAN_POINT('Ctrl Pts',(-19.6888096358805,-16.5614208757913,
124.893152467969)) ;
#102636 = CARTESIAN_POINT('Ctrl Pts',(-19.9380161975764,-16.5712685161386,
124.823385534915)) ;
#102637 = CARTESIAN_POINT('Ctrl Pts',(-20.1743666544338,-16.5812302315152,
124.710857010624)) ;
#102638 = CARTESIAN_POINT('Ctrl Pts',(-20.3888501617689,-16.591258855088,
124.557691167394)) ;
#102639 = CARTESIAN_POINT('Ctrl Pts',(-20.5713434225221,-16.6011692171544,
124.371907329123)) ;
#102640 = CARTESIAN_POINT('Ctrl Pts',(-20.7197488159772,-16.6111039108068,
124.157103939967)) ;
#102641 = CARTESIAN_POINT('Ctrl Pts',(-20.8295291223563,-16.6211457539347,
123.917148213344)) ;
#102642 = CARTESIAN_POINT('Ctrl Pts',(-20.8951698637997,-16.6310302595051,
123.665797293979)) ;
#102643 = CARTESIAN_POINT('Ctrl Pts',(-20.9167212692526,-16.6410323632903,
123.403875986852)) ;
#102644 = CARTESIAN_POINT('Ctrl Pts',(-20.8928773969328,-16.6509507147053,
123.1442814441)) ;
#102645 = CARTESIAN_POINT('Ctrl Pts',(-20.8233840795144,-16.6609983707262,
122.889591453258)) ;
#102646 = CARTESIAN_POINT('Ctrl Pts',(-20.7129252170611,-16.6708695637544,
122.654819502482)) ;
#102647 = CARTESIAN_POINT('Ctrl Pts',(-20.5605354982696,-16.6809352768979,
122.438686260115)) ;
#102648 = CARTESIAN_POINT('Ctrl Pts',(-20.3770240889657,-16.6907877374706,
122.255936128519)) ;
#102649 = CARTESIAN_POINT('Ctrl Pts',(-20.087548406569,-16.7042162001931,
122.054303583676)) ;
#102650 = CARTESIAN_POINT('Ctrl Pts',(-19.7606789820006,-16.7172971477102,
121.935420000031)) ;
#102651 = CARTESIAN_POINT('Ctrl Pts',(-19.4080350522028,-16.7307716459448,
121.904256007586)) ;
#102652 = CARTESIAN_POINT('Ctrl Pts',(-19.1506104608583,-16.7406037495542,
121.926903242143)) ;
#102653 = CARTESIAN_POINT('Ctrl Pts',(-18.8974323765611,-16.7505696526809,
121.993771587501)) ;
#102654 = CARTESIAN_POINT('Ctrl Pts',(-18.6583554923555,-16.7605970619911,
122.104659747869)) ;
#102655 = CARTESIAN_POINT('Ctrl Pts',(-18.4446854779983,-16.7705080933577,
122.253532722493)) ;
#102656 = CARTESIAN_POINT('Ctrl Pts',(-18.1971636646785,-16.7837524009787,
122.498316557246)) ;
#102657 = CARTESIAN_POINT('Ctrl Pts',(-17.9735940338532,-16.8004528836499,
122.881662292758)) ;
#102658 = CARTESIAN_POINT('Ctrl Pts',(-17.8949269013525,-16.8169597128057,
123.313347762815)) ;
#102659 = CARTESIAN_POINT('Ctrl Pts',(-17.9226464741625,-16.8302703410433,
123.661998443756)) ;
#102660 = CARTESIAN_POINT('Ctrl Pts',(-17.9885500170473,-16.8402629045834,
123.916229875979)) ;
#102661 = CARTESIAN_POINT('Ctrl Pts',(-18.0982623423877,-16.8502929875849,
124.155855958058)) ;
#102662 = CARTESIAN_POINT('Ctrl Pts',(-18.2942872666369,-16.8634665915827,
124.441278247379)) ;
#102663 = CARTESIAN_POINT('Ctrl Pts',(-18.6299061183238,-16.8801042968141,
124.728954007652)) ;
#102664 = CARTESIAN_POINT('Ctrl Pts',(-19.1244459055575,-16.8999860593815,
124.915699707355)) ;
#102665 = CARTESIAN_POINT('Ctrl Pts',(-19.5680324815316,-16.916682411598,
124.921092180331)) ;
#102666 = CARTESIAN_POINT('Ctrl Pts',(-19.9032333390617,-16.9298394393871,
124.836022746457)) ;
#102667 = CARTESIAN_POINT('Ctrl Pts',(-20.2240355606206,-16.9432167940307,
124.692342653553)) ;
#102668 = CARTESIAN_POINT('Ctrl Pts',(-20.564889178668,-16.9597476282895,
124.415021464963)) ;
#102669 = CARTESIAN_POINT('Ctrl Pts',(-20.8382412988788,-16.9797123180326,
123.960277734278)) ;
#102670 = CARTESIAN_POINT('Ctrl Pts',(-20.9392835418282,-16.9996288114562,
123.440651482369)) ;
#102671 = CARTESIAN_POINT('Ctrl Pts',(-20.8580861687626,-17.0195185308058,
122.918235270945)) ;
#102672 = CARTESIAN_POINT('Ctrl Pts',(-20.6016768774655,-17.0395252604536,
122.452481906483)) ;
#102673 = CARTESIAN_POINT('Ctrl Pts',(-20.2052175288422,-17.0593633141005,
122.104716301636)) ;
#102674 = CARTESIAN_POINT('Ctrl Pts',(-19.7104254026965,-17.0793566523141,
121.911189175635)) ;
#102675 = CARTESIAN_POINT('Ctrl Pts',(-19.1820266687273,-17.0992394517207,
121.898521473643)) ;
#102676 = CARTESIAN_POINT('Ctrl Pts',(-18.6807377304385,-17.1191316326394,
122.066075438973)) ;
#102677 = CARTESIAN_POINT('Ctrl Pts',(-18.2657133225145,-17.1390338111345,
122.394294335146)) ;
#102678 = CARTESIAN_POINT('Ctrl Pts',(-17.9866603659834,-17.1590711223382,
122.847724178873)) ;
#102679 = CARTESIAN_POINT('Ctrl Pts',(-17.8794978535988,-17.1788835638791,
123.363523177826)) ;
#102680 = CARTESIAN_POINT('Ctrl Pts',(-17.9558402348989,-17.198948804614,
123.891074767645)) ;
#102681 = CARTESIAN_POINT('Ctrl Pts',(-18.2036314096174,-17.2187060094698,
124.354333762872)) ;
#102682 = CARTESIAN_POINT('Ctrl Pts',(-18.5991823651955,-17.2387392821155,
124.710365554542)) ;
#102683 = CARTESIAN_POINT('Ctrl Pts',(-19.0875497902478,-17.2585521905694,
124.907973528954)) ;
#102684 = CARTESIAN_POINT('Ctrl Pts',(-19.6184027284767,-17.2785483366968,
124.927930635947)) ;
#102685 = CARTESIAN_POINT('Ctrl Pts',(-20.1213295234125,-17.2984100899193,
124.766739572709)) ;
#102686 = CARTESIAN_POINT('Ctrl Pts',(-20.5429252904641,-17.3184786070474,
124.440190715913)) ;
#102687 = CARTESIAN_POINT('Ctrl Pts',(-20.8242377074494,-17.3383094800442,
123.994332355414)) ;
#102688 = CARTESIAN_POINT('Ctrl Pts',(-20.9383799614121,-17.3582313908609,
123.477416013546)) ;
#102689 = CARTESIAN_POINT('Ctrl Pts',(-20.8690667085864,-17.3781608342962,
122.952191601519)) ;
#102690 = CARTESIAN_POINT('Ctrl Pts',(-20.6251748641544,-17.3980705044126,
122.482671780441)) ;
#102691 = CARTESIAN_POINT('Ctrl Pts',(-20.2369461402496,-17.4179438616755,
122.124424796588)) ;
#102692 = CARTESIAN_POINT('Ctrl Pts',(-19.7469586060816,-17.4379353962934,
121.919092941373)) ;
#102693 = CARTESIAN_POINT('Ctrl Pts',(-19.2195163903342,-17.4578010137041,
121.893229788818)) ;
#102694 = CARTESIAN_POINT('Ctrl Pts',(-18.7119189138773,-17.4777819435324,
122.049276613145)) ;
#102695 = CARTESIAN_POINT('Ctrl Pts',(-18.2892740598292,-17.4977204056155,
122.368981249758)) ;
#102696 = CARTESIAN_POINT('Ctrl Pts',(-18.0010468981692,-17.5176125988372,
122.812282126903)) ;
#102697 = CARTESIAN_POINT('Ctrl Pts',(-17.8812114661652,-17.5375833138726,
123.329247053136)) ;
#102698 = CARTESIAN_POINT('Ctrl Pts',(-17.9435998730545,-17.5573929855387,
123.852172416276)) ;
#102699 = CARTESIAN_POINT('Ctrl Pts',(-18.1823889066132,-17.5773862022299,
124.326665444011)) ;
#102700 = CARTESIAN_POINT('Ctrl Pts',(-18.5660143257143,-17.5972371144262,
124.689196530154)) ;
#102701 = CARTESIAN_POINT('Ctrl Pts',(-19.0555661838495,-17.6173117207453,
124.900996777746)) ;
#102702 = CARTESIAN_POINT('Ctrl Pts',(-19.4939397624789,-17.6338283526286,
124.927071266426)) ;
#102703 = CARTESIAN_POINT('Ctrl Pts',(-19.8373477851009,-17.6471670603227,
124.857183829402)) ;
#102704 = CARTESIAN_POINT('Ctrl Pts',(-20.0781861357582,-17.657009434631,
124.762756345354)) ;
#102705 = CARTESIAN_POINT('Ctrl Pts',(-20.3038016916689,-17.6670644546137,
124.625289262735)) ;
#102706 = CARTESIAN_POINT('Ctrl Pts',(-20.5648525379712,-17.6802966112713,
124.395511911604)) ;
#102707 = CARTESIAN_POINT('Ctrl Pts',(-20.8101382457707,-17.6969115786164,
124.028340182792)) ;
#102708 = CARTESIAN_POINT('Ctrl Pts',(-20.9150913429758,-17.7135061656276,
123.59996828002)) ;
#102709 = CARTESIAN_POINT('Ctrl Pts',(-20.9083194371966,-17.726739733983,
123.252245244698)) ;
#102710 = CARTESIAN_POINT('Ctrl Pts',(-20.8574972331854,-17.7367833517917,
122.993271365675)) ;
#102711 = CARTESIAN_POINT('Ctrl Pts',(-20.764029698907,-17.7466702760265,
122.750824428413)) ;
#102712 = CARTESIAN_POINT('Ctrl Pts',(-20.6288988859951,-17.7566609304733,
122.52574713789)) ;
#102713 = CARTESIAN_POINT('Ctrl Pts',(-20.4571856548047,-17.7666226889273,
122.328145639307)) ;
#102714 = CARTESIAN_POINT('Ctrl Pts',(-20.1849772827388,-17.7799625539945,
122.1071474189)) ;
#102715 = CARTESIAN_POINT('Ctrl Pts',(-19.8618446927866,-17.7932713369078,
121.963370845515)) ;
#102716 = CARTESIAN_POINT('Ctrl Pts',(-19.5194408838435,-17.8064670943519,
121.908500061453)) ;
#102717 = CARTESIAN_POINT('Ctrl Pts',(-19.2576702789978,-17.8164289780284,
121.911860337641)) ;
#102718 = CARTESIAN_POINT('Ctrl Pts',(-18.9984511732404,-17.826472087543,
121.961443066913)) ;
#102719 = CARTESIAN_POINT('Ctrl Pts',(-18.7563454905763,-17.8363243375422,
122.053214389354)) ;
#102720 = CARTESIAN_POINT('Ctrl Pts',(-18.5308613892002,-17.8462958744927,
122.186659294031)) ;
#102721 = CARTESIAN_POINT('Ctrl Pts',(-18.3314608275269,-17.8562911399702,
122.357696687906)) ;
#102722 = CARTESIAN_POINT('Ctrl Pts',(-18.1644321330469,-17.8663251128439,
122.56170136985)) ;
#102723 = CARTESIAN_POINT('Ctrl Pts',(-18.0372772522099,-17.8761805276062,
122.787357009147)) ;
#102724 = CARTESIAN_POINT('Ctrl Pts',(-17.9496644830433,-17.886179805115,
123.035043600757)) ;
#102725 = CARTESIAN_POINT('Ctrl Pts',(-17.9065487373405,-17.896074989278,
123.291524479843)) ;
#102726 = CARTESIAN_POINT('Ctrl Pts',(-17.9086851881469,-17.9061353689188,
123.555856178888)) ;
#102727 = CARTESIAN_POINT('Ctrl Pts',(-17.9555360244664,-17.9159852379269,
123.810451246354)) ;
#102728 = CARTESIAN_POINT('Ctrl Pts',(-18.0469682041802,-17.9260167991348,
124.057688557199)) ;
#102729 = CARTESIAN_POINT('Ctrl Pts',(-18.1801385787073,-17.9360272480171,
124.284582911936)) ;
#102730 = CARTESIAN_POINT('Ctrl Pts',(-18.3486755036932,-17.9459339874341,
124.482994407031)) ;
#102731 = CARTESIAN_POINT('Ctrl Pts',(-18.5494063023353,-17.9558720035025,
124.650040004162)) ;
#102732 = CARTESIAN_POINT('Ctrl Pts',(-18.7775774979802,-17.9658772499537,
124.780743652177)) ;
#102733 = CARTESIAN_POINT('Ctrl Pts',(-19.0258028917251,-17.97591131101,124.869663326483)) ;
#102734 = CARTESIAN_POINT('Ctrl Pts',(-19.2807552443101,-17.9857563920681,
124.913740300713)) ;
#102735 = CARTESIAN_POINT('Ctrl Pts',(-19.5431300648516,-17.9957421980216,
124.913357879036)) ;
#102736 = CARTESIAN_POINT('Ctrl Pts',(-19.8002551560576,-18.0056770185758,
124.867827638442)) ;
#102737 = CARTESIAN_POINT('Ctrl Pts',(-20.0484362054016,-18.015734543708,
124.777046260329)) ;
#102738 = CARTESIAN_POINT('Ctrl Pts',(-20.2719773851506,-18.0255561943594,
124.647968643264)) ;
#102739 = CARTESIAN_POINT('Ctrl Pts',(-20.4747082782769,-18.0356122578641,
124.478488060217)) ;
#102740 = CARTESIAN_POINT('Ctrl Pts',(-20.6426391301246,-18.045552924928,
124.278372755303)) ;
#102741 = CARTESIAN_POINT('Ctrl Pts',(-20.7735002160438,-18.055457318594,
124.05337893199)) ;
#102742 = CARTESIAN_POINT('Ctrl Pts',(-20.8644257535316,-18.065503842357,
123.805543745991)) ;
#102743 = CARTESIAN_POINT('Ctrl Pts',(-20.9105004800301,-18.0753999253734,
123.549551389803)) ;
#102744 = CARTESIAN_POINT('Ctrl Pts',(-20.9113777941463,-18.0854666246034,
123.285058179939)) ;
#102745 = CARTESIAN_POINT('Ctrl Pts',(-20.8676853361429,-18.0952902350045,
123.03058768618)) ;
#102746 = CARTESIAN_POINT('Ctrl Pts',(-20.7788729200758,-18.105346095182,
122.781737389733)) ;
#102747 = CARTESIAN_POINT('Ctrl Pts',(-20.6494706999831,-18.1152792414869,
122.555000037183)) ;
#102748 = CARTESIAN_POINT('Ctrl Pts',(-20.4829128435799,-18.1252244972575,
122.353637264426)) ;
#102749 = CARTESIAN_POINT('Ctrl Pts',(-20.2832491516113,-18.135207795696,
122.183403536089)) ;
#102750 = CARTESIAN_POINT('Ctrl Pts',(-20.0557030935706,-18.1452449758426,
122.050043065921)) ;
#102751 = CARTESIAN_POINT('Ctrl Pts',(-19.8130548469334,-18.1550995285521,
121.959496203721)) ;
#102752 = CARTESIAN_POINT('Ctrl Pts',(-19.5547600095876,-18.1650990469994,
121.911417252106)) ;
#102753 = CARTESIAN_POINT('Ctrl Pts',(-19.2946981607861,-18.1749941294615,
121.908665977267)) ;
#102754 = CARTESIAN_POINT('Ctrl Pts',(-19.0339004563328,-18.1850546749676,
121.951834448406)) ;
#102755 = CARTESIAN_POINT('Ctrl Pts',(-18.7896960288208,-18.1949039822156,
122.037668069937)) ;
#102756 = CARTESIAN_POINT('Ctrl Pts',(-18.559727806406,-18.204931072303,122.166293607386)) ;
#102757 = CARTESIAN_POINT('Ctrl Pts',(-18.3559794762093,-18.2149599764399,
122.333478186959)) ;
#102758 = CARTESIAN_POINT('Ctrl Pts',(-18.187145941362,-18.2248038415392,
122.529460192013)) ;
#102759 = CARTESIAN_POINT('Ctrl Pts',(-18.0523029774518,-18.2347996682476,
122.75488871841)) ;
#102760 = CARTESIAN_POINT('Ctrl Pts',(-17.9588260064402,-18.2448248848966,
123.001205208719)) ;
#102761 = CARTESIAN_POINT('Ctrl Pts',(-17.909859628747,-18.2547147170542,
123.256449962964)) ;
#102762 = CARTESIAN_POINT('Ctrl Pts',(-17.9055571019604,-18.2647055731389,
123.518955212677)) ;
#102763 = CARTESIAN_POINT('Ctrl Pts',(-17.946760077564,-18.2746506677318,
123.777033194957)) ;
#102764 = CARTESIAN_POINT('Ctrl Pts',(-18.0317466001249,-18.2846025714999,
124.024375730122)) ;
#102765 = CARTESIAN_POINT('Ctrl Pts',(-18.1596578210665,-18.2946389709693,
124.255020663488)) ;
#102766 = CARTESIAN_POINT('Ctrl Pts',(-18.3230984485718,-18.304528041058,
124.457076640382)) ;
#102767 = CARTESIAN_POINT('Ctrl Pts',(-18.5208050093406,-18.3145173304289,
124.629759420022)) ;
#102768 = CARTESIAN_POINT('Ctrl Pts',(-18.7449002910131,-18.3244758966386,
124.764905710238)) ;
#102769 = CARTESIAN_POINT('Ctrl Pts',(-18.9874020685132,-18.3343754678554,
124.859137657346)) ;
#102770 = CARTESIAN_POINT('Ctrl Pts',(-19.2463807699488,-18.3444233822697,
124.910491523554)) ;
#102771 = CARTESIAN_POINT('Ctrl Pts',(-19.5063983310136,-18.3543187251302,
124.916218951669)) ;
#102772 = CARTESIAN_POINT('Ctrl Pts',(-19.7677160165026,-18.3643804190777,
124.876094658187)) ;
#102773 = CARTESIAN_POINT('Ctrl Pts',(-20.0127459205571,-18.3742248721618,
124.793068730627)) ;
#102774 = CARTESIAN_POINT('Ctrl Pts',(-20.2427353819954,-18.3841855571203,
124.668108697324)) ;
#102775 = CARTESIAN_POINT('Ctrl Pts',(-20.4488207458198,-18.3942214896288,
124.503522047669)) ;
#102776 = CARTESIAN_POINT('Ctrl Pts',(-20.6208245138306,-18.4041101053169,
124.308738320437)) ;
#102777 = CARTESIAN_POINT('Ctrl Pts',(-20.7585778713558,-18.4141245144593,
124.084482018134)) ;
#102778 = CARTESIAN_POINT('Ctrl Pts',(-20.8548377910797,-18.4241583234171,
123.839019941139)) ;
#102779 = CARTESIAN_POINT('Ctrl Pts',(-20.9066734537542,-18.4339887776733,
123.585907801548)) ;
#102780 = CARTESIAN_POINT('Ctrl Pts',(-20.914035005145,-18.4440664452515,
123.321231030085)) ;
#102781 = CARTESIAN_POINT('Ctrl Pts',(-20.8763128759204,-18.4539183133737,
123.065039782378)) ;
#102782 = CARTESIAN_POINT('Ctrl Pts',(-20.7930887940635,-18.4639913509391,
122.813802107572)) ;
#102783 = CARTESIAN_POINT('Ctrl Pts',(-20.6703133695583,-18.47383390429,122.58612058865)) ;
#102784 = CARTESIAN_POINT('Ctrl Pts',(-20.5083368229073,-18.4838142997834,
122.379854902302)) ;
#102785 = CARTESIAN_POINT('Ctrl Pts',(-20.3119149758055,-18.4938327777612,
122.204557816278)) ;
#102786 = CARTESIAN_POINT('Ctrl Pts',(-20.0913199809114,-18.5037160920673,
122.067406308123)) ;
#102787 = CARTESIAN_POINT('Ctrl Pts',(-19.8457770815624,-18.513784394606,
121.968966609074)) ;
#102788 = CARTESIAN_POINT('Ctrl Pts',(-19.5929747381115,-18.5236144418794,
121.915623759485)) ;
#102789 = CARTESIAN_POINT('Ctrl Pts',(-19.3286319421843,-18.5336813132949,
121.906445897827)) ;
#102790 = CARTESIAN_POINT('Ctrl Pts',(-19.0712757729958,-18.543570352094,
121.942804033126)) ;
#102791 = CARTESIAN_POINT('Ctrl Pts',(-18.821355081623,-18.5535670502281,
122.023662185229)) ;
#102792 = CARTESIAN_POINT('Ctrl Pts',(-18.5903099011435,-18.5635194759401,
122.146260462174)) ;
#102793 = CARTESIAN_POINT('Ctrl Pts',(-18.3840985282772,-18.573460778173,
122.306624856923)) ;
#102794 = CARTESIAN_POINT('Ctrl Pts',(-18.2078826377361,-18.5834440172569,
122.501023786274)) ;
#102795 = CARTESIAN_POINT('Ctrl Pts',(-18.0676953784142,-18.5934828188255,
122.7244758304)) ;
#102796 = CARTESIAN_POINT('Ctrl Pts',(-17.9698362461543,-18.6033309249472,
122.964084842904)) ;
#102797 = CARTESIAN_POINT('Ctrl Pts',(-17.9136564349659,-18.6133911205225,
123.222395340427)) ;
#102798 = CARTESIAN_POINT('Ctrl Pts',(-17.9035861785321,-18.6232888038339,
123.482312245733)) ;
#102799 = CARTESIAN_POINT('Ctrl Pts',(-17.9380672693669,-18.6332198442079,
123.740997360846)) ;
#102800 = CARTESIAN_POINT('Ctrl Pts',(-18.0180952724909,-18.6432620618645,
123.992465098917)) ;
#102801 = CARTESIAN_POINT('Ctrl Pts',(-18.1385156099613,-18.6531487225985,
124.222698255833)) ;
#102802 = CARTESIAN_POINT('Ctrl Pts',(-18.2984251565987,-18.663141831201,
124.430989059659)) ;
#102803 = CARTESIAN_POINT('Ctrl Pts',(-18.4912300319267,-18.6730875298392,
124.607445393199)) ;
#102804 = CARTESIAN_POINT('Ctrl Pts',(-18.7115019926513,-18.6830347521103,
124.748223682838)) ;
#102805 = CARTESIAN_POINT('Ctrl Pts',(-18.9554118568086,-18.6930827776904,
124.849350889407)) ;
#102806 = CARTESIAN_POINT('Ctrl Pts',(-19.2079857719931,-18.7029300248333,
124.905664069437)) ;
#102807 = CARTESIAN_POINT('Ctrl Pts',(-19.4695005317294,-18.712893201924,
124.918229762502)) ;
#102808 = CARTESIAN_POINT('Ctrl Pts',(-19.7309117193007,-18.7229229229575,
124.884581451279)) ;
#102809 = CARTESIAN_POINT('Ctrl Pts',(-19.9794879753624,-18.7328273904903,
124.807331616421)) ;
#102810 = CARTESIAN_POINT('Ctrl Pts',(-20.2136713900044,-18.7428518763201,
124.686754120868)) ;
#102811 = CARTESIAN_POINT('Ctrl Pts',(-20.4210216017489,-18.752755711444,
124.529395994289)) ;
#102812 = CARTESIAN_POINT('Ctrl Pts',(-20.6005285093603,-18.762806902154,
124.335672824434)) ;
#102813 = CARTESIAN_POINT('Ctrl Pts',(-20.7413686076851,-18.7726913448123,
124.117385719784)) ;
#102814 = CARTESIAN_POINT('Ctrl Pts',(-20.8437048455114,-18.7826843526642,
123.875565880719)) ;
#102815 = CARTESIAN_POINT('Ctrl Pts',(-20.9021579365581,-18.7926326723805,
123.620735391782)) ;
#102816 = CARTESIAN_POINT('Ctrl Pts',(-20.9158318547924,-18.8025695110899,
123.359986539688)) ;
#102817 = CARTESIAN_POINT('Ctrl Pts',(-20.8841973543679,-18.8125525000095,
123.099524249898)) ;
#102818 = CARTESIAN_POINT('Ctrl Pts',(-20.806906706318,-18.8225963793736,
122.847184221893)) ;
#102819 = CARTESIAN_POINT('Ctrl Pts',(-20.6900671314966,-18.832424444732,
122.616806023797)) ;
#102820 = CARTESIAN_POINT('Ctrl Pts',(-20.5312234748615,-18.8425015332869,
122.40499355955)) ;
#102821 = CARTESIAN_POINT('Ctrl Pts',(-20.3423910055015,-18.8523516854432,
122.227844954724)) ;
#102822 = CARTESIAN_POINT('Ctrl Pts',(-20.1207728474674,-18.8624321658956,
122.082847269407)) ;
#102823 = CARTESIAN_POINT('Ctrl Pts',(-19.883742672593,-18.8722466636644,
121.981028207719)) ;
#102824 = CARTESIAN_POINT('Ctrl Pts',(-19.6263552357051,-18.8823149596845,
121.920005976906)) ;
#102825 = CARTESIAN_POINT('Ctrl Pts',(-19.3665955247242,-18.8922137921673,
121.904926016913)) ;
#102826 = CARTESIAN_POINT('Ctrl Pts',(-19.1042510947815,-18.9022666721818,
121.935545005745)) ;
#102827 = CARTESIAN_POINT('Ctrl Pts',(-18.8556439453619,-18.912136487678,
122.0096688688)) ;
#102828 = CARTESIAN_POINT('Ctrl Pts',(-18.618972458441,-18.9222091687608,
122.128110319243)) ;
#102829 = CARTESIAN_POINT('Ctrl Pts',(-18.4114114475345,-18.9320416473318,
122.282045205)) ;
#102830 = CARTESIAN_POINT('Ctrl Pts',(-18.2296251987227,-18.9420722813179,
122.472912692922)) ;
#102831 = CARTESIAN_POINT('Ctrl Pts',(-18.0843565052715,-18.952103838537,
122.692912211398)) ;
#102832 = CARTESIAN_POINT('Ctrl Pts',(-17.9811210290767,-18.9619335474087,
122.929682254542)) ;
#102833 = CARTESIAN_POINT('Ctrl Pts',(-17.9188134712932,-18.9719229962108,
123.184700918537)) ;
#102834 = CARTESIAN_POINT('Ctrl Pts',(-17.9023076564122,-18.9819668486108,
123.448123362392)) ;
#102835 = CARTESIAN_POINT('Ctrl Pts',(-17.9306090900977,-18.9917885619429,
123.704671597423)) ;
#102836 = CARTESIAN_POINT('Ctrl Pts',(-18.0039766331201,-19.0018235669316,
123.957968446456)) ;
#102837 = CARTESIAN_POINT('Ctrl Pts',(-18.1207526601657,-19.0118484053792,
124.194124766735)) ;
#102838 = CARTESIAN_POINT('Ctrl Pts',(-18.2736214503215,-19.0217006183344,
124.403083451732)) ;
#102839 = CARTESIAN_POINT('Ctrl Pts',(-18.4627386535141,-19.0316905745282,
124.585137888009)) ;
#102840 = CARTESIAN_POINT('Ctrl Pts',(-18.6792568285447,-19.0416186848114,
124.730717366156)) ;
#102841 = CARTESIAN_POINT('Ctrl Pts',(-18.9190451892015,-19.051607284891,
124.837516605335)) ;
#102842 = CARTESIAN_POINT('Ctrl Pts',(-19.17478938836,-19.0616338768185,124.900946309927)) ;
#102843 = CARTESIAN_POINT('Ctrl Pts',(-19.4339240466304,-19.0715190048827,
124.919023725335)) ;
#102844 = CARTESIAN_POINT('Ctrl Pts',(-19.6951092838121,-19.0815101223562,
124.892133492119)) ;
#102845 = CARTESIAN_POINT('Ctrl Pts',(-19.9487459478845,-19.091550738208,
124.819413432375)) ;
#102846 = CARTESIAN_POINT('Ctrl Pts',(-20.1811840640544,-19.1013837290617,
124.70653484289)) ;
#102847 = CARTESIAN_POINT('Ctrl Pts',(-20.3943411849958,-19.111376860512,
124.553155226563)) ;
#102848 = CARTESIAN_POINT('Ctrl Pts',(-20.5779607961446,-19.1214089089474,
124.363967453322)) ;
#102849 = CARTESIAN_POINT('Ctrl Pts',(-20.7237317632523,-19.1312741554898,
124.149599190906)) ;
#102850 = CARTESIAN_POINT('Ctrl Pts',(-20.8317939999319,-19.1412360303166,
123.911146942398)) ;
#102851 = CARTESIAN_POINT('Ctrl Pts',(-20.8968646296207,-19.1512709934279,
123.655608116611)) ;
#102852 = CARTESIAN_POINT('Ctrl Pts',(-20.9167254208125,-19.1611558378903,
123.396566812288)) ;
#102853 = CARTESIAN_POINT('Ctrl Pts',(-20.8907810854594,-19.171221890731,
123.133363415736)) ;
#102854 = CARTESIAN_POINT('Ctrl Pts',(-20.821401757124,-19.18105940664,122.884277322582)) ;
#102855 = CARTESIAN_POINT('Ctrl Pts',(-20.7074990989134,-19.1911281547489,
122.645503335447)) ;
#102856 = CARTESIAN_POINT('Ctrl Pts',(-20.5566118051901,-19.2010086717799,
122.434146389785)) ;
#102857 = CARTESIAN_POINT('Ctrl Pts',(-20.3696719514997,-19.2109998587144,
122.249837001454)) ;
#102858 = CARTESIAN_POINT('Ctrl Pts',(-20.1543532022229,-19.2209529249893,
122.101276348325)) ;
#102859 = CARTESIAN_POINT('Ctrl Pts',(-19.9145523374295,-19.2309887625219,
121.991556903284)) ;
#102860 = CARTESIAN_POINT('Ctrl Pts',(-19.6630559532501,-19.2408788887333,
121.925924400167)) ;
#102861 = CARTESIAN_POINT('Ctrl Pts',(-19.4013754300174,-19.2508710706413,
121.904322728888)) ;
#102862 = CARTESIAN_POINT('Ctrl Pts',(-19.1411235059261,-19.2608170105799,
121.928462871379)) ;
#102863 = CARTESIAN_POINT('Ctrl Pts',(-18.888832049536,-19.270764194344,121.996925162307)) ;
#102864 = CARTESIAN_POINT('Ctrl Pts',(-18.6500106042988,-19.2808121326514,
122.109537997861)) ;
#102865 = CARTESIAN_POINT('Ctrl Pts',(-18.4385333286377,-19.2906597673917,
122.258697701724)) ;
#102866 = CARTESIAN_POINT('Ctrl Pts',(-18.2534839295302,-19.3006214813655,
122.443848789793)) ;
#102867 = CARTESIAN_POINT('Ctrl Pts',(-18.1026428206701,-19.3106501161564,
122.659973777943)) ;
#102868 = CARTESIAN_POINT('Ctrl Pts',(-17.9928644421991,-19.3205604347535,
122.896125581501)) ;
#102869 = CARTESIAN_POINT('Ctrl Pts',(-17.9249226826456,-19.330495291065,
123.148217847419)) ;
#102870 = CARTESIAN_POINT('Ctrl Pts',(-17.9017919560051,-19.3405365270257,
123.411062876142)) ;
#102871 = CARTESIAN_POINT('Ctrl Pts',(-17.9240882463519,-19.3504232986057,
123.669943886338)) ;
#102872 = CARTESIAN_POINT('Ctrl Pts',(-17.9914404271819,-19.3604234773119,
123.923920647487)) ;
#102873 = CARTESIAN_POINT('Ctrl Pts',(-18.1007825311999,-19.3703407555215,
124.160537445714)) ;
#102874 = CARTESIAN_POINT('Ctrl Pts',(-18.2515181964316,-19.3803880019352,
124.377267386815)) ;
#102875 = CARTESIAN_POINT('Ctrl Pts',(-18.4342421500733,-19.3902618909165,
124.561551217845)) ;
#102876 = CARTESIAN_POINT('Ctrl Pts',(-18.6500824820261,-19.400323908497,
124.714238050506)) ;
#102877 = CARTESIAN_POINT('Ctrl Pts',(-18.8846797503778,-19.4101949702313,
124.824974685142)) ;
#102878 = CARTESIAN_POINT('Ctrl Pts',(-19.1378473143189,-19.4201890335916,
124.894848560065)) ;
#102879 = CARTESIAN_POINT('Ctrl Pts',(-19.4003460422337,-19.430221191625,
124.91921432023)) ;
#102880 = CARTESIAN_POINT('Ctrl Pts',(-19.6587612544916,-19.4400850678652,
124.898556778381)) ;
#102881 = CARTESIAN_POINT('Ctrl Pts',(-19.9148714014531,-19.4501555825034,
124.832021587794)) ;
#102882 = CARTESIAN_POINT('Ctrl Pts',(-20.1501011154799,-19.4599962194444,
124.7245403623)) ;
#102883 = CARTESIAN_POINT('Ctrl Pts',(-20.3662873595265,-19.4699633482846,
124.576700551369)) ;
#102884 = CARTESIAN_POINT('Ctrl Pts',(-20.554234692162,-19.4799773214091,
124.392483132149)) ;
#102885 = CARTESIAN_POINT('Ctrl Pts',(-20.757429884363,-19.4932620552724,
124.108579686335)) ;
#102886 = CARTESIAN_POINT('Ctrl Pts',(-20.8815848706378,-19.5064873199872,
123.779792856729)) ;
#102887 = CARTESIAN_POINT('Ctrl Pts',(-20.9167212645903,-19.519797842542,
123.431736281204)) ;
#102888 = CARTESIAN_POINT('Ctrl Pts',(-20.8970459424392,-19.5298264874442,
123.168938625735)) ;
#102889 = CARTESIAN_POINT('Ctrl Pts',(-20.8332169752799,-19.5397075197981,
122.917236633693)) ;
#102890 = CARTESIAN_POINT('Ctrl Pts',(-20.7260774305387,-19.5496884924782,
122.677830163903)) ;
#102891 = CARTESIAN_POINT('Ctrl Pts',(-20.5788138255665,-19.5596696200642,
122.46079673458)) ;
#102892 = CARTESIAN_POINT('Ctrl Pts',(-20.3368625325848,-19.5729128103256,
122.210551925323)) ;
#102893 = CARTESIAN_POINT('Ctrl Pts',(-19.9569993363786,-19.5895808056864,
121.982803218007)) ;
#102894 = CARTESIAN_POINT('Ctrl Pts',(-19.52596625381,-19.6061013056984,121.898737371643)) ;
#102895 = CARTESIAN_POINT('Ctrl Pts',(-19.1769558296142,-19.6194143220144,
121.922390771414)) ;
#102896 = CARTESIAN_POINT('Ctrl Pts',(-18.9238470842411,-19.6293308802474,
121.984587811698)) ;
#102897 = CARTESIAN_POINT('Ctrl Pts',(-18.6828424329629,-19.6393585485503,
122.091010950231)) ;
#102898 = CARTESIAN_POINT('Ctrl Pts',(-18.3945215350689,-19.652539138295,
122.283192537924)) ;
#102899 = CARTESIAN_POINT('Ctrl Pts',(-18.1010219937371,-19.6692872774143,
122.617581162048)) ;
#102900 = CARTESIAN_POINT('Ctrl Pts',(-17.909366822418,-19.6890820199249,
123.107805255079)) ;
#102901 = CARTESIAN_POINT('Ctrl Pts',(-17.895809920963,-19.7091264127337,
123.640196037311)) ;
#102902 = CARTESIAN_POINT('Ctrl Pts',(-18.0635546861433,-19.7289655950324,
124.140244908333)) ;
#102903 = CARTESIAN_POINT('Ctrl Pts',(-18.3921051298467,-19.7488909187253,
124.55542693416)) ;
#102904 = CARTESIAN_POINT('Ctrl Pts',(-18.8427943342149,-19.7688145567768,
124.833601017677)) ;
#102905 = CARTESIAN_POINT('Ctrl Pts',(-19.3612107685592,-19.7887394302423,
124.941419506668)) ;
#102906 = CARTESIAN_POINT('Ctrl Pts',(-19.8842729339696,-19.8086180373213,
124.866702744528)) ;
#102907 = CARTESIAN_POINT('Ctrl Pts',(-20.3528435141273,-19.8285954801532,
124.616989142278)) ;
#102908 = CARTESIAN_POINT('Ctrl Pts',(-20.7070256130225,-19.8485273282379,
124.222974020889)) ;
#102909 = CARTESIAN_POINT('Ctrl Pts',(-20.9055758496834,-19.8684225965805,
123.732917749961)) ;
#102910 = CARTESIAN_POINT('Ctrl Pts',(-20.9255964967024,-19.8883450949926,
123.203776230308)) ;
#102911 = CARTESIAN_POINT('Ctrl Pts',(-20.7634093889317,-19.9083045768686,
122.698654704023)) ;
#102912 = CARTESIAN_POINT('Ctrl Pts',(-20.4400618251657,-19.928182329328,
122.28094819623)) ;
#102913 = CARTESIAN_POINT('Ctrl Pts',(-19.9941413395738,-19.9480641200625,
121.997227995206)) ;
#102914 = CARTESIAN_POINT('Ctrl Pts',(-19.4731423142849,-19.9681374589135,
121.882681860744)) ;
#102915 = CARTESIAN_POINT('Ctrl Pts',(-18.9512149180484,-19.9879419261493,
121.95174640087)) ;
#102916 = CARTESIAN_POINT('Ctrl Pts',(-18.4795837406758,-20.0079252665571,
122.195835512753)) ;
#102917 = CARTESIAN_POINT('Ctrl Pts',(-18.121364945746,-20.0278402311551,
122.585509526284)) ;
#102918 = CARTESIAN_POINT('Ctrl Pts',(-17.9166956650287,-20.0477087658715,
123.072415316463)) ;
#102919 = CARTESIAN_POINT('Ctrl Pts',(-17.891101767472,-20.0677611500832,
123.604604745487)) ;
#102920 = CARTESIAN_POINT('Ctrl Pts',(-18.0458952100454,-20.0875351138724,
124.107071415621)) ;
#102921 = CARTESIAN_POINT('Ctrl Pts',(-18.3667694167037,-20.1075894928938,
124.532413135122)) ;
#102922 = CARTESIAN_POINT('Ctrl Pts',(-18.8082077697032,-20.127386230467,
124.819020798246)) ;
#102923 = CARTESIAN_POINT('Ctrl Pts',(-19.3247806063206,-20.1473540428185,
124.940185255998)) ;
#102924 = CARTESIAN_POINT('Ctrl Pts',(-19.8515809478242,-20.1673130188835,
124.876974888948)) ;
#102925 = CARTESIAN_POINT('Ctrl Pts',(-20.3237113753369,-20.1872079371609,
124.638913265828)) ;
#102926 = CARTESIAN_POINT('Ctrl Pts',(-20.6867453183494,-20.2071042496112,
124.254470582453)) ;
#102927 = CARTESIAN_POINT('Ctrl Pts',(-20.8974946288054,-20.2270121829853,
123.769091874929)) ;
#102928 = CARTESIAN_POINT('Ctrl Pts',(-20.9299647653081,-20.2469620732738,
123.239897350838)) ;
#102929 = CARTESIAN_POINT('Ctrl Pts',(-20.7809358296733,-20.2668393037751,
122.732995434889)) ;
#102930 = CARTESIAN_POINT('Ctrl Pts',(-20.4664775913345,-20.2868219726461,
122.30502079141)) ;
#102931 = CARTESIAN_POINT('Ctrl Pts',(-20.025672670458,-20.3067548592265,
122.011026793588)) ;
#102932 = CARTESIAN_POINT('Ctrl Pts',(-19.5117141072868,-20.3266676052444,
121.884911373776)) ;
#102933 = CARTESIAN_POINT('Ctrl Pts',(-19.0738174714557,-20.3432373265862,
121.931707774582)) ;
#102934 = CARTESIAN_POINT('Ctrl Pts',(-18.7476557838818,-20.3565373378912,
122.057330938408)) ;
#102935 = CARTESIAN_POINT('Ctrl Pts',(-18.4486713364495,-20.3698075256411,
122.236858838282)) ;
#102936 = CARTESIAN_POINT('Ctrl Pts',(-18.1413778651806,-20.3864349080065,
122.554468364598)) ;
#102937 = CARTESIAN_POINT('Ctrl Pts',(-17.9611321734678,-20.4030571977517,
122.957827369364)) ;
#102938 = CARTESIAN_POINT('Ctrl Pts',(-17.9059585339821,-20.4163024121462,
123.301491619911)) ;
#102939 = CARTESIAN_POINT('Ctrl Pts',(-17.9091824912486,-20.4262143771069,
123.561964967123)) ;
#102940 = CARTESIAN_POINT('Ctrl Pts',(-17.9585940033797,-20.4362730002714,
123.821606026611)) ;
#102941 = CARTESIAN_POINT('Ctrl Pts',(-18.0499666096224,-20.4461131143872,
124.063553454512)) ;
#102942 = CARTESIAN_POINT('Ctrl Pts',(-18.1847206871367,-20.4561788993448,
124.291128959096)) ;
#102943 = CARTESIAN_POINT('Ctrl Pts',(-18.3539526261617,-20.4660622171327,
124.488192945778)) ;
#102944 = CARTESIAN_POINT('Ctrl Pts',(-18.5565782082668,-20.4760516549913,
124.65505176709)) ;
#102945 = CARTESIAN_POINT('Ctrl Pts',(-18.7845893768725,-20.486015369044,
124.78379811177)) ;
#102946 = CARTESIAN_POINT('Ctrl Pts',(-19.0321816787144,-20.4960103807032,
124.871535154767)) ;
#102947 = CARTESIAN_POINT('Ctrl Pts',(-19.2923532152617,-20.5060466723975,
124.914716267996)) ;
#102948 = CARTESIAN_POINT('Ctrl Pts',(-19.551111783383,-20.5158930500909,
124.91253933925)) ;
#102949 = CARTESIAN_POINT('Ctrl Pts',(-19.8091810772664,-20.5258779942416,
124.865307212237)) ;
#102950 = CARTESIAN_POINT('Ctrl Pts',(-20.0540749680961,-20.5358149653716,
124.774537714815)) ;
#102951 = CARTESIAN_POINT('Ctrl Pts',(-20.2819182027391,-20.5458647500033,
124.641041024722)) ;
#102952 = CARTESIAN_POINT('Ctrl Pts',(-20.4792920820102,-20.5557152120808,
124.473524605348)) ;
#102953 = CARTESIAN_POINT('Ctrl Pts',(-20.6471130882054,-20.5656872256012,
124.272300643355)) ;
#102954 = CARTESIAN_POINT('Ctrl Pts',(-20.7777557364887,-20.5756823727206,
124.044383982858)) ;
#102955 = CARTESIAN_POINT('Ctrl Pts',(-20.8668637360059,-20.5857163424567,
123.796238570436)) ;
#102956 = CARTESIAN_POINT('Ctrl Pts',(-20.9111469349061,-20.5955718881273,
123.541034504517)) ;
#102957 = CARTESIAN_POINT('Ctrl Pts',(-20.910805235039,-20.6055706451405,
123.278320314921)) ;
#102958 = CARTESIAN_POINT('Ctrl Pts',(-20.8655510690392,-20.6154677803777,
123.022161686187)) ;
#102959 = CARTESIAN_POINT('Ctrl Pts',(-20.7751709880732,-20.6255208762173,
122.77394668237)) ;
#102960 = CARTESIAN_POINT('Ctrl Pts',(-20.6452938391844,-20.6354043849479,
122.549002249442)) ;
#102961 = CARTESIAN_POINT('Ctrl Pts',(-20.4769385117555,-20.645399257594,
122.347408995479)) ;
#102962 = CARTESIAN_POINT('Ctrl Pts',(-20.2753518309184,-20.6554192192297,
122.177984016377)) ;
#102963 = CARTESIAN_POINT('Ctrl Pts',(-20.0501418873973,-20.6653245830296,
122.047462176748)) ;
#102964 = CARTESIAN_POINT('Ctrl Pts',(-19.8050172500671,-20.6752651706371,
121.957212454347)) ;
#102965 = CARTESIAN_POINT('Ctrl Pts',(-19.5463161812984,-20.6852679887378,
121.910449024445)) ;
#102966 = CARTESIAN_POINT('Ctrl Pts',(-19.2826301691876,-20.6953027004619,
121.909741281856)) ;
#102967 = CARTESIAN_POINT('Ctrl Pts',(-19.0276353696205,-20.7051476071992,
121.953549369446)) ;
#102968 = CARTESIAN_POINT('Ctrl Pts',(-18.7805229407793,-20.7151334597682,
122.041734471525)) ;
#102969 = CARTESIAN_POINT('Ctrl Pts',(-18.5534712355845,-20.7250682681813,
122.170706323137)) ;
#102970 = CARTESIAN_POINT('Ctrl Pts',(-18.349994251646,-20.7351257952623,
122.339324859272)) ;
#102971 = CARTESIAN_POINT('Ctrl Pts',(-18.1825547646236,-20.7449474502594,
122.53578295703)) ;
#102972 = CARTESIAN_POINT('Ctrl Pts',(-18.0482494320608,-20.7550034944324,
122.763346656922)) ;
#102973 = CARTESIAN_POINT('Ctrl Pts',(-17.9569902871531,-20.7649442344776,
123.008132090239)) ;
#102974 = CARTESIAN_POINT('Ctrl Pts',(-17.9089930326973,-20.7748483555505,
123.263941618772)) ;
#102975 = CARTESIAN_POINT('Ctrl Pts',(-17.9062624092731,-20.7848958967047,
123.527947604449)) ;
#102976 = CARTESIAN_POINT('Ctrl Pts',(-17.9485941174404,-20.7947946483051,
123.784643968814)) ;
#102977 = CARTESIAN_POINT('Ctrl Pts',(-18.0360287409758,-20.8048431272709,
124.033781132418)) ;
#102978 = CARTESIAN_POINT('Ctrl Pts',(-18.1633313086099,-20.8147306243546,
124.260323795961)) ;
#102979 = CARTESIAN_POINT('Ctrl Pts',(-18.3293850310261,-20.8247237146527,
124.463737195209)) ;
#102980 = CARTESIAN_POINT('Ctrl Pts',(-18.5275098785062,-20.834675884713,
124.634482989374)) ;
#102981 = CARTESIAN_POINT('Ctrl Pts',(-18.7517494695922,-20.8446143046275,
124.768339766333)) ;
#102982 = CARTESIAN_POINT('Ctrl Pts',(-18.9969080813788,-20.8545994347131,
124.861956432317)) ;
#102983 = CARTESIAN_POINT('Ctrl Pts',(-19.2559596960838,-20.8646361241272,
124.911446981312)) ;
#102984 = CARTESIAN_POINT('Ctrl Pts',(-19.5149214807583,-20.8744908081197,
124.915551065454)) ;
#102985 = CARTESIAN_POINT('Ctrl Pts',(-19.7744091532939,-20.8844902921675,
124.874396265208)) ;
#102986 = CARTESIAN_POINT('Ctrl Pts',(-20.0203900027022,-20.8943853809444,
124.789938115145)) ;
#102987 = CARTESIAN_POINT('Ctrl Pts',(-20.2516933373412,-20.9044459355906,
124.661962233862)) ;
#102988 = CARTESIAN_POINT('Ctrl Pts',(-20.4530789831576,-20.9142951999635,
124.499338199125)) ;
#102989 = CARTESIAN_POINT('Ctrl Pts',(-20.6267269098642,-20.9243224524113,
124.301150734394)) ;
#102990 = CARTESIAN_POINT('Ctrl Pts',(-20.7627565155963,-20.9343507499815,
124.075425085885)) ;
#102991 = CARTESIAN_POINT('Ctrl Pts',(-20.8562610600109,-20.9441968789875,
123.834176131167)) ;
#102992 = CARTESIAN_POINT('Ctrl Pts',(-20.9078567319107,-20.9541907843496,
123.576665766039)) ;
#102993 = CARTESIAN_POINT('Ctrl Pts',(-20.9135030485814,-20.9642148820326,
123.313296632163)) ;
#102994 = CARTESIAN_POINT('Ctrl Pts',(-20.8741952660944,-20.9741047098866,
123.056387254007)) ;
#102995 = CARTESIAN_POINT('Ctrl Pts',(-20.7903835125516,-20.9840966913171,
122.807554523007)) ;
#102996 = CARTESIAN_POINT('Ctrl Pts',(-20.6651455635319,-20.9940436960829,
122.57811162279)) ;
#102997 = CARTESIAN_POINT('Ctrl Pts',(-20.5022967865992,-21.0039933474727,
122.373537200791)) ;
#102998 = CARTESIAN_POINT('Ctrl Pts',(-20.3045524600773,-21.0140303504501,
122.198999390987)) ;
#102999 = CARTESIAN_POINT('Ctrl Pts',(-20.0829076432047,-21.0239192588851,
122.063311855875)) ;
#103000 = CARTESIAN_POINT('Ctrl Pts',(-19.8388031235912,-21.0339085913626,
121.966768231352)) ;
#103001 = CARTESIAN_POINT('Ctrl Pts',(-19.5823974992214,-21.0438671467997,
121.914430184052)) ;
#103002 = CARTESIAN_POINT('Ctrl Pts',(-19.3223423892364,-21.0537667180002,
121.906807082868)) ;
#103003 = CARTESIAN_POINT('Ctrl Pts',(-19.0611133552447,-21.0638146432522,
121.9451043463)) ;
#103004 = CARTESIAN_POINT('Ctrl Pts',(-18.8141787709719,-21.0737099427782,
122.026742494562)) ;
#103005 = CARTESIAN_POINT('Ctrl Pts',(-18.5813642148825,-21.0837717992262,
122.152027144941)) ;
#103006 = CARTESIAN_POINT('Ctrl Pts',(-18.3782691537802,-21.0936156456428,
122.312269335965)) ;
#103007 = CARTESIAN_POINT('Ctrl Pts',(-18.2033434375949,-21.1035785947709,
122.507056289126)) ;
#103008 = CARTESIAN_POINT('Ctrl Pts',(-18.0642661544428,-21.1136126311989,
122.731089182587)) ;
#103009 = CARTESIAN_POINT('Ctrl Pts',(-17.9673844345331,-21.1235000581569,
122.972179630959)) ;
#103010 = CARTESIAN_POINT('Ctrl Pts',(-17.9126540899515,-21.1335144924933,
123.229612712998)) ;
#103011 = CARTESIAN_POINT('Ctrl Pts',(-17.904097359486,-21.1435494371282,
123.49316382186)) ;
#103012 = CARTESIAN_POINT('Ctrl Pts',(-17.9399843509663,-21.1533817871592,
123.749075900176)) ;
#103013 = CARTESIAN_POINT('Ctrl Pts',(-18.0216348559207,-21.1634572262764,
124.000890325645)) ;
#103014 = CARTESIAN_POINT('Ctrl Pts',(-18.1429385335259,-21.173309691511,
124.229691572108)) ;
#103015 = CARTESIAN_POINT('Ctrl Pts',(-18.3054583562848,-21.1833825690879,
124.438574276318)) ;
#103016 = CARTESIAN_POINT('Ctrl Pts',(-18.497363701808,-21.1932251652804,
124.612025900992)) ;
#103017 = CARTESIAN_POINT('Ctrl Pts',(-18.7190400369266,-21.2032055493957,
124.752173819842)) ;
#103018 = CARTESIAN_POINT('Ctrl Pts',(-18.9628084773325,-21.2132240300445,
124.85161003546)) ;
#103019 = CARTESIAN_POINT('Ctrl Pts',(-19.2165871989397,-21.2231073450449,
124.907009598453)) ;
#103020 = CARTESIAN_POINT('Ctrl Pts',(-19.480916018816,-21.2331756421353,
124.917579442169)) ;
#103021 = CARTESIAN_POINT('Ctrl Pts',(-19.7369923043346,-21.2430057105076,
124.883224806794)) ;
#103022 = CARTESIAN_POINT('Ctrl Pts',(-19.9891518722698,-21.253072502976,
124.803386738475)) ;
#103023 = CARTESIAN_POINT('Ctrl Pts',(-20.2195154038845,-21.2629618364645,
124.682990140707)) ;
#103024 = CARTESIAN_POINT('Ctrl Pts',(-20.4280013834281,-21.2729639678806,
124.523000164599)) ;
#103025 = CARTESIAN_POINT('Ctrl Pts',(-20.6043386706282,-21.2828878375016,
124.330801370048)) ;
#103026 = CARTESIAN_POINT('Ctrl Pts',(-20.7462043849423,-21.2929313530188,
124.108284226744)) ;
#103027 = CARTESIAN_POINT('Ctrl Pts',(-20.8459679731605,-21.3028135659071,
123.868464248691)) ;
#103028 = CARTESIAN_POINT('Ctrl Pts',(-20.9036138188214,-21.3128816431265,
123.610292216186)) ;
#103029 = CARTESIAN_POINT('Ctrl Pts',(-20.9155213503014,-21.3227201478607,
123.35197747628)) ;
#103030 = CARTESIAN_POINT('Ctrl Pts',(-20.882022828367,-21.3327829162901,
123.089701598877)) ;
#103031 = CARTESIAN_POINT('Ctrl Pts',(-20.8045024152321,-21.3426799095728,
122.841423981398)) ;
#103032 = CARTESIAN_POINT('Ctrl Pts',(-20.6854221679011,-21.3526111372076,
122.609199073492)) ;
#103033 = CARTESIAN_POINT('Ctrl Pts',(-20.5258361470351,-21.3626532958498,
122.399026647855)) ;
#103034 = CARTESIAN_POINT('Ctrl Pts',(-20.335295369946,-21.3725400053808,
122.222383437198)) ;
#103035 = CARTESIAN_POINT('Ctrl Pts',(-20.1148920105634,-21.3825329778094,
122.079633715009)) ;
#103036 = CARTESIAN_POINT('Ctrl Pts',(-19.874132060502,-21.392479172346,121.977899698688)) ;
#103037 = CARTESIAN_POINT('Ctrl Pts',(-19.619487828393,-21.4024245471975,
121.918954900384)) ;
#103038 = CARTESIAN_POINT('Ctrl Pts',(-19.355633681364,-21.4124794665574,
121.90537882635)) ;
#103039 = CARTESIAN_POINT('Ctrl Pts',(-19.0993925483528,-21.4223009860009,
121.936586065926)) ;
#103040 = CARTESIAN_POINT('Ctrl Pts',(-18.8463064545216,-21.4323667547678,
122.013350173819)) ;
#103041 = CARTESIAN_POINT('Ctrl Pts',(-18.6141903792283,-21.4422686764229,
122.131067840634)) ;
#103042 = CARTESIAN_POINT('Ctrl Pts',(-18.4029908552068,-21.4523117352439,
122.289297152131)) ;
#103043 = CARTESIAN_POINT('Ctrl Pts',(-18.2250163310526,-21.4622177292866,
122.479284295807)) ;
#103044 = CARTESIAN_POINT('Ctrl Pts',(-18.0816390507141,-21.4721555023684,
122.697559547165)) ;
#103045 = CARTESIAN_POINT('Ctrl Pts',(-17.9775347354648,-21.4821958661007,
122.93999855582)) ;
#103046 = CARTESIAN_POINT('Ctrl Pts',(-17.9178327043181,-21.4920832098242,
123.192889506299)) ;
#103047 = CARTESIAN_POINT('Ctrl Pts',(-17.9023592109416,-21.5020754403929,
123.455000740661)) ;
#103048 = CARTESIAN_POINT('Ctrl Pts',(-17.932574065848,-21.5120239681765,
123.714700805199)) ;
#103049 = CARTESIAN_POINT('Ctrl Pts',(-18.0069709592114,-21.5219607518998,
123.96498403759)) ;
#103050 = CARTESIAN_POINT('Ctrl Pts',(-18.1239652382464,-21.5319437526968,
124.19983233919)) ;
#103051 = CARTESIAN_POINT('Ctrl Pts',(-18.2812638755479,-21.5419876395375,
124.411744040751)) ;
#103052 = CARTESIAN_POINT('Ctrl Pts',(-18.4684771481932,-21.5518156631121,
124.589722525419)) ;
#103053 = CARTESIAN_POINT('Ctrl Pts',(-18.6890622519546,-21.5618929113257,
124.736146499577)) ;
#103054 = CARTESIAN_POINT('Ctrl Pts',(-18.9262831897705,-21.571742466631,
124.839866711791)) ;
#103055 = CARTESIAN_POINT('Ctrl Pts',(-19.1837109370141,-21.5818251748287,
124.902321257173)) ;
#103056 = CARTESIAN_POINT('Ctrl Pts',(-19.4410990137253,-21.5916377677552,
124.918921324758)) ;
#103057 = CARTESIAN_POINT('Ctrl Pts',(-19.7040389778254,-21.6017049600131,
124.890283048856)) ;
#103058 = CARTESIAN_POINT('Ctrl Pts',(-19.9538585647511,-21.6116037894757,
124.817532450528)) ;
#103059 = CARTESIAN_POINT('Ctrl Pts',(-20.190850254731,-21.6216577806659,
124.70086379783)) ;
#103060 = CARTESIAN_POINT('Ctrl Pts',(-20.4003453171427,-21.6315295054491,
124.547768619076)) ;
#103061 = CARTESIAN_POINT('Ctrl Pts',(-20.5836703121045,-21.6415999475793,
124.356973135958)) ;
#103062 = CARTESIAN_POINT('Ctrl Pts',(-20.7277436846726,-21.6514330260096,
124.142431575118)) ;
#103063 = CARTESIAN_POINT('Ctrl Pts',(-20.8351504550266,-21.661463499511,
123.90172744066)) ;
#103064 = CARTESIAN_POINT('Ctrl Pts',(-20.8983991892578,-21.6714950988097,
123.64579221545)) ;
#103065 = CARTESIAN_POINT('Ctrl Pts',(-20.9164245493496,-21.6813247998478,
123.38812458234)) ;
#103066 = CARTESIAN_POINT('Ctrl Pts',(-20.8897753449529,-21.6913142379043,
123.126960779477)) ;
#103067 = CARTESIAN_POINT('Ctrl Pts',(-20.8171517828939,-21.7013581411204,
122.873208967766)) ;
#103068 = CARTESIAN_POINT('Ctrl Pts',(-20.7046129996104,-21.7111796619339,
122.640934622164)) ;
#103069 = CARTESIAN_POINT('Ctrl Pts',(-20.5506729712625,-21.721215386181,
122.426803905934)) ;
#103070 = CARTESIAN_POINT('Ctrl Pts',(-20.3616525439628,-21.7312375401135,
122.243374779076)) ;
#103071 = CARTESIAN_POINT('Ctrl Pts',(-20.1474024551261,-21.7410997718708,
122.097582456974)) ;
#103072 = CARTESIAN_POINT('Ctrl Pts',(-19.9090500324287,-21.7510588423287,
121.989478779301)) ;
#103073 = CARTESIAN_POINT('Ctrl Pts',(-19.6535274553849,-21.7610940147049,
121.924306461596)) ;
#103074 = CARTESIAN_POINT('Ctrl Pts',(-19.3946169510934,-21.7709743998631,
121.904405437011)) ;
#103075 = CARTESIAN_POINT('Ctrl Pts',(-19.1316158970856,-21.7810311144571,
121.930107076783)) ;
#103076 = CARTESIAN_POINT('Ctrl Pts',(-18.881530454905,-21.7909103830291,
121.999860465545)) ;
#103077 = CARTESIAN_POINT('Ctrl Pts',(-18.6444162627727,-21.8009013405148,
122.112601623347)) ;
#103078 = CARTESIAN_POINT('Ctrl Pts',(-18.4297519054492,-21.81094199915,122.266033649848)) ;
#103079 = CARTESIAN_POINT('Ctrl Pts',(-18.2485066413197,-21.820774978858,
122.450203319049)) ;
#103080 = CARTESIAN_POINT('Ctrl Pts',(-18.0989867796727,-21.8307681121077,
122.666085929148)) ;
#103081 = CARTESIAN_POINT('Ctrl Pts',(-17.9892868503184,-21.8408001644911,
122.905823378761)) ;
#103082 = CARTESIAN_POINT('Ctrl Pts',(-17.9236804014323,-21.8506653934424,
123.156619439682)) ;
#103083 = CARTESIAN_POINT('Ctrl Pts',(-17.9016709296065,-21.8606273346856,
123.417488992324)) ;
#103084 = CARTESIAN_POINT('Ctrl Pts',(-17.9258855366859,-21.8706620497224,
123.680064384478)) ;
#103085 = CARTESIAN_POINT('Ctrl Pts',(-17.9939001600136,-21.8805478200664,
123.930823539983)) ;
#103086 = CARTESIAN_POINT('Ctrl Pts',(-18.1063745150095,-21.8906104174552,
124.170110652052)) ;
#103087 = CARTESIAN_POINT('Ctrl Pts',(-18.2554119033243,-21.9004608292904,
124.381785675874)) ;
#103088 = CARTESIAN_POINT('Ctrl Pts',(-18.4417337007626,-21.9104879985763,
124.568103740414)) ;
#103089 = CARTESIAN_POINT('Ctrl Pts',(-18.6579939619435,-21.9205154792905,
124.718691412592)) ;
#103090 = CARTESIAN_POINT('Ctrl Pts',(-18.8924886711707,-21.9303585318698,
124.827847491686)) ;
#103091 = CARTESIAN_POINT('Ctrl Pts',(-19.1460388774625,-21.9403524353084,
124.89630229536)) ;
#103092 = CARTESIAN_POINT('Ctrl Pts',(-19.4085429207099,-21.9503795580848,
124.919288369219)) ;
#103093 = CARTESIAN_POINT('Ctrl Pts',(-19.6675055964963,-21.9602702629769,
124.896983045597)) ;
#103094 = CARTESIAN_POINT('Ctrl Pts',(-19.9213201022087,-21.9702622898272,
124.829737172689)) ;
#103095 = CARTESIAN_POINT('Ctrl Pts',(-20.15847886615,-21.9802082713157,124.719877290548)) ;
#103096 = CARTESIAN_POINT('Ctrl Pts',(-20.3732998849386,-21.9901554439376,
124.5709137519)) ;
#103097 = CARTESIAN_POINT('Ctrl Pts',(-20.5606494682345,-22.0002033852638,
124.384856178844)) ;
#103098 = CARTESIAN_POINT('Ctrl Pts',(-20.7099988055723,-22.0100510190716,
124.173512790482)) ;
#103099 = CARTESIAN_POINT('Ctrl Pts',(-20.8223974749045,-22.0200127337566,
123.937100416277)) ;
#103100 = CARTESIAN_POINT('Ctrl Pts',(-20.8921927790865,-22.0300413666351,
123.68295199388)) ;
#103101 = CARTESIAN_POINT('Ctrl Pts',(-20.9165923031643,-22.0399516921703,
123.423675234886)) ;
#103102 = CARTESIAN_POINT('Ctrl Pts',(-20.8962261425128,-22.049886522642,
123.16338835777)) ;
#103103 = CARTESIAN_POINT('Ctrl Pts',(-20.8300596435393,-22.059927855024,
122.907943513216)) ;
#103104 = CARTESIAN_POINT('Ctrl Pts',(-20.7222498519845,-22.0698207284628,
122.671379324634)) ;
#103105 = CARTESIAN_POINT('Ctrl Pts',(-20.5744090303829,-22.0797898942807,
122.455088308952)) ;
#103106 = CARTESIAN_POINT('Ctrl Pts',(-20.3898730535669,-22.0898186279972,
122.266962233165)) ;
#103107 = CARTESIAN_POINT('Ctrl Pts',(-20.1081955733599,-22.1030111467684,
122.064734080855)) ;
#103108 = CARTESIAN_POINT('Ctrl Pts',(-19.7762060672709,-22.1163710148111,
121.939114499556)) ;
#103109 = CARTESIAN_POINT('Ctrl Pts',(-19.4303000677635,-22.1295963519599,
121.904601540361)) ;
#103110 = CARTESIAN_POINT('Ctrl Pts',(-19.1686956935908,-22.1395775778005,
121.92351886695)) ;
#103111 = CARTESIAN_POINT('Ctrl Pts',(-18.9130905640444,-22.1496131447834,
121.988419973829)) ;
#103112 = CARTESIAN_POINT('Ctrl Pts',(-18.6765215819154,-22.1594762227455,
122.094390069791)) ;
#103113 = CARTESIAN_POINT('Ctrl Pts',(-18.4574524440077,-22.1695465215466,
122.242803036002)) ;
#103114 = CARTESIAN_POINT('Ctrl Pts',(-18.2717635384097,-22.1793888201144,
122.422867545221)) ;
#103115 = CARTESIAN_POINT('Ctrl Pts',(-18.1175643025741,-22.1893495182842,
122.634377147575)) ;
#103116 = CARTESIAN_POINT('Ctrl Pts',(-18.0020115450616,-22.1993875524637,
122.871500055284)) ;
#103117 = CARTESIAN_POINT('Ctrl Pts',(-17.930094357224,-22.2092612893102,
123.120841153412)) ;
#103118 = CARTESIAN_POINT('Ctrl Pts',(-17.9020504852517,-22.2193330732354,
123.383989693628)) ;
#103119 = CARTESIAN_POINT('Ctrl Pts',(-17.919540669824,-22.2291651944366,
123.64179986069)) ;
#103120 = CARTESIAN_POINT('Ctrl Pts',(-17.9820987955185,-22.239198218462,
123.897915110287)) ;
#103121 = CARTESIAN_POINT('Ctrl Pts',(-18.0886241992968,-22.2492140986587,
124.138620611349)) ;
#103122 = CARTESIAN_POINT('Ctrl Pts',(-18.2329762887134,-22.2590976177529,
124.354539801381)) ;
#103123 = CARTESIAN_POINT('Ctrl Pts',(-18.4143130469841,-22.2690880301166,
124.544365461022)) ;
#103124 = CARTESIAN_POINT('Ctrl Pts',(-18.6951226688525,-22.28235119332,124.750870336267)) ;
#103125 = CARTESIAN_POINT('Ctrl Pts',(-19.0235872633062,-22.2956287635712,
124.879796807948)) ;
#103126 = CARTESIAN_POINT('Ctrl Pts',(-19.3717516624237,-22.3089590660778,
124.918805307772)) ;
#103127 = CARTESIAN_POINT('Ctrl Pts',(-19.6313839899899,-22.3188577478942,
124.902827623068)) ;
#103128 = CARTESIAN_POINT('Ctrl Pts',(-19.8866875692019,-22.3288472629417,
124.841760132005)) ;
#103129 = CARTESIAN_POINT('Ctrl Pts',(-20.1265240138423,-22.3387953147168,
124.73770586558)) ;
#103130 = CARTESIAN_POINT('Ctrl Pts',(-20.3446612835695,-22.3487367179953,
124.593976175479)) ;
#103131 = CARTESIAN_POINT('Ctrl Pts',(-20.5987501854537,-22.3620233827762,
124.354444327464)) ;
#103132 = CARTESIAN_POINT('Ctrl Pts',(-20.8307578098562,-22.378633804431,
123.978886976682)) ;
#103133 = CARTESIAN_POINT('Ctrl Pts',(-20.9389570638948,-22.3985450666818,
123.460837785839)) ;
#103134 = CARTESIAN_POINT('Ctrl Pts',(-20.8639559060425,-22.4184891958467,
122.936059319112)) ;
#103135 = CARTESIAN_POINT('Ctrl Pts',(-20.6146168497049,-22.4384123584518,
122.46896784405)) ;
#103136 = CARTESIAN_POINT('Ctrl Pts',(-20.2219980709567,-22.4583024808584,
122.114843596429)) ;
#103137 = CARTESIAN_POINT('Ctrl Pts',(-19.7292742311084,-22.4783074344585,
121.91524683107)) ;
#103138 = CARTESIAN_POINT('Ctrl Pts',(-19.2022755216154,-22.4981456914741,
121.895507427705)) ;
#103139 = CARTESIAN_POINT('Ctrl Pts',(-18.6962165202482,-22.5181399922607,
122.057490332449)) ;
#103140 = CARTESIAN_POINT('Ctrl Pts',(-18.278334233107,-22.5380252343051,
122.381092030376)) ;
#103141 = CARTESIAN_POINT('Ctrl Pts',(-17.9948603071649,-22.557900180781,
122.826830133635)) ;
#103142 = CARTESIAN_POINT('Ctrl Pts',(-17.8799975526661,-22.5779332507221,
123.3467920993)) ;
#103143 = CARTESIAN_POINT('Ctrl Pts',(-17.9496067756864,-22.5978217576225,
123.870746392189)) ;
#103144 = CARTESIAN_POINT('Ctrl Pts',(-18.1918518597554,-22.6176766174038,
124.339658601302)) ;
#103145 = CARTESIAN_POINT('Ctrl Pts',(-18.5838377446727,-22.6377274511915,
124.700512523635)) ;
#103146 = CARTESIAN_POINT('Ctrl Pts',(-19.0684699146769,-22.6574933930808,
124.903664781384)) ;
#103147 = CARTESIAN_POINT('Ctrl Pts',(-19.5995371461108,-22.6775061245401,
124.930607581671)) ;
#103148 = CARTESIAN_POINT('Ctrl Pts',(-20.1049471997775,-22.6973989594837,
124.774872824804)) ;
#103149 = CARTESIAN_POINT('Ctrl Pts',(-20.5274891334614,-22.7173059828232,
124.456654840816)) ;
#103150 = CARTESIAN_POINT('Ctrl Pts',(-20.8168362162769,-22.7372212477239,
124.013275946578)) ;
#103151 = CARTESIAN_POINT('Ctrl Pts',(-20.9375204682775,-22.7572529398836,
123.49476876115)) ;
#103152 = CARTESIAN_POINT('Ctrl Pts',(-20.8746410235034,-22.7770959864566,
122.971080233954)) ;
#103153 = CARTESIAN_POINT('Ctrl Pts',(-20.6370945925623,-22.7970125343564,
122.498111517226)) ;
#103154 = CARTESIAN_POINT('Ctrl Pts',(-20.2519505607722,-22.8169447773477,
122.134290696217)) ;
#103155 = CARTESIAN_POINT('Ctrl Pts',(-19.7666480927103,-22.836848612157,
121.923807479693)) ;
#103156 = CARTESIAN_POINT('Ctrl Pts',(-19.2387574124756,-22.8567490123445,
121.890907261899)) ;
#103157 = CARTESIAN_POINT('Ctrl Pts',(-18.7299851185306,-22.8766986887238,
122.040287415327)) ;
#103158 = CARTESIAN_POINT('Ctrl Pts',(-18.303172348133,-22.8966312129442,
122.354132363191)) ;
#103159 = CARTESIAN_POINT('Ctrl Pts',(-18.0088689587993,-22.9165512219304,
122.794285149037)) ;
#103160 = CARTESIAN_POINT('Ctrl Pts',(-17.8822993686623,-22.9365081281066,
123.309329742268)) ;
#103161 = CARTESIAN_POINT('Ctrl Pts',(-17.9384199625223,-22.9563939676081,
123.834975464313)) ;
#103162 = CARTESIAN_POINT('Ctrl Pts',(-18.1715050238201,-22.9763651397439,
124.311731312162)) ;
#103163 = CARTESIAN_POINT('Ctrl Pts',(-18.5499250225676,-22.9961793367283,
124.678096641438)) ;
#103164 = CARTESIAN_POINT('Ctrl Pts',(-19.0342409000383,-23.0161605226965,
124.895731433432)) ;
#103165 = CARTESIAN_POINT('Ctrl Pts',(-19.4736675616231,-23.0327360280858,
124.92808622069)) ;
#103166 = CARTESIAN_POINT('Ctrl Pts',(-19.8173439997547,-23.0460454759494,
124.863128979143)) ;
#103167 = CARTESIAN_POINT('Ctrl Pts',(-20.1458789841394,-23.059413173726,
124.738730813159)) ;
#103168 = CARTESIAN_POINT('Ctrl Pts',(-20.5018784820625,-23.0759037453919,
124.483077299164)) ;
#103169 = CARTESIAN_POINT('Ctrl Pts',(-20.8018393980275,-23.0958240177247,
124.046891204842)) ;
#103170 = CARTESIAN_POINT('Ctrl Pts',(-20.9126929215767,-23.1124410534457,
123.619343331214)) ;
#103171 = CARTESIAN_POINT('Ctrl Pts',(-20.9100857742586,-23.1257319037268,
123.27005760007)) ;
#103172 = CARTESIAN_POINT('Ctrl Pts',(-20.8627965255506,-23.1357009488813,
123.012413426442)) ;
#103173 = CARTESIAN_POINT('Ctrl Pts',(-20.7725539965667,-23.1456043395148,
122.768277127113)) ;
#103174 = CARTESIAN_POINT('Ctrl Pts',(-20.6391518971756,-23.1556621256276,
122.540138510924)) ;
#103175 = CARTESIAN_POINT('Ctrl Pts',(-20.4718019191149,-23.1655141622773,
122.342561323928)) ;
#103176 = CARTESIAN_POINT('Ctrl Pts',(-20.2020922063009,-23.1788792864205,
122.117601499153)) ;
#103177 = CARTESIAN_POINT('Ctrl Pts',(-19.8829803021328,-23.1921053493835,
121.970099825569)) ;
#103178 = CARTESIAN_POINT('Ctrl Pts',(-19.5386223026728,-23.2054089976658,
121.909883631359)) ;
#103179 = CARTESIAN_POINT('Ctrl Pts',(-19.2760224027654,-23.2154005288288,
121.910123653144)) ;
#103180 = CARTESIAN_POINT('Ctrl Pts',(-19.0163263874921,-23.2254399766281,
121.95651707498)) ;
#103181 = CARTESIAN_POINT('Ctrl Pts',(-18.7732899517778,-23.235283752142,
122.04517614713)) ;
#103182 = CARTESIAN_POINT('Ctrl Pts',(-18.5459000575662,-23.2452693935296,
122.176069505843)) ;
#103183 = CARTESIAN_POINT('Ctrl Pts',(-18.3455214781361,-23.2552061778914,
122.343576105247)) ;
#103184 = CARTESIAN_POINT('Ctrl Pts',(-18.1755060502448,-23.2652560123588,
122.545638346613)) ;
#103185 = CARTESIAN_POINT('Ctrl Pts',(-18.0455914330322,-23.2751064618619,
122.769558622391)) ;
#103186 = CARTESIAN_POINT('Ctrl Pts',(-17.9548073715586,-23.285078475844,
123.015349644938)) ;
#103187 = CARTESIAN_POINT('Ctrl Pts',(-17.907992236839,-23.2950736336911,
123.273849064806)) ;
#103188 = CARTESIAN_POINT('Ctrl Pts',(-17.9070860096866,-23.3051075600548,
123.53750621489)) ;
#103189 = CARTESIAN_POINT('Ctrl Pts',(-17.9507850137086,-23.3149632684872,
123.792814747735)) ;
#103190 = CARTESIAN_POINT('Ctrl Pts',(-18.0390356386596,-23.3249614178259,
124.040247090644)) ;
#103191 = CARTESIAN_POINT('Ctrl Pts',(-18.1674616556729,-23.3348608209994,
124.266527021118)) ;
#103192 = CARTESIAN_POINT('Ctrl Pts',(-18.3356817078808,-23.3449120178879,
124.47013072449)) ;
#103193 = CARTESIAN_POINT('Ctrl Pts',(-18.5333323575625,-23.3547943417008,
124.638615226352)) ;
#103194 = CARTESIAN_POINT('Ctrl Pts',(-18.7594616396992,-23.3647892373574,
124.772216137486)) ;
#103195 = CARTESIAN_POINT('Ctrl Pts',(-19.0061533314025,-23.3748103367399,
124.864411761759)) ;
#103196 = CARTESIAN_POINT('Ctrl Pts',(-19.2621116257065,-23.384717604602,
124.912027971084)) ;
#103197 = CARTESIAN_POINT('Ctrl Pts',(-19.5232470996749,-23.3946559484272,
124.915009816685)) ;
#103198 = CARTESIAN_POINT('Ctrl Pts',(-19.7826933987112,-23.4046593677277,
124.8724829918)) ;
#103199 = CARTESIAN_POINT('Ctrl Pts',(-20.0314009904622,-23.4146939184348,
124.784885032941)) ;
#103200 = CARTESIAN_POINT('Ctrl Pts',(-20.2570231739514,-23.4245388680404,
124.658249413978)) ;
#103201 = CARTESIAN_POINT('Ctrl Pts',(-20.4603618570071,-23.4345247101533,
124.492434927379)) ;
#103202 = CARTESIAN_POINT('Ctrl Pts',(-20.6311448680161,-23.4444595175224,
124.294901691016)) ;
#103203 = CARTESIAN_POINT('Ctrl Pts',(-20.7664417655646,-23.4545170592357,
124.067899599179)) ;
#103204 = CARTESIAN_POINT('Ctrl Pts',(-20.8584621327028,-23.4643386567478,
123.826728474679)) ;
#103205 = CARTESIAN_POINT('Ctrl Pts',(-20.9088445357203,-23.4743949162283,
123.567330995986)) ;
#103206 = CARTESIAN_POINT('Ctrl Pts',(-20.9129110800189,-23.4843348525287,
123.30613725382)) ;
#103207 = CARTESIAN_POINT('Ctrl Pts',(-20.8724772004398,-23.4942419732731,
123.048950368419)) ;
#103208 = CARTESIAN_POINT('Ctrl Pts',(-20.7867527465454,-23.5042848791984,
122.79935041922)) ;
#103209 = CARTESIAN_POINT('Ctrl Pts',(-20.6607477389128,-23.5141926602976,
122.57149371911)) ;
#103210 = CARTESIAN_POINT('Ctrl Pts',(-20.4957599634145,-23.5242030293,122.366590895835)) ;
#103211 = CARTESIAN_POINT('Ctrl Pts',(-20.2969506390713,-23.5342338678688,
122.193505240342)) ;
#103212 = CARTESIAN_POINT('Ctrl Pts',(-20.0753486418912,-23.5440867075085,
122.059578658416)) ;
#103213 = CARTESIAN_POINT('Ctrl Pts',(-19.8307446270475,-23.5540747086735,
121.964443905923)) ;
#103214 = CARTESIAN_POINT('Ctrl Pts',(-19.5748366256193,-23.5640035276526,
121.913518355391)) ;
#103215 = CARTESIAN_POINT('Ctrl Pts',(-19.3124297420902,-23.5739912303749,
121.907324493557)) ;
#103216 = CARTESIAN_POINT('Ctrl Pts',(-19.051770374588,-23.5840272301776,
121.947412427544)) ;
#103217 = CARTESIAN_POINT('Ctrl Pts',(-18.8063695565642,-23.593882099979,
122.03022500665)) ;
#103218 = CARTESIAN_POINT('Ctrl Pts',(-18.5756276914687,-23.6038815304026,
122.155865182355)) ;
#103219 = CARTESIAN_POINT('Ctrl Pts',(-18.3721072360953,-23.6137766478679,
122.317789039165)) ;
#103220 = CARTESIAN_POINT('Ctrl Pts',(-18.1969845029216,-23.6238371413848,
122.515805626587)) ;
#103221 = CARTESIAN_POINT('Ctrl Pts',(-18.0616521827604,-23.633686621586,
122.736464033145)) ;
#103222 = CARTESIAN_POINT('Ctrl Pts',(-17.96435863761,-23.6437130718498,122.981324009064)) ;
#103223 = CARTESIAN_POINT('Ctrl Pts',(-17.911742767229,-23.6537443623279,
123.239637252324)) ;
#103224 = CARTESIAN_POINT('Ctrl Pts',(-17.9043471354414,-23.6635857499797,
123.498155439338)) ;
#103225 = CARTESIAN_POINT('Ctrl Pts',(-17.9420608558698,-23.6735891508709,
123.758288393209)) ;
#103226 = CARTESIAN_POINT('Ctrl Pts',(-18.0243389591208,-23.6835735336621,
124.007481577347)) ;
#103227 = CARTESIAN_POINT('Ctrl Pts',(-18.1495030874067,-23.6936126236755,
124.23968716237)) ;
#103228 = CARTESIAN_POINT('Ctrl Pts',(-18.3096790121242,-23.7034584325847,
124.442908496677)) ;
#103229 = CARTESIAN_POINT('Ctrl Pts',(-18.5050267463786,-23.7134428554037,
124.618016503644)) ;
#103230 = CARTESIAN_POINT('Ctrl Pts',(-18.7268162305276,-23.7233824806449,
124.756058797154)) ;
#103231 = CARTESIAN_POINT('Ctrl Pts',(-18.9716149595931,-23.7334221701635,
124.854395810098)) ;
#103232 = CARTESIAN_POINT('Ctrl Pts',(-19.2258825394097,-23.7433103585821,
124.908048605825)) ;
#103233 = CARTESIAN_POINT('Ctrl Pts',(-19.4882244846222,-23.7532998845842,
124.917317622935)) ;
#103234 = CARTESIAN_POINT('Ctrl Pts',(-19.7473573898782,-23.7632583859393,
124.880808259512)) ;
#103235 = CARTESIAN_POINT('Ctrl Pts',(-19.9949628231632,-23.773157979943,
124.800942972097)) ;
#103236 = CARTESIAN_POINT('Ctrl Pts',(-20.2283026313404,-23.7832058680643,
124.677413983082)) ;
#103237 = CARTESIAN_POINT('Ctrl Pts',(-20.4336672103924,-23.7931012933098,
124.517825438712)) ;
#103238 = CARTESIAN_POINT('Ctrl Pts',(-20.6111084539714,-23.8031626840104,
124.321848670484)) ;
#103239 = CARTESIAN_POINT('Ctrl Pts',(-20.7488728942098,-23.8130082676971,
124.102826518574)) ;
#103240 = CARTESIAN_POINT('Ctrl Pts',(-20.8484840700568,-23.8229712410063,
123.860719317866)) ;
#103241 = CARTESIAN_POINT('Ctrl Pts',(-20.9045623846143,-23.8329969078321,
123.603275789807)) ;
#103242 = CARTESIAN_POINT('Ctrl Pts',(-20.9151111856894,-23.8429113856984,
123.342955717089)) ;
#103243 = CARTESIAN_POINT('Ctrl Pts',(-20.8805541691615,-23.8528999003734,
123.082731176444)) ;
#103244 = CARTESIAN_POINT('Ctrl Pts',(-20.8003735896472,-23.8629440112888,
122.831281031369)) ;
#103245 = CARTESIAN_POINT('Ctrl Pts',(-20.6809155331496,-23.8727721488834,
122.602251951149)) ;
#103246 = CARTESIAN_POINT('Ctrl Pts',(-20.5196793173917,-23.8828487169423,
122.392265985957)) ;
#103247 = CARTESIAN_POINT('Ctrl Pts',(-20.3287876662329,-23.8927008788465,
122.217275425299)) ;
#103248 = CARTESIAN_POINT('Ctrl Pts',(-20.1057229104058,-23.9027738408033,
122.07484100649)) ;
#103249 = CARTESIAN_POINT('Ctrl Pts',(-19.8668284491858,-23.9126164028062,
121.975632340931)) ;
#103250 = CARTESIAN_POINT('Ctrl Pts',(-19.6110271194591,-23.9225968393,121.917772023658)) ;
#103251 = CARTESIAN_POINT('Ctrl Pts',(-19.348039156227,-23.9326151446244,
121.905665438189)) ;
#103252 = CARTESIAN_POINT('Ctrl Pts',(-19.0903457175799,-23.9424991085438,
121.938422956603)) ;
#103253 = CARTESIAN_POINT('Ctrl Pts',(-18.8377656583219,-23.9525649852824,
122.016891898931)) ;
#103254 = CARTESIAN_POINT('Ctrl Pts',(-18.6078170760635,-23.9624040861433,
122.135169084714)) ;
#103255 = CARTESIAN_POINT('Ctrl Pts',(-18.3974656836165,-23.972437169009,
122.294107786328)) ;
#103256 = CARTESIAN_POINT('Ctrl Pts',(-18.2185683792125,-23.9824588542845,
122.487406407635)) ;
#103257 = CARTESIAN_POINT('Ctrl Pts',(-18.0778267832511,-23.992325549383,
122.705148566182)) ;
#103258 = CARTESIAN_POINT('Ctrl Pts',(-17.9754281452733,-24.0022854391175,
122.946034450272)) ;
#103259 = CARTESIAN_POINT('Ctrl Pts',(-17.9163664020501,-24.012320426943,
123.203027128536)) ;
#103260 = CARTESIAN_POINT('Ctrl Pts',(-17.9025895953296,-24.0222071310173,
123.462511054197)) ;
#103261 = CARTESIAN_POINT('Ctrl Pts',(-17.9347016359298,-24.0322722752502,
123.725012586656)) ;
#103262 = CARTESIAN_POINT('Ctrl Pts',(-18.0099434070378,-24.0421115659788,
123.972431513364)) ;
#103263 = CARTESIAN_POINT('Ctrl Pts',(-18.1293026069265,-24.0521741234172,
124.208359310973)) ;
#103264 = CARTESIAN_POINT('Ctrl Pts',(-18.2854573227797,-24.0620711746693,
124.416367480328)) ;
#103265 = CARTESIAN_POINT('Ctrl Pts',(-18.4754012568581,-24.0720023814176,
124.595335878726)) ;
#103266 = CARTESIAN_POINT('Ctrl Pts',(-18.6961331689866,-24.0820445656364,
124.739965453088)) ;
#103267 = CARTESIAN_POINT('Ctrl Pts',(-18.9348086365225,-24.0919311937473,
124.842639747619)) ;
#103268 = CARTESIAN_POINT('Ctrl Pts',(-19.1902871963049,-24.1019244662797,
124.903374527269)) ;
#103269 = CARTESIAN_POINT('Ctrl Pts',(-19.4511873709055,-24.1118695418212,
124.918665438026)) ;
#103270 = CARTESIAN_POINT('Ctrl Pts',(-19.710965208711,-24.1218190925494,
124.888914128674)) ;
#103271 = CARTESIAN_POINT('Ctrl Pts',(-19.9637977980599,-24.1318584273974,
124.813604045651)) ;
#103272 = CARTESIAN_POINT('Ctrl Pts',(-20.1962508109109,-24.1417445663413,
124.697537862331)) ;
#103273 = CARTESIAN_POINT('Ctrl Pts',(-20.4075413438775,-24.151742679315,
124.541421995671)) ;
#103274 = CARTESIAN_POINT('Ctrl Pts',(-20.5872538313161,-24.1616624416675,
124.352546831275)) ;
#103275 = CARTESIAN_POINT('Ctrl Pts',(-20.7332244854721,-24.1717018372801,
124.132799237148)) ;
#103276 = CARTESIAN_POINT('Ctrl Pts',(-20.8373860226975,-24.1816110230684,
123.894133566146)) ;
#103277 = CARTESIAN_POINT('Ctrl Pts',(-20.8993974610776,-24.1915462072259,
123.640515964323)) ;
#103278 = CARTESIAN_POINT('Ctrl Pts',(-20.9163526621693,-24.2015872646118,
123.377199581861)) ;
#103279 = CARTESIAN_POINT('Ctrl Pts',(-20.8879577850495,-24.2114744226451,
123.118917113448)) ;
#103280 = CARTESIAN_POINT('Ctrl Pts',(-20.8148023044872,-24.221466702321,
122.866745567144)) ;
#103281 = CARTESIAN_POINT('Ctrl Pts',(-20.6994003311654,-24.2314152193661,
122.632140907791)) ;
#103282 = CARTESIAN_POINT('Ctrl Pts',(-20.5455176565627,-24.2413519969365,
122.421198517231)) ;
#103283 = CARTESIAN_POINT('Ctrl Pts',(-20.3566602491827,-24.2513350330834,
122.239059803708)) ;
#103284 = CARTESIAN_POINT('Ctrl Pts',(-20.1375054315778,-24.2613787846771,
122.092024451961)) ;
#103285 = CARTESIAN_POINT('Ctrl Pts',(-19.9015041198329,-24.2712073138897,
121.986982801871)) ;
#103286 = CARTESIAN_POINT('Ctrl Pts',(-19.6446783076409,-24.2812826747984,
121.922828883931)) ;
#103287 = CARTESIAN_POINT('Ctrl Pts',(-19.3862469986077,-24.2911392736856,
121.904547729095)) ;
#103288 = CARTESIAN_POINT('Ctrl Pts',(-19.1232503151631,-24.3012022677035,
121.931694916148)) ;
#103289 = CARTESIAN_POINT('Ctrl Pts',(-18.8735504660237,-24.311080201993,
122.002807613392)) ;
#103290 = CARTESIAN_POINT('Ctrl Pts',(-18.6369978578341,-24.321080849551,
122.117198755573)) ;
#103291 = CARTESIAN_POINT('Ctrl Pts',(-18.4254739722375,-24.3309986959891,
122.269548153979)) ;
#103292 = CARTESIAN_POINT('Ctrl Pts',(-18.2412881647919,-24.3410498129947,
122.458807705072)) ;
#103293 = CARTESIAN_POINT('Ctrl Pts',(-18.0951342855222,-24.3509205483053,
122.673164916615)) ;
#103294 = CARTESIAN_POINT('Ctrl Pts',(-17.9862472480919,-24.3609912555483,
122.91432710992)) ;
#103295 = CARTESIAN_POINT('Ctrl Pts',(-17.922299610322,-24.3708242630002,
123.164716216814)) ;
#103296 = CARTESIAN_POINT('Ctrl Pts',(-17.9016599057692,-24.3808547553025,
123.427488017808)) ;
#103297 = CARTESIAN_POINT('Ctrl Pts',(-17.927729522015,-24.3908863503759,
123.689830426704)) ;
#103298 = CARTESIAN_POINT('Ctrl Pts',(-17.9969934501606,-24.4007160495141,
123.938667781932)) ;
#103299 = CARTESIAN_POINT('Ctrl Pts',(-18.1095255107703,-24.4107054993957,
124.175845661491)) ;
#103300 = CARTESIAN_POINT('Ctrl Pts',(-18.2628973236103,-24.4207493572114,
124.390649715885)) ;
#103301 = CARTESIAN_POINT('Ctrl Pts',(-18.446698072111,-24.4305710478016,
124.571855631295)) ;
#103302 = CARTESIAN_POINT('Ctrl Pts',(-18.6634180756333,-24.440606138342,
124.722101523937)) ;
#103303 = CARTESIAN_POINT('Ctrl Pts',(-18.9029943040956,-24.4506306573247,
124.831691995518)) ;
#103304 = CARTESIAN_POINT('Ctrl Pts',(-19.1536255156033,-24.4604905027349,
124.897348733624)) ;
#103305 = CARTESIAN_POINT('Ctrl Pts',(-19.4144301291462,-24.4704502790506,
124.91942556247)) ;
#103306 = CARTESIAN_POINT('Ctrl Pts',(-19.6768553029751,-24.4804784763652,
124.895358567147)) ;
#103307 = CARTESIAN_POINT('Ctrl Pts',(-19.9281616014576,-24.4903860186555,
124.827216116485)) ;
#103308 = CARTESIAN_POINT('Ctrl Pts',(-20.1667953840457,-24.5004186692194,
124.715174244585)) ;
#103309 = CARTESIAN_POINT('Ctrl Pts',(-20.3792224588511,-24.510302625646,
124.565695978752)) ;
#103310 = CARTESIAN_POINT('Ctrl Pts',(-20.5648889688196,-24.5202923270079,
124.380098753571)) ;
#103311 = CARTESIAN_POINT('Ctrl Pts',(-20.7158198781951,-24.5303333222839,
124.163660029453)) ;
#103312 = CARTESIAN_POINT('Ctrl Pts',(-20.8249600257777,-24.5401662115523,
123.929446633066)) ;
#103313 = CARTESIAN_POINT('Ctrl Pts',(-20.8935923937664,-24.5501593699197,
123.675968287344)) ;
#103314 = CARTESIAN_POINT('Ctrl Pts',(-20.9167162661487,-24.5601914122718,
123.413340508638)) ;
#103315 = CARTESIAN_POINT('Ctrl Pts',(-20.8945884232422,-24.5700566562302,
123.155051255594)) ;
#103316 = CARTESIAN_POINT('Ctrl Pts',(-20.828007978736,-24.5800185474762,
122.901863765743)) ;
#103317 = CARTESIAN_POINT('Ctrl Pts',(-20.717293798241,-24.5900534474947,
122.662538389889)) ;
#103318 = CARTESIAN_POINT('Ctrl Pts',(-20.5692808803268,-24.5999385279093,
122.449020508724)) ;
#103319 = CARTESIAN_POINT('Ctrl Pts',(-20.3831408459186,-24.6100037000341,
122.261151555758)) ;
#103320 = CARTESIAN_POINT('Ctrl Pts',(-20.171921014445,-24.6198509347576,
122.11160502399)) ;
#103321 = CARTESIAN_POINT('Ctrl Pts',(-19.9338866398181,-24.6298817460754,
121.998402424725)) ;
#103322 = CARTESIAN_POINT('Ctrl Pts',(-19.6801598924702,-24.6398913619889,
121.928905420214)) ;
#103323 = CARTESIAN_POINT('Ctrl Pts',(-19.4208842732656,-24.6498021413926,
121.904510087934)) ;
#103324 = CARTESIAN_POINT('Ctrl Pts',(-19.1607378646813,-24.6597314071816,
121.9248939004)) ;
#103325 = CARTESIAN_POINT('Ctrl Pts',(-18.9052752384676,-24.6697741004942,
121.991093795154)) ;
#103326 = CARTESIAN_POINT('Ctrl Pts',(-18.6688266886926,-24.679660633189,
122.098797729048)) ;
#103327 = CARTESIAN_POINT('Ctrl Pts',(-18.4521339671131,-24.6896537782922,
122.247123614488)) ;
#103328 = CARTESIAN_POINT('Ctrl Pts',(-18.2654374954735,-24.6995994589663,
122.430030788731)) ;
#103329 = CARTESIAN_POINT('Ctrl Pts',(-18.1128695966725,-24.709546716593,
122.642308610488)) ;
#103330 = CARTESIAN_POINT('Ctrl Pts',(-17.9986071950966,-24.7195946187145,
122.880344723335)) ;
#103331 = CARTESIAN_POINT('Ctrl Pts',(-17.9286177670027,-24.7294423243362,
123.129489608421)) ;
#103332 = CARTESIAN_POINT('Ctrl Pts',(-17.901833142117,-24.7394037909703,
123.389883113504)) ;
#103333 = CARTESIAN_POINT('Ctrl Pts',(-17.9211529777508,-24.7494333442385,
123.652749954878)) ;
#103334 = CARTESIAN_POINT('Ctrl Pts',(-17.9848845095932,-24.7593402362659,
123.905175045904)) ;
#103335 = CARTESIAN_POINT('Ctrl Pts',(-18.0914434456593,-24.7692878803789,
124.143861709539)) ;
#103336 = CARTESIAN_POINT('Ctrl Pts',(-18.2384939760854,-24.7792879234078,
124.361699048924)) ;
#103337 = CARTESIAN_POINT('Ctrl Pts',(-18.4221409649936,-24.7893266894018,
124.55106080361)) ;
#103338 = CARTESIAN_POINT('Ctrl Pts',(-18.6310369633877,-24.7991517514241,
124.702833388253)) ;
#103339 = CARTESIAN_POINT('Ctrl Pts',(-18.8683103182096,-24.8092062987504,
124.819051009912)) ;
#103340 = CARTESIAN_POINT('Ctrl Pts',(-19.1194973611782,-24.8191495421996,
124.8910663407)) ;
#103341 = CARTESIAN_POINT('Ctrl Pts',(-19.3782090444937,-24.8290517138075,
124.91906462524)) ;
#103342 = CARTESIAN_POINT('Ctrl Pts',(-19.6417776433998,-24.8391045494177,
124.901291092302)) ;
#103343 = CARTESIAN_POINT('Ctrl Pts',(-19.8937151208383,-24.8489776071032,
124.839250660961)) ;
#103344 = CARTESIAN_POINT('Ctrl Pts',(-20.134240507652,-24.8589728686289,
124.733710267886)) ;
#103345 = CARTESIAN_POINT('Ctrl Pts',(-20.3531898254097,-24.8689982380494,
124.587174639634)) ;
#103346 = CARTESIAN_POINT('Ctrl Pts',(-20.5410415166913,-24.878888070576,
124.407554509467)) ;
#103347 = CARTESIAN_POINT('Ctrl Pts',(-20.7481549549559,-24.8921860413854,
124.126143799265)) ;
#103348 = CARTESIAN_POINT('Ctrl Pts',(-20.8766424273959,-24.9053844364946,
123.799684327235)) ;
#103349 = CARTESIAN_POINT('Ctrl Pts',(-20.9162637139669,-24.918779878774,
123.449918888424)) ;
#103350 = CARTESIAN_POINT('Ctrl Pts',(-20.9004773781569,-24.928655717013,
123.19083322637)) ;
#103351 = CARTESIAN_POINT('Ctrl Pts',(-20.838947304478,-24.9387171196107,
122.93373140854)) ;
#103352 = CARTESIAN_POINT('Ctrl Pts',(-20.7358027985603,-24.9485821765459,
122.695849306882)) ;
#103353 = CARTESIAN_POINT('Ctrl Pts',(-20.5912214248637,-24.9585942724947,
122.47606681639)) ;
#103354 = CARTESIAN_POINT('Ctrl Pts',(-20.3516992972503,-24.9718715816401,
122.222302728919)) ;
#103355 = CARTESIAN_POINT('Ctrl Pts',(-19.9764454446067,-24.9884706071474,
121.990340344157)) ;
#103356 = CARTESIAN_POINT('Ctrl Pts',(-19.5445902666721,-25.0050696551804,
121.900306518793)) ;
#103357 = CARTESIAN_POINT('Ctrl Pts',(-19.1970560702189,-25.0183130672114,
121.919332976408)) ;
#103358 = CARTESIAN_POINT('Ctrl Pts',(-18.940168786962,-25.0283504948998,
121.979150759205)) ;
#103359 = CARTESIAN_POINT('Ctrl Pts',(-18.7007881441074,-25.0382547968554,
122.081334287763)) ;
#103360 = CARTESIAN_POINT('Ctrl Pts',(-18.4082675107088,-25.0515216368306,
122.271046777023)) ;
#103361 = CARTESIAN_POINT('Ctrl Pts',(-18.1123456266158,-25.0681478349205,
122.599207663256)) ;
#103362 = CARTESIAN_POINT('Ctrl Pts',(-17.9131353960091,-25.0880669503039,
123.08973418129)) ;
#103363 = CARTESIAN_POINT('Ctrl Pts',(-17.8962113866272,-25.1046733734382,
123.530770659968)) ;
#103364 = CARTESIAN_POINT('Ctrl Pts',(-17.9736439459162,-25.1179695939339,
123.871497784587)) ;
#103365 = CARTESIAN_POINT('Ctrl Pts',(-18.108093327351,-25.1312384262753,
124.193307694941)) ;
#103366 = CARTESIAN_POINT('Ctrl Pts',(-18.3795961224267,-25.1479296743084,
124.544018559131)) ;
#103367 = CARTESIAN_POINT('Ctrl Pts',(-18.8243636417243,-25.1677394059812,
124.825912141057)) ;
#103368 = CARTESIAN_POINT('Ctrl Pts',(-19.342674885588,-25.1877170133098,
124.941073667171)) ;
#103369 = CARTESIAN_POINT('Ctrl Pts',(-19.8676499505085,-25.2076433223676,
124.871666354727)) ;
#103370 = CARTESIAN_POINT('Ctrl Pts',(-20.3358800280026,-25.2274601825323,
124.630171750087)) ;
#103371 = CARTESIAN_POINT('Ctrl Pts',(-20.6978730394626,-25.2475599981263,
124.237542291265)) ;
#103372 = CARTESIAN_POINT('Ctrl Pts',(-20.9010231320322,-25.2673169620089,
123.753088339619)) ;
#103373 = CARTESIAN_POINT('Ctrl Pts',(-20.9280483314068,-25.2873538880783,
123.221407603216)) ;
#103374 = CARTESIAN_POINT('Ctrl Pts',(-20.7724317346109,-25.3072234704598,
122.71661402828)) ;
#103375 = CARTESIAN_POINT('Ctrl Pts',(-20.4545450312064,-25.327128042213,
122.293870066593)) ;
#103376 = CARTESIAN_POINT('Ctrl Pts',(-20.0102205883016,-25.3470806444115,
122.004220843473)) ;
#103377 = CARTESIAN_POINT('Ctrl Pts',(-19.4949958995402,-25.3669901353818,
121.884058486716)) ;
#103378 = CARTESIAN_POINT('Ctrl Pts',(-18.9708179026118,-25.3868415040812,
121.945295970142)) ;
#103379 = CARTESIAN_POINT('Ctrl Pts',(-18.4941285719003,-25.4069217002172,
122.185052393846)) ;
#103380 = CARTESIAN_POINT('Ctrl Pts',(-18.1327894364014,-25.4267226437926,
122.56786400409)) ;
#103381 = CARTESIAN_POINT('Ctrl Pts',(-17.9208325642514,-25.4467066203021,
123.05478916787)) ;
#103382 = CARTESIAN_POINT('Ctrl Pts',(-17.8886895489191,-25.4666225832777,
123.583143521269)) ;
#103383 = CARTESIAN_POINT('Ctrl Pts',(-18.0370599385116,-25.4864930180996,
124.090104054025)) ;
#103384 = CARTESIAN_POINT('Ctrl Pts',(-18.352917711476,-25.5065433033327,
124.519121936274)) ;
#103385 = CARTESIAN_POINT('Ctrl Pts',(-18.7899901791199,-25.526317272092,
124.811357077356)) ;
#103386 = CARTESIAN_POINT('Ctrl Pts',(-19.3073428474073,-25.5463737302116,
124.938951376792)) ;
#103387 = CARTESIAN_POINT('Ctrl Pts',(-19.8306108133503,-25.5661686132026,
124.882860177028)) ;
#103388 = CARTESIAN_POINT('Ctrl Pts',(-20.3078500603457,-25.5861352685049,
124.651027917224)) ;
#103389 = CARTESIAN_POINT('Ctrl Pts',(-20.6767072840341,-25.6060942385814,
124.269637862864)) ;
#103390 = CARTESIAN_POINT('Ctrl Pts',(-20.892889706575,-25.6259903261715,
123.787070999815)) ;
#103391 = CARTESIAN_POINT('Ctrl Pts',(-20.9320520392546,-25.6458884960831,
123.259707282722)) ;
#103392 = CARTESIAN_POINT('Ctrl Pts',(-20.7893672747436,-25.6657943314502,
122.750206541709)) ;
#103393 = CARTESIAN_POINT('Ctrl Pts',(-20.4807383967051,-25.6857442563881,
122.319104917186)) ;
#103394 = CARTESIAN_POINT('Ctrl Pts',(-20.045270569466,-25.7056234462985,
122.019794561741)) ;
#103395 = CARTESIAN_POINT('Ctrl Pts',(-19.5313435803427,-25.7256047705791,
121.886125315559)) ;
#103396 = CARTESIAN_POINT('Ctrl Pts',(-19.0038849568637,-25.7455345547874,
121.936016700359)) ;
#103397 = CARTESIAN_POINT('Ctrl Pts',(-18.525515022913,-25.7654545441782,
122.162593470176)) ;
#103398 = CARTESIAN_POINT('Ctrl Pts',(-18.1533644802171,-25.7853097395322,
122.53692696707)) ;
#103399 = CARTESIAN_POINT('Ctrl Pts',(-17.9297308534324,-25.8053557411916,
123.020366144601)) ;
#103400 = CARTESIAN_POINT('Ctrl Pts',(-17.8922938015895,-25.8218554884014,
123.457435365614)) ;
#103401 = CARTESIAN_POINT('Ctrl Pts',(-17.9536238747597,-25.8352440928495,
123.803839654938)) ;
#103402 = CARTESIAN_POINT('Ctrl Pts',(-18.0424362921009,-25.8451059211844,
124.047317440358)) ;
#103403 = CARTESIAN_POINT('Ctrl Pts',(-18.1728280726504,-25.855072063942,
124.274457577211)) ;
#103404 = CARTESIAN_POINT('Ctrl Pts',(-18.398321114858,-25.8684338100669,
124.543544062883)) ;
#103405 = CARTESIAN_POINT('Ctrl Pts',(-18.755759039261,-25.884888139022,124.795782547806)) ;
#103406 = CARTESIAN_POINT('Ctrl Pts',(-19.1855136266191,-25.9016553840703,
124.913062176517)) ;
#103407 = CARTESIAN_POINT('Ctrl Pts',(-19.532168225036,-25.9148419493443,
124.914179977617)) ;
#103408 = CARTESIAN_POINT('Ctrl Pts',(-19.7909083811726,-25.9248314080889,
124.870235424795)) ;
#103409 = CARTESIAN_POINT('Ctrl Pts',(-20.0373350366272,-25.93478518057,124.78235238562)) ;
#103410 = CARTESIAN_POINT('Ctrl Pts',(-20.2667304823186,-25.9448329971027,
124.651656840753)) ;
#103411 = CARTESIAN_POINT('Ctrl Pts',(-20.4660137570292,-25.9546745302252,
124.486773533974)) ;
#103412 = CARTESIAN_POINT('Ctrl Pts',(-20.6364871909167,-25.9646607724449,
124.287312743345)) ;
#103413 = CARTESIAN_POINT('Ctrl Pts',(-20.7692327835376,-25.9745973958698,
124.062396894432)) ;
#103414 = CARTESIAN_POINT('Ctrl Pts',(-20.8618050261484,-25.9846472732528,
123.815081089085)) ;
#103415 = CARTESIAN_POINT('Ctrl Pts',(-20.9092717379176,-25.9944977120304,
123.560591541361)) ;
#103416 = CARTESIAN_POINT('Ctrl Pts',(-20.9125449101557,-26.0044697259991,
123.298590931221)) ;
#103417 = CARTESIAN_POINT('Ctrl Pts',(-20.8701309095838,-26.0144648946252,
123.039333300211)) ;
#103418 = CARTESIAN_POINT('Ctrl Pts',(-20.7827323588806,-26.0244987778864,
122.790580963316)) ;
#103419 = CARTESIAN_POINT('Ctrl Pts',(-20.6560870606578,-26.0343546479497,
122.564632684647)) ;
#103420 = CARTESIAN_POINT('Ctrl Pts',(-20.4901308476962,-26.0443521938669,
122.360995763402)) ;
#103421 = CARTESIAN_POINT('Ctrl Pts',(-20.2931406735799,-26.0542603207662,
122.190714868031)) ;
#103422 = CARTESIAN_POINT('Ctrl Pts',(-20.0675018032836,-26.0642706922883,
122.055453597697)) ;
#103423 = CARTESIAN_POINT('Ctrl Pts',(-19.8211228425715,-26.0743011350357,
121.961795007237)) ;
#103424 = CARTESIAN_POINT('Ctrl Pts',(-19.5670204257272,-26.084149087589,
121.912639787958)) ;
#103425 = CARTESIAN_POINT('Ctrl Pts',(-19.3026492624248,-26.09421175661,121.90805310051)) ;
#103426 = CARTESIAN_POINT('Ctrl Pts',(-19.0458449512174,-26.1041061320739,
121.948938241374)) ;
#103427 = CARTESIAN_POINT('Ctrl Pts',(-18.7986876737216,-26.1140479303921,
122.033518099344)) ;
#103428 = CARTESIAN_POINT('Ctrl Pts',(-18.5684665254471,-26.1240504241194,
122.160442177422)) ;
#103429 = CARTESIAN_POINT('Ctrl Pts',(-18.3634215513688,-26.1340852226263,
122.32623577368)) ;
#103430 = CARTESIAN_POINT('Ctrl Pts',(-18.1932054122655,-26.1439301066057,
122.521089565676)) ;
#103431 = CARTESIAN_POINT('Ctrl Pts',(-18.0570995412716,-26.1539159634237,
122.745402537664)) ;
#103432 = CARTESIAN_POINT('Ctrl Pts',(-17.9622893499498,-26.1638507775985,
122.988707568704)) ;
#103433 = CARTESIAN_POINT('Ctrl Pts',(-17.9107815245154,-26.1739082773838,
123.247901857506)) ;
#103434 = CARTESIAN_POINT('Ctrl Pts',(-17.9047991830589,-26.1837300358021,
123.505966538132)) ;
#103435 = CARTESIAN_POINT('Ctrl Pts',(-17.9441442274353,-26.1937856935861,
123.767250890417)) ;
#103436 = CARTESIAN_POINT('Ctrl Pts',(-18.0277702636983,-26.2037278757661,
124.014790591981)) ;
#103437 = CARTESIAN_POINT('Ctrl Pts',(-18.1519364138045,-26.2136330844608,
124.243561611834)) ;
#103438 = CARTESIAN_POINT('Ctrl Pts',(-18.3162378863457,-26.2236748754233,
124.450054470379)) ;
#103439 = CARTESIAN_POINT('Ctrl Pts',(-18.5112522329825,-26.2335826498955,
124.622580587665)) ;
#103440 = CARTESIAN_POINT('Ctrl Pts',(-18.7353273261032,-26.2435941501231,
124.760461732387)) ;
#103441 = CARTESIAN_POINT('Ctrl Pts',(-18.9806532290191,-26.2536269105158,
124.857033178814)) ;
#103442 = CARTESIAN_POINT('Ctrl Pts',(-19.2342454890907,-26.2634774796507,
124.909034939315)) ;
#103443 = CARTESIAN_POINT('Ctrl Pts',(-19.4965987108979,-26.2734660891806,
124.916810782346)) ;
#103444 = CARTESIAN_POINT('Ctrl Pts',(-19.7547866552497,-26.2833947452047,
124.879136485383)) ;
#103445 = CARTESIAN_POINT('Ctrl Pts',(-20.0041305403617,-26.2933824913825,
124.797137527614)) ;
#103446 = CARTESIAN_POINT('Ctrl Pts',(-20.2363343622143,-26.3034184803182,
124.672111002003)) ;
#103447 = CARTESIAN_POINT('Ctrl Pts',(-20.4398589272357,-26.3132733501318,
124.511932238385)) ;
#103448 = CARTESIAN_POINT('Ctrl Pts',(-20.6152342524679,-26.3232727913736,
124.31630284965)) ;
#103449 = CARTESIAN_POINT('Ctrl Pts',(-20.7528133990326,-26.3331678655537,
124.095596185869)) ;
#103450 = CARTESIAN_POINT('Ctrl Pts',(-20.8515508555085,-26.3432285213934,
123.850379097098)) ;
#103451 = CARTESIAN_POINT('Ctrl Pts',(-20.9052171035059,-26.353077395589,
123.597165515688)) ;
#103452 = CARTESIAN_POINT('Ctrl Pts',(-20.9149275362801,-26.3631061075523,
123.333804327786)) ;
#103453 = CARTESIAN_POINT('Ctrl Pts',(-20.8780488245703,-26.3731355081354,
123.072830177121)) ;
#103454 = CARTESIAN_POINT('Ctrl Pts',(-20.7985044978986,-26.3829757017522,
122.826773840961)) ;
#103455 = CARTESIAN_POINT('Ctrl Pts',(-20.6758816110649,-26.3929791243274,
122.594275668135)) ;
#103456 = CARTESIAN_POINT('Ctrl Pts',(-20.5149293057162,-26.4029646614205,
122.386968480829)) ;
#103457 = CARTESIAN_POINT('Ctrl Pts',(-20.31922052082,-26.4130056659073,122.210020619574)) ;
#103458 = CARTESIAN_POINT('Ctrl Pts',(-20.1003044621469,-26.4228492048485,
122.072178443787)) ;
#103459 = CARTESIAN_POINT('Ctrl Pts',(-19.8575995136209,-26.4328342358393,
121.972550199408)) ;
#103460 = CARTESIAN_POINT('Ctrl Pts',(-19.6024003493209,-26.4427736983613,
121.916713979077)) ;
#103461 = CARTESIAN_POINT('Ctrl Pts',(-19.3388058340675,-26.4528134305851,
121.90599082884)) ;
#103462 = CARTESIAN_POINT('Ctrl Pts',(-19.081247010349,-26.4627016109023,
121.940544837108)) ;
#103463 = CARTESIAN_POINT('Ctrl Pts',(-18.8309359774389,-26.4726911266048,
122.019624319406)) ;
#103464 = CARTESIAN_POINT('Ctrl Pts',(-18.5989724252165,-26.4826496772595,
122.140768935798)) ;
#103465 = CARTESIAN_POINT('Ctrl Pts',(-18.3923839555713,-26.4925490843645,
122.298903634733)) ;
#103466 = CARTESIAN_POINT('Ctrl Pts',(-18.2138538015984,-26.5025976707808,
122.493431045269)) ;
#103467 = CARTESIAN_POINT('Ctrl Pts',(-18.0737554054241,-26.5124904897453,
122.712487918614)) ;
#103468 = CARTESIAN_POINT('Ctrl Pts',(-17.9721496783014,-26.5225616072751,
122.956807055062)) ;
#103469 = CARTESIAN_POINT('Ctrl Pts',(-17.915609636616,-26.5323773012411,
123.208531310025)) ;
#103470 = CARTESIAN_POINT('Ctrl Pts',(-17.9029543104203,-26.5424436787384,
123.472705679931)) ;
#103471 = CARTESIAN_POINT('Ctrl Pts',(-17.935897733344,-26.5523426648203,
123.730812155219)) ;
#103472 = CARTESIAN_POINT('Ctrl Pts',(-18.014233583311,-26.5623968448138,
123.983084960881)) ;
#103473 = CARTESIAN_POINT('Ctrl Pts',(-18.1328039031903,-26.5722676577465,
124.213863466518)) ;
#103474 = CARTESIAN_POINT('Ctrl Pts',(-18.2928009544337,-26.5823415586003,
124.424696701549)) ;
#103475 = CARTESIAN_POINT('Ctrl Pts',(-18.481957944128,-26.592161713987,124.600332560415)) ;
#103476 = CARTESIAN_POINT('Ctrl Pts',(-18.7042016187812,-26.6022404209392,
124.744286478818)) ;
#103477 = CARTESIAN_POINT('Ctrl Pts',(-18.9426510348648,-26.612092009478,
124.84527092973)) ;
#103478 = CARTESIAN_POINT('Ctrl Pts',(-19.2005267069829,-26.622165126003,
124.904825642053)) ;
#103479 = CARTESIAN_POINT('Ctrl Pts',(-19.4588480419624,-26.6320076430988,
124.918344794272)) ;
#103480 = CARTESIAN_POINT('Ctrl Pts',(-19.7192610296387,-26.6419881046528,
124.887242445633)) ;
#103481 = CARTESIAN_POINT('Ctrl Pts',(-19.9711299204489,-26.6520063546435,
124.810621311574)) ;
#103482 = CARTESIAN_POINT('Ctrl Pts',(-20.2029952789095,-26.6618905148373,
124.693490844691)) ;
#103483 = CARTESIAN_POINT('Ctrl Pts',(-20.4147300329701,-26.6719556618123,
124.535018461326)) ;
#103484 = CARTESIAN_POINT('Ctrl Pts',(-20.5918552565131,-26.6817974854531,
124.34653140005)) ;
#103485 = CARTESIAN_POINT('Ctrl Pts',(-20.7368429063532,-26.6918269579139,
124.126436778143)) ;
#103486 = CARTESIAN_POINT('Ctrl Pts',(-20.8407127963112,-26.701853813176,
123.884271925495)) ;
#103487 = CARTESIAN_POINT('Ctrl Pts',(-20.9004565941376,-26.7116970632865,
123.632590888649)) ;
#103488 = CARTESIAN_POINT('Ctrl Pts',(-20.9162662490879,-26.7217455028697,
123.369009850146)) ;
#103489 = CARTESIAN_POINT('Ctrl Pts',(-20.885954490215,-26.7316949971176,
123.10930910727)) ;
#103490 = CARTESIAN_POINT('Ctrl Pts',(-20.8120690123609,-26.7416028528436,
122.859628892042)) ;
#103491 = CARTESIAN_POINT('Ctrl Pts',(-20.6939444643144,-26.7516623294935,
122.623167405143)) ;
#103492 = CARTESIAN_POINT('Ctrl Pts',(-20.5402234175417,-26.7615031389022,
122.415167308829)) ;
#103493 = CARTESIAN_POINT('Ctrl Pts',(-20.3487772899462,-26.771565289203,
122.232813349028)) ;
#103494 = CARTESIAN_POINT('Ctrl Pts',(-20.1320035757308,-26.7814624503255,
122.089071576219)) ;
#103495 = CARTESIAN_POINT('Ctrl Pts',(-19.8931105141142,-26.7913936247296,
121.984008253171)) ;
#103496 = CARTESIAN_POINT('Ctrl Pts',(-19.6366994920837,-26.8014358284546,
121.921607841887)) ;
#103497 = CARTESIAN_POINT('Ctrl Pts',(-19.3774249698779,-26.8113224108851,
121.904748137254)) ;
#103498 = CARTESIAN_POINT('Ctrl Pts',(-19.1163507559219,-26.8213158466334,
121.933036255571)) ;
#103499 = CARTESIAN_POINT('Ctrl Pts',(-18.8653956232192,-26.8312603149915,
122.005949625202)) ;
#103500 = CARTESIAN_POINT('Ctrl Pts',(-18.6305138282973,-26.8412121312371,
122.120975690623)) ;
#103501 = CARTESIAN_POINT('Ctrl Pts',(-18.4175163362835,-26.8512495673516,
122.276543163367)) ;
#103502 = CARTESIAN_POINT('Ctrl Pts',(-18.2373351265548,-26.8611345265279,
122.463693629074)) ;
#103503 = CARTESIAN_POINT('Ctrl Pts',(-18.0904991651695,-26.8711326447399,
122.681535599845)) ;
#103504 = CARTESIAN_POINT('Ctrl Pts',(-17.9843530492391,-26.8810535772519,
122.919692108216)) ;
#103505 = CARTESIAN_POINT('Ctrl Pts',(-17.9203477663553,-26.8910948774739,
123.175673758796)) ;
#103506 = CARTESIAN_POINT('Ctrl Pts',(-17.9020982876714,-26.9010017958639,
123.435379748587)) ;
#103507 = CARTESIAN_POINT('Ctrl Pts',(-17.9285541259772,-26.910937587573,
123.695139779583)) ;
#103508 = CARTESIAN_POINT('Ctrl Pts',(-18.0007184221001,-26.9209784821509,
123.948937619437)) ;
#103509 = CARTESIAN_POINT('Ctrl Pts',(-18.1139303893867,-26.9308656838647,
124.182817100163)) ;
#103510 = CARTESIAN_POINT('Ctrl Pts',(-18.2672757035253,-26.9408579516263,
124.395953976354)) ;
#103511 = CARTESIAN_POINT('Ctrl Pts',(-18.4545501643307,-26.9508064726481,
124.578396414551)) ;
#103512 = CARTESIAN_POINT('Ctrl Pts',(-18.6701650173284,-26.9607432462258,
124.725660975012)) ;
#103513 = CARTESIAN_POINT('Ctrl Pts',(-18.9090955124712,-26.9707262943668,
124.834075515904)) ;
#103514 = CARTESIAN_POINT('Ctrl Pts',(-19.1648254639869,-26.9807700019769,
124.899273151225)) ;
#103515 = CARTESIAN_POINT('Ctrl Pts',(-19.4223734198373,-26.9905986951302,
124.919249383875)) ;
#103516 = CARTESIAN_POINT('Ctrl Pts',(-19.6858583169006,-27.0006734442596,
124.893767425328)) ;
#103517 = CARTESIAN_POINT('Ctrl Pts',(-19.9356635840617,-27.0105387700552,
124.824321326066)) ;
#103518 = CARTESIAN_POINT('Ctrl Pts',(-20.1735911071489,-27.0205609444121,
124.711404071088)) ;
#103519 = CARTESIAN_POINT('Ctrl Pts',(-20.3880282939192,-27.030586997619,
124.558287322886)) ;
#103520 = CARTESIAN_POINT('Ctrl Pts',(-20.5697220257241,-27.0404406944653,
124.37381614118)) ;
#103521 = CARTESIAN_POINT('Ctrl Pts',(-20.7188663292308,-27.0504000992183,
124.158736104022)) ;
#103522 = CARTESIAN_POINT('Ctrl Pts',(-20.8288305573601,-27.0604383449232,
123.918970632662)) ;
#103523 = CARTESIAN_POINT('Ctrl Pts',(-20.8948668691598,-27.0703125290852,
123.667995182178)) ;
#103524 = CARTESIAN_POINT('Ctrl Pts',(-20.9167303039655,-27.0803823122231,
123.404313305881)) ;
#103525 = CARTESIAN_POINT('Ctrl Pts',(-20.8931805328912,-27.0902155672439,
123.146958571034)) ;
#103526 = CARTESIAN_POINT('Ctrl Pts',(-20.824670241342,-27.1002459933756,
122.892437582924)) ;
#103527 = CARTESIAN_POINT('Ctrl Pts',(-20.7122904917515,-27.1102776055626,
122.653954853305)) ;
#103528 = CARTESIAN_POINT('Ctrl Pts',(-20.5637282026505,-27.1201073024172,
122.442656891977)) ;
#103529 = CARTESIAN_POINT('Ctrl Pts',(-20.3782970637714,-27.1300967443197,
122.256829442602)) ;
#103530 = CARTESIAN_POINT('Ctrl Pts',(-20.1618698640858,-27.1401406363354,
122.105753614521)) ;
#103531 = CARTESIAN_POINT('Ctrl Pts',(-19.9280207270723,-27.1499621981046,
121.996530490058)) ;
#103532 = CARTESIAN_POINT('Ctrl Pts',(-19.6734949265312,-27.1599977697288,
121.927473665208)) ;
#103533 = CARTESIAN_POINT('Ctrl Pts',(-19.4109421353314,-27.1700270440106,
121.90446294825)) ;
#103534 = CARTESIAN_POINT('Ctrl Pts',(-19.1534313361619,-27.1798608811293,
121.926253148212)) ;
#103535 = CARTESIAN_POINT('Ctrl Pts',(-18.898003021736,-27.1899132772174,
121.993580901922)) ;
#103536 = CARTESIAN_POINT('Ctrl Pts',(-18.6610217719392,-27.1998500441679,
122.103281606099)) ;
#103537 = CARTESIAN_POINT('Ctrl Pts',(-18.4463698462864,-27.2097842791472,
122.25186257191)) ;
#103538 = CARTESIAN_POINT('Ctrl Pts',(-18.2592181860011,-27.219808042474,
122.437226698214)) ;
#103539 = CARTESIAN_POINT('Ctrl Pts',(-18.1090236019886,-27.2296943838587,
122.649213146899)) ;
#103540 = CARTESIAN_POINT('Ctrl Pts',(-17.9962080355324,-27.2396834326256,
122.886245303825)) ;
#103541 = CARTESIAN_POINT('Ctrl Pts',(-17.926428885886,-27.249724653323,123.140723215572)) ;
#103542 = CARTESIAN_POINT('Ctrl Pts',(-17.9019836209174,-27.2595572935009,
123.39795176562)) ;
#103543 = CARTESIAN_POINT('Ctrl Pts',(-17.9221604508856,-27.2695512228089,
123.659804082905)) ;
#103544 = CARTESIAN_POINT('Ctrl Pts',(-17.9882691006007,-27.2795804304894,
123.914937301455)) ;
#103545 = CARTESIAN_POINT('Ctrl Pts',(-18.0956205406589,-27.2894562421935,
124.151236044307)) ;
#103546 = CARTESIAN_POINT('Ctrl Pts',(-18.2439379922689,-27.2994554691649,
124.368102576697)) ;
#103547 = CARTESIAN_POINT('Ctrl Pts',(-18.4258819153618,-27.3093649503206,
124.554462932273)) ;
#103548 = CARTESIAN_POINT('Ctrl Pts',(-18.6404545665967,-27.3194181806215,
124.70853834946)) ;
#103549 = CARTESIAN_POINT('Ctrl Pts',(-18.8741825848005,-27.3292887971726,
124.821069860757)) ;
#103550 = CARTESIAN_POINT('Ctrl Pts',(-19.1275411645829,-27.3393104589046,
124.89294005617)) ;
#103551 = CARTESIAN_POINT('Ctrl Pts',(-19.389638167874,-27.3493332720857,
124.919131495704)) ;
#103552 = CARTESIAN_POINT('Ctrl Pts',(-19.6482300943565,-27.3592004365456,
124.900157768861)) ;
#103553 = CARTESIAN_POINT('Ctrl Pts',(-19.902982223414,-27.3691938787656,
124.836337874072)) ;
#103554 = CARTESIAN_POINT('Ctrl Pts',(-20.1434831381173,-27.3792255523659,
124.728378827775)) ;
#103555 = CARTESIAN_POINT('Ctrl Pts',(-20.3582270580471,-27.3890919874789,
124.583062625148)) ;
#103556 = CARTESIAN_POINT('Ctrl Pts',(-20.5470277371676,-27.399079438012,
124.400791657339)) ;
#103557 = CARTESIAN_POINT('Ctrl Pts',(-20.7008098488123,-27.4090243678399,
124.189436437923)) ;
#103558 = CARTESIAN_POINT('Ctrl Pts',(-20.816549998755,-27.4190692628951,
123.952221298349)) ;
#103559 = CARTESIAN_POINT('Ctrl Pts',(-20.8882501680196,-27.4289313245809,
123.703152220642)) ;
#103560 = CARTESIAN_POINT('Ctrl Pts',(-20.9164927273383,-27.4389230473678,
123.442124426353)) ;
#103561 = CARTESIAN_POINT('Ctrl Pts',(-20.8989909248932,-27.4488552616077,
123.181700468198)) ;
#103562 = CARTESIAN_POINT('Ctrl Pts',(-20.8370759801895,-27.4587945801734,
122.927942517171)) ;
#103563 = CARTESIAN_POINT('Ctrl Pts',(-20.730715480515,-27.4688387549493,
122.686374273125)) ;
#103564 = CARTESIAN_POINT('Ctrl Pts',(-20.5866771788675,-27.4787093090143,
122.470655142122)) ;
#103565 = CARTESIAN_POINT('Ctrl Pts',(-20.4062035407217,-27.4886742913685,
122.280905191679)) ;
#103566 = CARTESIAN_POINT('Ctrl Pts',(-20.1939015897808,-27.4987049942583,
122.124677894178)) ;
#103567 = CARTESIAN_POINT('Ctrl Pts',(-19.9610897598874,-27.5085973342835,
122.008944236056)) ;
#103568 = CARTESIAN_POINT('Ctrl Pts',(-19.7077373937747,-27.5186505674435,
121.934188358121)) ;
#103569 = CARTESIAN_POINT('Ctrl Pts',(-19.4496805193891,-27.5285318119202,
121.904898728865)) ;
#103570 = CARTESIAN_POINT('Ctrl Pts',(-19.1865551873291,-27.5385649327912,
121.920906361169)) ;
#103571 = CARTESIAN_POINT('Ctrl Pts',(-18.9339397336339,-27.5484461430663,
121.981224484517)) ;
#103572 = CARTESIAN_POINT('Ctrl Pts',(-18.691328088118,-27.5585082188356,
122.086276388266)) ;
#103573 = CARTESIAN_POINT('Ctrl Pts',(-18.4750234074904,-27.5683652772174,
122.228858024191)) ;
#103574 = CARTESIAN_POINT('Ctrl Pts',(-18.2838294855732,-27.5783598325064,
122.408874205211)) ;
#103575 = CARTESIAN_POINT('Ctrl Pts',(-18.1277548944552,-27.5882857200419,
122.617914347121)) ;
#103576 = CARTESIAN_POINT('Ctrl Pts',(-18.0091317372431,-27.5983107400372,
122.853121697837)) ;
#103577 = CARTESIAN_POINT('Ctrl Pts',(-17.9340214141047,-27.6082081171408,
123.102140704683)) ;
#103578 = CARTESIAN_POINT('Ctrl Pts',(-17.9024321371092,-27.6181983542217,
123.362773427688)) ;
#103579 = CARTESIAN_POINT('Ctrl Pts',(-17.9171489581271,-27.6282349670305,
123.626110492432)) ;
#103580 = CARTESIAN_POINT('Ctrl Pts',(-17.9758389387995,-27.6380848504485,
123.87822330786)) ;
#103581 = CARTESIAN_POINT('Ctrl Pts',(-18.0784974374125,-27.648088467351,
124.120206414581)) ;
#103582 = CARTESIAN_POINT('Ctrl Pts',(-18.221566977611,-27.6580778791161,
124.340354726405)) ;
#103583 = CARTESIAN_POINT('Ctrl Pts',(-18.4012882013648,-27.6680966404609,
124.532720748786)) ;
#103584 = CARTESIAN_POINT('Ctrl Pts',(-18.6786387524991,-27.681315315842,
124.741958869502)) ;
#103585 = CARTESIAN_POINT('Ctrl Pts',(-19.0063093815083,-27.6946256230867,
124.875054460151)) ;
#103586 = CARTESIAN_POINT('Ctrl Pts',(-19.3515549171491,-27.7078632893127,
124.918075531925)) ;
#103587 = CARTESIAN_POINT('Ctrl Pts',(-19.6119415048006,-27.7177829847234,
124.905729342981)) ;
#103588 = CARTESIAN_POINT('Ctrl Pts',(-19.8695625085415,-27.727835851722,
124.847299116356)) ;
#103589 = CARTESIAN_POINT('Ctrl Pts',(-20.1084867849093,-27.7376912600512,
124.747289288074)) ;
#103590 = CARTESIAN_POINT('Ctrl Pts',(-20.3306708426081,-27.7477298917278,
124.605097635172)) ;
#103591 = CARTESIAN_POINT('Ctrl Pts',(-20.5876397867162,-27.7610320739948,
124.36808782252)) ;
#103592 = CARTESIAN_POINT('Ctrl Pts',(-20.8234771617487,-27.7775770870777,
123.996910194884)) ;
#103593 = CARTESIAN_POINT('Ctrl Pts',(-20.9191962357907,-27.7942291031539,
123.564870810933)) ;
#103594 = CARTESIAN_POINT('Ctrl Pts',(-20.9040912184694,-27.8074521940591,
123.217672285098)) ;
#103595 = CARTESIAN_POINT('Ctrl Pts',(-20.8481766667372,-27.8174131536185,
122.96195496133)) ;
#103596 = CARTESIAN_POINT('Ctrl Pts',(-20.7477729122101,-27.8274379503696,
122.718403212381)) ;
#103597 = CARTESIAN_POINT('Ctrl Pts',(-20.561939019658,-27.8406623977654,
122.424695634254)) ;
#103598 = CARTESIAN_POINT('Ctrl Pts',(-20.2373190885059,-27.8572961824645,
122.124659826914)) ;
#103599 = CARTESIAN_POINT('Ctrl Pts',(-19.7495668232349,-27.8771988491894,
121.919809101773)) ;
#103600 = CARTESIAN_POINT('Ctrl Pts',(-19.2213679190859,-27.8970990769713,
121.893008326786)) ;
#103601 = CARTESIAN_POINT('Ctrl Pts',(-18.715153312022,-27.9170165645028,
122.047856538397)) ;
#103602 = CARTESIAN_POINT('Ctrl Pts',(-18.2916891277542,-27.9369460903197,
122.366103012824)) ;
#103603 = CARTESIAN_POINT('Ctrl Pts',(-18.0018513470074,-27.956908358206,
122.810537750514)) ;
#103604 = CARTESIAN_POINT('Ctrl Pts',(-17.8814933307081,-27.9767985531582,
123.325230056623)) ;
#103605 = CARTESIAN_POINT('Ctrl Pts',(-17.9426919986489,-27.9966887979044,
123.850442308538)) ;
#103606 = CARTESIAN_POINT('Ctrl Pts',(-18.1825385104849,-28.0167631704669,
124.326958710587)) ;
#103607 = CARTESIAN_POINT('Ctrl Pts',(-18.5649934168931,-28.0365485478272,
124.687973141665)) ;
#103608 = CARTESIAN_POINT('Ctrl Pts',(-19.0512254181737,-28.0565104218943,
124.900140533655)) ;
#103609 = CARTESIAN_POINT('Ctrl Pts',(-19.5812937356846,-28.0764903973848,
124.932412249247)) ;
#103610 = CARTESIAN_POINT('Ctrl Pts',(-20.0865931632847,-28.0963028272628,
124.784107050787)) ;
#103611 = CARTESIAN_POINT('Ctrl Pts',(-20.5148466735547,-28.1162829353531,
124.47026534295)) ;
#103612 = CARTESIAN_POINT('Ctrl Pts',(-20.8089552859383,-28.1361773189503,
124.030706928548)) ;
#103613 = CARTESIAN_POINT('Ctrl Pts',(-20.9360272834398,-28.1561042469275,
123.516674362654)) ;
#103614 = CARTESIAN_POINT('Ctrl Pts',(-20.8808267606801,-28.1759991042288,
122.990669662517)) ;
#103615 = CARTESIAN_POINT('Ctrl Pts',(-20.6473558405069,-28.1960382978324,
122.512016538107)) ;
#103616 = CARTESIAN_POINT('Ctrl Pts',(-20.2682120927934,-28.2158782657432,
122.145457364838)) ;
#103617 = CARTESIAN_POINT('Ctrl Pts',(-19.785573235683,-28.2357930827073,
121.928259829755)) ;
#103618 = CARTESIAN_POINT('Ctrl Pts',(-19.2570294438198,-28.2557353281035,
121.889112208248)) ;
#103619 = CARTESIAN_POINT('Ctrl Pts',(-18.748255376725,-28.275607376218,122.031351959434)) ;
#103620 = CARTESIAN_POINT('Ctrl Pts',(-18.3160158182085,-28.2956184411721,
122.340969391106)) ;
#103621 = CARTESIAN_POINT('Ctrl Pts',(-18.0174587947323,-28.3154299654757,
122.774994815369)) ;
#103622 = CARTESIAN_POINT('Ctrl Pts',(-17.8834629208939,-28.3355251774391,
123.291794909492)) ;
#103623 = CARTESIAN_POINT('Ctrl Pts',(-17.9332094404965,-28.3553059013589,
123.815384857237)) ;
#103624 = CARTESIAN_POINT('Ctrl Pts',(-18.1597591708436,-28.3752969770017,
124.29577732644)) ;
#103625 = CARTESIAN_POINT('Ctrl Pts',(-18.535084662371,-28.3951789160447,
124.667967825516)) ;
#103626 = CARTESIAN_POINT('Ctrl Pts',(-19.0161323560632,-28.415131520548,
124.890965555242)) ;
#103627 = CARTESIAN_POINT('Ctrl Pts',(-19.5431194959095,-28.4350303892786,
124.936306005945)) ;
#103628 = CARTESIAN_POINT('Ctrl Pts',(-20.0538297867874,-28.4549237890882,
124.799800715195)) ;
#103629 = CARTESIAN_POINT('Ctrl Pts',(-20.4882774828277,-28.4748329199282,
124.497523572711)) ;
#103630 = CARTESIAN_POINT('Ctrl Pts',(-20.7946918595222,-28.4948650196918,
124.062188352273)) ;
#103631 = CARTESIAN_POINT('Ctrl Pts',(-20.9099543609712,-28.5113970928613,
123.638087952506)) ;
#103632 = CARTESIAN_POINT('Ctrl Pts',(-20.9115545856091,-28.5247324334672,
123.287701393177)) ;
#103633 = CARTESIAN_POINT('Ctrl Pts',(-20.8682617470415,-28.5345749920069,
123.032666470944)) ;
#103634 = CARTESIAN_POINT('Ctrl Pts',(-20.7797764681059,-28.5446268988568,
122.783811473852)) ;
#103635 = CARTESIAN_POINT('Ctrl Pts',(-20.607853787178,-28.5578754132477,
122.48100626112)) ;
#103636 = CARTESIAN_POINT('Ctrl Pts',(-20.298677518794,-28.5744745881955,
122.166364976161)) ;
#103637 = CARTESIAN_POINT('Ctrl Pts',(-19.9009534723476,-28.5910633739905,
121.97606456656)) ;
#103638 = CARTESIAN_POINT('Ctrl Pts',(-19.5580552678904,-28.6043391903325,
121.911740597711)) ;
#103639 = CARTESIAN_POINT('Ctrl Pts',(-19.2959587737664,-28.6143130411263,
121.908503082593)) ;
#103640 = CARTESIAN_POINT('Ctrl Pts',(-19.0359171764911,-28.6243420732187,
121.951334244634)) ;
#103641 = CARTESIAN_POINT('Ctrl Pts',(-18.7905934021712,-28.6342321987206,
122.037205531534)) ;
#103642 = CARTESIAN_POINT('Ctrl Pts',(-18.5614284408685,-28.6442246769921,
122.165353939574)) ;
#103643 = CARTESIAN_POINT('Ctrl Pts',(-18.3586907974813,-28.6541758920895,
122.330596840673)) ;
#103644 = CARTESIAN_POINT('Ctrl Pts',(-18.1862612792095,-28.6642243938445,
122.530554327297)) ;
#103645 = CARTESIAN_POINT('Ctrl Pts',(-18.0536697103203,-28.6740657434613,
122.752628426208)) ;
#103646 = CARTESIAN_POINT('Ctrl Pts',(-17.959795093823,-28.6840520344815,
122.997646993215)) ;
#103647 = CARTESIAN_POINT('Ctrl Pts',(-17.9099939640272,-28.6939886462101,
123.254022115635)) ;
#103648 = CARTESIAN_POINT('Ctrl Pts',(-17.9055461660976,-28.7040385215777,
123.518058015356)) ;
#103649 = CARTESIAN_POINT('Ctrl Pts',(-17.9460039147784,-28.7138889801131,
123.773755758102)) ;
#103650 = CARTESIAN_POINT('Ctrl Pts',(-18.0306176772818,-28.7238609170659,
124.021737244033)) ;
#103651 = CARTESIAN_POINT('Ctrl Pts',(-18.157373568169,-28.733856373998,124.251845030224)) ;
#103652 = CARTESIAN_POINT('Ctrl Pts',(-18.3229702726794,-28.7438891810511,
124.456980828054)) ;
#103653 = CARTESIAN_POINT('Ctrl Pts',(-18.5180369157073,-28.7537490676411,
124.627546708464)) ;
#103654 = CARTESIAN_POINT('Ctrl Pts',(-18.7423754605247,-28.7637381482063,
124.763810474959)) ;
#103655 = CARTESIAN_POINT('Ctrl Pts',(-18.9855849680071,-28.7736696274155,
124.858511073407)) ;
#103656 = CARTESIAN_POINT('Ctrl Pts',(-19.2428700750694,-28.7836554868614,
124.910249736956)) ;
#103657 = CARTESIAN_POINT('Ctrl Pts',(-19.5065796970745,-28.7936936375086,
124.916096312179)) ;
#103658 = CARTESIAN_POINT('Ctrl Pts',(-19.7624834465028,-28.803541728013,
124.8773385409)) ;
#103659 = CARTESIAN_POINT('Ctrl Pts',(-20.0130929085487,-28.813602636531,
124.793179654348)) ;
#103660 = CARTESIAN_POINT('Ctrl Pts',(-20.2414099175365,-28.8234974836889,
124.668689114803)) ;
#103661 = CARTESIAN_POINT('Ctrl Pts',(-20.4459946353188,-28.833439155734,
124.506257858748)) ;
#103662 = CARTESIAN_POINT('Ctrl Pts',(-20.6204504823077,-28.8434416828595,
124.309593013046)) ;
#103663 = CARTESIAN_POINT('Ctrl Pts',(-20.7581704433979,-28.8534764740469,
124.084728431915)) ;
#103664 = CARTESIAN_POINT('Ctrl Pts',(-20.8533438150002,-28.863321353906,
123.844138419902)) ;
#103665 = CARTESIAN_POINT('Ctrl Pts',(-20.906513020906,-28.8733072345245,
123.58720590988)) ;
#103666 = CARTESIAN_POINT('Ctrl Pts',(-20.9144137492764,-28.8832419576177,
123.326201887984)) ;
#103667 = CARTESIAN_POINT('Ctrl Pts',(-20.8761831412985,-28.8932997979289,
123.064712473205)) ;
#103668 = CARTESIAN_POINT('Ctrl Pts',(-20.7954623118713,-28.9031202853254,
122.819554004774)) ;
#103669 = CARTESIAN_POINT('Ctrl Pts',(-20.6708356973687,-28.9131806866705,
122.58643084235)) ;
#103670 = CARTESIAN_POINT('Ctrl Pts',(-20.5094087231614,-28.9231116522234,
122.381333168133)) ;
#103671 = CARTESIAN_POINT('Ctrl Pts',(-20.3150976137856,-28.9330505145599,
122.20684661921)) ;
#103672 = CARTESIAN_POINT('Ctrl Pts',(-20.0924409972061,-28.9430362454861,
122.067919162026)) ;
#103673 = CARTESIAN_POINT('Ctrl Pts',(-19.8480433403635,-28.9530606309135,
121.969659854682)) ;
#103674 = CARTESIAN_POINT('Ctrl Pts',(-19.593440719786,-28.9629639152668,
121.915584792922)) ;
#103675 = CARTESIAN_POINT('Ctrl Pts',(-19.3292629768362,-28.9730239198448,
121.906485243782)) ;
#103676 = CARTESIAN_POINT('Ctrl Pts',(-19.0730746939001,-28.9828671889139,
121.942426938591)) ;
#103677 = CARTESIAN_POINT('Ctrl Pts',(-18.8232042085164,-28.9928577545216,
122.022902031652)) ;
#103678 = CARTESIAN_POINT('Ctrl Pts',(-18.5925340794096,-29.0027858863004,
122.14483093452)) ;
#103679 = CARTESIAN_POINT('Ctrl Pts',(-18.3850181563791,-29.0127737733813,
122.305561886804)) ;
#103680 = CARTESIAN_POINT('Ctrl Pts',(-18.2080606746573,-29.02280972295,122.501102325155)) ;
#103681 = CARTESIAN_POINT('Ctrl Pts',(-18.0698934323502,-29.0326646093288,
122.720167187635)) ;
#103682 = CARTESIAN_POINT('Ctrl Pts',(-17.9701183498815,-29.0426640236767,
122.963214409578)) ;
#103683 = CARTESIAN_POINT('Ctrl Pts',(-17.9143532599889,-29.0525591888672,
123.217244013255)) ;
#103684 = CARTESIAN_POINT('Ctrl Pts',(-17.9033934026888,-29.0626195075592,
123.481356106685)) ;
#103685 = CARTESIAN_POINT('Ctrl Pts',(-17.937582380809,-29.0724696393352,
123.737963166861)) ;
#103686 = CARTESIAN_POINT('Ctrl Pts',(-18.0166363100834,-29.0825002097855,
123.98940960622)) ;
#103687 = CARTESIAN_POINT('Ctrl Pts',(-18.1384821139156,-29.0925143604583,
124.222680263997)) ;
#103688 = CARTESIAN_POINT('Ctrl Pts',(-18.2966985543212,-29.1024072940037,
124.428975038743)) ;
#103689 = CARTESIAN_POINT('Ctrl Pts',(-18.4899775082618,-29.112396807994,
124.606580208232)) ;
#103690 = CARTESIAN_POINT('Ctrl Pts',(-18.7103271424368,-29.1223505786464,
124.747601568313)) ;
#103691 = CARTESIAN_POINT('Ctrl Pts',(-18.9541278519356,-29.132398347307,
124.848928066334)) ;
#103692 = CARTESIAN_POINT('Ctrl Pts',(-19.2065149359924,-29.1422400737468,
124.905514667488)) ;
#103693 = CARTESIAN_POINT('Ctrl Pts',(-19.4685786980452,-29.1522255905695,
124.918161518453)) ;
#103694 = CARTESIAN_POINT('Ctrl Pts',(-19.7277435431009,-29.1621649222651,
124.88535161819)) ;
#103695 = CARTESIAN_POINT('Ctrl Pts',(-19.979722346189,-29.1722046919626,
124.807223134211)) ;
#103696 = CARTESIAN_POINT('Ctrl Pts',(-20.2108569771339,-29.1820928532114,
124.688449404783)) ;
#103697 = CARTESIAN_POINT('Ctrl Pts',(-20.4202579427664,-29.1920824077138,
124.530143768635)) ;
#103698 = CARTESIAN_POINT('Ctrl Pts',(-20.5982897639513,-29.2020408222374,
124.338345472997)) ;
#103699 = CARTESIAN_POINT('Ctrl Pts',(-20.7400265330737,-29.2119407350668,
124.120168216643)) ;
#103700 = CARTESIAN_POINT('Ctrl Pts',(-20.843149350905,-29.2219874347167,
123.877151468186)) ;
#103701 = CARTESIAN_POINT('Ctrl Pts',(-20.9018183233676,-29.2318872950223,
123.62365382285)) ;
#103702 = CARTESIAN_POINT('Ctrl Pts',(-20.9158738240307,-29.2419386992278,
123.359924987347)) ;
#103703 = CARTESIAN_POINT('Ctrl Pts',(-20.8845500593917,-29.2518197361489,
123.102119232617)) ;
#103704 = CARTESIAN_POINT('Ctrl Pts',(-20.8083953396157,-29.2618195683264,
122.850656174921)) ;
#103705 = CARTESIAN_POINT('Ctrl Pts',(-20.6908578374418,-29.2717375713113,
122.617977476822)) ;
#103706 = CARTESIAN_POINT('Ctrl Pts',(-20.5325918654927,-29.2817888771858,
122.406561035641)) ;
#103707 = CARTESIAN_POINT('Ctrl Pts',(-20.3436416646335,-29.2916587005774,
122.228799630198)) ;
#103708 = CARTESIAN_POINT('Ctrl Pts',(-20.1222938931846,-29.3017328666277,
122.083680730194)) ;
#103709 = CARTESIAN_POINT('Ctrl Pts',(-19.8852598986933,-29.3115529507693,
121.981494645576)) ;
#103710 = CARTESIAN_POINT('Ctrl Pts',(-19.6276501727185,-29.3216316775052,
121.920236702777)) ;
#103711 = CARTESIAN_POINT('Ctrl Pts',(-19.3691535481643,-29.3314832581547,
121.904894321861)) ;
#103712 = CARTESIAN_POINT('Ctrl Pts',(-19.106218855204,-29.3415563864531,
121.935094557525)) ;
#103713 = CARTESIAN_POINT('Ctrl Pts',(-18.8582742358518,-29.3513988643445,
122.008822694386)) ;
#103714 = CARTESIAN_POINT('Ctrl Pts',(-18.6232933239942,-29.3613794709426,
122.125302992374)) ;
#103715 = CARTESIAN_POINT('Ctrl Pts',(-18.4116059083099,-29.3713971799614,
122.281799157481)) ;
#103716 = CARTESIAN_POINT('Ctrl Pts',(-18.2323066249273,-29.3812833589988,
122.469835868044)) ;
#103717 = CARTESIAN_POINT('Ctrl Pts',(-18.0858943600191,-29.3913409715712,
122.689852873575)) ;
#103718 = CARTESIAN_POINT('Ctrl Pts',(-17.9817783185599,-29.4012173649433,
122.927613195183)) ;
#103719 = CARTESIAN_POINT('Ctrl Pts',(-17.9191599044313,-29.4112123930937,
123.182690994245)) ;
#103720 = CARTESIAN_POINT('Ctrl Pts',(-17.9021863708431,-29.4212331399397,
123.445489631793)) ;
#103721 = CARTESIAN_POINT('Ctrl Pts',(-17.9304545075469,-29.4311352086061,
123.704163371341)) ;
#103722 = CARTESIAN_POINT('Ctrl Pts',(-18.0034882290822,-29.4411259484258,
123.956348533631)) ;
#103723 = CARTESIAN_POINT('Ctrl Pts',(-18.1190484241088,-29.4510891446361,
124.191274632941)) ;
#103724 = CARTESIAN_POINT('Ctrl Pts',(-18.2722296949224,-29.4609933289362,
124.40172526488)) ;
#103725 = CARTESIAN_POINT('Ctrl Pts',(-18.4626960378833,-29.4710537893271,
124.585031387986)) ;
#103726 = CARTESIAN_POINT('Ctrl Pts',(-18.6771724124148,-29.4808943351979,
124.729570547776)) ;
#103727 = CARTESIAN_POINT('Ctrl Pts',(-18.9186146981797,-29.4909565559097,
124.837323844312)) ;
#103728 = CARTESIAN_POINT('Ctrl Pts',(-19.1709983128989,-29.5008536989262,
124.900212053229)) ;
#103729 = CARTESIAN_POINT('Ctrl Pts',(-19.4312786043944,-29.5107848753434,
124.91924979015)) ;
#103730 = CARTESIAN_POINT('Ctrl Pts',(-19.6937852247348,-29.520827089122,
124.892221026757)) ;
#103731 = CARTESIAN_POINT('Ctrl Pts',(-19.9437477862045,-29.5307136293248,
124.821322725191)) ;
#103732 = CARTESIAN_POINT('Ctrl Pts',(-20.180288045457,-29.5407072239302,
124.707269113637)) ;
#103733 = CARTESIAN_POINT('Ctrl Pts',(-20.3923769599037,-29.5506510990877,
124.554587106928)) ;
#103734 = CARTESIAN_POINT('Ctrl Pts',(-20.5752625312194,-29.5606116352025,
124.367347599523)) ;
#103735 = CARTESIAN_POINT('Ctrl Pts',(-20.72354941688,-29.5706082385252,124.150467949388)) ;
#103736 = CARTESIAN_POINT('Ctrl Pts',(-20.8319671128854,-29.5806413214798,
123.910138102214)) ;
#103737 = CARTESIAN_POINT('Ctrl Pts',(-20.8961474318755,-29.5904924901813,
123.659345397393)) ;
#103738 = CARTESIAN_POINT('Ctrl Pts',(-20.9167993806516,-29.6004549808802,
123.398366694536)) ;
#103739 = CARTESIAN_POINT('Ctrl Pts',(-20.8913305106108,-29.6104834092979,
123.136048663369)) ;
#103740 = CARTESIAN_POINT('Ctrl Pts',(-20.8216212819003,-29.6203937766625,
122.885129389924)) ;
#103741 = CARTESIAN_POINT('Ctrl Pts',(-20.7097346900633,-29.6303286442776,
122.649232722637)) ;
#103742 = CARTESIAN_POINT('Ctrl Pts',(-20.5567809496011,-29.6403697862566,
122.434225112138)) ;
#103743 = CARTESIAN_POINT('Ctrl Pts',(-20.3718123627429,-29.6502569224598,
122.251734656416)) ;
#103744 = CARTESIAN_POINT('Ctrl Pts',(-20.1559695220388,-29.6602492048632,
122.102221999296)) ;
#103745 = CARTESIAN_POINT('Ctrl Pts',(-19.9184286726715,-29.6701977328284,
121.992991017142)) ;
#103746 = CARTESIAN_POINT('Ctrl Pts',(-19.6659588181329,-29.6801344639905,
121.92639428733)) ;
#103747 = CARTESIAN_POINT('Ctrl Pts',(-19.4045177020907,-29.6901176748505,
121.904213276698)) ;
#103748 = CARTESIAN_POINT('Ctrl Pts',(-19.1417307690133,-29.7001607740004,
121.928370870773)) ;
#103749 = CARTESIAN_POINT('Ctrl Pts',(-18.8922988626319,-29.7099917382753,
121.99578172201)) ;
#103750 = CARTESIAN_POINT('Ctrl Pts',(-18.6525893183493,-29.7200645906612,
122.107969662871)) ;
#103751 = CARTESIAN_POINT('Ctrl Pts',(-18.4404574740798,-29.729928718373,
122.257000197973)) ;
#103752 = CARTESIAN_POINT('Ctrl Pts',(-18.254059518917,-29.7399509205079,
122.443053886192)) ;
#103753 = CARTESIAN_POINT('Ctrl Pts',(-18.1032189608842,-29.7499781134763,
122.659132604409)) ;
#103754 = CARTESIAN_POINT('Ctrl Pts',(-17.9937340921863,-29.7598337074433,
122.893827180796)) ;
#103755 = CARTESIAN_POINT('Ctrl Pts',(-17.9252122856315,-29.7697908793086,
123.146369882271)) ;
#103756 = CARTESIAN_POINT('Ctrl Pts',(-17.9018420304546,-29.779829723307,
123.409126956835)) ;
#103757 = CARTESIAN_POINT('Ctrl Pts',(-17.9236263816137,-29.7897037471826,
123.667725112118)) ;
#103758 = CARTESIAN_POINT('Ctrl Pts',(-17.9912864175734,-29.799773573173,
123.923515498743)) ;
#103759 = CARTESIAN_POINT('Ctrl Pts',(-18.0996226494323,-29.8096068170702,
124.158141189941)) ;
#103760 = CARTESIAN_POINT('Ctrl Pts',(-18.2493770206669,-29.8196372448433,
124.375047214786)) ;
#103761 = CARTESIAN_POINT('Ctrl Pts',(-18.4351019059383,-29.8296688615884,
124.562155648745)) ;
#103762 = CARTESIAN_POINT('Ctrl Pts',(-18.6458216898426,-29.8394985385691,
124.711535811242)) ;
#103763 = CARTESIAN_POINT('Ctrl Pts',(-18.8827605878955,-29.8494880554091,
124.824574613372)) ;
#103764 = CARTESIAN_POINT('Ctrl Pts',(-19.1372642265583,-29.8595316675488,
124.894487285034)) ;
#103765 = CARTESIAN_POINT('Ctrl Pts',(-19.3942156196338,-29.8693542738841,
124.919144261192)) ;
#103766 = CARTESIAN_POINT('Ctrl Pts',(-19.6572275024493,-29.8793925037834,
124.898964132523)) ;
#103767 = CARTESIAN_POINT('Ctrl Pts',(-19.9119226482974,-29.8894035385753,
124.833001295873)) ;
#103768 = CARTESIAN_POINT('Ctrl Pts',(-20.1487376855666,-29.8993012695424,
124.725440344783)) ;
#103769 = CARTESIAN_POINT('Ctrl Pts',(-20.3654668126922,-29.9092908973929,
124.577311610302)) ;
#103770 = CARTESIAN_POINT('Ctrl Pts',(-20.5524835794486,-29.9192466878389,
124.394358132936)) ;
#103771 = CARTESIAN_POINT('Ctrl Pts',(-20.7048712583227,-29.929174086401,
124.182597989786)) ;
#103772 = CARTESIAN_POINT('Ctrl Pts',(-20.8192188729646,-29.9391996815108,
123.945254326094)) ;
#103773 = CARTESIAN_POINT('Ctrl Pts',(-20.8897800766452,-29.9490855321804,
123.69522895607)) ;
#103774 = CARTESIAN_POINT('Ctrl Pts',(-20.9167483241174,-29.9590747120246,
123.434105477145)) ;
#103775 = CARTESIAN_POINT('Ctrl Pts',(-20.8973194907971,-29.9691158991282,
123.170950732625)) ;
#103776 = CARTESIAN_POINT('Ctrl Pts',(-20.8342523640167,-29.9789485426041,
122.920378094351)) ;
#103777 = CARTESIAN_POINT('Ctrl Pts',(-20.7275885104511,-29.9889424923136,
122.680384913153)) ;
#103778 = CARTESIAN_POINT('Ctrl Pts',(-20.579894444544,-29.9989716150901,
122.462098463616)) ;
#103779 = CARTESIAN_POINT('Ctrl Pts',(-20.3996308019777,-30.0088477460088,
122.275363644049)) ;
#103780 = CARTESIAN_POINT('Ctrl Pts',(-20.1873078177901,-30.0188457810258,
122.120658794249)) ;
#103781 = CARTESIAN_POINT('Ctrl Pts',(-19.9533643834114,-30.0287597107845,
122.005933368096)) ;
#103782 = CARTESIAN_POINT('Ctrl Pts',(-19.6998574292392,-30.0388028985223,
121.932589562807)) ;
#103783 = CARTESIAN_POINT('Ctrl Pts',(-19.4411790736658,-30.0487027406627,
121.90475991674)) ;
#103784 = CARTESIAN_POINT('Ctrl Pts',(-19.1791749601021,-30.0586940074707,
121.92187067356)) ;
#103785 = CARTESIAN_POINT('Ctrl Pts',(-18.923186636168,-30.0687261096027,
121.984912250954)) ;
#103786 = CARTESIAN_POINT('Ctrl Pts',(-18.6858740646116,-30.0785929905574,
122.089372660142)) ;
#103787 = CARTESIAN_POINT('Ctrl Pts',(-18.4672188643047,-30.0885847818456,
122.234760413876)) ;
#103788 = CARTESIAN_POINT('Ctrl Pts',(-18.2767186120029,-30.0986168977571,
122.417001484085)) ;
#103789 = CARTESIAN_POINT('Ctrl Pts',(-18.1230072719438,-30.1084832145571,
122.625814784531)) ;
#103790 = CARTESIAN_POINT('Ctrl Pts',(-18.0061089947537,-30.1184706960307,
122.860769222352)) ;
#103791 = CARTESIAN_POINT('Ctrl Pts',(-17.931945641768,-30.1284156204096,
123.111407763213)) ;
#103792 = CARTESIAN_POINT('Ctrl Pts',(-17.902285286713,-30.1384605063203,
123.373680593113)) ;
#103793 = CARTESIAN_POINT('Ctrl Pts',(-17.9180936234547,-30.1483226100329,
123.632382529412)) ;
#103794 = CARTESIAN_POINT('Ctrl Pts',(-17.9788508601599,-30.1583141738574,
123.887804420223)) ;
#103795 = CARTESIAN_POINT('Ctrl Pts',(-18.082529173865,-30.1682469819203,
124.127353680839)) ;
#103796 = CARTESIAN_POINT('Ctrl Pts',(-18.2257613189898,-30.1781840841566,
124.345723367739)) ;
#103797 = CARTESIAN_POINT('Ctrl Pts',(-18.4070409249013,-30.188236530427,
124.5378471688)) ;
#103798 = CARTESIAN_POINT('Ctrl Pts',(-18.6143892810352,-30.1980826460086,
124.692661848958)) ;
#103799 = CARTESIAN_POINT('Ctrl Pts',(-18.8499856052171,-30.2081306657235,
124.811858051994)) ;
#103800 = CARTESIAN_POINT('Ctrl Pts',(-19.1001693147782,-30.2180726173524,
124.887190172848)) ;
#103801 = CARTESIAN_POINT('Ctrl Pts',(-19.3594615062715,-30.2280113983515,
124.918568712032)) ;
#103802 = CARTESIAN_POINT('Ctrl Pts',(-19.6225225666885,-30.2380374470776,
124.904126517866)) ;
#103803 = CARTESIAN_POINT('Ctrl Pts',(-19.8756411196743,-30.2479243074858,
124.845369531856)) ;
#103804 = CARTESIAN_POINT('Ctrl Pts',(-20.118180857874,-30.2579555826176,
124.742207394591)) ;
#103805 = CARTESIAN_POINT('Ctrl Pts',(-20.3360835875436,-30.267838559918,
124.600793521788)) ;
#103806 = CARTESIAN_POINT('Ctrl Pts',(-20.5293833327197,-30.2778954133252,
124.420660784419)) ;
#103807 = CARTESIAN_POINT('Ctrl Pts',(-20.7382619738942,-30.2910636544011,
124.14463477347)) ;
#103808 = CARTESIAN_POINT('Ctrl Pts',(-20.8725752561866,-30.3044646836276,
123.814915042498)) ;
#103809 = CARTESIAN_POINT('Ctrl Pts',(-20.9154721242773,-30.3176776003585,
123.470246273929)) ;
#103810 = CARTESIAN_POINT('Ctrl Pts',(-20.9031284982682,-30.3276059948117,
123.20968534208)) ;
#103811 = CARTESIAN_POINT('Ctrl Pts',(-20.845595566202,-30.3375874949398,
122.953729921305)) ;
#103812 = CARTESIAN_POINT('Ctrl Pts',(-20.7435783328316,-30.3476280382099,
122.71041030184)) ;
#103813 = CARTESIAN_POINT('Ctrl Pts',(-20.6038586708441,-30.357477369993,
122.492526903474)) ;
#103814 = CARTESIAN_POINT('Ctrl Pts',(-20.4263290632736,-30.3674727744647,
122.298938318789)) ;
#103815 = CARTESIAN_POINT('Ctrl Pts',(-20.2171560775748,-30.3774891019133,
122.139151077078)) ;
#103816 = CARTESIAN_POINT('Ctrl Pts',(-19.9087977156383,-30.3907127590798,
121.978849459773)) ;
#103817 = CARTESIAN_POINT('Ctrl Pts',(-19.5640016254491,-30.4040070504692,
121.902023533072)) ;
#103818 = CARTESIAN_POINT('Ctrl Pts',(-19.2151474722154,-30.4172914014007,
121.916899099156)) ;
#103819 = CARTESIAN_POINT('Ctrl Pts',(-18.959233385577,-30.4272637824625,
121.973159220254)) ;
#103820 = CARTESIAN_POINT('Ctrl Pts',(-18.7182905622047,-30.4371721620881,
122.071965239815)) ;
#103821 = CARTESIAN_POINT('Ctrl Pts',(-18.4950446956191,-30.4472261608362,
122.213218249538)) ;
#103822 = CARTESIAN_POINT('Ctrl Pts',(-18.3032677066978,-30.4570883579525,
122.387584195892)) ;
#103823 = CARTESIAN_POINT('Ctrl Pts',(-18.0882294345681,-30.4704354843266,
122.664654341648)) ;
#103824 = CARTESIAN_POINT('Ctrl Pts',(-17.9176691090608,-30.486972449968,
123.069789026375)) ;
#103825 = CARTESIAN_POINT('Ctrl Pts',(-17.8947689247543,-30.5036070541419,
123.511224766583)) ;
#103826 = CARTESIAN_POINT('Ctrl Pts',(-17.9677597605264,-30.5168968473846,
123.852822963271)) ;
#103827 = CARTESIAN_POINT('Ctrl Pts',(-18.0656623988113,-30.526849478644,
124.095320844935)) ;
#103828 = CARTESIAN_POINT('Ctrl Pts',(-18.2039451181577,-30.5368014459487,
124.31733383176)) ;
#103829 = CARTESIAN_POINT('Ctrl Pts',(-18.4387419579372,-30.5501687044125,
124.578559199658)) ;
#103830 = CARTESIAN_POINT('Ctrl Pts',(-18.8064348754556,-30.5666855163617,
124.818604195386)) ;
#103831 = CARTESIAN_POINT('Ctrl Pts',(-19.3245278534393,-30.586711411368,
124.939938502557)) ;
#103832 = CARTESIAN_POINT('Ctrl Pts',(-19.8475129838899,-30.6065221414982,
124.877995909629)) ;
#103833 = CARTESIAN_POINT('Ctrl Pts',(-20.3222986651346,-30.626499357628,
124.640403874148)) ;
#103834 = CARTESIAN_POINT('Ctrl Pts',(-20.6858947191827,-30.6464262330233,
124.255351813827)) ;
#103835 = CARTESIAN_POINT('Ctrl Pts',(-20.8967545754839,-30.6662476944996,
123.772491153533)) ;
#103836 = CARTESIAN_POINT('Ctrl Pts',(-20.930246289183,-30.6863220123089,
123.240081051915)) ;
#103837 = CARTESIAN_POINT('Ctrl Pts',(-20.7811801654248,-30.7061699813168,
122.733903286621)) ;
#103838 = CARTESIAN_POINT('Ctrl Pts',(-20.4678029638556,-30.72611701538,122.306420902074)) ;
#103839 = CARTESIAN_POINT('Ctrl Pts',(-20.0282836711341,-30.7460129663522,
122.012316933034)) ;
#103840 = CARTESIAN_POINT('Ctrl Pts',(-19.5150768163013,-30.7659084459704,
121.885022994691)) ;
#103841 = CARTESIAN_POINT('Ctrl Pts',(-18.9875493940089,-30.7858645569352,
121.940557548858)) ;
#103842 = CARTESIAN_POINT('Ctrl Pts',(-18.5120413479308,-30.8057691049752,
122.172263938977)) ;
#103843 = CARTESIAN_POINT('Ctrl Pts',(-18.1436329888451,-30.8256432292943,
122.550941964326)) ;
#103844 = CARTESIAN_POINT('Ctrl Pts',(-17.9253626279483,-30.8456977592933,
123.037127679994)) ;
#103845 = CARTESIAN_POINT('Ctrl Pts',(-17.8864163514803,-30.8655052730533,
123.562247075706)) ;
#103846 = CARTESIAN_POINT('Ctrl Pts',(-18.0291401244099,-30.885488628821,
124.073759282254)) ;
#103847 = CARTESIAN_POINT('Ctrl Pts',(-18.337533170565,-30.905406931405,124.504045807)) ;
#103848 = CARTESIAN_POINT('Ctrl Pts',(-18.7724388146455,-30.9252751468507,
124.803748537153)) ;
#103849 = CARTESIAN_POINT('Ctrl Pts',(-19.2881535897615,-30.945325463647,
124.937391160665)) ;
#103850 = CARTESIAN_POINT('Ctrl Pts',(-19.8116899255017,-30.9651015255295,
124.888384619558)) ;
#103851 = CARTESIAN_POINT('Ctrl Pts',(-20.2935526937828,-30.9851561312219,
124.661040470171)) ;
#103852 = CARTESIAN_POINT('Ctrl Pts',(-20.6641765582672,-31.0049498203778,
124.287452176797)) ;
#103853 = CARTESIAN_POINT('Ctrl Pts',(-20.8882002760577,-31.0249165119722,
123.806498159826)) ;
#103854 = CARTESIAN_POINT('Ctrl Pts',(-20.9338306071532,-31.0448765577232,
123.277860730245)) ;
#103855 = CARTESIAN_POINT('Ctrl Pts',(-20.7971227735034,-31.0647748178734,
122.767005346309)) ;
#103856 = CARTESIAN_POINT('Ctrl Pts',(-20.4948654308344,-31.0846697334226,
122.333164844512)) ;
#103857 = CARTESIAN_POINT('Ctrl Pts',(-20.0626416343406,-31.1045799138362,
122.027862379224)) ;
#103858 = CARTESIAN_POINT('Ctrl Pts',(-19.5515649705631,-31.1245157129505,
121.887964693884)) ;
#103859 = CARTESIAN_POINT('Ctrl Pts',(-19.0233903317203,-31.1444535746046,
121.930837086588)) ;
#103860 = CARTESIAN_POINT('Ctrl Pts',(-18.5418366268255,-31.1643726212422,
122.150882202806)) ;
#103861 = CARTESIAN_POINT('Ctrl Pts',(-18.1636869672622,-31.1843215192964,
122.522527872868)) ;
#103862 = CARTESIAN_POINT('Ctrl Pts',(-17.9354131762966,-31.2042273467395,
122.999837740766)) ;
#103863 = CARTESIAN_POINT('Ctrl Pts',(-17.8918991358355,-31.2208100421048,
123.438354996093)) ;
#103864 = CARTESIAN_POINT('Ctrl Pts',(-17.9480303730611,-31.2340842558284,
123.782695879663)) ;
#103865 = CARTESIAN_POINT('Ctrl Pts',(-18.0352352200072,-31.2441309750277,
124.03186648313)) ;
#103866 = CARTESIAN_POINT('Ctrl Pts',(-18.1615436066062,-31.2539750096734,
124.257643973845)) ;
#103867 = CARTESIAN_POINT('Ctrl Pts',(-18.3825173779386,-31.267309394578,
124.529587378034)) ;
#103868 = CARTESIAN_POINT('Ctrl Pts',(-18.7397346727777,-31.2838966118777,
124.78803912099)) ;
#103869 = CARTESIAN_POINT('Ctrl Pts',(-19.1646878984276,-31.3005298239156,
124.909727244072)) ;
#103870 = CARTESIAN_POINT('Ctrl Pts',(-19.5137260263734,-31.3138122661878,
124.915613465627)) ;
#103871 = CARTESIAN_POINT('Ctrl Pts',(-19.7708785665905,-31.323718154102,
124.875271313858)) ;
#103872 = CARTESIAN_POINT('Ctrl Pts',(-20.0193071233012,-31.3337065722071,
124.790489336724)) ;
#103873 = CARTESIAN_POINT('Ctrl Pts',(-20.2499079130323,-31.3437299994459,
124.663170280754)) ;
#103874 = CARTESIAN_POINT('Ctrl Pts',(-20.4525383938523,-31.3536344305629,
124.499840451095)) ;
#103875 = CARTESIAN_POINT('Ctrl Pts',(-20.6825176632985,-31.3668975831733,
124.237884196334)) ;
#103876 = CARTESIAN_POINT('Ctrl Pts',(-20.839220789519,-31.3802224810772,
123.920354669002)) ;
#103877 = CARTESIAN_POINT('Ctrl Pts',(-20.9074451283038,-31.3934782246928,
123.578700871149)) ;
#103878 = CARTESIAN_POINT('Ctrl Pts',(-20.9137386766837,-31.4034375981401,
123.317088900445)) ;
#103879 = CARTESIAN_POINT('Ctrl Pts',(-20.8748902920232,-31.4133814220671,
123.058646926955)) ;
#103880 = CARTESIAN_POINT('Ctrl Pts',(-20.790689481649,-31.4234293662144,
122.808403316486)) ;
#103881 = CARTESIAN_POINT('Ctrl Pts',(-20.6669783773769,-31.4332803374325,
122.580985502148)) ;
#103882 = CARTESIAN_POINT('Ctrl Pts',(-20.5042373768889,-31.4432521548746,
122.375633944712)) ;
#103883 = CARTESIAN_POINT('Ctrl Pts',(-20.3077702956413,-31.4532475771667,
122.201235204252)) ;
#103884 = CARTESIAN_POINT('Ctrl Pts',(-20.0830574195363,-31.4632806422904,
122.06333895259)) ;
#103885 = CARTESIAN_POINT('Ctrl Pts',(-19.8420046926258,-31.4731459749556,
121.967937569208)) ;
#103886 = CARTESIAN_POINT('Ctrl Pts',(-19.5857419131994,-31.4831065175532,
121.914580261074)) ;
#103887 = CARTESIAN_POINT('Ctrl Pts',(-19.3221912582714,-31.4931402030549,
121.906915941249)) ;
#103888 = CARTESIAN_POINT('Ctrl Pts',(-19.065070194438,-31.5030250350452,
121.944123034841)) ;
#103889 = CARTESIAN_POINT('Ctrl Pts',(-18.8138525163385,-31.513092461805,
122.026943078941)) ;
#103890 = CARTESIAN_POINT('Ctrl Pts',(-18.5859328586663,-31.5229309509638,
122.149094334289)) ;
#103891 = CARTESIAN_POINT('Ctrl Pts',(-18.3778842949295,-31.532994432154,
122.312293350143)) ;
#103892 = CARTESIAN_POINT('Ctrl Pts',(-18.2044268971495,-31.5428885899691,
122.506025289575)) ;
#103893 = CARTESIAN_POINT('Ctrl Pts',(-18.0660101087034,-31.5528304467134,
122.72756803597)) ;
#103894 = CARTESIAN_POINT('Ctrl Pts',(-17.9674492874552,-31.5628329243848,
122.971283743603)) ;
#103895 = CARTESIAN_POINT('Ctrl Pts',(-17.9129429280483,-31.5728677286891,
123.229275923166)) ;
#103896 = CARTESIAN_POINT('Ctrl Pts',(-17.9037929635874,-31.5827126055348,
123.487844790178)) ;
#103897 = CARTESIAN_POINT('Ctrl Pts',(-17.9396945692853,-31.5926984850903,
123.747752720024)) ;
#103898 = CARTESIAN_POINT('Ctrl Pts',(-18.0196152582505,-31.6026332154488,
123.996346627986)) ;
#103899 = CARTESIAN_POINT('Ctrl Pts',(-18.1431719765742,-31.6126910277617,
124.229948303937)) ;
#103900 = CARTESIAN_POINT('Ctrl Pts',(-18.3012886866371,-31.6225116198861,
124.433968126404)) ;
#103901 = CARTESIAN_POINT('Ctrl Pts',(-18.4969247202593,-31.6325782054958,
124.611955117681)) ;
#103902 = CARTESIAN_POINT('Ctrl Pts',(-18.7169060912058,-31.6424777860777,
124.750945809857)) ;
#103903 = CARTESIAN_POINT('Ctrl Pts',(-18.9612356540636,-31.6525293857559,
124.851194511038)) ;
#103904 = CARTESIAN_POINT('Ctrl Pts',(-19.2147603866341,-31.6624035721729,
124.906716070212)) ;
#103905 = CARTESIAN_POINT('Ctrl Pts',(-19.4787552825283,-31.6724600480538,
124.917736501395)) ;
#103906 = CARTESIAN_POINT('Ctrl Pts',(-19.7365095844923,-31.6823529793564,
124.883403147334)) ;
#103907 = CARTESIAN_POINT('Ctrl Pts',(-19.9885638779388,-31.692415758069,
124.803566593134)) ;
#103908 = CARTESIAN_POINT('Ctrl Pts',(-20.2179239107843,-31.7022582836502,
124.683939181233)) ;
#103909 = CARTESIAN_POINT('Ctrl Pts',(-20.4264476740645,-31.7122490490751,
124.524468053743)) ;
#103910 = CARTESIAN_POINT('Ctrl Pts',(-20.6029964283698,-31.7221771250731,
124.332359890327)) ;
#103911 = CARTESIAN_POINT('Ctrl Pts',(-20.7447399387057,-31.7321650354601,
124.111438651362)) ;
#103912 = CARTESIAN_POINT('Ctrl Pts',(-20.8460360924056,-31.7422009475851,
123.86794571088)) ;
#103913 = CARTESIAN_POINT('Ctrl Pts',(-20.9029032854347,-31.7520559604328,
123.615266109282)) ;
#103914 = CARTESIAN_POINT('Ctrl Pts',(-20.9155733480408,-31.762054906349,
123.352852263318)) ;
#103915 = CARTESIAN_POINT('Ctrl Pts',(-20.8830661672857,-31.771951818797,
123.094770422917)) ;
#103916 = CARTESIAN_POINT('Ctrl Pts',(-20.805075041774,-31.7820056168905,
122.842374659832)) ;
#103917 = CARTESIAN_POINT('Ctrl Pts',(-20.6865579770331,-31.7918865377172,
122.611306695334)) ;
#103918 = CARTESIAN_POINT('Ctrl Pts',(-20.5281726394026,-31.8018910637149,
122.401499882872)) ;
#103919 = CARTESIAN_POINT('Ctrl Pts',(-20.3360508018856,-31.8118750273324,
122.222755856703)) ;
#103920 = CARTESIAN_POINT('Ctrl Pts',(-20.114501453404,-31.8219146678837,
122.079534168689)) ;
#103921 = CARTESIAN_POINT('Ctrl Pts',(-19.8762895233033,-31.8317586934984,
121.978654244204)) ;
#103922 = CARTESIAN_POINT('Ctrl Pts',(-19.6205867174948,-31.8417496993158,
121.91906612885)) ;
#103923 = CARTESIAN_POINT('Ctrl Pts',(-19.3571632790607,-31.8517874908479,
121.905315885654)) ;
#103924 = CARTESIAN_POINT('Ctrl Pts',(-19.1003324547463,-31.8616318906363,
121.936442553235)) ;
#103925 = CARTESIAN_POINT('Ctrl Pts',(-18.8491694989756,-31.8716166911931,
122.012255191191)) ;
#103926 = CARTESIAN_POINT('Ctrl Pts',(-18.6159330601628,-31.8815562146042,
122.129920757266)) ;
#103927 = CARTESIAN_POINT('Ctrl Pts',(-18.4046433765393,-31.8915959337052,
122.287888249749)) ;
#103928 = CARTESIAN_POINT('Ctrl Pts',(-18.2265989768632,-31.9014841056245,
122.477178257837)) ;
#103929 = CARTESIAN_POINT('Ctrl Pts',(-18.0822682824921,-31.9114736680415,
122.696445093943)) ;
#103930 = CARTESIAN_POINT('Ctrl Pts',(-17.9787051620355,-31.9214320402362,
122.93677177021)) ;
#103931 = CARTESIAN_POINT('Ctrl Pts',(-17.9181842500413,-31.9313321144669,
123.189808215858)) ;
#103932 = CARTESIAN_POINT('Ctrl Pts',(-17.9023233424814,-31.9413782108405,
123.453319896886)) ;
#103933 = CARTESIAN_POINT('Ctrl Pts',(-17.9320326075536,-31.9512867948376,
123.712019221572)) ;
#103934 = CARTESIAN_POINT('Ctrl Pts',(-18.0065039243755,-31.9612973734285,
123.964329620109)) ;
#103935 = CARTESIAN_POINT('Ctrl Pts',(-18.1243506026566,-31.9713265315413,
124.200081050847)) ;
#103936 = CARTESIAN_POINT('Ctrl Pts',(-18.2782680242316,-31.9811794133794,
124.40826979115)) ;
#103937 = CARTESIAN_POINT('Ctrl Pts',(-18.4674892383523,-31.9911389745304,
124.589102665901)) ;
#103938 = CARTESIAN_POINT('Ctrl Pts',(-18.6872050266719,-32.0011774091195,
124.735068510236)) ;
#103939 = CARTESIAN_POINT('Ctrl Pts',(-18.9248081639537,-32.0110506813466,
124.839402319845)) ;
#103940 = CARTESIAN_POINT('Ctrl Pts',(-19.181949548147,-32.0211239233402,
124.90203769337)) ;
#103941 = CARTESIAN_POINT('Ctrl Pts',(-19.4395184189377,-32.0309442548732,
124.918991539094)) ;
#103942 = CARTESIAN_POINT('Ctrl Pts',(-19.7027715416863,-32.0410229161,124.89048408525)) ;
#103943 = CARTESIAN_POINT('Ctrl Pts',(-19.9514922038896,-32.0508745113942,
124.818414826773)) ;
#103944 = CARTESIAN_POINT('Ctrl Pts',(-20.1891501198683,-32.060947646623,
124.701943720578)) ;
#103945 = CARTESIAN_POINT('Ctrl Pts',(-20.3981122420389,-32.0707900821481,
124.549474888868)) ;
#103946 = CARTESIAN_POINT('Ctrl Pts',(-20.5805492966347,-32.0807708512815,
124.36105417391)) ;
#103947 = CARTESIAN_POINT('Ctrl Pts',(-20.7276369905565,-32.0907879525253,
124.142742755628)) ;
#103948 = CARTESIAN_POINT('Ctrl Pts',(-20.8336659742362,-32.1006764001272,
123.905478070317)) ;
#103949 = CARTESIAN_POINT('Ctrl Pts',(-20.89797251278,-32.110732114308,123.64919325748)) ;
#103950 = CARTESIAN_POINT('Ctrl Pts',(-20.9165067433349,-32.1206073207219,
123.390327809579)) ;
#103951 = CARTESIAN_POINT('Ctrl Pts',(-20.8901191956421,-32.1306023731946,
123.129004709564)) ;
#103952 = CARTESIAN_POINT('Ctrl Pts',(-20.8181509922566,-32.1406242571567,
122.875653953952)) ;
#103953 = CARTESIAN_POINT('Ctrl Pts',(-20.7049044906202,-32.150528229686,
122.641318954081)) ;
#103954 = CARTESIAN_POINT('Ctrl Pts',(-20.5516953308021,-32.1605167263469,
122.428181402184)) ;
#103955 = CARTESIAN_POINT('Ctrl Pts',(-20.364157218951,-32.1704805235949,
122.245474808793)) ;
#103956 = CARTESIAN_POINT('Ctrl Pts',(-20.1493697802425,-32.1803845469029,
122.09844282486)) ;
#103957 = CARTESIAN_POINT('Ctrl Pts',(-19.9085318955107,-32.1904450502245,
121.98946512821)) ;
#103958 = CARTESIAN_POINT('Ctrl Pts',(-19.6580461891382,-32.2002855853644,
121.925056304293)) ;
#103959 = CARTESIAN_POINT('Ctrl Pts',(-19.3944634329032,-32.210347806069,
121.904337209597)) ;
#103960 = CARTESIAN_POINT('Ctrl Pts',(-19.1355881131664,-32.2202449598452,
121.929557911688)) ;
#103961 = CARTESIAN_POINT('Ctrl Pts',(-18.8839506136458,-32.2301760932307,
121.998741559516)) ;
#103962 = CARTESIAN_POINT('Ctrl Pts',(-18.6456320558467,-32.2402184683764,
122.112083948383)) ;
#103963 = CARTESIAN_POINT('Ctrl Pts',(-18.4338299848013,-32.2501044061426,
122.262549762622)) ;
#103964 = CARTESIAN_POINT('Ctrl Pts',(-18.2490783902629,-32.2601002491274,
122.449250229283)) ;
#103965 = CARTESIAN_POINT('Ctrl Pts',(-18.1003611064684,-32.270042227006,
122.664076171763)) ;
#103966 = CARTESIAN_POINT('Ctrl Pts',(-17.9907012439229,-32.280001601487,
122.901700707296)) ;
#103967 = CARTESIAN_POINT('Ctrl Pts',(-17.9235757952326,-32.2899982173208,
123.155708820772)) ;
#103968 = CARTESIAN_POINT('Ctrl Pts',(-17.9018434365828,-32.3000324358943,
123.418492645025)) ;
#103969 = CARTESIAN_POINT('Ctrl Pts',(-17.9253190230438,-32.3098855031049,
123.676351623004)) ;
#103970 = CARTESIAN_POINT('Ctrl Pts',(-17.9932107833042,-32.3198457609825,
123.929129584466)) ;
#103971 = CARTESIAN_POINT('Ctrl Pts',(-18.1050181199454,-32.3298747876881,
124.167805856083)) ;
#103972 = CARTESIAN_POINT('Ctrl Pts',(-18.2546963393557,-32.3397849947225,
124.380912347066)) ;
#103973 = CARTESIAN_POINT('Ctrl Pts',(-18.4390908104522,-32.3497199053701,
124.565750061479)) ;
#103974 = CARTESIAN_POINT('Ctrl Pts',(-18.655191043716,-32.3597610355494,
124.717155840492)) ;
#103975 = CARTESIAN_POINT('Ctrl Pts',(-18.8905747900674,-32.3696481759193,
124.827204201677)) ;
#103976 = CARTESIAN_POINT('Ctrl Pts',(-19.1440130868697,-32.3796404534553,
124.895842668681)) ;
#103977 = CARTESIAN_POINT('Ctrl Pts',(-19.4044139426701,-32.3895889967236,
124.919259338434)) ;
#103978 = CARTESIAN_POINT('Ctrl Pts',(-19.6646123363536,-32.3995256715408,
124.897507120475)) ;
#103979 = CARTESIAN_POINT('Ctrl Pts',(-19.9183942075054,-32.4095090924772,
124.830886610359)) ;
#103980 = CARTESIAN_POINT('Ctrl Pts',(-20.1579441016645,-32.4195514076664,
124.720194156336)) ;
#103981 = CARTESIAN_POINT('Ctrl Pts',(-20.3705294988008,-32.4293917251056,
124.572953421427)) ;
#103982 = CARTESIAN_POINT('Ctrl Pts',(-20.5582907454371,-32.4394214291631,
124.387976381289)) ;
#103983 = CARTESIAN_POINT('Ctrl Pts',(-20.7103679401522,-32.4494423858856,
124.172987380055)) ;
#103984 = CARTESIAN_POINT('Ctrl Pts',(-20.8216818684755,-32.4593089281892,
123.938794053993)) ;
#103985 = CARTESIAN_POINT('Ctrl Pts',(-20.8920616476232,-32.4693800281344,
123.68369126668)) ;
#103986 = CARTESIAN_POINT('Ctrl Pts',(-20.9165062443481,-32.4792221023119,
123.426199168448)) ;
#103987 = CARTESIAN_POINT('Ctrl Pts',(-20.8965853084581,-32.489182896899,
123.165204807569)) ;
#103988 = CARTESIAN_POINT('Ctrl Pts',(-20.8306424357435,-32.4992207697998,
122.909804904941)) ;
#103989 = CARTESIAN_POINT('Ctrl Pts',(-20.7235568389697,-32.5090950553439,
122.673410322637)) ;
#103990 = CARTESIAN_POINT('Ctrl Pts',(-20.5741779867741,-32.5191648057578,
122.455025135462)) ;
#103991 = CARTESIAN_POINT('Ctrl Pts',(-20.3935542879197,-32.5289980902925,
122.270197537221)) ;
#103992 = CARTESIAN_POINT('Ctrl Pts',(-20.1798353645603,-32.5390284310925,
122.115931069202)) ;
#103993 = CARTESIAN_POINT('Ctrl Pts',(-19.9421855351004,-32.5490603550921,
122.00178683298)) ;
#103994 = CARTESIAN_POINT('Ctrl Pts',(-19.6936476667716,-32.558888890028,
121.931549021349)) ;
#103995 = CARTESIAN_POINT('Ctrl Pts',(-19.4324328552306,-32.5688826677927,
121.904377531945)) ;
#103996 = CARTESIAN_POINT('Ctrl Pts',(-19.1696058306266,-32.5789103782782,
121.923555881501)) ;
#103997 = CARTESIAN_POINT('Ctrl Pts',(-18.9175767373303,-32.5887987891122,
121.986866859931)) ;
#103998 = CARTESIAN_POINT('Ctrl Pts',(-18.6780807546885,-32.5987756396477,
122.093498427882)) ;
#103999 = CARTESIAN_POINT('Ctrl Pts',(-18.4603518607013,-32.6087674361982,
122.240328150281)) ;
#104000 = CARTESIAN_POINT('Ctrl Pts',(-18.2708550108699,-32.6188034422919,
122.423729946212)) ;
#104001 = CARTESIAN_POINT('Ctrl Pts',(-18.1185911041515,-32.6286541765547,
122.633104887947)) ;
#104002 = CARTESIAN_POINT('Ctrl Pts',(-18.0029925436642,-32.6386454350829,
122.868805920096)) ;
#104003 = CARTESIAN_POINT('Ctrl Pts',(-17.9304420380305,-32.6485633299861,
123.119171510775)) ;
#104004 = CARTESIAN_POINT('Ctrl Pts',(-17.9020933992958,-32.6585914716491,
123.381149752802)) ;
#104005 = CARTESIAN_POINT('Ctrl Pts',(-17.9193058243358,-32.668476639765,
123.640357610124)) ;
#104006 = CARTESIAN_POINT('Ctrl Pts',(-17.9812965034311,-32.678466003271,
123.895448517053)) ;
#104007 = CARTESIAN_POINT('Ctrl Pts',(-18.0876915909878,-32.6885071382811,
124.136918337839)) ;
#104008 = CARTESIAN_POINT('Ctrl Pts',(-18.2309953121228,-32.6983398064691,
124.351926017212)) ;
#104009 = CARTESIAN_POINT('Ctrl Pts',(-18.4118383831064,-32.7083337094236,
124.542370821151)) ;
#104010 = CARTESIAN_POINT('Ctrl Pts',(-18.6240841226523,-32.7183629945081,
124.698627680039)) ;
#104011 = CARTESIAN_POINT('Ctrl Pts',(-18.8564392926519,-32.72823852295,124.814248563428)) ;
#104012 = CARTESIAN_POINT('Ctrl Pts',(-19.108357609205,-32.7382388055661,
124.888964680306)) ;
#104013 = CARTESIAN_POINT('Ctrl Pts',(-19.3671572036663,-32.7481508216231,
124.91875728521)) ;
#104014 = CARTESIAN_POINT('Ctrl Pts',(-19.6305640135305,-32.7581928969621,
124.903027332527)) ;
#104015 = CARTESIAN_POINT('Ctrl Pts',(-19.8836327781885,-32.7680927296182,
124.842652966499)) ;
#104016 = CARTESIAN_POINT('Ctrl Pts',(-20.1248258731489,-32.7780851301962,
124.738828307188)) ;
#104017 = CARTESIAN_POINT('Ctrl Pts',(-20.3449875884632,-32.7881191519556,
124.593707305374)) ;
#104018 = CARTESIAN_POINT('Ctrl Pts',(-20.5335942693008,-32.7979837627968,
124.415869847909)) ;
#104019 = CARTESIAN_POINT('Ctrl Pts',(-20.6909834644273,-32.807976162258,
124.205669296647)) ;
#104020 = CARTESIAN_POINT('Ctrl Pts',(-20.8094889241104,-32.8180081155909,
123.970176958909)) ;
#104021 = CARTESIAN_POINT('Ctrl Pts',(-20.8844377190578,-32.8278744745325,
123.721956675228)) ;
#104022 = CARTESIAN_POINT('Ctrl Pts',(-20.915945398737,-32.8378619500183,
123.46142651116)) ;
#104023 = CARTESIAN_POINT('Ctrl Pts',(-20.9019344264893,-32.8478068562068,
123.200421706081)) ;
#104024 = CARTESIAN_POINT('Ctrl Pts',(-20.8420906768917,-32.857851820867,
122.943349727935)) ;
#104025 = CARTESIAN_POINT('Ctrl Pts',(-20.7406060025703,-32.8677136277719,
122.704864899941)) ;
#104026 = CARTESIAN_POINT('Ctrl Pts',(-20.5978277819379,-32.8777063000777,
122.484507609776)) ;
#104027 = CARTESIAN_POINT('Ctrl Pts',(-20.4200501081656,-32.887634971023,
122.29350842051)) ;
#104028 = CARTESIAN_POINT('Ctrl Pts',(-20.2115950206297,-32.8975875132483,
122.135579849619)) ;
#104029 = CARTESIAN_POINT('Ctrl Pts',(-19.9777664676753,-32.9075888692442,
122.015514768882)) ;
#104030 = CARTESIAN_POINT('Ctrl Pts',(-19.7258893468962,-32.9176174815189,
121.938018230432)) ;
#104031 = CARTESIAN_POINT('Ctrl Pts',(-19.4686840401609,-32.9274818160684,
121.905586079296)) ;
#104032 = CARTESIAN_POINT('Ctrl Pts',(-19.2064279001672,-32.937474140145,
121.918060847947)) ;
#104033 = CARTESIAN_POINT('Ctrl Pts',(-18.9518780958547,-32.9474016325109,
121.9753702803)) ;
#104034 = CARTESIAN_POINT('Ctrl Pts',(-18.7087932303638,-32.9574289910617,
122.077002166667)) ;
#104035 = CARTESIAN_POINT('Ctrl Pts',(-18.489955040994,-32.9673154091128,
122.217103045502)) ;
#104036 = CARTESIAN_POINT('Ctrl Pts',(-18.2959274596919,-32.9773471438482,
122.395505831268)) ;
#104037 = CARTESIAN_POINT('Ctrl Pts',(-18.1379626696296,-32.9872287250915,
122.601670693589)) ;
#104038 = CARTESIAN_POINT('Ctrl Pts',(-18.0159920766457,-32.9972907031238,
122.836231079081)) ;
#104039 = CARTESIAN_POINT('Ctrl Pts',(-17.9381053441153,-33.0071477814855,
123.083316174594)) ;
#104040 = CARTESIAN_POINT('Ctrl Pts',(-17.9033191170827,-33.0171423545915,
123.343606451348)) ;
#104041 = CARTESIAN_POINT('Ctrl Pts',(-17.9140894742016,-33.0270681508791,
123.604259742982)) ;
#104042 = CARTESIAN_POINT('Ctrl Pts',(-17.9704344775412,-33.0370935180488,
123.861598418745)) ;
#104043 = CARTESIAN_POINT('Ctrl Pts',(-18.0692237668632,-33.0469895977027,
124.10217377657)) ;
#104044 = CARTESIAN_POINT('Ctrl Pts',(-18.2092225151571,-33.0569846774083,
124.324417544489)) ;
#104045 = CARTESIAN_POINT('Ctrl Pts',(-18.3865446424699,-33.0670097652241,
124.519256056386)) ;
#104046 = CARTESIAN_POINT('Ctrl Pts',(-18.6603047019322,-33.0801935875914,
124.731592942589)) ;
#104047 = CARTESIAN_POINT('Ctrl Pts',(-18.9863004972768,-33.0935157057373,
124.869727826814)) ;
#104048 = CARTESIAN_POINT('Ctrl Pts',(-19.3347071906035,-33.1068949153649,
124.91736369268)) ;
#104049 = CARTESIAN_POINT('Ctrl Pts',(-19.5930892399671,-33.1167331526091,
124.908073601812)) ;
#104050 = CARTESIAN_POINT('Ctrl Pts',(-19.8519494157696,-33.1268060758678,
124.852893187197)) ;
#104051 = CARTESIAN_POINT('Ctrl Pts',(-20.0920658651421,-33.1366627173229,
124.755687076181)) ;
#104052 = CARTESIAN_POINT('Ctrl Pts',(-20.3148680362745,-33.146648092829,
124.617083859547)) ;
#104053 = CARTESIAN_POINT('Ctrl Pts',(-20.5745145257892,-33.1599321242894,
124.383830412476)) ;
#104054 = CARTESIAN_POINT('Ctrl Pts',(-20.8154972870975,-33.1764509161598,
124.016642542163)) ;
#104055 = CARTESIAN_POINT('Ctrl Pts',(-20.9173126871173,-33.1932366331664,
123.582410699086)) ;
#104056 = CARTESIAN_POINT('Ctrl Pts',(-20.9065209327429,-33.2063497816754,
123.23789572756)) ;
#104057 = CARTESIAN_POINT('Ctrl Pts',(-20.8536580502004,-33.2163853307556,
122.979562774912)) ;
#104058 = CARTESIAN_POINT('Ctrl Pts',(-20.756198899228,-33.226401386935,122.735025148292)) ;
#104059 = CARTESIAN_POINT('Ctrl Pts',(-20.5747412709195,-33.239579422801,
122.44012359768)) ;
#104060 = CARTESIAN_POINT('Ctrl Pts',(-20.2550698779711,-33.2561812999881,
122.13585359014)) ;
#104061 = CARTESIAN_POINT('Ctrl Pts',(-19.7659385098357,-33.276244444604,
121.92353087025)) ;
#104062 = CARTESIAN_POINT('Ctrl Pts',(-19.2406100026333,-33.2960453346877,
121.890966023112)) ;
#104063 = CARTESIAN_POINT('Ctrl Pts',(-18.7318475042929,-33.3159884599664,
122.039373055726)) ;
#104064 = CARTESIAN_POINT('Ctrl Pts',(-18.3053808778122,-33.335886505086,
122.352108672438)) ;
#104065 = CARTESIAN_POINT('Ctrl Pts',(-18.0102720492938,-33.3557722647127,
122.790666346431)) ;
#104066 = CARTESIAN_POINT('Ctrl Pts',(-17.8822194175528,-33.3758374398926,
123.308319761272)) ;
#104067 = CARTESIAN_POINT('Ctrl Pts',(-17.9380299181868,-33.3956640829954,
123.832405348603)) ;
#104068 = CARTESIAN_POINT('Ctrl Pts',(-18.1688789178654,-33.4155727924438,
124.308378401184)) ;
#104069 = CARTESIAN_POINT('Ctrl Pts',(-18.5492341213423,-33.4355246294756,
124.678096369158)) ;
#104070 = CARTESIAN_POINT('Ctrl Pts',(-19.0344596868479,-33.4555331041787,
124.895580763503)) ;
#104071 = CARTESIAN_POINT('Ctrl Pts',(-19.559310109334,-33.4753345629402,
124.934655150607)) ;
#104072 = CARTESIAN_POINT('Ctrl Pts',(-20.0703244585672,-33.4952914511762,
124.792494318584)) ;
#104073 = CARTESIAN_POINT('Ctrl Pts',(-20.5020203609189,-33.5152752885903,
124.48310031143)) ;
#104074 = CARTESIAN_POINT('Ctrl Pts',(-20.8005186071669,-33.5350837278112,
124.049341107837)) ;
#104075 = CARTESIAN_POINT('Ctrl Pts',(-20.9347384844056,-33.5550694371914,
123.535554589158)) ;
#104076 = CARTESIAN_POINT('Ctrl Pts',(-20.885999032978,-33.5749389602067,
123.009493296955)) ;
#104077 = CARTESIAN_POINT('Ctrl Pts',(-20.6589346591422,-33.5949596993239,
122.528474746676)) ;
#104078 = CARTESIAN_POINT('Ctrl Pts',(-20.2856374495452,-33.6147637643009,
122.157109094538)) ;
#104079 = CARTESIAN_POINT('Ctrl Pts',(-19.8021945775454,-33.6348257280316,
121.932516764001)) ;
#104080 = CARTESIAN_POINT('Ctrl Pts',(-19.2768728976166,-33.6546589083201,
121.887399060282)) ;
#104081 = CARTESIAN_POINT('Ctrl Pts',(-18.7653006877327,-33.6745781056462,
122.023356004672)) ;
#104082 = CARTESIAN_POINT('Ctrl Pts',(-18.3305408655223,-33.6945161307595,
122.326341401192)) ;
#104083 = CARTESIAN_POINT('Ctrl Pts',(-18.0255479439294,-33.7143941768156,
122.757806077686)) ;
#104084 = CARTESIAN_POINT('Ctrl Pts',(-17.8853382109855,-33.7343789111036,
123.270057467913)) ;
#104085 = CARTESIAN_POINT('Ctrl Pts',(-17.9281121953389,-33.7542897277821,
123.797675941426)) ;
#104086 = CARTESIAN_POINT('Ctrl Pts',(-18.149539016089,-33.7742887033008,
124.280760470711)) ;
#104087 = CARTESIAN_POINT('Ctrl Pts',(-18.5185934989486,-33.794093623946,
124.656245044893)) ;
#104088 = CARTESIAN_POINT('Ctrl Pts',(-18.997373933869,-33.8140775842373,
124.885911032148)) ;
#104089 = CARTESIAN_POINT('Ctrl Pts',(-19.5234533792043,-33.8339637879612,
124.937945343118)) ;
#104090 = CARTESIAN_POINT('Ctrl Pts',(-20.0373357964093,-33.8539129662844,
124.807538175658)) ;
#104091 = CARTESIAN_POINT('Ctrl Pts',(-20.4747860229475,-33.8738147655239,
124.510187926931)) ;
#104092 = CARTESIAN_POINT('Ctrl Pts',(-20.785074811108,-33.8936933705763,
124.082527143795)) ;
#104093 = CARTESIAN_POINT('Ctrl Pts',(-20.9316937197507,-33.913725730302,
123.570655928487)) ;
#104094 = CARTESIAN_POINT('Ctrl Pts',(-20.9004897306885,-33.9303074562581,
123.131030340982)) ;
#104095 = CARTESIAN_POINT('Ctrl Pts',(-20.7882684765667,-33.943501626556,
122.802987512697)) ;
#104096 = CARTESIAN_POINT('Ctrl Pts',(-20.6197818577463,-33.9568138046492,
122.496403457349)) ;
#104097 = CARTESIAN_POINT('Ctrl Pts',(-20.3152140845606,-33.9733799842425,
122.178400060443)) ;
#104098 = CARTESIAN_POINT('Ctrl Pts',(-19.9192007524352,-33.9900081791027,
121.982335153568)) ;
#104099 = CARTESIAN_POINT('Ctrl Pts',(-19.576747692222,-34.0032967608125,
121.913686472833)) ;
#104100 = CARTESIAN_POINT('Ctrl Pts',(-19.3148922545305,-34.0132650089161,
121.907350759988)) ;
#104101 = CARTESIAN_POINT('Ctrl Pts',(-19.0572295014437,-34.0231797651722,
121.946049655107)) ;
#104102 = CARTESIAN_POINT('Ctrl Pts',(-18.8076465700997,-34.0331929158234,
122.029449840894)) ;
#104103 = CARTESIAN_POINT('Ctrl Pts',(-18.5765650235715,-34.0432056230254,
122.155268181664)) ;
#104104 = CARTESIAN_POINT('Ctrl Pts',(-18.3044971100231,-34.0564249117167,
122.371356277676)) ;
#104105 = CARTESIAN_POINT('Ctrl Pts',(-18.0412576763726,-34.0730435927147,
122.725882225526)) ;
#104106 = CARTESIAN_POINT('Ctrl Pts',(-17.9146105948963,-34.0896085004882,
123.147637150237)) ;
#104107 = CARTESIAN_POINT('Ctrl Pts',(-17.9043687423779,-34.103006972099,
123.499575218403)) ;
#104108 = CARTESIAN_POINT('Ctrl Pts',(-17.9415930567521,-34.112848227586,
123.755521607053)) ;
#104109 = CARTESIAN_POINT('Ctrl Pts',(-18.0233210818594,-34.1228345431742,
124.004856080344)) ;
#104110 = CARTESIAN_POINT('Ctrl Pts',(-18.1464135141684,-34.1327711507606,
124.235196202202)) ;
#104111 = CARTESIAN_POINT('Ctrl Pts',(-18.3095276453939,-34.1428210181289,
124.442869779362)) ;
#104112 = CARTESIAN_POINT('Ctrl Pts',(-18.5022256684344,-34.1526715128037,
124.615746588946)) ;
#104113 = CARTESIAN_POINT('Ctrl Pts',(-18.7243127245786,-34.1626433131982,
124.754775173138)) ;
#104114 = CARTESIAN_POINT('Ctrl Pts',(-18.9678384247013,-34.172639280224,
124.85337105192)) ;
#104115 = CARTESIAN_POINT('Ctrl Pts',(-19.2258575868419,-34.1826767396052,
124.908046464362)) ;
#104116 = CARTESIAN_POINT('Ctrl Pts',(-19.4843104936355,-34.1925174405059,
124.917404320897)) ;
#104117 = CARTESIAN_POINT('Ctrl Pts',(-19.7458819055264,-34.2025654617733,
124.881383594767)) ;
#104118 = CARTESIAN_POINT('Ctrl Pts',(-19.994593911652,-34.212512854856,124.80089995164)) ;
#104119 = CARTESIAN_POINT('Ctrl Pts',(-20.2250703242114,-34.2224230009024,
124.679611870156)) ;
#104120 = CARTESIAN_POINT('Ctrl Pts',(-20.4338613113264,-34.232481914752,
124.517543138453)) ;
#104121 = CARTESIAN_POINT('Ctrl Pts',(-20.6078020302223,-34.2423226850413,
124.32612918028)) ;
#104122 = CARTESIAN_POINT('Ctrl Pts',(-20.7492058428909,-34.2523855546199,
124.10270869485)) ;
#104123 = CARTESIAN_POINT('Ctrl Pts',(-20.847812874156,-34.2622798777504,
123.862089517083)) ;
#104124 = CARTESIAN_POINT('Ctrl Pts',(-20.904086498051,-34.2722216848449,
123.606994705096)) ;
#104125 = CARTESIAN_POINT('Ctrl Pts',(-20.9153820636518,-34.2822241958002,
123.344346331972)) ;
#104126 = CARTESIAN_POINT('Ctrl Pts',(-20.8803877326518,-34.2922589166186,
123.082992800506)) ;
#104127 = CARTESIAN_POINT('Ctrl Pts',(-20.8024516591558,-34.3021040941243,
122.836273538118)) ;
#104128 = CARTESIAN_POINT('Ctrl Pts',(-20.6816477236636,-34.3120888545254,
122.603389496116)) ;
#104129 = CARTESIAN_POINT('Ctrl Pts',(-20.5230276886739,-34.3220277608418,
122.395838571946)) ;
#104130 = CARTESIAN_POINT('Ctrl Pts',(-20.3287681107798,-34.3320699884775,
122.217255861103)) ;
#104131 = CARTESIAN_POINT('Ctrl Pts',(-20.1099811799375,-34.3419552000619,
122.077150319919)) ;
#104132 = CARTESIAN_POINT('Ctrl Pts',(-19.8676254465882,-34.3519541302638,
121.975725272331)) ;
#104133 = CARTESIAN_POINT('Ctrl Pts',(-19.6133933778577,-34.3618715531743,
121.918181079743)) ;
#104134 = CARTESIAN_POINT('Ctrl Pts',(-19.3496858460423,-34.371919485253,
121.905544647266)) ;
#104135 = CARTESIAN_POINT('Ctrl Pts',(-19.0921210729,-34.3817968610624,121.938080116923)) ;
#104136 = CARTESIAN_POINT('Ctrl Pts',(-18.8397327982224,-34.3918507542303,
122.016059532604)) ;
#104137 = CARTESIAN_POINT('Ctrl Pts',(-18.6083220936022,-34.4017443774836,
122.134691793531)) ;
#104138 = CARTESIAN_POINT('Ctrl Pts',(-18.3975365720198,-34.4118069711066,
122.294293213652)) ;
#104139 = CARTESIAN_POINT('Ctrl Pts',(-18.221449334239,-34.4216495450957,
122.48379388163)) ;
#104140 = CARTESIAN_POINT('Ctrl Pts',(-18.0783350961048,-34.4316403019786,
122.703865275403)) ;
#104141 = CARTESIAN_POINT('Ctrl Pts',(-17.9762751140817,-34.4415683637365,
122.943987568166)) ;
#104142 = CARTESIAN_POINT('Ctrl Pts',(-17.9166590105638,-34.4515563396257,
123.199611820243)) ;
#104143 = CARTESIAN_POINT('Ctrl Pts',(-17.9027062380668,-34.4615920039821,
123.462961293951)) ;
#104144 = CARTESIAN_POINT('Ctrl Pts',(-17.933717657988,-34.4714479424018,
123.720115766356)) ;
#104145 = CARTESIAN_POINT('Ctrl Pts',(-18.0095487390398,-34.4814434337987,
123.971573845822)) ;
#104146 = CARTESIAN_POINT('Ctrl Pts',(-18.1268227634101,-34.4913532387521,
124.204107141822)) ;
#104147 = CARTESIAN_POINT('Ctrl Pts',(-18.2839549689648,-34.5013654610189,
124.415151864782)) ;
#104148 = CARTESIAN_POINT('Ctrl Pts',(-18.4759941420734,-34.5113933417117,
124.595612359368)) ;
#104149 = CARTESIAN_POINT('Ctrl Pts',(-18.6924351175168,-34.5212497376943,
124.737885950365)) ;
#104150 = CARTESIAN_POINT('Ctrl Pts',(-18.9341417298191,-34.5312745348743,
124.842676381104)) ;
#104151 = CARTESIAN_POINT('Ctrl Pts',(-19.1906831675197,-34.5413054648581,
124.903315208341)) ;
#104152 = CARTESIAN_POINT('Ctrl Pts',(-19.4489213711089,-34.5511500673668,
124.918671165046)) ;
#104153 = CARTESIAN_POINT('Ctrl Pts',(-19.7098195492988,-34.5611409185909,
124.889221245161)) ;
#104154 = CARTESIAN_POINT('Ctrl Pts',(-19.9626496481009,-34.5711787516021,
124.814004405205)) ;
#104155 = CARTESIAN_POINT('Ctrl Pts',(-20.1942456922768,-34.5810231400675,
124.698703249967)) ;
#104156 = CARTESIAN_POINT('Ctrl Pts',(-20.4055430068826,-34.5910079444371,
124.543191888676)) ;
#104157 = CARTESIAN_POINT('Ctrl Pts',(-20.5859384433338,-34.6009474639199,
124.354242415491)) ;
#104158 = CARTESIAN_POINT('Ctrl Pts',(-20.7321627122965,-34.6109871949213,
124.134661855341)) ;
#104159 = CARTESIAN_POINT('Ctrl Pts',(-20.8365752606534,-34.6208753231676,
123.896695311078)) ;
#104160 = CARTESIAN_POINT('Ctrl Pts',(-20.8991832382357,-34.6308650483761,
123.64176102009)) ;
#104161 = CARTESIAN_POINT('Ctrl Pts',(-20.9163315622063,-34.6408228130776,
123.38064749872)) ;
#104162 = CARTESIAN_POINT('Ctrl Pts',(-20.8886454540213,-34.6507251544896,
123.121892083077)) ;
#104163 = CARTESIAN_POINT('Ctrl Pts',(-20.8153990760022,-34.660769350196,
122.868321304354)) ;
#104164 = CARTESIAN_POINT('Ctrl Pts',(-20.7008328237061,-34.6706767509553,
122.634510958014)) ;
#104165 = CARTESIAN_POINT('Ctrl Pts',(-20.5461918698344,-34.6806873508296,
122.421689518067)) ;
#104166 = CARTESIAN_POINT('Ctrl Pts',(-20.356218405505,-34.6907176467418,
122.238956157989)) ;
#104167 = CARTESIAN_POINT('Ctrl Pts',(-20.1414501229982,-34.7005724263915,
122.094270407089)) ;
#104168 = CARTESIAN_POINT('Ctrl Pts',(-19.9026628587002,-34.710529754609,
121.987240288001)) ;
#104169 = CARTESIAN_POINT('Ctrl Pts',(-19.6467491890605,-34.7205687875159,
121.923231809031)) ;
#104170 = CARTESIAN_POINT('Ctrl Pts',(-19.3879322276226,-34.7304418994052,
121.904452349722)) ;
#104171 = CARTESIAN_POINT('Ctrl Pts',(-19.1246574566547,-34.7405151844323,
121.931502979762)) ;
#104172 = CARTESIAN_POINT('Ctrl Pts',(-18.8762721005754,-34.7503355041691,
122.00174381202)) ;
#104173 = CARTESIAN_POINT('Ctrl Pts',(-18.6377474793643,-34.7604141695475,
122.116725949468)) ;
#104174 = CARTESIAN_POINT('Ctrl Pts',(-18.4274983885584,-34.7702657600313,
122.267892441874)) ;
#104175 = CARTESIAN_POINT('Ctrl Pts',(-18.2425373512532,-34.7803389103502,
122.457196688926)) ;
#104176 = CARTESIAN_POINT('Ctrl Pts',(-18.0966633908561,-34.7901812903253,
122.670815316167)) ;
#104177 = CARTESIAN_POINT('Ctrl Pts',(-17.9878295922109,-34.8001622665683,
122.909438203553)) ;
#104178 = CARTESIAN_POINT('Ctrl Pts',(-17.9222703050761,-34.8101785949236,
123.164375896419)) ;
#104179 = CARTESIAN_POINT('Ctrl Pts',(-17.9018852891634,-34.8200763919147,
123.423670303325)) ;
#104180 = CARTESIAN_POINT('Ctrl Pts',(-17.9266758265072,-34.8300889486468,
123.68563868434)) ;
#104181 = CARTESIAN_POINT('Ctrl Pts',(-17.9973050867461,-34.8401209834933,
123.939619669183)) ;
#104182 = CARTESIAN_POINT('Ctrl Pts',(-18.108211849478,-34.8499603843087,
124.173219295066)) ;
#104183 = CARTESIAN_POINT('Ctrl Pts',(-18.2612467515474,-34.8600261699603,
124.388936498966)) ;
#104184 = CARTESIAN_POINT('Ctrl Pts',(-18.4462622689806,-34.8699166250749,
124.571521646405)) ;
#104185 = CARTESIAN_POINT('Ctrl Pts',(-18.6620141059748,-34.8799087437107,
124.721167028218)) ;
#104186 = CARTESIAN_POINT('Ctrl Pts',(-18.8998816261791,-34.8898715704737,
124.830535614185)) ;
#104187 = CARTESIAN_POINT('Ctrl Pts',(-19.1514976451602,-34.8997758537466,
124.897195876227)) ;
#104188 = CARTESIAN_POINT('Ctrl Pts',(-19.4149200232022,-34.9098362876937,
124.919269231619)) ;
#104189 = CARTESIAN_POINT('Ctrl Pts',(-19.6725159065114,-34.9196768403669,
124.896117457243)) ;
#104190 = CARTESIAN_POINT('Ctrl Pts',(-19.9278288963677,-34.9297390603126,
124.82741158987)) ;
#104191 = CARTESIAN_POINT('Ctrl Pts',(-20.1633279388494,-34.9396361995912,
124.71699231362)) ;
#104192 = CARTESIAN_POINT('Ctrl Pts',(-20.3772931771489,-34.9495673917262,
124.567567370087)) ;
#104193 = CARTESIAN_POINT('Ctrl Pts',(-20.5639178571973,-34.9596095463713,
124.380994866377)) ;
#104194 = CARTESIAN_POINT('Ctrl Pts',(-20.7131614275899,-34.9694963073906,
124.16829573498)) ;
#104195 = CARTESIAN_POINT('Ctrl Pts',(-20.8247390624128,-34.9794956091078,
123.930428506013)) ;
#104196 = CARTESIAN_POINT('Ctrl Pts',(-20.8929709285114,-34.9894164072746,
123.678769811225)) ;
#104197 = CARTESIAN_POINT('Ctrl Pts',(-20.9167602208572,-34.9994504608713,
123.416190287807)) ;
#104198 = CARTESIAN_POINT('Ctrl Pts',(-20.894992050459,-35.0093735784377,
123.156290901073)) ;
#104199 = CARTESIAN_POINT('Ctrl Pts',(-20.8274967913366,-35.0194297019368,
122.900819039929)) ;
#104200 = CARTESIAN_POINT('Ctrl Pts',(-20.7190767997193,-35.0292751435917,
122.665891135999)) ;
#104201 = CARTESIAN_POINT('Ctrl Pts',(-20.570484633187,-35.0392374447158,
122.450367538193)) ;
#104202 = CARTESIAN_POINT('Ctrl Pts',(-20.385235603018,-35.0492659239909,
122.262899380844)) ;
#104203 = CARTESIAN_POINT('Ctrl Pts',(-20.1728579932209,-35.0591762775006,
122.112184527522)) ;
#104204 = CARTESIAN_POINT('Ctrl Pts',(-19.9372295987882,-35.0691111496778,
121.99973320743)) ;
#104205 = CARTESIAN_POINT('Ctrl Pts',(-19.6829151498438,-35.0791522872635,
121.929396810072)) ;
#104206 = CARTESIAN_POINT('Ctrl Pts',(-19.4242729791093,-35.0890394364781,
121.904487487386)) ;
#104207 = CARTESIAN_POINT('Ctrl Pts',(-19.1624800113372,-35.0990316712291,
121.924641589573)) ;
#104208 = CARTESIAN_POINT('Ctrl Pts',(-18.9092594100541,-35.1089803767921,
121.989743199417)) ;
#104209 = CARTESIAN_POINT('Ctrl Pts',(-18.6713636061917,-35.1189164452158,
122.097326151971)) ;
#104210 = CARTESIAN_POINT('Ctrl Pts',(-18.454478724191,-35.1289021294316,
122.24509401698)) ;
#104211 = CARTESIAN_POINT('Ctrl Pts',(-18.2658365440842,-35.1389425560002,
122.429551256226)) ;
#104212 = CARTESIAN_POINT('Ctrl Pts',(-18.1148079749497,-35.148781669464,
122.639425740109)) ;
#104213 = CARTESIAN_POINT('Ctrl Pts',(-17.9998053864142,-35.1588114036398,
122.8765872657)) ;
#104214 = CARTESIAN_POINT('Ctrl Pts',(-17.928444715581,-35.1688335031457,
123.130103094815)) ;
#104215 = CARTESIAN_POINT('Ctrl Pts',(-17.9019396037341,-35.1787019430391,
123.388097438941)) ;
#104216 = CARTESIAN_POINT('Ctrl Pts',(-17.9210166574151,-35.1887708077248,
123.651983894416)) ;
#104217 = CARTESIAN_POINT('Ctrl Pts',(-17.984171428927,-35.1986134808234,
123.902820263154)) ;
#104218 = CARTESIAN_POINT('Ctrl Pts',(-18.0903067406265,-35.2085741149858,
124.142086367296)) ;
#104219 = CARTESIAN_POINT('Ctrl Pts',(-18.2379359596469,-35.2186120306639,
124.360681074975)) ;
#104220 = CARTESIAN_POINT('Ctrl Pts',(-18.4179730017366,-35.2284863055234,
124.547593591424)) ;
#104221 = CARTESIAN_POINT('Ctrl Pts',(-18.6318350939192,-35.2385560558985,
124.703379138659)) ;
#104222 = CARTESIAN_POINT('Ctrl Pts',(-18.8639071984874,-35.248389351273,
124.817084015315)) ;
#104223 = CARTESIAN_POINT('Ctrl Pts',(-19.11693425595,-35.2584196487526,124.890913312346)) ;
#104224 = CARTESIAN_POINT('Ctrl Pts',(-19.3790865211221,-35.2684517351941,
124.918922276281)) ;
#104225 = CARTESIAN_POINT('Ctrl Pts',(-19.6367832596118,-35.278279663683,
124.901921160071)) ;
#104226 = CARTESIAN_POINT('Ctrl Pts',(-19.8920793713658,-35.2882757047938,
124.840064446587)) ;
#104227 = CARTESIAN_POINT('Ctrl Pts',(-20.1332785051419,-35.298301516895,
124.734035625676)) ;
#104228 = CARTESIAN_POINT('Ctrl Pts',(-20.3495593000044,-35.3081887517898,
124.590041155415)) ;
#104229 = CARTESIAN_POINT('Ctrl Pts',(-20.5395393226793,-35.3181656180008,
124.409385624439)) ;
#104230 = CARTESIAN_POINT('Ctrl Pts',(-20.6955864544945,-35.3281585618726,
124.198129769349)) ;
#104231 = CARTESIAN_POINT('Ctrl Pts',(-20.8127836789868,-35.338196484544,
123.96183104994)) ;
#104232 = CARTESIAN_POINT('Ctrl Pts',(-20.8861530777465,-35.3480449488057,
123.713620356544)) ;
#104233 = CARTESIAN_POINT('Ctrl Pts',(-20.9161936009875,-35.3580368155497,
123.45280719969)) ;
#104234 = CARTESIAN_POINT('Ctrl Pts',(-20.9007516754071,-35.3679545475909,
123.192603234289)) ;
#104235 = CARTESIAN_POINT('Ctrl Pts',(-20.8397730358761,-35.3779827324862,
122.936247392291)) ;
#104236 = CARTESIAN_POINT('Ctrl Pts',(-20.7367882330966,-35.387867890535,
122.6977541823)) ;
#104237 = CARTESIAN_POINT('Ctrl Pts',(-20.5929867212805,-35.3978572510767,
122.478128741953)) ;
#104238 = CARTESIAN_POINT('Ctrl Pts',(-20.41190098255,-35.4078984080111,122.286202465482)) ;
#104239 = CARTESIAN_POINT('Ctrl Pts',(-20.204896171008,-35.4177309914662,
122.131565664669)) ;
#104240 = CARTESIAN_POINT('Ctrl Pts',(-19.9707294456194,-35.4277252114282,
122.012642748326)) ;
#104241 = CARTESIAN_POINT('Ctrl Pts',(-19.7184528815529,-35.4377533132155,
121.936438351148)) ;
#104242 = CARTESIAN_POINT('Ctrl Pts',(-19.4606890511142,-35.4476332578386,
121.905289560067)) ;
#104243 = CARTESIAN_POINT('Ctrl Pts',(-19.1985341207604,-35.4576235843956,
121.919121980411)) ;
#104244 = CARTESIAN_POINT('Ctrl Pts',(-18.9440062626121,-35.4675645160499,
121.977973922439)) ;
#104245 = CARTESIAN_POINT('Ctrl Pts',(-18.702288047515,-35.4775516345528,
122.080260803996)) ;
#104246 = CARTESIAN_POINT('Ctrl Pts',(-18.4812400627169,-35.48758496745,122.22395297179)) ;
#104247 = CARTESIAN_POINT('Ctrl Pts',(-18.2913303413505,-35.4974510718947,
122.400506732355)) ;
#104248 = CARTESIAN_POINT('Ctrl Pts',(-18.1317782703175,-35.5075171857751,
122.611460438523)) ;
#104249 = CARTESIAN_POINT('Ctrl Pts',(-18.0137583413935,-35.5173731975435,
122.842035312612)) ;
#104250 = CARTESIAN_POINT('Ctrl Pts',(-17.9357612978985,-35.5273679011748,
123.092829842602)) ;
#104251 = CARTESIAN_POINT('Ctrl Pts',(-17.9029316319615,-35.5373992368997,
123.354395189712)) ;
#104252 = CARTESIAN_POINT('Ctrl Pts',(-17.9153901928163,-35.5472657621033,
123.613386874804)) ;
#104253 = CARTESIAN_POINT('Ctrl Pts',(-17.9729086714527,-35.5572531901491,
123.869433841305)) ;
#104254 = CARTESIAN_POINT('Ctrl Pts',(-18.0734780654367,-35.5671981198355,
124.110692535374)) ;
#104255 = CARTESIAN_POINT('Ctrl Pts',(-18.2159187908367,-35.5772430379441,
124.332902903788)) ;
#104256 = CARTESIAN_POINT('Ctrl Pts',(-18.3913816758931,-35.587105007558,
124.523661515827)) ;
#104257 = CARTESIAN_POINT('Ctrl Pts',(-18.5996689527745,-35.5970970755792,
124.683509885584)) ;
#104258 = CARTESIAN_POINT('Ctrl Pts',(-18.8311813513176,-35.6070280009538,
124.804001201604)) ;
#104259 = CARTESIAN_POINT('Ctrl Pts',(-19.0804266703559,-35.6169786291772,
124.883027052009)) ;
#104260 = CARTESIAN_POINT('Ctrl Pts',(-19.3409266350383,-35.6269788682363,
124.917904087463)) ;
#104261 = CARTESIAN_POINT('Ctrl Pts',(-19.6042114461551,-35.6370073236055,
124.906610760373)) ;
#104262 = CARTESIAN_POINT('Ctrl Pts',(-19.8574743469857,-35.6468733581888,
124.851072017746)) ;
#104263 = CARTESIAN_POINT('Ctrl Pts',(-20.1004455793922,-35.6568656799362,
124.751552866436)) ;
#104264 = CARTESIAN_POINT('Ctrl Pts',(-20.3211734802122,-35.6667979696132,
124.612212133575)) ;
#104265 = CARTESIAN_POINT('Ctrl Pts',(-20.5158560562824,-35.676799614584,
124.435643769386)) ;
#104266 = CARTESIAN_POINT('Ctrl Pts',(-20.7301399819969,-35.690112248,124.159089650513)) ;
#104267 = CARTESIAN_POINT('Ctrl Pts',(-20.8667522508955,-35.7033439973816,
123.835042103651)) ;
#104268 = CARTESIAN_POINT('Ctrl Pts',(-20.9147585986983,-35.7166672621986,
123.488226045327)) ;
#104269 = CARTESIAN_POINT('Ctrl Pts',(-20.9055563612278,-35.7265429684163,
123.228855650435)) ;
#104270 = CARTESIAN_POINT('Ctrl Pts',(-20.8511781735933,-35.7365325595163,
122.972062262268)) ;
#104271 = CARTESIAN_POINT('Ctrl Pts',(-20.7537899401684,-35.7464596559717,
122.730015204372)) ;
#104272 = CARTESIAN_POINT('Ctrl Pts',(-20.6145469935305,-35.7564848044763,
122.5063968681)) ;
#104273 = CARTESIAN_POINT('Ctrl Pts',(-20.440953874785,-35.766380458623,122.312743006268)) ;
#104274 = CARTESIAN_POINT('Ctrl Pts',(-20.2344106821349,-35.7763839930012,
122.150158260611)) ;
#104275 = CARTESIAN_POINT('Ctrl Pts',(-20.0031308315218,-35.7863691314413,
122.026126833219)) ;
#104276 = CARTESIAN_POINT('Ctrl Pts',(-19.7525288450674,-35.7964050560366,
121.943988637764)) ;
#104277 = CARTESIAN_POINT('Ctrl Pts',(-19.4963068640577,-35.8062563314643,
121.906992639844)) ;
#104278 = CARTESIAN_POINT('Ctrl Pts',(-19.2338168958201,-35.8162485926257,
121.914412989473)) ;
#104279 = CARTESIAN_POINT('Ctrl Pts',(-18.9755341093132,-35.8262884766433,
121.968199019845)) ;
#104280 = CARTESIAN_POINT('Ctrl Pts',(-18.7352349967454,-35.8361232511457,
122.063423387653)) ;
#104281 = CARTESIAN_POINT('Ctrl Pts',(-18.5097250642947,-35.846199632166,
122.202132211928)) ;
#104282 = CARTESIAN_POINT('Ctrl Pts',(-18.3161426476442,-35.8560459053166,
122.373872640162)) ;
#104283 = CARTESIAN_POINT('Ctrl Pts',(-18.0973698099313,-35.8694104266019,
122.648612771073)) ;
#104284 = CARTESIAN_POINT('Ctrl Pts',(-17.9574290045863,-35.8826166710363,
122.970502256562)) ;
#104285 = CARTESIAN_POINT('Ctrl Pts',(-17.9048223282448,-35.8958816257135,
123.315086227926)) ;
#104286 = CARTESIAN_POINT('Ctrl Pts',(-17.9110124910834,-35.9059139062652,
123.578657913582)) ;
#104287 = CARTESIAN_POINT('Ctrl Pts',(-17.9622121074336,-35.9158226397831,
123.833960372486)) ;
#104288 = CARTESIAN_POINT('Ctrl Pts',(-18.0566097123555,-35.9257601906506,
124.077460099996)) ;
#104289 = CARTESIAN_POINT('Ctrl Pts',(-18.1932802459593,-35.9357900382445,
124.302802968924)) ;
#104290 = CARTESIAN_POINT('Ctrl Pts',(-18.4222315307494,-35.949025178165,
124.564734759773)) ;
#104291 = CARTESIAN_POINT('Ctrl Pts',(-18.7900589109443,-35.9656936425361,
124.81140834834)) ;
#104292 = CARTESIAN_POINT('Ctrl Pts',(-19.3028156410116,-35.98556465441,124.938691204447)) ;
#104293 = CARTESIAN_POINT('Ctrl Pts',(-19.7442837615988,-36.002271738793,
124.892072174902)) ;
#104294 = CARTESIAN_POINT('Ctrl Pts',(-20.0675701271114,-36.0154490201036,
124.767809053067)) ;
#104295 = CARTESIAN_POINT('Ctrl Pts',(-20.3669739906252,-36.0287164806177,
124.589185848761)) ;
#104296 = CARTESIAN_POINT('Ctrl Pts',(-20.6747981802351,-36.0453303713049,
124.272594034034)) ;
#104297 = CARTESIAN_POINT('Ctrl Pts',(-20.8925558078183,-36.0652791707323,
123.789111611109)) ;
#104298 = CARTESIAN_POINT('Ctrl Pts',(-20.9320991006498,-36.0852002822632,
123.261193418432)) ;
#104299 = CARTESIAN_POINT('Ctrl Pts',(-20.7905276952024,-36.1050667304361,
122.752423768458)) ;
#104300 = CARTESIAN_POINT('Ctrl Pts',(-20.4811904266978,-36.1250930770532,
122.319344712288)) ;
#104301 = CARTESIAN_POINT('Ctrl Pts',(-20.0460525668454,-36.1449551214427,
122.020296381209)) ;
#104302 = CARTESIAN_POINT('Ctrl Pts',(-19.5332139354113,-36.1649004241238,
121.886365238136)) ;
#104303 = CARTESIAN_POINT('Ctrl Pts',(-19.0067003117622,-36.1847957311827,
121.935446627592)) ;
#104304 = CARTESIAN_POINT('Ctrl Pts',(-18.528185304181,-36.2046890013503,
122.160367750237)) ;
#104305 = CARTESIAN_POINT('Ctrl Pts',(-18.153899886363,-36.2246545940308,
122.536490933432)) ;
#104306 = CARTESIAN_POINT('Ctrl Pts',(-17.9310800836286,-36.2445299177156,
123.015484089359)) ;
#104307 = CARTESIAN_POINT('Ctrl Pts',(-17.8843234008794,-36.2645049802905,
123.544349544099)) ;
#104308 = CARTESIAN_POINT('Ctrl Pts',(-18.0214642489446,-36.2844573899217,
124.056610899457)) ;
#104309 = CARTESIAN_POINT('Ctrl Pts',(-18.3225697130406,-36.3042934441578,
124.489372589314)) ;
#104310 = CARTESIAN_POINT('Ctrl Pts',(-18.7560217521226,-36.3242713555753,
124.796062315731)) ;
#104311 = CARTESIAN_POINT('Ctrl Pts',(-19.2667087137698,-36.3441894050788,
124.935393803099)) ;
#104312 = CARTESIAN_POINT('Ctrl Pts',(-19.7932215456907,-36.3640575488469,
124.893573225547)) ;
#104313 = CARTESIAN_POINT('Ctrl Pts',(-20.2777203069031,-36.3841084054342,
124.671934669039)) ;
#104314 = CARTESIAN_POINT('Ctrl Pts',(-20.6529715193524,-36.4038888418901,
124.303513156347)) ;
#104315 = CARTESIAN_POINT('Ctrl Pts',(-20.8834919669097,-36.4239188975679,
123.823777378833)) ;
#104316 = CARTESIAN_POINT('Ctrl Pts',(-20.9351946084238,-36.4438000027427,
123.297815458133)) ;
#104317 = CARTESIAN_POINT('Ctrl Pts',(-20.805795972203,-36.4636804651105,
122.785569836397)) ;
#104318 = CARTESIAN_POINT('Ctrl Pts',(-20.5076408598673,-36.4836656122549,
122.345949379548)) ;
#104319 = CARTESIAN_POINT('Ctrl Pts',(-20.0793293333916,-36.5035561907912,
122.036043896619)) ;
#104320 = CARTESIAN_POINT('Ctrl Pts',(-19.5711616761895,-36.5234502106656,
121.889982105805)) ;
#104321 = CARTESIAN_POINT('Ctrl Pts',(-19.0429949662243,-36.543371655392,
121.926004249393)) ;
#104322 = CARTESIAN_POINT('Ctrl Pts',(-18.5587989821738,-36.5632697934474,
122.139082068904)) ;
#104323 = CARTESIAN_POINT('Ctrl Pts',(-18.1739452502748,-36.5833405486635,
122.508343006404)) ;
#104324 = CARTESIAN_POINT('Ctrl Pts',(-17.9412347696197,-36.6031260987147,
122.980047031886)) ;
#104325 = CARTESIAN_POINT('Ctrl Pts',(-17.8816250601364,-36.6231091735921,
123.507711042693)) ;
#104326 = CARTESIAN_POINT('Ctrl Pts',(-18.0060238701936,-36.643018256238,
124.02203763036)) ;
#104327 = CARTESIAN_POINT('Ctrl Pts',(-18.2964921624861,-36.6628768153608,
124.46281239647)) ;
#104328 = CARTESIAN_POINT('Ctrl Pts',(-18.7241093152604,-36.6829202591995,
124.780336057724)) ;
#104329 = CARTESIAN_POINT('Ctrl Pts',(-19.1443370740696,-36.6994203239287,
124.906201446965)) ;
#104330 = CARTESIAN_POINT('Ctrl Pts',(-19.4959912524148,-36.7128100637776,
124.916825364665)) ;
#104331 = CARTESIAN_POINT('Ctrl Pts',(-19.7523753879943,-36.722666964986,
124.879659208056)) ;
#104332 = CARTESIAN_POINT('Ctrl Pts',(-20.0018654730257,-36.7326584908325,
124.797967905292)) ;
#104333 = CARTESIAN_POINT('Ctrl Pts',(-20.2319502039447,-36.7425831712835,
124.675071044301)) ;
#104334 = CARTESIAN_POINT('Ctrl Pts',(-20.4389774416339,-36.7525937613279,
124.512826396115)) ;
#104335 = CARTESIAN_POINT('Ctrl Pts',(-20.6721055369594,-36.7658530220315,
124.253740187377)) ;
#104336 = CARTESIAN_POINT('Ctrl Pts',(-20.8329407184448,-36.7792040971818,
123.937561551758)) ;
#104337 = CARTESIAN_POINT('Ctrl Pts',(-20.9051385764094,-36.7924104064166,
123.598034123751)) ;
#104338 = CARTESIAN_POINT('Ctrl Pts',(-20.9148485286139,-36.8023972400069,
123.335815354596)) ;
#104339 = CARTESIAN_POINT('Ctrl Pts',(-20.8791206018551,-36.812349967503,
123.076674163905)) ;
#104340 = CARTESIAN_POINT('Ctrl Pts',(-20.7979834514624,-36.8223980643446,
122.82542587721)) ;
#104341 = CARTESIAN_POINT('Ctrl Pts',(-20.6772389440555,-36.8322395212164,
122.596690972918)) ;
#104342 = CARTESIAN_POINT('Ctrl Pts',(-20.5167636139699,-36.8422257881299,
122.389100234004)) ;
#104343 = CARTESIAN_POINT('Ctrl Pts',(-20.3236708136036,-36.8521623890303,
122.213249918781)) ;
#104344 = CARTESIAN_POINT('Ctrl Pts',(-20.1004488354142,-36.8622123318174,
122.072155044208)) ;
#104345 = CARTESIAN_POINT('Ctrl Pts',(-19.8610080268969,-36.8720625315031,
121.973756839385)) ;
#104346 = CARTESIAN_POINT('Ctrl Pts',(-19.6051634992664,-36.8820354364352,
121.917073652596)) ;
#104347 = CARTESIAN_POINT('Ctrl Pts',(-19.3426292753776,-36.8920338109148,
121.905727253449)) ;
#104348 = CARTESIAN_POINT('Ctrl Pts',(-19.0816097097037,-36.9020539847848,
121.940395605371)) ;
#104349 = CARTESIAN_POINT('Ctrl Pts',(-18.8334770246781,-36.9119550287268,
122.018703957336)) ;
#104350 = CARTESIAN_POINT('Ctrl Pts',(-18.6004816712349,-36.9219438324511,
122.139601545774)) ;
#104351 = CARTESIAN_POINT('Ctrl Pts',(-18.3926262261631,-36.9319092992829,
122.298887280516)) ;
#104352 = CARTESIAN_POINT('Ctrl Pts',(-18.2161960419998,-36.9418128615559,
122.490246883237)) ;
#104353 = CARTESIAN_POINT('Ctrl Pts',(-18.0736583691123,-36.9518735394339,
122.71287674179)) ;
#104354 = CARTESIAN_POINT('Ctrl Pts',(-17.9738349551272,-36.9617138373834,
122.951466470919)) ;
#104355 = CARTESIAN_POINT('Ctrl Pts',(-17.9153712422102,-36.9717768322928,
123.209332478486)) ;
#104356 = CARTESIAN_POINT('Ctrl Pts',(-17.9029963259701,-36.9816711264399,
123.469077685749)) ;
#104357 = CARTESIAN_POINT('Ctrl Pts',(-17.9353566103363,-36.9916129241368,
123.728293552518)) ;
#104358 = CARTESIAN_POINT('Ctrl Pts',(-18.0126312483315,-37.0016155016659,
123.979571905711)) ;
#104359 = CARTESIAN_POINT('Ctrl Pts',(-18.1330836135204,-37.011649965587,
124.214133981755)) ;
#104360 = CARTESIAN_POINT('Ctrl Pts',(-18.2891332508582,-37.0214961041081,
124.420537477893)) ;
#104361 = CARTESIAN_POINT('Ctrl Pts',(-18.4808302087652,-37.0314772773451,
124.599534219672)) ;
#104362 = CARTESIAN_POINT('Ctrl Pts',(-18.7001169445162,-37.0414295713023,
124.742077120558)) ;
#104363 = CARTESIAN_POINT('Ctrl Pts',(-18.9418253000939,-37.0514283664369,
124.845176341214)) ;
#104364 = CARTESIAN_POINT('Ctrl Pts',(-19.1988750598665,-37.0614674746977,
124.904479146326)) ;
#104365 = CARTESIAN_POINT('Ctrl Pts',(-19.4566988811573,-37.0712924161369,
124.918510704658)) ;
#104366 = CARTESIAN_POINT('Ctrl Pts',(-19.7190563874513,-37.0813471032113,
124.887274074788)) ;
#104367 = CARTESIAN_POINT('Ctrl Pts',(-19.969084030359,-37.0912899081514,
124.811372573199)) ;
#104368 = CARTESIAN_POINT('Ctrl Pts',(-20.2015786291338,-37.1011936941479,
124.694388313774)) ;
#104369 = CARTESIAN_POINT('Ctrl Pts',(-20.4131234868588,-37.1112405107127,
124.536454481788)) ;
#104370 = CARTESIAN_POINT('Ctrl Pts',(-20.5915236174634,-37.1211360301914,
124.347197240255)) ;
#104371 = CARTESIAN_POINT('Ctrl Pts',(-20.7367129157612,-37.1311981155158,
124.126248181755)) ;
#104372 = CARTESIAN_POINT('Ctrl Pts',(-20.8392138555914,-37.1410408264737,
123.888736566478)) ;
#104373 = CARTESIAN_POINT('Ctrl Pts',(-20.9004065395447,-37.1510315437798,
123.633455653351)) ;
#104374 = CARTESIAN_POINT('Ctrl Pts',(-20.9162024817298,-37.1609596268764,
123.373022214613)) ;
#104375 = CARTESIAN_POINT('Ctrl Pts',(-20.8868147103716,-37.1709475569881,
123.112189441755)) ;
#104376 = CARTESIAN_POINT('Ctrl Pts',(-20.8118080923206,-37.1809833831154,
122.859358313321)) ;
#104377 = CARTESIAN_POINT('Ctrl Pts',(-20.6965192508004,-37.190838720229,
122.627429700826)) ;
#104378 = CARTESIAN_POINT('Ctrl Pts',(-20.5408489070488,-37.2008364550792,
122.415819448535)) ;
#104379 = CARTESIAN_POINT('Ctrl Pts',(-20.3525399698651,-37.2107443590637,
122.235991135141)) ;
#104380 = CARTESIAN_POINT('Ctrl Pts',(-20.1338594498065,-37.2207554336121,
122.08972321814)) ;
#104381 = CARTESIAN_POINT('Ctrl Pts',(-19.8924886139935,-37.2307832891477,
121.98396490072)) ;
#104382 = CARTESIAN_POINT('Ctrl Pts',(-19.640883973354,-37.240640883053,121.922329058917)) ;
#104383 = CARTESIAN_POINT('Ctrl Pts',(-19.3779934736836,-37.2506675698911,
121.904487880375)) ;
#104384 = CARTESIAN_POINT('Ctrl Pts',(-19.1160127976239,-37.2606962390448,
121.933223522823)) ;
#104385 = CARTESIAN_POINT('Ctrl Pts',(-18.8675153981344,-37.2705414473262,
122.00519292378)) ;
#104386 = CARTESIAN_POINT('Ctrl Pts',(-18.6315296424855,-37.2805321362893,
122.120275185745)) ;
#104387 = CARTESIAN_POINT('Ctrl Pts',(-18.4184607715103,-37.2905700125716,
122.275783232046)) ;
#104388 = CARTESIAN_POINT('Ctrl Pts',(-18.2388199959597,-37.3004143902138,
122.46195567079)) ;
#104389 = CARTESIAN_POINT('Ctrl Pts',(-18.0917661888766,-37.3103991946052,
122.67922397644)) ;
#104390 = CARTESIAN_POINT('Ctrl Pts',(-17.9850247084905,-37.3203387248238,
122.917657976795)) ;
#104391 = CARTESIAN_POINT('Ctrl Pts',(-17.9207357281408,-37.3303784128607,
123.173516578115)) ;
#104392 = CARTESIAN_POINT('Ctrl Pts',(-17.9020031979114,-37.340266702229,
123.432709689292)) ;
#104393 = CARTESIAN_POINT('Ctrl Pts',(-17.9283346512609,-37.3502558259138,
123.693880259981)) ;
#104394 = CARTESIAN_POINT('Ctrl Pts',(-17.9996040811772,-37.3602158355884,
123.945724561577)) ;
#104395 = CARTESIAN_POINT('Ctrl Pts',(-18.1122851368062,-37.3701162652927,
124.180239595587)) ;
#104396 = CARTESIAN_POINT('Ctrl Pts',(-18.2661582318279,-37.3801593466994,
124.394649731977)) ;
#104397 = CARTESIAN_POINT('Ctrl Pts',(-18.4523869695707,-37.390066740607,
124.576615327164)) ;
#104398 = CARTESIAN_POINT('Ctrl Pts',(-18.6693614592825,-37.4000784715962,
124.725422533845)) ;
#104399 = CARTESIAN_POINT('Ctrl Pts',(-18.9095896394235,-37.410110689311,
124.834045138727)) ;
#104400 = CARTESIAN_POINT('Ctrl Pts',(-19.1603449861125,-37.4199631985572,
124.898470131179)) ;
#104401 = CARTESIAN_POINT('Ctrl Pts',(-19.4211984555545,-37.4299211351002,
124.919402923825)) ;
#104402 = CARTESIAN_POINT('Ctrl Pts',(-19.6837710962987,-37.4399600051085,
124.894054750711)) ;
#104403 = CARTESIAN_POINT('Ctrl Pts',(-19.9339449292123,-37.4498331602667,
124.825117088921)) ;
#104404 = CARTESIAN_POINT('Ctrl Pts',(-20.1729772826254,-37.4599064351164,
124.711500299774)) ;
#104405 = CARTESIAN_POINT('Ctrl Pts',(-20.3835223993662,-37.4697267522938,
124.562169109503)) ;
#104406 = CARTESIAN_POINT('Ctrl Pts',(-20.5697990348495,-37.4798054380873,
124.373977558108)) ;
#104407 = CARTESIAN_POINT('Ctrl Pts',(-20.7173197608685,-37.4896569494704,
124.16115630228)) ;
#104408 = CARTESIAN_POINT('Ctrl Pts',(-20.8282432976094,-37.499730395777,
123.920852463059)) ;
#104409 = CARTESIAN_POINT('Ctrl Pts',(-20.8942031840611,-37.5095716709017,
123.670756297551)) ;
#104410 = CARTESIAN_POINT('Ctrl Pts',(-20.9168622044648,-37.5195567705585,
123.409363382907)) ;
#104411 = CARTESIAN_POINT('Ctrl Pts',(-20.8933700263742,-37.5295642466928,
123.147408998468)) ;
#104412 = CARTESIAN_POINT('Ctrl Pts',(-20.8255717865833,-37.5394868344017,
122.895635106772)) ;
#104413 = CARTESIAN_POINT('Ctrl Pts',(-20.7147447437026,-37.5494734386751,
122.657720062072)) ;
#104414 = CARTESIAN_POINT('Ctrl Pts',(-20.5631062336304,-37.5595135670092,
122.441830793233)) ;
#104415 = CARTESIAN_POINT('Ctrl Pts',(-20.3803844725439,-37.5693530015426,
122.258841212078)) ;
#104416 = CARTESIAN_POINT('Ctrl Pts',(-20.1640074372698,-37.5794170560336,
122.106822876259)) ;
#104417 = CARTESIAN_POINT('Ctrl Pts',(-19.9285377911858,-37.5893079752708,
121.996693203954)) ;
#104418 = CARTESIAN_POINT('Ctrl Pts',(-19.6751435403959,-37.5992999685768,
121.927901435656)) ;
#104419 = CARTESIAN_POINT('Ctrl Pts',(-19.4143879012816,-37.6092628325361,
121.904463322897)) ;
#104420 = CARTESIAN_POINT('Ctrl Pts',(-19.1549736893451,-37.6191670923539,
121.925872135699)) ;
#104421 = CARTESIAN_POINT('Ctrl Pts',(-18.8993583114686,-37.6292275829253,
121.993249334213)) ;
#104422 = CARTESIAN_POINT('Ctrl Pts',(-18.6643727563373,-37.6390679325563,
122.101285905373)) ;
#104423 = CARTESIAN_POINT('Ctrl Pts',(-18.4467827532205,-37.6491309080463,
122.251509215231)) ;
#104424 = CARTESIAN_POINT('Ctrl Pts',(-18.2618415785691,-37.6590252281897,
122.434315181423)) ;
#104425 = CARTESIAN_POINT('Ctrl Pts',(-18.1101921979794,-37.6689669413213,
122.647012356503)) ;
#104426 = CARTESIAN_POINT('Ctrl Pts',(-17.9969505425752,-37.6789698311154,
122.884279729018)) ;
#104427 = CARTESIAN_POINT('Ctrl Pts',(-17.9268499593331,-37.6890096882759,
123.138607114906)) ;
#104428 = CARTESIAN_POINT('Ctrl Pts',(-17.9019179207587,-37.6988338691135,
123.395591251844)) ;
#104429 = CARTESIAN_POINT('Ctrl Pts',(-17.9220940157087,-37.7088908426167,
123.659084863121)) ;
#104430 = CARTESIAN_POINT('Ctrl Pts',(-17.9872042427552,-37.7188189668038,
123.911746027591)) ;
#104431 = CARTESIAN_POINT('Ctrl Pts',(-18.0948316129578,-37.7287726618772,
124.1501526263)) ;
#104432 = CARTESIAN_POINT('Ctrl Pts',(-18.2438973494036,-37.7388188554525,
124.368042069497)) ;
#104433 = CARTESIAN_POINT('Ctrl Pts',(-18.4247143523808,-37.7486669578124,
124.55319376787)) ;
#104434 = CARTESIAN_POINT('Ctrl Pts',(-18.6368737321832,-37.75862854604,124.706527900158)) ;
#104435 = CARTESIAN_POINT('Ctrl Pts',(-18.8741889123257,-37.7686572161963,
124.82117776678)) ;
#104436 = CARTESIAN_POINT('Ctrl Pts',(-19.1247639980567,-37.778567519078,
124.892107534021)) ;
#104437 = CARTESIAN_POINT('Ctrl Pts',(-19.3844408619282,-37.7885024028859,
124.919199981509)) ;
#104438 = CARTESIAN_POINT('Ctrl Pts',(-19.6476287569967,-37.7985435445765,
124.900351524568)) ;
#104439 = CARTESIAN_POINT('Ctrl Pts',(-19.8996880891423,-37.8084306657405,
124.837248718803)) ;
#104440 = CARTESIAN_POINT('Ctrl Pts',(-20.1396351561268,-37.818423008589,
124.730624721644)) ;
#104441 = CARTESIAN_POINT('Ctrl Pts',(-20.3564483081695,-37.828371309813,
124.584525305613)) ;
#104442 = CARTESIAN_POINT('Ctrl Pts',(-20.5446407648115,-37.8383088874951,
124.403488389917)) ;
#104443 = CARTESIAN_POINT('Ctrl Pts',(-20.6995353445836,-37.8482954619457,
124.19161538296)) ;
#104444 = CARTESIAN_POINT('Ctrl Pts',(-20.8154970734678,-37.8583242718541,
123.954954138649)) ;
#104445 = CARTESIAN_POINT('Ctrl Pts',(-20.8877508953249,-37.8682025931609,
123.705622620261)) ;
#104446 = CARTESIAN_POINT('Ctrl Pts',(-20.9165491642619,-37.8781942405083,
123.444627694951)) ;
#104447 = CARTESIAN_POINT('Ctrl Pts',(-20.8989830904194,-37.8882287639461,
123.181528801038)) ;
#104448 = CARTESIAN_POINT('Ctrl Pts',(-20.8375900725936,-37.8980921208247,
122.929677120428)) ;
#104449 = CARTESIAN_POINT('Ctrl Pts',(-20.7312850440034,-37.908162347505,
122.687363711049)) ;
#104450 = CARTESIAN_POINT('Ctrl Pts',(-20.5878097989603,-37.9180046556397,
122.472146620804)) ;
#104451 = CARTESIAN_POINT('Ctrl Pts',(-20.4077072811251,-37.9279653876631,
122.282207293624)) ;
#104452 = CARTESIAN_POINT('Ctrl Pts',(-20.1954236191509,-37.9380032768612,
122.125639435878)) ;
#104453 = CARTESIAN_POINT('Ctrl Pts',(-19.9632067506179,-37.94787755978,122.009773260868)) ;
#104454 = CARTESIAN_POINT('Ctrl Pts',(-19.7095351983791,-37.9579473043975,
121.934560773782)) ;
#104455 = CARTESIAN_POINT('Ctrl Pts',(-19.4527900585432,-37.9677806147431,
121.905097719252)) ;
#104456 = CARTESIAN_POINT('Ctrl Pts',(-19.1896456423422,-37.9778108580958,
121.920221120939)) ;
#104457 = CARTESIAN_POINT('Ctrl Pts',(-18.9332428132667,-37.9878431460742,
121.981587866224)) ;
#104458 = CARTESIAN_POINT('Ctrl Pts',(-18.6960940925784,-37.9976703225423,
122.083833011387)) ;
#104459 = CARTESIAN_POINT('Ctrl Pts',(-18.4761183695582,-38.0076757054092,
122.227800110012)) ;
#104460 = CARTESIAN_POINT('Ctrl Pts',(-18.2849162844405,-38.0176583444019,
122.40748589956)) ;
#104461 = CARTESIAN_POINT('Ctrl Pts',(-18.12715679948,-38.0277024115385,122.619066068581)) ;
#104462 = CARTESIAN_POINT('Ctrl Pts',(-18.0107464436038,-38.0375236303425,
122.849423615457)) ;
#104463 = CARTESIAN_POINT('Ctrl Pts',(-17.9338217319753,-38.0475604692805,
123.101709933647)) ;
#104464 = CARTESIAN_POINT('Ctrl Pts',(-17.90265430105,-38.0575848813783,123.363299617885)) ;
#104465 = CARTESIAN_POINT('Ctrl Pts',(-17.9165551681965,-38.0674369657836,
123.621833332223)) ;
#104466 = CARTESIAN_POINT('Ctrl Pts',(-17.9755624279843,-38.0774278625268,
123.877634519735)) ;
#104467 = CARTESIAN_POINT('Ctrl Pts',(-18.0772087987277,-38.0873458544277,
124.117665217245)) ;
#104468 = CARTESIAN_POINT('Ctrl Pts',(-18.2204811522142,-38.0973739698847,
124.33881969572)) ;
#104469 = CARTESIAN_POINT('Ctrl Pts',(-18.3973561188024,-38.1072591458268,
124.529083160064)) ;
#104470 = CARTESIAN_POINT('Ctrl Pts',(-18.6063780250938,-38.1172485042337,
124.687904172725)) ;
#104471 = CARTESIAN_POINT('Ctrl Pts',(-18.8412609312879,-38.127289651814,
124.808143474274)) ;
#104472 = CARTESIAN_POINT('Ctrl Pts',(-19.0880878425469,-38.1371222748204,
124.884569704916)) ;
#104473 = CARTESIAN_POINT('Ctrl Pts',(-19.3485474897113,-38.1471163459312,
124.918245536733)) ;
#104474 = CARTESIAN_POINT('Ctrl Pts',(-19.6118018432702,-38.1571450035721,
124.905623026337)) ;
#104475 = CARTESIAN_POINT('Ctrl Pts',(-19.8652033688323,-38.1670293297649,
124.848603449057)) ;
#104476 = CARTESIAN_POINT('Ctrl Pts',(-20.1070976067128,-38.1769950732555,
124.748213951497)) ;
#104477 = CARTESIAN_POINT('Ctrl Pts',(-20.3290517854793,-38.1870234523867,
124.606153348801)) ;
#104478 = CARTESIAN_POINT('Ctrl Pts',(-20.5208025509905,-38.1969242985936,
124.430241432871)) ;
#104479 = CARTESIAN_POINT('Ctrl Pts',(-20.6815171132775,-38.2069829560107,
124.220431994097)) ;
#104480 = CARTESIAN_POINT('Ctrl Pts',(-20.8012070122064,-38.2168405187926,
123.990641916311)) ;
#104481 = CARTESIAN_POINT('Ctrl Pts',(-20.880986737264,-38.2269089213458,
123.738410661885)) ;
#104482 = CARTESIAN_POINT('Ctrl Pts',(-20.9150057915804,-38.2367643200854,
123.48164244073)) ;
#104483 = CARTESIAN_POINT('Ctrl Pts',(-20.9045577592598,-38.2467591871593,
123.219204450533)) ;
#104484 = CARTESIAN_POINT('Ctrl Pts',(-20.847938397475,-38.2567904821428,
122.961739544388)) ;
#104485 = CARTESIAN_POINT('Ctrl Pts',(-20.749506310943,-38.2666570068693,
122.721858258568)) ;
#104486 = CARTESIAN_POINT('Ctrl Pts',(-20.6095975475329,-38.276644477565,
122.499835152768)) ;
#104487 = CARTESIAN_POINT('Ctrl Pts',(-20.4340771525001,-38.2865892371289,
122.306157365648)) ;
#104488 = CARTESIAN_POINT('Ctrl Pts',(-20.2254558520578,-38.2966347930777,
122.144445923788)) ;
#104489 = CARTESIAN_POINT('Ctrl Pts',(-19.9963237905782,-38.3064943814529,
122.023421108531)) ;
#104490 = CARTESIAN_POINT('Ctrl Pts',(-19.7463143416056,-38.3164953365889,
121.942527032134)) ;
#104491 = CARTESIAN_POINT('Ctrl Pts',(-19.488519326872,-38.3263995638665,
121.906409654677)) ;
#104492 = CARTESIAN_POINT('Ctrl Pts',(-19.2248216455674,-38.3364416407616,
121.915654492875)) ;
#104493 = CARTESIAN_POINT('Ctrl Pts',(-18.9700831262293,-38.3463492534478,
121.96970219596)) ;
#104494 = CARTESIAN_POINT('Ctrl Pts',(-18.725090400626,-38.3564037840635,
122.06855506497)) ;
#104495 = CARTESIAN_POINT('Ctrl Pts',(-18.5051609091542,-38.3662645706124,
122.205658540537)) ;
#104496 = CARTESIAN_POINT('Ctrl Pts',(-18.309510262844,-38.3762583256834,
122.38078922624)) ;
#104497 = CARTESIAN_POINT('Ctrl Pts',(-18.1481992555944,-38.3861836859234,
122.585804588426)) ;
#104498 = CARTESIAN_POINT('Ctrl Pts',(-18.0236898301112,-38.3962116153187,
122.818019304383)) ;
#104499 = CARTESIAN_POINT('Ctrl Pts',(-17.9422763014649,-38.406097882118,
123.064775411848)) ;
#104500 = CARTESIAN_POINT('Ctrl Pts',(-17.9042719720946,-38.4161296510163,
123.325601599264)) ;
#104501 = CARTESIAN_POINT('Ctrl Pts',(-17.9117644560896,-38.4260112468599,
123.585218113154)) ;
#104502 = CARTESIAN_POINT('Ctrl Pts',(-17.9650952399222,-38.4360731323278,
123.844159329746)) ;
#104503 = CARTESIAN_POINT('Ctrl Pts',(-18.0605428012265,-38.4459305663467,
124.085012614075)) ;
#104504 = CARTESIAN_POINT('Ctrl Pts',(-18.1977237107639,-38.4559238093887,
124.308906706103)) ;
#104505 = CARTESIAN_POINT('Ctrl Pts',(-18.3706274266826,-38.465854570275,
124.504401204195)) ;
#104506 = CARTESIAN_POINT('Ctrl Pts',(-18.6449345264328,-38.4792035624722,
124.723116581102)) ;
#104507 = CARTESIAN_POINT('Ctrl Pts',(-18.9682302464026,-38.4924719352886,
124.863914087516)) ;
#104508 = CARTESIAN_POINT('Ctrl Pts',(-19.3133620154976,-38.505754876673,
124.916356944705)) ;
#104509 = CARTESIAN_POINT('Ctrl Pts',(-19.5771786980068,-38.5157976625152,
124.909903565302)) ;
#104510 = CARTESIAN_POINT('Ctrl Pts',(-19.8309832614376,-38.5256476050673,
124.859016008072)) ;
#104511 = CARTESIAN_POINT('Ctrl Pts',(-20.0759219776748,-38.5356448379863,
124.764044983854)) ;
#104512 = CARTESIAN_POINT('Ctrl Pts',(-20.3008573210295,-38.5456597333208,
124.627383085711)) ;
#104513 = CARTESIAN_POINT('Ctrl Pts',(-20.5625428004282,-38.558899409959,
124.398103758951)) ;
#104514 = CARTESIAN_POINT('Ctrl Pts',(-20.807908613215,-38.5754466343643,
124.033145256858)) ;
#104515 = CARTESIAN_POINT('Ctrl Pts',(-20.9148745686964,-38.5920940714954,
123.603813235972)) ;
#104516 = CARTESIAN_POINT('Ctrl Pts',(-20.9084002065562,-38.6053835689736,
123.254614227225)) ;
#104517 = CARTESIAN_POINT('Ctrl Pts',(-20.8593805891934,-38.615256976796,
122.999823493722)) ;
#104518 = CARTESIAN_POINT('Ctrl Pts',(-20.7652368411073,-38.6253093543887,
122.753014839041)) ;
#104519 = CARTESIAN_POINT('Ctrl Pts',(-20.6315634106382,-38.6352130079296,
122.529686605686)) ;
#104520 = CARTESIAN_POINT('Ctrl Pts',(-20.4609554845938,-38.6451572769249,
122.33178149402)) ;
#104521 = CARTESIAN_POINT('Ctrl Pts',(-20.1896720233983,-38.6584882852576,
122.110006814825)) ;
#104522 = CARTESIAN_POINT('Ctrl Pts',(-19.7868146270394,-38.6751098657819,
121.928869257225)) ;
#104523 = CARTESIAN_POINT('Ctrl Pts',(-19.3484026500655,-38.6916525364803,
121.895341800195)) ;
#104524 = CARTESIAN_POINT('Ctrl Pts',(-19.0036115337529,-38.7050016960432,
121.959975648739)) ;
#104525 = CARTESIAN_POINT('Ctrl Pts',(-18.6780675299039,-38.7182298462027,
122.081998336567)) ;
#104526 = CARTESIAN_POINT('Ctrl Pts',(-18.318189296983,-38.7348605233402,
122.338529958053)) ;
#104527 = CARTESIAN_POINT('Ctrl Pts',(-18.0180618486451,-38.7547634626283,
122.774214527966)) ;
#104528 = CARTESIAN_POINT('Ctrl Pts',(-17.8841363367089,-38.7746663292316,
123.285862111396)) ;
#104529 = CARTESIAN_POINT('Ctrl Pts',(-17.9320867719657,-38.7945794943364,
123.813063123829)) ;
#104530 = CARTESIAN_POINT('Ctrl Pts',(-18.1591211464769,-38.8146153234777,
124.29467830062)) ;
#104531 = CARTESIAN_POINT('Ctrl Pts',(-18.5326984939295,-38.8344338983558,
124.666208169951)) ;
#104532 = CARTESIAN_POINT('Ctrl Pts',(-19.0136620305705,-38.8544041993978,
124.890287109403)) ;
#104533 = CARTESIAN_POINT('Ctrl Pts',(-19.5404886042975,-38.8742957317623,
124.936806064682)) ;
#104534 = CARTESIAN_POINT('Ctrl Pts',(-20.0545416964585,-38.8943188295789,
124.79955145257)) ;
#104535 = CARTESIAN_POINT('Ctrl Pts',(-20.4863312832862,-38.9141155824988,
124.498762007318)) ;
#104536 = CARTESIAN_POINT('Ctrl Pts',(-20.7931734977669,-38.9340766709876,
124.066022444128)) ;
#104537 = CARTESIAN_POINT('Ctrl Pts',(-20.9330014112939,-38.9540549399198,
123.553728971444)) ;
#104538 = CARTESIAN_POINT('Ctrl Pts',(-20.8907327724234,-38.9738749547108,
123.02869475274)) ;
#104539 = CARTESIAN_POINT('Ctrl Pts',(-20.671741885746,-38.9938133639626,
122.546100539438)) ;
#104540 = CARTESIAN_POINT('Ctrl Pts',(-20.2983058535929,-39.013860481355,
122.165949512377)) ;
#104541 = CARTESIAN_POINT('Ctrl Pts',(-19.8223852491387,-39.0337067271889,
121.938630866729)) ;
#104542 = CARTESIAN_POINT('Ctrl Pts',(-19.2975107818307,-39.0535556957009,
121.88528017714)) ;
#104543 = CARTESIAN_POINT('Ctrl Pts',(-18.7809909805652,-39.0736059980122,
122.016192548372)) ;
#104544 = CARTESIAN_POINT('Ctrl Pts',(-18.3447992174342,-39.0934409204434,
122.312485774824)) ;
#104545 = CARTESIAN_POINT('Ctrl Pts',(-18.0337712867575,-39.1133713216693,
122.741023909243)) ;
#104546 = CARTESIAN_POINT('Ctrl Pts',(-17.8872243556571,-39.1332562670282,
123.249020163311)) ;
#104547 = CARTESIAN_POINT('Ctrl Pts',(-17.9240100369502,-39.1533288751795,
123.781146880013)) ;
#104548 = CARTESIAN_POINT('Ctrl Pts',(-18.1371362656377,-39.1731201915077,
124.262143080741)) ;
#104549 = CARTESIAN_POINT('Ctrl Pts',(-18.5035341697257,-39.1930849812749,
124.645907690736)) ;
#104550 = CARTESIAN_POINT('Ctrl Pts',(-18.9799661770289,-39.2130679370252,
124.880649319702)) ;
#104551 = CARTESIAN_POINT('Ctrl Pts',(-19.5032134048626,-39.2328764590014,
124.939294610312)) ;
#104552 = CARTESIAN_POINT('Ctrl Pts',(-20.0196253121338,-39.2528620337372,
124.815383030727)) ;
#104553 = CARTESIAN_POINT('Ctrl Pts',(-20.4606098925301,-39.2727446738056,
124.523969753369)) ;
#104554 = CARTESIAN_POINT('Ctrl Pts',(-20.7770307675651,-39.2926999859375,
124.098449337436)) ;
#104555 = CARTESIAN_POINT('Ctrl Pts',(-20.9290125086487,-39.3125743425453,
123.592464133645)) ;
#104556 = CARTESIAN_POINT('Ctrl Pts',(-20.8993955940314,-39.3325565494064,
123.062255599716)) ;
#104557 = CARTESIAN_POINT('Ctrl Pts',(-20.6908311188949,-39.3524876273563,
122.575184100747)) ;
#104558 = CARTESIAN_POINT('Ctrl Pts',(-20.3288513423794,-39.3724146022113,
122.188711260408)) ;
#104559 = CARTESIAN_POINT('Ctrl Pts',(-19.8592740611879,-39.3922470611602,
121.949092111192)) ;
#104560 = CARTESIAN_POINT('Ctrl Pts',(-19.4200714383122,-39.4089047453354,
121.894176350712)) ;
#104561 = CARTESIAN_POINT('Ctrl Pts',(-19.0750845374092,-39.4221539692425,
121.941823263879)) ;
#104562 = CARTESIAN_POINT('Ctrl Pts',(-18.8237314955638,-39.4322029906937,
122.022704050237)) ;
#104563 = CARTESIAN_POINT('Ctrl Pts',(-18.5945719587257,-39.4420629989242,
122.143637046641)) ;
#104564 = CARTESIAN_POINT('Ctrl Pts',(-18.3180933172419,-39.4553465121488,
122.356805711671)) ;
#104565 = CARTESIAN_POINT('Ctrl Pts',(-18.0500122798187,-39.4719924311496,
122.708686652931)) ;
#104566 = CARTESIAN_POINT('Ctrl Pts',(-17.9182229494711,-39.4885464089657,
123.128502561202)) ;
#104567 = CARTESIAN_POINT('Ctrl Pts',(-17.9033037209562,-39.5019061379373,
123.479260538537)) ;
#104568 = CARTESIAN_POINT('Ctrl Pts',(-17.9373243166265,-39.511799189734,
123.73702185097)) ;
#104569 = CARTESIAN_POINT('Ctrl Pts',(-18.0159991395794,-39.521789155015,
123.987450031677)) ;
#104570 = CARTESIAN_POINT('Ctrl Pts',(-18.1363948183346,-39.5317410358759,
124.219660059973)) ;
#104571 = CARTESIAN_POINT('Ctrl Pts',(-18.2969567303426,-39.5417893875677,
124.429261495582)) ;
#104572 = CARTESIAN_POINT('Ctrl Pts',(-18.4872968694705,-39.5516306716739,
124.604383387252)) ;
#104573 = CARTESIAN_POINT('Ctrl Pts',(-18.7080132350859,-39.5616173747996,
124.746280915969)) ;
#104574 = CARTESIAN_POINT('Ctrl Pts',(-18.9487894622265,-39.571552403617,
124.847360989506)) ;
#104575 = CARTESIAN_POINT('Ctrl Pts',(-19.2065140511912,-39.5816081985239,
124.905565796026)) ;
#104576 = CARTESIAN_POINT('Ctrl Pts',(-19.4645174692471,-39.5914365618132,
124.918256133084)) ;
#104577 = CARTESIAN_POINT('Ctrl Pts',(-19.7268451727224,-39.6014975317111,
124.885572668199)) ;
#104578 = CARTESIAN_POINT('Ctrl Pts',(-19.975826615135,-39.6114118106009,
124.808745771758)) ;
#104579 = CARTESIAN_POINT('Ctrl Pts',(-20.2101147526998,-39.6214208050691,
124.689190878813)) ;
#104580 = CARTESIAN_POINT('Ctrl Pts',(-20.4201917083197,-39.6314506396329,
124.530016381586)) ;
#104581 = CARTESIAN_POINT('Ctrl Pts',(-20.5967480738789,-39.6413088697051,
124.340408988415)) ;
#104582 = CARTESIAN_POINT('Ctrl Pts',(-20.7399416116488,-39.6513075754475,
124.120151495225)) ;
#104583 = CARTESIAN_POINT('Ctrl Pts',(-20.8419667401955,-39.6612022313663,
123.880930605465)) ;
#104584 = CARTESIAN_POINT('Ctrl Pts',(-20.9018070177436,-39.6712652957503,
123.623389631562)) ;
#104585 = CARTESIAN_POINT('Ctrl Pts',(-20.9159959456146,-39.6811049540302,
123.365160498217)) ;
#104586 = CARTESIAN_POINT('Ctrl Pts',(-20.8847744321172,-39.691168121112,
123.102597212556)) ;
#104587 = CARTESIAN_POINT('Ctrl Pts',(-20.809489673972,-39.7010623662391,
122.85369436539)) ;
#104588 = CARTESIAN_POINT('Ctrl Pts',(-20.6922282780621,-39.7110041878437,
122.620263504091)) ;
#104589 = CARTESIAN_POINT('Ctrl Pts',(-20.5353015269347,-39.7210067187618,
122.409347149382)) ;
#104590 = CARTESIAN_POINT('Ctrl Pts',(-20.3432781213976,-39.7310413452193,
122.228634378221)) ;
#104591 = CARTESIAN_POINT('Ctrl Pts',(-20.1271560894029,-39.7408868802057,
122.086376137188)) ;
#104592 = CARTESIAN_POINT('Ctrl Pts',(-19.8865438462401,-39.7508703050448,
121.98185816591)) ;
#104593 = CARTESIAN_POINT('Ctrl Pts',(-19.6322426627051,-39.7608206954098,
121.920952858451)) ;
#104594 = CARTESIAN_POINT('Ctrl Pts',(-19.3699963296536,-39.7708183357069,
121.904697658829)) ;
#104595 = CARTESIAN_POINT('Ctrl Pts',(-19.1079263014732,-39.7808574162701,
121.934869440675)) ;
#104596 = CARTESIAN_POINT('Ctrl Pts',(-18.860246320499,-39.7906835670392,
122.007945708083)) ;
#104597 = CARTESIAN_POINT('Ctrl Pts',(-18.6234343625826,-39.8007401419683,
122.125222897049)) ;
#104598 = CARTESIAN_POINT('Ctrl Pts',(-18.4132900657496,-39.8106806813486,
122.280411411779)) ;
#104599 = CARTESIAN_POINT('Ctrl Pts',(-18.2333513169746,-39.820585074325,
122.468477752401)) ;
#104600 = CARTESIAN_POINT('Ctrl Pts',(-18.0868790875031,-39.8306317285299,
122.688109809972)) ;
#104601 = CARTESIAN_POINT('Ctrl Pts',(-17.9821196213691,-39.8405272904683,
122.926166157976)) ;
#104602 = CARTESIAN_POINT('Ctrl Pts',(-17.919264861442,-39.8505893683139,
123.182968808)) ;
#104603 = CARTESIAN_POINT('Ctrl Pts',(-17.902179100725,-39.8604320667276,
123.441089403448)) ;
#104604 = CARTESIAN_POINT('Ctrl Pts',(-17.9299684986018,-39.8704228416891,
123.702127740088)) ;
#104605 = CARTESIAN_POINT('Ctrl Pts',(-18.0022538608553,-39.8803507067082,
123.952822926741)) ;
#104606 = CARTESIAN_POINT('Ctrl Pts',(-18.1172750648444,-39.8903394514744,
124.18878013499)) ;
#104607 = CARTESIAN_POINT('Ctrl Pts',(-18.2725120158301,-39.9003722370613,
124.401889306387)) ;
#104608 = CARTESIAN_POINT('Ctrl Pts',(-18.4590581539121,-39.910238921682,
124.581959456617)) ;
#104609 = CARTESIAN_POINT('Ctrl Pts',(-18.6756999438248,-39.9202008138451,
124.728934492756)) ;
#104610 = CARTESIAN_POINT('Ctrl Pts',(-18.9164434449401,-39.9302342907577,
124.836443452761)) ;
#104611 = CARTESIAN_POINT('Ctrl Pts',(-19.1683377738206,-39.940118632006,
124.899975771883)) ;
#104612 = CARTESIAN_POINT('Ctrl Pts',(-19.4320522241906,-39.9501815741271,
124.919144828217)) ;
#104613 = CARTESIAN_POINT('Ctrl Pts',(-19.6895996842893,-39.9600319757467,
124.89292120347)) ;
#104614 = CARTESIAN_POINT('Ctrl Pts',(-19.9432985792622,-39.9700588645364,
124.821762394978)) ;
#104615 = CARTESIAN_POINT('Ctrl Pts',(-20.1805473148166,-39.9800874794926,
124.706983894137)) ;
#104616 = CARTESIAN_POINT('Ctrl Pts',(-20.3906194099252,-39.9899327026126,
124.555988101706)) ;
#104617 = CARTESIAN_POINT('Ctrl Pts',(-20.5744702495279,-39.9999233864186,
124.368552094175)) ;
#104618 = CARTESIAN_POINT('Ctrl Pts',(-20.7231943261795,-40.009961268491,
124.150693894303)) ;
#104619 = CARTESIAN_POINT('Ctrl Pts',(-20.8301547375358,-40.0198056281299,
123.915129884966)) ;
#104620 = CARTESIAN_POINT('Ctrl Pts',(-20.8959976047034,-40.0297904987446,
123.661170320315)) ;
#104621 = CARTESIAN_POINT('Ctrl Pts',(-20.9167748834998,-40.0397297820733,
123.400765241907)) ;
#104622 = CARTESIAN_POINT('Ctrl Pts',(-20.8916933004371,-40.0497703914464,
123.138130792356)) ;
#104623 = CARTESIAN_POINT('Ctrl Pts',(-20.8226519350043,-40.0596552423596,
122.887678558748)) ;
#104624 = CARTESIAN_POINT('Ctrl Pts',(-20.7101676316189,-40.0696571985284,
122.650166731446)) ;
#104625 = CARTESIAN_POINT('Ctrl Pts',(-20.5595427373319,-40.0795757952489,
122.437393424481)) ;
#104626 = CARTESIAN_POINT('Ctrl Pts',(-20.3718862888207,-40.0896226173247,
122.251727314683)) ;
#104627 = CARTESIAN_POINT('Ctrl Pts',(-20.1586418375335,-40.0994968984374,
122.103798399595)) ;
#104628 = CARTESIAN_POINT('Ctrl Pts',(-19.9188066374815,-40.109551098482,
121.993056383595)) ;
#104629 = CARTESIAN_POINT('Ctrl Pts',(-19.6673552313463,-40.1194465281173,
121.926576698577)) ;
#104630 = CARTESIAN_POINT('Ctrl Pts',(-19.403915213379,-40.1295081564346,
121.904345230977)) ;
#104631 = CARTESIAN_POINT('Ctrl Pts',(-19.1462503218584,-40.1393527852645,
121.927649389564)) ;
#104632 = CARTESIAN_POINT('Ctrl Pts',(-18.8933867189319,-40.1493128328701,
121.995219488322)) ;
#104633 = CARTESIAN_POINT('Ctrl Pts',(-18.6544595208045,-40.1593511390442,
122.107002406275)) ;
#104634 = CARTESIAN_POINT('Ctrl Pts',(-18.4417892571476,-40.1692244384768,
122.255702785229)) ;
#104635 = CARTESIAN_POINT('Ctrl Pts',(-18.2545782722109,-40.1792977000631,
122.44277820839)) ;
#104636 = CARTESIAN_POINT('Ctrl Pts',(-18.1061634154911,-40.1891179260198,
122.653968585527)) ;
#104637 = CARTESIAN_POINT('Ctrl Pts',(-17.9936299888844,-40.1991969899593,
122.893665938314)) ;
#104638 = CARTESIAN_POINT('Ctrl Pts',(-17.9258431923376,-40.2090470799791,
123.143555897094)) ;
#104639 = CARTESIAN_POINT('Ctrl Pts',(-17.9018083217025,-40.2191258335929,
123.407254879522)) ;
#104640 = CARTESIAN_POINT('Ctrl Pts',(-17.92317260739,-40.2289473008524,123.664525748583)) ;
#104641 = CARTESIAN_POINT('Ctrl Pts',(-17.9900923585646,-40.23901289921,123.920371717973)) ;
#104642 = CARTESIAN_POINT('Ctrl Pts',(-18.0987485022891,-40.2489155549847,
124.156904978574)) ;
#104643 = CARTESIAN_POINT('Ctrl Pts',(-18.248904465991,-40.2589663808143,
124.374130409106)) ;
#104644 = CARTESIAN_POINT('Ctrl Pts',(-18.4311339191493,-40.2688405851532,
124.558938498704)) ;
#104645 = CARTESIAN_POINT('Ctrl Pts',(-18.64682823792,-40.2789130351923,124.71226441453)) ;
#104646 = CARTESIAN_POINT('Ctrl Pts',(-18.8800799546237,-40.2887420519658,
124.823334593116)) ;
#104647 = CARTESIAN_POINT('Ctrl Pts',(-19.1349090565034,-40.2988088978806,
124.894208967306)) ;
#104648 = CARTESIAN_POINT('Ctrl Pts',(-19.3936461150515,-40.3086990691824,
124.919152044099)) ;
#104649 = CARTESIAN_POINT('Ctrl Pts',(-19.6554532124092,-40.3186912628062,
124.899160184907)) ;
#104650 = CARTESIAN_POINT('Ctrl Pts',(-19.9090113028745,-40.3286540734297,
124.833961970796)) ;
#104651 = CARTESIAN_POINT('Ctrl Pts',(-20.146294812703,-40.3385583462731,
124.72695427471)) ;
#104652 = CARTESIAN_POINT('Ctrl Pts',(-20.3646113413137,-40.3486188380777,
124.577901009706)) ;
#104653 = CARTESIAN_POINT('Ctrl Pts',(-20.5498777891069,-40.3584591697501,
124.39744010255)) ;
#104654 = CARTESIAN_POINT('Ctrl Pts',(-20.7046324746843,-40.3685222158418,
124.183046356769)) ;
#104655 = CARTESIAN_POINT('Ctrl Pts',(-20.8177094322231,-40.3784162715369,
123.948887583133)) ;
#104656 = CARTESIAN_POINT('Ctrl Pts',(-20.889431383718,-40.3883589718599,
123.697670525039)) ;
#104657 = CARTESIAN_POINT('Ctrl Pts',(-20.9166730793873,-40.3983647127875,
123.436117530858)) ;
#104658 = CARTESIAN_POINT('Ctrl Pts',(-20.8977644606213,-40.408385623303,
123.173464560564)) ;
#104659 = CARTESIAN_POINT('Ctrl Pts',(-20.8346596888786,-40.418276358753,
122.921314553624)) ;
#104660 = CARTESIAN_POINT('Ctrl Pts',(-20.7280148134984,-40.4282678994818,
122.681391753882)) ;
#104661 = CARTESIAN_POINT('Ctrl Pts',(-20.5819059977354,-40.4382157599035,
122.464616950572)) ;
#104662 = CARTESIAN_POINT('Ctrl Pts',(-20.4007589940039,-40.4481624290898,
122.276156866354)) ;
#104663 = CARTESIAN_POINT('Ctrl Pts',(-20.1873379860688,-40.4582105052254,
122.120688929112)) ;
#104664 = CARTESIAN_POINT('Ctrl Pts',(-19.9549808379891,-40.468058103231,
122.006755225708)) ;
#104665 = CARTESIAN_POINT('Ctrl Pts',(-19.7037329672669,-40.4780198263155,
121.933279690208)) ;
#104666 = CARTESIAN_POINT('Ctrl Pts',(-19.4417310980554,-40.4880484613985,
121.904681422218)) ;
#104667 = CARTESIAN_POINT('Ctrl Pts',(-19.1818683091589,-40.4979587697165,
121.921718478784)) ;
#104668 = CARTESIAN_POINT('Ctrl Pts',(-18.9281025160491,-40.5078936668524,
121.983111466972)) ;
#104669 = CARTESIAN_POINT('Ctrl Pts',(-18.6864066527644,-40.517934749795,
122.088968537774)) ;
#104670 = CARTESIAN_POINT('Ctrl Pts',(-18.4700085972782,-40.5278220926232,
122.232808818307)) ;
#104671 = CARTESIAN_POINT('Ctrl Pts',(-18.2795999896644,-40.5378136075626,
122.413579933739)) ;
#104672 = CARTESIAN_POINT('Ctrl Pts',(-18.1241747121208,-40.5477649987591,
122.6239004086)) ;
#104673 = CARTESIAN_POINT('Ctrl Pts',(-18.0074485776265,-40.5576975320917,
122.857361394326)) ;
#104674 = CARTESIAN_POINT('Ctrl Pts',(-17.9324508010301,-40.5676946899911,
123.10913336402)) ;
#104675 = CARTESIAN_POINT('Ctrl Pts',(-17.9022406529459,-40.5776797001546,
123.369825342602)) ;
#104676 = CARTESIAN_POINT('Ctrl Pts',(-17.9182261140399,-40.5877225267244,
123.633219631623)) ;
#104677 = CARTESIAN_POINT('Ctrl Pts',(-17.9778420179096,-40.5975527610294,
123.884617651115)) ;
#104678 = CARTESIAN_POINT('Ctrl Pts',(-18.082615365187,-40.607628786264,124.127734830538)) ;
#104679 = CARTESIAN_POINT('Ctrl Pts',(-18.2247286077959,-40.6174810227549,
124.344219676141)) ;
#104680 = CARTESIAN_POINT('Ctrl Pts',(-18.4060222671009,-40.627554229189,
124.537048390398)) ;
#104681 = CARTESIAN_POINT('Ctrl Pts',(-18.6132579836576,-40.6373957386962,
124.691803922634)) ;
#104682 = CARTESIAN_POINT('Ctrl Pts',(-18.8465505513508,-40.647356685476,
124.810505779796)) ;
#104683 = CARTESIAN_POINT('Ctrl Pts',(-19.0989962736122,-40.657394514276,
124.886982239754)) ;
#104684 = CARTESIAN_POINT('Ctrl Pts',(-19.3566017243631,-40.6672688240305,
124.918434301797)) ;
#104685 = CARTESIAN_POINT('Ctrl Pts',(-19.6208150027249,-40.6773385217037,
124.904396748732)) ;
#104686 = CARTESIAN_POINT('Ctrl Pts',(-19.8726147197196,-40.6871719929911,
124.846216573453)) ;
#104687 = CARTESIAN_POINT('Ctrl Pts',(-20.1155053857362,-40.697201639521,
124.743893434288)) ;
#104688 = CARTESIAN_POINT('Ctrl Pts',(-20.3366189670899,-40.7072361538484,
124.600200710188)) ;
#104689 = CARTESIAN_POINT('Ctrl Pts',(-20.525825198918,-40.7170614393193,
124.424506374465)) ;
#104690 = CARTESIAN_POINT('Ctrl Pts',(-20.68491390274,-40.7270656808678,124.215241512207)) ;
#104691 = CARTESIAN_POINT('Ctrl Pts',(-20.8049296705375,-40.7370483259469,
123.981914452977)) ;
#104692 = CARTESIAN_POINT('Ctrl Pts',(-20.8827863098033,-40.7470935230384,
123.729709556929)) ;
#104693 = CARTESIAN_POINT('Ctrl Pts',(-20.915379084268,-40.7569166387985,
123.473623942466)) ;
#104694 = CARTESIAN_POINT('Ctrl Pts',(-20.9034107635186,-40.7669512505988,
123.210200309604)) ;
#104695 = CARTESIAN_POINT('Ctrl Pts',(-20.8452197947678,-40.776976259372,
122.953252483694)) ;
#104696 = CARTESIAN_POINT('Ctrl Pts',(-20.7455808245074,-40.7868281842135,
122.714289948241)) ;
#104697 = CARTESIAN_POINT('Ctrl Pts',(-20.6043528530783,-40.7968191225363,
122.492995525235)) ;
#104698 = CARTESIAN_POINT('Ctrl Pts',(-20.4282240529534,-40.8067371076827,
122.300836023741)) ;
#104699 = CARTESIAN_POINT('Ctrl Pts',(-20.219189537808,-40.8167652085782,
122.140396675837)) ;
#104700 = CARTESIAN_POINT('Ctrl Pts',(-19.9888292012109,-40.8266504495208,
122.02031551487)) ;
#104701 = CARTESIAN_POINT('Ctrl Pts',(-19.7387079643851,-40.8366395624874,
121.940619087225)) ;
#104702 = CARTESIAN_POINT('Ctrl Pts',(-19.4771067125699,-40.8466816268282,
121.90595198204)) ;
#104703 = CARTESIAN_POINT('Ctrl Pts',(-19.2190107936235,-40.8565108282327,
121.916506045072)) ;
#104704 = CARTESIAN_POINT('Ctrl Pts',(-18.9620250651059,-40.8665176689909,
121.972140998041)) ;
#104705 = CARTESIAN_POINT('Ctrl Pts',(-18.7190636625384,-40.8765051931828,
122.071533195608)) ;
#104706 = CARTESIAN_POINT('Ctrl Pts',(-18.4962689240686,-40.8865348389914,
122.212311168412)) ;
#104707 = CARTESIAN_POINT('Ctrl Pts',(-18.3040798981206,-40.8964088697302,
122.386686890598)) ;
#104708 = CARTESIAN_POINT('Ctrl Pts',(-18.1428560506009,-40.9064081925943,
122.594132528104)) ;
#104709 = CARTESIAN_POINT('Ctrl Pts',(-18.0209192869641,-40.9163190281699,
122.824322396063)) ;
#104710 = CARTESIAN_POINT('Ctrl Pts',(-17.939762056432,-40.9263732761439,
123.075720211064)) ;
#104711 = CARTESIAN_POINT('Ctrl Pts',(-17.9038796152349,-40.9362320204066,
123.332346566764)) ;
#104712 = CARTESIAN_POINT('Ctrl Pts',(-17.9131359934758,-40.9463001064796,
123.59672475981)) ;
#104713 = CARTESIAN_POINT('Ctrl Pts',(-17.9670267901645,-40.9561555896591,
123.850070178166)) ;
#104714 = CARTESIAN_POINT('Ctrl Pts',(-18.0647187939215,-40.9661504354533,
124.09387118481)) ;
#104715 = CARTESIAN_POINT('Ctrl Pts',(-18.2042534659946,-40.9761817311159,
124.317531681712)) ;
#104716 = CARTESIAN_POINT('Ctrl Pts',(-18.3773037920473,-40.9860482744057,
124.510626572137)) ;
#104717 = CARTESIAN_POINT('Ctrl Pts',(-18.5834579512395,-40.9960356701691,
124.673010282947)) ;
#104718 = CARTESIAN_POINT('Ctrl Pts',(-18.8136905659678,-41.0059807108991,
124.796762194156)) ;
#104719 = CARTESIAN_POINT('Ctrl Pts',(-19.0643800763501,-41.0160252171158,
124.879316585335)) ;
#104720 = CARTESIAN_POINT('Ctrl Pts',(-19.3209063355399,-41.0258887232531,
124.916648200667)) ;
#104721 = CARTESIAN_POINT('Ctrl Pts',(-19.5833652350963,-41.0358815840892,
124.909236656653)) ;
#104722 = CARTESIAN_POINT('Ctrl Pts',(-19.838933260049,-41.0458077778081,
124.856823666464)) ;
#104723 = CARTESIAN_POINT('Ctrl Pts',(-20.08373963909,-41.0558267038407,124.760006771853)) ;
#104724 = CARTESIAN_POINT('Ctrl Pts',(-20.3058788547958,-41.0657417032083,
124.623756791964)) ;
#104725 = CARTESIAN_POINT('Ctrl Pts',(-20.5036454816884,-41.0757964747656,
124.448577731493)) ;
#104726 = CARTESIAN_POINT('Ctrl Pts',(-20.6649615792407,-41.0856554370632,
124.245802378159)) ;
#104727 = CARTESIAN_POINT('Ctrl Pts',(-20.7907129716142,-41.095649680901,
124.015274099518)) ;
#104728 = CARTESIAN_POINT('Ctrl Pts',(-20.8740909164821,-41.1055749103252,
123.768092059042)) ;
#104729 = CARTESIAN_POINT('Ctrl Pts',(-20.9136888180014,-41.1156028742167,
123.507595045891)) ;
#104730 = CARTESIAN_POINT('Ctrl Pts',(-20.9078085172522,-41.1254891338471,
123.247821927504)) ;
#104731 = CARTESIAN_POINT('Ctrl Pts',(-20.8563139433764,-41.1355208969249,
122.989320648716)) ;
#104732 = CARTESIAN_POINT('Ctrl Pts',(-20.7623509133108,-41.1454025232191,
122.747188328021)) ;
#104733 = CARTESIAN_POINT('Ctrl Pts',(-20.6254238376886,-41.1554642927052,
122.521036729548)) ;
#104734 = CARTESIAN_POINT('Ctrl Pts',(-20.4548494543705,-41.1653221602007,
122.326024259616)) ;
#104735 = CARTESIAN_POINT('Ctrl Pts',(-20.2506808427215,-41.1753137853181,
122.160974102844)) ;
#104736 = CARTESIAN_POINT('Ctrl Pts',(-20.0221515737594,-41.1852505844263,
122.034598195036)) ;
#104737 = CARTESIAN_POINT('Ctrl Pts',(-19.7739435190989,-41.1952414139836,
121.949006315307)) ;
#104738 = CARTESIAN_POINT('Ctrl Pts',(-19.5137514171269,-41.2052646496968,
121.907979672832)) ;
#104739 = CARTESIAN_POINT('Ctrl Pts',(-19.2537296731998,-41.215160997726,
121.912474207258)) ;
#104740 = CARTESIAN_POINT('Ctrl Pts',(-18.9959084829037,-41.2251505602285,
121.9619692281)) ;
#104741 = CARTESIAN_POINT('Ctrl Pts',(-18.7495657819261,-41.235190867913,
122.056441570099)) ;
#104742 = CARTESIAN_POINT('Ctrl Pts',(-18.5275452867294,-41.2450331712602,
122.189166374381)) ;
#104743 = CARTESIAN_POINT('Ctrl Pts',(-18.3281548287422,-41.2550568795393,
122.361237377681)) ;
#104744 = CARTESIAN_POINT('Ctrl Pts',(-18.1083697767218,-41.268279057007,
122.630432167841)) ;
#104745 = CARTESIAN_POINT('Ctrl Pts',(-17.9628107520037,-41.2815716420663,
122.952236618744)) ;
#104746 = CARTESIAN_POINT('Ctrl Pts',(-17.906179171894,-41.2948564979879,
123.296802175274)) ;
#104747 = CARTESIAN_POINT('Ctrl Pts',(-17.9090306066105,-41.3048287251607,
123.558807567158)) ;
#104748 = CARTESIAN_POINT('Ctrl Pts',(-17.956592126779,-41.3147373415997,
123.814847983363)) ;
#104749 = CARTESIAN_POINT('Ctrl Pts',(-18.0492993140407,-41.3247905469834,
124.062207468228)) ;
#104750 = CARTESIAN_POINT('Ctrl Pts',(-18.1809181516501,-41.3346556807437,
124.285582948487)) ;
#104751 = CARTESIAN_POINT('Ctrl Pts',(-18.4080967270928,-41.34799473837,124.552513462829)) ;
#104752 = CARTESIAN_POINT('Ctrl Pts',(-18.770623265762,-41.3645639257032,
124.802648338429)) ;
#104753 = CARTESIAN_POINT('Ctrl Pts',(-19.1984831391044,-41.3812090655542,
124.914853897133)) ;
#104754 = CARTESIAN_POINT('Ctrl Pts',(-19.5473217004566,-41.3944813680276,
124.912961520179)) ;
#104755 = CARTESIAN_POINT('Ctrl Pts',(-19.8054060000368,-41.4044623314752,
124.866340893151)) ;
#104756 = CARTESIAN_POINT('Ctrl Pts',(-20.0506155228347,-41.4144041635445,
124.776102300555)) ;
#104757 = CARTESIAN_POINT('Ctrl Pts',(-20.3531550397601,-41.42772373276,124.600157011431)) ;
#104758 = CARTESIAN_POINT('Ctrl Pts',(-20.6634973166793,-41.4442538876927,
124.289018525257)) ;
#104759 = CARTESIAN_POINT('Ctrl Pts',(-20.8878936866745,-41.4642756131848,
123.806648609792)) ;
#104760 = CARTESIAN_POINT('Ctrl Pts',(-20.9340514789459,-41.4840870097916,
123.281992417524)) ;
#104761 = CARTESIAN_POINT('Ctrl Pts',(-20.7981312719008,-41.5040722585005,
122.768629034436)) ;
#104762 = CARTESIAN_POINT('Ctrl Pts',(-20.4961530601248,-41.5239663211364,
122.334489849304)) ;
#104763 = CARTESIAN_POINT('Ctrl Pts',(-20.0638683825088,-41.54389800031,122.028293719276)) ;
#104764 = CARTESIAN_POINT('Ctrl Pts',(-19.5521109509209,-41.563862054782,
121.888097482406)) ;
#104765 = CARTESIAN_POINT('Ctrl Pts',(-19.0253800918483,-41.5837429565449,
121.930378296614)) ;
#104766 = CARTESIAN_POINT('Ctrl Pts',(-18.5431404788178,-41.6036816181533,
122.150032410846)) ;
#104767 = CARTESIAN_POINT('Ctrl Pts',(-18.1655334411876,-41.6235781434086,
122.52023469084)) ;
#104768 = CARTESIAN_POINT('Ctrl Pts',(-17.9361452856179,-41.6434731818629,
122.996685523952)) ;
#104769 = CARTESIAN_POINT('Ctrl Pts',(-17.8830117703529,-41.663437005169,
123.524584694649)) ;
#104770 = CARTESIAN_POINT('Ctrl Pts',(-18.0122651695746,-41.6833111292981,
124.03678760612)) ;
#104771 = CARTESIAN_POINT('Ctrl Pts',(-18.3096364829872,-41.7032862050253,
124.47662297454)) ;
#104772 = CARTESIAN_POINT('Ctrl Pts',(-18.7392073244081,-41.7232397743819,
124.78761036798)) ;
#104773 = CARTESIAN_POINT('Ctrl Pts',(-19.2458943339169,-41.7430776845698,
124.933458741482)) ;
#104774 = CARTESIAN_POINT('Ctrl Pts',(-19.7756310784011,-41.7630535131407,
124.897960696145)) ;
#104775 = CARTESIAN_POINT('Ctrl Pts',(-20.2597826091099,-41.782971557851,
124.683924222372)) ;
#104776 = CARTESIAN_POINT('Ctrl Pts',(-20.6419494519346,-41.8028418036386,
124.31927167099)) ;
#104777 = CARTESIAN_POINT('Ctrl Pts',(-20.8780338315248,-41.8228908067382,
123.841704887354)) ;
#104778 = CARTESIAN_POINT('Ctrl Pts',(-20.9367994539904,-41.842670047979,
123.319145032248)) ;
#104779 = CARTESIAN_POINT('Ctrl Pts',(-20.8130020447445,-41.8627001116879,
122.801495938331)) ;
#104780 = CARTESIAN_POINT('Ctrl Pts',(-20.5213260449873,-41.8825823965899,
122.360747751626)) ;
#104781 = CARTESIAN_POINT('Ctrl Pts',(-20.0977332665932,-41.9024646974829,
122.044888722237)) ;
#104782 = CARTESIAN_POINT('Ctrl Pts',(-19.5891103850463,-41.9224478071012,
121.891915834153)) ;
#104783 = CARTESIAN_POINT('Ctrl Pts',(-19.0612570378797,-41.9423382024791,
121.921619505175)) ;
#104784 = CARTESIAN_POINT('Ctrl Pts',(-18.5748533541873,-41.9622349925134,
122.12896396189)) ;
#104785 = CARTESIAN_POINT('Ctrl Pts',(-18.1875398551015,-41.982152046455,
122.489857562728)) ;
#104786 = CARTESIAN_POINT('Ctrl Pts',(-17.9457214835328,-42.0021555946585,
122.963422399835)) ;
#104787 = CARTESIAN_POINT('Ctrl Pts',(-17.8810265727572,-42.0220938883111,
123.489360284753)) ;
#104788 = CARTESIAN_POINT('Ctrl Pts',(-17.9977456916004,-42.041915375744,
124.003097477831)) ;
#104789 = CARTESIAN_POINT('Ctrl Pts',(-18.2845368526884,-42.0618937687349,
124.44990914885)) ;
#104790 = CARTESIAN_POINT('Ctrl Pts',(-18.7052001843518,-42.0817921503486,
124.770575674907)) ;
#104791 = CARTESIAN_POINT('Ctrl Pts',(-19.1255759866277,-42.0983750810785,
124.902691008963)) ;
#104792 = CARTESIAN_POINT('Ctrl Pts',(-19.4741352236223,-42.1116493166673,
124.918003242186)) ;
#104793 = CARTESIAN_POINT('Ctrl Pts',(-19.7358481841753,-42.1216957341235,
124.883486155696)) ;
#104794 = CARTESIAN_POINT('Ctrl Pts',(-19.9826831156594,-42.1315409593428,
124.805898248086)) ;
#104795 = CARTESIAN_POINT('Ctrl Pts',(-20.293988571428,-42.1448759303822,
124.64504920141)) ;
#104796 = CARTESIAN_POINT('Ctrl Pts',(-20.6198940492843,-42.1614587871748,
124.348199125728)) ;
#104797 = CARTESIAN_POINT('Ctrl Pts',(-20.8257028894447,-42.1781017895242,
123.956759520653)) ;
#104798 = CARTESIAN_POINT('Ctrl Pts',(-20.9027397201207,-42.1913455205559,
123.617281377377)) ;
#104799 = CARTESIAN_POINT('Ctrl Pts',(-20.9155836796199,-42.2013999152305,
123.353425803393)) ;
#104800 = CARTESIAN_POINT('Ctrl Pts',(-20.8834418745023,-42.2112409766191,
123.096770719865)) ;
#104801 = CARTESIAN_POINT('Ctrl Pts',(-20.8057549628219,-42.2213072009756,
122.843952261428)) ;
#104802 = CARTESIAN_POINT('Ctrl Pts',(-20.6874624206494,-42.2311878138952,
122.612764298362)) ;
#104803 = CARTESIAN_POINT('Ctrl Pts',(-20.5294874690542,-42.2411811070548,
122.403032653655)) ;
#104804 = CARTESIAN_POINT('Ctrl Pts',(-20.3383117523044,-42.2511321152785,
122.224541202617)) ;
#104805 = CARTESIAN_POINT('Ctrl Pts',(-20.1168527899179,-42.2611806296404,
122.080769292945)) ;
#104806 = CARTESIAN_POINT('Ctrl Pts',(-19.8788671687555,-42.2710221357031,
121.979466983407)) ;
#104807 = CARTESIAN_POINT('Ctrl Pts',(-19.6234113043599,-42.2810077883328,
121.919624716556)) ;
#104808 = CARTESIAN_POINT('Ctrl Pts',(-19.3625935822749,-42.2909467971777,
121.905011062528)) ;
#104809 = CARTESIAN_POINT('Ctrl Pts',(-19.1006128120326,-42.3009877224707,
121.936283706494)) ;
#104810 = CARTESIAN_POINT('Ctrl Pts',(-18.8517403555237,-42.3108780442256,
122.011291662105)) ;
#104811 = CARTESIAN_POINT('Ctrl Pts',(-18.617058468293,-42.320874017559,122.129257065168)) ;
#104812 = CARTESIAN_POINT('Ctrl Pts',(-18.4077464929747,-42.3308054171411,
122.285168774027)) ;
#104813 = CARTESIAN_POINT('Ctrl Pts',(-18.2270758492578,-42.3408109576181,
122.476218167005)) ;
#104814 = CARTESIAN_POINT('Ctrl Pts',(-18.0823406849302,-42.3508439415494,
122.696584921019)) ;
#104815 = CARTESIAN_POINT('Ctrl Pts',(-17.9794776416119,-42.3606995723763,
122.934300246061)) ;
#104816 = CARTESIAN_POINT('Ctrl Pts',(-17.9182607268367,-42.3706989745694,
123.18979755983)) ;
#104817 = CARTESIAN_POINT('Ctrl Pts',(-17.902198858114,-42.3805934439305,
123.449365848482)) ;
#104818 = CARTESIAN_POINT('Ctrl Pts',(-17.932016938791,-42.3906565580947,
123.712081637151)) ;
#104819 = CARTESIAN_POINT('Ctrl Pts',(-18.0050842699126,-42.4004962038111,
123.960163628557)) ;
#104820 = CARTESIAN_POINT('Ctrl Pts',(-18.12239287798,-42.4105593713669,124.197129769659)) ;
#104821 = CARTESIAN_POINT('Ctrl Pts',(-18.2766507483452,-42.4204536271617,
124.406474059086)) ;
#104822 = CARTESIAN_POINT('Ctrl Pts',(-18.4652833345317,-42.4303954056214,
124.587187892246)) ;
#104823 = CARTESIAN_POINT('Ctrl Pts',(-18.6837622031099,-42.4403980984516,
124.733409125687)) ;
#104824 = CARTESIAN_POINT('Ctrl Pts',(-18.9251828526098,-42.4504321204054,
124.839419707781)) ;
#104825 = CARTESIAN_POINT('Ctrl Pts',(-19.1765152614719,-42.4602799114944,
124.901132876178)) ;
#104826 = CARTESIAN_POINT('Ctrl Pts',(-19.4381823082108,-42.4702614360435,
124.919076853109)) ;
#104827 = CARTESIAN_POINT('Ctrl Pts',(-19.6981732583165,-42.4802106595344,
124.891361524154)) ;
#104828 = CARTESIAN_POINT('Ctrl Pts',(-19.9507299142993,-42.490208315751,
124.818885956961)) ;
#104829 = CARTESIAN_POINT('Ctrl Pts',(-20.1876133040232,-42.500248528806,
124.70273061815)) ;
#104830 = CARTESIAN_POINT('Ctrl Pts',(-20.3965851121659,-42.5100765760823,
124.550933160528)) ;
#104831 = CARTESIAN_POINT('Ctrl Pts',(-20.5804323450624,-42.5201309231147,
124.361187474538)) ;
#104832 = CARTESIAN_POINT('Ctrl Pts',(-20.7265203102694,-42.5300720594432,
124.14459996954)) ;
#104833 = CARTESIAN_POINT('Ctrl Pts',(-20.8331238061989,-42.5399762925229,
123.907153791526)) ;
#104834 = CARTESIAN_POINT('Ctrl Pts',(-20.8976296265304,-42.5500229893665,
123.651161969945)) ;
#104835 = CARTESIAN_POINT('Ctrl Pts',(-20.9166605708197,-42.5599185406468,
123.39177211738)) ;
#104836 = CARTESIAN_POINT('Ctrl Pts',(-20.8899295673934,-42.5699806184863,
123.128744028995)) ;
#104837 = CARTESIAN_POINT('Ctrl Pts',(-20.8196282304126,-42.5798233275824,
122.87979426522)) ;
#104838 = CARTESIAN_POINT('Ctrl Pts',(-20.7060650961516,-42.5898140598208,
122.643116802018)) ;
#104839 = CARTESIAN_POINT('Ctrl Pts',(-20.5540301203929,-42.5997420850496,
122.431077814992)) ;
#104840 = CARTESIAN_POINT('Ctrl Pts',(-20.3666760452894,-42.6097302317001,
122.247240006)) ;
#104841 = CARTESIAN_POINT('Ctrl Pts',(-20.1490062279118,-42.6197652495401,
122.098362587121)) ;
#104842 = CARTESIAN_POINT('Ctrl Pts',(-19.9129916906241,-42.6296300466453,
121.991144549183)) ;
#104843 = CARTESIAN_POINT('Ctrl Pts',(-19.6596809800496,-42.6395907790014,
121.925159819885)) ;
#104844 = CARTESIAN_POINT('Ctrl Pts',(-19.3968379506002,-42.6496242413984,
121.904448248065)) ;
#104845 = CARTESIAN_POINT('Ctrl Pts',(-19.1381776310196,-42.6595097756098,
121.928888325179)) ;
#104846 = CARTESIAN_POINT('Ctrl Pts',(-18.8832107613372,-42.6695746162898,
121.999112842521)) ;
#104847 = CARTESIAN_POINT('Ctrl Pts',(-18.6493558817514,-42.6794227480187,
122.11001697531)) ;
#104848 = CARTESIAN_POINT('Ctrl Pts',(-18.4340956755043,-42.6894502450088,
122.26199628503)) ;
#104849 = CARTESIAN_POINT('Ctrl Pts',(-18.2489571690901,-42.6994786970539,
122.449567162524)) ;
#104850 = CARTESIAN_POINT('Ctrl Pts',(-18.1015454019537,-42.709323963618,
122.662170651268)) ;
#104851 = CARTESIAN_POINT('Ctrl Pts',(-17.9910414028632,-42.7193146365589,
122.900334782034)) ;
#104852 = CARTESIAN_POINT('Ctrl Pts',(-17.9238206505132,-42.7293525186474,
123.155408137514)) ;
#104853 = CARTESIAN_POINT('Ctrl Pts',(-17.9018814338395,-42.739196889087,
123.41318653434)) ;
#104854 = CARTESIAN_POINT('Ctrl Pts',(-17.924844360066,-42.7491817164824,
123.674534933171)) ;
#104855 = CARTESIAN_POINT('Ctrl Pts',(-17.9924345358582,-42.7591211618877,
123.926875989498)) ;
#104856 = CARTESIAN_POINT('Ctrl Pts',(-18.1039701355728,-42.7691611661736,
124.165953010271)) ;
#104857 = CARTESIAN_POINT('Ctrl Pts',(-18.2529049853571,-42.7790482753592,
124.378889495216)) ;
#104858 = CARTESIAN_POINT('Ctrl Pts',(-18.4383679788379,-42.7890483352617,
124.565011599206)) ;
#104859 = CARTESIAN_POINT('Ctrl Pts',(-18.6514946875924,-42.7989657511764,
124.715085242335)) ;
#104860 = CARTESIAN_POINT('Ctrl Pts',(-18.8904787338854,-42.8090125659172,
124.827216311811)) ;
#104861 = CARTESIAN_POINT('Ctrl Pts',(-19.1409637043585,-42.8188880431139,
124.89525183759)) ;
#104862 = CARTESIAN_POINT('Ctrl Pts',(-19.4040830147248,-42.8289441388351,
124.919328928823)) ;
#104863 = CARTESIAN_POINT('Ctrl Pts',(-19.6632223451092,-42.8388373008502,
124.897799579971)) ;
#104864 = CARTESIAN_POINT('Ctrl Pts',(-19.9189229517029,-42.8488995368728,
124.830568230373)) ;
#104865 = CARTESIAN_POINT('Ctrl Pts',(-20.1539191213786,-42.8587440025017,
124.722359394121)) ;
#104866 = CARTESIAN_POINT('Ctrl Pts',(-20.3695791509415,-42.8687040952058,
124.574045748429)) ;
#104867 = CARTESIAN_POINT('Ctrl Pts',(-20.5573059185515,-42.8787423841869,
124.388734758303)) ;
#104868 = CARTESIAN_POINT('Ctrl Pts',(-20.7079330225329,-42.8886157072931,
124.177424425734)) ;
#104869 = CARTESIAN_POINT('Ctrl Pts',(-20.8217253254102,-42.8986888913782,
123.938476998425)) ;
#104870 = CARTESIAN_POINT('Ctrl Pts',(-20.8908827499387,-42.9085094036661,
123.689783809996)) ;
#104871 = CARTESIAN_POINT('Ctrl Pts',(-20.9167041508658,-42.9185873997819,
123.426269445096)) ;
#104872 = CARTESIAN_POINT('Ctrl Pts',(-20.8968822449302,-42.9284414747652,
123.168014102348)) ;
#104873 = CARTESIAN_POINT('Ctrl Pts',(-20.8314569368461,-42.9385053563489,
122.911818705928)) ;
#104874 = CARTESIAN_POINT('Ctrl Pts',(-20.7244115567648,-42.9483887823227,
122.675128176596)) ;
#104875 = CARTESIAN_POINT('Ctrl Pts',(-20.5765556238842,-42.9583893862437,
122.45791601346)) ;
#104876 = CARTESIAN_POINT('Ctrl Pts',(-20.3947650338374,-42.9683091705816,
122.271014843434)) ;
#104877 = CARTESIAN_POINT('Ctrl Pts',(-20.1806024800397,-42.9783565209384,
122.116660959539)) ;
#104878 = CARTESIAN_POINT('Ctrl Pts',(-19.9469622159444,-42.9882338631727,
122.003462045273)) ;
#104879 = CARTESIAN_POINT('Ctrl Pts',(-19.6924449489111,-42.9983037442474,
121.931213874839)) ;
#104880 = CARTESIAN_POINT('Ctrl Pts',(-19.4354546046545,-43.008133449449,
121.904618856356)) ;
#104881 = CARTESIAN_POINT('Ctrl Pts',(-19.1716059344272,-43.0182001106154,
121.923134771065)) ;
#104882 = CARTESIAN_POINT('Ctrl Pts',(-18.9194441886432,-43.0280903324827,
121.986237501983)) ;
#104883 = CARTESIAN_POINT('Ctrl Pts',(-18.6794320360846,-43.0380825085929,
122.092711334672)) ;
#104884 = CARTESIAN_POINT('Ctrl Pts',(-18.4623247536949,-43.0480453387055,
122.239022821817)) ;
#104885 = CARTESIAN_POINT('Ctrl Pts',(-18.2745479615962,-43.0579495511058,
122.419282436697)) ;
#104886 = CARTESIAN_POINT('Ctrl Pts',(-18.1187192118051,-43.0680102651937,
122.632820549184)) ;
#104887 = CARTESIAN_POINT('Ctrl Pts',(-18.0045425253802,-43.0778497681765,
122.864864491798)) ;
#104888 = CARTESIAN_POINT('Ctrl Pts',(-17.9304931125037,-43.0879159067429,
123.118771690062)) ;
#104889 = CARTESIAN_POINT('Ctrl Pts',(-17.9022688621809,-43.0977984212289,
123.376975393947)) ;
#104890 = CARTESIAN_POINT('Ctrl Pts',(-17.9189748412503,-43.1077907205845,
123.638990434993)) ;
#104891 = CARTESIAN_POINT('Ctrl Pts',(-17.980632945577,-43.1177437875379,
123.89321577407)) ;
#104892 = CARTESIAN_POINT('Ctrl Pts',(-18.0864334578628,-43.1277784957431,
124.134740590676)) ;
#104893 = CARTESIAN_POINT('Ctrl Pts',(-18.2302918456432,-43.1376667166473,
124.35115739606)) ;
#104894 = CARTESIAN_POINT('Ctrl Pts',(-18.4111337778499,-43.1476611396777,
124.54160421321)) ;
#104895 = CARTESIAN_POINT('Ctrl Pts',(-18.6213333522746,-43.1576064791239,
124.696916870791)) ;
#104896 = CARTESIAN_POINT('Ctrl Pts',(-18.8551254938992,-43.1675538237352,
124.813883031266)) ;
#104897 = CARTESIAN_POINT('Ctrl Pts',(-19.1082720190948,-43.1776017191462,
124.888940157989)) ;
#104898 = CARTESIAN_POINT('Ctrl Pts',(-19.3653633267677,-43.1874493646256,
124.918525063394)) ;
#104899 = CARTESIAN_POINT('Ctrl Pts',(-19.6267119617915,-43.1974110785396,
124.903661025087)) ;
#104900 = CARTESIAN_POINT('Ctrl Pts',(-19.8831726151699,-43.2074397028305,
124.842909625161)) ;
#104901 = CARTESIAN_POINT('Ctrl Pts',(-20.1223420758362,-43.2173500634872,
124.739869624029)) ;
#104902 = CARTESIAN_POINT('Ctrl Pts',(-20.3409183277363,-43.2272847620605,
124.597079858644)) ;
#104903 = CARTESIAN_POINT('Ctrl Pts',(-20.5332396283574,-43.2373265869147,
124.416406754811)) ;
#104904 = CARTESIAN_POINT('Ctrl Pts',(-20.6889998581201,-43.2472111606591,
124.20850068406)) ;
#104905 = CARTESIAN_POINT('Ctrl Pts',(-20.8079393724832,-43.2572130100223,
123.974153556956)) ;
#104906 = CARTESIAN_POINT('Ctrl Pts',(-20.8839549135246,-43.2671323115963,
123.724778206695)) ;
#104907 = CARTESIAN_POINT('Ctrl Pts',(-20.9159120162296,-43.2771764199416,
123.462793249305)) ;
#104908 = CARTESIAN_POINT('Ctrl Pts',(-20.9021938783438,-43.2870608433839,
123.203391169595)) ;
#104909 = CARTESIAN_POINT('Ctrl Pts',(-20.8434325546442,-43.2970772052933,
122.946804609188)) ;
#104910 = CARTESIAN_POINT('Ctrl Pts',(-20.7401748840849,-43.3071138607987,
122.704120206209)) ;
#104911 = CARTESIAN_POINT('Ctrl Pts',(-20.5998726346924,-43.316943990988,
122.487178184028)) ;
#104912 = CARTESIAN_POINT('Ctrl Pts',(-20.4197573959054,-43.3270200440779,
122.293157016589)) ;
#104913 = CARTESIAN_POINT('Ctrl Pts',(-20.2133796379951,-43.3368722732637,
122.136730156183)) ;
#104914 = CARTESIAN_POINT('Ctrl Pts',(-19.9779977934411,-43.346945481063,
122.015709849871)) ;
#104915 = CARTESIAN_POINT('Ctrl Pts',(-19.7309152909117,-43.3567869924144,
121.939250075785)) ;
#104916 = CARTESIAN_POINT('Ctrl Pts',(-19.4713473599111,-43.3667479304519,
121.905485975715)) ;
#104917 = CARTESIAN_POINT('Ctrl Pts',(-19.2078648410812,-43.3767857923769,
121.917923560275)) ;
#104918 = CARTESIAN_POINT('Ctrl Pts',(-18.9545933568594,-43.386659978374,
121.974511790238)) ;
#104919 = CARTESIAN_POINT('Ctrl Pts',(-18.7103144862265,-43.3967301379519,
122.076190688667)) ;
#104920 = CARTESIAN_POINT('Ctrl Pts',(-18.4925372665596,-43.4065618853777,
122.215260760015)) ;
#104921 = CARTESIAN_POINT('Ctrl Pts',(-18.2978258112365,-43.416597965449,
122.393131044889)) ;
#104922 = CARTESIAN_POINT('Ctrl Pts',(-18.1377717670256,-43.4266150123015,
122.602137878926)) ;
#104923 = CARTESIAN_POINT('Ctrl Pts',(-18.0176420342896,-43.4364972704681,
122.832383191886)) ;
#104924 = CARTESIAN_POINT('Ctrl Pts',(-17.9382017148114,-43.4464849532645,
123.082509715295)) ;
#104925 = CARTESIAN_POINT('Ctrl Pts',(-17.9033225321258,-43.4564316099812,
123.341600746611)) ;
#104926 = CARTESIAN_POINT('Ctrl Pts',(-17.9143468061501,-43.4664886680613,
123.605630312253)) ;
#104927 = CARTESIAN_POINT('Ctrl Pts',(-17.9693606834189,-43.4763068476108,
123.857723199161)) ;
#104928 = CARTESIAN_POINT('Ctrl Pts',(-18.068813138395,-43.4863427820498,
124.101979443464)) ;
#104929 = CARTESIAN_POINT('Ctrl Pts',(-18.2096563573265,-43.4963674364788,
124.324617133283)) ;
#104930 = CARTESIAN_POINT('Ctrl Pts',(-18.3835357390967,-43.5062194560583,
124.516444902272)) ;
#104931 = CARTESIAN_POINT('Ctrl Pts',(-18.5906910966535,-43.5162103697732,
124.677699425909)) ;
#104932 = CARTESIAN_POINT('Ctrl Pts',(-18.8209814559814,-43.5261283586128,
124.799818206441)) ;
#104933 = CARTESIAN_POINT('Ctrl Pts',(-19.0716619099763,-43.5361564693436,
124.881031637692)) ;
#104934 = CARTESIAN_POINT('Ctrl Pts',(-19.3289275583956,-43.546041667252,
124.91707739968)) ;
#104935 = CARTESIAN_POINT('Ctrl Pts',(-19.5913007390015,-43.55603094252,124.90845061953)) ;
#104936 = CARTESIAN_POINT('Ctrl Pts',(-19.8494016769146,-43.5660724006895,
124.853560006416)) ;
#104937 = CARTESIAN_POINT('Ctrl Pts',(-20.089126965417,-43.5759038644778,
124.757190574389)) ;
#104938 = CARTESIAN_POINT('Ctrl Pts',(-20.3126215899426,-43.5859087967817,
124.618769996767)) ;
#104939 = CARTESIAN_POINT('Ctrl Pts',(-20.5082846379011,-43.5958951606764,
124.443812980393)) ;
#104940 = CARTESIAN_POINT('Ctrl Pts',(-20.6710952998736,-43.6059247895623,
124.236573038023)) ;
#104941 = CARTESIAN_POINT('Ctrl Pts',(-20.7938534841655,-43.6158000116707,
124.007904553605)) ;
#104942 = CARTESIAN_POINT('Ctrl Pts',(-20.8763533612149,-43.6258012240678,
123.758410827057)) ;
#104943 = CARTESIAN_POINT('Ctrl Pts',(-20.914185635291,-43.6357098033033,
123.500740267426)) ;
#104944 = CARTESIAN_POINT('Ctrl Pts',(-20.9065152821478,-43.6457646558593,
123.236663666246)) ;
#104945 = CARTESIAN_POINT('Ctrl Pts',(-20.8544254443002,-43.6556232381341,
122.982834271091)) ;
#104946 = CARTESIAN_POINT('Ctrl Pts',(-20.7572075900671,-43.6656913675768,
122.736804469327)) ;
#104947 = CARTESIAN_POINT('Ctrl Pts',(-20.6216226854685,-43.6755468392659,
122.516112932406)) ;
#104948 = CARTESIAN_POINT('Ctrl Pts',(-20.4479582876326,-43.6855416876521,
122.319076542541)) ;
#104949 = CARTESIAN_POINT('Ctrl Pts',(-20.2416064978002,-43.6955729844366,
122.155024885299)) ;
#104950 = CARTESIAN_POINT('Ctrl Pts',(-20.0139042025043,-43.7054395206467,
122.030994761445)) ;
#104951 = CARTESIAN_POINT('Ctrl Pts',(-19.7652860328304,-43.7154269436075,
121.946983535015)) ;
#104952 = CARTESIAN_POINT('Ctrl Pts',(-19.5069160345804,-43.7253718826273,
121.907441269783)) ;
#104953 = CARTESIAN_POINT('Ctrl Pts',(-19.2430357316301,-43.7354167684873,
121.913545634588)) ;
#104954 = CARTESIAN_POINT('Ctrl Pts',(-18.9887149200403,-43.7452853035735,
121.964332757131)) ;
#104955 = CARTESIAN_POINT('Ctrl Pts',(-18.7444455097126,-43.7552511715802,
122.05874888763)) ;
#104956 = CARTESIAN_POINT('Ctrl Pts',(-18.5191315338864,-43.7652738190327,
122.195184429335)) ;
#104957 = CARTESIAN_POINT('Ctrl Pts',(-18.3228637036449,-43.7751974580403,
122.366880554806)) ;
#104958 = CARTESIAN_POINT('Ctrl Pts',(-18.1585688776028,-43.785140183046,
122.570066593669)) ;
#104959 = CARTESIAN_POINT('Ctrl Pts',(-18.0310320495463,-43.7951857890979,
122.801185890142)) ;
#104960 = CARTESIAN_POINT('Ctrl Pts',(-17.9468480696797,-43.805047211619,
123.046302545055)) ;
#104961 = CARTESIAN_POINT('Ctrl Pts',(-17.9055287972533,-43.8150407800682,
123.305614180194)) ;
#104962 = CARTESIAN_POINT('Ctrl Pts',(-17.9096981897941,-43.8249662508235,
123.566450318182)) ;
#104963 = CARTESIAN_POINT('Ctrl Pts',(-17.959577021804,-43.8349939247794,
123.825170364264)) ;
#104964 = CARTESIAN_POINT('Ctrl Pts',(-18.0520913255646,-43.8448811028211,
124.068003666983)) ;
#104965 = CARTESIAN_POINT('Ctrl Pts',(-18.1870726266539,-43.8549094821892,
124.29430476118)) ;
#104966 = CARTESIAN_POINT('Ctrl Pts',(-18.356931127565,-43.8648037249107,
124.491207973471)) ;
#104967 = CARTESIAN_POINT('Ctrl Pts',(-18.6285761936577,-43.8781566415616,
124.713286249922)) ;
#104968 = CARTESIAN_POINT('Ctrl Pts',(-18.948383164132,-43.8913591593083,
124.857812283669)) ;
#104969 = CARTESIAN_POINT('Ctrl Pts',(-19.2946498883519,-43.9047150645893,
124.914940485275)) ;
#104970 = CARTESIAN_POINT('Ctrl Pts',(-19.5547438289061,-43.9146117132271,
124.912309586641)) ;
#104971 = CARTESIAN_POINT('Ctrl Pts',(-19.8143049394651,-43.9246598512796,
124.863922492952)) ;
#104972 = CARTESIAN_POINT('Ctrl Pts',(-20.0576815747362,-43.9345508114574,
124.77263287154)) ;
#104973 = CARTESIAN_POINT('Ctrl Pts',(-20.2841489081808,-43.9445436473341,
124.639680505844)) ;
#104974 = CARTESIAN_POINT('Ctrl Pts',(-20.4846062456997,-43.9545827423357,
124.468189074761)) ;
#104975 = CARTESIAN_POINT('Ctrl Pts',(-20.6493647056431,-43.9644200981869,
124.268942295104)) ;
#104976 = CARTESIAN_POINT('Ctrl Pts',(-20.8232997802523,-43.9778130461176,
123.96303203667)) ;
#104977 = CARTESIAN_POINT('Ctrl Pts',(-20.9119483564918,-43.9909797225445,
123.624406077728)) ;
#104978 = CARTESIAN_POINT('Ctrl Pts',(-20.910325463326,-44.0043645039513,
123.272727081459)) ;
#104979 = CARTESIAN_POINT('Ctrl Pts',(-20.864238880758,-44.0142262865952,
123.01765838927)) ;
#104980 = CARTESIAN_POINT('Ctrl Pts',(-20.7737497681902,-44.0242254345482,
122.771019118975)) ;
#104981 = CARTESIAN_POINT('Ctrl Pts',(-20.6432368005239,-44.0341282271653,
122.545814143778)) ;
#104982 = CARTESIAN_POINT('Ctrl Pts',(-20.4731399955561,-44.0441778070562,
122.343878608251)) ;
#104983 = CARTESIAN_POINT('Ctrl Pts',(-20.2076059725452,-44.0573648808657,
122.121012079082)) ;
#104984 = CARTESIAN_POINT('Ctrl Pts',(-19.8041322252334,-44.0741176708369,
121.933097855495)) ;
#104985 = CARTESIAN_POINT('Ctrl Pts',(-19.3673869325287,-44.0906063229316,
121.894835933027)) ;
#104986 = CARTESIAN_POINT('Ctrl Pts',(-19.0216674963533,-44.103963149115,
121.955027343524)) ;
#104987 = CARTESIAN_POINT('Ctrl Pts',(-18.7770005207847,-44.1138595339929,
122.043352858125)) ;
#104988 = CARTESIAN_POINT('Ctrl Pts',(-18.5489164371702,-44.1238660485134,
122.17407896693)) ;
#104989 = CARTESIAN_POINT('Ctrl Pts',(-18.2820370334625,-44.1370561720298,
122.395456324411)) ;
#104990 = CARTESIAN_POINT('Ctrl Pts',(-18.0248472685587,-44.1538227331793,
122.759183838279)) ;
#104991 = CARTESIAN_POINT('Ctrl Pts',(-17.886054152953,-44.1736072218874,
123.266528761718)) ;
#104992 = CARTESIAN_POINT('Ctrl Pts',(-17.9274102999763,-44.1935526694839,
123.794897481469)) ;
#104993 = CARTESIAN_POINT('Ctrl Pts',(-18.1467356431328,-44.2134643316398,
124.276542042476)) ;
#104994 = CARTESIAN_POINT('Ctrl Pts',(-18.5161061142021,-44.2333565236587,
124.654929487936)) ;
#104995 = CARTESIAN_POINT('Ctrl Pts',(-18.9962004191449,-44.2533976542133,
124.885489162055)) ;
#104996 = CARTESIAN_POINT('Ctrl Pts',(-19.5204345314535,-44.2732159888289,
124.938089811446)) ;
#104997 = CARTESIAN_POINT('Ctrl Pts',(-20.0350360289523,-44.2931885540485,
124.808536609141)) ;
#104998 = CARTESIAN_POINT('Ctrl Pts',(-20.473093222117,-44.3130777702201,
124.512295701165)) ;
#104999 = CARTESIAN_POINT('Ctrl Pts',(-20.7853732663462,-44.3331013445428,
124.08151681092)) ;
#105000 = CARTESIAN_POINT('Ctrl Pts',(-20.9306784904965,-44.352898507631,
123.575705617938)) ;
#105001 = CARTESIAN_POINT('Ctrl Pts',(-20.8956409075036,-44.3728640014548,
123.046325488981)) ;
#105002 = CARTESIAN_POINT('Ctrl Pts',(-20.681482209836,-44.3928177091962,
122.560997313909)) ;
#105003 = CARTESIAN_POINT('Ctrl Pts',(-20.3156124672634,-44.4127250859228,
122.178943118097)) ;
#105004 = CARTESIAN_POINT('Ctrl Pts',(-19.8430851406969,-44.4325772974714,
121.94396651336)) ;
#105005 = CARTESIAN_POINT('Ctrl Pts',(-19.3129697699881,-44.4526496844171,
121.88421408573)) ;
#105006 = CARTESIAN_POINT('Ctrl Pts',(-18.8004875339095,-44.4724875540574,
122.008175589583)) ;
#105007 = CARTESIAN_POINT('Ctrl Pts',(-18.3595296194666,-44.4923382086105,
122.297851154628)) ;
#105008 = CARTESIAN_POINT('Ctrl Pts',(-18.0413388756731,-44.512390142951,
122.725336395254)) ;
#105009 = CARTESIAN_POINT('Ctrl Pts',(-17.8898208181151,-44.532223330517,
123.23034909197)) ;
#105010 = CARTESIAN_POINT('Ctrl Pts',(-17.9188074653872,-44.5521525427477,
123.759044469505)) ;
#105011 = CARTESIAN_POINT('Ctrl Pts',(-18.1255875324458,-44.5720375079621,
124.245643141328)) ;
#105012 = CARTESIAN_POINT('Ctrl Pts',(-18.4898169288741,-44.5921112491067,
124.635352509745)) ;
#105013 = CARTESIAN_POINT('Ctrl Pts',(-18.9586647938728,-44.6119044308871,
124.874137361605)) ;
#105014 = CARTESIAN_POINT('Ctrl Pts',(-19.4850008685489,-44.6318671388898,
124.940732867098)) ;
#105015 = CARTESIAN_POINT('Ctrl Pts',(-20.0027588463674,-44.6518500906322,
124.822336742244)) ;
#105016 = CARTESIAN_POINT('Ctrl Pts',(-20.4457804417171,-44.6716607104044,
124.537702205694)) ;
#105017 = CARTESIAN_POINT('Ctrl Pts',(-20.7682682433341,-44.6916444264373,
124.115825296363)) ;
#105018 = CARTESIAN_POINT('Ctrl Pts',(-20.9266119031138,-44.7115258903346,
123.611552263103)) ;
#105019 = CARTESIAN_POINT('Ctrl Pts',(-20.9036659950878,-44.731481220179,
123.08177562687)) ;
#105020 = CARTESIAN_POINT('Ctrl Pts',(-20.7024070889565,-44.7513566809845,
122.593268939263)) ;
#105021 = CARTESIAN_POINT('Ctrl Pts',(-20.3449059579803,-44.771341001036,
122.200518916191)) ;
#105022 = CARTESIAN_POINT('Ctrl Pts',(-19.8758735906964,-44.7912690338256,
121.954214849087)) ;
#105023 = CARTESIAN_POINT('Ctrl Pts',(-19.438578805638,-44.8078777957654,
121.894601445144)) ;
#105024 = CARTESIAN_POINT('Ctrl Pts',(-19.0946773195498,-44.8210654344555,
121.9376322726)) ;
#105025 = CARTESIAN_POINT('Ctrl Pts',(-18.8437209444758,-44.8310518688156,
122.014347849568)) ;
#105026 = CARTESIAN_POINT('Ctrl Pts',(-18.6094583387565,-44.841061242775,
122.133996670007)) ;
#105027 = CARTESIAN_POINT('Ctrl Pts',(-18.3305913715183,-44.8543512763403,
122.344268776071)) ;
#105028 = CARTESIAN_POINT('Ctrl Pts',(-18.0587975390607,-44.8709452640027,
122.691629909638)) ;
#105029 = CARTESIAN_POINT('Ctrl Pts',(-17.9215519402964,-44.8875775192782,
123.111821893515)) ;
#105030 = CARTESIAN_POINT('Ctrl Pts',(-17.9026701922283,-44.9008199029461,
123.459315264525)) ;
#105031 = CARTESIAN_POINT('Ctrl Pts',(-17.9331210763156,-44.9107341111735,
123.718074029776)) ;
#105032 = CARTESIAN_POINT('Ctrl Pts',(-18.0093944626743,-44.9207907504452,
123.971085550191)) ;
#105033 = CARTESIAN_POINT('Ctrl Pts',(-18.1256855379854,-44.9306365568653,
124.202241165926)) ;
#105034 = CARTESIAN_POINT('Ctrl Pts',(-18.2830906349234,-44.9406815564985,
124.414133633977)) ;
#105035 = CARTESIAN_POINT('Ctrl Pts',(-18.5370488897799,-44.9539625788713,
124.653520523732)) ;
#105036 = CARTESIAN_POINT('Ctrl Pts',(-18.8452706151881,-44.9671600253959,
124.820978374713)) ;
#105037 = CARTESIAN_POINT('Ctrl Pts',(-19.1881208578501,-44.9805743232029,
124.903002035483)) ;
#105038 = CARTESIAN_POINT('Ctrl Pts',(-19.4462158275204,-44.9904133886056,
124.918740428839)) ;
#105039 = CARTESIAN_POINT('Ctrl Pts',(-19.7069222802875,-45.0003965948833,
124.889687530317)) ;
#105040 = CARTESIAN_POINT('Ctrl Pts',(-19.9578337616693,-45.0103478297961,
124.815948358153)) ;
#105041 = CARTESIAN_POINT('Ctrl Pts',(-20.1934407068406,-45.0203488294977,
124.699467451423)) ;
#105042 = CARTESIAN_POINT('Ctrl Pts',(-20.4056291656955,-45.0303801752851,
124.543050170843)) ;
#105043 = CARTESIAN_POINT('Ctrl Pts',(-20.5844817934518,-45.0402339399901,
124.355784465079)) ;
#105044 = CARTESIAN_POINT('Ctrl Pts',(-20.730306116653,-45.0502045936584,
124.138128056574)) ;
#105045 = CARTESIAN_POINT('Ctrl Pts',(-20.8364235167749,-45.0602018373156,
123.897752942443)) ;
#105046 = CARTESIAN_POINT('Ctrl Pts',(-20.8990754352481,-45.0702352932598,
123.641658311866)) ;
#105047 = CARTESIAN_POINT('Ctrl Pts',(-20.9164257862816,-45.0800907975602,
123.383222452894)) ;
#105048 = CARTESIAN_POINT('Ctrl Pts',(-20.8885903520797,-45.0900902338463,
123.121973185214)) ;
#105049 = CARTESIAN_POINT('Ctrl Pts',(-20.8168393384412,-45.0999846933622,
122.872001936455)) ;
#105050 = CARTESIAN_POINT('Ctrl Pts',(-20.7008020992867,-45.1100478128138,
122.634422440595)) ;
#105051 = CARTESIAN_POINT('Ctrl Pts',(-20.5489090568532,-45.1198874472258,
122.425109333317)) ;
#105052 = CARTESIAN_POINT('Ctrl Pts',(-20.3590464678608,-45.1299506547116,
122.241080148602)) ;
#105053 = CARTESIAN_POINT('Ctrl Pts',(-20.143616765248,-45.1398447620908,
122.095446265196)) ;
#105054 = CARTESIAN_POINT('Ctrl Pts',(-19.90536102435,-45.1497870942832,121.988302155594)) ;
#105055 = CARTESIAN_POINT('Ctrl Pts',(-19.6505929754798,-45.1597877205982,
121.923634229427)) ;
#105056 = CARTESIAN_POINT('Ctrl Pts',(-19.3874182812413,-45.1698294548801,
121.904600717031)) ;
#105057 = CARTESIAN_POINT('Ctrl Pts',(-19.1304894002943,-45.1796548808292,
121.930404916149)) ;
#105058 = CARTESIAN_POINT('Ctrl Pts',(-18.8760225613039,-45.1897117073569,
122.001688985524)) ;
#105059 = CARTESIAN_POINT('Ctrl Pts',(-18.6409922371268,-45.1996391404784,
122.114947366633)) ;
#105060 = CARTESIAN_POINT('Ctrl Pts',(-18.428283078681,-45.2095891328847,
122.267030398883)) ;
#105061 = CARTESIAN_POINT('Ctrl Pts',(-18.2436293548006,-45.2196443339587,
122.456017242193)) ;
#105062 = CARTESIAN_POINT('Ctrl Pts',(-18.0976408516097,-45.229466608011,
122.66891028545)) ;
#105063 = CARTESIAN_POINT('Ctrl Pts',(-17.9878817132479,-45.2395225019702,
122.909275777523)) ;
#105064 = CARTESIAN_POINT('Ctrl Pts',(-17.9227281996274,-45.2494632238153,
123.162262403673)) ;
#105065 = CARTESIAN_POINT('Ctrl Pts',(-17.9017528415054,-45.2593675679019,
123.421696578876)) ;
#105066 = CARTESIAN_POINT('Ctrl Pts',(-17.9266573662769,-45.2694142352014,
123.684512768429)) ;
#105067 = CARTESIAN_POINT('Ctrl Pts',(-17.9955501165954,-45.2793097936513,
123.935309673887)) ;
#105068 = CARTESIAN_POINT('Ctrl Pts',(-18.1087830964484,-45.289371872356,
124.174216936959)) ;
#105069 = CARTESIAN_POINT('Ctrl Pts',(-18.258360118383,-45.2992145708218,
124.385273109242)) ;
#105070 = CARTESIAN_POINT('Ctrl Pts',(-18.4445967016622,-45.3092053447163,
124.570285917934)) ;
#105071 = CARTESIAN_POINT('Ctrl Pts',(-18.6588336632447,-45.3191332139512,
124.719195960976)) ;
#105072 = CARTESIAN_POINT('Ctrl Pts',(-18.8969306208894,-45.329121942921,
124.829738528518)) ;
#105073 = CARTESIAN_POINT('Ctrl Pts',(-19.1519909533467,-45.3391613449048,
124.89712446642)) ;
#105074 = CARTESIAN_POINT('Ctrl Pts',(-19.4096451598501,-45.3490015126416,
124.919272539632)) ;
#105075 = CARTESIAN_POINT('Ctrl Pts',(-19.6726846522424,-45.3590497230161,
124.896250057788)) ;
#105076 = CARTESIAN_POINT('Ctrl Pts',(-19.9250744800764,-45.3689968933038,
124.828188273529)) ;
#105077 = CARTESIAN_POINT('Ctrl Pts',(-20.161282054125,-45.3789077415589,
124.718447480095)) ;
#105078 = CARTESIAN_POINT('Ctrl Pts',(-20.3778191542026,-45.3889640692367,
124.566982119744)) ;
#105079 = CARTESIAN_POINT('Ctrl Pts',(-20.561118268851,-45.3988144820052,
124.384182606979)) ;
#105080 = CARTESIAN_POINT('Ctrl Pts',(-20.7130730814684,-45.4088413678389,
124.168919868791)) ;
#105081 = CARTESIAN_POINT('Ctrl Pts',(-20.8247497780107,-45.4188699834697,
123.930196528526)) ;
#105082 = CARTESIAN_POINT('Ctrl Pts',(-20.8924915813861,-45.4287152068472,
123.680514258014)) ;
#105083 = CARTESIAN_POINT('Ctrl Pts',(-20.9169002130611,-45.4387058889488,
123.419099763425)) ;
#105084 = CARTESIAN_POINT('Ctrl Pts',(-20.8948617738519,-45.4487437775813,
123.156239641148)) ;
#105085 = CARTESIAN_POINT('Ctrl Pts',(-20.8292495192011,-45.4585881126844,
122.905988466619)) ;
#105086 = CARTESIAN_POINT('Ctrl Pts',(-20.7201268218568,-45.4685730748819,
122.667400439687)) ;
#105087 = CARTESIAN_POINT('Ctrl Pts',(-20.5719794951113,-45.4785120164153,
122.45224941859)) ;
#105088 = CARTESIAN_POINT('Ctrl Pts',(-20.3868125283129,-45.4885539013867,
122.264265761858)) ;
#105089 = CARTESIAN_POINT('Ctrl Pts',(-20.1751991039344,-45.498440449295,
122.11348960682)) ;
#105090 = CARTESIAN_POINT('Ctrl Pts',(-19.9382932298207,-45.508434374795,
122.000209516617)) ;
#105091 = CARTESIAN_POINT('Ctrl Pts',(-19.6867430666025,-45.5183704659215,
121.930054267057)) ;
#105092 = CARTESIAN_POINT('Ctrl Pts',(-19.4244653461354,-45.5283997349014,
121.904461919994)) ;
#105093 = CARTESIAN_POINT('Ctrl Pts',(-19.1654769790705,-45.5382821174607,
121.924176829305)) ;
#105094 = CARTESIAN_POINT('Ctrl Pts',(-18.9095701072339,-45.5483346345486,
121.989564875615)) ;
#105095 = CARTESIAN_POINT('Ctrl Pts',(-18.6725611805939,-45.5582287553725,
122.096593974873)) ;
#105096 = CARTESIAN_POINT('Ctrl Pts',(-18.454122249887,-45.5682907347929,
122.245538250937)) ;
#105097 = CARTESIAN_POINT('Ctrl Pts',(-18.2689013297403,-45.5781352680218,
122.426165536045)) ;
#105098 = CARTESIAN_POINT('Ctrl Pts',(-18.1153278593355,-45.5880953469281,
122.638111849472)) ;
#105099 = CARTESIAN_POINT('Ctrl Pts',(-18.0004594417563,-45.5981336235007,
122.875570696473)) ;
#105100 = CARTESIAN_POINT('Ctrl Pts',(-17.9292550530874,-45.6080070100386,
123.125112116281)) ;
#105101 = CARTESIAN_POINT('Ctrl Pts',(-17.9020057930579,-45.6180799528056,
123.388361038033)) ;
#105102 = CARTESIAN_POINT('Ctrl Pts',(-17.9201003440477,-45.6279013669339,
123.645873411878)) ;
#105103 = CARTESIAN_POINT('Ctrl Pts',(-17.9839117490165,-45.6379759970062,
123.902769129534)) ;
#105104 = CARTESIAN_POINT('Ctrl Pts',(-18.0892730735631,-45.6478426343231,
124.139717934225)) ;
#105105 = CARTESIAN_POINT('Ctrl Pts',(-18.2358937929281,-45.6578661796949,
124.358532526418)) ;
#105106 = CARTESIAN_POINT('Ctrl Pts',(-18.4187982736359,-45.6678919312121,
124.548186844112)) ;
#105107 = CARTESIAN_POINT('Ctrl Pts',(-18.6279179687575,-45.6777455182215,
124.70087294293)) ;
#105108 = CARTESIAN_POINT('Ctrl Pts',(-18.8629921401903,-45.6877224784494,
124.816991235765)) ;
#105109 = CARTESIAN_POINT('Ctrl Pts',(-19.1158783884608,-45.6977436214779,
124.89042196862)) ;
#105110 = CARTESIAN_POINT('Ctrl Pts',(-19.3740455309343,-45.7076262274978,
124.918960029226)) ;
#105111 = CARTESIAN_POINT('Ctrl Pts',(-19.6380339189301,-45.7176946981305,
124.901825038415)) ;
#105112 = CARTESIAN_POINT('Ctrl Pts',(-19.8891097184639,-45.7275247813142,
124.840868485324)) ;
#105113 = CARTESIAN_POINT('Ctrl Pts',(-20.1315378133277,-45.7375913409946,
124.735100678908)) ;
#105114 = CARTESIAN_POINT('Ctrl Pts',(-20.3480312971626,-45.7474815908238,
124.591231930884)) ;
#105115 = CARTESIAN_POINT('Ctrl Pts',(-20.5385576486232,-45.7574737565726,
124.410560471012)) ;
#105116 = CARTESIAN_POINT('Ctrl Pts',(-20.6941656126137,-45.7674366001687,
124.200016201695)) ;
#105117 = CARTESIAN_POINT('Ctrl Pts',(-20.8107718164535,-45.7773407689965,
123.967301371836)) ;
#105118 = CARTESIAN_POINT('Ctrl Pts',(-20.8861323700367,-45.7874016438908,
123.713916570777)) ;
#105119 = CARTESIAN_POINT('Ctrl Pts',(-20.9160536921598,-45.7972405472202,
123.457055277836)) ;
#105120 = CARTESIAN_POINT('Ctrl Pts',(-20.9008271947572,-45.8073089235941,
123.192950934259)) ;
#105121 = CARTESIAN_POINT('Ctrl Pts',(-20.8410053145688,-45.8171895402267,
122.940244040831)) ;
#105122 = CARTESIAN_POINT('Ctrl Pts',(-20.7375809204795,-45.8271807004557,
122.698956739296)) ;
#105123 = CARTESIAN_POINT('Ctrl Pts',(-20.5943728761297,-45.8371337738878,
122.48004171132)) ;
#105124 = CARTESIAN_POINT('Ctrl Pts',(-20.4138196588889,-45.8471696095005,
122.287835517682)) ;
#105125 = CARTESIAN_POINT('Ctrl Pts',(-20.2057772654205,-45.8570597362306,
122.132027016977)) ;
#105126 = CARTESIAN_POINT('Ctrl Pts',(-19.9716662871303,-45.8670519179999,
122.013135288899)) ;
#105127 = CARTESIAN_POINT('Ctrl Pts',(-19.7215916075349,-45.8769978579744,
121.937133118513)) ;
#105128 = CARTESIAN_POINT('Ctrl Pts',(-19.4621372390162,-45.8869450417339,
121.905174548949)) ;
#105129 = CARTESIAN_POINT('Ctrl Pts',(-19.1984689476946,-45.8969929800242,
121.919182730932)) ;
#105130 = CARTESIAN_POINT('Ctrl Pts',(-18.9463055895591,-45.9068406148377,
121.977361332279)) ;
#105131 = CARTESIAN_POINT('Ctrl Pts',(-18.7050086728077,-45.9168023285357,
122.078849493128)) ;
#105132 = CARTESIAN_POINT('Ctrl Pts',(-18.4836777713451,-45.9268309643569,
122.22194223654)) ;
#105133 = CARTESIAN_POINT('Ctrl Pts',(-18.2927960619033,-45.9367412791087,
122.399094647672)) ;
#105134 = CARTESIAN_POINT('Ctrl Pts',(-18.1346245699497,-45.9466761497713,
122.606816266762)) ;
#105135 = CARTESIAN_POINT('Ctrl Pts',(-18.0138763110192,-45.9567173321731,
122.841426333629)) ;
#105136 = CARTESIAN_POINT('Ctrl Pts',(-17.9366880133725,-45.9666043036378,
123.089539209515)) ;
#105137 = CARTESIAN_POINT('Ctrl Pts',(-17.903054057272,-45.9766037359004,
123.350118250912)) ;
#105138 = CARTESIAN_POINT('Ctrl Pts',(-17.9149071079887,-45.986523801157,
123.61056930821)) ;
#105139 = CARTESIAN_POINT('Ctrl Pts',(-17.9724111669176,-45.9965606537412,
123.867967455661)) ;
#105140 = CARTESIAN_POINT('Ctrl Pts',(-18.0724951338109,-46.0064733130812,
124.108473552812)) ;
#105141 = CARTESIAN_POINT('Ctrl Pts',(-18.2134549140274,-46.0164645249961,
124.33000369932)) ;
#105142 = CARTESIAN_POINT('Ctrl Pts',(-18.392045730638,-46.0265061663992,
124.5242428558)) ;
#105143 = CARTESIAN_POINT('Ctrl Pts',(-18.5968569497117,-46.0363349606062,
124.681674981038)) ;
#105144 = CARTESIAN_POINT('Ctrl Pts',(-18.8315310091888,-46.0464113717275,
124.804221895689)) ;
#105145 = CARTESIAN_POINT('Ctrl Pts',(-19.0783635224015,-46.05626350477,124.882541551475)) ;
#105146 = CARTESIAN_POINT('Ctrl Pts',(-19.3406766420535,-46.0663367391113,
124.917791398394)) ;
#105147 = CARTESIAN_POINT('Ctrl Pts',(-19.5990992068201,-46.0761782404379,
124.907133995908)) ;
#105148 = CARTESIAN_POINT('Ctrl Pts',(-19.8549956383658,-46.0861391920327,
124.852064477482)) ;
#105149 = CARTESIAN_POINT('Ctrl Pts',(-20.0991149474506,-46.0961770097533,
124.752149387544)) ;
#105150 = CARTESIAN_POINT('Ctrl Pts',(-20.3188362146847,-46.1060513590104,
124.614043715742)) ;
#105151 = CARTESIAN_POINT('Ctrl Pts',(-20.5149807322072,-46.1161209097526,
124.436476561148)) ;
#105152 = CARTESIAN_POINT('Ctrl Pts',(-20.6736722161345,-46.1259549292612,
124.232479163217)) ;
#105153 = CARTESIAN_POINT('Ctrl Pts',(-20.7975880198892,-46.1359890838408,
123.999738628895)) ;
#105154 = CARTESIAN_POINT('Ctrl Pts',(-20.8784509574842,-46.1460050096632,
123.749243628566)) ;
#105155 = CARTESIAN_POINT('Ctrl Pts',(-20.914569442512,-46.1558872648575,
123.492067690217)) ;
#105156 = CARTESIAN_POINT('Ctrl Pts',(-20.9057131906475,-46.1658760713684,
123.229750694541)) ;
#105157 = CARTESIAN_POINT('Ctrl Pts',(-20.8518432319464,-46.1758246386311,
122.973880767554)) ;
#105158 = CARTESIAN_POINT('Ctrl Pts',(-20.7530881949105,-46.1858794439331,
122.728830454846)) ;
#105159 = CARTESIAN_POINT('Ctrl Pts',(-20.616861039315,-46.1956982271967,
122.509679270386)) ;
#105160 = CARTESIAN_POINT('Ctrl Pts',(-20.4413862067466,-46.2057339995573,
122.312807403627)) ;
#105161 = CARTESIAN_POINT('Ctrl Pts',(-20.2341435625144,-46.2157586985859,
122.150156536869)) ;
#105162 = CARTESIAN_POINT('Ctrl Pts',(-20.0060839751312,-46.225610701845,
122.027597836043)) ;
#105163 = CARTESIAN_POINT('Ctrl Pts',(-19.7569013276047,-46.2356016362422,
121.944987272963)) ;
#105164 = CARTESIAN_POINT('Ctrl Pts',(-19.4990198248001,-46.2455195586733,
121.906997442967)) ;
#105165 = CARTESIAN_POINT('Ctrl Pts',(-19.2356109355224,-46.2555479143556,
121.91438415743)) ;
#105166 = CARTESIAN_POINT('Ctrl Pts',(-18.9811375988693,-46.2654321988662,
121.9665159898)) ;
#105167 = CARTESIAN_POINT('Ctrl Pts',(-18.7367232904005,-46.2754248827741,
122.062532371143)) ;
#105168 = CARTESIAN_POINT('Ctrl Pts',(-18.5121245339067,-46.2854536197818,
122.200417548312)) ;
#105169 = CARTESIAN_POINT('Ctrl Pts',(-18.3174648059646,-46.2953390164107,
122.372455585845)) ;
#105170 = CARTESIAN_POINT('Ctrl Pts',(-18.1536854309232,-46.3053269018246,
122.577525230124)) ;
#105171 = CARTESIAN_POINT('Ctrl Pts',(-18.0283328197363,-46.3152776044852,
122.807058543816)) ;
#105172 = CARTESIAN_POINT('Ctrl Pts',(-17.9441425252922,-46.3253179225826,
123.057086661871)) ;
#105173 = CARTESIAN_POINT('Ctrl Pts',(-17.9050337144746,-46.3351924879158,
123.313645809229)) ;
#105174 = CARTESIAN_POINT('Ctrl Pts',(-17.9108065541753,-46.3451921479769,
123.576320024146)) ;
#105175 = CARTESIAN_POINT('Ctrl Pts',(-17.9614072155006,-46.3551011431446,
123.831801481986)) ;
#105176 = CARTESIAN_POINT('Ctrl Pts',(-18.0570299497226,-46.3651558843079,
124.078073850991)) ;
#105177 = CARTESIAN_POINT('Ctrl Pts',(-18.1910796797002,-46.3750144962217,
124.299825387159)) ;
#105178 = CARTESIAN_POINT('Ctrl Pts',(-18.3650434011911,-46.385082618501,
124.499120432854)) ;
#105179 = CARTESIAN_POINT('Ctrl Pts',(-18.5666792864394,-46.3949380892042,
124.661696531821)) ;
#105180 = CARTESIAN_POINT('Ctrl Pts',(-18.7962802236369,-46.4049329486976,
124.789235436467)) ;
#105181 = CARTESIAN_POINT('Ctrl Pts',(-19.0456405246855,-46.4149642020395,
124.874751408958)) ;
#105182 = CARTESIAN_POINT('Ctrl Pts',(-19.3017283009167,-46.4248309009126,
124.91540592978)) ;
#105183 = CARTESIAN_POINT('Ctrl Pts',(-19.5641107930564,-46.4348177166638,
124.911356078805)) ;
#105184 = CARTESIAN_POINT('Ctrl Pts',(-19.8208682713964,-46.4447649218593,
124.86211148328)) ;
#105185 = CARTESIAN_POINT('Ctrl Pts',(-20.0674353060267,-46.4548079099855,
124.768047551192)) ;
#105186 = CARTESIAN_POINT('Ctrl Pts',(-20.2900663287834,-46.464675264607,
124.6350864802)) ;
#105187 = CARTESIAN_POINT('Ctrl Pts',(-20.4886338862107,-46.4746411579051,
124.464343377395)) ;
#105188 = CARTESIAN_POINT('Ctrl Pts',(-20.6553083272588,-46.4846649352812,
124.260344882409)) ;
#105189 = CARTESIAN_POINT('Ctrl Pts',(-20.7828063712465,-46.4945904832129,
124.032811453884)) ;
#105190 = CARTESIAN_POINT('Ctrl Pts',(-20.8695819126354,-46.5045309596339,
123.786403623247)) ;
#105191 = CARTESIAN_POINT('Ctrl Pts',(-20.9124062871689,-46.5145771692968,
123.525912277354)) ;
#105192 = CARTESIAN_POINT('Ctrl Pts',(-20.9096836689865,-46.5244384259586,
123.266760258342)) ;
#105193 = CARTESIAN_POINT('Ctrl Pts',(-20.8618196513803,-46.5344320542339,
123.00857542062)) ;
#105194 = CARTESIAN_POINT('Ctrl Pts',(-20.7705820075892,-46.5443574515441,
122.76418240708)) ;
#105195 = CARTESIAN_POINT('Ctrl Pts',(-20.6369729547702,-46.5543853594543,
122.537081187664)) ;
#105196 = CARTESIAN_POINT('Ctrl Pts',(-20.4685329267532,-46.5642716751235,
122.339230363842)) ;
#105197 = CARTESIAN_POINT('Ctrl Pts',(-20.2655078356452,-46.5743032700273,
122.171141137268)) ;
#105198 = CARTESIAN_POINT('Ctrl Pts',(-20.039837488491,-46.584185512979,122.042547711301)) ;
#105199 = CARTESIAN_POINT('Ctrl Pts',(-19.790986603335,-46.5942449840088,
121.953442353936)) ;
#105200 = CARTESIAN_POINT('Ctrl Pts',(-19.5353950516732,-46.604111428672,
121.909781009716)) ;
#105201 = CARTESIAN_POINT('Ctrl Pts',(-19.2735030852152,-46.6140775531207,
121.910349350795)) ;
#105202 = CARTESIAN_POINT('Ctrl Pts',(-19.0140998320504,-46.6241077965118,
121.957095565601)) ;
#105203 = CARTESIAN_POINT('Ctrl Pts',(-18.7699834924998,-46.6340008314649,
122.046588137892)) ;
#105204 = CARTESIAN_POINT('Ctrl Pts',(-18.5415305597084,-46.6440517457017,
122.179105067727)) ;
#105205 = CARTESIAN_POINT('Ctrl Pts',(-18.342750038039,-46.6539415719263,
122.346547562767)) ;
#105206 = CARTESIAN_POINT('Ctrl Pts',(-18.1174517400336,-46.6672763869732,
122.614995956526)) ;
#105207 = CARTESIAN_POINT('Ctrl Pts',(-17.9686392139361,-46.6805534781447,
122.934913128643)) ;
#105208 = CARTESIAN_POINT('Ctrl Pts',(-17.9076787941137,-46.693801766743,
123.277725883847)) ;
#105209 = CARTESIAN_POINT('Ctrl Pts',(-17.9074679543351,-46.7038566082371,
123.541916040785)) ;
#105210 = CARTESIAN_POINT('Ctrl Pts',(-17.9516976277524,-46.7136875975446,
123.796495795355)) ;
#105211 = CARTESIAN_POINT('Ctrl Pts',(-18.0414367212003,-46.7237641618679,
124.045580065804)) ;
#105212 = CARTESIAN_POINT('Ctrl Pts',(-18.17013546342,-46.7336134870018,124.27017655509)) ;
#105213 = CARTESIAN_POINT('Ctrl Pts',(-18.3940809637255,-46.7469614866391,
124.540176759679)) ;
#105214 = CARTESIAN_POINT('Ctrl Pts',(-18.7539781559382,-46.7635462461757,
124.794640265119)) ;
#105215 = CARTESIAN_POINT('Ctrl Pts',(-19.178401102146,-46.7801147975237,
124.911971266093)) ;
#105216 = CARTESIAN_POINT('Ctrl Pts',(-19.5295056773098,-46.7934746223427,
124.914512890267)) ;
#105217 = CARTESIAN_POINT('Ctrl Pts',(-19.786214189388,-46.8033800311734,
124.871368392262)) ;
#105218 = CARTESIAN_POINT('Ctrl Pts',(-20.0329826854452,-46.8133400577574,
124.784198105326)) ;
#105219 = CARTESIAN_POINT('Ctrl Pts',(-20.3365985781968,-46.8265976419427,
124.613256266791)) ;
#105220 = CARTESIAN_POINT('Ctrl Pts',(-20.6530444857131,-46.8432488534374,
124.303863399263)) ;
#105221 = CARTESIAN_POINT('Ctrl Pts',(-20.8822282307178,-46.8631670675477,
123.826681959305)) ;
#105222 = CARTESIAN_POINT('Ctrl Pts',(-20.935851847913,-46.8830448307685,
123.301015754195)) ;
#105223 = CARTESIAN_POINT('Ctrl Pts',(-20.8055768749785,-46.9030574985557,
122.785411934825)) ;
#105224 = CARTESIAN_POINT('Ctrl Pts',(-20.5104582098003,-46.9228700212223,
122.349177441695)) ;
#105225 = CARTESIAN_POINT('Ctrl Pts',(-20.0811735104229,-46.9428533212222,
122.03661245177)) ;
#105226 = CARTESIAN_POINT('Ctrl Pts',(-19.5729864649457,-46.9627475983235,
121.890277286916)) ;
#105227 = CARTESIAN_POINT('Ctrl Pts',(-19.0443848766618,-46.9826803600813,
121.925379962756)) ;
#105228 = CARTESIAN_POINT('Ctrl Pts',(-18.5588179767112,-47.002646365846,
122.139461236973)) ;
#105229 = CARTESIAN_POINT('Ctrl Pts',(-18.1768456454212,-47.0225248980109,
122.504529177378)) ;
#105230 = CARTESIAN_POINT('Ctrl Pts',(-17.9412439125184,-47.0424645646712,
122.979181644419)) ;
#105231 = CARTESIAN_POINT('Ctrl Pts',(-17.8817257735614,-47.0623594393166,
123.504649624854)) ;
#105232 = CARTESIAN_POINT('Ctrl Pts',(-18.0046212015472,-47.0822665786099,
124.019152970604)) ;
#105233 = CARTESIAN_POINT('Ctrl Pts',(-18.2951649063741,-47.1021771266884,
124.461654024879)) ;
#105234 = CARTESIAN_POINT('Ctrl Pts',(-18.7231345570902,-47.1222457120455,
124.779809750388)) ;
#105235 = CARTESIAN_POINT('Ctrl Pts',(-19.226804714384,-47.1420275093603,
124.931228062656)) ;
#105236 = CARTESIAN_POINT('Ctrl Pts',(-19.7575681893512,-47.1620350563049,
124.902143874691)) ;
#105237 = CARTESIAN_POINT('Ctrl Pts',(-20.2423345965883,-47.1818567946077,
124.695505400649)) ;
#105238 = CARTESIAN_POINT('Ctrl Pts',(-20.6310620977836,-47.2018368145119,
124.333831088968)) ;
#105239 = CARTESIAN_POINT('Ctrl Pts',(-20.87170569344,-47.2217542657741,123.862294488323)) ;
#105240 = CARTESIAN_POINT('Ctrl Pts',(-20.9380824059377,-47.2416291869468,
123.338204944686)) ;
#105241 = CARTESIAN_POINT('Ctrl Pts',(-20.8204345579771,-47.2616535554976,
122.819191362508)) ;
#105242 = CARTESIAN_POINT('Ctrl Pts',(-20.5348082570627,-47.2815202398711,
122.37498839788)) ;
#105243 = CARTESIAN_POINT('Ctrl Pts',(-20.1137434665979,-47.3014640617173,
122.053088573225)) ;
#105244 = CARTESIAN_POINT('Ctrl Pts',(-19.6089193112748,-47.3213714309688,
121.894637053931)) ;
#105245 = CARTESIAN_POINT('Ctrl Pts',(-19.0811597470671,-47.3412461287155,
121.916943088499)) ;
#105246 = CARTESIAN_POINT('Ctrl Pts',(-18.5899719411168,-47.3612280712373,
122.118985961882)) ;
#105247 = CARTESIAN_POINT('Ctrl Pts',(-18.1991382375035,-47.3811307381481,
122.475368348256)) ;
#105248 = CARTESIAN_POINT('Ctrl Pts',(-17.9525186514706,-47.4009860956868,
122.942006158882)) ;
#105249 = CARTESIAN_POINT('Ctrl Pts',(-17.8797909685168,-47.4210501344028,
123.470209837654)) ;
#105250 = CARTESIAN_POINT('Ctrl Pts',(-17.9907794764626,-47.4409053141279,
123.986324657528)) ;
#105251 = CARTESIAN_POINT('Ctrl Pts',(-18.2724218178292,-47.4608854187923,
124.436282396569)) ;
#105252 = CARTESIAN_POINT('Ctrl Pts',(-18.6870135330641,-47.4806945239621,
124.761041750837)) ;
#105253 = CARTESIAN_POINT('Ctrl Pts',(-19.1917055879886,-47.5006871443028,
124.926757544361)) ;
#105254 = CARTESIAN_POINT('Ctrl Pts',(-19.6312174551831,-47.5172266268069,
124.913212879468)) ;
#105255 = CARTESIAN_POINT('Ctrl Pts',(-19.9675049947243,-47.5305909448711,
124.812128857147)) ;
#105256 = CARTESIAN_POINT('Ctrl Pts',(-20.277984697308,-47.5438085473726,
124.656243961923)) ;
#105257 = CARTESIAN_POINT('Ctrl Pts',(-20.6088670104154,-47.5604661416504,
124.362251795255)) ;
#105258 = CARTESIAN_POINT('Ctrl Pts',(-20.8603828060034,-47.5803318436921,
123.897898755475)) ;
#105259 = CARTESIAN_POINT('Ctrl Pts',(-20.9262201830231,-47.5969615703822,
123.460927621038)) ;
#105260 = CARTESIAN_POINT('Ctrl Pts',(-20.8869884578192,-47.61025068552,123.113852351726)) ;
#105261 = CARTESIAN_POINT('Ctrl Pts',(-20.8131428594769,-47.6202150324971,
122.86264462755)) ;
#105262 = CARTESIAN_POINT('Ctrl Pts',(-20.6973777337453,-47.6301434004986,
122.628839141613)) ;
#105263 = CARTESIAN_POINT('Ctrl Pts',(-20.4910418838649,-47.6434268335873,
122.347219669949)) ;
#105264 = CARTESIAN_POINT('Ctrl Pts',(-20.1458317228279,-47.6600789113277,
122.070296589039)) ;
#105265 = CARTESIAN_POINT('Ctrl Pts',(-19.7294313556018,-47.6766302806285,
121.928443166844)) ;
#105266 = CARTESIAN_POINT('Ctrl Pts',(-19.3810509337029,-47.6899177087775,
121.904509175098)) ;
#105267 = CARTESIAN_POINT('Ctrl Pts',(-19.1186147780108,-47.6999622484776,
121.932674760528)) ;
#105268 = CARTESIAN_POINT('Ctrl Pts',(-18.8700289913605,-47.7098050903014,
122.004211514632)) ;
#105269 = CARTESIAN_POINT('Ctrl Pts',(-18.6340718128688,-47.7197893745484,
122.118894210686)) ;
#105270 = CARTESIAN_POINT('Ctrl Pts',(-18.4223500836401,-47.7297390199475,
122.272337242117)) ;
#105271 = CARTESIAN_POINT('Ctrl Pts',(-18.2393375261666,-47.7397387816359,
122.460934913689)) ;
#105272 = CARTESIAN_POINT('Ctrl Pts',(-18.0917561865663,-47.7497701275948,
122.67936089865)) ;
#105273 = CARTESIAN_POINT('Ctrl Pts',(-17.9858813511188,-47.7596250820719,
122.915713531507)) ;
#105274 = CARTESIAN_POINT('Ctrl Pts',(-17.921313983943,-47.7695976200724,
123.169675068302)) ;
#105275 = CARTESIAN_POINT('Ctrl Pts',(-17.9017937695438,-47.7795926138074,
123.431647087822)) ;
#105276 = CARTESIAN_POINT('Ctrl Pts',(-17.928475189429,-47.7896266726015,
123.693955509307)) ;
#105277 = CARTESIAN_POINT('Ctrl Pts',(-17.9986334721321,-47.7994820154245,
123.943286670898)) ;
#105278 = CARTESIAN_POINT('Ctrl Pts',(-18.1123113435393,-47.8094814947701,
124.180149064765)) ;
#105279 = CARTESIAN_POINT('Ctrl Pts',(-18.2635967217222,-47.8193759435254,
124.39168267558)) ;
#105280 = CARTESIAN_POINT('Ctrl Pts',(-18.4524654950994,-47.8294390629599,
124.576715764561)) ;
#105281 = CARTESIAN_POINT('Ctrl Pts',(-18.6656604141753,-47.8392787082011,
124.723110773571)) ;
#105282 = CARTESIAN_POINT('Ctrl Pts',(-18.9061698010973,-47.8493418723872,
124.832971195248)) ;
#105283 = CARTESIAN_POINT('Ctrl Pts',(-19.1579245355548,-47.859236142136,
124.898091649154)) ;
#105284 = CARTESIAN_POINT('Ctrl Pts',(-19.418285236118,-47.8691778681498,
124.919307392181)) ;
#105285 = CARTESIAN_POINT('Ctrl Pts',(-19.6800605824406,-47.8791807568092,
124.894950207823)) ;
#105286 = CARTESIAN_POINT('Ctrl Pts',(-19.9343759736803,-47.8892206056032,
124.824805409366)) ;
#105287 = CARTESIAN_POINT('Ctrl Pts',(-20.1678242012441,-47.8990448210641,
124.714511643013)) ;
#105288 = CARTESIAN_POINT('Ctrl Pts',(-20.3837446801702,-47.9091016645576,
124.562152333181)) ;
#105289 = CARTESIAN_POINT('Ctrl Pts',(-20.5673352422377,-47.9190302739536,
124.376743540514)) ;
#105290 = CARTESIAN_POINT('Ctrl Pts',(-20.7168951714096,-47.9289821579915,
124.162191214488)) ;
#105291 = CARTESIAN_POINT('Ctrl Pts',(-20.82760319258,-47.9390351107991,123.92234566536)) ;
#105292 = CARTESIAN_POINT('Ctrl Pts',(-20.8939170780824,-47.9488579872653,
123.672853622298)) ;
#105293 = CARTESIAN_POINT('Ctrl Pts',(-20.9168841773058,-47.9589137198354,
123.409617614338)) ;
#105294 = CARTESIAN_POINT('Ctrl Pts',(-20.8935971778619,-47.9688544848231,
123.149415027689)) ;
#105295 = CARTESIAN_POINT('Ctrl Pts',(-20.8265214718633,-47.9787588177287,
122.897925847122)) ;
#105296 = CARTESIAN_POINT('Ctrl Pts',(-20.7150807429793,-47.9888054866094,
122.658606916278)) ;
#105297 = CARTESIAN_POINT('Ctrl Pts',(-20.5662122954325,-47.9987010499152,
122.445338160024)) ;
#105298 = CARTESIAN_POINT('Ctrl Pts',(-20.3795420640069,-48.0087631076155,
122.258115625074)) ;
#105299 = CARTESIAN_POINT('Ctrl Pts',(-20.1679441914161,-48.018605885243,
122.109301615718)) ;
#105300 = CARTESIAN_POINT('Ctrl Pts',(-19.9305295366812,-48.0285963634949,
121.997305134393)) ;
#105301 = CARTESIAN_POINT('Ctrl Pts',(-19.6787754200259,-48.0385253361384,
121.928681255677)) ;
#105302 = CARTESIAN_POINT('Ctrl Pts',(-19.4173556033698,-48.048516473018,
121.904257464178)) ;
#105303 = CARTESIAN_POINT('Ctrl Pts',(-19.154877813197,-48.0585385905069,
121.925978978752)) ;
#105304 = CARTESIAN_POINT('Ctrl Pts',(-18.9031878540514,-48.0684391009091,
121.991894698316)) ;
#105305 = CARTESIAN_POINT('Ctrl Pts',(-18.6644862196403,-48.0784280936552,
122.101106808281)) ;
#105306 = CARTESIAN_POINT('Ctrl Pts',(-18.4489980875861,-48.0883933377058,
122.24989675199)) ;
#105307 = CARTESIAN_POINT('Ctrl Pts',(-18.2633058629821,-48.098297602219,
122.432301210842)) ;
#105308 = CARTESIAN_POINT('Ctrl Pts',(-18.1099186316045,-48.1083556939172,
122.647530199542)) ;
#105309 = CARTESIAN_POINT('Ctrl Pts',(-17.9983934158616,-48.1182056343456,
122.881135521714)) ;
#105310 = CARTESIAN_POINT('Ctrl Pts',(-17.9272566245635,-48.1282326455192,
123.134845982042)) ;
#105311 = CARTESIAN_POINT('Ctrl Pts',(-17.9019314072819,-48.1382612321312,
123.397179595128)) ;
#105312 = CARTESIAN_POINT('Ctrl Pts',(-17.9216733250897,-48.1481064462439,
123.655133881955)) ;
#105313 = CARTESIAN_POINT('Ctrl Pts',(-17.9861782975322,-48.1580971944235,
123.909638987768)) ;
#105314 = CARTESIAN_POINT('Ctrl Pts',(-18.0949265686973,-48.168134828009,
124.149957160556)) ;
#105315 = CARTESIAN_POINT('Ctrl Pts',(-18.2405451274193,-48.1779801172218,
124.363815242263)) ;
#105316 = CARTESIAN_POINT('Ctrl Pts',(-18.4231455792606,-48.1879615180277,
124.552092371215)) ;
#105317 = CARTESIAN_POINT('Ctrl Pts',(-18.6351018542138,-48.1979137510176,
124.705319799365)) ;
#105318 = CARTESIAN_POINT('Ctrl Pts',(-18.8714073387186,-48.2079125624742,
124.820264398588)) ;
#105319 = CARTESIAN_POINT('Ctrl Pts',(-19.1252041777286,-48.2179516664049,
124.892225670979)) ;
#105320 = CARTESIAN_POINT('Ctrl Pts',(-19.3820164657569,-48.2277766088242,
124.919009855094)) ;
#105321 = CARTESIAN_POINT('Ctrl Pts',(-19.645598927116,-48.2378312963002,
124.900805826221)) ;
#105322 = CARTESIAN_POINT('Ctrl Pts',(-19.8990789793834,-48.247774098657,
124.837381251023)) ;
#105323 = CARTESIAN_POINT('Ctrl Pts',(-20.1370819206861,-48.2576778945968,
124.732055560425)) ;
#105324 = CARTESIAN_POINT('Ctrl Pts',(-20.3561905129845,-48.2677246739718,
124.584794460895)) ;
#105325 = CARTESIAN_POINT('Ctrl Pts',(-20.5437409268307,-48.2776203322664,
124.404601015632)) ;
#105326 = CARTESIAN_POINT('Ctrl Pts',(-20.699711817272,-48.287681899517,124.19113144653)) ;
#105327 = CARTESIAN_POINT('Ctrl Pts',(-20.8137891111206,-48.2975265439543,
123.958924282819)) ;
#105328 = CARTESIAN_POINT('Ctrl Pts',(-20.8875575622636,-48.307486590197,
123.707798631624)) ;
#105329 = CARTESIAN_POINT('Ctrl Pts',(-20.9163145705718,-48.3175248862154,
123.445587612575)) ;
#105330 = CARTESIAN_POINT('Ctrl Pts',(-20.8998826835862,-48.3273982276337,
123.186607836747)) ;
#105331 = CARTESIAN_POINT('Ctrl Pts',(-20.8374393368674,-48.337471331433,
122.929420568722)) ;
#105332 = CARTESIAN_POINT('Ctrl Pts',(-20.7342018444484,-48.3472921465519,
122.692831515298)) ;
#105333 = CARTESIAN_POINT('Ctrl Pts',(-20.5880398528313,-48.3573690116299,
122.472072060764)) ;
#105334 = CARTESIAN_POINT('Ctrl Pts',(-20.4094765525404,-48.3672337512852,
122.284097068372)) ;
#105335 = CARTESIAN_POINT('Ctrl Pts',(-20.1980999492212,-48.3772561545265,
122.126990352241)) ;
#105336 = CARTESIAN_POINT('Ctrl Pts',(-19.9622589109079,-48.387281878815,
122.009510754625)) ;
#105337 = CARTESIAN_POINT('Ctrl Pts',(-19.7140688412835,-48.3971366618363,
121.935611134121)) ;
#105338 = CARTESIAN_POINT('Ctrl Pts',(-19.4536367372929,-48.4071155055596,
121.904873002265)) ;
#105339 = CARTESIAN_POINT('Ctrl Pts',(-19.1908180123101,-48.4171343977962,
121.920334070307)) ;
#105340 = CARTESIAN_POINT('Ctrl Pts',(-18.9379752442509,-48.4270176068372,
121.979857228131)) ;
#105341 = CARTESIAN_POINT('Ctrl Pts',(-18.6949553095141,-48.4370859161774,
122.084369573566)) ;
#105342 = CARTESIAN_POINT('Ctrl Pts',(-18.4787661619225,-48.4469160415101,
122.225852664431)) ;
#105343 = CARTESIAN_POINT('Ctrl Pts',(-18.2857271344628,-48.4569825938871,
122.406667621698)) ;
#105344 = CARTESIAN_POINT('Ctrl Pts',(-18.1298795565182,-48.4668728307808,
122.61470398107)) ;
#105345 = CARTESIAN_POINT('Ctrl Pts',(-18.0108214031935,-48.4768650555748,
122.848729665131)) ;
#105346 = CARTESIAN_POINT('Ctrl Pts',(-17.9346625480558,-48.4868276759257,
123.099210441547)) ;
#105347 = CARTESIAN_POINT('Ctrl Pts',(-17.9026921520471,-48.4967326786889,
123.357550683362)) ;
#105348 = CARTESIAN_POINT('Ctrl Pts',(-17.9164495946662,-48.506790441087,
123.621476523787)) ;
#105349 = CARTESIAN_POINT('Ctrl Pts',(-17.9744028993469,-48.5166409604658,
123.873788410068)) ;
#105350 = CARTESIAN_POINT('Ctrl Pts',(-18.0765915286139,-48.526672537464,
124.116777343657)) ;
#105351 = CARTESIAN_POINT('Ctrl Pts',(-18.2195583870351,-48.5366822725689,
124.337613358447)) ;
#105352 = CARTESIAN_POINT('Ctrl Pts',(-18.3967026397366,-48.5465918491952,
124.528462578557)) ;
#105353 = CARTESIAN_POINT('Ctrl Pts',(-18.6042899116757,-48.5565192350519,
124.686490326835)) ;
#105354 = CARTESIAN_POINT('Ctrl Pts',(-18.8389855979222,-48.5665641695422,
124.807288343278)) ;
#105355 = CARTESIAN_POINT('Ctrl Pts',(-19.0870807049156,-48.5764501017301,
124.88441804605)) ;
#105356 = CARTESIAN_POINT('Ctrl Pts',(-19.3475102915803,-48.5864434076831,
124.918100928947)) ;
#105357 = CARTESIAN_POINT('Ctrl Pts',(-19.6085921832354,-48.596389045465,
124.906007103596)) ;
#105358 = CARTESIAN_POINT('Ctrl Pts',(-19.8637789792283,-48.6063363138109,
124.849275357252)) ;
#105359 = CARTESIAN_POINT('Ctrl Pts',(-20.1075477045523,-48.616384215948,
124.74781718916)) ;
#105360 = CARTESIAN_POINT('Ctrl Pts',(-20.3256903200238,-48.6262319107882,
124.60858627602)) ;
#105361 = CARTESIAN_POINT('Ctrl Pts',(-20.5190970658779,-48.6361934205326,
124.432188062646)) ;
#105362 = CARTESIAN_POINT('Ctrl Pts',(-20.679759546878,-48.6462228121415,
124.223243847713)) ;
#105363 = CARTESIAN_POINT('Ctrl Pts',(-20.8003422433532,-48.6561303076962,
123.992489355231)) ;
#105364 = CARTESIAN_POINT('Ctrl Pts',(-20.8798178028071,-48.6660756993592,
123.743533785496)) ;
#105365 = CARTESIAN_POINT('Ctrl Pts',(-20.9152202636129,-48.6760776169566,
123.483053144482)) ;
#105366 = CARTESIAN_POINT('Ctrl Pts',(-20.9043330847647,-48.6861176845088,
123.219459711109)) ;
#105367 = CARTESIAN_POINT('Ctrl Pts',(-20.8496202639193,-48.6959419959486,
122.967128154732)) ;
#105368 = CARTESIAN_POINT('Ctrl Pts',(-20.7499746982012,-48.7059982371047,
122.722395397519)) ;
#105369 = CARTESIAN_POINT('Ctrl Pts',(-20.6108122326477,-48.7159291588403,
122.501585804045)) ;
#105370 = CARTESIAN_POINT('Ctrl Pts',(-20.4356439584125,-48.7258723949166,
122.307742246963)) ;
#105371 = CARTESIAN_POINT('Ctrl Pts',(-20.228787585752,-48.735853678929,122.146399919613)) ;
#105372 = CARTESIAN_POINT('Ctrl Pts',(-19.9954475040825,-48.7458979805547,
122.023085563198)) ;
#105373 = CARTESIAN_POINT('Ctrl Pts',(-19.7497625805735,-48.7557260617741,
121.943308130325)) ;
#105374 = CARTESIAN_POINT('Ctrl Pts',(-19.4876032964969,-48.7658026646233,
121.906379105152)) ;
#105375 = CARTESIAN_POINT('Ctrl Pts',(-19.22879428654,-48.7756547437418,121.915201234916)) ;
#105376 = CARTESIAN_POINT('Ctrl Pts',(-18.9698136227784,-48.7857280020508,
121.969789340118)) ;
#105377 = CARTESIAN_POINT('Ctrl Pts',(-18.7298662537344,-48.7955694614311,
122.066333319079)) ;
#105378 = CARTESIAN_POINT('Ctrl Pts',(-18.5071641353739,-48.8055305568434,
122.20388639306)) ;
#105379 = CARTESIAN_POINT('Ctrl Pts',(-18.3105756785114,-48.8155678412401,
122.379738566765)) ;
#105380 = CARTESIAN_POINT('Ctrl Pts',(-18.1497440179017,-48.8254441799754,
122.583476122298)) ;
#105381 = CARTESIAN_POINT('Ctrl Pts',(-18.0244030217807,-48.8355063061287,
122.8162654372)) ;
#105382 = CARTESIAN_POINT('Ctrl Pts',(-17.942905899043,-48.8453744801052,
123.062485485328)) ;
#105383 = CARTESIAN_POINT('Ctrl Pts',(-17.9043608091258,-48.855380028609,
123.322544901866)) ;
#105384 = CARTESIAN_POINT('Ctrl Pts',(-17.911631882069,-48.8653626605046,
123.584825264922)) ;
#105385 = CARTESIAN_POINT('Ctrl Pts',(-17.96491145671,-48.8754066029264,123.843313454049)) ;
#105386 = CARTESIAN_POINT('Ctrl Pts',(-18.0598585764052,-48.8852347509536,
124.083501852298)) ;
#105387 = CARTESIAN_POINT('Ctrl Pts',(-18.1965745857908,-48.8952246183279,
124.307617145225)) ;
#105388 = CARTESIAN_POINT('Ctrl Pts',(-18.37157698631,-48.9052683572834,124.505196859197)) ;
#105389 = CARTESIAN_POINT('Ctrl Pts',(-18.5733245027204,-48.9150901058214,
124.666180890081)) ;
#105390 = CARTESIAN_POINT('Ctrl Pts',(-18.804570190676,-48.9251250834311,
124.79293891988)) ;
#105391 = CARTESIAN_POINT('Ctrl Pts',(-19.0543037323984,-48.9351499961888,
124.876841632141)) ;
#105392 = CARTESIAN_POINT('Ctrl Pts',(-19.3102311694343,-48.9450019392826,
124.91599016344)) ;
#105393 = CARTESIAN_POINT('Ctrl Pts',(-19.5726920168574,-48.9549929006117,
124.910425982327)) ;
#105394 = CARTESIAN_POINT('Ctrl Pts',(-19.8284128705692,-48.9649107754802,
124.859903942216)) ;
#105395 = CARTESIAN_POINT('Ctrl Pts',(-20.074156743072,-48.9749392944814,
124.764768705151)) ;
#105396 = CARTESIAN_POINT('Ctrl Pts',(-20.2964901168158,-48.9848229732793,
124.630476227167)) ;
#105397 = CARTESIAN_POINT('Ctrl Pts',(-20.4947028792025,-48.994817916719,
124.458139223687)) ;
#105398 = CARTESIAN_POINT('Ctrl Pts',(-20.6601584139195,-49.0048447705414,
124.253066383284)) ;
#105399 = CARTESIAN_POINT('Ctrl Pts',(-20.7859988178692,-49.0147289348803,
124.025827024865)) ;
#105400 = CARTESIAN_POINT('Ctrl Pts',(-20.8716773612727,-49.0247170329227,
123.777755041357)) ;
#105401 = CARTESIAN_POINT('Ctrl Pts',(-20.9129810731439,-49.0346681393798,
123.51949960993)) ;
#105402 = CARTESIAN_POINT('Ctrl Pts',(-20.908629938218,-49.0447131905479,
123.25557749533)) ;
#105403 = CARTESIAN_POINT('Ctrl Pts',(-20.859571512365,-49.0545749509062,
123.001104813214)) ;
#105404 = CARTESIAN_POINT('Ctrl Pts',(-20.7668806910983,-49.0645377677367,
122.756248061331)) ;
#105405 = CARTESIAN_POINT('Ctrl Pts',(-20.6317353832147,-49.0745724490174,
122.529824314885)) ;
#105406 = CARTESIAN_POINT('Ctrl Pts',(-20.4622046891527,-49.0844574787982,
122.332954833504)) ;
#105407 = CARTESIAN_POINT('Ctrl Pts',(-20.2574156100896,-49.0945230721962,
122.165604849423)) ;
#105408 = CARTESIAN_POINT('Ctrl Pts',(-20.0319252978085,-49.1043622405577,
122.038994712386)) ;
#105409 = CARTESIAN_POINT('Ctrl Pts',(-19.7825239386548,-49.1144248382992,
121.951198971752)) ;
#105410 = CARTESIAN_POINT('Ctrl Pts',(-19.5258681356092,-49.1243218507061,
121.909018990511)) ;
#105411 = CARTESIAN_POINT('Ctrl Pts',(-19.2648981101993,-49.1342531725317,
121.911184944876)) ;
#105412 = CARTESIAN_POINT('Ctrl Pts',(-19.0054644614894,-49.1442949352862,
121.959440242708)) ;
#105413 = CARTESIAN_POINT('Ctrl Pts',(-18.7620464793974,-49.1541831341769,
122.050426042176)) ;
#105414 = CARTESIAN_POINT('Ctrl Pts',(-18.5355498526046,-49.1641770727768,
122.183327970392)) ;
#105415 = CARTESIAN_POINT('Ctrl Pts',(-18.3366151190307,-49.1741178938136,
122.352671265509)) ;
#105416 = CARTESIAN_POINT('Ctrl Pts',(-18.1695582708548,-49.1840772761019,
122.554123401537)) ;
#105417 = CARTESIAN_POINT('Ctrl Pts',(-18.0393609910467,-49.1940750357542,
122.78235492102)) ;
#105418 = CARTESIAN_POINT('Ctrl Pts',(-17.9507830524061,-49.2041111719565,
123.030767337162)) ;
#105419 = CARTESIAN_POINT('Ctrl Pts',(-17.9071961511575,-49.2139619694474,
123.285938131175)) ;
#105420 = CARTESIAN_POINT('Ctrl Pts',(-17.9078135555546,-49.2239228345237,
123.547689302551)) ;
#105421 = CARTESIAN_POINT('Ctrl Pts',(-17.9545028435727,-49.2339517021541,
123.807083872471)) ;
#105422 = CARTESIAN_POINT('Ctrl Pts',(-18.0443614900807,-49.2438619382905,
124.051509569397)) ;
#105423 = CARTESIAN_POINT('Ctrl Pts',(-18.1750394781189,-49.253796891605,
124.277540500382)) ;
#105424 = CARTESIAN_POINT('Ctrl Pts',(-18.3449458767919,-49.2638378220146,
124.479414892215)) ;
#105425 = CARTESIAN_POINT('Ctrl Pts',(-18.5441450587453,-49.2737257187962,
124.646279157345)) ;
#105426 = CARTESIAN_POINT('Ctrl Pts',(-18.7713454870044,-49.2837151704549,
124.777768598755)) ;
#105427 = CARTESIAN_POINT('Ctrl Pts',(-19.0172462602511,-49.2936742608203,
124.867340329081)) ;
#105428 = CARTESIAN_POINT('Ctrl Pts',(-19.2732737968385,-49.3035715731266,
124.913231451981)) ;
#105429 = CARTESIAN_POINT('Ctrl Pts',(-19.5375236712753,-49.3136279990268,
124.913856788478)) ;
#105430 = CARTESIAN_POINT('Ctrl Pts',(-19.7931094413585,-49.3234980016166,
124.869551884532)) ;
#105431 = CARTESIAN_POINT('Ctrl Pts',(-20.0405595157066,-49.3335019347938,
124.780858628891)) ;
#105432 = CARTESIAN_POINT('Ctrl Pts',(-20.268461346366,-49.3434891952577,
124.650609341134)) ;
#105433 = CARTESIAN_POINT('Ctrl Pts',(-20.470944358427,-49.3535162468434,
124.482019340126)) ;
#105434 = CARTESIAN_POINT('Ctrl Pts',(-20.6389945572842,-49.3634073366695,
124.283693917084)) ;
#105435 = CARTESIAN_POINT('Ctrl Pts',(-20.8155279114935,-49.3767050914506,
123.982169929469)) ;
#105436 = CARTESIAN_POINT('Ctrl Pts',(-20.9091683649831,-49.3899031510587,
123.644067313166)) ;
#105437 = CARTESIAN_POINT('Ctrl Pts',(-20.9119671066389,-49.4032998916279,
123.292047468722)) ;
#105438 = CARTESIAN_POINT('Ctrl Pts',(-20.86922905483,-49.4131708037013,123.036144564407)) ;
#105439 = CARTESIAN_POINT('Ctrl Pts',(-20.7809586057459,-49.4232443654695,
122.786633988022)) ;
#105440 = CARTESIAN_POINT('Ctrl Pts',(-20.65417958686,-49.4330657780578,122.561751573419)) ;
#105441 = CARTESIAN_POINT('Ctrl Pts',(-20.4863376664184,-49.4431397952888,
122.357107851664)) ;
#105442 = CARTESIAN_POINT('Ctrl Pts',(-20.2240643845596,-49.4562985822534,
122.131632384811)) ;
#105443 = CARTESIAN_POINT('Ctrl Pts',(-19.904402249654,-49.4696646853476,
121.976914104498)) ;
#105444 = CARTESIAN_POINT('Ctrl Pts',(-19.5604858538446,-49.4829786202367,
121.912034841933)) ;
#105445 = CARTESIAN_POINT('Ctrl Pts',(-19.3003871649201,-49.4928786596841,
121.908349652686)) ;
#105446 = CARTESIAN_POINT('Ctrl Pts',(-19.0418061619267,-49.5028430628186,
121.949723315538)) ;
#105447 = CARTESIAN_POINT('Ctrl Pts',(-18.7927980800568,-49.5128730299398,
122.036150682678)) ;
#105448 = CARTESIAN_POINT('Ctrl Pts',(-18.565468855254,-49.5227753065488,
122.162762109831)) ;
#105449 = CARTESIAN_POINT('Ctrl Pts',(-18.2943922464803,-49.536041235718,
122.382027616931)) ;
#105450 = CARTESIAN_POINT('Ctrl Pts',(-18.0346360175635,-49.5526627668244,
122.739267143311)) ;
#105451 = CARTESIAN_POINT('Ctrl Pts',(-17.8877054079863,-49.5725375954691,
123.246737253887)) ;
#105452 = CARTESIAN_POINT('Ctrl Pts',(-17.9170062305799,-49.5892108035709,
123.688865187622)) ;
#105453 = CARTESIAN_POINT('Ctrl Pts',(-18.0293993130542,-49.6024619285522,
124.018479147189)) ;
#105454 = CARTESIAN_POINT('Ctrl Pts',(-18.1961111258911,-49.615704247373,
124.32401157025)) ;
#105455 = CARTESIAN_POINT('Ctrl Pts',(-18.5033429645354,-49.6324374877125,
124.645464754067)) ;
#105456 = CARTESIAN_POINT('Ctrl Pts',(-18.975740249179,-49.6522666359005,
124.879352518781)) ;
#105457 = CARTESIAN_POINT('Ctrl Pts',(-19.5017593847413,-49.6721913310011,
124.939533147707)) ;
#105458 = CARTESIAN_POINT('Ctrl Pts',(-20.0168814997899,-49.6921145595845,
124.816509691594)) ;
#105459 = CARTESIAN_POINT('Ctrl Pts',(-20.4591559559091,-49.7120416987106,
124.52524484642)) ;
#105460 = CARTESIAN_POINT('Ctrl Pts',(-20.7752892855415,-49.7319181613263,
124.101950919271)) ;
#105461 = CARTESIAN_POINT('Ctrl Pts',(-20.9290303017219,-49.7518953899316,
123.593740830601)) ;
#105462 = CARTESIAN_POINT('Ctrl Pts',(-20.8997552792579,-49.7718302479053,
123.064668541065)) ;
#105463 = CARTESIAN_POINT('Ctrl Pts',(-20.6926247770607,-49.7917266968361,
122.578151319081)) ;
#105464 = CARTESIAN_POINT('Ctrl Pts',(-20.3318449657526,-49.8116479809027,
122.190587914378)) ;
#105465 = CARTESIAN_POINT('Ctrl Pts',(-19.8595490175129,-49.8316046305737,
121.949122369929)) ;
#105466 = CARTESIAN_POINT('Ctrl Pts',(-19.3354133917941,-49.8514819236853,
121.883428245473)) ;
#105467 = CARTESIAN_POINT('Ctrl Pts',(-18.8196514980791,-49.8713683959137,
121.999250184421)) ;
#105468 = CARTESIAN_POINT('Ctrl Pts',(-18.3709182764398,-49.8914299618377,
122.287287346707)) ;
#105469 = CARTESIAN_POINT('Ctrl Pts',(-18.0514065132604,-49.9112703693785,
122.706761226316)) ;
#105470 = CARTESIAN_POINT('Ctrl Pts',(-17.8920110217991,-49.9311216933514,
123.209742540466)) ;
#105471 = CARTESIAN_POINT('Ctrl Pts',(-17.9148505895717,-49.9511749633028,
123.742166975697)) ;
#105472 = CARTESIAN_POINT('Ctrl Pts',(-18.1156270801346,-49.9709956206862,
124.229362048374)) ;
#105473 = CARTESIAN_POINT('Ctrl Pts',(-18.4724553006617,-49.9909670420167,
124.622102771765)) ;
#105474 = CARTESIAN_POINT('Ctrl Pts',(-18.9403141167353,-50.0108605343804,
124.868821111013)) ;
#105475 = CARTESIAN_POINT('Ctrl Pts',(-19.4674698621008,-50.0308846206214,
124.941152365213)) ;
#105476 = CARTESIAN_POINT('Ctrl Pts',(-19.9821925019439,-50.0506894997343,
124.830721241803)) ;
#105477 = CARTESIAN_POINT('Ctrl Pts',(-20.4325069663933,-50.0706485154322,
124.550354233972)) ;
#105478 = CARTESIAN_POINT('Ctrl Pts',(-20.7595911996121,-50.0906345390612,
124.131812199693)) ;
#105479 = CARTESIAN_POINT('Ctrl Pts',(-20.9237526047702,-50.1104430348217,
123.631533408587)) ;
#105480 = CARTESIAN_POINT('Ctrl Pts',(-20.9078620156029,-50.1304256739273,
123.10077833293)) ;
#105481 = CARTESIAN_POINT('Ctrl Pts',(-20.7125831300337,-50.1503071217213,
122.609626261788)) ;
#105482 = CARTESIAN_POINT('Ctrl Pts',(-20.3605756213218,-50.1702635884589,
122.213009119955)) ;
#105483 = CARTESIAN_POINT('Ctrl Pts',(-19.8961971448971,-50.1901409854144,
121.960910506346)) ;
#105484 = CARTESIAN_POINT('Ctrl Pts',(-19.371100043134,-50.2101229315897,
121.881727304474)) ;
#105485 = CARTESIAN_POINT('Ctrl Pts',(-18.8517714383784,-50.2300520306265,
121.986501624577)) ;
#105486 = CARTESIAN_POINT('Ctrl Pts',(-18.3995164456027,-50.2499806538391,
122.262017321329)) ;
#105487 = CARTESIAN_POINT('Ctrl Pts',(-18.069133225432,-50.2698149779455,
122.672869051133)) ;
#105488 = CARTESIAN_POINT('Ctrl Pts',(-17.9257188048663,-50.2864672653289,
123.091488247469)) ;
#105489 = CARTESIAN_POINT('Ctrl Pts',(-17.9020768429416,-50.2997277663511,
123.439219687815)) ;
#105490 = CARTESIAN_POINT('Ctrl Pts',(-17.9295576940747,-50.3097292435524,
123.700602593401)) ;
#105491 = CARTESIAN_POINT('Ctrl Pts',(-18.002656042515,-50.3197612644119,
123.953904108933)) ;
#105492 = CARTESIAN_POINT('Ctrl Pts',(-18.116386829973,-50.3296248081375,
124.186815776923)) ;
#105493 = CARTESIAN_POINT('Ctrl Pts',(-18.2699017108944,-50.3395935218076,
124.399094862358)) ;
#105494 = CARTESIAN_POINT('Ctrl Pts',(-18.5219731604255,-50.3529392692113,
124.642904643336)) ;
#105495 = CARTESIAN_POINT('Ctrl Pts',(-18.8271317055665,-50.366089824284,
124.813386630416)) ;
#105496 = CARTESIAN_POINT('Ctrl Pts',(-19.1680474112168,-50.3794752048338,
124.899924395506)) ;
#105497 = CARTESIAN_POINT('Ctrl Pts',(-19.4272102985137,-50.3893631408267,
124.919149230218)) ;
#105498 = CARTESIAN_POINT('Ctrl Pts',(-19.6884530721006,-50.3993543306393,
124.893257415268)) ;
#105499 = CARTESIAN_POINT('Ctrl Pts',(-19.9403450283617,-50.4093064291776,
124.822764313045)) ;
#105500 = CARTESIAN_POINT('Ctrl Pts',(-20.1782748640547,-50.4193526856281,
124.708404581415)) ;
#105501 = CARTESIAN_POINT('Ctrl Pts',(-20.3886616952028,-50.4292021330222,
124.55762525938)) ;
#105502 = CARTESIAN_POINT('Ctrl Pts',(-20.5723317337679,-50.4391647855174,
124.371065949195)) ;
#105503 = CARTESIAN_POINT('Ctrl Pts',(-20.7214333851646,-50.4491878711595,
124.153934546895)) ;
#105504 = CARTESIAN_POINT('Ctrl Pts',(-20.8297858694376,-50.4591129869164,
123.916652445147)) ;
#105505 = CARTESIAN_POINT('Ctrl Pts',(-20.8960168696597,-50.4691654653163,
123.660946913908)) ;
#105506 = CARTESIAN_POINT('Ctrl Pts',(-20.9166037059943,-50.479016964019,
123.402860359197)) ;
#105507 = CARTESIAN_POINT('Ctrl Pts',(-20.8924513733458,-50.4889887032215,
123.141962294283)) ;
#105508 = CARTESIAN_POINT('Ctrl Pts',(-20.8231514064948,-50.4989839109872,
122.888561525086)) ;
#105509 = CARTESIAN_POINT('Ctrl Pts',(-20.7102071657759,-50.5090179124563,
122.650317770348)) ;
#105510 = CARTESIAN_POINT('Ctrl Pts',(-20.5606367267542,-50.5188732705486,
122.43885338085)) ;
#105511 = CARTESIAN_POINT('Ctrl Pts',(-20.3742312146974,-50.5288727461419,
122.253706506383)) ;
#105512 = CARTESIAN_POINT('Ctrl Pts',(-20.160865960504,-50.538767194637,122.10501554527)) ;
#105513 = CARTESIAN_POINT('Ctrl Pts',(-19.9209557482341,-50.5488303188647,
121.993876783106)) ;
#105514 = CARTESIAN_POINT('Ctrl Pts',(-19.6710568689781,-50.5586699451933,
121.927289939446)) ;
#105515 = CARTESIAN_POINT('Ctrl Pts',(-19.4076455171057,-50.5687331802363,
121.904273103064)) ;
#105516 = CARTESIAN_POINT('Ctrl Pts',(-19.1486245172378,-50.5786271854703,
121.927179702334)) ;
#105517 = CARTESIAN_POINT('Ctrl Pts',(-18.8961488717579,-50.5885698986861,
121.994338288272)) ;
#105518 = CARTESIAN_POINT('Ctrl Pts',(-18.6575937125495,-50.5985756384843,
122.10498927942)) ;
#105519 = CARTESIAN_POINT('Ctrl Pts',(-18.4417453764348,-50.6085965406307,
122.255832615603)) ;
#105520 = CARTESIAN_POINT('Ctrl Pts',(-18.2575664390002,-50.6184873106796,
122.439245530965)) ;
#105521 = CARTESIAN_POINT('Ctrl Pts',(-18.106199313767,-50.6284787214593,
122.653775573156)) ;
#105522 = CARTESIAN_POINT('Ctrl Pts',(-17.994939377062,-50.6384270671238,
122.890345311721)) ;
#105523 = CARTESIAN_POINT('Ctrl Pts',(-17.9259303257963,-50.648371925185,
123.142434021388)) ;
#105524 = CARTESIAN_POINT('Ctrl Pts',(-17.9018642723726,-50.6584267605779,
123.40554120748)) ;
#105525 = CARTESIAN_POINT('Ctrl Pts',(-17.9228963383738,-50.6682491326794,
123.662827558674)) ;
#105526 = CARTESIAN_POINT('Ctrl Pts',(-17.9893655669342,-50.6783050001231,
123.918569075764)) ;
#105527 = CARTESIAN_POINT('Ctrl Pts',(-18.0984078853654,-50.688245729981,
124.155965789907)) ;
#105528 = CARTESIAN_POINT('Ctrl Pts',(-18.2457954157067,-50.6981500685321,
124.370495273016)) ;
#105529 = CARTESIAN_POINT('Ctrl Pts',(-18.4309155957162,-50.7081967499607,
124.558705815909)) ;
#105530 = CARTESIAN_POINT('Ctrl Pts',(-18.6425827603139,-50.7180922574299,
124.709841133587)) ;
#105531 = CARTESIAN_POINT('Ctrl Pts',(-18.8811592255437,-50.7281545259285,
124.823777836074)) ;
#105532 = CARTESIAN_POINT('Ctrl Pts',(-19.1303439298088,-50.7379965161991,
124.893182940593)) ;
#105533 = CARTESIAN_POINT('Ctrl Pts',(-19.3916248824372,-50.7479899330801,
124.919232757977)) ;
#105534 = CARTESIAN_POINT('Ctrl Pts',(-19.6517236646734,-50.7579144209322,
124.899673740811)) ;
#105535 = CARTESIAN_POINT('Ctrl Pts',(-19.9064096763508,-50.7679140548407,
124.835042611516)) ;
#105536 = CARTESIAN_POINT('Ctrl Pts',(-20.1457402038609,-50.7779001650975,
124.727300269212)) ;
#105537 = CARTESIAN_POINT('Ctrl Pts',(-20.3636013964809,-50.7879361162846,
124.578709908681)) ;
#105538 = CARTESIAN_POINT('Ctrl Pts',(-20.5492892152705,-50.7977927546194,
124.398083228579)) ;
#105539 = CARTESIAN_POINT('Ctrl Pts',(-20.7032288955082,-50.8077917146974,
124.18519187754)) ;
#105540 = CARTESIAN_POINT('Ctrl Pts',(-20.8169684935158,-50.8176869450112,
123.95130100847)) ;
#105541 = CARTESIAN_POINT('Ctrl Pts',(-20.8895126689177,-50.8277474574798,
123.697104486411)) ;
#105542 = CARTESIAN_POINT('Ctrl Pts',(-20.9163960233827,-50.837596749026,
123.439654669857)) ;
#105543 = CARTESIAN_POINT('Ctrl Pts',(-20.8985077215947,-50.8476239349582,
123.176765287496)) ;
#105544 = CARTESIAN_POINT('Ctrl Pts',(-20.8345597388551,-50.8576524714175,
122.921088430059)) ;
#105545 = CARTESIAN_POINT('Ctrl Pts',(-20.7296110651712,-50.8674977113825,
122.684622614722)) ;
#105546 = CARTESIAN_POINT('Ctrl Pts',(-20.5836373894201,-50.8774884063057,
122.466391230492)) ;
#105547 = CARTESIAN_POINT('Ctrl Pts',(-20.4007156047811,-50.8875262270643,
122.276336681186)) ;
#105548 = CARTESIAN_POINT('Ctrl Pts',(-20.1919297062301,-50.8973708208412,
122.123562264612)) ;
#105549 = CARTESIAN_POINT('Ctrl Pts',(-19.9567750355557,-50.9073548162173,
122.007254388353)) ;
#105550 = CARTESIAN_POINT('Ctrl Pts',(-19.7058360968949,-50.9173038647787,
121.933818914546)) ;
#105551 = CARTESIAN_POINT('Ctrl Pts',(-19.4445977592879,-50.9273063037532,
121.904634485153)) ;
#105552 = CARTESIAN_POINT('Ctrl Pts',(-19.1817978691591,-50.9373275450496,
121.921640529881)) ;
#105553 = CARTESIAN_POINT('Ctrl Pts',(-18.9291516129592,-50.9472202234891,
121.982914385195)) ;
#105554 = CARTESIAN_POINT('Ctrl Pts',(-18.6884726742296,-50.9572102774367,
122.087763857683)) ;
#105555 = CARTESIAN_POINT('Ctrl Pts',(-18.4704576208751,-50.9671686385852,
122.232502141319)) ;
#105556 = CARTESIAN_POINT('Ctrl Pts',(-18.2815439794151,-50.97706826547,122.411385729391)) ;
#105557 = CARTESIAN_POINT('Ctrl Pts',(-18.1243401709287,-50.9871161622734,
122.623503415483)) ;
#105558 = CARTESIAN_POINT('Ctrl Pts',(-18.0079328095563,-50.9970115199094,
122.856078803486)) ;
#105559 = CARTESIAN_POINT('Ctrl Pts',(-17.9324125309766,-51.0070731723661,
123.109443165395)) ;
#105560 = CARTESIAN_POINT('Ctrl Pts',(-17.9026431920304,-51.016917776638,
123.366440022436)) ;
#105561 = CARTESIAN_POINT('Ctrl Pts',(-17.9171914556696,-51.026877898336,
123.627772544712)) ;
#105562 = CARTESIAN_POINT('Ctrl Pts',(-17.9778575855944,-51.0369159326985,
123.884480568244)) ;
#105563 = CARTESIAN_POINT('Ctrl Pts',(-18.0800533841894,-51.046790245285,
124.123030915168)) ;
#105564 = CARTESIAN_POINT('Ctrl Pts',(-18.2248973712066,-51.0568597260677,
124.344440963174)) ;
#105565 = CARTESIAN_POINT('Ctrl Pts',(-18.4016942575522,-51.0666940620848,
124.532971381553)) ;
#105566 = CARTESIAN_POINT('Ctrl Pts',(-18.6122597307479,-51.076727019813,
124.691628705257)) ;
#105567 = CARTESIAN_POINT('Ctrl Pts',(-18.8472201491043,-51.0867474183882,
124.810522126315)) ;
#105568 = CARTESIAN_POINT('Ctrl Pts',(-19.095186956978,-51.0966129921594,
124.886265732947)) ;
#105569 = CARTESIAN_POINT('Ctrl Pts',(-19.357793794437,-51.1066818668155,
124.918452072339)) ;
#105570 = CARTESIAN_POINT('Ctrl Pts',(-19.6161806221117,-51.116527297721,
124.904898127975)) ;
#105571 = CARTESIAN_POINT('Ctrl Pts',(-19.871892695951,-51.1265069225917,
124.846720906365)) ;
#105572 = CARTESIAN_POINT('Ctrl Pts',(-20.1143711448199,-51.1365256055058,
124.744169162022)) ;
#105573 = CARTESIAN_POINT('Ctrl Pts',(-20.3327050133308,-51.1464088706896,
124.603447512875)) ;
#105574 = CARTESIAN_POINT('Ctrl Pts',(-20.5267220753818,-51.156477164781,
124.423616988893)) ;
#105575 = CARTESIAN_POINT('Ctrl Pts',(-20.6830811763147,-51.1663072949663,
124.217930329721)) ;
#105576 = CARTESIAN_POINT('Ctrl Pts',(-20.8044599409609,-51.1763738431815,
123.982929680634)) ;
#105577 = CARTESIAN_POINT('Ctrl Pts',(-20.881680652614,-51.1862640918701,
123.734726833842)) ;
#105578 = CARTESIAN_POINT('Ctrl Pts',(-20.9155355018185,-51.1962562736461,
123.474349688364)) ;
#105579 = CARTESIAN_POINT('Ctrl Pts',(-20.9034548595314,-51.2062190542739,
123.212821923773)) ;
#105580 = CARTESIAN_POINT('Ctrl Pts',(-20.8471147183909,-51.2161234589477,
122.958696270811)) ;
#105581 = CARTESIAN_POINT('Ctrl Pts',(-20.7457750358566,-51.2261834534267,
122.714550697447)) ;
#105582 = CARTESIAN_POINT('Ctrl Pts',(-20.6067346798878,-51.2360320753965,
122.496235768435)) ;
#105583 = CARTESIAN_POINT('Ctrl Pts',(-20.4291331957846,-51.2460625148083,
122.301482009075)) ;
#105584 = CARTESIAN_POINT('Ctrl Pts',(-20.2204863343757,-51.2560722304431,
122.14124999381)) ;
#105585 = CARTESIAN_POINT('Ctrl Pts',(-19.9896575967978,-51.2659829831357,
122.020681381118)) ;
#105586 = CARTESIAN_POINT('Ctrl Pts',(-19.7411001533727,-51.2759122560821,
121.941241152723)) ;
#105587 = CARTESIAN_POINT('Ctrl Pts',(-19.4795647357375,-51.2859549474748,
121.905989503812)) ;
#105588 = CARTESIAN_POINT('Ctrl Pts',(-19.2199484999009,-51.2958414806923,
121.916349708964)) ;
#105589 = CARTESIAN_POINT('Ctrl Pts',(-18.9632715215848,-51.3058346256243,
121.971785234731)) ;
#105590 = CARTESIAN_POINT('Ctrl Pts',(-18.7212976545593,-51.3157803064608,
122.070573488031)) ;
#105591 = CARTESIAN_POINT('Ctrl Pts',(-18.49982192186,-51.3257275636094,122.209451826745)) ;
#105592 = CARTESIAN_POINT('Ctrl Pts',(-18.3040765935433,-51.3357754674813,
122.386654309068)) ;
#105593 = CARTESIAN_POINT('Ctrl Pts',(-18.1451228804641,-51.3456231665793,
122.590872919258)) ;
#105594 = CARTESIAN_POINT('Ctrl Pts',(-18.0219193554534,-51.355584657558,
122.821834110184)) ;
#105595 = CARTESIAN_POINT('Ctrl Pts',(-17.9404646597919,-51.3656141199719,
123.072506175138)) ;
#105596 = CARTESIAN_POINT('Ctrl Pts',(-17.9040809682296,-51.3755213510718,
123.330303605166)) ;
#105597 = CARTESIAN_POINT('Ctrl Pts',(-17.9125155161275,-51.3854677297493,
123.591532484831)) ;
#105598 = CARTESIAN_POINT('Ctrl Pts',(-17.9664112488074,-51.3954724985581,
123.848886998314)) ;
#105599 = CARTESIAN_POINT('Ctrl Pts',(-18.0646024092112,-51.4054936195783,
124.093235374132)) ;
#105600 = CARTESIAN_POINT('Ctrl Pts',(-18.2016748070809,-51.4153844854309,
124.314086593535)) ;
#105601 = CARTESIAN_POINT('Ctrl Pts',(-18.3764583415646,-51.4253752941902,
124.509980152437)) ;
#105602 = CARTESIAN_POINT('Ctrl Pts',(-18.5818247469521,-51.4353259523705,
124.671874876727)) ;
#105603 = CARTESIAN_POINT('Ctrl Pts',(-18.8116522149616,-51.4452621620126,
124.795765081185)) ;
#105604 = CARTESIAN_POINT('Ctrl Pts',(-19.0606147398016,-51.4552453287375,
124.87859535558)) ;
#105605 = CARTESIAN_POINT('Ctrl Pts',(-19.3217627463815,-51.4652891259478,
124.916679949028)) ;
#105606 = CARTESIAN_POINT('Ctrl Pts',(-19.5799813331497,-51.4751173421161,
124.909619362426)) ;
#105607 = CARTESIAN_POINT('Ctrl Pts',(-19.8393782432694,-51.4851939095853,
124.856664288692)) ;
#105608 = CARTESIAN_POINT('Ctrl Pts',(-20.0803045545237,-51.4950459952747,
124.761719728551)) ;
#105609 = CARTESIAN_POINT('Ctrl Pts',(-20.306073135477,-51.5051192626801,
124.623591191497)) ;
#105610 = CARTESIAN_POINT('Ctrl Pts',(-20.4998622506351,-51.5149606791037,
124.452299627734)) ;
#105611 = CARTESIAN_POINT('Ctrl Pts',(-20.6636747138412,-51.5249219372464,
124.24813177878)) ;
#105612 = CARTESIAN_POINT('Ctrl Pts',(-20.7900568456154,-51.5349586136784,
124.016635338935)) ;
#105613 = CARTESIAN_POINT('Ctrl Pts',(-20.8734225094882,-51.5448372215422,
123.770756105118)) ;
#105614 = CARTESIAN_POINT('Ctrl Pts',(-20.9136026213356,-51.554897450181,
123.509489974879)) ;
#105615 = CARTESIAN_POINT('Ctrl Pts',(-20.9079937843595,-51.5647644343418,
123.250223069463)) ;
#105616 = CARTESIAN_POINT('Ctrl Pts',(-20.8572543274689,-51.5747700005945,
122.992264994515)) ;
#105617 = CARTESIAN_POINT('Ctrl Pts',(-20.7626104316149,-51.5847537890091,
122.747517362774)) ;
#105618 = CARTESIAN_POINT('Ctrl Pts',(-20.6258531267802,-51.5947996458117,
122.521731422933)) ;
#105619 = CARTESIAN_POINT('Ctrl Pts',(-20.4560156427673,-51.6046255230277,
122.327231639573)) ;
#105620 = CARTESIAN_POINT('Ctrl Pts',(-20.2521594332448,-51.614615998869,
122.161794290385)) ;
#105621 = CARTESIAN_POINT('Ctrl Pts',(-20.0211183356917,-51.6246595747678,
122.034194822812)) ;
#105622 = CARTESIAN_POINT('Ctrl Pts',(-19.7771218627311,-51.6344813670658,
121.950027748403)) ;
#105623 = CARTESIAN_POINT('Ctrl Pts',(-19.5167861488625,-51.6445163326917,
121.907987506781)) ;
#105624 = CARTESIAN_POINT('Ctrl Pts',(-19.2533739592759,-51.6545412496248,
121.912518592309)) ;
#105625 = CARTESIAN_POINT('Ctrl Pts',(-18.9991057307771,-51.6643931880009,
121.961295351794)) ;
#105626 = CARTESIAN_POINT('Ctrl Pts',(-18.7536483063783,-51.6743841640256,
122.054393070436)) ;
#105627 = CARTESIAN_POINT('Ctrl Pts',(-18.5295887727591,-51.6843019848293,
122.187596659951)) ;
#105628 = CARTESIAN_POINT('Ctrl Pts',(-18.3298720780152,-51.6943307053939,
122.35950935101)) ;
#105629 = CARTESIAN_POINT('Ctrl Pts',(-18.1652929595481,-51.7042136320031,
122.560450226182)) ;
#105630 = CARTESIAN_POINT('Ctrl Pts',(-18.0362039840031,-51.7142179171226,
122.78944338197)) ;
#105631 = CARTESIAN_POINT('Ctrl Pts',(-17.9490199350489,-51.7242015983304,
123.03694165535)) ;
#105632 = CARTESIAN_POINT('Ctrl Pts',(-17.9061972167895,-51.7342425970603,
123.297290625367)) ;
#105633 = CARTESIAN_POINT('Ctrl Pts',(-17.908803361231,-51.7440750419275,
123.555667262023)) ;
#105634 = CARTESIAN_POINT('Ctrl Pts',(-17.9562536617095,-51.7540700403578,
123.813996341053)) ;
#105635 = CARTESIAN_POINT('Ctrl Pts',(-18.0487087052507,-51.7641015891074,
124.060885187494)) ;
#105636 = CARTESIAN_POINT('Ctrl Pts',(-18.1801140761451,-51.7739669674129,
124.284351123223)) ;
#105637 = CARTESIAN_POINT('Ctrl Pts',(-18.3494200817977,-51.7839288148732,
124.484031080375)) ;
#105638 = CARTESIAN_POINT('Ctrl Pts',(-18.5525603287765,-51.7939637556874,
124.65216255298)) ;
#105639 = CARTESIAN_POINT('Ctrl Pts',(-18.7782099405819,-51.8038487167046,
124.780926155321)) ;
#105640 = CARTESIAN_POINT('Ctrl Pts',(-19.0272027318683,-51.8139143256234,
124.870073403993)) ;
#105641 = CARTESIAN_POINT('Ctrl Pts',(-19.2820659565915,-51.8237535006651,
124.913900713737)) ;
#105642 = CARTESIAN_POINT('Ctrl Pts',(-19.5464673888862,-51.833816056165,
124.913150026589)) ;
#105643 = CARTESIAN_POINT('Ctrl Pts',(-19.8024397374806,-51.843713230858,
124.866983100272)) ;
#105644 = CARTESIAN_POINT('Ctrl Pts',(-20.0476185001334,-51.8536439457813,
124.777597590516)) ;
#105645 = CARTESIAN_POINT('Ctrl Pts',(-20.2759776925336,-51.8636879738589,
124.645246173051)) ;
#105646 = CARTESIAN_POINT('Ctrl Pts',(-20.4748636938545,-51.8735741757122,
124.47806599248)) ;
#105647 = CARTESIAN_POINT('Ctrl Pts',(-20.6437806069074,-51.8835673421791,
124.277027652235)) ;
#105648 = CARTESIAN_POINT('Ctrl Pts',(-20.7746158733982,-51.8935068131662,
124.050921132866)) ;
#105649 = CARTESIAN_POINT('Ctrl Pts',(-20.864926632437,-51.9035233275204,
123.803704134483)) ;
#105650 = CARTESIAN_POINT('Ctrl Pts',(-20.9107718686361,-51.9134533539972,
123.546775177275)) ;
#105651 = CARTESIAN_POINT('Ctrl Pts',(-20.9111996492547,-51.9235058895067,
123.282627938416)) ;
#105652 = CARTESIAN_POINT('Ctrl Pts',(-20.8668285985531,-51.9333522927264,
123.027698354872)) ;
#105653 = CARTESIAN_POINT('Ctrl Pts',(-20.7786383276928,-51.9433143355804,
122.781223584953)) ;
#105654 = CARTESIAN_POINT('Ctrl Pts',(-20.6478126513841,-51.9533428863711,
122.552428957357)) ;
#105655 = CARTESIAN_POINT('Ctrl Pts',(-20.4813210380991,-51.9632532120887,
122.352179823965)) ;
#105656 = CARTESIAN_POINT('Ctrl Pts',(-20.2825219245844,-51.9731881239183,
122.182930241448)) ;
#105657 = CARTESIAN_POINT('Ctrl Pts',(-20.0548415494281,-51.9832291306864,
122.049575194896)) ;
#105658 = CARTESIAN_POINT('Ctrl Pts',(-19.8112844642767,-51.9931167635186,
121.959011480888)) ;
#105659 = CARTESIAN_POINT('Ctrl Pts',(-19.5531552028146,-52.0031071946166,
121.911171970469)) ;
#105660 = CARTESIAN_POINT('Ctrl Pts',(-19.2915375054555,-52.0130626311739,
121.909027597134)) ;
#105661 = CARTESIAN_POINT('Ctrl Pts',(-19.034617991688,-52.0229735792732,
121.951673016826)) ;
#105662 = CARTESIAN_POINT('Ctrl Pts',(-18.7863603364124,-52.0329856553709,
122.038889445469)) ;
#105663 = CARTESIAN_POINT('Ctrl Pts',(-18.5569711609349,-52.0430129774459,
122.168521876009)) ;
#105664 = CARTESIAN_POINT('Ctrl Pts',(-18.3565229470281,-52.0528717524,122.332741737178)) ;
#105665 = CARTESIAN_POINT('Ctrl Pts',(-18.1268595349139,-52.0662979452124,
122.600459541872)) ;
#105666 = CARTESIAN_POINT('Ctrl Pts',(-17.9756578065929,-52.0793819609939,
122.913770905691)) ;
#105667 = CARTESIAN_POINT('Ctrl Pts',(-17.9092075693229,-52.0928554097491,
123.261476632465)) ;
#105668 = CARTESIAN_POINT('Ctrl Pts',(-17.9058669085398,-52.1026883675549,
123.519888511161)) ;
#105669 = CARTESIAN_POINT('Ctrl Pts',(-17.9468914650355,-52.1126516410056,
123.778461358619)) ;
#105670 = CARTESIAN_POINT('Ctrl Pts',(-18.0333653429648,-52.1226887148236,
124.027643619177)) ;
#105671 = CARTESIAN_POINT('Ctrl Pts',(-18.1593058164668,-52.1325637178352,
124.254574691994)) ;
#105672 = CARTESIAN_POINT('Ctrl Pts',(-18.3258898060172,-52.1426313974614,
124.460065581407)) ;
#105673 = CARTESIAN_POINT('Ctrl Pts',(-18.5210760121677,-52.1524722476791,
124.629759584367)) ;
#105674 = CARTESIAN_POINT('Ctrl Pts',(-18.821066323113,-52.1658084461551,
124.810893970577)) ;
#105675 = CARTESIAN_POINT('Ctrl Pts',(-19.1585367061457,-52.1790259699695,
124.908593466705)) ;
#105676 = CARTESIAN_POINT('Ctrl Pts',(-19.5088651508526,-52.1923608964608,
124.916062617369)) ;
#105677 = CARTESIAN_POINT('Ctrl Pts',(-19.7681923500913,-52.2023439970554,
124.87610822169)) ;
#105678 = CARTESIAN_POINT('Ctrl Pts',(-20.017988630059,-52.212388772955,124.790864379723)) ;
#105679 = CARTESIAN_POINT('Ctrl Pts',(-20.244250111229,-52.2222066961409,
124.6668494841)) ;
#105680 = CARTESIAN_POINT('Ctrl Pts',(-20.450605569741,-52.2322560100963,
124.502062270369)) ;
#105681 = CARTESIAN_POINT('Ctrl Pts',(-20.681220352099,-52.2455597507188,
124.239335951063)) ;
#105682 = CARTESIAN_POINT('Ctrl Pts',(-20.8766427398963,-52.2620499461955,
123.846935211259)) ;
#105683 = CARTESIAN_POINT('Ctrl Pts',(-20.9269324311696,-52.2787691111201,
123.40555050436)) ;
#105684 = CARTESIAN_POINT('Ctrl Pts',(-20.8757860399941,-52.2919301047903,
123.06342307163)) ;
#105685 = CARTESIAN_POINT('Ctrl Pts',(-20.7933342692634,-52.3019263268955,
122.814030291687)) ;
#105686 = CARTESIAN_POINT('Ctrl Pts',(-20.6679526627159,-52.3119501664292,
122.582364382692)) ;
#105687 = CARTESIAN_POINT('Ctrl Pts',(-20.4530759574167,-52.3251434884225,
122.310238877443)) ;
#105688 = CARTESIAN_POINT('Ctrl Pts',(-20.0984661627794,-52.3418026601998,
122.045166826132)) ;
#105689 = CARTESIAN_POINT('Ctrl Pts',(-19.5917771670296,-52.3617128356855,
121.892473324342)) ;
#105690 = CARTESIAN_POINT('Ctrl Pts',(-19.0638317581949,-52.3816028235299,
121.920720400418)) ;
#105691 = CARTESIAN_POINT('Ctrl Pts',(-18.5747188817248,-52.4016082715447,
122.129015928262)) ;
#105692 = CARTESIAN_POINT('Ctrl Pts',(-18.1887873835307,-52.421444665572,
122.488412492527)) ;
#105693 = CARTESIAN_POINT('Ctrl Pts',(-17.9465342575995,-52.4414524594687,
122.961640970763)) ;
#105694 = CARTESIAN_POINT('Ctrl Pts',(-17.8806979911709,-52.4612790957627,
123.484567234561)) ;
#105695 = CARTESIAN_POINT('Ctrl Pts',(-17.9971902184704,-52.4812580387165,
124.002618696318)) ;
#105696 = CARTESIAN_POINT('Ctrl Pts',(-18.283564362864,-52.5011898405856,
124.44821305183)) ;
#105697 = CARTESIAN_POINT('Ctrl Pts',(-18.7016410326483,-52.5210141410831,
124.769156799688)) ;
#105698 = CARTESIAN_POINT('Ctrl Pts',(-19.2109481937342,-52.5411101424229,
124.929334135715)) ;
#105699 = CARTESIAN_POINT('Ctrl Pts',(-19.7359311031487,-52.5608685585269,
124.907024725982)) ;
#105700 = CARTESIAN_POINT('Ctrl Pts',(-20.2295133744255,-52.580962251411,
124.703919481245)) ;
#105701 = CARTESIAN_POINT('Ctrl Pts',(-20.4872495056866,-52.5940732173177,
124.469072010777)) ;
#105702 = CARTESIAN_POINT('Ctrl Pts',(-20.5950554345716,-52.6007865921055,
124.330331920903)) ;
#105703 = CARTESIAN_POINT('',(-18.0926293799299,-13.5522956097346,122.693350211338)) ;
#105704 = CARTESIAN_POINT('Ctrl Pts',(-18.4227818193872,-12.5498512937297,
124.541625342821)) ;
#105705 = CARTESIAN_POINT('Ctrl Pts',(-18.4694019331331,-12.5522145745311,
124.582298797486)) ;
#105706 = CARTESIAN_POINT('Ctrl Pts',(-18.5877612762874,-12.5579111037291,
124.673475350218)) ;
#105707 = CARTESIAN_POINT('Ctrl Pts',(-18.794133205315,-12.5668945320791,
124.78820420773)) ;
#105708 = CARTESIAN_POINT('Ctrl Pts',(-19.0439677038418,-12.5769520351743,
124.874329341901)) ;
#105709 = CARTESIAN_POINT('Ctrl Pts',(-19.2988434093258,-12.5867736915449,
124.91519672569)) ;
#105710 = CARTESIAN_POINT('Ctrl Pts',(-19.5630599609083,-12.59682975421,124.911586781273)) ;
#105711 = CARTESIAN_POINT('Ctrl Pts',(-19.8196010841879,-12.6067704189132,
124.862254027796)) ;
#105712 = CARTESIAN_POINT('Ctrl Pts',(-20.0630721998832,-12.6166748228617,
124.770231291142)) ;
#105713 = CARTESIAN_POINT('Ctrl Pts',(-20.2899726794303,-12.6267213078553,
124.63529723127)) ;
#105714 = CARTESIAN_POINT('Ctrl Pts',(-20.4871951419804,-12.636617535667,
124.46572279971)) ;
#105715 = CARTESIAN_POINT('Ctrl Pts',(-20.6546905094441,-12.6466771192305,
124.261238010029)) ;
#105716 = CARTESIAN_POINT('Ctrl Pts',(-20.7815104793504,-12.6565291288993,
124.035511186315)) ;
#105717 = CARTESIAN_POINT('Ctrl Pts',(-20.8689934761397,-12.6664916603389,
123.788768205197)) ;
#105718 = CARTESIAN_POINT('Ctrl Pts',(-20.9122064367509,-12.6765232085783,
123.528706986233)) ;
#105719 = CARTESIAN_POINT('Ctrl Pts',(-20.9098929873906,-12.6864146197913,
123.268781131544)) ;
#105720 = CARTESIAN_POINT('Ctrl Pts',(-20.8623508858351,-12.6964308734993,
123.009883889903)) ;
#105721 = CARTESIAN_POINT('Ctrl Pts',(-20.769920509206,-12.706460976344,122.763045735835)) ;
#105722 = CARTESIAN_POINT('Ctrl Pts',(-20.6387698639911,-12.7163174252977,
122.539667034596)) ;
#105723 = CARTESIAN_POINT('Ctrl Pts',(-20.468686507231,-12.72631643607,122.339431415899)) ;
#105724 = CARTESIAN_POINT('Ctrl Pts',(-20.2686378940791,-12.736211652988,
122.173234495552)) ;
#105725 = CARTESIAN_POINT('Ctrl Pts',(-20.0390498000103,-12.7462721683453,
122.042207516489)) ;
#105726 = CARTESIAN_POINT('Ctrl Pts',(-19.7954221880598,-12.7561214617324,
121.954750952006)) ;
#105727 = CARTESIAN_POINT('Ctrl Pts',(-19.5358430756164,-12.7661486374124,
121.909479848498)) ;
#105728 = CARTESIAN_POINT('Ctrl Pts',(-19.2722925736252,-12.7761772130396,
121.910661435614)) ;
#105729 = CARTESIAN_POINT('Ctrl Pts',(-19.0176320504801,-12.7860223065854,
121.956236242395)) ;
#105730 = CARTESIAN_POINT('Ctrl Pts',(-18.7708959417052,-12.7960135480172,
122.046015059974)) ;
#105731 = CARTESIAN_POINT('Ctrl Pts',(-18.5427539301237,-12.8060493291605,
122.178333355514)) ;
#105732 = CARTESIAN_POINT('Ctrl Pts',(-18.344530793837,-12.8159015348902,
122.344872755127)) ;
#105733 = CARTESIAN_POINT('Ctrl Pts',(-18.1757936891155,-12.8258636290072,
122.545026044335)) ;
#105734 = CARTESIAN_POINT('Ctrl Pts',(-18.0438514585141,-12.8358861898343,
122.772976611802)) ;
#105735 = CARTESIAN_POINT('Ctrl Pts',(-17.9540972344567,-12.8458139614859,
123.017969138429)) ;
#105736 = CARTESIAN_POINT('Ctrl Pts',(-17.9077512439174,-12.8558563456107,
123.27775092553)) ;
#105737 = CARTESIAN_POINT('Ctrl Pts',(-17.9071170334874,-12.8657455696813,
123.537644244839)) ;
#105738 = CARTESIAN_POINT('Ctrl Pts',(-17.951578905651,-12.8757348178486,
123.796349682054)) ;
#105739 = CARTESIAN_POINT('Ctrl Pts',(-18.0402013685863,-12.8856933948906,
124.042581000348)) ;
#105740 = CARTESIAN_POINT('Ctrl Pts',(-18.1689146990719,-12.8955929639819,
124.268677154619)) ;
#105741 = CARTESIAN_POINT('Ctrl Pts',(-18.3374623673469,-12.9056408760659,
124.471898543285)) ;
#105742 = CARTESIAN_POINT('Ctrl Pts',(-18.5355994492501,-12.9155362303731,
124.640372901657)) ;
#105743 = CARTESIAN_POINT('Ctrl Pts',(-18.7636696514608,-12.9255978808643,
124.774091983327)) ;
#105744 = CARTESIAN_POINT('Ctrl Pts',(-19.0061700042819,-12.9354424963268,
124.864243378729)) ;
#105745 = CARTESIAN_POINT('Ctrl Pts',(-19.263440320499,-12.9454025752282,
124.912387637213)) ;
#105746 = CARTESIAN_POINT('Ctrl Pts',(-19.527213442044,-12.9554407695865,
124.914637912278)) ;
#105747 = CARTESIAN_POINT('Ctrl Pts',(-19.7832305957041,-12.9653144849861,
124.872237771651)) ;
#105748 = CARTESIAN_POINT('Ctrl Pts',(-20.0328289090505,-12.9753861945204,
124.784297245069)) ;
#105749 = CARTESIAN_POINT('Ctrl Pts',(-20.2580129538926,-12.9852186349729,
124.65754226709)) ;
#105750 = CARTESIAN_POINT('Ctrl Pts',(-20.4622619532301,-12.9952504558983,
124.49087643455)) ;
#105751 = CARTESIAN_POINT('Ctrl Pts',(-20.6337103450931,-13.0052708257839,
124.291008668358)) ;
#105752 = CARTESIAN_POINT('Ctrl Pts',(-20.7663859266914,-13.0151375969176,
124.068214529218)) ;
#105753 = CARTESIAN_POINT('Ctrl Pts',(-20.860238962856,-13.025208368107,123.82079438421)) ;
#105754 = CARTESIAN_POINT('Ctrl Pts',(-20.9086253549924,-13.0350515286286,
123.566676912894)) ;
#105755 = CARTESIAN_POINT('Ctrl Pts',(-20.913063221591,-13.045031761815,123.304452798709)) ;
#105756 = CARTESIAN_POINT('Ctrl Pts',(-20.871244216678,-13.0550502818502,
123.044526148757)) ;
#105757 = CARTESIAN_POINT('Ctrl Pts',(-20.7866033496793,-13.0649335902339,
122.798947963481)) ;
#105758 = CARTESIAN_POINT('Ctrl Pts',(-20.6581851562813,-13.0750018744047,
122.567668252138)) ;
#105759 = CARTESIAN_POINT('Ctrl Pts',(-20.4956824752415,-13.0848320010723,
122.366800045795)) ;
#105760 = CARTESIAN_POINT('Ctrl Pts',(-20.2963739380565,-13.0948985732789,
122.192919639631)) ;
#105761 = CARTESIAN_POINT('Ctrl Pts',(-20.0737240319191,-13.1047887295196,
122.058778426284)) ;
#105762 = CARTESIAN_POINT('Ctrl Pts',(-19.8289059210494,-13.114781257096,
121.963856125823)) ;
#105763 = CARTESIAN_POINT('Ctrl Pts',(-19.5720652391397,-13.1247427469703,
121.913259794537)) ;
#105764 = CARTESIAN_POINT('Ctrl Pts',(-19.3117143442224,-13.1346519688575,
121.907457127883)) ;
#105765 = CARTESIAN_POINT('Ctrl Pts',(-19.0507318169299,-13.1447005486678,
121.947593231427)) ;
#105766 = CARTESIAN_POINT('Ctrl Pts',(-18.8047453884644,-13.1545835231379,
122.030958261685)) ;
#105767 = CARTESIAN_POINT('Ctrl Pts',(-18.5741383843272,-13.1645784342806,
122.156672491579)) ;
#105768 = CARTESIAN_POINT('Ctrl Pts',(-18.3685451174446,-13.1745988208542,
122.321235274363)) ;
#105769 = CARTESIAN_POINT('Ctrl Pts',(-18.1964735381612,-13.1845089247113,
122.516696286049)) ;
#105770 = CARTESIAN_POINT('Ctrl Pts',(-18.0601155303138,-13.1944366369212,
122.739126636729)) ;
#105771 = CARTESIAN_POINT('Ctrl Pts',(-17.9635520490142,-13.2044797466884,
122.984738187644)) ;
#105772 = CARTESIAN_POINT('Ctrl Pts',(-17.9117515043607,-13.214366167144,
123.23934198587)) ;
#105773 = CARTESIAN_POINT('Ctrl Pts',(-17.9044262701095,-13.2243593447496,
123.501835598151)) ;
#105774 = CARTESIAN_POINT('Ctrl Pts',(-17.9427087756384,-13.2343050076535,
123.760379203083)) ;
#105775 = CARTESIAN_POINT('Ctrl Pts',(-18.0248121016097,-13.2442523038587,
124.008568584514)) ;
#105776 = CARTESIAN_POINT('Ctrl Pts',(-18.1502624018748,-13.2543000694366,
124.240900424645)) ;
#105777 = CARTESIAN_POINT('Ctrl Pts',(-18.3107346122859,-13.2641482826542,
124.443940073215)) ;
#105778 = CARTESIAN_POINT('Ctrl Pts',(-18.505634717484,-13.2741078554483,
124.618624665501)) ;
#105779 = CARTESIAN_POINT('Ctrl Pts',(-18.7298622874998,-13.2841444764808,
124.757486690818)) ;
#105780 = CARTESIAN_POINT('Ctrl Pts',(-18.9708689515076,-13.2940249912912,
124.854174107934)) ;
#105781 = CARTESIAN_POINT('Ctrl Pts',(-19.2293446499912,-13.3040776425982,
124.908560044492)) ;
#105782 = CARTESIAN_POINT('Ctrl Pts',(-19.4892871259414,-13.3139730408782,
124.917212832017)) ;
#105783 = CARTESIAN_POINT('Ctrl Pts',(-19.7507469643642,-13.3240231625843,
124.88015632989)) ;
#105784 = CARTESIAN_POINT('Ctrl Pts',(-19.9977291617165,-13.3339074421262,
124.799637378817)) ;
#105785 = CARTESIAN_POINT('Ctrl Pts',(-20.2297273479885,-13.3439022234181,
124.676550308236)) ;
#105786 = CARTESIAN_POINT('Ctrl Pts',(-20.4358283328775,-13.3538500686049,
124.515703848554)) ;
#105787 = CARTESIAN_POINT('Ctrl Pts',(-20.6109332605582,-13.3637870319923,
124.322011504396)) ;
#105788 = CARTESIAN_POINT('Ctrl Pts',(-20.750697973779,-13.3737699967295,
124.099960077421)) ;
#105789 = CARTESIAN_POINT('Ctrl Pts',(-20.8499157138425,-13.3838138481452,
123.855409348359)) ;
#105790 = CARTESIAN_POINT('Ctrl Pts',(-20.9045890531855,-13.3936420494799,
123.602946647312)) ;
#105791 = CARTESIAN_POINT('Ctrl Pts',(-20.9149711028211,-13.403718622078,
123.338403239339)) ;
#105792 = CARTESIAN_POINT('Ctrl Pts',(-20.8801719456267,-13.4135707020855,
123.081792606934)) ;
#105793 = CARTESIAN_POINT('Ctrl Pts',(-20.7998200890708,-13.4236439870896,
122.829613269708)) ;
#105794 = CARTESIAN_POINT('Ctrl Pts',(-20.6796429969365,-13.4334853388001,
122.600587873272)) ;
#105795 = CARTESIAN_POINT('Ctrl Pts',(-20.5203827330306,-13.4434468381966,
122.392848692112)) ;
#105796 = CARTESIAN_POINT('Ctrl Pts',(-20.3257020959426,-13.4534826143266,
122.214922798792)) ;
#105797 = CARTESIAN_POINT('Ctrl Pts',(-20.106509157136,-13.4633710409642,
122.075355463823)) ;
#105798 = CARTESIAN_POINT('Ctrl Pts',(-19.8635102674347,-13.4733863630391,
121.974225744482)) ;
#105799 = CARTESIAN_POINT('Ctrl Pts',(-19.6061332113171,-13.4834167119393,
121.917339791102)) ;
#105800 = CARTESIAN_POINT('Ctrl Pts',(-19.34772624537,-13.493260087546,121.905698547325)) ;
#105801 = CARTESIAN_POINT('Ctrl Pts',(-19.0862905181186,-13.5032895244431,
121.939151509404)) ;
#105802 = CARTESIAN_POINT('Ctrl Pts',(-18.8347838962689,-13.513321402376,
122.018199528681)) ;
#105803 = CARTESIAN_POINT('Ctrl Pts',(-18.6053189853568,-13.5231510254815,
122.136788620459)) ;
#105804 = CARTESIAN_POINT('Ctrl Pts',(-18.3960964023697,-13.5331404966346,
122.295352843074)) ;
#105805 = CARTESIAN_POINT('Ctrl Pts',(-18.2215971874487,-13.5429325945739,
122.484470246641)) ;
#105806 = CARTESIAN_POINT('Ctrl Pts',(-18.1309048848651,-13.5492395742091,
122.623087899681)) ;
#105807 = CARTESIAN_POINT('Ctrl Pts',(-18.0926293799299,-13.5522956097346,
122.693350211338)) ;
#105808 = CARTESIAN_POINT('Ctrl Pts',(-18.7495450167619,-13.6947924674762,
122.391633028028)) ;
#105809 = CARTESIAN_POINT('Ctrl Pts',(-18.6912075925582,-13.6822848109805,
122.399567618011)) ;
#105810 = CARTESIAN_POINT('Ctrl Pts',(-18.6328057351464,-13.669867630349,
122.411999690746)) ;
#105811 = CARTESIAN_POINT('Ctrl Pts',(-18.5235036267721,-13.6467016771095,
122.443881102542)) ;
#105812 = CARTESIAN_POINT('Ctrl Pts',(-18.4655747236248,-13.634580439305,
122.46483228122)) ;
#105813 = CARTESIAN_POINT('Ctrl Pts',(-18.3479127458884,-13.6094612987599,
122.519438361635)) ;
#105814 = CARTESIAN_POINT('Ctrl Pts',(-18.2944791653156,-13.597810926533,
122.548528575909)) ;
#105815 = CARTESIAN_POINT('Ctrl Pts',(-18.1905723761229,-13.57473812355,122.614744875633)) ;
#105816 = CARTESIAN_POINT('Ctrl Pts',(-18.1407505415898,-13.5635055402557,
122.651971024577)) ;
#105817 = CARTESIAN_POINT('Ctrl Pts',(-18.09262937993,-13.5522956097346,122.693350211338)) ;
#105818 = CARTESIAN_POINT('Ctrl Pts',(-17.9902032695621,-11.7999200508426,
123.897608969663)) ;
#105819 = CARTESIAN_POINT('Ctrl Pts',(-18.0463644113343,-11.8065469016607,
124.06174960631)) ;
#105820 = CARTESIAN_POINT('Ctrl Pts',(-18.215825846161,-11.8197775281417,
124.369882260699)) ;
#105821 = CARTESIAN_POINT('Ctrl Pts',(-18.6148423423544,-11.8397531494004,
124.720117056252)) ;
#105822 = CARTESIAN_POINT('Ctrl Pts',(-19.1081264048667,-11.8596704843023,
124.912158369366)) ;
#105823 = CARTESIAN_POINT('Ctrl Pts',(-19.63621175278,-11.8795437610183,124.925514984982)) ;
#105824 = CARTESIAN_POINT('Ctrl Pts',(-20.1407585698648,-11.8995682511823,
124.756261059837)) ;
#105825 = CARTESIAN_POINT('Ctrl Pts',(-20.5540259374414,-11.919436092333,
124.427422694935)) ;
#105826 = CARTESIAN_POINT('Ctrl Pts',(-20.8319874786041,-11.9393817432125,
123.976081276933)) ;
#105827 = CARTESIAN_POINT('Ctrl Pts',(-20.9388398779409,-11.9592871438295,
123.457931852337)) ;
#105828 = CARTESIAN_POINT('Ctrl Pts',(-20.863615478076,-11.9791613716459,
122.93508911423)) ;
#105829 = CARTESIAN_POINT('Ctrl Pts',(-20.613117221254,-11.9991471625235,
122.466658528729)) ;
#105830 = CARTESIAN_POINT('Ctrl Pts',(-20.2194522950349,-12.0190414051832,
122.113709218852)) ;
#105831 = CARTESIAN_POINT('Ctrl Pts',(-19.7297864118389,-12.0389201212553,
121.91511024488)) ;
#105832 = CARTESIAN_POINT('Ctrl Pts',(-19.1975736063229,-12.0589595710999,
121.896014807318)) ;
#105833 = CARTESIAN_POINT('Ctrl Pts',(-18.6950368718382,-12.0788227326378,
122.05828741974)) ;
#105834 = CARTESIAN_POINT('Ctrl Pts',(-18.2756725670237,-12.098802100652,
122.383766305065)) ;
#105835 = CARTESIAN_POINT('Ctrl Pts',(-17.9943094984244,-12.1186126811748,
122.828946957063)) ;
#105836 = CARTESIAN_POINT('Ctrl Pts',(-17.8800596440357,-12.1385936094604,
123.347467939146)) ;
#105837 = CARTESIAN_POINT('Ctrl Pts',(-17.9496692515209,-12.1584862813298,
123.871640709025)) ;
#105838 = CARTESIAN_POINT('Ctrl Pts',(-18.1935441283311,-12.1784126116169,
124.341758564742)) ;
#105839 = CARTESIAN_POINT('Ctrl Pts',(-18.5843886944494,-12.1983831657092,
124.700872483781)) ;
#105840 = CARTESIAN_POINT('Ctrl Pts',(-18.9897923054451,-12.2149150047968,
124.870323217842)) ;
#105841 = CARTESIAN_POINT('Ctrl Pts',(-19.3371476852066,-12.2282547436244,
124.917728259279)) ;
#105842 = CARTESIAN_POINT('Ctrl Pts',(-19.600561904579,-12.238286985843,124.907080238284)) ;
#105843 = CARTESIAN_POINT('Ctrl Pts',(-19.8537454249195,-12.2481446864865,
124.852220196248)) ;
#105844 = CARTESIAN_POINT('Ctrl Pts',(-20.0969791918245,-12.2581365511257,
124.753349389585)) ;
#105845 = CARTESIAN_POINT('Ctrl Pts',(-20.3177843724854,-12.2680591008858,
124.614668652868)) ;
#105846 = CARTESIAN_POINT('Ctrl Pts',(-20.5772027359822,-12.2813368743793,
124.381219928393)) ;
#105847 = CARTESIAN_POINT('Ctrl Pts',(-20.7701060086633,-12.2946842133199,
124.083600779959)) ;
#105848 = CARTESIAN_POINT('Ctrl Pts',(-20.8774610072183,-12.3078914451131,
123.753491686556)) ;
#105849 = CARTESIAN_POINT('Ctrl Pts',(-20.9145338769675,-12.3178785612028,
123.493715853778)) ;
#105850 = CARTESIAN_POINT('Ctrl Pts',(-20.9061360148182,-12.3278294667826,
123.23230208977)) ;
#105851 = CARTESIAN_POINT('Ctrl Pts',(-20.8516341650625,-12.33788456879,122.973783899849)) ;
#105852 = CARTESIAN_POINT('Ctrl Pts',(-20.7557577833189,-12.3477062421111,
122.734117231834)) ;
#105853 = CARTESIAN_POINT('Ctrl Pts',(-20.6168413508988,-12.357764713186,
122.509268747216)) ;
#105854 = CARTESIAN_POINT('Ctrl Pts',(-20.4430459892397,-12.3676893243625,
122.314784540958)) ;
#105855 = CARTESIAN_POINT('Ctrl Pts',(-20.1694463091453,-12.3809666632629,
122.098206721406)) ;
#105856 = CARTESIAN_POINT('Ctrl Pts',(-19.8449906513278,-12.3942655425005,
121.958127734837)) ;
#105857 = CARTESIAN_POINT('Ctrl Pts',(-19.5008114094801,-12.4075044146712,
121.90717382515)) ;
#105858 = CARTESIAN_POINT('Ctrl Pts',(-19.2379277204331,-12.4175110328078,
121.913961440906)) ;
#105859 = CARTESIAN_POINT('Ctrl Pts',(-18.9797053775943,-12.4275419778693,
121.966916880926)) ;
#105860 = CARTESIAN_POINT('Ctrl Pts',(-18.7386719801883,-12.4373981512211,
122.061779312103)) ;
#105861 = CARTESIAN_POINT('Ctrl Pts',(-18.5144450957222,-12.447397422184,
122.198699572919)) ;
#105862 = CARTESIAN_POINT('Ctrl Pts',(-18.3191930175226,-12.4572918739413,
122.370484946934)) ;
#105863 = CARTESIAN_POINT('Ctrl Pts',(-18.1540884055978,-12.4673551897507,
122.577006721768)) ;
#105864 = CARTESIAN_POINT('Ctrl Pts',(-18.0298693325494,-12.4771940464903,
122.803819660122)) ;
#105865 = CARTESIAN_POINT('Ctrl Pts',(-17.9447542096665,-12.4872601683079,
123.054234502604)) ;
#105866 = CARTESIAN_POINT('Ctrl Pts',(-17.9052530449946,-12.4971433960322,
123.310969073969)) ;
#105867 = CARTESIAN_POINT('Ctrl Pts',(-17.9104144562362,-12.5071328573109,
123.573404577314)) ;
#105868 = CARTESIAN_POINT('Ctrl Pts',(-17.9610348989325,-12.5170965677374,
123.830313519484)) ;
#105869 = CARTESIAN_POINT('Ctrl Pts',(-18.055535313053,-12.5270915704683,
124.075403882281)) ;
#105870 = CARTESIAN_POINT('Ctrl Pts',(-18.1920541401854,-12.5371279014786,
124.301051073442)) ;
#105871 = CARTESIAN_POINT('Ctrl Pts',(-18.3620887052775,-12.5469741308209,
124.496109020729)) ;
#105872 = CARTESIAN_POINT('Ctrl Pts',(-18.5659035124381,-12.5569596290961,
124.661323909438)) ;
#105873 = CARTESIAN_POINT('Ctrl Pts',(-18.794133205315,-12.5668945320791,
124.78820420773)) ;
#105874 = CARTESIAN_POINT('Ctrl Pts',(-19.0439677038418,-12.5769520351743,
124.874329341901)) ;
#105875 = CARTESIAN_POINT('Ctrl Pts',(-19.2988434093258,-12.5867736915449,
124.91519672569)) ;
#105876 = CARTESIAN_POINT('Ctrl Pts',(-19.5630599609083,-12.59682975421,124.911586781273)) ;
#105877 = CARTESIAN_POINT('Ctrl Pts',(-19.8196010841879,-12.6067704189132,
124.862254027796)) ;
#105878 = CARTESIAN_POINT('Ctrl Pts',(-20.0630721998832,-12.6166748228617,
124.770231291142)) ;
#105879 = CARTESIAN_POINT('Ctrl Pts',(-20.2899726794303,-12.6267213078553,
124.63529723127)) ;
#105880 = CARTESIAN_POINT('Ctrl Pts',(-20.4871951419804,-12.636617535667,
124.46572279971)) ;
#105881 = CARTESIAN_POINT('Ctrl Pts',(-20.6546905094441,-12.6466771192305,
124.261238010029)) ;
#105882 = CARTESIAN_POINT('Ctrl Pts',(-20.7815104793504,-12.6565291288993,
124.035511186315)) ;
#105883 = CARTESIAN_POINT('Ctrl Pts',(-20.8689934761397,-12.6664916603389,
123.788768205197)) ;
#105884 = CARTESIAN_POINT('Ctrl Pts',(-20.9122064367509,-12.6765232085783,
123.528706986233)) ;
#105885 = CARTESIAN_POINT('Ctrl Pts',(-20.9098929873906,-12.6864146197913,
123.268781131544)) ;
#105886 = CARTESIAN_POINT('Ctrl Pts',(-20.8623508858351,-12.6964308734993,
123.009883889903)) ;
#105887 = CARTESIAN_POINT('Ctrl Pts',(-20.769920509206,-12.706460976344,122.763045735835)) ;
#105888 = CARTESIAN_POINT('Ctrl Pts',(-20.6387698639911,-12.7163174252977,
122.539667034596)) ;
#105889 = CARTESIAN_POINT('Ctrl Pts',(-20.468686507231,-12.72631643607,122.339431415899)) ;
#105890 = CARTESIAN_POINT('Ctrl Pts',(-20.2686378940791,-12.736211652988,
122.173234495552)) ;
#105891 = CARTESIAN_POINT('Ctrl Pts',(-20.0390498000103,-12.7462721683453,
122.042207516489)) ;
#105892 = CARTESIAN_POINT('Ctrl Pts',(-19.7954221880598,-12.7561214617324,
121.954750952006)) ;
#105893 = CARTESIAN_POINT('Ctrl Pts',(-19.5358430756164,-12.7661486374124,
121.909479848498)) ;
#105894 = CARTESIAN_POINT('Ctrl Pts',(-19.2722925736252,-12.7761772130396,
121.910661435614)) ;
#105895 = CARTESIAN_POINT('Ctrl Pts',(-19.0176320504801,-12.7860223065854,
121.956236242395)) ;
#105896 = CARTESIAN_POINT('Ctrl Pts',(-18.7708959417052,-12.7960135480172,
122.046015059974)) ;
#105897 = CARTESIAN_POINT('Ctrl Pts',(-18.5427539301237,-12.8060493291605,
122.178333355514)) ;
#105898 = CARTESIAN_POINT('Ctrl Pts',(-18.344530793837,-12.8159015348902,
122.344872755127)) ;
#105899 = CARTESIAN_POINT('Ctrl Pts',(-18.1757936891155,-12.8258636290072,
122.545026044335)) ;
#105900 = CARTESIAN_POINT('Ctrl Pts',(-18.0438514585141,-12.8358861898343,
122.772976611802)) ;
#105901 = CARTESIAN_POINT('Ctrl Pts',(-17.9540972344567,-12.8458139614859,
123.017969138429)) ;
#105902 = CARTESIAN_POINT('Ctrl Pts',(-17.9077512439174,-12.8558563456107,
123.27775092553)) ;
#105903 = CARTESIAN_POINT('Ctrl Pts',(-17.9071170334874,-12.8657455696813,
123.537644244839)) ;
#105904 = CARTESIAN_POINT('Ctrl Pts',(-17.951578905651,-12.8757348178486,
123.796349682054)) ;
#105905 = CARTESIAN_POINT('Ctrl Pts',(-18.0402013685863,-12.8856933948906,
124.042581000348)) ;
#105906 = CARTESIAN_POINT('Ctrl Pts',(-18.1689146990719,-12.8955929639819,
124.268677154619)) ;
#105907 = CARTESIAN_POINT('Ctrl Pts',(-18.3374623673469,-12.9056408760659,
124.471898543285)) ;
#105908 = CARTESIAN_POINT('Ctrl Pts',(-18.5355994492501,-12.9155362303731,
124.640372901657)) ;
#105909 = CARTESIAN_POINT('Ctrl Pts',(-18.7636696514608,-12.9255978808643,
124.774091983327)) ;
#105910 = CARTESIAN_POINT('Ctrl Pts',(-19.0061700042819,-12.9354424963268,
124.864243378729)) ;
#105911 = CARTESIAN_POINT('Ctrl Pts',(-19.263440320499,-12.9454025752282,
124.912387637213)) ;
#105912 = CARTESIAN_POINT('Ctrl Pts',(-19.527213442044,-12.9554407695865,
124.914637912278)) ;
#105913 = CARTESIAN_POINT('Ctrl Pts',(-19.7832305957041,-12.9653144849861,
124.872237771651)) ;
#105914 = CARTESIAN_POINT('Ctrl Pts',(-20.0328289090505,-12.9753861945204,
124.784297245069)) ;
#105915 = CARTESIAN_POINT('Ctrl Pts',(-20.2580129538926,-12.9852186349729,
124.65754226709)) ;
#105916 = CARTESIAN_POINT('Ctrl Pts',(-20.4622619532301,-12.9952504558983,
124.49087643455)) ;
#105917 = CARTESIAN_POINT('Ctrl Pts',(-20.6337103450931,-13.0052708257839,
124.291008668358)) ;
#105918 = CARTESIAN_POINT('Ctrl Pts',(-20.7663859266914,-13.0151375969176,
124.068214529218)) ;
#105919 = CARTESIAN_POINT('Ctrl Pts',(-20.860238962856,-13.025208368107,123.82079438421)) ;
#105920 = CARTESIAN_POINT('Ctrl Pts',(-20.9086253549924,-13.0350515286286,
123.566676912894)) ;
#105921 = CARTESIAN_POINT('Ctrl Pts',(-20.913063221591,-13.045031761815,123.304452798709)) ;
#105922 = CARTESIAN_POINT('Ctrl Pts',(-20.871244216678,-13.0550502818502,
123.044526148757)) ;
#105923 = CARTESIAN_POINT('Ctrl Pts',(-20.7866033496793,-13.0649335902339,
122.798947963481)) ;
#105924 = CARTESIAN_POINT('Ctrl Pts',(-20.6581851562813,-13.0750018744047,
122.567668252138)) ;
#105925 = CARTESIAN_POINT('Ctrl Pts',(-20.4956824752415,-13.0848320010723,
122.366800045795)) ;
#105926 = CARTESIAN_POINT('Ctrl Pts',(-20.2963739380565,-13.0948985732789,
122.192919639631)) ;
#105927 = CARTESIAN_POINT('Ctrl Pts',(-20.0737240319191,-13.1047887295196,
122.058778426284)) ;
#105928 = CARTESIAN_POINT('Ctrl Pts',(-19.8289059210494,-13.114781257096,
121.963856125823)) ;
#105929 = CARTESIAN_POINT('Ctrl Pts',(-19.5720652391397,-13.1247427469703,
121.913259794537)) ;
#105930 = CARTESIAN_POINT('Ctrl Pts',(-19.3117143442224,-13.1346519688575,
121.907457127883)) ;
#105931 = CARTESIAN_POINT('Ctrl Pts',(-19.0507318169299,-13.1447005486678,
121.947593231427)) ;
#105932 = CARTESIAN_POINT('Ctrl Pts',(-18.8047453884644,-13.1545835231379,
122.030958261685)) ;
#105933 = CARTESIAN_POINT('Ctrl Pts',(-18.5741383843272,-13.1645784342806,
122.156672491579)) ;
#105934 = CARTESIAN_POINT('Ctrl Pts',(-18.3685451174446,-13.1745988208542,
122.321235274363)) ;
#105935 = CARTESIAN_POINT('Ctrl Pts',(-18.1964735381612,-13.1845089247113,
122.516696286049)) ;
#105936 = CARTESIAN_POINT('Ctrl Pts',(-18.0601155303138,-13.1944366369212,
122.739126636729)) ;
#105937 = CARTESIAN_POINT('Ctrl Pts',(-17.9635520490142,-13.2044797466884,
122.984738187644)) ;
#105938 = CARTESIAN_POINT('Ctrl Pts',(-17.9117515043607,-13.214366167144,
123.23934198587)) ;
#105939 = CARTESIAN_POINT('Ctrl Pts',(-17.9044262701095,-13.2243593447496,
123.501835598151)) ;
#105940 = CARTESIAN_POINT('Ctrl Pts',(-17.9427087756384,-13.2343050076535,
123.760379203083)) ;
#105941 = CARTESIAN_POINT('Ctrl Pts',(-18.0248121016097,-13.2442523038587,
124.008568584514)) ;
#105942 = CARTESIAN_POINT('Ctrl Pts',(-18.1502624018748,-13.2543000694366,
124.240900424645)) ;
#105943 = CARTESIAN_POINT('Ctrl Pts',(-18.3107346122859,-13.2641482826542,
124.443940073215)) ;
#105944 = CARTESIAN_POINT('Ctrl Pts',(-18.505634717484,-13.2741078554483,
124.618624665501)) ;
#105945 = CARTESIAN_POINT('Ctrl Pts',(-18.7298622874998,-13.2841444764808,
124.757486690818)) ;
#105946 = CARTESIAN_POINT('Ctrl Pts',(-18.9708689515076,-13.2940249912912,
124.854174107934)) ;
#105947 = CARTESIAN_POINT('Ctrl Pts',(-19.2293446499912,-13.3040776425982,
124.908560044492)) ;
#105948 = CARTESIAN_POINT('Ctrl Pts',(-19.4892871259414,-13.3139730408782,
124.917212832017)) ;
#105949 = CARTESIAN_POINT('Ctrl Pts',(-19.7507469643642,-13.3240231625843,
124.88015632989)) ;
#105950 = CARTESIAN_POINT('Ctrl Pts',(-19.9977291617165,-13.3339074421262,
124.799637378817)) ;
#105951 = CARTESIAN_POINT('Ctrl Pts',(-20.2297273479885,-13.3439022234181,
124.676550308236)) ;
#105952 = CARTESIAN_POINT('Ctrl Pts',(-20.4358283328775,-13.3538500686049,
124.515703848554)) ;
#105953 = CARTESIAN_POINT('Ctrl Pts',(-20.6109332605582,-13.3637870319923,
124.322011504396)) ;
#105954 = CARTESIAN_POINT('Ctrl Pts',(-20.750697973779,-13.3737699967295,
124.099960077421)) ;
#105955 = CARTESIAN_POINT('Ctrl Pts',(-20.8499157138425,-13.3838138481452,
123.855409348359)) ;
#105956 = CARTESIAN_POINT('Ctrl Pts',(-20.9045890531855,-13.3936420494799,
123.602946647312)) ;
#105957 = CARTESIAN_POINT('Ctrl Pts',(-20.9149711028211,-13.403718622078,
123.338403239339)) ;
#105958 = CARTESIAN_POINT('Ctrl Pts',(-20.8801719456267,-13.4135707020855,
123.081792606934)) ;
#105959 = CARTESIAN_POINT('Ctrl Pts',(-20.7998200890708,-13.4236439870896,
122.829613269708)) ;
#105960 = CARTESIAN_POINT('Ctrl Pts',(-20.6796429969365,-13.4334853388001,
122.600587873272)) ;
#105961 = CARTESIAN_POINT('Ctrl Pts',(-20.5203827330306,-13.4434468381966,
122.392848692112)) ;
#105962 = CARTESIAN_POINT('Ctrl Pts',(-20.3257020959426,-13.4534826143266,
122.214922798792)) ;
#105963 = CARTESIAN_POINT('Ctrl Pts',(-20.106509157136,-13.4633710409642,
122.075355463823)) ;
#105964 = CARTESIAN_POINT('Ctrl Pts',(-19.8635102674347,-13.4733863630391,
121.974225744482)) ;
#105965 = CARTESIAN_POINT('Ctrl Pts',(-19.6061332113171,-13.4834167119393,
121.917339791102)) ;
#105966 = CARTESIAN_POINT('Ctrl Pts',(-19.34772624537,-13.493260087546,121.905698547325)) ;
#105967 = CARTESIAN_POINT('Ctrl Pts',(-19.0862905181186,-13.5032895244431,
121.939151509404)) ;
#105968 = CARTESIAN_POINT('Ctrl Pts',(-18.834783896269,-13.513321402376,122.018199528681)) ;
#105969 = CARTESIAN_POINT('Ctrl Pts',(-18.6053189853568,-13.5231510254815,
122.136788620459)) ;
#105970 = CARTESIAN_POINT('Ctrl Pts',(-18.3960964023697,-13.5331404966346,
122.295352843074)) ;
#105971 = CARTESIAN_POINT('Ctrl Pts',(-18.2171108841806,-13.543184345397,
122.489332377545)) ;
#105972 = CARTESIAN_POINT('Ctrl Pts',(-18.0772280467266,-13.5530060509287,
122.706244029415)) ;
#105973 = CARTESIAN_POINT('Ctrl Pts',(-17.974363913469,-13.5630410907565,
122.949063789534)) ;
#105974 = CARTESIAN_POINT('Ctrl Pts',(-17.9159925554736,-13.573065797648,
123.205963898225)) ;
#105975 = CARTESIAN_POINT('Ctrl Pts',(-17.9027881139224,-13.5829185019887,
123.464545531986)) ;
#105976 = CARTESIAN_POINT('Ctrl Pts',(-17.934663913364,-13.5929066241964,
123.725061221392)) ;
#105977 = CARTESIAN_POINT('Ctrl Pts',(-18.0108264809125,-13.6028350943037,
123.974614154487)) ;
#105978 = CARTESIAN_POINT('Ctrl Pts',(-18.1294981550369,-13.6128240714709,
124.208771928652)) ;
#105979 = CARTESIAN_POINT('Ctrl Pts',(-18.2881434789744,-13.6228618787506,
124.419507237109)) ;
#105980 = CARTESIAN_POINT('Ctrl Pts',(-18.4770091475431,-13.6327081796139,
124.596377248716)) ;
#105981 = CARTESIAN_POINT('Ctrl Pts',(-18.6973442789797,-13.6427339229932,
124.740836596543)) ;
#105982 = CARTESIAN_POINT('Ctrl Pts',(-18.9398133035653,-13.6527647894322,
124.844267400033)) ;
#105983 = CARTESIAN_POINT('Ctrl Pts',(-19.1914704015603,-13.662602148231,
124.903374596811)) ;
#105984 = CARTESIAN_POINT('Ctrl Pts',(-19.4535935830303,-13.6725941091647,
124.918819329345)) ;
#105985 = CARTESIAN_POINT('Ctrl Pts',(-19.7154208059744,-13.6826264717213,
124.887866426181)) ;
#105986 = CARTESIAN_POINT('Ctrl Pts',(-19.9637570360245,-13.6924916322957,
124.813493884598)) ;
#105987 = CARTESIAN_POINT('Ctrl Pts',(-20.1980303243043,-13.7024535368734,
124.69664719285)) ;
#105988 = CARTESIAN_POINT('Ctrl Pts',(-20.4097244466647,-13.7124884669491,
124.539422352633)) ;
#105989 = CARTESIAN_POINT('Ctrl Pts',(-20.5885492429424,-13.7223734138028,
124.350956304226)) ;
#105990 = CARTESIAN_POINT('Ctrl Pts',(-20.7344600840413,-13.7324390901142,
124.130377299098)) ;
#105991 = CARTESIAN_POINT('Ctrl Pts',(-20.837759491418,-13.7422780097491,
123.893305056922)) ;
#105992 = CARTESIAN_POINT('Ctrl Pts',(-20.9000224691976,-13.7523415194835,
123.636319401091)) ;
#105993 = CARTESIAN_POINT('Ctrl Pts',(-20.9162263459812,-13.7622351326453,
123.376800328538)) ;
#105994 = CARTESIAN_POINT('Ctrl Pts',(-20.8876702021662,-13.7721791394587,
123.117082703603)) ;
#105995 = CARTESIAN_POINT('Ctrl Pts',(-20.8141299534446,-13.782180093813,
122.864725111302)) ;
#105996 = CARTESIAN_POINT('Ctrl Pts',(-20.697056137545,-13.7922188515053,
122.628344090505)) ;
#105997 = CARTESIAN_POINT('Ctrl Pts',(-20.5444882130351,-13.8020430356753,
122.420051830506)) ;
#105998 = CARTESIAN_POINT('Ctrl Pts',(-20.3539349773995,-13.8121011012747,
122.236913035828)) ;
#105999 = CARTESIAN_POINT('Ctrl Pts',(-20.1370466125606,-13.8220311480494,
122.091780837515)) ;
#106000 = CARTESIAN_POINT('Ctrl Pts',(-19.8980293610127,-13.8319825903865,
121.9856600342)) ;
#106001 = CARTESIAN_POINT('Ctrl Pts',(-19.6417039464166,-13.8420293875658,
121.922400808479)) ;
#106002 = CARTESIAN_POINT('Ctrl Pts',(-19.3835149611134,-13.8518773282459,
121.904719817845)) ;
#106003 = CARTESIAN_POINT('Ctrl Pts',(-19.1231332375772,-13.8618389595885,
121.931644427789)) ;
#106004 = CARTESIAN_POINT('Ctrl Pts',(-18.8697526821085,-13.8718676189644,
122.004180140349)) ;
#106005 = CARTESIAN_POINT('Ctrl Pts',(-18.6355992228795,-13.8817779218526,
122.118159162644)) ;
#106006 = CARTESIAN_POINT('Ctrl Pts',(-18.4238530398286,-13.8917128164148,
122.270900422556)) ;
#106007 = CARTESIAN_POINT('Ctrl Pts',(-18.2400856096355,-13.9017539150817,
122.460247612701)) ;
#106008 = CARTESIAN_POINT('Ctrl Pts',(-18.0940931471758,-13.9116411975861,
122.675199141709)) ;
#106009 = CARTESIAN_POINT('Ctrl Pts',(-17.9861233201671,-13.9216329380966,
122.914527586321)) ;
#106010 = CARTESIAN_POINT('Ctrl Pts',(-17.9216953674469,-13.931583487332,
123.167969398232)) ;
#106011 = CARTESIAN_POINT('Ctrl Pts',(-17.9018949026966,-13.9415191649668,
123.42830067272)) ;
#106012 = CARTESIAN_POINT('Ctrl Pts',(-17.9274500776535,-13.9515045827596,
123.689479910381)) ;
#106013 = CARTESIAN_POINT('Ctrl Pts',(-17.9985820584167,-13.9615333756301,
123.943243286239)) ;
#106014 = CARTESIAN_POINT('Ctrl Pts',(-18.1107467629068,-13.9714128868581,
124.17738299688)) ;
#106015 = CARTESIAN_POINT('Ctrl Pts',(-18.2631231043819,-13.981406423531,
124.391289132976)) ;
#106016 = CARTESIAN_POINT('Ctrl Pts',(-18.4514209232036,-13.9914386917948,
124.575796061507)) ;
#106017 = CARTESIAN_POINT('Ctrl Pts',(-18.6649638633447,-14.0013026538007,
124.722784990796)) ;
#106018 = CARTESIAN_POINT('Ctrl Pts',(-18.9056437592007,-14.0113727151456,
124.832730221074)) ;
#106019 = CARTESIAN_POINT('Ctrl Pts',(-19.1560068384201,-14.0212150794943,
124.897711370076)) ;
#106020 = CARTESIAN_POINT('Ctrl Pts',(-19.4168544379476,-14.0311757519968,
124.919442596206)) ;
#106021 = CARTESIAN_POINT('Ctrl Pts',(-19.6794838048793,-14.0412138230646,
124.894842525918)) ;
#106022 = CARTESIAN_POINT('Ctrl Pts',(-19.9298640848764,-14.051087438025,
124.826625554233)) ;
#106023 = CARTESIAN_POINT('Ctrl Pts',(-20.1692084064,-14.0611596726063,124.713720144365)) ;
#106024 = CARTESIAN_POINT('Ctrl Pts',(-20.3802392463019,-14.0709836910551,
124.564918211062)) ;
#106025 = CARTESIAN_POINT('Ctrl Pts',(-20.5668561717494,-14.0810486120311,
124.377563316902)) ;
#106026 = CARTESIAN_POINT('Ctrl Pts',(-20.7654766766846,-14.0942589103259,
124.0927478502)) ;
#106027 = CARTESIAN_POINT('Ctrl Pts',(-20.8864738113405,-14.1075743570578,
123.760309528833)) ;
#106028 = CARTESIAN_POINT('Ctrl Pts',(-20.9168468780944,-14.1208646023251,
123.412265267831)) ;
#106029 = CARTESIAN_POINT('Ctrl Pts',(-20.8936192942763,-14.1309153519322,
123.149220731085)) ;
#106030 = CARTESIAN_POINT('Ctrl Pts',(-20.8271655478931,-14.1407279589144,
122.900025043608)) ;
#106031 = CARTESIAN_POINT('Ctrl Pts',(-20.7159396250951,-14.1507990569087,
122.659911955936)) ;
#106032 = CARTESIAN_POINT('Ctrl Pts',(-20.56718818496,-14.1606886296836,122.446781682834)) ;
#106033 = CARTESIAN_POINT('Ctrl Pts',(-20.3217392336305,-14.1739587364869,
122.199053239677)) ;
#106034 = CARTESIAN_POINT('Ctrl Pts',(-19.9402855601747,-14.1905754234094,
121.976506432685)) ;
#106035 = CARTESIAN_POINT('Ctrl Pts',(-19.5069617032543,-14.2071494667256,
121.897358315389)) ;
#106036 = CARTESIAN_POINT('Ctrl Pts',(-19.1586307174601,-14.2204460341574,
121.925257438203)) ;
#106037 = CARTESIAN_POINT('Ctrl Pts',(-18.9035554294054,-14.2304760977348,
121.991681270408)) ;
#106038 = CARTESIAN_POINT('Ctrl Pts',(-18.6671524907511,-14.240369989584,
122.099857115475)) ;
#106039 = CARTESIAN_POINT('Ctrl Pts',(-18.379673843965,-14.2536227453696,
122.296566106968)) ;
#106040 = CARTESIAN_POINT('Ctrl Pts',(-18.0908336692114,-14.270350850362,
122.63447857022)) ;
#106041 = CARTESIAN_POINT('Ctrl Pts',(-17.9056126156248,-14.2901816868405,
123.128030955025)) ;
#106042 = CARTESIAN_POINT('Ctrl Pts',(-17.8986114852488,-14.3101070787307,
123.657451709172)) ;
#106043 = CARTESIAN_POINT('Ctrl Pts',(-18.0728191190956,-14.3300322920827,
124.157646493931)) ;
#106044 = CARTESIAN_POINT('Ctrl Pts',(-18.4070617662362,-14.3499573055678,
124.56833572685)) ;
#106045 = CARTESIAN_POINT('Ctrl Pts',(-18.8599856109715,-14.3698337772678,
124.840324566468)) ;
#106046 = CARTESIAN_POINT('Ctrl Pts',(-19.3811370011753,-14.3898130951767,
124.942174609197)) ;
#106047 = CARTESIAN_POINT('Ctrl Pts',(-19.9045318981702,-14.4097460987527,
124.859860883971)) ;
#106048 = CARTESIAN_POINT('Ctrl Pts',(-20.3677488802651,-14.4296413687804,
124.604895458802)) ;
#106049 = CARTESIAN_POINT('Ctrl Pts',(-20.7170554974423,-14.4495627066862,
124.206961263789)) ;
#106050 = CARTESIAN_POINT('Ctrl Pts',(-20.9098459944052,-14.4695203299524,
123.712767673844)) ;
#106051 = CARTESIAN_POINT('Ctrl Pts',(-20.922491622849,-14.4894001619096,
123.184628566672)) ;
#106052 = CARTESIAN_POINT('Ctrl Pts',(-20.755460182351,-14.5092820132065,
122.683188642338)) ;
#106053 = CARTESIAN_POINT('Ctrl Pts',(-20.423531062275,-14.5293530303103,
122.265665610548)) ;
#106054 = CARTESIAN_POINT('Ctrl Pts',(-19.974929403366,-14.5491602540634,
121.989985430984)) ;
#106055 = CARTESIAN_POINT('Ctrl Pts',(-19.4550455765242,-14.5691413896322,
121.881815479055)) ;
#106056 = CARTESIAN_POINT('Ctrl Pts',(-18.9310151634136,-14.5890688829714,
121.958367056807)) ;
#106057 = CARTESIAN_POINT('Ctrl Pts',(-18.4660434814142,-14.6088895443292,
122.206302838715)) ;
#106058 = CARTESIAN_POINT('Ctrl Pts',(-18.1095293436928,-14.628986733551,
122.603802596907)) ;
#106059 = CARTESIAN_POINT('Ctrl Pts',(-17.9128741620564,-14.6487504125593,
123.091161865379)) ;
#106060 = CARTESIAN_POINT('Ctrl Pts',(-17.8934588628578,-14.6688076912324,
123.623664539736)) ;
#106061 = CARTESIAN_POINT('Ctrl Pts',(-18.0551924437206,-14.6886031149798,
124.124467473723)) ;
#106062 = CARTESIAN_POINT('Ctrl Pts',(-18.3794344442589,-14.7085667597074,
124.544396149328)) ;
#106063 = CARTESIAN_POINT('Ctrl Pts',(-18.8287062890011,-14.7285502509815,
124.827696849197)) ;
#106064 = CARTESIAN_POINT('Ctrl Pts',(-19.3429243244761,-14.7483577461308,
124.940748089482)) ;
#106065 = CARTESIAN_POINT('Ctrl Pts',(-19.8693900875644,-14.7683403368509,
124.871549887896)) ;
#106066 = CARTESIAN_POINT('Ctrl Pts',(-20.338450413313,-14.7882229908422,
124.627888050851)) ;
#106067 = CARTESIAN_POINT('Ctrl Pts',(-20.6977033226581,-14.8081812357052,
124.237747977146)) ;
#106068 = CARTESIAN_POINT('Ctrl Pts',(-20.9017825247716,-14.8280568227468,
123.750413738946)) ;
#106069 = CARTESIAN_POINT('Ctrl Pts',(-20.9278144322441,-14.8480377108821,
123.220027941428)) ;
#106070 = CARTESIAN_POINT('Ctrl Pts',(-20.7712200432278,-14.8679728519931,
122.71377974773)) ;
#106071 = CARTESIAN_POINT('Ctrl Pts',(-20.4520163194474,-14.8878848700041,
122.291712583774)) ;
#106072 = CARTESIAN_POINT('Ctrl Pts',(-20.0087342255776,-14.9077730882477,
122.003738662211)) ;
#106073 = CARTESIAN_POINT('Ctrl Pts',(-19.5791146983023,-14.9243713920946,
121.903719525723)) ;
#106074 = CARTESIAN_POINT('Ctrl Pts',(-19.2304737179914,-14.9376439819974,
121.914992836126)) ;
#106075 = CARTESIAN_POINT('Ctrl Pts',(-18.9730417117785,-14.9476513969483,
121.968739479905)) ;
#106076 = CARTESIAN_POINT('Ctrl Pts',(-18.7289294126291,-14.9576587436809,
122.066586725819)) ;
#106077 = CARTESIAN_POINT('Ctrl Pts',(-18.4326429910154,-14.9709251034825,
122.250333383344)) ;
#106078 = CARTESIAN_POINT('Ctrl Pts',(-18.1316429666294,-14.9874397611055,
122.569709091786)) ;
#106079 = CARTESIAN_POINT('Ctrl Pts',(-17.9558737385504,-15.0040371943481,
122.974282100994)) ;
#106080 = CARTESIAN_POINT('Ctrl Pts',(-17.904543027528,-15.0173851914931,
123.321319034395)) ;
#106081 = CARTESIAN_POINT('Ctrl Pts',(-17.9113794336415,-15.0272809458447,
123.581279394884)) ;
#106082 = CARTESIAN_POINT('Ctrl Pts',(-17.9634145199472,-15.0372688997761,
123.838522822041)) ;
#106083 = CARTESIAN_POINT('Ctrl Pts',(-18.0589406118144,-15.0472261234808,
124.082161343153)) ;
#106084 = CARTESIAN_POINT('Ctrl Pts',(-18.1964717964565,-15.0572616700375,
124.307162841967)) ;
#106085 = CARTESIAN_POINT('Ctrl Pts',(-18.3682756912085,-15.0671487813136,
124.502099452208)) ;
#106086 = CARTESIAN_POINT('Ctrl Pts',(-18.5731742379269,-15.0771401864144,
124.666262805335)) ;
#106087 = CARTESIAN_POINT('Ctrl Pts',(-18.8024583865383,-15.0870858076292,
124.791713131631)) ;
#106088 = CARTESIAN_POINT('Ctrl Pts',(-19.0499764287922,-15.0970350558975,
124.875984692672)) ;
#106089 = CARTESIAN_POINT('Ctrl Pts',(-19.3109131330844,-15.1070815510661,
124.916080673972)) ;
#106090 = CARTESIAN_POINT('Ctrl Pts',(-19.5697514855712,-15.1169328938577,
124.910630529631)) ;
#106091 = CARTESIAN_POINT('Ctrl Pts',(-19.8269017656823,-15.126904673985,
124.860363871182)) ;
#106092 = CARTESIAN_POINT('Ctrl Pts',(-20.0720498237182,-15.1368998739627,
124.765937816148)) ;
#106093 = CARTESIAN_POINT('Ctrl Pts',(-20.2977304710566,-15.1469338656587,
124.62961150485)) ;
#106094 = CARTESIAN_POINT('Ctrl Pts',(-20.4930841782723,-15.1567892706313,
124.459536040626)) ;
#106095 = CARTESIAN_POINT('Ctrl Pts',(-20.6585517530445,-15.166788568477,
124.255463871845)) ;
#106096 = CARTESIAN_POINT('Ctrl Pts',(-20.7850316142127,-15.1766836810822,
124.028212839193)) ;
#106097 = CARTESIAN_POINT('Ctrl Pts',(-20.8715023711015,-15.1867443266172,
123.778406430621)) ;
#106098 = CARTESIAN_POINT('Ctrl Pts',(-20.9125613873073,-15.1965932036064,
123.522845334443)) ;
#106099 = CARTESIAN_POINT('Ctrl Pts',(-20.9092158790002,-15.2066219147,123.259326277466)) ;
#106100 = CARTESIAN_POINT('Ctrl Pts',(-20.8594566128838,-15.2166513159561,
123.000498815782)) ;
#106101 = CARTESIAN_POINT('Ctrl Pts',(-20.7678229214068,-15.2264915077521,
122.758684061677)) ;
#106102 = CARTESIAN_POINT('Ctrl Pts',(-20.6338348815506,-15.2364949369451,
122.532544532535)) ;
#106103 = CARTESIAN_POINT('Ctrl Pts',(-20.4628129096101,-15.2464804494113,
122.33346329065)) ;
#106104 = CARTESIAN_POINT('Ctrl Pts',(-20.2585778330809,-15.2565215457953,
122.166426384082)) ;
#106105 = CARTESIAN_POINT('Ctrl Pts',(-20.0331117499585,-15.2663647417463,
122.039593657452)) ;
#106106 = CARTESIAN_POINT('Ctrl Pts',(-19.7857377349932,-15.2763510528007,
121.952117481947)) ;
#106107 = CARTESIAN_POINT('Ctrl Pts',(-19.5282066790328,-15.2862857380584,
121.908956316518)) ;
#106108 = CARTESIAN_POINT('Ctrl Pts',(-19.2639544547073,-15.2963432992754,
121.911425908328)) ;
#106109 = CARTESIAN_POINT('Ctrl Pts',(-19.0101023053987,-15.306164940884,
121.958231357651)) ;
#106110 = CARTESIAN_POINT('Ctrl Pts',(-18.7623358060744,-15.316221004475,
122.050074589458)) ;
#106111 = CARTESIAN_POINT('Ctrl Pts',(-18.5371068804422,-15.3261616802368,
122.18243432679)) ;
#106112 = CARTESIAN_POINT('Ctrl Pts',(-18.3384838834569,-15.3360660390251,
122.350644943413)) ;
#106113 = CARTESIAN_POINT('Ctrl Pts',(-18.1698386204844,-15.3461126936009,
122.553750325067)) ;
#106114 = CARTESIAN_POINT('Ctrl Pts',(-18.0407575415116,-15.3560082882438,
122.779542857678)) ;
#106115 = CARTESIAN_POINT('Ctrl Pts',(-17.951363279996,-15.3660702349007,
123.028358749357)) ;
#106116 = CARTESIAN_POINT('Ctrl Pts',(-17.9074208492035,-15.3759198588328,
123.283453459673)) ;
#106117 = CARTESIAN_POINT('Ctrl Pts',(-17.907585086851,-15.3858830978627,
123.54526162962)) ;
#106118 = CARTESIAN_POINT('Ctrl Pts',(-17.9538494830513,-15.3959076726385,
123.804618186356)) ;
#106119 = CARTESIAN_POINT('Ctrl Pts',(-18.0433208232661,-15.4058262353262,
124.049423298802)) ;
#106120 = CARTESIAN_POINT('Ctrl Pts',(-18.174519926167,-15.4158184220502,
124.276899412306)) ;
#106121 = CARTESIAN_POINT('Ctrl Pts',(-18.3442899942266,-15.4258532206344,
124.478672382218)) ;
#106122 = CARTESIAN_POINT('Ctrl Pts',(-18.5426343556928,-15.4357084113081,
124.645234433512)) ;
#106123 = CARTESIAN_POINT('Ctrl Pts',(-18.7699348084434,-15.4457077594611,
124.776994967355)) ;
#106124 = CARTESIAN_POINT('Ctrl Pts',(-19.0140737912038,-15.4556028851362,
124.866639752962)) ;
#106125 = CARTESIAN_POINT('Ctrl Pts',(-19.2742769091682,-15.4656634280843,
124.913258287484)) ;
#106126 = CARTESIAN_POINT('Ctrl Pts',(-19.5331248026427,-15.4755127023512,
124.914120014404)) ;
#106127 = CARTESIAN_POINT('Ctrl Pts',(-19.79288378634,-15.4855399269211,124.869889067141)) ;
#106128 = CARTESIAN_POINT('Ctrl Pts',(-20.0408339347153,-15.4955683261089,
124.780561213655)) ;
#106129 = CARTESIAN_POINT('Ctrl Pts',(-20.265554252512,-15.5054140765224,
124.652356312208)) ;
#106130 = CARTESIAN_POINT('Ctrl Pts',(-20.4679841696938,-15.5154028669231,
124.485226414823)) ;
#106131 = CARTESIAN_POINT('Ctrl Pts',(-20.6387526733419,-15.5254477953228,
124.283949581756)) ;
#106132 = CARTESIAN_POINT('Ctrl Pts',(-20.769587922937,-15.5352722801118,
124.061360477081)) ;
#106133 = CARTESIAN_POINT('Ctrl Pts',(-20.8622706680033,-15.545329677653,
123.813869585061)) ;
#106134 = CARTESIAN_POINT('Ctrl Pts',(-20.9096129923147,-15.5552557692392,
123.557334968006)) ;
#106135 = CARTESIAN_POINT('Ctrl Pts',(-20.9123764589189,-15.5652105543838,
123.295750825225)) ;
#106136 = CARTESIAN_POINT('Ctrl Pts',(-20.8690342234856,-15.5752479240414,
123.035565948603)) ;
#106137 = CARTESIAN_POINT('Ctrl Pts',(-20.7826602440331,-15.585136734163,
122.790464902437)) ;
#106138 = CARTESIAN_POINT('Ctrl Pts',(-20.6541601211365,-15.5951260932141,
122.561562829618)) ;
#106139 = CARTESIAN_POINT('Ctrl Pts',(-20.4882301659971,-15.6050846406702,
122.35920139353)) ;
#106140 = CARTESIAN_POINT('Ctrl Pts',(-20.2912598494344,-15.6149842172212,
122.189232159666)) ;
#106141 = CARTESIAN_POINT('Ctrl Pts',(-20.064410532344,-15.6250321290519,
122.054152289427)) ;
#106142 = CARTESIAN_POINT('Ctrl Pts',(-19.8213096590749,-15.6349274769125,
121.961719281926)) ;
#106143 = CARTESIAN_POINT('Ctrl Pts',(-19.5616355544387,-15.6449891534437,
121.912056861961)) ;
#106144 = CARTESIAN_POINT('Ctrl Pts',(-19.3029494038399,-15.6548336711928,
121.908276718303)) ;
#106145 = CARTESIAN_POINT('Ctrl Pts',(-19.0443982485231,-15.6647941149076,
121.949033267111)) ;
#106146 = CARTESIAN_POINT('Ctrl Pts',(-18.7951121911755,-15.6748309477258,
122.035180093776)) ;
#106147 = CARTESIAN_POINT('Ctrl Pts',(-18.5679663971267,-15.6847097444726,
122.160928349971)) ;
#106148 = CARTESIAN_POINT('Ctrl Pts',(-18.3624049359324,-15.694769060601,
122.327091148207)) ;
#106149 = CARTESIAN_POINT('Ctrl Pts',(-18.1920448569954,-15.7046395073542,
122.522708702974)) ;
#106150 = CARTESIAN_POINT('Ctrl Pts',(-18.0559811065904,-15.7146321456122,
122.747306071798)) ;
#106151 = CARTESIAN_POINT('Ctrl Pts',(-17.9611408622094,-15.7246641611601,
122.993277215718)) ;
#106152 = CARTESIAN_POINT('Ctrl Pts',(-17.9107294356664,-15.7345300174667,
123.24762027853)) ;
#106153 = CARTESIAN_POINT('Ctrl Pts',(-17.9051095124023,-15.7445993069358,
123.51214125627)) ;
#106154 = CARTESIAN_POINT('Ctrl Pts',(-17.9445756716794,-15.7544428644871,
123.767807266494)) ;
#106155 = CARTESIAN_POINT('Ctrl Pts',(-18.0281685488562,-15.764422991275,
124.0163870536)) ;
#106156 = CARTESIAN_POINT('Ctrl Pts',(-18.1545808942031,-15.7744415398749,
124.247322075514)) ;
#106157 = CARTESIAN_POINT('Ctrl Pts',(-18.3165419591898,-15.7843248403981,
124.450401497455)) ;
#106158 = CARTESIAN_POINT('Ctrl Pts',(-18.5149688305721,-15.7943931274462,
124.625353826907)) ;
#106159 = CARTESIAN_POINT('Ctrl Pts',(-18.7353342852211,-15.8042232504649,
124.76023996317)) ;
#106160 = CARTESIAN_POINT('Ctrl Pts',(-18.9813486671262,-15.8142898343902,
124.857374264135)) ;
#106161 = CARTESIAN_POINT('Ctrl Pts',(-19.2360561428616,-15.8241799474047,
124.909251656804)) ;
#106162 = CARTESIAN_POINT('Ctrl Pts',(-19.4985245159601,-15.8341726361673,
124.916741048985)) ;
#106163 = CARTESIAN_POINT('Ctrl Pts',(-19.7574871436884,-15.8441335245231,
124.878478534596)) ;
#106164 = CARTESIAN_POINT('Ctrl Pts',(-20.004915765595,-15.8540514694031,
124.796623445015)) ;
#106165 = CARTESIAN_POINT('Ctrl Pts',(-20.2366326706973,-15.8640592224993,
124.672179876595)) ;
#106166 = CARTESIAN_POINT('Ctrl Pts',(-20.4433415773837,-15.8740903164583,
124.508618623269)) ;
#106167 = CARTESIAN_POINT('Ctrl Pts',(-20.6157693686603,-15.8839382844863,
124.31560845638)) ;
#106168 = CARTESIAN_POINT('Ctrl Pts',(-20.7552008635607,-15.8940002406122,
124.090965026465)) ;
#106169 = CARTESIAN_POINT('Ctrl Pts',(-20.8516852314679,-15.9038974522133,
123.849423164374)) ;
#106170 = CARTESIAN_POINT('Ctrl Pts',(-20.905785380101,-15.9138286188779,
123.59411597792)) ;
#106171 = CARTESIAN_POINT('Ctrl Pts',(-20.9145476357222,-15.9238708030821,
123.330367383369)) ;
#106172 = CARTESIAN_POINT('Ctrl Pts',(-20.8781404899739,-15.9337574713353,
123.073106868608)) ;
#106173 = CARTESIAN_POINT('Ctrl Pts',(-20.7971769554529,-15.9437505833135,
122.823304869138)) ;
#106174 = CARTESIAN_POINT('Ctrl Pts',(-20.6745604614457,-15.9536962609293,
122.592489803753)) ;
#106175 = CARTESIAN_POINT('Ctrl Pts',(-20.5141161128324,-15.9636435639143,
122.386100293049)) ;
#106176 = CARTESIAN_POINT('Ctrl Pts',(-20.3181349029705,-15.9736912876611,
122.20916311758)) ;
#106177 = CARTESIAN_POINT('Ctrl Pts',(-20.0989517012309,-15.9835396614236,
122.071551117016)) ;
#106178 = CARTESIAN_POINT('Ctrl Pts',(-19.8568380440018,-15.9934986338693,
121.97218342843)) ;
#106179 = CARTESIAN_POINT('Ctrl Pts',(-19.5990047972081,-16.0035374957505,
121.916385466121)) ;
#106180 = CARTESIAN_POINT('Ctrl Pts',(-19.3395875748729,-16.0134160999223,
121.905950820223)) ;
#106181 = CARTESIAN_POINT('Ctrl Pts',(-19.0778432793215,-16.0234676411256,
121.941206263373)) ;
#106182 = CARTESIAN_POINT('Ctrl Pts',(-18.8300030362905,-16.0333630391059,
122.020074331794)) ;
#106183 = CARTESIAN_POINT('Ctrl Pts',(-18.5959998150771,-16.0434142716512,
122.142513812537)) ;
#106184 = CARTESIAN_POINT('Ctrl Pts',(-18.3901773440873,-16.0533004622755,
122.301092280295)) ;
#106185 = CARTESIAN_POINT('Ctrl Pts',(-18.2128102595661,-16.0632930015913,
122.494699854183)) ;
#106186 = CARTESIAN_POINT('Ctrl Pts',(-18.0724264392633,-16.073241447486,
122.715265898288)) ;
#106187 = CARTESIAN_POINT('Ctrl Pts',(-17.9722610725586,-16.0831782500179,
122.956395392167)) ;
#106188 = CARTESIAN_POINT('Ctrl Pts',(-17.9148856828891,-16.0931612574692,
123.212421827305)) ;
#106189 = CARTESIAN_POINT('Ctrl Pts',(-17.9032506732785,-16.103205098884,
123.476076424428)) ;
#106190 = CARTESIAN_POINT('Ctrl Pts',(-17.9362383494643,-16.1130332975079,
123.732276332531)) ;
#106191 = CARTESIAN_POINT('Ctrl Pts',(-18.0150068697524,-16.1231098909501,
123.985034482931)) ;
#106192 = CARTESIAN_POINT('Ctrl Pts',(-18.1336923054321,-16.1329618902917,
124.215193158101)) ;
#106193 = CARTESIAN_POINT('Ctrl Pts',(-18.293828954018,-16.1430354771156,
124.425930990448)) ;
#106194 = CARTESIAN_POINT('Ctrl Pts',(-18.4837073307471,-16.152875702213,
124.601509441711)) ;
#106195 = CARTESIAN_POINT('Ctrl Pts',(-18.703422599687,-16.1628414062417,
124.743985806514)) ;
#106196 = CARTESIAN_POINT('Ctrl Pts',(-18.94619596473,-16.1728680395483,124.846435307099)) ;
#106197 = CARTESIAN_POINT('Ctrl Pts',(-19.2001320498308,-16.1827823352601,
124.904684366609)) ;
#106198 = CARTESIAN_POINT('Ctrl Pts',(-19.4622641622427,-16.1927706239526,
124.918531528286)) ;
#106199 = CARTESIAN_POINT('Ctrl Pts',(-19.7240529144461,-16.2028093571109,
124.886019110933)) ;
#106200 = CARTESIAN_POINT('Ctrl Pts',(-19.971447916316,-16.2126526889385,
124.810469269486)) ;
#106201 = CARTESIAN_POINT('Ctrl Pts',(-20.2065617889263,-16.2226804148181,
124.691454476011)) ;
#106202 = CARTESIAN_POINT('Ctrl Pts',(-20.4171114197521,-16.2327127512066,
124.532774031864)) ;
#106203 = CARTESIAN_POINT('Ctrl Pts',(-20.5936406689353,-16.2425422515072,
124.344218105052)) ;
#106204 = CARTESIAN_POINT('Ctrl Pts',(-20.7377182461283,-16.252531755424,
124.124767080073)) ;
#106205 = CARTESIAN_POINT('Ctrl Pts',(-20.8414473437141,-16.2625755959364,
123.882065493061)) ;
#106206 = CARTESIAN_POINT('Ctrl Pts',(-20.900653673808,-16.2723973017045,
123.630843512612)) ;
#106207 = CARTESIAN_POINT('Ctrl Pts',(-20.9163042732894,-16.2824323488368,
123.36759911716)) ;
#106208 = CARTESIAN_POINT('Ctrl Pts',(-20.8853162273939,-16.2924570262737,
123.105980618669)) ;
#106209 = CARTESIAN_POINT('Ctrl Pts',(-20.8112016290082,-16.3023098411282,
122.857893201183)) ;
#106210 = CARTESIAN_POINT('Ctrl Pts',(-20.6939684927004,-16.3122975507357,
122.623085044289)) ;
#106211 = CARTESIAN_POINT('Ctrl Pts',(-20.5386409517621,-16.3222275607298,
122.413386814365)) ;
#106212 = CARTESIAN_POINT('Ctrl Pts',(-20.3484048238338,-16.332217315949,
122.232473149134)) ;
#106213 = CARTESIAN_POINT('Ctrl Pts',(-20.1286513400148,-16.3422439246319,
122.087087277406)) ;
#106214 = CARTESIAN_POINT('Ctrl Pts',(-19.8905383570704,-16.3521278646537,
121.983335342418)) ;
#106215 = CARTESIAN_POINT('Ctrl Pts',(-19.6354682256549,-16.3621170921922,
121.921258549847)) ;
#106216 = CARTESIAN_POINT('Ctrl Pts',(-19.3720634366755,-16.3721599627159,
121.904869502532)) ;
#106217 = CARTESIAN_POINT('Ctrl Pts',(-19.115265317879,-16.3819923494713,
121.933435787349)) ;
#106218 = CARTESIAN_POINT('Ctrl Pts',(-18.8630593043573,-16.3919856426429,
122.006615981384)) ;
#106219 = CARTESIAN_POINT('Ctrl Pts',(-18.6267060253685,-16.4020176482913,
122.123427107478)) ;
#106220 = CARTESIAN_POINT('Ctrl Pts',(-18.4175878783122,-16.4118829042603,
122.276634889428)) ;
#106221 = CARTESIAN_POINT('Ctrl Pts',(-18.235941989852,-16.4218447841678,
122.465159983501)) ;
#106222 = CARTESIAN_POINT('Ctrl Pts',(-18.0890877174542,-16.4318797175297,
122.684175710584)) ;
#106223 = CARTESIAN_POINT('Ctrl Pts',(-17.9836645209362,-16.441764675909,
122.92162846115)) ;
#106224 = CARTESIAN_POINT('Ctrl Pts',(-17.9200049383359,-16.4518303028317,
123.178322908577)) ;
#106225 = CARTESIAN_POINT('Ctrl Pts',(-17.9020225616626,-16.461669408496,
123.436301022822)) ;
#106226 = CARTESIAN_POINT('Ctrl Pts',(-17.9293636219284,-16.4717322235013,
123.699287948739)) ;
#106227 = CARTESIAN_POINT('Ctrl Pts',(-18.0009973197692,-16.48162842955,123.949318087485)) ;
#106228 = CARTESIAN_POINT('Ctrl Pts',(-18.1147911167,-16.4915692525753,124.184432400747)) ;
#106229 = CARTESIAN_POINT('Ctrl Pts',(-18.2686434852337,-16.501573835554,
124.397661532984)) ;
#106230 = CARTESIAN_POINT('Ctrl Pts',(-18.4576877170773,-16.5115947299987,
124.580981693684)) ;
#106231 = CARTESIAN_POINT('Ctrl Pts',(-18.6727140788603,-16.5214866505881,
124.727067000492)) ;
#106232 = CARTESIAN_POINT('Ctrl Pts',(-18.9121040759921,-16.5314800829335,
124.835026163748)) ;
#106233 = CARTESIAN_POINT('Ctrl Pts',(-19.1654138675533,-16.5414256878334,
124.899390294724)) ;
#106234 = CARTESIAN_POINT('Ctrl Pts',(-19.4260705655085,-16.5513729613149,
124.91932812352)) ;
#106235 = CARTESIAN_POINT('Ctrl Pts',(-19.6888096358805,-16.5614208757913,
124.893152467969)) ;
#106236 = CARTESIAN_POINT('Ctrl Pts',(-19.9380161975764,-16.5712685161386,
124.823385534915)) ;
#106237 = CARTESIAN_POINT('Ctrl Pts',(-20.1743666544338,-16.5812302315152,
124.710857010624)) ;
#106238 = CARTESIAN_POINT('Ctrl Pts',(-20.3888501617689,-16.591258855088,
124.557691167394)) ;
#106239 = CARTESIAN_POINT('Ctrl Pts',(-20.5713434225221,-16.6011692171544,
124.371907329123)) ;
#106240 = CARTESIAN_POINT('Ctrl Pts',(-20.7197488159772,-16.6111039108068,
124.157103939967)) ;
#106241 = CARTESIAN_POINT('Ctrl Pts',(-20.8295291223563,-16.6211457539347,
123.917148213344)) ;
#106242 = CARTESIAN_POINT('Ctrl Pts',(-20.8951698637997,-16.6310302595051,
123.665797293979)) ;
#106243 = CARTESIAN_POINT('Ctrl Pts',(-20.9167212692526,-16.6410323632903,
123.403875986852)) ;
#106244 = CARTESIAN_POINT('Ctrl Pts',(-20.8928773969328,-16.6509507147053,
123.1442814441)) ;
#106245 = CARTESIAN_POINT('Ctrl Pts',(-20.8233840795144,-16.6609983707262,
122.889591453258)) ;
#106246 = CARTESIAN_POINT('Ctrl Pts',(-20.7129252170611,-16.6708695637544,
122.654819502482)) ;
#106247 = CARTESIAN_POINT('Ctrl Pts',(-20.5605354982696,-16.6809352768979,
122.438686260115)) ;
#106248 = CARTESIAN_POINT('Ctrl Pts',(-20.3770240889657,-16.6907877374706,
122.255936128519)) ;
#106249 = CARTESIAN_POINT('Ctrl Pts',(-20.087548406569,-16.7042162001931,
122.054303583676)) ;
#106250 = CARTESIAN_POINT('Ctrl Pts',(-19.7606789820006,-16.7172971477102,
121.935420000031)) ;
#106251 = CARTESIAN_POINT('Ctrl Pts',(-19.4080350522028,-16.7307716459448,
121.904256007586)) ;
#106252 = CARTESIAN_POINT('Ctrl Pts',(-19.1506104608583,-16.7406037495542,
121.926903242143)) ;
#106253 = CARTESIAN_POINT('Ctrl Pts',(-18.8974323765611,-16.7505696526809,
121.993771587501)) ;
#106254 = CARTESIAN_POINT('Ctrl Pts',(-18.6583554923555,-16.7605970619911,
122.104659747869)) ;
#106255 = CARTESIAN_POINT('Ctrl Pts',(-18.4446854779983,-16.7705080933577,
122.253532722493)) ;
#106256 = CARTESIAN_POINT('Ctrl Pts',(-18.1971636646785,-16.7837524009787,
122.498316557246)) ;
#106257 = CARTESIAN_POINT('Ctrl Pts',(-17.9735940338532,-16.8004528836499,
122.881662292758)) ;
#106258 = CARTESIAN_POINT('Ctrl Pts',(-17.8949269013525,-16.8169597128057,
123.313347762815)) ;
#106259 = CARTESIAN_POINT('Ctrl Pts',(-17.9226464741625,-16.8302703410433,
123.661998443756)) ;
#106260 = CARTESIAN_POINT('Ctrl Pts',(-17.9885500170473,-16.8402629045834,
123.916229875979)) ;
#106261 = CARTESIAN_POINT('Ctrl Pts',(-18.0982623423877,-16.8502929875849,
124.155855958058)) ;
#106262 = CARTESIAN_POINT('Ctrl Pts',(-18.2942872666369,-16.8634665915827,
124.441278247379)) ;
#106263 = CARTESIAN_POINT('Ctrl Pts',(-18.6299061183238,-16.8801042968141,
124.728954007652)) ;
#106264 = CARTESIAN_POINT('Ctrl Pts',(-19.1244459055575,-16.8999860593815,
124.915699707355)) ;
#106265 = CARTESIAN_POINT('Ctrl Pts',(-19.5680324815316,-16.916682411598,
124.921092180331)) ;
#106266 = CARTESIAN_POINT('Ctrl Pts',(-19.9032333390617,-16.9298394393871,
124.836022746457)) ;
#106267 = CARTESIAN_POINT('Ctrl Pts',(-20.2240355606206,-16.9432167940307,
124.692342653553)) ;
#106268 = CARTESIAN_POINT('Ctrl Pts',(-20.564889178668,-16.9597476282895,
124.415021464963)) ;
#106269 = CARTESIAN_POINT('Ctrl Pts',(-20.8382412988788,-16.9797123180326,
123.960277734278)) ;
#106270 = CARTESIAN_POINT('Ctrl Pts',(-20.9392835418282,-16.9996288114562,
123.440651482369)) ;
#106271 = CARTESIAN_POINT('Ctrl Pts',(-20.8580861687626,-17.0195185308058,
122.918235270945)) ;
#106272 = CARTESIAN_POINT('Ctrl Pts',(-20.6016768774655,-17.0395252604536,
122.452481906483)) ;
#106273 = CARTESIAN_POINT('Ctrl Pts',(-20.2052175288422,-17.0593633141005,
122.104716301636)) ;
#106274 = CARTESIAN_POINT('Ctrl Pts',(-19.7104254026965,-17.0793566523141,
121.911189175635)) ;
#106275 = CARTESIAN_POINT('Ctrl Pts',(-19.1820266687273,-17.0992394517207,
121.898521473643)) ;
#106276 = CARTESIAN_POINT('Ctrl Pts',(-18.6807377304385,-17.1191316326394,
122.066075438973)) ;
#106277 = CARTESIAN_POINT('Ctrl Pts',(-18.2657133225145,-17.1390338111345,
122.394294335146)) ;
#106278 = CARTESIAN_POINT('Ctrl Pts',(-17.9866603659834,-17.1590711223382,
122.847724178873)) ;
#106279 = CARTESIAN_POINT('Ctrl Pts',(-17.8794978535988,-17.1788835638791,
123.363523177826)) ;
#106280 = CARTESIAN_POINT('Ctrl Pts',(-17.9558402348989,-17.198948804614,
123.891074767645)) ;
#106281 = CARTESIAN_POINT('Ctrl Pts',(-18.2036314096174,-17.2187060094698,
124.354333762872)) ;
#106282 = CARTESIAN_POINT('Ctrl Pts',(-18.5991823651955,-17.2387392821155,
124.710365554542)) ;
#106283 = CARTESIAN_POINT('Ctrl Pts',(-19.0875497902478,-17.2585521905694,
124.907973528954)) ;
#106284 = CARTESIAN_POINT('Ctrl Pts',(-19.6184027284767,-17.2785483366968,
124.927930635947)) ;
#106285 = CARTESIAN_POINT('Ctrl Pts',(-20.1213295234125,-17.2984100899193,
124.766739572709)) ;
#106286 = CARTESIAN_POINT('Ctrl Pts',(-20.5429252904641,-17.3184786070474,
124.440190715913)) ;
#106287 = CARTESIAN_POINT('Ctrl Pts',(-20.8242377074494,-17.3383094800442,
123.994332355414)) ;
#106288 = CARTESIAN_POINT('Ctrl Pts',(-20.9383799614121,-17.3582313908609,
123.477416013546)) ;
#106289 = CARTESIAN_POINT('Ctrl Pts',(-20.8690667085864,-17.3781608342962,
122.952191601519)) ;
#106290 = CARTESIAN_POINT('Ctrl Pts',(-20.6251748641544,-17.3980705044126,
122.482671780441)) ;
#106291 = CARTESIAN_POINT('Ctrl Pts',(-20.2369461402496,-17.4179438616755,
122.124424796588)) ;
#106292 = CARTESIAN_POINT('Ctrl Pts',(-19.7469586060816,-17.4379353962934,
121.919092941373)) ;
#106293 = CARTESIAN_POINT('Ctrl Pts',(-19.2195163903342,-17.4578010137041,
121.893229788818)) ;
#106294 = CARTESIAN_POINT('Ctrl Pts',(-18.7119189138773,-17.4777819435324,
122.049276613145)) ;
#106295 = CARTESIAN_POINT('Ctrl Pts',(-18.2892740598292,-17.4977204056155,
122.368981249758)) ;
#106296 = CARTESIAN_POINT('Ctrl Pts',(-18.0010468981692,-17.5176125988372,
122.812282126903)) ;
#106297 = CARTESIAN_POINT('Ctrl Pts',(-17.8812114661652,-17.5375833138726,
123.329247053136)) ;
#106298 = CARTESIAN_POINT('Ctrl Pts',(-17.9435998730545,-17.5573929855387,
123.852172416276)) ;
#106299 = CARTESIAN_POINT('Ctrl Pts',(-18.1823889066132,-17.5773862022299,
124.326665444011)) ;
#106300 = CARTESIAN_POINT('Ctrl Pts',(-18.5660143257143,-17.5972371144262,
124.689196530154)) ;
#106301 = CARTESIAN_POINT('Ctrl Pts',(-19.0555661838495,-17.6173117207453,
124.900996777746)) ;
#106302 = CARTESIAN_POINT('Ctrl Pts',(-19.4939397624789,-17.6338283526286,
124.927071266426)) ;
#106303 = CARTESIAN_POINT('Ctrl Pts',(-19.8373477851009,-17.6471670603227,
124.857183829402)) ;
#106304 = CARTESIAN_POINT('Ctrl Pts',(-20.0781861357582,-17.657009434631,
124.762756345354)) ;
#106305 = CARTESIAN_POINT('Ctrl Pts',(-20.3038016916689,-17.6670644546137,
124.625289262735)) ;
#106306 = CARTESIAN_POINT('Ctrl Pts',(-20.5648525379712,-17.6802966112713,
124.395511911604)) ;
#106307 = CARTESIAN_POINT('Ctrl Pts',(-20.8101382457707,-17.6969115786164,
124.028340182792)) ;
#106308 = CARTESIAN_POINT('Ctrl Pts',(-20.9150913429758,-17.7135061656276,
123.59996828002)) ;
#106309 = CARTESIAN_POINT('Ctrl Pts',(-20.9083194371966,-17.726739733983,
123.252245244698)) ;
#106310 = CARTESIAN_POINT('Ctrl Pts',(-20.8574972331854,-17.7367833517917,
122.993271365675)) ;
#106311 = CARTESIAN_POINT('Ctrl Pts',(-20.764029698907,-17.7466702760265,
122.750824428413)) ;
#106312 = CARTESIAN_POINT('Ctrl Pts',(-20.6288988859951,-17.7566609304733,
122.52574713789)) ;
#106313 = CARTESIAN_POINT('Ctrl Pts',(-20.4571856548047,-17.7666226889273,
122.328145639307)) ;
#106314 = CARTESIAN_POINT('Ctrl Pts',(-20.1849772827388,-17.7799625539945,
122.1071474189)) ;
#106315 = CARTESIAN_POINT('Ctrl Pts',(-19.8618446927866,-17.7932713369078,
121.963370845515)) ;
#106316 = CARTESIAN_POINT('Ctrl Pts',(-19.5194408838435,-17.8064670943519,
121.908500061453)) ;
#106317 = CARTESIAN_POINT('Ctrl Pts',(-19.2576702789978,-17.8164289780284,
121.911860337641)) ;
#106318 = CARTESIAN_POINT('Ctrl Pts',(-18.9984511732404,-17.826472087543,
121.961443066913)) ;
#106319 = CARTESIAN_POINT('Ctrl Pts',(-18.7563454905763,-17.8363243375422,
122.053214389354)) ;
#106320 = CARTESIAN_POINT('Ctrl Pts',(-18.5308613892002,-17.8462958744927,
122.186659294031)) ;
#106321 = CARTESIAN_POINT('Ctrl Pts',(-18.3314608275269,-17.8562911399702,
122.357696687906)) ;
#106322 = CARTESIAN_POINT('Ctrl Pts',(-18.1644321330469,-17.8663251128439,
122.56170136985)) ;
#106323 = CARTESIAN_POINT('Ctrl Pts',(-18.0372772522099,-17.8761805276062,
122.787357009147)) ;
#106324 = CARTESIAN_POINT('Ctrl Pts',(-17.9496644830433,-17.886179805115,
123.035043600757)) ;
#106325 = CARTESIAN_POINT('Ctrl Pts',(-17.9065487373405,-17.896074989278,
123.291524479843)) ;
#106326 = CARTESIAN_POINT('Ctrl Pts',(-17.9086851881469,-17.9061353689188,
123.555856178888)) ;
#106327 = CARTESIAN_POINT('Ctrl Pts',(-17.9555360244664,-17.9159852379269,
123.810451246354)) ;
#106328 = CARTESIAN_POINT('Ctrl Pts',(-18.0469682041802,-17.9260167991348,
124.057688557199)) ;
#106329 = CARTESIAN_POINT('Ctrl Pts',(-18.1801385787073,-17.9360272480171,
124.284582911936)) ;
#106330 = CARTESIAN_POINT('Ctrl Pts',(-18.3486755036932,-17.9459339874341,
124.482994407031)) ;
#106331 = CARTESIAN_POINT('Ctrl Pts',(-18.5494063023353,-17.9558720035025,
124.650040004162)) ;
#106332 = CARTESIAN_POINT('Ctrl Pts',(-18.7775774979802,-17.9658772499537,
124.780743652177)) ;
#106333 = CARTESIAN_POINT('Ctrl Pts',(-19.0258028917251,-17.97591131101,124.869663326483)) ;
#106334 = CARTESIAN_POINT('Ctrl Pts',(-19.2807552443101,-17.9857563920681,
124.913740300713)) ;
#106335 = CARTESIAN_POINT('Ctrl Pts',(-19.5431300648516,-17.9957421980216,
124.913357879036)) ;
#106336 = CARTESIAN_POINT('Ctrl Pts',(-19.8002551560576,-18.0056770185758,
124.867827638442)) ;
#106337 = CARTESIAN_POINT('Ctrl Pts',(-20.0484362054016,-18.015734543708,
124.777046260329)) ;
#106338 = CARTESIAN_POINT('Ctrl Pts',(-20.2719773851506,-18.0255561943594,
124.647968643264)) ;
#106339 = CARTESIAN_POINT('Ctrl Pts',(-20.4747082782769,-18.0356122578641,
124.478488060217)) ;
#106340 = CARTESIAN_POINT('Ctrl Pts',(-20.6426391301246,-18.045552924928,
124.278372755303)) ;
#106341 = CARTESIAN_POINT('Ctrl Pts',(-20.7735002160438,-18.055457318594,
124.05337893199)) ;
#106342 = CARTESIAN_POINT('Ctrl Pts',(-20.8644257535316,-18.065503842357,
123.805543745991)) ;
#106343 = CARTESIAN_POINT('Ctrl Pts',(-20.9105004800301,-18.0753999253734,
123.549551389803)) ;
#106344 = CARTESIAN_POINT('Ctrl Pts',(-20.9113777941463,-18.0854666246034,
123.285058179939)) ;
#106345 = CARTESIAN_POINT('Ctrl Pts',(-20.8676853361429,-18.0952902350045,
123.03058768618)) ;
#106346 = CARTESIAN_POINT('Ctrl Pts',(-20.7788729200758,-18.105346095182,
122.781737389733)) ;
#106347 = CARTESIAN_POINT('Ctrl Pts',(-20.6494706999831,-18.1152792414869,
122.555000037183)) ;
#106348 = CARTESIAN_POINT('Ctrl Pts',(-20.4829128435799,-18.1252244972575,
122.353637264426)) ;
#106349 = CARTESIAN_POINT('Ctrl Pts',(-20.2832491516113,-18.135207795696,
122.183403536089)) ;
#106350 = CARTESIAN_POINT('Ctrl Pts',(-20.0557030935706,-18.1452449758426,
122.050043065921)) ;
#106351 = CARTESIAN_POINT('Ctrl Pts',(-19.8130548469334,-18.1550995285521,
121.959496203721)) ;
#106352 = CARTESIAN_POINT('Ctrl Pts',(-19.5547600095876,-18.1650990469994,
121.911417252106)) ;
#106353 = CARTESIAN_POINT('Ctrl Pts',(-19.2946981607861,-18.1749941294615,
121.908665977267)) ;
#106354 = CARTESIAN_POINT('Ctrl Pts',(-19.0339004563328,-18.1850546749676,
121.951834448406)) ;
#106355 = CARTESIAN_POINT('Ctrl Pts',(-18.7896960288208,-18.1949039822156,
122.037668069937)) ;
#106356 = CARTESIAN_POINT('Ctrl Pts',(-18.559727806406,-18.204931072303,122.166293607386)) ;
#106357 = CARTESIAN_POINT('Ctrl Pts',(-18.3559794762093,-18.2149599764399,
122.333478186959)) ;
#106358 = CARTESIAN_POINT('Ctrl Pts',(-18.187145941362,-18.2248038415392,
122.529460192013)) ;
#106359 = CARTESIAN_POINT('Ctrl Pts',(-18.0523029774518,-18.2347996682476,
122.75488871841)) ;
#106360 = CARTESIAN_POINT('Ctrl Pts',(-17.9588260064402,-18.2448248848966,
123.001205208719)) ;
#106361 = CARTESIAN_POINT('Ctrl Pts',(-17.909859628747,-18.2547147170542,
123.256449962964)) ;
#106362 = CARTESIAN_POINT('Ctrl Pts',(-17.9055571019604,-18.2647055731389,
123.518955212677)) ;
#106363 = CARTESIAN_POINT('Ctrl Pts',(-17.946760077564,-18.2746506677318,
123.777033194957)) ;
#106364 = CARTESIAN_POINT('Ctrl Pts',(-18.0317466001249,-18.2846025714999,
124.024375730122)) ;
#106365 = CARTESIAN_POINT('Ctrl Pts',(-18.1596578210665,-18.2946389709693,
124.255020663488)) ;
#106366 = CARTESIAN_POINT('Ctrl Pts',(-18.3230984485718,-18.304528041058,
124.457076640382)) ;
#106367 = CARTESIAN_POINT('Ctrl Pts',(-18.5208050093406,-18.3145173304289,
124.629759420022)) ;
#106368 = CARTESIAN_POINT('Ctrl Pts',(-18.7449002910131,-18.3244758966386,
124.764905710238)) ;
#106369 = CARTESIAN_POINT('Ctrl Pts',(-18.9874020685132,-18.3343754678554,
124.859137657346)) ;
#106370 = CARTESIAN_POINT('Ctrl Pts',(-19.2463807699488,-18.3444233822697,
124.910491523554)) ;
#106371 = CARTESIAN_POINT('Ctrl Pts',(-19.5063983310136,-18.3543187251302,
124.916218951669)) ;
#106372 = CARTESIAN_POINT('Ctrl Pts',(-19.7677160165026,-18.3643804190777,
124.876094658187)) ;
#106373 = CARTESIAN_POINT('Ctrl Pts',(-20.0127459205571,-18.3742248721618,
124.793068730627)) ;
#106374 = CARTESIAN_POINT('Ctrl Pts',(-20.2427353819954,-18.3841855571203,
124.668108697324)) ;
#106375 = CARTESIAN_POINT('Ctrl Pts',(-20.4488207458198,-18.3942214896288,
124.503522047669)) ;
#106376 = CARTESIAN_POINT('Ctrl Pts',(-20.6208245138306,-18.4041101053169,
124.308738320437)) ;
#106377 = CARTESIAN_POINT('Ctrl Pts',(-20.7585778713558,-18.4141245144593,
124.084482018134)) ;
#106378 = CARTESIAN_POINT('Ctrl Pts',(-20.8548377910797,-18.4241583234171,
123.839019941139)) ;
#106379 = CARTESIAN_POINT('Ctrl Pts',(-20.9066734537542,-18.4339887776733,
123.585907801548)) ;
#106380 = CARTESIAN_POINT('Ctrl Pts',(-20.914035005145,-18.4440664452515,
123.321231030085)) ;
#106381 = CARTESIAN_POINT('Ctrl Pts',(-20.8763128759204,-18.4539183133737,
123.065039782378)) ;
#106382 = CARTESIAN_POINT('Ctrl Pts',(-20.7930887940635,-18.4639913509391,
122.813802107572)) ;
#106383 = CARTESIAN_POINT('Ctrl Pts',(-20.6703133695583,-18.47383390429,122.58612058865)) ;
#106384 = CARTESIAN_POINT('Ctrl Pts',(-20.5083368229073,-18.4838142997834,
122.379854902302)) ;
#106385 = CARTESIAN_POINT('Ctrl Pts',(-20.3119149758055,-18.4938327777612,
122.204557816278)) ;
#106386 = CARTESIAN_POINT('Ctrl Pts',(-20.0913199809114,-18.5037160920673,
122.067406308123)) ;
#106387 = CARTESIAN_POINT('Ctrl Pts',(-19.8457770815624,-18.513784394606,
121.968966609074)) ;
#106388 = CARTESIAN_POINT('Ctrl Pts',(-19.5929747381115,-18.5236144418794,
121.915623759485)) ;
#106389 = CARTESIAN_POINT('Ctrl Pts',(-19.3286319421843,-18.5336813132949,
121.906445897827)) ;
#106390 = CARTESIAN_POINT('Ctrl Pts',(-19.0712757729958,-18.543570352094,
121.942804033126)) ;
#106391 = CARTESIAN_POINT('Ctrl Pts',(-18.821355081623,-18.5535670502281,
122.023662185229)) ;
#106392 = CARTESIAN_POINT('Ctrl Pts',(-18.5903099011435,-18.5635194759401,
122.146260462174)) ;
#106393 = CARTESIAN_POINT('Ctrl Pts',(-18.3840985282772,-18.573460778173,
122.306624856923)) ;
#106394 = CARTESIAN_POINT('Ctrl Pts',(-18.2078826377361,-18.5834440172569,
122.501023786274)) ;
#106395 = CARTESIAN_POINT('Ctrl Pts',(-18.0676953784142,-18.5934828188255,
122.7244758304)) ;
#106396 = CARTESIAN_POINT('Ctrl Pts',(-17.9698362461543,-18.6033309249472,
122.964084842904)) ;
#106397 = CARTESIAN_POINT('Ctrl Pts',(-17.9136564349659,-18.6133911205225,
123.222395340427)) ;
#106398 = CARTESIAN_POINT('Ctrl Pts',(-17.9035861785321,-18.6232888038339,
123.482312245733)) ;
#106399 = CARTESIAN_POINT('Ctrl Pts',(-17.9380672693669,-18.6332198442079,
123.740997360846)) ;
#106400 = CARTESIAN_POINT('Ctrl Pts',(-18.0180952724909,-18.6432620618645,
123.992465098917)) ;
#106401 = CARTESIAN_POINT('Ctrl Pts',(-18.1385156099613,-18.6531487225985,
124.222698255833)) ;
#106402 = CARTESIAN_POINT('Ctrl Pts',(-18.2984251565987,-18.663141831201,
124.430989059659)) ;
#106403 = CARTESIAN_POINT('Ctrl Pts',(-18.4912300319267,-18.6730875298392,
124.607445393199)) ;
#106404 = CARTESIAN_POINT('Ctrl Pts',(-18.7115019926513,-18.6830347521103,
124.748223682838)) ;
#106405 = CARTESIAN_POINT('Ctrl Pts',(-18.9554118568086,-18.6930827776904,
124.849350889407)) ;
#106406 = CARTESIAN_POINT('Ctrl Pts',(-19.2079857719931,-18.7029300248333,
124.905664069437)) ;
#106407 = CARTESIAN_POINT('Ctrl Pts',(-19.4695005317294,-18.712893201924,
124.918229762502)) ;
#106408 = CARTESIAN_POINT('Ctrl Pts',(-19.7309117193007,-18.7229229229575,
124.884581451279)) ;
#106409 = CARTESIAN_POINT('Ctrl Pts',(-19.9794879753624,-18.7328273904903,
124.807331616421)) ;
#106410 = CARTESIAN_POINT('Ctrl Pts',(-20.2136713900044,-18.7428518763201,
124.686754120868)) ;
#106411 = CARTESIAN_POINT('Ctrl Pts',(-20.4210216017489,-18.752755711444,
124.529395994289)) ;
#106412 = CARTESIAN_POINT('Ctrl Pts',(-20.6005285093603,-18.762806902154,
124.335672824434)) ;
#106413 = CARTESIAN_POINT('Ctrl Pts',(-20.7413686076851,-18.7726913448123,
124.117385719784)) ;
#106414 = CARTESIAN_POINT('Ctrl Pts',(-20.8437048455114,-18.7826843526642,
123.875565880719)) ;
#106415 = CARTESIAN_POINT('Ctrl Pts',(-20.9021579365581,-18.7926326723805,
123.620735391782)) ;
#106416 = CARTESIAN_POINT('Ctrl Pts',(-20.9158318547924,-18.8025695110899,
123.359986539688)) ;
#106417 = CARTESIAN_POINT('Ctrl Pts',(-20.8841973543679,-18.8125525000095,
123.099524249898)) ;
#106418 = CARTESIAN_POINT('Ctrl Pts',(-20.806906706318,-18.8225963793736,
122.847184221893)) ;
#106419 = CARTESIAN_POINT('Ctrl Pts',(-20.6900671314966,-18.832424444732,
122.616806023797)) ;
#106420 = CARTESIAN_POINT('Ctrl Pts',(-20.5312234748615,-18.8425015332869,
122.40499355955)) ;
#106421 = CARTESIAN_POINT('Ctrl Pts',(-20.3423910055015,-18.8523516854432,
122.227844954724)) ;
#106422 = CARTESIAN_POINT('Ctrl Pts',(-20.1207728474674,-18.8624321658956,
122.082847269407)) ;
#106423 = CARTESIAN_POINT('Ctrl Pts',(-19.883742672593,-18.8722466636644,
121.981028207719)) ;
#106424 = CARTESIAN_POINT('Ctrl Pts',(-19.6263552357051,-18.8823149596845,
121.920005976906)) ;
#106425 = CARTESIAN_POINT('Ctrl Pts',(-19.3665955247242,-18.8922137921673,
121.904926016913)) ;
#106426 = CARTESIAN_POINT('Ctrl Pts',(-19.1042510947815,-18.9022666721818,
121.935545005745)) ;
#106427 = CARTESIAN_POINT('Ctrl Pts',(-18.8556439453619,-18.912136487678,
122.0096688688)) ;
#106428 = CARTESIAN_POINT('Ctrl Pts',(-18.618972458441,-18.9222091687608,
122.128110319243)) ;
#106429 = CARTESIAN_POINT('Ctrl Pts',(-18.4114114475345,-18.9320416473318,
122.282045205)) ;
#106430 = CARTESIAN_POINT('Ctrl Pts',(-18.2296251987227,-18.9420722813179,
122.472912692922)) ;
#106431 = CARTESIAN_POINT('Ctrl Pts',(-18.0843565052715,-18.952103838537,
122.692912211398)) ;
#106432 = CARTESIAN_POINT('Ctrl Pts',(-17.9811210290767,-18.9619335474087,
122.929682254542)) ;
#106433 = CARTESIAN_POINT('Ctrl Pts',(-17.9188134712932,-18.9719229962108,
123.184700918537)) ;
#106434 = CARTESIAN_POINT('Ctrl Pts',(-17.9023076564122,-18.9819668486108,
123.448123362392)) ;
#106435 = CARTESIAN_POINT('Ctrl Pts',(-17.9306090900977,-18.9917885619429,
123.704671597423)) ;
#106436 = CARTESIAN_POINT('Ctrl Pts',(-18.0039766331201,-19.0018235669316,
123.957968446456)) ;
#106437 = CARTESIAN_POINT('Ctrl Pts',(-18.1207526601657,-19.0118484053792,
124.194124766735)) ;
#106438 = CARTESIAN_POINT('Ctrl Pts',(-18.2736214503215,-19.0217006183344,
124.403083451732)) ;
#106439 = CARTESIAN_POINT('Ctrl Pts',(-18.4627386535141,-19.0316905745282,
124.585137888009)) ;
#106440 = CARTESIAN_POINT('Ctrl Pts',(-18.6792568285447,-19.0416186848114,
124.730717366156)) ;
#106441 = CARTESIAN_POINT('Ctrl Pts',(-18.9190451892015,-19.051607284891,
124.837516605335)) ;
#106442 = CARTESIAN_POINT('Ctrl Pts',(-19.17478938836,-19.0616338768185,124.900946309927)) ;
#106443 = CARTESIAN_POINT('Ctrl Pts',(-19.4339240466304,-19.0715190048827,
124.919023725335)) ;
#106444 = CARTESIAN_POINT('Ctrl Pts',(-19.6951092838121,-19.0815101223562,
124.892133492119)) ;
#106445 = CARTESIAN_POINT('Ctrl Pts',(-19.9487459478845,-19.091550738208,
124.819413432375)) ;
#106446 = CARTESIAN_POINT('Ctrl Pts',(-20.1811840640544,-19.1013837290617,
124.70653484289)) ;
#106447 = CARTESIAN_POINT('Ctrl Pts',(-20.3943411849958,-19.111376860512,
124.553155226563)) ;
#106448 = CARTESIAN_POINT('Ctrl Pts',(-20.5779607961446,-19.1214089089474,
124.363967453322)) ;
#106449 = CARTESIAN_POINT('Ctrl Pts',(-20.7237317632523,-19.1312741554898,
124.149599190906)) ;
#106450 = CARTESIAN_POINT('Ctrl Pts',(-20.8317939999319,-19.1412360303166,
123.911146942398)) ;
#106451 = CARTESIAN_POINT('Ctrl Pts',(-20.8968646296207,-19.1512709934279,
123.655608116611)) ;
#106452 = CARTESIAN_POINT('Ctrl Pts',(-20.9167254208125,-19.1611558378903,
123.396566812288)) ;
#106453 = CARTESIAN_POINT('Ctrl Pts',(-20.8907810854594,-19.171221890731,
123.133363415736)) ;
#106454 = CARTESIAN_POINT('Ctrl Pts',(-20.821401757124,-19.18105940664,122.884277322582)) ;
#106455 = CARTESIAN_POINT('Ctrl Pts',(-20.7074990989134,-19.1911281547489,
122.645503335447)) ;
#106456 = CARTESIAN_POINT('Ctrl Pts',(-20.5566118051901,-19.2010086717799,
122.434146389785)) ;
#106457 = CARTESIAN_POINT('Ctrl Pts',(-20.3696719514997,-19.2109998587144,
122.249837001454)) ;
#106458 = CARTESIAN_POINT('Ctrl Pts',(-20.1543532022229,-19.2209529249893,
122.101276348325)) ;
#106459 = CARTESIAN_POINT('Ctrl Pts',(-19.9145523374295,-19.2309887625219,
121.991556903284)) ;
#106460 = CARTESIAN_POINT('Ctrl Pts',(-19.6630559532501,-19.2408788887333,
121.925924400167)) ;
#106461 = CARTESIAN_POINT('Ctrl Pts',(-19.4013754300174,-19.2508710706413,
121.904322728888)) ;
#106462 = CARTESIAN_POINT('Ctrl Pts',(-19.1411235059261,-19.2608170105799,
121.928462871379)) ;
#106463 = CARTESIAN_POINT('Ctrl Pts',(-18.888832049536,-19.270764194344,121.996925162307)) ;
#106464 = CARTESIAN_POINT('Ctrl Pts',(-18.6500106042988,-19.2808121326514,
122.109537997861)) ;
#106465 = CARTESIAN_POINT('Ctrl Pts',(-18.4385333286377,-19.2906597673917,
122.258697701724)) ;
#106466 = CARTESIAN_POINT('Ctrl Pts',(-18.2534839295302,-19.3006214813655,
122.443848789793)) ;
#106467 = CARTESIAN_POINT('Ctrl Pts',(-18.1026428206701,-19.3106501161564,
122.659973777943)) ;
#106468 = CARTESIAN_POINT('Ctrl Pts',(-17.9928644421991,-19.3205604347535,
122.896125581501)) ;
#106469 = CARTESIAN_POINT('Ctrl Pts',(-17.9249226826456,-19.330495291065,
123.148217847419)) ;
#106470 = CARTESIAN_POINT('Ctrl Pts',(-17.9017919560051,-19.3405365270257,
123.411062876142)) ;
#106471 = CARTESIAN_POINT('Ctrl Pts',(-17.9240882463519,-19.3504232986057,
123.669943886338)) ;
#106472 = CARTESIAN_POINT('Ctrl Pts',(-17.9914404271819,-19.3604234773119,
123.923920647487)) ;
#106473 = CARTESIAN_POINT('Ctrl Pts',(-18.1007825311999,-19.3703407555215,
124.160537445714)) ;
#106474 = CARTESIAN_POINT('Ctrl Pts',(-18.2515181964316,-19.3803880019352,
124.377267386815)) ;
#106475 = CARTESIAN_POINT('Ctrl Pts',(-18.4342421500733,-19.3902618909165,
124.561551217845)) ;
#106476 = CARTESIAN_POINT('Ctrl Pts',(-18.6500824820261,-19.400323908497,
124.714238050506)) ;
#106477 = CARTESIAN_POINT('Ctrl Pts',(-18.8846797503778,-19.4101949702313,
124.824974685142)) ;
#106478 = CARTESIAN_POINT('Ctrl Pts',(-19.1378473143189,-19.4201890335916,
124.894848560065)) ;
#106479 = CARTESIAN_POINT('Ctrl Pts',(-19.4003460422337,-19.430221191625,
124.91921432023)) ;
#106480 = CARTESIAN_POINT('Ctrl Pts',(-19.6587612544916,-19.4400850678652,
124.898556778381)) ;
#106481 = CARTESIAN_POINT('Ctrl Pts',(-19.9148714014531,-19.4501555825034,
124.832021587794)) ;
#106482 = CARTESIAN_POINT('Ctrl Pts',(-20.1501011154799,-19.4599962194444,
124.7245403623)) ;
#106483 = CARTESIAN_POINT('Ctrl Pts',(-20.3662873595265,-19.4699633482846,
124.576700551369)) ;
#106484 = CARTESIAN_POINT('Ctrl Pts',(-20.554234692162,-19.4799773214091,
124.392483132149)) ;
#106485 = CARTESIAN_POINT('Ctrl Pts',(-20.757429884363,-19.4932620552724,
124.108579686335)) ;
#106486 = CARTESIAN_POINT('Ctrl Pts',(-20.8815848706378,-19.5064873199872,
123.779792856729)) ;
#106487 = CARTESIAN_POINT('Ctrl Pts',(-20.9167212645903,-19.519797842542,
123.431736281204)) ;
#106488 = CARTESIAN_POINT('Ctrl Pts',(-20.8970459424392,-19.5298264874442,
123.168938625735)) ;
#106489 = CARTESIAN_POINT('Ctrl Pts',(-20.8332169752799,-19.5397075197981,
122.917236633693)) ;
#106490 = CARTESIAN_POINT('Ctrl Pts',(-20.7260774305387,-19.5496884924782,
122.677830163903)) ;
#106491 = CARTESIAN_POINT('Ctrl Pts',(-20.5788138255665,-19.5596696200642,
122.46079673458)) ;
#106492 = CARTESIAN_POINT('Ctrl Pts',(-20.3368625325848,-19.5729128103256,
122.210551925323)) ;
#106493 = CARTESIAN_POINT('Ctrl Pts',(-19.9569993363786,-19.5895808056864,
121.982803218007)) ;
#106494 = CARTESIAN_POINT('Ctrl Pts',(-19.52596625381,-19.6061013056984,121.898737371643)) ;
#106495 = CARTESIAN_POINT('Ctrl Pts',(-19.1769558296142,-19.6194143220144,
121.922390771414)) ;
#106496 = CARTESIAN_POINT('Ctrl Pts',(-18.9238470842411,-19.6293308802474,
121.984587811698)) ;
#106497 = CARTESIAN_POINT('Ctrl Pts',(-18.6828424329629,-19.6393585485503,
122.091010950231)) ;
#106498 = CARTESIAN_POINT('Ctrl Pts',(-18.3945215350689,-19.652539138295,
122.283192537924)) ;
#106499 = CARTESIAN_POINT('Ctrl Pts',(-18.1010219937371,-19.6692872774143,
122.617581162048)) ;
#106500 = CARTESIAN_POINT('Ctrl Pts',(-17.909366822418,-19.6890820199249,
123.107805255079)) ;
#106501 = CARTESIAN_POINT('Ctrl Pts',(-17.895809920963,-19.7091264127337,
123.640196037311)) ;
#106502 = CARTESIAN_POINT('Ctrl Pts',(-18.0635546861433,-19.7289655950324,
124.140244908333)) ;
#106503 = CARTESIAN_POINT('Ctrl Pts',(-18.3921051298467,-19.7488909187253,
124.55542693416)) ;
#106504 = CARTESIAN_POINT('Ctrl Pts',(-18.8427943342149,-19.7688145567768,
124.833601017677)) ;
#106505 = CARTESIAN_POINT('Ctrl Pts',(-19.3612107685592,-19.7887394302423,
124.941419506668)) ;
#106506 = CARTESIAN_POINT('Ctrl Pts',(-19.8842729339696,-19.8086180373213,
124.866702744528)) ;
#106507 = CARTESIAN_POINT('Ctrl Pts',(-20.3528435141273,-19.8285954801532,
124.616989142278)) ;
#106508 = CARTESIAN_POINT('Ctrl Pts',(-20.7070256130225,-19.8485273282379,
124.222974020889)) ;
#106509 = CARTESIAN_POINT('Ctrl Pts',(-20.9055758496834,-19.8684225965805,
123.732917749961)) ;
#106510 = CARTESIAN_POINT('Ctrl Pts',(-20.9255964967024,-19.8883450949926,
123.203776230308)) ;
#106511 = CARTESIAN_POINT('Ctrl Pts',(-20.7634093889317,-19.9083045768686,
122.698654704023)) ;
#106512 = CARTESIAN_POINT('Ctrl Pts',(-20.4400618251657,-19.928182329328,
122.28094819623)) ;
#106513 = CARTESIAN_POINT('Ctrl Pts',(-19.9941413395738,-19.9480641200625,
121.997227995206)) ;
#106514 = CARTESIAN_POINT('Ctrl Pts',(-19.4731423142849,-19.9681374589135,
121.882681860744)) ;
#106515 = CARTESIAN_POINT('Ctrl Pts',(-18.9512149180484,-19.9879419261493,
121.95174640087)) ;
#106516 = CARTESIAN_POINT('Ctrl Pts',(-18.4795837406758,-20.0079252665571,
122.195835512753)) ;
#106517 = CARTESIAN_POINT('Ctrl Pts',(-18.121364945746,-20.0278402311551,
122.585509526284)) ;
#106518 = CARTESIAN_POINT('Ctrl Pts',(-17.9166956650287,-20.0477087658715,
123.072415316463)) ;
#106519 = CARTESIAN_POINT('Ctrl Pts',(-17.891101767472,-20.0677611500832,
123.604604745487)) ;
#106520 = CARTESIAN_POINT('Ctrl Pts',(-18.0458952100454,-20.0875351138724,
124.107071415621)) ;
#106521 = CARTESIAN_POINT('Ctrl Pts',(-18.3667694167037,-20.1075894928938,
124.532413135122)) ;
#106522 = CARTESIAN_POINT('Ctrl Pts',(-18.8082077697032,-20.127386230467,
124.819020798246)) ;
#106523 = CARTESIAN_POINT('Ctrl Pts',(-19.3247806063206,-20.1473540428185,
124.940185255998)) ;
#106524 = CARTESIAN_POINT('Ctrl Pts',(-19.8515809478242,-20.1673130188835,
124.876974888948)) ;
#106525 = CARTESIAN_POINT('Ctrl Pts',(-20.3237113753369,-20.1872079371609,
124.638913265828)) ;
#106526 = CARTESIAN_POINT('Ctrl Pts',(-20.6867453183494,-20.2071042496112,
124.254470582453)) ;
#106527 = CARTESIAN_POINT('Ctrl Pts',(-20.8974946288054,-20.2270121829853,
123.769091874929)) ;
#106528 = CARTESIAN_POINT('Ctrl Pts',(-20.9299647653081,-20.2469620732738,
123.239897350838)) ;
#106529 = CARTESIAN_POINT('Ctrl Pts',(-20.7809358296733,-20.2668393037751,
122.732995434889)) ;
#106530 = CARTESIAN_POINT('Ctrl Pts',(-20.4664775913345,-20.2868219726461,
122.30502079141)) ;
#106531 = CARTESIAN_POINT('Ctrl Pts',(-20.025672670458,-20.3067548592265,
122.011026793588)) ;
#106532 = CARTESIAN_POINT('Ctrl Pts',(-19.5117141072868,-20.3266676052444,
121.884911373776)) ;
#106533 = CARTESIAN_POINT('Ctrl Pts',(-19.0738174714557,-20.3432373265862,
121.931707774582)) ;
#106534 = CARTESIAN_POINT('Ctrl Pts',(-18.7476557838818,-20.3565373378912,
122.057330938408)) ;
#106535 = CARTESIAN_POINT('Ctrl Pts',(-18.4486713364495,-20.3698075256411,
122.236858838282)) ;
#106536 = CARTESIAN_POINT('Ctrl Pts',(-18.1413778651806,-20.3864349080065,
122.554468364598)) ;
#106537 = CARTESIAN_POINT('Ctrl Pts',(-17.9611321734678,-20.4030571977517,
122.957827369364)) ;
#106538 = CARTESIAN_POINT('Ctrl Pts',(-17.9059585339821,-20.4163024121462,
123.301491619911)) ;
#106539 = CARTESIAN_POINT('Ctrl Pts',(-17.9091824912486,-20.4262143771069,
123.561964967123)) ;
#106540 = CARTESIAN_POINT('Ctrl Pts',(-17.9585940033797,-20.4362730002714,
123.821606026611)) ;
#106541 = CARTESIAN_POINT('Ctrl Pts',(-18.0499666096224,-20.4461131143872,
124.063553454512)) ;
#106542 = CARTESIAN_POINT('Ctrl Pts',(-18.1847206871367,-20.4561788993448,
124.291128959096)) ;
#106543 = CARTESIAN_POINT('Ctrl Pts',(-18.3539526261617,-20.4660622171327,
124.488192945778)) ;
#106544 = CARTESIAN_POINT('Ctrl Pts',(-18.5565782082668,-20.4760516549913,
124.65505176709)) ;
#106545 = CARTESIAN_POINT('Ctrl Pts',(-18.7845893768725,-20.486015369044,
124.78379811177)) ;
#106546 = CARTESIAN_POINT('Ctrl Pts',(-19.0321816787144,-20.4960103807032,
124.871535154767)) ;
#106547 = CARTESIAN_POINT('Ctrl Pts',(-19.2923532152617,-20.5060466723975,
124.914716267996)) ;
#106548 = CARTESIAN_POINT('Ctrl Pts',(-19.551111783383,-20.5158930500909,
124.91253933925)) ;
#106549 = CARTESIAN_POINT('Ctrl Pts',(-19.8091810772664,-20.5258779942416,
124.865307212237)) ;
#106550 = CARTESIAN_POINT('Ctrl Pts',(-20.0540749680961,-20.5358149653716,
124.774537714815)) ;
#106551 = CARTESIAN_POINT('Ctrl Pts',(-20.2819182027391,-20.5458647500033,
124.641041024722)) ;
#106552 = CARTESIAN_POINT('Ctrl Pts',(-20.4792920820102,-20.5557152120808,
124.473524605348)) ;
#106553 = CARTESIAN_POINT('Ctrl Pts',(-20.6471130882054,-20.5656872256012,
124.272300643355)) ;
#106554 = CARTESIAN_POINT('Ctrl Pts',(-20.7777557364887,-20.5756823727206,
124.044383982858)) ;
#106555 = CARTESIAN_POINT('Ctrl Pts',(-20.8668637360059,-20.5857163424567,
123.796238570436)) ;
#106556 = CARTESIAN_POINT('Ctrl Pts',(-20.9111469349061,-20.5955718881273,
123.541034504517)) ;
#106557 = CARTESIAN_POINT('Ctrl Pts',(-20.910805235039,-20.6055706451405,
123.278320314921)) ;
#106558 = CARTESIAN_POINT('Ctrl Pts',(-20.8655510690392,-20.6154677803777,
123.022161686187)) ;
#106559 = CARTESIAN_POINT('Ctrl Pts',(-20.7751709880732,-20.6255208762173,
122.77394668237)) ;
#106560 = CARTESIAN_POINT('Ctrl Pts',(-20.6452938391844,-20.6354043849479,
122.549002249442)) ;
#106561 = CARTESIAN_POINT('Ctrl Pts',(-20.4769385117555,-20.645399257594,
122.347408995479)) ;
#106562 = CARTESIAN_POINT('Ctrl Pts',(-20.2753518309184,-20.6554192192297,
122.177984016377)) ;
#106563 = CARTESIAN_POINT('Ctrl Pts',(-20.0501418873973,-20.6653245830296,
122.047462176748)) ;
#106564 = CARTESIAN_POINT('Ctrl Pts',(-19.8050172500671,-20.6752651706371,
121.957212454347)) ;
#106565 = CARTESIAN_POINT('Ctrl Pts',(-19.5463161812984,-20.6852679887378,
121.910449024445)) ;
#106566 = CARTESIAN_POINT('Ctrl Pts',(-19.2826301691876,-20.6953027004619,
121.909741281856)) ;
#106567 = CARTESIAN_POINT('Ctrl Pts',(-19.0276353696205,-20.7051476071992,
121.953549369446)) ;
#106568 = CARTESIAN_POINT('Ctrl Pts',(-18.7805229407793,-20.7151334597682,
122.041734471525)) ;
#106569 = CARTESIAN_POINT('Ctrl Pts',(-18.5534712355845,-20.7250682681813,
122.170706323137)) ;
#106570 = CARTESIAN_POINT('Ctrl Pts',(-18.349994251646,-20.7351257952623,
122.339324859272)) ;
#106571 = CARTESIAN_POINT('Ctrl Pts',(-18.1825547646236,-20.7449474502594,
122.53578295703)) ;
#106572 = CARTESIAN_POINT('Ctrl Pts',(-18.0482494320608,-20.7550034944324,
122.763346656922)) ;
#106573 = CARTESIAN_POINT('Ctrl Pts',(-17.9569902871531,-20.7649442344776,
123.008132090239)) ;
#106574 = CARTESIAN_POINT('Ctrl Pts',(-17.9089930326973,-20.7748483555505,
123.263941618772)) ;
#106575 = CARTESIAN_POINT('Ctrl Pts',(-17.9062624092731,-20.7848958967047,
123.527947604449)) ;
#106576 = CARTESIAN_POINT('Ctrl Pts',(-17.9485941174404,-20.7947946483051,
123.784643968814)) ;
#106577 = CARTESIAN_POINT('Ctrl Pts',(-18.0360287409758,-20.8048431272709,
124.033781132418)) ;
#106578 = CARTESIAN_POINT('Ctrl Pts',(-18.1633313086099,-20.8147306243546,
124.260323795961)) ;
#106579 = CARTESIAN_POINT('Ctrl Pts',(-18.3293850310261,-20.8247237146527,
124.463737195209)) ;
#106580 = CARTESIAN_POINT('Ctrl Pts',(-18.5275098785062,-20.834675884713,
124.634482989374)) ;
#106581 = CARTESIAN_POINT('Ctrl Pts',(-18.7517494695922,-20.8446143046275,
124.768339766333)) ;
#106582 = CARTESIAN_POINT('Ctrl Pts',(-18.9969080813788,-20.8545994347131,
124.861956432317)) ;
#106583 = CARTESIAN_POINT('Ctrl Pts',(-19.2559596960838,-20.8646361241272,
124.911446981312)) ;
#106584 = CARTESIAN_POINT('Ctrl Pts',(-19.5149214807583,-20.8744908081197,
124.915551065454)) ;
#106585 = CARTESIAN_POINT('Ctrl Pts',(-19.7744091532939,-20.8844902921675,
124.874396265208)) ;
#106586 = CARTESIAN_POINT('Ctrl Pts',(-20.0203900027022,-20.8943853809444,
124.789938115145)) ;
#106587 = CARTESIAN_POINT('Ctrl Pts',(-20.2516933373412,-20.9044459355906,
124.661962233862)) ;
#106588 = CARTESIAN_POINT('Ctrl Pts',(-20.4530789831576,-20.9142951999635,
124.499338199125)) ;
#106589 = CARTESIAN_POINT('Ctrl Pts',(-20.6267269098642,-20.9243224524113,
124.301150734394)) ;
#106590 = CARTESIAN_POINT('Ctrl Pts',(-20.7627565155963,-20.9343507499815,
124.075425085885)) ;
#106591 = CARTESIAN_POINT('Ctrl Pts',(-20.8562610600109,-20.9441968789875,
123.834176131167)) ;
#106592 = CARTESIAN_POINT('Ctrl Pts',(-20.9078567319107,-20.9541907843496,
123.576665766039)) ;
#106593 = CARTESIAN_POINT('Ctrl Pts',(-20.9135030485814,-20.9642148820326,
123.313296632163)) ;
#106594 = CARTESIAN_POINT('Ctrl Pts',(-20.8741952660944,-20.9741047098866,
123.056387254007)) ;
#106595 = CARTESIAN_POINT('Ctrl Pts',(-20.7903835125516,-20.9840966913171,
122.807554523007)) ;
#106596 = CARTESIAN_POINT('Ctrl Pts',(-20.6651455635319,-20.9940436960829,
122.57811162279)) ;
#106597 = CARTESIAN_POINT('Ctrl Pts',(-20.5022967865992,-21.0039933474727,
122.373537200791)) ;
#106598 = CARTESIAN_POINT('Ctrl Pts',(-20.3045524600773,-21.0140303504501,
122.198999390987)) ;
#106599 = CARTESIAN_POINT('Ctrl Pts',(-20.0829076432047,-21.0239192588851,
122.063311855875)) ;
#106600 = CARTESIAN_POINT('Ctrl Pts',(-19.8388031235912,-21.0339085913626,
121.966768231352)) ;
#106601 = CARTESIAN_POINT('Ctrl Pts',(-19.5823974992214,-21.0438671467997,
121.914430184052)) ;
#106602 = CARTESIAN_POINT('Ctrl Pts',(-19.3223423892364,-21.0537667180002,
121.906807082868)) ;
#106603 = CARTESIAN_POINT('Ctrl Pts',(-19.0611133552447,-21.0638146432522,
121.9451043463)) ;
#106604 = CARTESIAN_POINT('Ctrl Pts',(-18.8141787709719,-21.0737099427782,
122.026742494562)) ;
#106605 = CARTESIAN_POINT('Ctrl Pts',(-18.5813642148825,-21.0837717992262,
122.152027144941)) ;
#106606 = CARTESIAN_POINT('Ctrl Pts',(-18.3782691537802,-21.0936156456428,
122.312269335965)) ;
#106607 = CARTESIAN_POINT('Ctrl Pts',(-18.2033434375949,-21.1035785947709,
122.507056289126)) ;
#106608 = CARTESIAN_POINT('Ctrl Pts',(-18.0642661544428,-21.1136126311989,
122.731089182587)) ;
#106609 = CARTESIAN_POINT('Ctrl Pts',(-17.9673844345331,-21.1235000581569,
122.972179630959)) ;
#106610 = CARTESIAN_POINT('Ctrl Pts',(-17.9126540899515,-21.1335144924933,
123.229612712998)) ;
#106611 = CARTESIAN_POINT('Ctrl Pts',(-17.904097359486,-21.1435494371282,
123.49316382186)) ;
#106612 = CARTESIAN_POINT('Ctrl Pts',(-17.9399843509663,-21.1533817871592,
123.749075900176)) ;
#106613 = CARTESIAN_POINT('Ctrl Pts',(-18.0216348559207,-21.1634572262764,
124.000890325645)) ;
#106614 = CARTESIAN_POINT('Ctrl Pts',(-18.1429385335259,-21.173309691511,
124.229691572108)) ;
#106615 = CARTESIAN_POINT('Ctrl Pts',(-18.3054583562848,-21.1833825690879,
124.438574276318)) ;
#106616 = CARTESIAN_POINT('Ctrl Pts',(-18.497363701808,-21.1932251652804,
124.612025900992)) ;
#106617 = CARTESIAN_POINT('Ctrl Pts',(-18.7190400369266,-21.2032055493957,
124.752173819842)) ;
#106618 = CARTESIAN_POINT('Ctrl Pts',(-18.9628084773325,-21.2132240300445,
124.85161003546)) ;
#106619 = CARTESIAN_POINT('Ctrl Pts',(-19.2165871989397,-21.2231073450449,
124.907009598453)) ;
#106620 = CARTESIAN_POINT('Ctrl Pts',(-19.480916018816,-21.2331756421353,
124.917579442169)) ;
#106621 = CARTESIAN_POINT('Ctrl Pts',(-19.7369923043346,-21.2430057105076,
124.883224806794)) ;
#106622 = CARTESIAN_POINT('Ctrl Pts',(-19.9891518722698,-21.253072502976,
124.803386738475)) ;
#106623 = CARTESIAN_POINT('Ctrl Pts',(-20.2195154038845,-21.2629618364645,
124.682990140707)) ;
#106624 = CARTESIAN_POINT('Ctrl Pts',(-20.4280013834281,-21.2729639678806,
124.523000164599)) ;
#106625 = CARTESIAN_POINT('Ctrl Pts',(-20.6043386706282,-21.2828878375016,
124.330801370048)) ;
#106626 = CARTESIAN_POINT('Ctrl Pts',(-20.7462043849423,-21.2929313530188,
124.108284226744)) ;
#106627 = CARTESIAN_POINT('Ctrl Pts',(-20.8459679731605,-21.3028135659071,
123.868464248691)) ;
#106628 = CARTESIAN_POINT('Ctrl Pts',(-20.9036138188214,-21.3128816431265,
123.610292216186)) ;
#106629 = CARTESIAN_POINT('Ctrl Pts',(-20.9155213503014,-21.3227201478607,
123.35197747628)) ;
#106630 = CARTESIAN_POINT('Ctrl Pts',(-20.882022828367,-21.3327829162901,
123.089701598877)) ;
#106631 = CARTESIAN_POINT('Ctrl Pts',(-20.8045024152321,-21.3426799095728,
122.841423981398)) ;
#106632 = CARTESIAN_POINT('Ctrl Pts',(-20.6854221679011,-21.3526111372076,
122.609199073492)) ;
#106633 = CARTESIAN_POINT('Ctrl Pts',(-20.5258361470351,-21.3626532958498,
122.399026647855)) ;
#106634 = CARTESIAN_POINT('Ctrl Pts',(-20.335295369946,-21.3725400053808,
122.222383437198)) ;
#106635 = CARTESIAN_POINT('Ctrl Pts',(-20.1148920105634,-21.3825329778094,
122.079633715009)) ;
#106636 = CARTESIAN_POINT('Ctrl Pts',(-19.874132060502,-21.392479172346,121.977899698688)) ;
#106637 = CARTESIAN_POINT('Ctrl Pts',(-19.619487828393,-21.4024245471975,
121.918954900384)) ;
#106638 = CARTESIAN_POINT('Ctrl Pts',(-19.355633681364,-21.4124794665574,
121.90537882635)) ;
#106639 = CARTESIAN_POINT('Ctrl Pts',(-19.0993925483528,-21.4223009860009,
121.936586065926)) ;
#106640 = CARTESIAN_POINT('Ctrl Pts',(-18.8463064545216,-21.4323667547678,
122.013350173819)) ;
#106641 = CARTESIAN_POINT('Ctrl Pts',(-18.6141903792283,-21.4422686764229,
122.131067840634)) ;
#106642 = CARTESIAN_POINT('Ctrl Pts',(-18.4029908552068,-21.4523117352439,
122.289297152131)) ;
#106643 = CARTESIAN_POINT('Ctrl Pts',(-18.2250163310526,-21.4622177292866,
122.479284295807)) ;
#106644 = CARTESIAN_POINT('Ctrl Pts',(-18.0816390507141,-21.4721555023684,
122.697559547165)) ;
#106645 = CARTESIAN_POINT('Ctrl Pts',(-17.9775347354648,-21.4821958661007,
122.93999855582)) ;
#106646 = CARTESIAN_POINT('Ctrl Pts',(-17.9178327043181,-21.4920832098242,
123.192889506299)) ;
#106647 = CARTESIAN_POINT('Ctrl Pts',(-17.9023592109416,-21.5020754403929,
123.455000740661)) ;
#106648 = CARTESIAN_POINT('Ctrl Pts',(-17.932574065848,-21.5120239681765,
123.714700805199)) ;
#106649 = CARTESIAN_POINT('Ctrl Pts',(-18.0069709592114,-21.5219607518998,
123.96498403759)) ;
#106650 = CARTESIAN_POINT('Ctrl Pts',(-18.1239652382464,-21.5319437526968,
124.19983233919)) ;
#106651 = CARTESIAN_POINT('Ctrl Pts',(-18.2812638755479,-21.5419876395375,
124.411744040751)) ;
#106652 = CARTESIAN_POINT('Ctrl Pts',(-18.4684771481932,-21.5518156631121,
124.589722525419)) ;
#106653 = CARTESIAN_POINT('Ctrl Pts',(-18.6890622519546,-21.5618929113257,
124.736146499577)) ;
#106654 = CARTESIAN_POINT('Ctrl Pts',(-18.9262831897705,-21.571742466631,
124.839866711791)) ;
#106655 = CARTESIAN_POINT('Ctrl Pts',(-19.1837109370141,-21.5818251748287,
124.902321257173)) ;
#106656 = CARTESIAN_POINT('Ctrl Pts',(-19.4410990137253,-21.5916377677552,
124.918921324758)) ;
#106657 = CARTESIAN_POINT('Ctrl Pts',(-19.7040389778254,-21.6017049600131,
124.890283048856)) ;
#106658 = CARTESIAN_POINT('Ctrl Pts',(-19.9538585647511,-21.6116037894757,
124.817532450528)) ;
#106659 = CARTESIAN_POINT('Ctrl Pts',(-20.190850254731,-21.6216577806659,
124.70086379783)) ;
#106660 = CARTESIAN_POINT('Ctrl Pts',(-20.4003453171427,-21.6315295054491,
124.547768619076)) ;
#106661 = CARTESIAN_POINT('Ctrl Pts',(-20.5836703121045,-21.6415999475793,
124.356973135958)) ;
#106662 = CARTESIAN_POINT('Ctrl Pts',(-20.7277436846726,-21.6514330260096,
124.142431575118)) ;
#106663 = CARTESIAN_POINT('Ctrl Pts',(-20.8351504550266,-21.661463499511,
123.90172744066)) ;
#106664 = CARTESIAN_POINT('Ctrl Pts',(-20.8983991892578,-21.6714950988097,
123.64579221545)) ;
#106665 = CARTESIAN_POINT('Ctrl Pts',(-20.9164245493496,-21.6813247998478,
123.38812458234)) ;
#106666 = CARTESIAN_POINT('Ctrl Pts',(-20.8897753449529,-21.6913142379043,
123.126960779477)) ;
#106667 = CARTESIAN_POINT('Ctrl Pts',(-20.8171517828939,-21.7013581411204,
122.873208967766)) ;
#106668 = CARTESIAN_POINT('Ctrl Pts',(-20.7046129996104,-21.7111796619339,
122.640934622164)) ;
#106669 = CARTESIAN_POINT('Ctrl Pts',(-20.5506729712625,-21.721215386181,
122.426803905934)) ;
#106670 = CARTESIAN_POINT('Ctrl Pts',(-20.3616525439628,-21.7312375401135,
122.243374779076)) ;
#106671 = CARTESIAN_POINT('Ctrl Pts',(-20.1474024551261,-21.7410997718708,
122.097582456974)) ;
#106672 = CARTESIAN_POINT('Ctrl Pts',(-19.9090500324287,-21.7510588423287,
121.989478779301)) ;
#106673 = CARTESIAN_POINT('Ctrl Pts',(-19.6535274553849,-21.7610940147049,
121.924306461596)) ;
#106674 = CARTESIAN_POINT('Ctrl Pts',(-19.3946169510934,-21.7709743998631,
121.904405437011)) ;
#106675 = CARTESIAN_POINT('Ctrl Pts',(-19.1316158970856,-21.7810311144571,
121.930107076783)) ;
#106676 = CARTESIAN_POINT('Ctrl Pts',(-18.881530454905,-21.7909103830291,
121.999860465545)) ;
#106677 = CARTESIAN_POINT('Ctrl Pts',(-18.6444162627727,-21.8009013405148,
122.112601623347)) ;
#106678 = CARTESIAN_POINT('Ctrl Pts',(-18.4297519054492,-21.81094199915,122.266033649848)) ;
#106679 = CARTESIAN_POINT('Ctrl Pts',(-18.2485066413197,-21.820774978858,
122.450203319049)) ;
#106680 = CARTESIAN_POINT('Ctrl Pts',(-18.0989867796727,-21.8307681121077,
122.666085929148)) ;
#106681 = CARTESIAN_POINT('Ctrl Pts',(-17.9892868503184,-21.8408001644911,
122.905823378761)) ;
#106682 = CARTESIAN_POINT('Ctrl Pts',(-17.9236804014323,-21.8506653934424,
123.156619439682)) ;
#106683 = CARTESIAN_POINT('Ctrl Pts',(-17.9016709296065,-21.8606273346856,
123.417488992324)) ;
#106684 = CARTESIAN_POINT('Ctrl Pts',(-17.9258855366859,-21.8706620497224,
123.680064384478)) ;
#106685 = CARTESIAN_POINT('Ctrl Pts',(-17.9939001600136,-21.8805478200664,
123.930823539983)) ;
#106686 = CARTESIAN_POINT('Ctrl Pts',(-18.1063745150095,-21.8906104174552,
124.170110652052)) ;
#106687 = CARTESIAN_POINT('Ctrl Pts',(-18.2554119033243,-21.9004608292904,
124.381785675874)) ;
#106688 = CARTESIAN_POINT('Ctrl Pts',(-18.4417337007626,-21.9104879985763,
124.568103740414)) ;
#106689 = CARTESIAN_POINT('Ctrl Pts',(-18.6579939619435,-21.9205154792905,
124.718691412592)) ;
#106690 = CARTESIAN_POINT('Ctrl Pts',(-18.8924886711707,-21.9303585318698,
124.827847491686)) ;
#106691 = CARTESIAN_POINT('Ctrl Pts',(-19.1460388774625,-21.9403524353084,
124.89630229536)) ;
#106692 = CARTESIAN_POINT('Ctrl Pts',(-19.4085429207099,-21.9503795580848,
124.919288369219)) ;
#106693 = CARTESIAN_POINT('Ctrl Pts',(-19.6675055964963,-21.9602702629769,
124.896983045597)) ;
#106694 = CARTESIAN_POINT('Ctrl Pts',(-19.9213201022087,-21.9702622898272,
124.829737172689)) ;
#106695 = CARTESIAN_POINT('Ctrl Pts',(-20.15847886615,-21.9802082713157,124.719877290548)) ;
#106696 = CARTESIAN_POINT('Ctrl Pts',(-20.3732998849386,-21.9901554439376,
124.5709137519)) ;
#106697 = CARTESIAN_POINT('Ctrl Pts',(-20.5606494682345,-22.0002033852638,
124.384856178844)) ;
#106698 = CARTESIAN_POINT('Ctrl Pts',(-20.7099988055723,-22.0100510190716,
124.173512790482)) ;
#106699 = CARTESIAN_POINT('Ctrl Pts',(-20.8223974749045,-22.0200127337566,
123.937100416277)) ;
#106700 = CARTESIAN_POINT('Ctrl Pts',(-20.8921927790865,-22.0300413666351,
123.68295199388)) ;
#106701 = CARTESIAN_POINT('Ctrl Pts',(-20.9165923031643,-22.0399516921703,
123.423675234886)) ;
#106702 = CARTESIAN_POINT('Ctrl Pts',(-20.8962261425128,-22.049886522642,
123.16338835777)) ;
#106703 = CARTESIAN_POINT('Ctrl Pts',(-20.8300596435393,-22.059927855024,
122.907943513216)) ;
#106704 = CARTESIAN_POINT('Ctrl Pts',(-20.7222498519845,-22.0698207284628,
122.671379324634)) ;
#106705 = CARTESIAN_POINT('Ctrl Pts',(-20.5744090303829,-22.0797898942807,
122.455088308952)) ;
#106706 = CARTESIAN_POINT('Ctrl Pts',(-20.3898730535669,-22.0898186279972,
122.266962233165)) ;
#106707 = CARTESIAN_POINT('Ctrl Pts',(-20.1081955733599,-22.1030111467684,
122.064734080855)) ;
#106708 = CARTESIAN_POINT('Ctrl Pts',(-19.7762060672709,-22.1163710148111,
121.939114499556)) ;
#106709 = CARTESIAN_POINT('Ctrl Pts',(-19.4303000677635,-22.1295963519599,
121.904601540361)) ;
#106710 = CARTESIAN_POINT('Ctrl Pts',(-19.1686956935908,-22.1395775778005,
121.92351886695)) ;
#106711 = CARTESIAN_POINT('Ctrl Pts',(-18.9130905640444,-22.1496131447834,
121.988419973829)) ;
#106712 = CARTESIAN_POINT('Ctrl Pts',(-18.6765215819154,-22.1594762227455,
122.094390069791)) ;
#106713 = CARTESIAN_POINT('Ctrl Pts',(-18.4574524440077,-22.1695465215466,
122.242803036002)) ;
#106714 = CARTESIAN_POINT('Ctrl Pts',(-18.2717635384097,-22.1793888201144,
122.422867545221)) ;
#106715 = CARTESIAN_POINT('Ctrl Pts',(-18.1175643025741,-22.1893495182842,
122.634377147575)) ;
#106716 = CARTESIAN_POINT('Ctrl Pts',(-18.0020115450616,-22.1993875524637,
122.871500055284)) ;
#106717 = CARTESIAN_POINT('Ctrl Pts',(-17.930094357224,-22.2092612893102,
123.120841153412)) ;
#106718 = CARTESIAN_POINT('Ctrl Pts',(-17.9020504852517,-22.2193330732354,
123.383989693628)) ;
#106719 = CARTESIAN_POINT('Ctrl Pts',(-17.919540669824,-22.2291651944366,
123.64179986069)) ;
#106720 = CARTESIAN_POINT('Ctrl Pts',(-17.9820987955185,-22.239198218462,
123.897915110287)) ;
#106721 = CARTESIAN_POINT('Ctrl Pts',(-18.0886241992968,-22.2492140986587,
124.138620611349)) ;
#106722 = CARTESIAN_POINT('Ctrl Pts',(-18.2329762887134,-22.2590976177529,
124.354539801381)) ;
#106723 = CARTESIAN_POINT('Ctrl Pts',(-18.4143130469841,-22.2690880301166,
124.544365461022)) ;
#106724 = CARTESIAN_POINT('Ctrl Pts',(-18.6951226688525,-22.28235119332,124.750870336267)) ;
#106725 = CARTESIAN_POINT('Ctrl Pts',(-19.0235872633062,-22.2956287635712,
124.879796807948)) ;
#106726 = CARTESIAN_POINT('Ctrl Pts',(-19.3717516624237,-22.3089590660778,
124.918805307772)) ;
#106727 = CARTESIAN_POINT('Ctrl Pts',(-19.6313839899899,-22.3188577478942,
124.902827623068)) ;
#106728 = CARTESIAN_POINT('Ctrl Pts',(-19.8866875692019,-22.3288472629417,
124.841760132005)) ;
#106729 = CARTESIAN_POINT('Ctrl Pts',(-20.1265240138423,-22.3387953147168,
124.73770586558)) ;
#106730 = CARTESIAN_POINT('Ctrl Pts',(-20.3446612835695,-22.3487367179953,
124.593976175479)) ;
#106731 = CARTESIAN_POINT('Ctrl Pts',(-20.5987501854537,-22.3620233827762,
124.354444327464)) ;
#106732 = CARTESIAN_POINT('Ctrl Pts',(-20.8307578098562,-22.378633804431,
123.978886976682)) ;
#106733 = CARTESIAN_POINT('Ctrl Pts',(-20.9389570638948,-22.3985450666818,
123.460837785839)) ;
#106734 = CARTESIAN_POINT('Ctrl Pts',(-20.8639559060425,-22.4184891958467,
122.936059319112)) ;
#106735 = CARTESIAN_POINT('Ctrl Pts',(-20.6146168497049,-22.4384123584518,
122.46896784405)) ;
#106736 = CARTESIAN_POINT('Ctrl Pts',(-20.2219980709567,-22.4583024808584,
122.114843596429)) ;
#106737 = CARTESIAN_POINT('Ctrl Pts',(-19.7292742311084,-22.4783074344585,
121.91524683107)) ;
#106738 = CARTESIAN_POINT('Ctrl Pts',(-19.2022755216154,-22.4981456914741,
121.895507427705)) ;
#106739 = CARTESIAN_POINT('Ctrl Pts',(-18.6962165202482,-22.5181399922607,
122.057490332449)) ;
#106740 = CARTESIAN_POINT('Ctrl Pts',(-18.278334233107,-22.5380252343051,
122.381092030376)) ;
#106741 = CARTESIAN_POINT('Ctrl Pts',(-17.9948603071649,-22.557900180781,
122.826830133635)) ;
#106742 = CARTESIAN_POINT('Ctrl Pts',(-17.8799975526661,-22.5779332507221,
123.3467920993)) ;
#106743 = CARTESIAN_POINT('Ctrl Pts',(-17.9496067756864,-22.5978217576225,
123.870746392189)) ;
#106744 = CARTESIAN_POINT('Ctrl Pts',(-18.1918518597554,-22.6176766174038,
124.339658601302)) ;
#106745 = CARTESIAN_POINT('Ctrl Pts',(-18.5838377446727,-22.6377274511915,
124.700512523635)) ;
#106746 = CARTESIAN_POINT('Ctrl Pts',(-19.0684699146769,-22.6574933930808,
124.903664781384)) ;
#106747 = CARTESIAN_POINT('Ctrl Pts',(-19.5995371461108,-22.6775061245401,
124.930607581671)) ;
#106748 = CARTESIAN_POINT('Ctrl Pts',(-20.1049471997775,-22.6973989594837,
124.774872824804)) ;
#106749 = CARTESIAN_POINT('Ctrl Pts',(-20.5274891334614,-22.7173059828232,
124.456654840816)) ;
#106750 = CARTESIAN_POINT('Ctrl Pts',(-20.8168362162769,-22.7372212477239,
124.013275946578)) ;
#106751 = CARTESIAN_POINT('Ctrl Pts',(-20.9375204682775,-22.7572529398836,
123.49476876115)) ;
#106752 = CARTESIAN_POINT('Ctrl Pts',(-20.8746410235034,-22.7770959864566,
122.971080233954)) ;
#106753 = CARTESIAN_POINT('Ctrl Pts',(-20.6370945925623,-22.7970125343564,
122.498111517226)) ;
#106754 = CARTESIAN_POINT('Ctrl Pts',(-20.2519505607722,-22.8169447773477,
122.134290696217)) ;
#106755 = CARTESIAN_POINT('Ctrl Pts',(-19.7666480927103,-22.836848612157,
121.923807479693)) ;
#106756 = CARTESIAN_POINT('Ctrl Pts',(-19.2387574124756,-22.8567490123445,
121.890907261899)) ;
#106757 = CARTESIAN_POINT('Ctrl Pts',(-18.7299851185306,-22.8766986887238,
122.040287415327)) ;
#106758 = CARTESIAN_POINT('Ctrl Pts',(-18.303172348133,-22.8966312129442,
122.354132363191)) ;
#106759 = CARTESIAN_POINT('Ctrl Pts',(-18.0088689587993,-22.9165512219304,
122.794285149037)) ;
#106760 = CARTESIAN_POINT('Ctrl Pts',(-17.8822993686623,-22.9365081281066,
123.309329742268)) ;
#106761 = CARTESIAN_POINT('Ctrl Pts',(-17.9384199625223,-22.9563939676081,
123.834975464313)) ;
#106762 = CARTESIAN_POINT('Ctrl Pts',(-18.1715050238201,-22.9763651397439,
124.311731312162)) ;
#106763 = CARTESIAN_POINT('Ctrl Pts',(-18.5499250225676,-22.9961793367283,
124.678096641438)) ;
#106764 = CARTESIAN_POINT('Ctrl Pts',(-19.0342409000383,-23.0161605226965,
124.895731433432)) ;
#106765 = CARTESIAN_POINT('Ctrl Pts',(-19.4736675616231,-23.0327360280858,
124.92808622069)) ;
#106766 = CARTESIAN_POINT('Ctrl Pts',(-19.8173439997547,-23.0460454759494,
124.863128979143)) ;
#106767 = CARTESIAN_POINT('Ctrl Pts',(-20.1458789841394,-23.059413173726,
124.738730813159)) ;
#106768 = CARTESIAN_POINT('Ctrl Pts',(-20.5018784820625,-23.0759037453919,
124.483077299164)) ;
#106769 = CARTESIAN_POINT('Ctrl Pts',(-20.8018393980275,-23.0958240177247,
124.046891204842)) ;
#106770 = CARTESIAN_POINT('Ctrl Pts',(-20.9126929215767,-23.1124410534457,
123.619343331214)) ;
#106771 = CARTESIAN_POINT('Ctrl Pts',(-20.9100857742586,-23.1257319037268,
123.27005760007)) ;
#106772 = CARTESIAN_POINT('Ctrl Pts',(-20.8627965255506,-23.1357009488813,
123.012413426442)) ;
#106773 = CARTESIAN_POINT('Ctrl Pts',(-20.7725539965667,-23.1456043395148,
122.768277127113)) ;
#106774 = CARTESIAN_POINT('Ctrl Pts',(-20.6391518971756,-23.1556621256276,
122.540138510924)) ;
#106775 = CARTESIAN_POINT('Ctrl Pts',(-20.4718019191149,-23.1655141622773,
122.342561323928)) ;
#106776 = CARTESIAN_POINT('Ctrl Pts',(-20.2020922063009,-23.1788792864205,
122.117601499153)) ;
#106777 = CARTESIAN_POINT('Ctrl Pts',(-19.8829803021328,-23.1921053493835,
121.970099825569)) ;
#106778 = CARTESIAN_POINT('Ctrl Pts',(-19.5386223026728,-23.2054089976658,
121.909883631359)) ;
#106779 = CARTESIAN_POINT('Ctrl Pts',(-19.2760224027654,-23.2154005288288,
121.910123653144)) ;
#106780 = CARTESIAN_POINT('Ctrl Pts',(-19.0163263874921,-23.2254399766281,
121.95651707498)) ;
#106781 = CARTESIAN_POINT('Ctrl Pts',(-18.7732899517778,-23.235283752142,
122.04517614713)) ;
#106782 = CARTESIAN_POINT('Ctrl Pts',(-18.5459000575662,-23.2452693935296,
122.176069505843)) ;
#106783 = CARTESIAN_POINT('Ctrl Pts',(-18.3455214781361,-23.2552061778914,
122.343576105247)) ;
#106784 = CARTESIAN_POINT('Ctrl Pts',(-18.1755060502448,-23.2652560123588,
122.545638346613)) ;
#106785 = CARTESIAN_POINT('Ctrl Pts',(-18.0455914330322,-23.2751064618619,
122.769558622391)) ;
#106786 = CARTESIAN_POINT('Ctrl Pts',(-17.9548073715586,-23.285078475844,
123.015349644938)) ;
#106787 = CARTESIAN_POINT('Ctrl Pts',(-17.907992236839,-23.2950736336911,
123.273849064806)) ;
#106788 = CARTESIAN_POINT('Ctrl Pts',(-17.9070860096866,-23.3051075600548,
123.53750621489)) ;
#106789 = CARTESIAN_POINT('Ctrl Pts',(-17.9507850137086,-23.3149632684872,
123.792814747735)) ;
#106790 = CARTESIAN_POINT('Ctrl Pts',(-18.0390356386596,-23.3249614178259,
124.040247090644)) ;
#106791 = CARTESIAN_POINT('Ctrl Pts',(-18.1674616556729,-23.3348608209994,
124.266527021118)) ;
#106792 = CARTESIAN_POINT('Ctrl Pts',(-18.3356817078808,-23.3449120178879,
124.47013072449)) ;
#106793 = CARTESIAN_POINT('Ctrl Pts',(-18.5333323575625,-23.3547943417008,
124.638615226352)) ;
#106794 = CARTESIAN_POINT('Ctrl Pts',(-18.7594616396992,-23.3647892373574,
124.772216137486)) ;
#106795 = CARTESIAN_POINT('Ctrl Pts',(-19.0061533314025,-23.3748103367399,
124.864411761759)) ;
#106796 = CARTESIAN_POINT('Ctrl Pts',(-19.2621116257065,-23.384717604602,
124.912027971084)) ;
#106797 = CARTESIAN_POINT('Ctrl Pts',(-19.5232470996749,-23.3946559484272,
124.915009816685)) ;
#106798 = CARTESIAN_POINT('Ctrl Pts',(-19.7826933987112,-23.4046593677277,
124.8724829918)) ;
#106799 = CARTESIAN_POINT('Ctrl Pts',(-20.0314009904622,-23.4146939184348,
124.784885032941)) ;
#106800 = CARTESIAN_POINT('Ctrl Pts',(-20.2570231739514,-23.4245388680404,
124.658249413978)) ;
#106801 = CARTESIAN_POINT('Ctrl Pts',(-20.4603618570071,-23.4345247101533,
124.492434927379)) ;
#106802 = CARTESIAN_POINT('Ctrl Pts',(-20.6311448680161,-23.4444595175224,
124.294901691016)) ;
#106803 = CARTESIAN_POINT('Ctrl Pts',(-20.7664417655646,-23.4545170592357,
124.067899599179)) ;
#106804 = CARTESIAN_POINT('Ctrl Pts',(-20.8584621327028,-23.4643386567478,
123.826728474679)) ;
#106805 = CARTESIAN_POINT('Ctrl Pts',(-20.9088445357203,-23.4743949162283,
123.567330995986)) ;
#106806 = CARTESIAN_POINT('Ctrl Pts',(-20.9129110800189,-23.4843348525287,
123.30613725382)) ;
#106807 = CARTESIAN_POINT('Ctrl Pts',(-20.8724772004398,-23.4942419732731,
123.048950368419)) ;
#106808 = CARTESIAN_POINT('Ctrl Pts',(-20.7867527465454,-23.5042848791984,
122.79935041922)) ;
#106809 = CARTESIAN_POINT('Ctrl Pts',(-20.6607477389128,-23.5141926602976,
122.57149371911)) ;
#106810 = CARTESIAN_POINT('Ctrl Pts',(-20.4957599634145,-23.5242030293,122.366590895835)) ;
#106811 = CARTESIAN_POINT('Ctrl Pts',(-20.2969506390713,-23.5342338678688,
122.193505240342)) ;
#106812 = CARTESIAN_POINT('Ctrl Pts',(-20.0753486418912,-23.5440867075085,
122.059578658416)) ;
#106813 = CARTESIAN_POINT('Ctrl Pts',(-19.8307446270475,-23.5540747086735,
121.964443905923)) ;
#106814 = CARTESIAN_POINT('Ctrl Pts',(-19.5748366256193,-23.5640035276526,
121.913518355391)) ;
#106815 = CARTESIAN_POINT('Ctrl Pts',(-19.3124297420902,-23.5739912303749,
121.907324493557)) ;
#106816 = CARTESIAN_POINT('Ctrl Pts',(-19.051770374588,-23.5840272301776,
121.947412427544)) ;
#106817 = CARTESIAN_POINT('Ctrl Pts',(-18.8063695565642,-23.593882099979,
122.03022500665)) ;
#106818 = CARTESIAN_POINT('Ctrl Pts',(-18.5756276914687,-23.6038815304026,
122.155865182355)) ;
#106819 = CARTESIAN_POINT('Ctrl Pts',(-18.3721072360953,-23.6137766478679,
122.317789039165)) ;
#106820 = CARTESIAN_POINT('Ctrl Pts',(-18.1969845029216,-23.6238371413848,
122.515805626587)) ;
#106821 = CARTESIAN_POINT('Ctrl Pts',(-18.0616521827604,-23.633686621586,
122.736464033145)) ;
#106822 = CARTESIAN_POINT('Ctrl Pts',(-17.96435863761,-23.6437130718498,122.981324009064)) ;
#106823 = CARTESIAN_POINT('Ctrl Pts',(-17.911742767229,-23.6537443623279,
123.239637252324)) ;
#106824 = CARTESIAN_POINT('Ctrl Pts',(-17.9043471354414,-23.6635857499797,
123.498155439338)) ;
#106825 = CARTESIAN_POINT('Ctrl Pts',(-17.9420608558698,-23.6735891508709,
123.758288393209)) ;
#106826 = CARTESIAN_POINT('Ctrl Pts',(-18.0243389591208,-23.6835735336621,
124.007481577347)) ;
#106827 = CARTESIAN_POINT('Ctrl Pts',(-18.1495030874067,-23.6936126236755,
124.23968716237)) ;
#106828 = CARTESIAN_POINT('Ctrl Pts',(-18.3096790121242,-23.7034584325847,
124.442908496677)) ;
#106829 = CARTESIAN_POINT('Ctrl Pts',(-18.5050267463786,-23.7134428554037,
124.618016503644)) ;
#106830 = CARTESIAN_POINT('Ctrl Pts',(-18.7268162305276,-23.7233824806449,
124.756058797154)) ;
#106831 = CARTESIAN_POINT('Ctrl Pts',(-18.9716149595931,-23.7334221701635,
124.854395810098)) ;
#106832 = CARTESIAN_POINT('Ctrl Pts',(-19.2258825394097,-23.7433103585821,
124.908048605825)) ;
#106833 = CARTESIAN_POINT('Ctrl Pts',(-19.4882244846222,-23.7532998845842,
124.917317622935)) ;
#106834 = CARTESIAN_POINT('Ctrl Pts',(-19.7473573898782,-23.7632583859393,
124.880808259512)) ;
#106835 = CARTESIAN_POINT('Ctrl Pts',(-19.9949628231632,-23.773157979943,
124.800942972097)) ;
#106836 = CARTESIAN_POINT('Ctrl Pts',(-20.2283026313404,-23.7832058680643,
124.677413983082)) ;
#106837 = CARTESIAN_POINT('Ctrl Pts',(-20.4336672103924,-23.7931012933098,
124.517825438712)) ;
#106838 = CARTESIAN_POINT('Ctrl Pts',(-20.6111084539714,-23.8031626840104,
124.321848670484)) ;
#106839 = CARTESIAN_POINT('Ctrl Pts',(-20.7488728942098,-23.8130082676971,
124.102826518574)) ;
#106840 = CARTESIAN_POINT('Ctrl Pts',(-20.8484840700568,-23.8229712410063,
123.860719317866)) ;
#106841 = CARTESIAN_POINT('Ctrl Pts',(-20.9045623846143,-23.8329969078321,
123.603275789807)) ;
#106842 = CARTESIAN_POINT('Ctrl Pts',(-20.9151111856894,-23.8429113856984,
123.342955717089)) ;
#106843 = CARTESIAN_POINT('Ctrl Pts',(-20.8805541691615,-23.8528999003734,
123.082731176444)) ;
#106844 = CARTESIAN_POINT('Ctrl Pts',(-20.8003735896472,-23.8629440112888,
122.831281031369)) ;
#106845 = CARTESIAN_POINT('Ctrl Pts',(-20.6809155331496,-23.8727721488834,
122.602251951149)) ;
#106846 = CARTESIAN_POINT('Ctrl Pts',(-20.5196793173917,-23.8828487169423,
122.392265985957)) ;
#106847 = CARTESIAN_POINT('Ctrl Pts',(-20.3287876662329,-23.8927008788465,
122.217275425299)) ;
#106848 = CARTESIAN_POINT('Ctrl Pts',(-20.1057229104058,-23.9027738408033,
122.07484100649)) ;
#106849 = CARTESIAN_POINT('Ctrl Pts',(-19.8668284491858,-23.9126164028062,
121.975632340931)) ;
#106850 = CARTESIAN_POINT('Ctrl Pts',(-19.6110271194591,-23.9225968393,121.917772023658)) ;
#106851 = CARTESIAN_POINT('Ctrl Pts',(-19.348039156227,-23.9326151446244,
121.905665438189)) ;
#106852 = CARTESIAN_POINT('Ctrl Pts',(-19.0903457175799,-23.9424991085438,
121.938422956603)) ;
#106853 = CARTESIAN_POINT('Ctrl Pts',(-18.8377656583219,-23.9525649852824,
122.016891898931)) ;
#106854 = CARTESIAN_POINT('Ctrl Pts',(-18.6078170760635,-23.9624040861433,
122.135169084714)) ;
#106855 = CARTESIAN_POINT('Ctrl Pts',(-18.3974656836165,-23.972437169009,
122.294107786328)) ;
#106856 = CARTESIAN_POINT('Ctrl Pts',(-18.2185683792125,-23.9824588542845,
122.487406407635)) ;
#106857 = CARTESIAN_POINT('Ctrl Pts',(-18.0778267832511,-23.992325549383,
122.705148566182)) ;
#106858 = CARTESIAN_POINT('Ctrl Pts',(-17.9754281452733,-24.0022854391175,
122.946034450272)) ;
#106859 = CARTESIAN_POINT('Ctrl Pts',(-17.9163664020501,-24.012320426943,
123.203027128536)) ;
#106860 = CARTESIAN_POINT('Ctrl Pts',(-17.9025895953296,-24.0222071310173,
123.462511054197)) ;
#106861 = CARTESIAN_POINT('Ctrl Pts',(-17.9347016359298,-24.0322722752502,
123.725012586656)) ;
#106862 = CARTESIAN_POINT('Ctrl Pts',(-18.0099434070378,-24.0421115659788,
123.972431513364)) ;
#106863 = CARTESIAN_POINT('Ctrl Pts',(-18.1293026069265,-24.0521741234172,
124.208359310973)) ;
#106864 = CARTESIAN_POINT('Ctrl Pts',(-18.2854573227797,-24.0620711746693,
124.416367480328)) ;
#106865 = CARTESIAN_POINT('Ctrl Pts',(-18.4754012568581,-24.0720023814176,
124.595335878726)) ;
#106866 = CARTESIAN_POINT('Ctrl Pts',(-18.6961331689866,-24.0820445656364,
124.739965453088)) ;
#106867 = CARTESIAN_POINT('Ctrl Pts',(-18.9348086365225,-24.0919311937473,
124.842639747619)) ;
#106868 = CARTESIAN_POINT('Ctrl Pts',(-19.1902871963049,-24.1019244662797,
124.903374527269)) ;
#106869 = CARTESIAN_POINT('Ctrl Pts',(-19.4511873709055,-24.1118695418212,
124.918665438026)) ;
#106870 = CARTESIAN_POINT('Ctrl Pts',(-19.710965208711,-24.1218190925494,
124.888914128674)) ;
#106871 = CARTESIAN_POINT('Ctrl Pts',(-19.9637977980599,-24.1318584273974,
124.813604045651)) ;
#106872 = CARTESIAN_POINT('Ctrl Pts',(-20.1962508109109,-24.1417445663413,
124.697537862331)) ;
#106873 = CARTESIAN_POINT('Ctrl Pts',(-20.4075413438775,-24.151742679315,
124.541421995671)) ;
#106874 = CARTESIAN_POINT('Ctrl Pts',(-20.5872538313161,-24.1616624416675,
124.352546831275)) ;
#106875 = CARTESIAN_POINT('Ctrl Pts',(-20.7332244854721,-24.1717018372801,
124.132799237148)) ;
#106876 = CARTESIAN_POINT('Ctrl Pts',(-20.8373860226975,-24.1816110230684,
123.894133566146)) ;
#106877 = CARTESIAN_POINT('Ctrl Pts',(-20.8993974610776,-24.1915462072259,
123.640515964323)) ;
#106878 = CARTESIAN_POINT('Ctrl Pts',(-20.9163526621693,-24.2015872646118,
123.377199581861)) ;
#106879 = CARTESIAN_POINT('Ctrl Pts',(-20.8879577850495,-24.2114744226451,
123.118917113448)) ;
#106880 = CARTESIAN_POINT('Ctrl Pts',(-20.8148023044872,-24.221466702321,
122.866745567144)) ;
#106881 = CARTESIAN_POINT('Ctrl Pts',(-20.6994003311654,-24.2314152193661,
122.632140907791)) ;
#106882 = CARTESIAN_POINT('Ctrl Pts',(-20.5455176565627,-24.2413519969365,
122.421198517231)) ;
#106883 = CARTESIAN_POINT('Ctrl Pts',(-20.3566602491827,-24.2513350330834,
122.239059803708)) ;
#106884 = CARTESIAN_POINT('Ctrl Pts',(-20.1375054315778,-24.2613787846771,
122.092024451961)) ;
#106885 = CARTESIAN_POINT('Ctrl Pts',(-19.9015041198329,-24.2712073138897,
121.986982801871)) ;
#106886 = CARTESIAN_POINT('Ctrl Pts',(-19.6446783076409,-24.2812826747984,
121.922828883931)) ;
#106887 = CARTESIAN_POINT('Ctrl Pts',(-19.3862469986077,-24.2911392736856,
121.904547729095)) ;
#106888 = CARTESIAN_POINT('Ctrl Pts',(-19.1232503151631,-24.3012022677035,
121.931694916148)) ;
#106889 = CARTESIAN_POINT('Ctrl Pts',(-18.8735504660237,-24.311080201993,
122.002807613392)) ;
#106890 = CARTESIAN_POINT('Ctrl Pts',(-18.6369978578341,-24.321080849551,
122.117198755573)) ;
#106891 = CARTESIAN_POINT('Ctrl Pts',(-18.4254739722375,-24.3309986959891,
122.269548153979)) ;
#106892 = CARTESIAN_POINT('Ctrl Pts',(-18.2412881647919,-24.3410498129947,
122.458807705072)) ;
#106893 = CARTESIAN_POINT('Ctrl Pts',(-18.0951342855222,-24.3509205483053,
122.673164916615)) ;
#106894 = CARTESIAN_POINT('Ctrl Pts',(-17.9862472480919,-24.3609912555483,
122.91432710992)) ;
#106895 = CARTESIAN_POINT('Ctrl Pts',(-17.922299610322,-24.3708242630002,
123.164716216814)) ;
#106896 = CARTESIAN_POINT('Ctrl Pts',(-17.9016599057692,-24.3808547553025,
123.427488017808)) ;
#106897 = CARTESIAN_POINT('Ctrl Pts',(-17.927729522015,-24.3908863503759,
123.689830426704)) ;
#106898 = CARTESIAN_POINT('Ctrl Pts',(-17.9969934501606,-24.4007160495141,
123.938667781932)) ;
#106899 = CARTESIAN_POINT('Ctrl Pts',(-18.1095255107703,-24.4107054993957,
124.175845661491)) ;
#106900 = CARTESIAN_POINT('Ctrl Pts',(-18.2628973236103,-24.4207493572114,
124.390649715885)) ;
#106901 = CARTESIAN_POINT('Ctrl Pts',(-18.446698072111,-24.4305710478016,
124.571855631295)) ;
#106902 = CARTESIAN_POINT('Ctrl Pts',(-18.6634180756333,-24.440606138342,
124.722101523937)) ;
#106903 = CARTESIAN_POINT('Ctrl Pts',(-18.9029943040956,-24.4506306573247,
124.831691995518)) ;
#106904 = CARTESIAN_POINT('Ctrl Pts',(-19.1536255156033,-24.4604905027349,
124.897348733624)) ;
#106905 = CARTESIAN_POINT('Ctrl Pts',(-19.4144301291462,-24.4704502790506,
124.91942556247)) ;
#106906 = CARTESIAN_POINT('Ctrl Pts',(-19.6768553029751,-24.4804784763652,
124.895358567147)) ;
#106907 = CARTESIAN_POINT('Ctrl Pts',(-19.9281616014576,-24.4903860186555,
124.827216116485)) ;
#106908 = CARTESIAN_POINT('Ctrl Pts',(-20.1667953840457,-24.5004186692194,
124.715174244585)) ;
#106909 = CARTESIAN_POINT('Ctrl Pts',(-20.3792224588511,-24.510302625646,
124.565695978752)) ;
#106910 = CARTESIAN_POINT('Ctrl Pts',(-20.5648889688196,-24.5202923270079,
124.380098753571)) ;
#106911 = CARTESIAN_POINT('Ctrl Pts',(-20.7158198781951,-24.5303333222839,
124.163660029453)) ;
#106912 = CARTESIAN_POINT('Ctrl Pts',(-20.8249600257777,-24.5401662115523,
123.929446633066)) ;
#106913 = CARTESIAN_POINT('Ctrl Pts',(-20.8935923937664,-24.5501593699197,
123.675968287344)) ;
#106914 = CARTESIAN_POINT('Ctrl Pts',(-20.9167162661487,-24.5601914122718,
123.413340508638)) ;
#106915 = CARTESIAN_POINT('Ctrl Pts',(-20.8945884232422,-24.5700566562302,
123.155051255594)) ;
#106916 = CARTESIAN_POINT('Ctrl Pts',(-20.828007978736,-24.5800185474762,
122.901863765743)) ;
#106917 = CARTESIAN_POINT('Ctrl Pts',(-20.717293798241,-24.5900534474947,
122.662538389889)) ;
#106918 = CARTESIAN_POINT('Ctrl Pts',(-20.5692808803268,-24.5999385279093,
122.449020508724)) ;
#106919 = CARTESIAN_POINT('Ctrl Pts',(-20.3831408459186,-24.6100037000341,
122.261151555758)) ;
#106920 = CARTESIAN_POINT('Ctrl Pts',(-20.171921014445,-24.6198509347576,
122.11160502399)) ;
#106921 = CARTESIAN_POINT('Ctrl Pts',(-19.9338866398181,-24.6298817460754,
121.998402424725)) ;
#106922 = CARTESIAN_POINT('Ctrl Pts',(-19.6801598924702,-24.6398913619889,
121.928905420214)) ;
#106923 = CARTESIAN_POINT('Ctrl Pts',(-19.4208842732656,-24.6498021413926,
121.904510087934)) ;
#106924 = CARTESIAN_POINT('Ctrl Pts',(-19.1607378646813,-24.6597314071816,
121.9248939004)) ;
#106925 = CARTESIAN_POINT('Ctrl Pts',(-18.9052752384676,-24.6697741004942,
121.991093795154)) ;
#106926 = CARTESIAN_POINT('Ctrl Pts',(-18.6688266886926,-24.679660633189,
122.098797729048)) ;
#106927 = CARTESIAN_POINT('Ctrl Pts',(-18.4521339671131,-24.6896537782922,
122.247123614488)) ;
#106928 = CARTESIAN_POINT('Ctrl Pts',(-18.2654374954735,-24.6995994589663,
122.430030788731)) ;
#106929 = CARTESIAN_POINT('Ctrl Pts',(-18.1128695966725,-24.709546716593,
122.642308610488)) ;
#106930 = CARTESIAN_POINT('Ctrl Pts',(-17.9986071950966,-24.7195946187145,
122.880344723335)) ;
#106931 = CARTESIAN_POINT('Ctrl Pts',(-17.9286177670027,-24.7294423243362,
123.129489608421)) ;
#106932 = CARTESIAN_POINT('Ctrl Pts',(-17.901833142117,-24.7394037909703,
123.389883113504)) ;
#106933 = CARTESIAN_POINT('Ctrl Pts',(-17.9211529777508,-24.7494333442385,
123.652749954878)) ;
#106934 = CARTESIAN_POINT('Ctrl Pts',(-17.9848845095932,-24.7593402362659,
123.905175045904)) ;
#106935 = CARTESIAN_POINT('Ctrl Pts',(-18.0914434456593,-24.7692878803789,
124.143861709539)) ;
#106936 = CARTESIAN_POINT('Ctrl Pts',(-18.2384939760854,-24.7792879234078,
124.361699048924)) ;
#106937 = CARTESIAN_POINT('Ctrl Pts',(-18.4221409649936,-24.7893266894018,
124.55106080361)) ;
#106938 = CARTESIAN_POINT('Ctrl Pts',(-18.6310369633877,-24.7991517514241,
124.702833388253)) ;
#106939 = CARTESIAN_POINT('Ctrl Pts',(-18.8683103182096,-24.8092062987504,
124.819051009912)) ;
#106940 = CARTESIAN_POINT('Ctrl Pts',(-19.1194973611782,-24.8191495421996,
124.8910663407)) ;
#106941 = CARTESIAN_POINT('Ctrl Pts',(-19.3782090444937,-24.8290517138075,
124.91906462524)) ;
#106942 = CARTESIAN_POINT('Ctrl Pts',(-19.6417776433998,-24.8391045494177,
124.901291092302)) ;
#106943 = CARTESIAN_POINT('Ctrl Pts',(-19.8937151208383,-24.8489776071032,
124.839250660961)) ;
#106944 = CARTESIAN_POINT('Ctrl Pts',(-20.134240507652,-24.8589728686289,
124.733710267886)) ;
#106945 = CARTESIAN_POINT('Ctrl Pts',(-20.3531898254097,-24.8689982380494,
124.587174639634)) ;
#106946 = CARTESIAN_POINT('Ctrl Pts',(-20.5410415166913,-24.878888070576,
124.407554509467)) ;
#106947 = CARTESIAN_POINT('Ctrl Pts',(-20.7481549549559,-24.8921860413854,
124.126143799265)) ;
#106948 = CARTESIAN_POINT('Ctrl Pts',(-20.8766424273959,-24.9053844364946,
123.799684327235)) ;
#106949 = CARTESIAN_POINT('Ctrl Pts',(-20.9162637139669,-24.918779878774,
123.449918888424)) ;
#106950 = CARTESIAN_POINT('Ctrl Pts',(-20.9004773781569,-24.928655717013,
123.19083322637)) ;
#106951 = CARTESIAN_POINT('Ctrl Pts',(-20.838947304478,-24.9387171196107,
122.93373140854)) ;
#106952 = CARTESIAN_POINT('Ctrl Pts',(-20.7358027985603,-24.9485821765459,
122.695849306882)) ;
#106953 = CARTESIAN_POINT('Ctrl Pts',(-20.5912214248637,-24.9585942724947,
122.47606681639)) ;
#106954 = CARTESIAN_POINT('Ctrl Pts',(-20.3516992972503,-24.9718715816401,
122.222302728919)) ;
#106955 = CARTESIAN_POINT('Ctrl Pts',(-19.9764454446067,-24.9884706071474,
121.990340344157)) ;
#106956 = CARTESIAN_POINT('Ctrl Pts',(-19.5445902666721,-25.0050696551804,
121.900306518793)) ;
#106957 = CARTESIAN_POINT('Ctrl Pts',(-19.1970560702189,-25.0183130672114,
121.919332976408)) ;
#106958 = CARTESIAN_POINT('Ctrl Pts',(-18.940168786962,-25.0283504948998,
121.979150759205)) ;
#106959 = CARTESIAN_POINT('Ctrl Pts',(-18.7007881441074,-25.0382547968554,
122.081334287763)) ;
#106960 = CARTESIAN_POINT('Ctrl Pts',(-18.4082675107088,-25.0515216368306,
122.271046777023)) ;
#106961 = CARTESIAN_POINT('Ctrl Pts',(-18.1123456266158,-25.0681478349205,
122.599207663256)) ;
#106962 = CARTESIAN_POINT('Ctrl Pts',(-17.9131353960091,-25.0880669503039,
123.08973418129)) ;
#106963 = CARTESIAN_POINT('Ctrl Pts',(-17.8962113866272,-25.1046733734382,
123.530770659968)) ;
#106964 = CARTESIAN_POINT('Ctrl Pts',(-17.9736439459162,-25.1179695939339,
123.871497784587)) ;
#106965 = CARTESIAN_POINT('Ctrl Pts',(-18.108093327351,-25.1312384262753,
124.193307694941)) ;
#106966 = CARTESIAN_POINT('Ctrl Pts',(-18.3795961224267,-25.1479296743084,
124.544018559131)) ;
#106967 = CARTESIAN_POINT('Ctrl Pts',(-18.8243636417243,-25.1677394059812,
124.825912141057)) ;
#106968 = CARTESIAN_POINT('Ctrl Pts',(-19.342674885588,-25.1877170133098,
124.941073667171)) ;
#106969 = CARTESIAN_POINT('Ctrl Pts',(-19.8676499505085,-25.2076433223676,
124.871666354727)) ;
#106970 = CARTESIAN_POINT('Ctrl Pts',(-20.3358800280026,-25.2274601825323,
124.630171750087)) ;
#106971 = CARTESIAN_POINT('Ctrl Pts',(-20.6978730394626,-25.2475599981263,
124.237542291265)) ;
#106972 = CARTESIAN_POINT('Ctrl Pts',(-20.9010231320322,-25.2673169620089,
123.753088339619)) ;
#106973 = CARTESIAN_POINT('Ctrl Pts',(-20.9280483314068,-25.2873538880783,
123.221407603216)) ;
#106974 = CARTESIAN_POINT('Ctrl Pts',(-20.7724317346109,-25.3072234704598,
122.71661402828)) ;
#106975 = CARTESIAN_POINT('Ctrl Pts',(-20.4545450312064,-25.327128042213,
122.293870066593)) ;
#106976 = CARTESIAN_POINT('Ctrl Pts',(-20.0102205883016,-25.3470806444115,
122.004220843473)) ;
#106977 = CARTESIAN_POINT('Ctrl Pts',(-19.4949958995402,-25.3669901353818,
121.884058486716)) ;
#106978 = CARTESIAN_POINT('Ctrl Pts',(-18.9708179026118,-25.3868415040812,
121.945295970142)) ;
#106979 = CARTESIAN_POINT('Ctrl Pts',(-18.4941285719003,-25.4069217002172,
122.185052393846)) ;
#106980 = CARTESIAN_POINT('Ctrl Pts',(-18.1327894364014,-25.4267226437926,
122.56786400409)) ;
#106981 = CARTESIAN_POINT('Ctrl Pts',(-17.9208325642514,-25.4467066203021,
123.05478916787)) ;
#106982 = CARTESIAN_POINT('Ctrl Pts',(-17.8886895489191,-25.4666225832777,
123.583143521269)) ;
#106983 = CARTESIAN_POINT('Ctrl Pts',(-18.0370599385116,-25.4864930180996,
124.090104054025)) ;
#106984 = CARTESIAN_POINT('Ctrl Pts',(-18.352917711476,-25.5065433033327,
124.519121936274)) ;
#106985 = CARTESIAN_POINT('Ctrl Pts',(-18.7899901791199,-25.526317272092,
124.811357077356)) ;
#106986 = CARTESIAN_POINT('Ctrl Pts',(-19.3073428474073,-25.5463737302116,
124.938951376792)) ;
#106987 = CARTESIAN_POINT('Ctrl Pts',(-19.8306108133503,-25.5661686132026,
124.882860177028)) ;
#106988 = CARTESIAN_POINT('Ctrl Pts',(-20.3078500603457,-25.5861352685049,
124.651027917224)) ;
#106989 = CARTESIAN_POINT('Ctrl Pts',(-20.6767072840341,-25.6060942385814,
124.269637862864)) ;
#106990 = CARTESIAN_POINT('Ctrl Pts',(-20.892889706575,-25.6259903261715,
123.787070999815)) ;
#106991 = CARTESIAN_POINT('Ctrl Pts',(-20.9320520392546,-25.6458884960831,
123.259707282722)) ;
#106992 = CARTESIAN_POINT('Ctrl Pts',(-20.7893672747436,-25.6657943314502,
122.750206541709)) ;
#106993 = CARTESIAN_POINT('Ctrl Pts',(-20.4807383967051,-25.6857442563881,
122.319104917186)) ;
#106994 = CARTESIAN_POINT('Ctrl Pts',(-20.045270569466,-25.7056234462985,
122.019794561741)) ;
#106995 = CARTESIAN_POINT('Ctrl Pts',(-19.5313435803427,-25.7256047705791,
121.886125315559)) ;
#106996 = CARTESIAN_POINT('Ctrl Pts',(-19.0038849568637,-25.7455345547874,
121.936016700359)) ;
#106997 = CARTESIAN_POINT('Ctrl Pts',(-18.525515022913,-25.7654545441782,
122.162593470176)) ;
#106998 = CARTESIAN_POINT('Ctrl Pts',(-18.1533644802171,-25.7853097395322,
122.53692696707)) ;
#106999 = CARTESIAN_POINT('Ctrl Pts',(-17.9297308534324,-25.8053557411916,
123.020366144601)) ;
#107000 = CARTESIAN_POINT('Ctrl Pts',(-17.8922938015895,-25.8218554884014,
123.457435365614)) ;
#107001 = CARTESIAN_POINT('Ctrl Pts',(-17.9536238747597,-25.8352440928495,
123.803839654938)) ;
#107002 = CARTESIAN_POINT('Ctrl Pts',(-18.0424362921009,-25.8451059211844,
124.047317440358)) ;
#107003 = CARTESIAN_POINT('Ctrl Pts',(-18.1728280726504,-25.855072063942,
124.274457577211)) ;
#107004 = CARTESIAN_POINT('Ctrl Pts',(-18.398321114858,-25.8684338100669,
124.543544062883)) ;
#107005 = CARTESIAN_POINT('Ctrl Pts',(-18.755759039261,-25.884888139022,124.795782547806)) ;
#107006 = CARTESIAN_POINT('Ctrl Pts',(-19.1855136266191,-25.9016553840703,
124.913062176517)) ;
#107007 = CARTESIAN_POINT('Ctrl Pts',(-19.532168225036,-25.9148419493443,
124.914179977617)) ;
#107008 = CARTESIAN_POINT('Ctrl Pts',(-19.7909083811726,-25.9248314080889,
124.870235424795)) ;
#107009 = CARTESIAN_POINT('Ctrl Pts',(-20.0373350366272,-25.93478518057,124.78235238562)) ;
#107010 = CARTESIAN_POINT('Ctrl Pts',(-20.2667304823186,-25.9448329971027,
124.651656840753)) ;
#107011 = CARTESIAN_POINT('Ctrl Pts',(-20.4660137570292,-25.9546745302252,
124.486773533974)) ;
#107012 = CARTESIAN_POINT('Ctrl Pts',(-20.6364871909167,-25.9646607724449,
124.287312743345)) ;
#107013 = CARTESIAN_POINT('Ctrl Pts',(-20.7692327835376,-25.9745973958698,
124.062396894432)) ;
#107014 = CARTESIAN_POINT('Ctrl Pts',(-20.8618050261484,-25.9846472732528,
123.815081089085)) ;
#107015 = CARTESIAN_POINT('Ctrl Pts',(-20.9092717379176,-25.9944977120304,
123.560591541361)) ;
#107016 = CARTESIAN_POINT('Ctrl Pts',(-20.9125449101557,-26.0044697259991,
123.298590931221)) ;
#107017 = CARTESIAN_POINT('Ctrl Pts',(-20.8701309095838,-26.0144648946252,
123.039333300211)) ;
#107018 = CARTESIAN_POINT('Ctrl Pts',(-20.7827323588806,-26.0244987778864,
122.790580963316)) ;
#107019 = CARTESIAN_POINT('Ctrl Pts',(-20.6560870606578,-26.0343546479497,
122.564632684647)) ;
#107020 = CARTESIAN_POINT('Ctrl Pts',(-20.4901308476962,-26.0443521938669,
122.360995763402)) ;
#107021 = CARTESIAN_POINT('Ctrl Pts',(-20.2931406735799,-26.0542603207662,
122.190714868031)) ;
#107022 = CARTESIAN_POINT('Ctrl Pts',(-20.0675018032836,-26.0642706922883,
122.055453597697)) ;
#107023 = CARTESIAN_POINT('Ctrl Pts',(-19.8211228425715,-26.0743011350357,
121.961795007237)) ;
#107024 = CARTESIAN_POINT('Ctrl Pts',(-19.5670204257272,-26.084149087589,
121.912639787958)) ;
#107025 = CARTESIAN_POINT('Ctrl Pts',(-19.3026492624248,-26.09421175661,121.90805310051)) ;
#107026 = CARTESIAN_POINT('Ctrl Pts',(-19.0458449512174,-26.1041061320739,
121.948938241374)) ;
#107027 = CARTESIAN_POINT('Ctrl Pts',(-18.7986876737216,-26.1140479303921,
122.033518099344)) ;
#107028 = CARTESIAN_POINT('Ctrl Pts',(-18.5684665254471,-26.1240504241194,
122.160442177422)) ;
#107029 = CARTESIAN_POINT('Ctrl Pts',(-18.3634215513688,-26.1340852226263,
122.32623577368)) ;
#107030 = CARTESIAN_POINT('Ctrl Pts',(-18.1932054122655,-26.1439301066057,
122.521089565676)) ;
#107031 = CARTESIAN_POINT('Ctrl Pts',(-18.0570995412716,-26.1539159634237,
122.745402537664)) ;
#107032 = CARTESIAN_POINT('Ctrl Pts',(-17.9622893499498,-26.1638507775985,
122.988707568704)) ;
#107033 = CARTESIAN_POINT('Ctrl Pts',(-17.9107815245154,-26.1739082773838,
123.247901857506)) ;
#107034 = CARTESIAN_POINT('Ctrl Pts',(-17.9047991830589,-26.1837300358021,
123.505966538132)) ;
#107035 = CARTESIAN_POINT('Ctrl Pts',(-17.9441442274353,-26.1937856935861,
123.767250890417)) ;
#107036 = CARTESIAN_POINT('Ctrl Pts',(-18.0277702636983,-26.2037278757661,
124.014790591981)) ;
#107037 = CARTESIAN_POINT('Ctrl Pts',(-18.1519364138045,-26.2136330844608,
124.243561611834)) ;
#107038 = CARTESIAN_POINT('Ctrl Pts',(-18.3162378863457,-26.2236748754233,
124.450054470379)) ;
#107039 = CARTESIAN_POINT('Ctrl Pts',(-18.5112522329825,-26.2335826498955,
124.622580587665)) ;
#107040 = CARTESIAN_POINT('Ctrl Pts',(-18.7353273261032,-26.2435941501231,
124.760461732387)) ;
#107041 = CARTESIAN_POINT('Ctrl Pts',(-18.9806532290191,-26.2536269105158,
124.857033178814)) ;
#107042 = CARTESIAN_POINT('Ctrl Pts',(-19.2342454890907,-26.2634774796507,
124.909034939315)) ;
#107043 = CARTESIAN_POINT('Ctrl Pts',(-19.4965987108979,-26.2734660891806,
124.916810782346)) ;
#107044 = CARTESIAN_POINT('Ctrl Pts',(-19.7547866552497,-26.2833947452047,
124.879136485383)) ;
#107045 = CARTESIAN_POINT('Ctrl Pts',(-20.0041305403617,-26.2933824913825,
124.797137527614)) ;
#107046 = CARTESIAN_POINT('Ctrl Pts',(-20.2363343622143,-26.3034184803182,
124.672111002003)) ;
#107047 = CARTESIAN_POINT('Ctrl Pts',(-20.4398589272357,-26.3132733501318,
124.511932238385)) ;
#107048 = CARTESIAN_POINT('Ctrl Pts',(-20.6152342524679,-26.3232727913736,
124.31630284965)) ;
#107049 = CARTESIAN_POINT('Ctrl Pts',(-20.7528133990326,-26.3331678655537,
124.095596185869)) ;
#107050 = CARTESIAN_POINT('Ctrl Pts',(-20.8515508555085,-26.3432285213934,
123.850379097098)) ;
#107051 = CARTESIAN_POINT('Ctrl Pts',(-20.9052171035059,-26.353077395589,
123.597165515688)) ;
#107052 = CARTESIAN_POINT('Ctrl Pts',(-20.9149275362801,-26.3631061075523,
123.333804327786)) ;
#107053 = CARTESIAN_POINT('Ctrl Pts',(-20.8780488245703,-26.3731355081354,
123.072830177121)) ;
#107054 = CARTESIAN_POINT('Ctrl Pts',(-20.7985044978986,-26.3829757017522,
122.826773840961)) ;
#107055 = CARTESIAN_POINT('Ctrl Pts',(-20.6758816110649,-26.3929791243274,
122.594275668135)) ;
#107056 = CARTESIAN_POINT('Ctrl Pts',(-20.5149293057162,-26.4029646614205,
122.386968480829)) ;
#107057 = CARTESIAN_POINT('Ctrl Pts',(-20.31922052082,-26.4130056659073,122.210020619574)) ;
#107058 = CARTESIAN_POINT('Ctrl Pts',(-20.1003044621469,-26.4228492048485,
122.072178443787)) ;
#107059 = CARTESIAN_POINT('Ctrl Pts',(-19.8575995136209,-26.4328342358393,
121.972550199408)) ;
#107060 = CARTESIAN_POINT('Ctrl Pts',(-19.6024003493209,-26.4427736983613,
121.916713979077)) ;
#107061 = CARTESIAN_POINT('Ctrl Pts',(-19.3388058340675,-26.4528134305851,
121.90599082884)) ;
#107062 = CARTESIAN_POINT('Ctrl Pts',(-19.081247010349,-26.4627016109023,
121.940544837108)) ;
#107063 = CARTESIAN_POINT('Ctrl Pts',(-18.8309359774389,-26.4726911266048,
122.019624319406)) ;
#107064 = CARTESIAN_POINT('Ctrl Pts',(-18.5989724252165,-26.4826496772595,
122.140768935798)) ;
#107065 = CARTESIAN_POINT('Ctrl Pts',(-18.3923839555713,-26.4925490843645,
122.298903634733)) ;
#107066 = CARTESIAN_POINT('Ctrl Pts',(-18.2138538015984,-26.5025976707808,
122.493431045269)) ;
#107067 = CARTESIAN_POINT('Ctrl Pts',(-18.0737554054241,-26.5124904897453,
122.712487918614)) ;
#107068 = CARTESIAN_POINT('Ctrl Pts',(-17.9721496783014,-26.5225616072751,
122.956807055062)) ;
#107069 = CARTESIAN_POINT('Ctrl Pts',(-17.915609636616,-26.5323773012411,
123.208531310025)) ;
#107070 = CARTESIAN_POINT('Ctrl Pts',(-17.9029543104203,-26.5424436787384,
123.472705679931)) ;
#107071 = CARTESIAN_POINT('Ctrl Pts',(-17.935897733344,-26.5523426648203,
123.730812155219)) ;
#107072 = CARTESIAN_POINT('Ctrl Pts',(-18.014233583311,-26.5623968448138,
123.983084960881)) ;
#107073 = CARTESIAN_POINT('Ctrl Pts',(-18.1328039031903,-26.5722676577465,
124.213863466518)) ;
#107074 = CARTESIAN_POINT('Ctrl Pts',(-18.2928009544337,-26.5823415586003,
124.424696701549)) ;
#107075 = CARTESIAN_POINT('Ctrl Pts',(-18.481957944128,-26.592161713987,124.600332560415)) ;
#107076 = CARTESIAN_POINT('Ctrl Pts',(-18.7042016187812,-26.6022404209392,
124.744286478818)) ;
#107077 = CARTESIAN_POINT('Ctrl Pts',(-18.9426510348648,-26.612092009478,
124.84527092973)) ;
#107078 = CARTESIAN_POINT('Ctrl Pts',(-19.2005267069829,-26.622165126003,
124.904825642053)) ;
#107079 = CARTESIAN_POINT('Ctrl Pts',(-19.4588480419624,-26.6320076430988,
124.918344794272)) ;
#107080 = CARTESIAN_POINT('Ctrl Pts',(-19.7192610296387,-26.6419881046528,
124.887242445633)) ;
#107081 = CARTESIAN_POINT('Ctrl Pts',(-19.9711299204489,-26.6520063546435,
124.810621311574)) ;
#107082 = CARTESIAN_POINT('Ctrl Pts',(-20.2029952789095,-26.6618905148373,
124.693490844691)) ;
#107083 = CARTESIAN_POINT('Ctrl Pts',(-20.4147300329701,-26.6719556618123,
124.535018461326)) ;
#107084 = CARTESIAN_POINT('Ctrl Pts',(-20.5918552565131,-26.6817974854531,
124.34653140005)) ;
#107085 = CARTESIAN_POINT('Ctrl Pts',(-20.7368429063532,-26.6918269579139,
124.126436778143)) ;
#107086 = CARTESIAN_POINT('Ctrl Pts',(-20.8407127963112,-26.701853813176,
123.884271925495)) ;
#107087 = CARTESIAN_POINT('Ctrl Pts',(-20.9004565941376,-26.7116970632865,
123.632590888649)) ;
#107088 = CARTESIAN_POINT('Ctrl Pts',(-20.9162662490879,-26.7217455028697,
123.369009850146)) ;
#107089 = CARTESIAN_POINT('Ctrl Pts',(-20.885954490215,-26.7316949971176,
123.10930910727)) ;
#107090 = CARTESIAN_POINT('Ctrl Pts',(-20.8120690123609,-26.7416028528436,
122.859628892042)) ;
#107091 = CARTESIAN_POINT('Ctrl Pts',(-20.6939444643144,-26.7516623294935,
122.623167405143)) ;
#107092 = CARTESIAN_POINT('Ctrl Pts',(-20.5402234175417,-26.7615031389022,
122.415167308829)) ;
#107093 = CARTESIAN_POINT('Ctrl Pts',(-20.3487772899462,-26.771565289203,
122.232813349028)) ;
#107094 = CARTESIAN_POINT('Ctrl Pts',(-20.1320035757308,-26.7814624503255,
122.089071576219)) ;
#107095 = CARTESIAN_POINT('Ctrl Pts',(-19.8931105141142,-26.7913936247296,
121.984008253171)) ;
#107096 = CARTESIAN_POINT('Ctrl Pts',(-19.6366994920837,-26.8014358284546,
121.921607841887)) ;
#107097 = CARTESIAN_POINT('Ctrl Pts',(-19.3774249698779,-26.8113224108851,
121.904748137254)) ;
#107098 = CARTESIAN_POINT('Ctrl Pts',(-19.1163507559219,-26.8213158466334,
121.933036255571)) ;
#107099 = CARTESIAN_POINT('Ctrl Pts',(-18.8653956232192,-26.8312603149915,
122.005949625202)) ;
#107100 = CARTESIAN_POINT('Ctrl Pts',(-18.6305138282973,-26.8412121312371,
122.120975690623)) ;
#107101 = CARTESIAN_POINT('Ctrl Pts',(-18.4175163362835,-26.8512495673516,
122.276543163367)) ;
#107102 = CARTESIAN_POINT('Ctrl Pts',(-18.2373351265548,-26.8611345265279,
122.463693629074)) ;
#107103 = CARTESIAN_POINT('Ctrl Pts',(-18.0904991651695,-26.8711326447399,
122.681535599845)) ;
#107104 = CARTESIAN_POINT('Ctrl Pts',(-17.9843530492391,-26.8810535772519,
122.919692108216)) ;
#107105 = CARTESIAN_POINT('Ctrl Pts',(-17.9203477663553,-26.8910948774739,
123.175673758796)) ;
#107106 = CARTESIAN_POINT('Ctrl Pts',(-17.9020982876714,-26.9010017958639,
123.435379748587)) ;
#107107 = CARTESIAN_POINT('Ctrl Pts',(-17.9285541259772,-26.910937587573,
123.695139779583)) ;
#107108 = CARTESIAN_POINT('Ctrl Pts',(-18.0007184221001,-26.9209784821509,
123.948937619437)) ;
#107109 = CARTESIAN_POINT('Ctrl Pts',(-18.1139303893867,-26.9308656838647,
124.182817100163)) ;
#107110 = CARTESIAN_POINT('Ctrl Pts',(-18.2672757035253,-26.9408579516263,
124.395953976354)) ;
#107111 = CARTESIAN_POINT('Ctrl Pts',(-18.4545501643307,-26.9508064726481,
124.578396414551)) ;
#107112 = CARTESIAN_POINT('Ctrl Pts',(-18.6701650173284,-26.9607432462258,
124.725660975012)) ;
#107113 = CARTESIAN_POINT('Ctrl Pts',(-18.9090955124712,-26.9707262943668,
124.834075515904)) ;
#107114 = CARTESIAN_POINT('Ctrl Pts',(-19.1648254639869,-26.9807700019769,
124.899273151225)) ;
#107115 = CARTESIAN_POINT('Ctrl Pts',(-19.4223734198373,-26.9905986951302,
124.919249383875)) ;
#107116 = CARTESIAN_POINT('Ctrl Pts',(-19.6858583169006,-27.0006734442596,
124.893767425328)) ;
#107117 = CARTESIAN_POINT('Ctrl Pts',(-19.9356635840617,-27.0105387700552,
124.824321326066)) ;
#107118 = CARTESIAN_POINT('Ctrl Pts',(-20.1735911071489,-27.0205609444121,
124.711404071088)) ;
#107119 = CARTESIAN_POINT('Ctrl Pts',(-20.3880282939192,-27.030586997619,
124.558287322886)) ;
#107120 = CARTESIAN_POINT('Ctrl Pts',(-20.5697220257241,-27.0404406944653,
124.37381614118)) ;
#107121 = CARTESIAN_POINT('Ctrl Pts',(-20.7188663292308,-27.0504000992183,
124.158736104022)) ;
#107122 = CARTESIAN_POINT('Ctrl Pts',(-20.8288305573601,-27.0604383449232,
123.918970632662)) ;
#107123 = CARTESIAN_POINT('Ctrl Pts',(-20.8948668691598,-27.0703125290852,
123.667995182178)) ;
#107124 = CARTESIAN_POINT('Ctrl Pts',(-20.9167303039655,-27.0803823122231,
123.404313305881)) ;
#107125 = CARTESIAN_POINT('Ctrl Pts',(-20.8931805328912,-27.0902155672439,
123.146958571034)) ;
#107126 = CARTESIAN_POINT('Ctrl Pts',(-20.824670241342,-27.1002459933756,
122.892437582924)) ;
#107127 = CARTESIAN_POINT('Ctrl Pts',(-20.7122904917515,-27.1102776055626,
122.653954853305)) ;
#107128 = CARTESIAN_POINT('Ctrl Pts',(-20.5637282026505,-27.1201073024172,
122.442656891977)) ;
#107129 = CARTESIAN_POINT('Ctrl Pts',(-20.3782970637714,-27.1300967443197,
122.256829442602)) ;
#107130 = CARTESIAN_POINT('Ctrl Pts',(-20.1618698640858,-27.1401406363354,
122.105753614521)) ;
#107131 = CARTESIAN_POINT('Ctrl Pts',(-19.9280207270723,-27.1499621981046,
121.996530490058)) ;
#107132 = CARTESIAN_POINT('Ctrl Pts',(-19.6734949265312,-27.1599977697288,
121.927473665208)) ;
#107133 = CARTESIAN_POINT('Ctrl Pts',(-19.4109421353314,-27.1700270440106,
121.90446294825)) ;
#107134 = CARTESIAN_POINT('Ctrl Pts',(-19.1534313361619,-27.1798608811293,
121.926253148212)) ;
#107135 = CARTESIAN_POINT('Ctrl Pts',(-18.898003021736,-27.1899132772174,
121.993580901922)) ;
#107136 = CARTESIAN_POINT('Ctrl Pts',(-18.6610217719392,-27.1998500441679,
122.103281606099)) ;
#107137 = CARTESIAN_POINT('Ctrl Pts',(-18.4463698462864,-27.2097842791472,
122.25186257191)) ;
#107138 = CARTESIAN_POINT('Ctrl Pts',(-18.2592181860011,-27.219808042474,
122.437226698214)) ;
#107139 = CARTESIAN_POINT('Ctrl Pts',(-18.1090236019886,-27.2296943838587,
122.649213146899)) ;
#107140 = CARTESIAN_POINT('Ctrl Pts',(-17.9962080355324,-27.2396834326256,
122.886245303825)) ;
#107141 = CARTESIAN_POINT('Ctrl Pts',(-17.926428885886,-27.249724653323,123.140723215572)) ;
#107142 = CARTESIAN_POINT('Ctrl Pts',(-17.9019836209174,-27.2595572935009,
123.39795176562)) ;
#107143 = CARTESIAN_POINT('Ctrl Pts',(-17.9221604508856,-27.2695512228089,
123.659804082905)) ;
#107144 = CARTESIAN_POINT('Ctrl Pts',(-17.9882691006007,-27.2795804304894,
123.914937301455)) ;
#107145 = CARTESIAN_POINT('Ctrl Pts',(-18.0956205406589,-27.2894562421935,
124.151236044307)) ;
#107146 = CARTESIAN_POINT('Ctrl Pts',(-18.2439379922689,-27.2994554691649,
124.368102576697)) ;
#107147 = CARTESIAN_POINT('Ctrl Pts',(-18.4258819153618,-27.3093649503206,
124.554462932273)) ;
#107148 = CARTESIAN_POINT('Ctrl Pts',(-18.6404545665967,-27.3194181806215,
124.70853834946)) ;
#107149 = CARTESIAN_POINT('Ctrl Pts',(-18.8741825848005,-27.3292887971726,
124.821069860757)) ;
#107150 = CARTESIAN_POINT('Ctrl Pts',(-19.1275411645829,-27.3393104589046,
124.89294005617)) ;
#107151 = CARTESIAN_POINT('Ctrl Pts',(-19.389638167874,-27.3493332720857,
124.919131495704)) ;
#107152 = CARTESIAN_POINT('Ctrl Pts',(-19.6482300943565,-27.3592004365456,
124.900157768861)) ;
#107153 = CARTESIAN_POINT('Ctrl Pts',(-19.902982223414,-27.3691938787656,
124.836337874072)) ;
#107154 = CARTESIAN_POINT('Ctrl Pts',(-20.1434831381173,-27.3792255523659,
124.728378827775)) ;
#107155 = CARTESIAN_POINT('Ctrl Pts',(-20.3582270580471,-27.3890919874789,
124.583062625148)) ;
#107156 = CARTESIAN_POINT('Ctrl Pts',(-20.5470277371676,-27.399079438012,
124.400791657339)) ;
#107157 = CARTESIAN_POINT('Ctrl Pts',(-20.7008098488123,-27.4090243678399,
124.189436437923)) ;
#107158 = CARTESIAN_POINT('Ctrl Pts',(-20.816549998755,-27.4190692628951,
123.952221298349)) ;
#107159 = CARTESIAN_POINT('Ctrl Pts',(-20.8882501680196,-27.4289313245809,
123.703152220642)) ;
#107160 = CARTESIAN_POINT('Ctrl Pts',(-20.9164927273383,-27.4389230473678,
123.442124426353)) ;
#107161 = CARTESIAN_POINT('Ctrl Pts',(-20.8989909248932,-27.4488552616077,
123.181700468198)) ;
#107162 = CARTESIAN_POINT('Ctrl Pts',(-20.8370759801895,-27.4587945801734,
122.927942517171)) ;
#107163 = CARTESIAN_POINT('Ctrl Pts',(-20.730715480515,-27.4688387549493,
122.686374273125)) ;
#107164 = CARTESIAN_POINT('Ctrl Pts',(-20.5866771788675,-27.4787093090143,
122.470655142122)) ;
#107165 = CARTESIAN_POINT('Ctrl Pts',(-20.4062035407217,-27.4886742913685,
122.280905191679)) ;
#107166 = CARTESIAN_POINT('Ctrl Pts',(-20.1939015897808,-27.4987049942583,
122.124677894178)) ;
#107167 = CARTESIAN_POINT('Ctrl Pts',(-19.9610897598874,-27.5085973342835,
122.008944236056)) ;
#107168 = CARTESIAN_POINT('Ctrl Pts',(-19.7077373937747,-27.5186505674435,
121.934188358121)) ;
#107169 = CARTESIAN_POINT('Ctrl Pts',(-19.4496805193891,-27.5285318119202,
121.904898728865)) ;
#107170 = CARTESIAN_POINT('Ctrl Pts',(-19.1865551873291,-27.5385649327912,
121.920906361169)) ;
#107171 = CARTESIAN_POINT('Ctrl Pts',(-18.9339397336339,-27.5484461430663,
121.981224484517)) ;
#107172 = CARTESIAN_POINT('Ctrl Pts',(-18.691328088118,-27.5585082188356,
122.086276388266)) ;
#107173 = CARTESIAN_POINT('Ctrl Pts',(-18.4750234074904,-27.5683652772174,
122.228858024191)) ;
#107174 = CARTESIAN_POINT('Ctrl Pts',(-18.2838294855732,-27.5783598325064,
122.408874205211)) ;
#107175 = CARTESIAN_POINT('Ctrl Pts',(-18.1277548944552,-27.5882857200419,
122.617914347121)) ;
#107176 = CARTESIAN_POINT('Ctrl Pts',(-18.0091317372431,-27.5983107400372,
122.853121697837)) ;
#107177 = CARTESIAN_POINT('Ctrl Pts',(-17.9340214141047,-27.6082081171408,
123.102140704683)) ;
#107178 = CARTESIAN_POINT('Ctrl Pts',(-17.9024321371092,-27.6181983542217,
123.362773427688)) ;
#107179 = CARTESIAN_POINT('Ctrl Pts',(-17.9171489581271,-27.6282349670305,
123.626110492432)) ;
#107180 = CARTESIAN_POINT('Ctrl Pts',(-17.9758389387995,-27.6380848504485,
123.87822330786)) ;
#107181 = CARTESIAN_POINT('Ctrl Pts',(-18.0784974374125,-27.648088467351,
124.120206414581)) ;
#107182 = CARTESIAN_POINT('Ctrl Pts',(-18.221566977611,-27.6580778791161,
124.340354726405)) ;
#107183 = CARTESIAN_POINT('Ctrl Pts',(-18.4012882013648,-27.6680966404609,
124.532720748786)) ;
#107184 = CARTESIAN_POINT('Ctrl Pts',(-18.6786387524991,-27.681315315842,
124.741958869502)) ;
#107185 = CARTESIAN_POINT('Ctrl Pts',(-19.0063093815083,-27.6946256230867,
124.875054460151)) ;
#107186 = CARTESIAN_POINT('Ctrl Pts',(-19.3515549171491,-27.7078632893127,
124.918075531925)) ;
#107187 = CARTESIAN_POINT('Ctrl Pts',(-19.6119415048006,-27.7177829847234,
124.905729342981)) ;
#107188 = CARTESIAN_POINT('Ctrl Pts',(-19.8695625085415,-27.727835851722,
124.847299116356)) ;
#107189 = CARTESIAN_POINT('Ctrl Pts',(-20.1084867849093,-27.7376912600512,
124.747289288074)) ;
#107190 = CARTESIAN_POINT('Ctrl Pts',(-20.3306708426081,-27.7477298917278,
124.605097635172)) ;
#107191 = CARTESIAN_POINT('Ctrl Pts',(-20.5876397867162,-27.7610320739948,
124.36808782252)) ;
#107192 = CARTESIAN_POINT('Ctrl Pts',(-20.8234771617487,-27.7775770870777,
123.996910194884)) ;
#107193 = CARTESIAN_POINT('Ctrl Pts',(-20.9191962357907,-27.7942291031539,
123.564870810933)) ;
#107194 = CARTESIAN_POINT('Ctrl Pts',(-20.9040912184694,-27.8074521940591,
123.217672285098)) ;
#107195 = CARTESIAN_POINT('Ctrl Pts',(-20.8481766667372,-27.8174131536185,
122.96195496133)) ;
#107196 = CARTESIAN_POINT('Ctrl Pts',(-20.7477729122101,-27.8274379503696,
122.718403212381)) ;
#107197 = CARTESIAN_POINT('Ctrl Pts',(-20.561939019658,-27.8406623977654,
122.424695634254)) ;
#107198 = CARTESIAN_POINT('Ctrl Pts',(-20.2373190885059,-27.8572961824645,
122.124659826914)) ;
#107199 = CARTESIAN_POINT('Ctrl Pts',(-19.7495668232349,-27.8771988491894,
121.919809101773)) ;
#107200 = CARTESIAN_POINT('Ctrl Pts',(-19.2213679190859,-27.8970990769713,
121.893008326786)) ;
#107201 = CARTESIAN_POINT('Ctrl Pts',(-18.715153312022,-27.9170165645028,
122.047856538397)) ;
#107202 = CARTESIAN_POINT('Ctrl Pts',(-18.2916891277542,-27.9369460903197,
122.366103012824)) ;
#107203 = CARTESIAN_POINT('Ctrl Pts',(-18.0018513470074,-27.956908358206,
122.810537750514)) ;
#107204 = CARTESIAN_POINT('Ctrl Pts',(-17.8814933307081,-27.9767985531582,
123.325230056623)) ;
#107205 = CARTESIAN_POINT('Ctrl Pts',(-17.9426919986489,-27.9966887979044,
123.850442308538)) ;
#107206 = CARTESIAN_POINT('Ctrl Pts',(-18.1825385104849,-28.0167631704669,
124.326958710587)) ;
#107207 = CARTESIAN_POINT('Ctrl Pts',(-18.5649934168931,-28.0365485478272,
124.687973141665)) ;
#107208 = CARTESIAN_POINT('Ctrl Pts',(-19.0512254181737,-28.0565104218943,
124.900140533655)) ;
#107209 = CARTESIAN_POINT('Ctrl Pts',(-19.5812937356846,-28.0764903973848,
124.932412249247)) ;
#107210 = CARTESIAN_POINT('Ctrl Pts',(-20.0865931632847,-28.0963028272628,
124.784107050787)) ;
#107211 = CARTESIAN_POINT('Ctrl Pts',(-20.5148466735547,-28.1162829353531,
124.47026534295)) ;
#107212 = CARTESIAN_POINT('Ctrl Pts',(-20.8089552859383,-28.1361773189503,
124.030706928548)) ;
#107213 = CARTESIAN_POINT('Ctrl Pts',(-20.9360272834398,-28.1561042469275,
123.516674362654)) ;
#107214 = CARTESIAN_POINT('Ctrl Pts',(-20.8808267606801,-28.1759991042288,
122.990669662517)) ;
#107215 = CARTESIAN_POINT('Ctrl Pts',(-20.6473558405069,-28.1960382978324,
122.512016538107)) ;
#107216 = CARTESIAN_POINT('Ctrl Pts',(-20.2682120927934,-28.2158782657432,
122.145457364838)) ;
#107217 = CARTESIAN_POINT('Ctrl Pts',(-19.785573235683,-28.2357930827073,
121.928259829755)) ;
#107218 = CARTESIAN_POINT('Ctrl Pts',(-19.2570294438198,-28.2557353281035,
121.889112208248)) ;
#107219 = CARTESIAN_POINT('Ctrl Pts',(-18.748255376725,-28.275607376218,122.031351959434)) ;
#107220 = CARTESIAN_POINT('Ctrl Pts',(-18.3160158182085,-28.2956184411721,
122.340969391106)) ;
#107221 = CARTESIAN_POINT('Ctrl Pts',(-18.0174587947323,-28.3154299654757,
122.774994815369)) ;
#107222 = CARTESIAN_POINT('Ctrl Pts',(-17.8834629208939,-28.3355251774391,
123.291794909492)) ;
#107223 = CARTESIAN_POINT('Ctrl Pts',(-17.9332094404965,-28.3553059013589,
123.815384857237)) ;
#107224 = CARTESIAN_POINT('Ctrl Pts',(-18.1597591708436,-28.3752969770017,
124.29577732644)) ;
#107225 = CARTESIAN_POINT('Ctrl Pts',(-18.535084662371,-28.3951789160447,
124.667967825516)) ;
#107226 = CARTESIAN_POINT('Ctrl Pts',(-19.0161323560632,-28.415131520548,
124.890965555242)) ;
#107227 = CARTESIAN_POINT('Ctrl Pts',(-19.5431194959095,-28.4350303892786,
124.936306005945)) ;
#107228 = CARTESIAN_POINT('Ctrl Pts',(-20.0538297867874,-28.4549237890882,
124.799800715195)) ;
#107229 = CARTESIAN_POINT('Ctrl Pts',(-20.4882774828277,-28.4748329199282,
124.497523572711)) ;
#107230 = CARTESIAN_POINT('Ctrl Pts',(-20.7946918595222,-28.4948650196918,
124.062188352273)) ;
#107231 = CARTESIAN_POINT('Ctrl Pts',(-20.9099543609712,-28.5113970928613,
123.638087952506)) ;
#107232 = CARTESIAN_POINT('Ctrl Pts',(-20.9115545856091,-28.5247324334672,
123.287701393177)) ;
#107233 = CARTESIAN_POINT('Ctrl Pts',(-20.8682617470415,-28.5345749920069,
123.032666470944)) ;
#107234 = CARTESIAN_POINT('Ctrl Pts',(-20.7797764681059,-28.5446268988568,
122.783811473852)) ;
#107235 = CARTESIAN_POINT('Ctrl Pts',(-20.607853787178,-28.5578754132477,
122.48100626112)) ;
#107236 = CARTESIAN_POINT('Ctrl Pts',(-20.298677518794,-28.5744745881955,
122.166364976161)) ;
#107237 = CARTESIAN_POINT('Ctrl Pts',(-19.9009534723476,-28.5910633739905,
121.97606456656)) ;
#107238 = CARTESIAN_POINT('Ctrl Pts',(-19.5580552678904,-28.6043391903325,
121.911740597711)) ;
#107239 = CARTESIAN_POINT('Ctrl Pts',(-19.2959587737664,-28.6143130411263,
121.908503082593)) ;
#107240 = CARTESIAN_POINT('Ctrl Pts',(-19.0359171764911,-28.6243420732187,
121.951334244634)) ;
#107241 = CARTESIAN_POINT('Ctrl Pts',(-18.7905934021712,-28.6342321987206,
122.037205531534)) ;
#107242 = CARTESIAN_POINT('Ctrl Pts',(-18.5614284408685,-28.6442246769921,
122.165353939574)) ;
#107243 = CARTESIAN_POINT('Ctrl Pts',(-18.3586907974813,-28.6541758920895,
122.330596840673)) ;
#107244 = CARTESIAN_POINT('Ctrl Pts',(-18.1862612792095,-28.6642243938445,
122.530554327297)) ;
#107245 = CARTESIAN_POINT('Ctrl Pts',(-18.0536697103203,-28.6740657434613,
122.752628426208)) ;
#107246 = CARTESIAN_POINT('Ctrl Pts',(-17.959795093823,-28.6840520344815,
122.997646993215)) ;
#107247 = CARTESIAN_POINT('Ctrl Pts',(-17.9099939640272,-28.6939886462101,
123.254022115635)) ;
#107248 = CARTESIAN_POINT('Ctrl Pts',(-17.9055461660976,-28.7040385215777,
123.518058015356)) ;
#107249 = CARTESIAN_POINT('Ctrl Pts',(-17.9460039147784,-28.7138889801131,
123.773755758102)) ;
#107250 = CARTESIAN_POINT('Ctrl Pts',(-18.0306176772818,-28.7238609170659,
124.021737244033)) ;
#107251 = CARTESIAN_POINT('Ctrl Pts',(-18.157373568169,-28.733856373998,124.251845030224)) ;
#107252 = CARTESIAN_POINT('Ctrl Pts',(-18.3229702726794,-28.7438891810511,
124.456980828054)) ;
#107253 = CARTESIAN_POINT('Ctrl Pts',(-18.5180369157073,-28.7537490676411,
124.627546708464)) ;
#107254 = CARTESIAN_POINT('Ctrl Pts',(-18.7423754605247,-28.7637381482063,
124.763810474959)) ;
#107255 = CARTESIAN_POINT('Ctrl Pts',(-18.9855849680071,-28.7736696274155,
124.858511073407)) ;
#107256 = CARTESIAN_POINT('Ctrl Pts',(-19.2428700750694,-28.7836554868614,
124.910249736956)) ;
#107257 = CARTESIAN_POINT('Ctrl Pts',(-19.5065796970745,-28.7936936375086,
124.916096312179)) ;
#107258 = CARTESIAN_POINT('Ctrl Pts',(-19.7624834465028,-28.803541728013,
124.8773385409)) ;
#107259 = CARTESIAN_POINT('Ctrl Pts',(-20.0130929085487,-28.813602636531,
124.793179654348)) ;
#107260 = CARTESIAN_POINT('Ctrl Pts',(-20.2414099175365,-28.8234974836889,
124.668689114803)) ;
#107261 = CARTESIAN_POINT('Ctrl Pts',(-20.4459946353188,-28.833439155734,
124.506257858748)) ;
#107262 = CARTESIAN_POINT('Ctrl Pts',(-20.6204504823077,-28.8434416828595,
124.309593013046)) ;
#107263 = CARTESIAN_POINT('Ctrl Pts',(-20.7581704433979,-28.8534764740469,
124.084728431915)) ;
#107264 = CARTESIAN_POINT('Ctrl Pts',(-20.8533438150002,-28.863321353906,
123.844138419902)) ;
#107265 = CARTESIAN_POINT('Ctrl Pts',(-20.906513020906,-28.8733072345245,
123.58720590988)) ;
#107266 = CARTESIAN_POINT('Ctrl Pts',(-20.9144137492764,-28.8832419576177,
123.326201887984)) ;
#107267 = CARTESIAN_POINT('Ctrl Pts',(-20.8761831412985,-28.8932997979289,
123.064712473205)) ;
#107268 = CARTESIAN_POINT('Ctrl Pts',(-20.7954623118713,-28.9031202853254,
122.819554004774)) ;
#107269 = CARTESIAN_POINT('Ctrl Pts',(-20.6708356973687,-28.9131806866705,
122.58643084235)) ;
#107270 = CARTESIAN_POINT('Ctrl Pts',(-20.5094087231614,-28.9231116522234,
122.381333168133)) ;
#107271 = CARTESIAN_POINT('Ctrl Pts',(-20.3150976137856,-28.9330505145599,
122.20684661921)) ;
#107272 = CARTESIAN_POINT('Ctrl Pts',(-20.0924409972061,-28.9430362454861,
122.067919162026)) ;
#107273 = CARTESIAN_POINT('Ctrl Pts',(-19.8480433403635,-28.9530606309135,
121.969659854682)) ;
#107274 = CARTESIAN_POINT('Ctrl Pts',(-19.593440719786,-28.9629639152668,
121.915584792922)) ;
#107275 = CARTESIAN_POINT('Ctrl Pts',(-19.3292629768362,-28.9730239198448,
121.906485243782)) ;
#107276 = CARTESIAN_POINT('Ctrl Pts',(-19.0730746939001,-28.9828671889139,
121.942426938591)) ;
#107277 = CARTESIAN_POINT('Ctrl Pts',(-18.8232042085164,-28.9928577545216,
122.022902031652)) ;
#107278 = CARTESIAN_POINT('Ctrl Pts',(-18.5925340794096,-29.0027858863004,
122.14483093452)) ;
#107279 = CARTESIAN_POINT('Ctrl Pts',(-18.3850181563791,-29.0127737733813,
122.305561886804)) ;
#107280 = CARTESIAN_POINT('Ctrl Pts',(-18.2080606746573,-29.02280972295,122.501102325155)) ;
#107281 = CARTESIAN_POINT('Ctrl Pts',(-18.0698934323502,-29.0326646093288,
122.720167187635)) ;
#107282 = CARTESIAN_POINT('Ctrl Pts',(-17.9701183498815,-29.0426640236767,
122.963214409578)) ;
#107283 = CARTESIAN_POINT('Ctrl Pts',(-17.9143532599889,-29.0525591888672,
123.217244013255)) ;
#107284 = CARTESIAN_POINT('Ctrl Pts',(-17.9033934026888,-29.0626195075592,
123.481356106685)) ;
#107285 = CARTESIAN_POINT('Ctrl Pts',(-17.937582380809,-29.0724696393352,
123.737963166861)) ;
#107286 = CARTESIAN_POINT('Ctrl Pts',(-18.0166363100834,-29.0825002097855,
123.98940960622)) ;
#107287 = CARTESIAN_POINT('Ctrl Pts',(-18.1384821139156,-29.0925143604583,
124.222680263997)) ;
#107288 = CARTESIAN_POINT('Ctrl Pts',(-18.2966985543212,-29.1024072940037,
124.428975038743)) ;
#107289 = CARTESIAN_POINT('Ctrl Pts',(-18.4899775082618,-29.112396807994,
124.606580208232)) ;
#107290 = CARTESIAN_POINT('Ctrl Pts',(-18.7103271424368,-29.1223505786464,
124.747601568313)) ;
#107291 = CARTESIAN_POINT('Ctrl Pts',(-18.9541278519356,-29.132398347307,
124.848928066334)) ;
#107292 = CARTESIAN_POINT('Ctrl Pts',(-19.2065149359924,-29.1422400737468,
124.905514667488)) ;
#107293 = CARTESIAN_POINT('Ctrl Pts',(-19.4685786980452,-29.1522255905695,
124.918161518453)) ;
#107294 = CARTESIAN_POINT('Ctrl Pts',(-19.7277435431009,-29.1621649222651,
124.88535161819)) ;
#107295 = CARTESIAN_POINT('Ctrl Pts',(-19.979722346189,-29.1722046919626,
124.807223134211)) ;
#107296 = CARTESIAN_POINT('Ctrl Pts',(-20.2108569771339,-29.1820928532114,
124.688449404783)) ;
#107297 = CARTESIAN_POINT('Ctrl Pts',(-20.4202579427664,-29.1920824077138,
124.530143768635)) ;
#107298 = CARTESIAN_POINT('Ctrl Pts',(-20.5982897639513,-29.2020408222374,
124.338345472997)) ;
#107299 = CARTESIAN_POINT('Ctrl Pts',(-20.7400265330737,-29.2119407350668,
124.120168216643)) ;
#107300 = CARTESIAN_POINT('Ctrl Pts',(-20.843149350905,-29.2219874347167,
123.877151468186)) ;
#107301 = CARTESIAN_POINT('Ctrl Pts',(-20.9018183233676,-29.2318872950223,
123.62365382285)) ;
#107302 = CARTESIAN_POINT('Ctrl Pts',(-20.9158738240307,-29.2419386992278,
123.359924987347)) ;
#107303 = CARTESIAN_POINT('Ctrl Pts',(-20.8845500593917,-29.2518197361489,
123.102119232617)) ;
#107304 = CARTESIAN_POINT('Ctrl Pts',(-20.8083953396157,-29.2618195683264,
122.850656174921)) ;
#107305 = CARTESIAN_POINT('Ctrl Pts',(-20.6908578374418,-29.2717375713113,
122.617977476822)) ;
#107306 = CARTESIAN_POINT('Ctrl Pts',(-20.5325918654927,-29.2817888771858,
122.406561035641)) ;
#107307 = CARTESIAN_POINT('Ctrl Pts',(-20.3436416646335,-29.2916587005774,
122.228799630198)) ;
#107308 = CARTESIAN_POINT('Ctrl Pts',(-20.1222938931846,-29.3017328666277,
122.083680730194)) ;
#107309 = CARTESIAN_POINT('Ctrl Pts',(-19.8852598986933,-29.3115529507693,
121.981494645576)) ;
#107310 = CARTESIAN_POINT('Ctrl Pts',(-19.6276501727185,-29.3216316775052,
121.920236702777)) ;
#107311 = CARTESIAN_POINT('Ctrl Pts',(-19.3691535481643,-29.3314832581547,
121.904894321861)) ;
#107312 = CARTESIAN_POINT('Ctrl Pts',(-19.106218855204,-29.3415563864531,
121.935094557525)) ;
#107313 = CARTESIAN_POINT('Ctrl Pts',(-18.8582742358518,-29.3513988643445,
122.008822694386)) ;
#107314 = CARTESIAN_POINT('Ctrl Pts',(-18.6232933239942,-29.3613794709426,
122.125302992374)) ;
#107315 = CARTESIAN_POINT('Ctrl Pts',(-18.4116059083099,-29.3713971799614,
122.281799157481)) ;
#107316 = CARTESIAN_POINT('Ctrl Pts',(-18.2323066249273,-29.3812833589988,
122.469835868044)) ;
#107317 = CARTESIAN_POINT('Ctrl Pts',(-18.0858943600191,-29.3913409715712,
122.689852873575)) ;
#107318 = CARTESIAN_POINT('Ctrl Pts',(-17.9817783185599,-29.4012173649433,
122.927613195183)) ;
#107319 = CARTESIAN_POINT('Ctrl Pts',(-17.9191599044313,-29.4112123930937,
123.182690994245)) ;
#107320 = CARTESIAN_POINT('Ctrl Pts',(-17.9021863708431,-29.4212331399397,
123.445489631793)) ;
#107321 = CARTESIAN_POINT('Ctrl Pts',(-17.9304545075469,-29.4311352086061,
123.704163371341)) ;
#107322 = CARTESIAN_POINT('Ctrl Pts',(-18.0034882290822,-29.4411259484258,
123.956348533631)) ;
#107323 = CARTESIAN_POINT('Ctrl Pts',(-18.1190484241088,-29.4510891446361,
124.191274632941)) ;
#107324 = CARTESIAN_POINT('Ctrl Pts',(-18.2722296949224,-29.4609933289362,
124.40172526488)) ;
#107325 = CARTESIAN_POINT('Ctrl Pts',(-18.4626960378833,-29.4710537893271,
124.585031387986)) ;
#107326 = CARTESIAN_POINT('Ctrl Pts',(-18.6771724124148,-29.4808943351979,
124.729570547776)) ;
#107327 = CARTESIAN_POINT('Ctrl Pts',(-18.9186146981797,-29.4909565559097,
124.837323844312)) ;
#107328 = CARTESIAN_POINT('Ctrl Pts',(-19.1709983128989,-29.5008536989262,
124.900212053229)) ;
#107329 = CARTESIAN_POINT('Ctrl Pts',(-19.4312786043944,-29.5107848753434,
124.91924979015)) ;
#107330 = CARTESIAN_POINT('Ctrl Pts',(-19.6937852247348,-29.520827089122,
124.892221026757)) ;
#107331 = CARTESIAN_POINT('Ctrl Pts',(-19.9437477862045,-29.5307136293248,
124.821322725191)) ;
#107332 = CARTESIAN_POINT('Ctrl Pts',(-20.180288045457,-29.5407072239302,
124.707269113637)) ;
#107333 = CARTESIAN_POINT('Ctrl Pts',(-20.3923769599037,-29.5506510990877,
124.554587106928)) ;
#107334 = CARTESIAN_POINT('Ctrl Pts',(-20.5752625312194,-29.5606116352025,
124.367347599523)) ;
#107335 = CARTESIAN_POINT('Ctrl Pts',(-20.72354941688,-29.5706082385252,124.150467949388)) ;
#107336 = CARTESIAN_POINT('Ctrl Pts',(-20.8319671128854,-29.5806413214798,
123.910138102214)) ;
#107337 = CARTESIAN_POINT('Ctrl Pts',(-20.8961474318755,-29.5904924901813,
123.659345397393)) ;
#107338 = CARTESIAN_POINT('Ctrl Pts',(-20.9167993806516,-29.6004549808802,
123.398366694536)) ;
#107339 = CARTESIAN_POINT('Ctrl Pts',(-20.8913305106108,-29.6104834092979,
123.136048663369)) ;
#107340 = CARTESIAN_POINT('Ctrl Pts',(-20.8216212819003,-29.6203937766625,
122.885129389924)) ;
#107341 = CARTESIAN_POINT('Ctrl Pts',(-20.7097346900633,-29.6303286442776,
122.649232722637)) ;
#107342 = CARTESIAN_POINT('Ctrl Pts',(-20.5567809496011,-29.6403697862566,
122.434225112138)) ;
#107343 = CARTESIAN_POINT('Ctrl Pts',(-20.3718123627429,-29.6502569224598,
122.251734656416)) ;
#107344 = CARTESIAN_POINT('Ctrl Pts',(-20.1559695220388,-29.6602492048632,
122.102221999296)) ;
#107345 = CARTESIAN_POINT('Ctrl Pts',(-19.9184286726715,-29.6701977328284,
121.992991017142)) ;
#107346 = CARTESIAN_POINT('Ctrl Pts',(-19.6659588181329,-29.6801344639905,
121.92639428733)) ;
#107347 = CARTESIAN_POINT('Ctrl Pts',(-19.4045177020907,-29.6901176748505,
121.904213276698)) ;
#107348 = CARTESIAN_POINT('Ctrl Pts',(-19.1417307690133,-29.7001607740004,
121.928370870773)) ;
#107349 = CARTESIAN_POINT('Ctrl Pts',(-18.8922988626319,-29.7099917382753,
121.99578172201)) ;
#107350 = CARTESIAN_POINT('Ctrl Pts',(-18.6525893183493,-29.7200645906612,
122.107969662871)) ;
#107351 = CARTESIAN_POINT('Ctrl Pts',(-18.4404574740798,-29.729928718373,
122.257000197973)) ;
#107352 = CARTESIAN_POINT('Ctrl Pts',(-18.254059518917,-29.7399509205079,
122.443053886192)) ;
#107353 = CARTESIAN_POINT('Ctrl Pts',(-18.1032189608842,-29.7499781134763,
122.659132604409)) ;
#107354 = CARTESIAN_POINT('Ctrl Pts',(-17.9937340921863,-29.7598337074433,
122.893827180796)) ;
#107355 = CARTESIAN_POINT('Ctrl Pts',(-17.9252122856315,-29.7697908793086,
123.146369882271)) ;
#107356 = CARTESIAN_POINT('Ctrl Pts',(-17.9018420304546,-29.779829723307,
123.409126956835)) ;
#107357 = CARTESIAN_POINT('Ctrl Pts',(-17.9236263816137,-29.7897037471826,
123.667725112118)) ;
#107358 = CARTESIAN_POINT('Ctrl Pts',(-17.9912864175734,-29.799773573173,
123.923515498743)) ;
#107359 = CARTESIAN_POINT('Ctrl Pts',(-18.0996226494323,-29.8096068170702,
124.158141189941)) ;
#107360 = CARTESIAN_POINT('Ctrl Pts',(-18.2493770206669,-29.8196372448433,
124.375047214786)) ;
#107361 = CARTESIAN_POINT('Ctrl Pts',(-18.4351019059383,-29.8296688615884,
124.562155648745)) ;
#107362 = CARTESIAN_POINT('Ctrl Pts',(-18.6458216898426,-29.8394985385691,
124.711535811242)) ;
#107363 = CARTESIAN_POINT('Ctrl Pts',(-18.8827605878955,-29.8494880554091,
124.824574613372)) ;
#107364 = CARTESIAN_POINT('Ctrl Pts',(-19.1372642265583,-29.8595316675488,
124.894487285034)) ;
#107365 = CARTESIAN_POINT('Ctrl Pts',(-19.3942156196338,-29.8693542738841,
124.919144261192)) ;
#107366 = CARTESIAN_POINT('Ctrl Pts',(-19.6572275024493,-29.8793925037834,
124.898964132523)) ;
#107367 = CARTESIAN_POINT('Ctrl Pts',(-19.9119226482974,-29.8894035385753,
124.833001295873)) ;
#107368 = CARTESIAN_POINT('Ctrl Pts',(-20.1487376855666,-29.8993012695424,
124.725440344783)) ;
#107369 = CARTESIAN_POINT('Ctrl Pts',(-20.3654668126922,-29.9092908973929,
124.577311610302)) ;
#107370 = CARTESIAN_POINT('Ctrl Pts',(-20.5524835794486,-29.9192466878389,
124.394358132936)) ;
#107371 = CARTESIAN_POINT('Ctrl Pts',(-20.7048712583227,-29.929174086401,
124.182597989786)) ;
#107372 = CARTESIAN_POINT('Ctrl Pts',(-20.8192188729646,-29.9391996815108,
123.945254326094)) ;
#107373 = CARTESIAN_POINT('Ctrl Pts',(-20.8897800766452,-29.9490855321804,
123.69522895607)) ;
#107374 = CARTESIAN_POINT('Ctrl Pts',(-20.9167483241174,-29.9590747120246,
123.434105477145)) ;
#107375 = CARTESIAN_POINT('Ctrl Pts',(-20.8973194907971,-29.9691158991282,
123.170950732625)) ;
#107376 = CARTESIAN_POINT('Ctrl Pts',(-20.8342523640167,-29.9789485426041,
122.920378094351)) ;
#107377 = CARTESIAN_POINT('Ctrl Pts',(-20.7275885104511,-29.9889424923136,
122.680384913153)) ;
#107378 = CARTESIAN_POINT('Ctrl Pts',(-20.579894444544,-29.9989716150901,
122.462098463616)) ;
#107379 = CARTESIAN_POINT('Ctrl Pts',(-20.3996308019777,-30.0088477460088,
122.275363644049)) ;
#107380 = CARTESIAN_POINT('Ctrl Pts',(-20.1873078177901,-30.0188457810258,
122.120658794249)) ;
#107381 = CARTESIAN_POINT('Ctrl Pts',(-19.9533643834114,-30.0287597107845,
122.005933368096)) ;
#107382 = CARTESIAN_POINT('Ctrl Pts',(-19.6998574292392,-30.0388028985223,
121.932589562807)) ;
#107383 = CARTESIAN_POINT('Ctrl Pts',(-19.4411790736658,-30.0487027406627,
121.90475991674)) ;
#107384 = CARTESIAN_POINT('Ctrl Pts',(-19.1791749601021,-30.0586940074707,
121.92187067356)) ;
#107385 = CARTESIAN_POINT('Ctrl Pts',(-18.923186636168,-30.0687261096027,
121.984912250954)) ;
#107386 = CARTESIAN_POINT('Ctrl Pts',(-18.6858740646116,-30.0785929905574,
122.089372660142)) ;
#107387 = CARTESIAN_POINT('Ctrl Pts',(-18.4672188643047,-30.0885847818456,
122.234760413876)) ;
#107388 = CARTESIAN_POINT('Ctrl Pts',(-18.2767186120029,-30.0986168977571,
122.417001484085)) ;
#107389 = CARTESIAN_POINT('Ctrl Pts',(-18.1230072719438,-30.1084832145571,
122.625814784531)) ;
#107390 = CARTESIAN_POINT('Ctrl Pts',(-18.0061089947537,-30.1184706960307,
122.860769222352)) ;
#107391 = CARTESIAN_POINT('Ctrl Pts',(-17.931945641768,-30.1284156204096,
123.111407763213)) ;
#107392 = CARTESIAN_POINT('Ctrl Pts',(-17.902285286713,-30.1384605063203,
123.373680593113)) ;
#107393 = CARTESIAN_POINT('Ctrl Pts',(-17.9180936234547,-30.1483226100329,
123.632382529412)) ;
#107394 = CARTESIAN_POINT('Ctrl Pts',(-17.9788508601599,-30.1583141738574,
123.887804420223)) ;
#107395 = CARTESIAN_POINT('Ctrl Pts',(-18.082529173865,-30.1682469819203,
124.127353680839)) ;
#107396 = CARTESIAN_POINT('Ctrl Pts',(-18.2257613189898,-30.1781840841566,
124.345723367739)) ;
#107397 = CARTESIAN_POINT('Ctrl Pts',(-18.4070409249013,-30.188236530427,
124.5378471688)) ;
#107398 = CARTESIAN_POINT('Ctrl Pts',(-18.6143892810352,-30.1980826460086,
124.692661848958)) ;
#107399 = CARTESIAN_POINT('Ctrl Pts',(-18.8499856052171,-30.2081306657235,
124.811858051994)) ;
#107400 = CARTESIAN_POINT('Ctrl Pts',(-19.1001693147782,-30.2180726173524,
124.887190172848)) ;
#107401 = CARTESIAN_POINT('Ctrl Pts',(-19.3594615062715,-30.2280113983515,
124.918568712032)) ;
#107402 = CARTESIAN_POINT('Ctrl Pts',(-19.6225225666885,-30.2380374470776,
124.904126517866)) ;
#107403 = CARTESIAN_POINT('Ctrl Pts',(-19.8756411196743,-30.2479243074858,
124.845369531856)) ;
#107404 = CARTESIAN_POINT('Ctrl Pts',(-20.118180857874,-30.2579555826176,
124.742207394591)) ;
#107405 = CARTESIAN_POINT('Ctrl Pts',(-20.3360835875436,-30.267838559918,
124.600793521788)) ;
#107406 = CARTESIAN_POINT('Ctrl Pts',(-20.5293833327197,-30.2778954133252,
124.420660784419)) ;
#107407 = CARTESIAN_POINT('Ctrl Pts',(-20.7382619738942,-30.2910636544011,
124.14463477347)) ;
#107408 = CARTESIAN_POINT('Ctrl Pts',(-20.8725752561866,-30.3044646836276,
123.814915042498)) ;
#107409 = CARTESIAN_POINT('Ctrl Pts',(-20.9154721242773,-30.3176776003585,
123.470246273929)) ;
#107410 = CARTESIAN_POINT('Ctrl Pts',(-20.9031284982682,-30.3276059948117,
123.20968534208)) ;
#107411 = CARTESIAN_POINT('Ctrl Pts',(-20.845595566202,-30.3375874949398,
122.953729921305)) ;
#107412 = CARTESIAN_POINT('Ctrl Pts',(-20.7435783328316,-30.3476280382099,
122.71041030184)) ;
#107413 = CARTESIAN_POINT('Ctrl Pts',(-20.6038586708441,-30.357477369993,
122.492526903474)) ;
#107414 = CARTESIAN_POINT('Ctrl Pts',(-20.4263290632736,-30.3674727744647,
122.298938318789)) ;
#107415 = CARTESIAN_POINT('Ctrl Pts',(-20.2171560775748,-30.3774891019133,
122.139151077078)) ;
#107416 = CARTESIAN_POINT('Ctrl Pts',(-19.9087977156383,-30.3907127590798,
121.978849459773)) ;
#107417 = CARTESIAN_POINT('Ctrl Pts',(-19.5640016254491,-30.4040070504692,
121.902023533072)) ;
#107418 = CARTESIAN_POINT('Ctrl Pts',(-19.2151474722154,-30.4172914014007,
121.916899099156)) ;
#107419 = CARTESIAN_POINT('Ctrl Pts',(-18.959233385577,-30.4272637824625,
121.973159220254)) ;
#107420 = CARTESIAN_POINT('Ctrl Pts',(-18.7182905622047,-30.4371721620881,
122.071965239815)) ;
#107421 = CARTESIAN_POINT('Ctrl Pts',(-18.4950446956191,-30.4472261608362,
122.213218249538)) ;
#107422 = CARTESIAN_POINT('Ctrl Pts',(-18.3032677066978,-30.4570883579525,
122.387584195892)) ;
#107423 = CARTESIAN_POINT('Ctrl Pts',(-18.0882294345681,-30.4704354843266,
122.664654341648)) ;
#107424 = CARTESIAN_POINT('Ctrl Pts',(-17.9176691090608,-30.486972449968,
123.069789026375)) ;
#107425 = CARTESIAN_POINT('Ctrl Pts',(-17.8947689247543,-30.5036070541419,
123.511224766583)) ;
#107426 = CARTESIAN_POINT('Ctrl Pts',(-17.9677597605264,-30.5168968473846,
123.852822963271)) ;
#107427 = CARTESIAN_POINT('Ctrl Pts',(-18.0656623988113,-30.526849478644,
124.095320844935)) ;
#107428 = CARTESIAN_POINT('Ctrl Pts',(-18.2039451181577,-30.5368014459487,
124.31733383176)) ;
#107429 = CARTESIAN_POINT('Ctrl Pts',(-18.4387419579372,-30.5501687044125,
124.578559199658)) ;
#107430 = CARTESIAN_POINT('Ctrl Pts',(-18.8064348754556,-30.5666855163617,
124.818604195386)) ;
#107431 = CARTESIAN_POINT('Ctrl Pts',(-19.3245278534393,-30.586711411368,
124.939938502557)) ;
#107432 = CARTESIAN_POINT('Ctrl Pts',(-19.8475129838899,-30.6065221414982,
124.877995909629)) ;
#107433 = CARTESIAN_POINT('Ctrl Pts',(-20.3222986651346,-30.626499357628,
124.640403874148)) ;
#107434 = CARTESIAN_POINT('Ctrl Pts',(-20.6858947191827,-30.6464262330233,
124.255351813827)) ;
#107435 = CARTESIAN_POINT('Ctrl Pts',(-20.8967545754839,-30.6662476944996,
123.772491153533)) ;
#107436 = CARTESIAN_POINT('Ctrl Pts',(-20.930246289183,-30.6863220123089,
123.240081051915)) ;
#107437 = CARTESIAN_POINT('Ctrl Pts',(-20.7811801654248,-30.7061699813168,
122.733903286621)) ;
#107438 = CARTESIAN_POINT('Ctrl Pts',(-20.4678029638556,-30.72611701538,122.306420902074)) ;
#107439 = CARTESIAN_POINT('Ctrl Pts',(-20.0282836711341,-30.7460129663522,
122.012316933034)) ;
#107440 = CARTESIAN_POINT('Ctrl Pts',(-19.5150768163013,-30.7659084459704,
121.885022994691)) ;
#107441 = CARTESIAN_POINT('Ctrl Pts',(-18.9875493940089,-30.7858645569352,
121.940557548858)) ;
#107442 = CARTESIAN_POINT('Ctrl Pts',(-18.5120413479308,-30.8057691049752,
122.172263938977)) ;
#107443 = CARTESIAN_POINT('Ctrl Pts',(-18.1436329888451,-30.8256432292943,
122.550941964326)) ;
#107444 = CARTESIAN_POINT('Ctrl Pts',(-17.9253626279483,-30.8456977592933,
123.037127679994)) ;
#107445 = CARTESIAN_POINT('Ctrl Pts',(-17.8864163514803,-30.8655052730533,
123.562247075706)) ;
#107446 = CARTESIAN_POINT('Ctrl Pts',(-18.0291401244099,-30.885488628821,
124.073759282254)) ;
#107447 = CARTESIAN_POINT('Ctrl Pts',(-18.337533170565,-30.905406931405,124.504045807)) ;
#107448 = CARTESIAN_POINT('Ctrl Pts',(-18.7724388146455,-30.9252751468507,
124.803748537153)) ;
#107449 = CARTESIAN_POINT('Ctrl Pts',(-19.2881535897615,-30.945325463647,
124.937391160665)) ;
#107450 = CARTESIAN_POINT('Ctrl Pts',(-19.8116899255017,-30.9651015255295,
124.888384619558)) ;
#107451 = CARTESIAN_POINT('Ctrl Pts',(-20.2935526937828,-30.9851561312219,
124.661040470171)) ;
#107452 = CARTESIAN_POINT('Ctrl Pts',(-20.6641765582672,-31.0049498203778,
124.287452176797)) ;
#107453 = CARTESIAN_POINT('Ctrl Pts',(-20.8882002760577,-31.0249165119722,
123.806498159826)) ;
#107454 = CARTESIAN_POINT('Ctrl Pts',(-20.9338306071532,-31.0448765577232,
123.277860730245)) ;
#107455 = CARTESIAN_POINT('Ctrl Pts',(-20.7971227735034,-31.0647748178734,
122.767005346309)) ;
#107456 = CARTESIAN_POINT('Ctrl Pts',(-20.4948654308344,-31.0846697334226,
122.333164844512)) ;
#107457 = CARTESIAN_POINT('Ctrl Pts',(-20.0626416343406,-31.1045799138362,
122.027862379224)) ;
#107458 = CARTESIAN_POINT('Ctrl Pts',(-19.5515649705631,-31.1245157129505,
121.887964693884)) ;
#107459 = CARTESIAN_POINT('Ctrl Pts',(-19.0233903317203,-31.1444535746046,
121.930837086588)) ;
#107460 = CARTESIAN_POINT('Ctrl Pts',(-18.5418366268255,-31.1643726212422,
122.150882202806)) ;
#107461 = CARTESIAN_POINT('Ctrl Pts',(-18.1636869672622,-31.1843215192964,
122.522527872868)) ;
#107462 = CARTESIAN_POINT('Ctrl Pts',(-17.9354131762966,-31.2042273467395,
122.999837740766)) ;
#107463 = CARTESIAN_POINT('Ctrl Pts',(-17.8918991358355,-31.2208100421048,
123.438354996093)) ;
#107464 = CARTESIAN_POINT('Ctrl Pts',(-17.9480303730611,-31.2340842558284,
123.782695879663)) ;
#107465 = CARTESIAN_POINT('Ctrl Pts',(-18.0352352200072,-31.2441309750277,
124.03186648313)) ;
#107466 = CARTESIAN_POINT('Ctrl Pts',(-18.1615436066062,-31.2539750096734,
124.257643973845)) ;
#107467 = CARTESIAN_POINT('Ctrl Pts',(-18.3825173779386,-31.267309394578,
124.529587378034)) ;
#107468 = CARTESIAN_POINT('Ctrl Pts',(-18.7397346727777,-31.2838966118777,
124.78803912099)) ;
#107469 = CARTESIAN_POINT('Ctrl Pts',(-19.1646878984276,-31.3005298239156,
124.909727244072)) ;
#107470 = CARTESIAN_POINT('Ctrl Pts',(-19.5137260263734,-31.3138122661878,
124.915613465627)) ;
#107471 = CARTESIAN_POINT('Ctrl Pts',(-19.7708785665905,-31.323718154102,
124.875271313858)) ;
#107472 = CARTESIAN_POINT('Ctrl Pts',(-20.0193071233012,-31.3337065722071,
124.790489336724)) ;
#107473 = CARTESIAN_POINT('Ctrl Pts',(-20.2499079130323,-31.3437299994459,
124.663170280754)) ;
#107474 = CARTESIAN_POINT('Ctrl Pts',(-20.4525383938523,-31.3536344305629,
124.499840451095)) ;
#107475 = CARTESIAN_POINT('Ctrl Pts',(-20.6825176632985,-31.3668975831733,
124.237884196334)) ;
#107476 = CARTESIAN_POINT('Ctrl Pts',(-20.839220789519,-31.3802224810772,
123.920354669002)) ;
#107477 = CARTESIAN_POINT('Ctrl Pts',(-20.9074451283038,-31.3934782246928,
123.578700871149)) ;
#107478 = CARTESIAN_POINT('Ctrl Pts',(-20.9137386766837,-31.4034375981401,
123.317088900445)) ;
#107479 = CARTESIAN_POINT('Ctrl Pts',(-20.8748902920232,-31.4133814220671,
123.058646926955)) ;
#107480 = CARTESIAN_POINT('Ctrl Pts',(-20.790689481649,-31.4234293662144,
122.808403316486)) ;
#107481 = CARTESIAN_POINT('Ctrl Pts',(-20.6669783773769,-31.4332803374325,
122.580985502148)) ;
#107482 = CARTESIAN_POINT('Ctrl Pts',(-20.5042373768889,-31.4432521548746,
122.375633944712)) ;
#107483 = CARTESIAN_POINT('Ctrl Pts',(-20.3077702956413,-31.4532475771667,
122.201235204252)) ;
#107484 = CARTESIAN_POINT('Ctrl Pts',(-20.0830574195363,-31.4632806422904,
122.06333895259)) ;
#107485 = CARTESIAN_POINT('Ctrl Pts',(-19.8420046926258,-31.4731459749556,
121.967937569208)) ;
#107486 = CARTESIAN_POINT('Ctrl Pts',(-19.5857419131994,-31.4831065175532,
121.914580261074)) ;
#107487 = CARTESIAN_POINT('Ctrl Pts',(-19.3221912582714,-31.4931402030549,
121.906915941249)) ;
#107488 = CARTESIAN_POINT('Ctrl Pts',(-19.065070194438,-31.5030250350452,
121.944123034841)) ;
#107489 = CARTESIAN_POINT('Ctrl Pts',(-18.8138525163385,-31.513092461805,
122.026943078941)) ;
#107490 = CARTESIAN_POINT('Ctrl Pts',(-18.5859328586663,-31.5229309509638,
122.149094334289)) ;
#107491 = CARTESIAN_POINT('Ctrl Pts',(-18.3778842949295,-31.532994432154,
122.312293350143)) ;
#107492 = CARTESIAN_POINT('Ctrl Pts',(-18.2044268971495,-31.5428885899691,
122.506025289575)) ;
#107493 = CARTESIAN_POINT('Ctrl Pts',(-18.0660101087034,-31.5528304467134,
122.72756803597)) ;
#107494 = CARTESIAN_POINT('Ctrl Pts',(-17.9674492874552,-31.5628329243848,
122.971283743603)) ;
#107495 = CARTESIAN_POINT('Ctrl Pts',(-17.9129429280483,-31.5728677286891,
123.229275923166)) ;
#107496 = CARTESIAN_POINT('Ctrl Pts',(-17.9037929635874,-31.5827126055348,
123.487844790178)) ;
#107497 = CARTESIAN_POINT('Ctrl Pts',(-17.9396945692853,-31.5926984850903,
123.747752720024)) ;
#107498 = CARTESIAN_POINT('Ctrl Pts',(-18.0196152582505,-31.6026332154488,
123.996346627986)) ;
#107499 = CARTESIAN_POINT('Ctrl Pts',(-18.1431719765742,-31.6126910277617,
124.229948303937)) ;
#107500 = CARTESIAN_POINT('Ctrl Pts',(-18.3012886866371,-31.6225116198861,
124.433968126404)) ;
#107501 = CARTESIAN_POINT('Ctrl Pts',(-18.4969247202593,-31.6325782054958,
124.611955117681)) ;
#107502 = CARTESIAN_POINT('Ctrl Pts',(-18.7169060912058,-31.6424777860777,
124.750945809857)) ;
#107503 = CARTESIAN_POINT('Ctrl Pts',(-18.9612356540636,-31.6525293857559,
124.851194511038)) ;
#107504 = CARTESIAN_POINT('Ctrl Pts',(-19.2147603866341,-31.6624035721729,
124.906716070212)) ;
#107505 = CARTESIAN_POINT('Ctrl Pts',(-19.4787552825283,-31.6724600480538,
124.917736501395)) ;
#107506 = CARTESIAN_POINT('Ctrl Pts',(-19.7365095844923,-31.6823529793564,
124.883403147334)) ;
#107507 = CARTESIAN_POINT('Ctrl Pts',(-19.9885638779388,-31.692415758069,
124.803566593134)) ;
#107508 = CARTESIAN_POINT('Ctrl Pts',(-20.2179239107843,-31.7022582836502,
124.683939181233)) ;
#107509 = CARTESIAN_POINT('Ctrl Pts',(-20.4264476740645,-31.7122490490751,
124.524468053743)) ;
#107510 = CARTESIAN_POINT('Ctrl Pts',(-20.6029964283698,-31.7221771250731,
124.332359890327)) ;
#107511 = CARTESIAN_POINT('Ctrl Pts',(-20.7447399387057,-31.7321650354601,
124.111438651362)) ;
#107512 = CARTESIAN_POINT('Ctrl Pts',(-20.8460360924056,-31.7422009475851,
123.86794571088)) ;
#107513 = CARTESIAN_POINT('Ctrl Pts',(-20.9029032854347,-31.7520559604328,
123.615266109282)) ;
#107514 = CARTESIAN_POINT('Ctrl Pts',(-20.9155733480408,-31.762054906349,
123.352852263318)) ;
#107515 = CARTESIAN_POINT('Ctrl Pts',(-20.8830661672857,-31.771951818797,
123.094770422917)) ;
#107516 = CARTESIAN_POINT('Ctrl Pts',(-20.805075041774,-31.7820056168905,
122.842374659832)) ;
#107517 = CARTESIAN_POINT('Ctrl Pts',(-20.6865579770331,-31.7918865377172,
122.611306695334)) ;
#107518 = CARTESIAN_POINT('Ctrl Pts',(-20.5281726394026,-31.8018910637149,
122.401499882872)) ;
#107519 = CARTESIAN_POINT('Ctrl Pts',(-20.3360508018856,-31.8118750273324,
122.222755856703)) ;
#107520 = CARTESIAN_POINT('Ctrl Pts',(-20.114501453404,-31.8219146678837,
122.079534168689)) ;
#107521 = CARTESIAN_POINT('Ctrl Pts',(-19.8762895233033,-31.8317586934984,
121.978654244204)) ;
#107522 = CARTESIAN_POINT('Ctrl Pts',(-19.6205867174948,-31.8417496993158,
121.91906612885)) ;
#107523 = CARTESIAN_POINT('Ctrl Pts',(-19.3571632790607,-31.8517874908479,
121.905315885654)) ;
#107524 = CARTESIAN_POINT('Ctrl Pts',(-19.1003324547463,-31.8616318906363,
121.936442553235)) ;
#107525 = CARTESIAN_POINT('Ctrl Pts',(-18.8491694989756,-31.8716166911931,
122.012255191191)) ;
#107526 = CARTESIAN_POINT('Ctrl Pts',(-18.6159330601628,-31.8815562146042,
122.129920757266)) ;
#107527 = CARTESIAN_POINT('Ctrl Pts',(-18.4046433765393,-31.8915959337052,
122.287888249749)) ;
#107528 = CARTESIAN_POINT('Ctrl Pts',(-18.2265989768632,-31.9014841056245,
122.477178257837)) ;
#107529 = CARTESIAN_POINT('Ctrl Pts',(-18.0822682824921,-31.9114736680415,
122.696445093943)) ;
#107530 = CARTESIAN_POINT('Ctrl Pts',(-17.9787051620355,-31.9214320402362,
122.93677177021)) ;
#107531 = CARTESIAN_POINT('Ctrl Pts',(-17.9181842500413,-31.9313321144669,
123.189808215858)) ;
#107532 = CARTESIAN_POINT('Ctrl Pts',(-17.9023233424814,-31.9413782108405,
123.453319896886)) ;
#107533 = CARTESIAN_POINT('Ctrl Pts',(-17.9320326075536,-31.9512867948376,
123.712019221572)) ;
#107534 = CARTESIAN_POINT('Ctrl Pts',(-18.0065039243755,-31.9612973734285,
123.964329620109)) ;
#107535 = CARTESIAN_POINT('Ctrl Pts',(-18.1243506026566,-31.9713265315413,
124.200081050847)) ;
#107536 = CARTESIAN_POINT('Ctrl Pts',(-18.2782680242316,-31.9811794133794,
124.40826979115)) ;
#107537 = CARTESIAN_POINT('Ctrl Pts',(-18.4674892383523,-31.9911389745304,
124.589102665901)) ;
#107538 = CARTESIAN_POINT('Ctrl Pts',(-18.6872050266719,-32.0011774091195,
124.735068510236)) ;
#107539 = CARTESIAN_POINT('Ctrl Pts',(-18.9248081639537,-32.0110506813466,
124.839402319845)) ;
#107540 = CARTESIAN_POINT('Ctrl Pts',(-19.181949548147,-32.0211239233402,
124.90203769337)) ;
#107541 = CARTESIAN_POINT('Ctrl Pts',(-19.4395184189377,-32.0309442548732,
124.918991539094)) ;
#107542 = CARTESIAN_POINT('Ctrl Pts',(-19.7027715416863,-32.0410229161,124.89048408525)) ;
#107543 = CARTESIAN_POINT('Ctrl Pts',(-19.9514922038896,-32.0508745113942,
124.818414826773)) ;
#107544 = CARTESIAN_POINT('Ctrl Pts',(-20.1891501198683,-32.060947646623,
124.701943720578)) ;
#107545 = CARTESIAN_POINT('Ctrl Pts',(-20.3981122420389,-32.0707900821481,
124.549474888868)) ;
#107546 = CARTESIAN_POINT('Ctrl Pts',(-20.5805492966347,-32.0807708512815,
124.36105417391)) ;
#107547 = CARTESIAN_POINT('Ctrl Pts',(-20.7276369905565,-32.0907879525253,
124.142742755628)) ;
#107548 = CARTESIAN_POINT('Ctrl Pts',(-20.8336659742362,-32.1006764001272,
123.905478070317)) ;
#107549 = CARTESIAN_POINT('Ctrl Pts',(-20.89797251278,-32.110732114308,123.64919325748)) ;
#107550 = CARTESIAN_POINT('Ctrl Pts',(-20.9165067433349,-32.1206073207219,
123.390327809579)) ;
#107551 = CARTESIAN_POINT('Ctrl Pts',(-20.8901191956421,-32.1306023731946,
123.129004709564)) ;
#107552 = CARTESIAN_POINT('Ctrl Pts',(-20.8181509922566,-32.1406242571567,
122.875653953952)) ;
#107553 = CARTESIAN_POINT('Ctrl Pts',(-20.7049044906202,-32.150528229686,
122.641318954081)) ;
#107554 = CARTESIAN_POINT('Ctrl Pts',(-20.5516953308021,-32.1605167263469,
122.428181402184)) ;
#107555 = CARTESIAN_POINT('Ctrl Pts',(-20.364157218951,-32.1704805235949,
122.245474808793)) ;
#107556 = CARTESIAN_POINT('Ctrl Pts',(-20.1493697802425,-32.1803845469029,
122.09844282486)) ;
#107557 = CARTESIAN_POINT('Ctrl Pts',(-19.9085318955107,-32.1904450502245,
121.98946512821)) ;
#107558 = CARTESIAN_POINT('Ctrl Pts',(-19.6580461891382,-32.2002855853644,
121.925056304293)) ;
#107559 = CARTESIAN_POINT('Ctrl Pts',(-19.3944634329032,-32.210347806069,
121.904337209597)) ;
#107560 = CARTESIAN_POINT('Ctrl Pts',(-19.1355881131664,-32.2202449598452,
121.929557911688)) ;
#107561 = CARTESIAN_POINT('Ctrl Pts',(-18.8839506136458,-32.2301760932307,
121.998741559516)) ;
#107562 = CARTESIAN_POINT('Ctrl Pts',(-18.6456320558467,-32.2402184683764,
122.112083948383)) ;
#107563 = CARTESIAN_POINT('Ctrl Pts',(-18.4338299848013,-32.2501044061426,
122.262549762622)) ;
#107564 = CARTESIAN_POINT('Ctrl Pts',(-18.2490783902629,-32.2601002491274,
122.449250229283)) ;
#107565 = CARTESIAN_POINT('Ctrl Pts',(-18.1003611064684,-32.270042227006,
122.664076171763)) ;
#107566 = CARTESIAN_POINT('Ctrl Pts',(-17.9907012439229,-32.280001601487,
122.901700707296)) ;
#107567 = CARTESIAN_POINT('Ctrl Pts',(-17.9235757952326,-32.2899982173208,
123.155708820772)) ;
#107568 = CARTESIAN_POINT('Ctrl Pts',(-17.9018434365828,-32.3000324358943,
123.418492645025)) ;
#107569 = CARTESIAN_POINT('Ctrl Pts',(-17.9253190230438,-32.3098855031049,
123.676351623004)) ;
#107570 = CARTESIAN_POINT('Ctrl Pts',(-17.9932107833042,-32.3198457609825,
123.929129584466)) ;
#107571 = CARTESIAN_POINT('Ctrl Pts',(-18.1050181199454,-32.3298747876881,
124.167805856083)) ;
#107572 = CARTESIAN_POINT('Ctrl Pts',(-18.2546963393557,-32.3397849947225,
124.380912347066)) ;
#107573 = CARTESIAN_POINT('Ctrl Pts',(-18.4390908104522,-32.3497199053701,
124.565750061479)) ;
#107574 = CARTESIAN_POINT('Ctrl Pts',(-18.655191043716,-32.3597610355494,
124.717155840492)) ;
#107575 = CARTESIAN_POINT('Ctrl Pts',(-18.8905747900674,-32.3696481759193,
124.827204201677)) ;
#107576 = CARTESIAN_POINT('Ctrl Pts',(-19.1440130868697,-32.3796404534553,
124.895842668681)) ;
#107577 = CARTESIAN_POINT('Ctrl Pts',(-19.4044139426701,-32.3895889967236,
124.919259338434)) ;
#107578 = CARTESIAN_POINT('Ctrl Pts',(-19.6646123363536,-32.3995256715408,
124.897507120475)) ;
#107579 = CARTESIAN_POINT('Ctrl Pts',(-19.9183942075054,-32.4095090924772,
124.830886610359)) ;
#107580 = CARTESIAN_POINT('Ctrl Pts',(-20.1579441016645,-32.4195514076664,
124.720194156336)) ;
#107581 = CARTESIAN_POINT('Ctrl Pts',(-20.3705294988008,-32.4293917251056,
124.572953421427)) ;
#107582 = CARTESIAN_POINT('Ctrl Pts',(-20.5582907454371,-32.4394214291631,
124.387976381289)) ;
#107583 = CARTESIAN_POINT('Ctrl Pts',(-20.7103679401522,-32.4494423858856,
124.172987380055)) ;
#107584 = CARTESIAN_POINT('Ctrl Pts',(-20.8216818684755,-32.4593089281892,
123.938794053993)) ;
#107585 = CARTESIAN_POINT('Ctrl Pts',(-20.8920616476232,-32.4693800281344,
123.68369126668)) ;
#107586 = CARTESIAN_POINT('Ctrl Pts',(-20.9165062443481,-32.4792221023119,
123.426199168448)) ;
#107587 = CARTESIAN_POINT('Ctrl Pts',(-20.8965853084581,-32.489182896899,
123.165204807569)) ;
#107588 = CARTESIAN_POINT('Ctrl Pts',(-20.8306424357435,-32.4992207697998,
122.909804904941)) ;
#107589 = CARTESIAN_POINT('Ctrl Pts',(-20.7235568389697,-32.5090950553439,
122.673410322637)) ;
#107590 = CARTESIAN_POINT('Ctrl Pts',(-20.5741779867741,-32.5191648057578,
122.455025135462)) ;
#107591 = CARTESIAN_POINT('Ctrl Pts',(-20.3935542879197,-32.5289980902925,
122.270197537221)) ;
#107592 = CARTESIAN_POINT('Ctrl Pts',(-20.1798353645603,-32.5390284310925,
122.115931069202)) ;
#107593 = CARTESIAN_POINT('Ctrl Pts',(-19.9421855351004,-32.5490603550921,
122.00178683298)) ;
#107594 = CARTESIAN_POINT('Ctrl Pts',(-19.6936476667716,-32.558888890028,
121.931549021349)) ;
#107595 = CARTESIAN_POINT('Ctrl Pts',(-19.4324328552306,-32.5688826677927,
121.904377531945)) ;
#107596 = CARTESIAN_POINT('Ctrl Pts',(-19.1696058306266,-32.5789103782782,
121.923555881501)) ;
#107597 = CARTESIAN_POINT('Ctrl Pts',(-18.9175767373303,-32.5887987891122,
121.986866859931)) ;
#107598 = CARTESIAN_POINT('Ctrl Pts',(-18.6780807546885,-32.5987756396477,
122.093498427882)) ;
#107599 = CARTESIAN_POINT('Ctrl Pts',(-18.4603518607013,-32.6087674361982,
122.240328150281)) ;
#107600 = CARTESIAN_POINT('Ctrl Pts',(-18.2708550108699,-32.6188034422919,
122.423729946212)) ;
#107601 = CARTESIAN_POINT('Ctrl Pts',(-18.1185911041515,-32.6286541765547,
122.633104887947)) ;
#107602 = CARTESIAN_POINT('Ctrl Pts',(-18.0029925436642,-32.6386454350829,
122.868805920096)) ;
#107603 = CARTESIAN_POINT('Ctrl Pts',(-17.9304420380305,-32.6485633299861,
123.119171510775)) ;
#107604 = CARTESIAN_POINT('Ctrl Pts',(-17.9020933992958,-32.6585914716491,
123.381149752802)) ;
#107605 = CARTESIAN_POINT('Ctrl Pts',(-17.9193058243358,-32.668476639765,
123.640357610124)) ;
#107606 = CARTESIAN_POINT('Ctrl Pts',(-17.9812965034311,-32.678466003271,
123.895448517053)) ;
#107607 = CARTESIAN_POINT('Ctrl Pts',(-18.0876915909878,-32.6885071382811,
124.136918337839)) ;
#107608 = CARTESIAN_POINT('Ctrl Pts',(-18.2309953121228,-32.6983398064691,
124.351926017212)) ;
#107609 = CARTESIAN_POINT('Ctrl Pts',(-18.4118383831064,-32.7083337094236,
124.542370821151)) ;
#107610 = CARTESIAN_POINT('Ctrl Pts',(-18.6240841226523,-32.7183629945081,
124.698627680039)) ;
#107611 = CARTESIAN_POINT('Ctrl Pts',(-18.8564392926519,-32.72823852295,124.814248563428)) ;
#107612 = CARTESIAN_POINT('Ctrl Pts',(-19.108357609205,-32.7382388055661,
124.888964680306)) ;
#107613 = CARTESIAN_POINT('Ctrl Pts',(-19.3671572036663,-32.7481508216231,
124.91875728521)) ;
#107614 = CARTESIAN_POINT('Ctrl Pts',(-19.6305640135305,-32.7581928969621,
124.903027332527)) ;
#107615 = CARTESIAN_POINT('Ctrl Pts',(-19.8836327781885,-32.7680927296182,
124.842652966499)) ;
#107616 = CARTESIAN_POINT('Ctrl Pts',(-20.1248258731489,-32.7780851301962,
124.738828307188)) ;
#107617 = CARTESIAN_POINT('Ctrl Pts',(-20.3449875884632,-32.7881191519556,
124.593707305374)) ;
#107618 = CARTESIAN_POINT('Ctrl Pts',(-20.5335942693008,-32.7979837627968,
124.415869847909)) ;
#107619 = CARTESIAN_POINT('Ctrl Pts',(-20.6909834644273,-32.807976162258,
124.205669296647)) ;
#107620 = CARTESIAN_POINT('Ctrl Pts',(-20.8094889241104,-32.8180081155909,
123.970176958909)) ;
#107621 = CARTESIAN_POINT('Ctrl Pts',(-20.8844377190578,-32.8278744745325,
123.721956675228)) ;
#107622 = CARTESIAN_POINT('Ctrl Pts',(-20.915945398737,-32.8378619500183,
123.46142651116)) ;
#107623 = CARTESIAN_POINT('Ctrl Pts',(-20.9019344264893,-32.8478068562068,
123.200421706081)) ;
#107624 = CARTESIAN_POINT('Ctrl Pts',(-20.8420906768917,-32.857851820867,
122.943349727935)) ;
#107625 = CARTESIAN_POINT('Ctrl Pts',(-20.7406060025703,-32.8677136277719,
122.704864899941)) ;
#107626 = CARTESIAN_POINT('Ctrl Pts',(-20.5978277819379,-32.8777063000777,
122.484507609776)) ;
#107627 = CARTESIAN_POINT('Ctrl Pts',(-20.4200501081656,-32.887634971023,
122.29350842051)) ;
#107628 = CARTESIAN_POINT('Ctrl Pts',(-20.2115950206297,-32.8975875132483,
122.135579849619)) ;
#107629 = CARTESIAN_POINT('Ctrl Pts',(-19.9777664676753,-32.9075888692442,
122.015514768882)) ;
#107630 = CARTESIAN_POINT('Ctrl Pts',(-19.7258893468962,-32.9176174815189,
121.938018230432)) ;
#107631 = CARTESIAN_POINT('Ctrl Pts',(-19.4686840401609,-32.9274818160684,
121.905586079296)) ;
#107632 = CARTESIAN_POINT('Ctrl Pts',(-19.2064279001672,-32.937474140145,
121.918060847947)) ;
#107633 = CARTESIAN_POINT('Ctrl Pts',(-18.9518780958547,-32.9474016325109,
121.9753702803)) ;
#107634 = CARTESIAN_POINT('Ctrl Pts',(-18.7087932303638,-32.9574289910617,
122.077002166667)) ;
#107635 = CARTESIAN_POINT('Ctrl Pts',(-18.489955040994,-32.9673154091128,
122.217103045502)) ;
#107636 = CARTESIAN_POINT('Ctrl Pts',(-18.2959274596919,-32.9773471438482,
122.395505831268)) ;
#107637 = CARTESIAN_POINT('Ctrl Pts',(-18.1379626696296,-32.9872287250915,
122.601670693589)) ;
#107638 = CARTESIAN_POINT('Ctrl Pts',(-18.0159920766457,-32.9972907031238,
122.836231079081)) ;
#107639 = CARTESIAN_POINT('Ctrl Pts',(-17.9381053441153,-33.0071477814855,
123.083316174594)) ;
#107640 = CARTESIAN_POINT('Ctrl Pts',(-17.9033191170827,-33.0171423545915,
123.343606451348)) ;
#107641 = CARTESIAN_POINT('Ctrl Pts',(-17.9140894742016,-33.0270681508791,
123.604259742982)) ;
#107642 = CARTESIAN_POINT('Ctrl Pts',(-17.9704344775412,-33.0370935180488,
123.861598418745)) ;
#107643 = CARTESIAN_POINT('Ctrl Pts',(-18.0692237668632,-33.0469895977027,
124.10217377657)) ;
#107644 = CARTESIAN_POINT('Ctrl Pts',(-18.2092225151571,-33.0569846774083,
124.324417544489)) ;
#107645 = CARTESIAN_POINT('Ctrl Pts',(-18.3865446424699,-33.0670097652241,
124.519256056386)) ;
#107646 = CARTESIAN_POINT('Ctrl Pts',(-18.6603047019322,-33.0801935875914,
124.731592942589)) ;
#107647 = CARTESIAN_POINT('Ctrl Pts',(-18.9863004972768,-33.0935157057373,
124.869727826814)) ;
#107648 = CARTESIAN_POINT('Ctrl Pts',(-19.3347071906035,-33.1068949153649,
124.91736369268)) ;
#107649 = CARTESIAN_POINT('Ctrl Pts',(-19.5930892399671,-33.1167331526091,
124.908073601812)) ;
#107650 = CARTESIAN_POINT('Ctrl Pts',(-19.8519494157696,-33.1268060758678,
124.852893187197)) ;
#107651 = CARTESIAN_POINT('Ctrl Pts',(-20.0920658651421,-33.1366627173229,
124.755687076181)) ;
#107652 = CARTESIAN_POINT('Ctrl Pts',(-20.3148680362745,-33.146648092829,
124.617083859547)) ;
#107653 = CARTESIAN_POINT('Ctrl Pts',(-20.5745145257892,-33.1599321242894,
124.383830412476)) ;
#107654 = CARTESIAN_POINT('Ctrl Pts',(-20.8154972870975,-33.1764509161598,
124.016642542163)) ;
#107655 = CARTESIAN_POINT('Ctrl Pts',(-20.9173126871173,-33.1932366331664,
123.582410699086)) ;
#107656 = CARTESIAN_POINT('Ctrl Pts',(-20.9065209327429,-33.2063497816754,
123.23789572756)) ;
#107657 = CARTESIAN_POINT('Ctrl Pts',(-20.8536580502004,-33.2163853307556,
122.979562774912)) ;
#107658 = CARTESIAN_POINT('Ctrl Pts',(-20.756198899228,-33.226401386935,122.735025148292)) ;
#107659 = CARTESIAN_POINT('Ctrl Pts',(-20.5747412709195,-33.239579422801,
122.44012359768)) ;
#107660 = CARTESIAN_POINT('Ctrl Pts',(-20.2550698779711,-33.2561812999881,
122.13585359014)) ;
#107661 = CARTESIAN_POINT('Ctrl Pts',(-19.7659385098357,-33.276244444604,
121.92353087025)) ;
#107662 = CARTESIAN_POINT('Ctrl Pts',(-19.2406100026333,-33.2960453346877,
121.890966023112)) ;
#107663 = CARTESIAN_POINT('Ctrl Pts',(-18.7318475042929,-33.3159884599664,
122.039373055726)) ;
#107664 = CARTESIAN_POINT('Ctrl Pts',(-18.3053808778122,-33.335886505086,
122.352108672438)) ;
#107665 = CARTESIAN_POINT('Ctrl Pts',(-18.0102720492938,-33.3557722647127,
122.790666346431)) ;
#107666 = CARTESIAN_POINT('Ctrl Pts',(-17.8822194175528,-33.3758374398926,
123.308319761272)) ;
#107667 = CARTESIAN_POINT('Ctrl Pts',(-17.9380299181868,-33.3956640829954,
123.832405348603)) ;
#107668 = CARTESIAN_POINT('Ctrl Pts',(-18.1688789178654,-33.4155727924438,
124.308378401184)) ;
#107669 = CARTESIAN_POINT('Ctrl Pts',(-18.5492341213423,-33.4355246294756,
124.678096369158)) ;
#107670 = CARTESIAN_POINT('Ctrl Pts',(-19.0344596868479,-33.4555331041787,
124.895580763503)) ;
#107671 = CARTESIAN_POINT('Ctrl Pts',(-19.559310109334,-33.4753345629402,
124.934655150607)) ;
#107672 = CARTESIAN_POINT('Ctrl Pts',(-20.0703244585672,-33.4952914511762,
124.792494318584)) ;
#107673 = CARTESIAN_POINT('Ctrl Pts',(-20.5020203609189,-33.5152752885903,
124.48310031143)) ;
#107674 = CARTESIAN_POINT('Ctrl Pts',(-20.8005186071669,-33.5350837278112,
124.049341107837)) ;
#107675 = CARTESIAN_POINT('Ctrl Pts',(-20.9347384844056,-33.5550694371914,
123.535554589158)) ;
#107676 = CARTESIAN_POINT('Ctrl Pts',(-20.885999032978,-33.5749389602067,
123.009493296955)) ;
#107677 = CARTESIAN_POINT('Ctrl Pts',(-20.6589346591422,-33.5949596993239,
122.528474746676)) ;
#107678 = CARTESIAN_POINT('Ctrl Pts',(-20.2856374495452,-33.6147637643009,
122.157109094538)) ;
#107679 = CARTESIAN_POINT('Ctrl Pts',(-19.8021945775454,-33.6348257280316,
121.932516764001)) ;
#107680 = CARTESIAN_POINT('Ctrl Pts',(-19.2768728976166,-33.6546589083201,
121.887399060282)) ;
#107681 = CARTESIAN_POINT('Ctrl Pts',(-18.7653006877327,-33.6745781056462,
122.023356004672)) ;
#107682 = CARTESIAN_POINT('Ctrl Pts',(-18.3305408655223,-33.6945161307595,
122.326341401192)) ;
#107683 = CARTESIAN_POINT('Ctrl Pts',(-18.0255479439294,-33.7143941768156,
122.757806077686)) ;
#107684 = CARTESIAN_POINT('Ctrl Pts',(-17.8853382109855,-33.7343789111036,
123.270057467913)) ;
#107685 = CARTESIAN_POINT('Ctrl Pts',(-17.9281121953389,-33.7542897277821,
123.797675941426)) ;
#107686 = CARTESIAN_POINT('Ctrl Pts',(-18.149539016089,-33.7742887033008,
124.280760470711)) ;
#107687 = CARTESIAN_POINT('Ctrl Pts',(-18.5185934989486,-33.794093623946,
124.656245044893)) ;
#107688 = CARTESIAN_POINT('Ctrl Pts',(-18.997373933869,-33.8140775842373,
124.885911032148)) ;
#107689 = CARTESIAN_POINT('Ctrl Pts',(-19.5234533792043,-33.8339637879612,
124.937945343118)) ;
#107690 = CARTESIAN_POINT('Ctrl Pts',(-20.0373357964093,-33.8539129662844,
124.807538175658)) ;
#107691 = CARTESIAN_POINT('Ctrl Pts',(-20.4747860229475,-33.8738147655239,
124.510187926931)) ;
#107692 = CARTESIAN_POINT('Ctrl Pts',(-20.785074811108,-33.8936933705763,
124.082527143795)) ;
#107693 = CARTESIAN_POINT('Ctrl Pts',(-20.9316937197507,-33.913725730302,
123.570655928487)) ;
#107694 = CARTESIAN_POINT('Ctrl Pts',(-20.9004897306885,-33.9303074562581,
123.131030340982)) ;
#107695 = CARTESIAN_POINT('Ctrl Pts',(-20.7882684765667,-33.943501626556,
122.802987512697)) ;
#107696 = CARTESIAN_POINT('Ctrl Pts',(-20.6197818577463,-33.9568138046492,
122.496403457349)) ;
#107697 = CARTESIAN_POINT('Ctrl Pts',(-20.3152140845606,-33.9733799842425,
122.178400060443)) ;
#107698 = CARTESIAN_POINT('Ctrl Pts',(-19.9192007524352,-33.9900081791027,
121.982335153568)) ;
#107699 = CARTESIAN_POINT('Ctrl Pts',(-19.576747692222,-34.0032967608125,
121.913686472833)) ;
#107700 = CARTESIAN_POINT('Ctrl Pts',(-19.3148922545305,-34.0132650089161,
121.907350759988)) ;
#107701 = CARTESIAN_POINT('Ctrl Pts',(-19.0572295014437,-34.0231797651722,
121.946049655107)) ;
#107702 = CARTESIAN_POINT('Ctrl Pts',(-18.8076465700997,-34.0331929158234,
122.029449840894)) ;
#107703 = CARTESIAN_POINT('Ctrl Pts',(-18.5765650235715,-34.0432056230254,
122.155268181664)) ;
#107704 = CARTESIAN_POINT('Ctrl Pts',(-18.3044971100231,-34.0564249117167,
122.371356277676)) ;
#107705 = CARTESIAN_POINT('Ctrl Pts',(-18.0412576763726,-34.0730435927147,
122.725882225526)) ;
#107706 = CARTESIAN_POINT('Ctrl Pts',(-17.9146105948963,-34.0896085004882,
123.147637150237)) ;
#107707 = CARTESIAN_POINT('Ctrl Pts',(-17.9043687423779,-34.103006972099,
123.499575218403)) ;
#107708 = CARTESIAN_POINT('Ctrl Pts',(-17.9415930567521,-34.112848227586,
123.755521607053)) ;
#107709 = CARTESIAN_POINT('Ctrl Pts',(-18.0233210818594,-34.1228345431742,
124.004856080344)) ;
#107710 = CARTESIAN_POINT('Ctrl Pts',(-18.1464135141684,-34.1327711507606,
124.235196202202)) ;
#107711 = CARTESIAN_POINT('Ctrl Pts',(-18.3095276453939,-34.1428210181289,
124.442869779362)) ;
#107712 = CARTESIAN_POINT('Ctrl Pts',(-18.5022256684344,-34.1526715128037,
124.615746588946)) ;
#107713 = CARTESIAN_POINT('Ctrl Pts',(-18.7243127245786,-34.1626433131982,
124.754775173138)) ;
#107714 = CARTESIAN_POINT('Ctrl Pts',(-18.9678384247013,-34.172639280224,
124.85337105192)) ;
#107715 = CARTESIAN_POINT('Ctrl Pts',(-19.2258575868419,-34.1826767396052,
124.908046464362)) ;
#107716 = CARTESIAN_POINT('Ctrl Pts',(-19.4843104936355,-34.1925174405059,
124.917404320897)) ;
#107717 = CARTESIAN_POINT('Ctrl Pts',(-19.7458819055264,-34.2025654617733,
124.881383594767)) ;
#107718 = CARTESIAN_POINT('Ctrl Pts',(-19.994593911652,-34.212512854856,124.80089995164)) ;
#107719 = CARTESIAN_POINT('Ctrl Pts',(-20.2250703242114,-34.2224230009024,
124.679611870156)) ;
#107720 = CARTESIAN_POINT('Ctrl Pts',(-20.4338613113264,-34.232481914752,
124.517543138453)) ;
#107721 = CARTESIAN_POINT('Ctrl Pts',(-20.6078020302223,-34.2423226850413,
124.32612918028)) ;
#107722 = CARTESIAN_POINT('Ctrl Pts',(-20.7492058428909,-34.2523855546199,
124.10270869485)) ;
#107723 = CARTESIAN_POINT('Ctrl Pts',(-20.847812874156,-34.2622798777504,
123.862089517083)) ;
#107724 = CARTESIAN_POINT('Ctrl Pts',(-20.904086498051,-34.2722216848449,
123.606994705096)) ;
#107725 = CARTESIAN_POINT('Ctrl Pts',(-20.9153820636518,-34.2822241958002,
123.344346331972)) ;
#107726 = CARTESIAN_POINT('Ctrl Pts',(-20.8803877326518,-34.2922589166186,
123.082992800506)) ;
#107727 = CARTESIAN_POINT('Ctrl Pts',(-20.8024516591558,-34.3021040941243,
122.836273538118)) ;
#107728 = CARTESIAN_POINT('Ctrl Pts',(-20.6816477236636,-34.3120888545254,
122.603389496116)) ;
#107729 = CARTESIAN_POINT('Ctrl Pts',(-20.5230276886739,-34.3220277608418,
122.395838571946)) ;
#107730 = CARTESIAN_POINT('Ctrl Pts',(-20.3287681107798,-34.3320699884775,
122.217255861103)) ;
#107731 = CARTESIAN_POINT('Ctrl Pts',(-20.1099811799375,-34.3419552000619,
122.077150319919)) ;
#107732 = CARTESIAN_POINT('Ctrl Pts',(-19.8676254465882,-34.3519541302638,
121.975725272331)) ;
#107733 = CARTESIAN_POINT('Ctrl Pts',(-19.6133933778577,-34.3618715531743,
121.918181079743)) ;
#107734 = CARTESIAN_POINT('Ctrl Pts',(-19.3496858460423,-34.371919485253,
121.905544647266)) ;
#107735 = CARTESIAN_POINT('Ctrl Pts',(-19.0921210729,-34.3817968610624,121.938080116923)) ;
#107736 = CARTESIAN_POINT('Ctrl Pts',(-18.8397327982224,-34.3918507542303,
122.016059532604)) ;
#107737 = CARTESIAN_POINT('Ctrl Pts',(-18.6083220936022,-34.4017443774836,
122.134691793531)) ;
#107738 = CARTESIAN_POINT('Ctrl Pts',(-18.3975365720198,-34.4118069711066,
122.294293213652)) ;
#107739 = CARTESIAN_POINT('Ctrl Pts',(-18.221449334239,-34.4216495450957,
122.48379388163)) ;
#107740 = CARTESIAN_POINT('Ctrl Pts',(-18.0783350961048,-34.4316403019786,
122.703865275403)) ;
#107741 = CARTESIAN_POINT('Ctrl Pts',(-17.9762751140817,-34.4415683637365,
122.943987568166)) ;
#107742 = CARTESIAN_POINT('Ctrl Pts',(-17.9166590105638,-34.4515563396257,
123.199611820243)) ;
#107743 = CARTESIAN_POINT('Ctrl Pts',(-17.9027062380668,-34.4615920039821,
123.462961293951)) ;
#107744 = CARTESIAN_POINT('Ctrl Pts',(-17.933717657988,-34.4714479424018,
123.720115766356)) ;
#107745 = CARTESIAN_POINT('Ctrl Pts',(-18.0095487390398,-34.4814434337987,
123.971573845822)) ;
#107746 = CARTESIAN_POINT('Ctrl Pts',(-18.1268227634101,-34.4913532387521,
124.204107141822)) ;
#107747 = CARTESIAN_POINT('Ctrl Pts',(-18.2839549689648,-34.5013654610189,
124.415151864782)) ;
#107748 = CARTESIAN_POINT('Ctrl Pts',(-18.4759941420734,-34.5113933417117,
124.595612359368)) ;
#107749 = CARTESIAN_POINT('Ctrl Pts',(-18.6924351175168,-34.5212497376943,
124.737885950365)) ;
#107750 = CARTESIAN_POINT('Ctrl Pts',(-18.9341417298191,-34.5312745348743,
124.842676381104)) ;
#107751 = CARTESIAN_POINT('Ctrl Pts',(-19.1906831675197,-34.5413054648581,
124.903315208341)) ;
#107752 = CARTESIAN_POINT('Ctrl Pts',(-19.4489213711089,-34.5511500673668,
124.918671165046)) ;
#107753 = CARTESIAN_POINT('Ctrl Pts',(-19.7098195492988,-34.5611409185909,
124.889221245161)) ;
#107754 = CARTESIAN_POINT('Ctrl Pts',(-19.9626496481009,-34.5711787516021,
124.814004405205)) ;
#107755 = CARTESIAN_POINT('Ctrl Pts',(-20.1942456922768,-34.5810231400675,
124.698703249967)) ;
#107756 = CARTESIAN_POINT('Ctrl Pts',(-20.4055430068826,-34.5910079444371,
124.543191888676)) ;
#107757 = CARTESIAN_POINT('Ctrl Pts',(-20.5859384433338,-34.6009474639199,
124.354242415491)) ;
#107758 = CARTESIAN_POINT('Ctrl Pts',(-20.7321627122965,-34.6109871949213,
124.134661855341)) ;
#107759 = CARTESIAN_POINT('Ctrl Pts',(-20.8365752606534,-34.6208753231676,
123.896695311078)) ;
#107760 = CARTESIAN_POINT('Ctrl Pts',(-20.8991832382357,-34.6308650483761,
123.64176102009)) ;
#107761 = CARTESIAN_POINT('Ctrl Pts',(-20.9163315622063,-34.6408228130776,
123.38064749872)) ;
#107762 = CARTESIAN_POINT('Ctrl Pts',(-20.8886454540213,-34.6507251544896,
123.121892083077)) ;
#107763 = CARTESIAN_POINT('Ctrl Pts',(-20.8153990760022,-34.660769350196,
122.868321304354)) ;
#107764 = CARTESIAN_POINT('Ctrl Pts',(-20.7008328237061,-34.6706767509553,
122.634510958014)) ;
#107765 = CARTESIAN_POINT('Ctrl Pts',(-20.5461918698344,-34.6806873508296,
122.421689518067)) ;
#107766 = CARTESIAN_POINT('Ctrl Pts',(-20.356218405505,-34.6907176467418,
122.238956157989)) ;
#107767 = CARTESIAN_POINT('Ctrl Pts',(-20.1414501229982,-34.7005724263915,
122.094270407089)) ;
#107768 = CARTESIAN_POINT('Ctrl Pts',(-19.9026628587002,-34.710529754609,
121.987240288001)) ;
#107769 = CARTESIAN_POINT('Ctrl Pts',(-19.6467491890605,-34.7205687875159,
121.923231809031)) ;
#107770 = CARTESIAN_POINT('Ctrl Pts',(-19.3879322276226,-34.7304418994052,
121.904452349722)) ;
#107771 = CARTESIAN_POINT('Ctrl Pts',(-19.1246574566547,-34.7405151844323,
121.931502979762)) ;
#107772 = CARTESIAN_POINT('Ctrl Pts',(-18.8762721005754,-34.7503355041691,
122.00174381202)) ;
#107773 = CARTESIAN_POINT('Ctrl Pts',(-18.6377474793643,-34.7604141695475,
122.116725949468)) ;
#107774 = CARTESIAN_POINT('Ctrl Pts',(-18.4274983885584,-34.7702657600313,
122.267892441874)) ;
#107775 = CARTESIAN_POINT('Ctrl Pts',(-18.2425373512532,-34.7803389103502,
122.457196688926)) ;
#107776 = CARTESIAN_POINT('Ctrl Pts',(-18.0966633908561,-34.7901812903253,
122.670815316167)) ;
#107777 = CARTESIAN_POINT('Ctrl Pts',(-17.9878295922109,-34.8001622665683,
122.909438203553)) ;
#107778 = CARTESIAN_POINT('Ctrl Pts',(-17.9222703050761,-34.8101785949236,
123.164375896419)) ;
#107779 = CARTESIAN_POINT('Ctrl Pts',(-17.9018852891634,-34.8200763919147,
123.423670303325)) ;
#107780 = CARTESIAN_POINT('Ctrl Pts',(-17.9266758265072,-34.8300889486468,
123.68563868434)) ;
#107781 = CARTESIAN_POINT('Ctrl Pts',(-17.9973050867461,-34.8401209834933,
123.939619669183)) ;
#107782 = CARTESIAN_POINT('Ctrl Pts',(-18.108211849478,-34.8499603843087,
124.173219295066)) ;
#107783 = CARTESIAN_POINT('Ctrl Pts',(-18.2612467515474,-34.8600261699603,
124.388936498966)) ;
#107784 = CARTESIAN_POINT('Ctrl Pts',(-18.4462622689806,-34.8699166250749,
124.571521646405)) ;
#107785 = CARTESIAN_POINT('Ctrl Pts',(-18.6620141059748,-34.8799087437107,
124.721167028218)) ;
#107786 = CARTESIAN_POINT('Ctrl Pts',(-18.8998816261791,-34.8898715704737,
124.830535614185)) ;
#107787 = CARTESIAN_POINT('Ctrl Pts',(-19.1514976451602,-34.8997758537466,
124.897195876227)) ;
#107788 = CARTESIAN_POINT('Ctrl Pts',(-19.4149200232022,-34.9098362876937,
124.919269231619)) ;
#107789 = CARTESIAN_POINT('Ctrl Pts',(-19.6725159065114,-34.9196768403669,
124.896117457243)) ;
#107790 = CARTESIAN_POINT('Ctrl Pts',(-19.9278288963677,-34.9297390603126,
124.82741158987)) ;
#107791 = CARTESIAN_POINT('Ctrl Pts',(-20.1633279388494,-34.9396361995912,
124.71699231362)) ;
#107792 = CARTESIAN_POINT('Ctrl Pts',(-20.3772931771489,-34.9495673917262,
124.567567370087)) ;
#107793 = CARTESIAN_POINT('Ctrl Pts',(-20.5639178571973,-34.9596095463713,
124.380994866377)) ;
#107794 = CARTESIAN_POINT('Ctrl Pts',(-20.7131614275899,-34.9694963073906,
124.16829573498)) ;
#107795 = CARTESIAN_POINT('Ctrl Pts',(-20.8247390624128,-34.9794956091078,
123.930428506013)) ;
#107796 = CARTESIAN_POINT('Ctrl Pts',(-20.8929709285114,-34.9894164072746,
123.678769811225)) ;
#107797 = CARTESIAN_POINT('Ctrl Pts',(-20.9167602208572,-34.9994504608713,
123.416190287807)) ;
#107798 = CARTESIAN_POINT('Ctrl Pts',(-20.894992050459,-35.0093735784377,
123.156290901073)) ;
#107799 = CARTESIAN_POINT('Ctrl Pts',(-20.8274967913366,-35.0194297019368,
122.900819039929)) ;
#107800 = CARTESIAN_POINT('Ctrl Pts',(-20.7190767997193,-35.0292751435917,
122.665891135999)) ;
#107801 = CARTESIAN_POINT('Ctrl Pts',(-20.570484633187,-35.0392374447158,
122.450367538193)) ;
#107802 = CARTESIAN_POINT('Ctrl Pts',(-20.385235603018,-35.0492659239909,
122.262899380844)) ;
#107803 = CARTESIAN_POINT('Ctrl Pts',(-20.1728579932209,-35.0591762775006,
122.112184527522)) ;
#107804 = CARTESIAN_POINT('Ctrl Pts',(-19.9372295987882,-35.0691111496778,
121.99973320743)) ;
#107805 = CARTESIAN_POINT('Ctrl Pts',(-19.6829151498438,-35.0791522872635,
121.929396810072)) ;
#107806 = CARTESIAN_POINT('Ctrl Pts',(-19.4242729791093,-35.0890394364781,
121.904487487386)) ;
#107807 = CARTESIAN_POINT('Ctrl Pts',(-19.1624800113372,-35.0990316712291,
121.924641589573)) ;
#107808 = CARTESIAN_POINT('Ctrl Pts',(-18.9092594100541,-35.1089803767921,
121.989743199417)) ;
#107809 = CARTESIAN_POINT('Ctrl Pts',(-18.6713636061917,-35.1189164452158,
122.097326151971)) ;
#107810 = CARTESIAN_POINT('Ctrl Pts',(-18.454478724191,-35.1289021294316,
122.24509401698)) ;
#107811 = CARTESIAN_POINT('Ctrl Pts',(-18.2658365440842,-35.1389425560002,
122.429551256226)) ;
#107812 = CARTESIAN_POINT('Ctrl Pts',(-18.1148079749497,-35.148781669464,
122.639425740109)) ;
#107813 = CARTESIAN_POINT('Ctrl Pts',(-17.9998053864142,-35.1588114036398,
122.8765872657)) ;
#107814 = CARTESIAN_POINT('Ctrl Pts',(-17.928444715581,-35.1688335031457,
123.130103094815)) ;
#107815 = CARTESIAN_POINT('Ctrl Pts',(-17.9019396037341,-35.1787019430391,
123.388097438941)) ;
#107816 = CARTESIAN_POINT('Ctrl Pts',(-17.9210166574151,-35.1887708077248,
123.651983894416)) ;
#107817 = CARTESIAN_POINT('Ctrl Pts',(-17.984171428927,-35.1986134808234,
123.902820263154)) ;
#107818 = CARTESIAN_POINT('Ctrl Pts',(-18.0903067406265,-35.2085741149858,
124.142086367296)) ;
#107819 = CARTESIAN_POINT('Ctrl Pts',(-18.2379359596469,-35.2186120306639,
124.360681074975)) ;
#107820 = CARTESIAN_POINT('Ctrl Pts',(-18.4179730017366,-35.2284863055234,
124.547593591424)) ;
#107821 = CARTESIAN_POINT('Ctrl Pts',(-18.6318350939192,-35.2385560558985,
124.703379138659)) ;
#107822 = CARTESIAN_POINT('Ctrl Pts',(-18.8639071984874,-35.248389351273,
124.817084015315)) ;
#107823 = CARTESIAN_POINT('Ctrl Pts',(-19.11693425595,-35.2584196487526,124.890913312346)) ;
#107824 = CARTESIAN_POINT('Ctrl Pts',(-19.3790865211221,-35.2684517351941,
124.918922276281)) ;
#107825 = CARTESIAN_POINT('Ctrl Pts',(-19.6367832596118,-35.278279663683,
124.901921160071)) ;
#107826 = CARTESIAN_POINT('Ctrl Pts',(-19.8920793713658,-35.2882757047938,
124.840064446587)) ;
#107827 = CARTESIAN_POINT('Ctrl Pts',(-20.1332785051419,-35.298301516895,
124.734035625676)) ;
#107828 = CARTESIAN_POINT('Ctrl Pts',(-20.3495593000044,-35.3081887517898,
124.590041155415)) ;
#107829 = CARTESIAN_POINT('Ctrl Pts',(-20.5395393226793,-35.3181656180008,
124.409385624439)) ;
#107830 = CARTESIAN_POINT('Ctrl Pts',(-20.6955864544945,-35.3281585618726,
124.198129769349)) ;
#107831 = CARTESIAN_POINT('Ctrl Pts',(-20.8127836789868,-35.338196484544,
123.96183104994)) ;
#107832 = CARTESIAN_POINT('Ctrl Pts',(-20.8861530777465,-35.3480449488057,
123.713620356544)) ;
#107833 = CARTESIAN_POINT('Ctrl Pts',(-20.9161936009875,-35.3580368155497,
123.45280719969)) ;
#107834 = CARTESIAN_POINT('Ctrl Pts',(-20.9007516754071,-35.3679545475909,
123.192603234289)) ;
#107835 = CARTESIAN_POINT('Ctrl Pts',(-20.8397730358761,-35.3779827324862,
122.936247392291)) ;
#107836 = CARTESIAN_POINT('Ctrl Pts',(-20.7367882330966,-35.387867890535,
122.6977541823)) ;
#107837 = CARTESIAN_POINT('Ctrl Pts',(-20.5929867212805,-35.3978572510767,
122.478128741953)) ;
#107838 = CARTESIAN_POINT('Ctrl Pts',(-20.41190098255,-35.4078984080111,122.286202465482)) ;
#107839 = CARTESIAN_POINT('Ctrl Pts',(-20.204896171008,-35.4177309914662,
122.131565664669)) ;
#107840 = CARTESIAN_POINT('Ctrl Pts',(-19.9707294456194,-35.4277252114282,
122.012642748326)) ;
#107841 = CARTESIAN_POINT('Ctrl Pts',(-19.7184528815529,-35.4377533132155,
121.936438351148)) ;
#107842 = CARTESIAN_POINT('Ctrl Pts',(-19.4606890511142,-35.4476332578386,
121.905289560067)) ;
#107843 = CARTESIAN_POINT('Ctrl Pts',(-19.1985341207604,-35.4576235843956,
121.919121980411)) ;
#107844 = CARTESIAN_POINT('Ctrl Pts',(-18.9440062626121,-35.4675645160499,
121.977973922439)) ;
#107845 = CARTESIAN_POINT('Ctrl Pts',(-18.702288047515,-35.4775516345528,
122.080260803996)) ;
#107846 = CARTESIAN_POINT('Ctrl Pts',(-18.4812400627169,-35.48758496745,122.22395297179)) ;
#107847 = CARTESIAN_POINT('Ctrl Pts',(-18.2913303413505,-35.4974510718947,
122.400506732355)) ;
#107848 = CARTESIAN_POINT('Ctrl Pts',(-18.1317782703175,-35.5075171857751,
122.611460438523)) ;
#107849 = CARTESIAN_POINT('Ctrl Pts',(-18.0137583413935,-35.5173731975435,
122.842035312612)) ;
#107850 = CARTESIAN_POINT('Ctrl Pts',(-17.9357612978985,-35.5273679011748,
123.092829842602)) ;
#107851 = CARTESIAN_POINT('Ctrl Pts',(-17.9029316319615,-35.5373992368997,
123.354395189712)) ;
#107852 = CARTESIAN_POINT('Ctrl Pts',(-17.9153901928163,-35.5472657621033,
123.613386874804)) ;
#107853 = CARTESIAN_POINT('Ctrl Pts',(-17.9729086714527,-35.5572531901491,
123.869433841305)) ;
#107854 = CARTESIAN_POINT('Ctrl Pts',(-18.0734780654367,-35.5671981198355,
124.110692535374)) ;
#107855 = CARTESIAN_POINT('Ctrl Pts',(-18.2159187908367,-35.5772430379441,
124.332902903788)) ;
#107856 = CARTESIAN_POINT('Ctrl Pts',(-18.3913816758931,-35.587105007558,
124.523661515827)) ;
#107857 = CARTESIAN_POINT('Ctrl Pts',(-18.5996689527745,-35.5970970755792,
124.683509885584)) ;
#107858 = CARTESIAN_POINT('Ctrl Pts',(-18.8311813513176,-35.6070280009538,
124.804001201604)) ;
#107859 = CARTESIAN_POINT('Ctrl Pts',(-19.0804266703559,-35.6169786291772,
124.883027052009)) ;
#107860 = CARTESIAN_POINT('Ctrl Pts',(-19.3409266350383,-35.6269788682363,
124.917904087463)) ;
#107861 = CARTESIAN_POINT('Ctrl Pts',(-19.6042114461551,-35.6370073236055,
124.906610760373)) ;
#107862 = CARTESIAN_POINT('Ctrl Pts',(-19.8574743469857,-35.6468733581888,
124.851072017746)) ;
#107863 = CARTESIAN_POINT('Ctrl Pts',(-20.1004455793922,-35.6568656799362,
124.751552866436)) ;
#107864 = CARTESIAN_POINT('Ctrl Pts',(-20.3211734802122,-35.6667979696132,
124.612212133575)) ;
#107865 = CARTESIAN_POINT('Ctrl Pts',(-20.5158560562824,-35.676799614584,
124.435643769386)) ;
#107866 = CARTESIAN_POINT('Ctrl Pts',(-20.7301399819969,-35.690112248,124.159089650513)) ;
#107867 = CARTESIAN_POINT('Ctrl Pts',(-20.8667522508955,-35.7033439973816,
123.835042103651)) ;
#107868 = CARTESIAN_POINT('Ctrl Pts',(-20.9147585986983,-35.7166672621986,
123.488226045327)) ;
#107869 = CARTESIAN_POINT('Ctrl Pts',(-20.9055563612278,-35.7265429684163,
123.228855650435)) ;
#107870 = CARTESIAN_POINT('Ctrl Pts',(-20.8511781735933,-35.7365325595163,
122.972062262268)) ;
#107871 = CARTESIAN_POINT('Ctrl Pts',(-20.7537899401684,-35.7464596559717,
122.730015204372)) ;
#107872 = CARTESIAN_POINT('Ctrl Pts',(-20.6145469935305,-35.7564848044763,
122.5063968681)) ;
#107873 = CARTESIAN_POINT('Ctrl Pts',(-20.440953874785,-35.766380458623,122.312743006268)) ;
#107874 = CARTESIAN_POINT('Ctrl Pts',(-20.2344106821349,-35.7763839930012,
122.150158260611)) ;
#107875 = CARTESIAN_POINT('Ctrl Pts',(-20.0031308315218,-35.7863691314413,
122.026126833219)) ;
#107876 = CARTESIAN_POINT('Ctrl Pts',(-19.7525288450674,-35.7964050560366,
121.943988637764)) ;
#107877 = CARTESIAN_POINT('Ctrl Pts',(-19.4963068640577,-35.8062563314643,
121.906992639844)) ;
#107878 = CARTESIAN_POINT('Ctrl Pts',(-19.2338168958201,-35.8162485926257,
121.914412989473)) ;
#107879 = CARTESIAN_POINT('Ctrl Pts',(-18.9755341093132,-35.8262884766433,
121.968199019845)) ;
#107880 = CARTESIAN_POINT('Ctrl Pts',(-18.7352349967454,-35.8361232511457,
122.063423387653)) ;
#107881 = CARTESIAN_POINT('Ctrl Pts',(-18.5097250642947,-35.846199632166,
122.202132211928)) ;
#107882 = CARTESIAN_POINT('Ctrl Pts',(-18.3161426476442,-35.8560459053166,
122.373872640162)) ;
#107883 = CARTESIAN_POINT('Ctrl Pts',(-18.0973698099313,-35.8694104266019,
122.648612771073)) ;
#107884 = CARTESIAN_POINT('Ctrl Pts',(-17.9574290045863,-35.8826166710363,
122.970502256562)) ;
#107885 = CARTESIAN_POINT('Ctrl Pts',(-17.9048223282448,-35.8958816257135,
123.315086227926)) ;
#107886 = CARTESIAN_POINT('Ctrl Pts',(-17.9110124910834,-35.9059139062652,
123.578657913582)) ;
#107887 = CARTESIAN_POINT('Ctrl Pts',(-17.9622121074336,-35.9158226397831,
123.833960372486)) ;
#107888 = CARTESIAN_POINT('Ctrl Pts',(-18.0566097123555,-35.9257601906506,
124.077460099996)) ;
#107889 = CARTESIAN_POINT('Ctrl Pts',(-18.1932802459593,-35.9357900382445,
124.302802968924)) ;
#107890 = CARTESIAN_POINT('Ctrl Pts',(-18.4222315307494,-35.949025178165,
124.564734759773)) ;
#107891 = CARTESIAN_POINT('Ctrl Pts',(-18.7900589109443,-35.9656936425361,
124.81140834834)) ;
#107892 = CARTESIAN_POINT('Ctrl Pts',(-19.3028156410116,-35.98556465441,124.938691204447)) ;
#107893 = CARTESIAN_POINT('Ctrl Pts',(-19.7442837615988,-36.002271738793,
124.892072174902)) ;
#107894 = CARTESIAN_POINT('Ctrl Pts',(-20.0675701271114,-36.0154490201036,
124.767809053067)) ;
#107895 = CARTESIAN_POINT('Ctrl Pts',(-20.3669739906252,-36.0287164806177,
124.589185848761)) ;
#107896 = CARTESIAN_POINT('Ctrl Pts',(-20.6747981802351,-36.0453303713049,
124.272594034034)) ;
#107897 = CARTESIAN_POINT('Ctrl Pts',(-20.8925558078183,-36.0652791707323,
123.789111611109)) ;
#107898 = CARTESIAN_POINT('Ctrl Pts',(-20.9320991006498,-36.0852002822632,
123.261193418432)) ;
#107899 = CARTESIAN_POINT('Ctrl Pts',(-20.7905276952024,-36.1050667304361,
122.752423768458)) ;
#107900 = CARTESIAN_POINT('Ctrl Pts',(-20.4811904266978,-36.1250930770532,
122.319344712288)) ;
#107901 = CARTESIAN_POINT('Ctrl Pts',(-20.0460525668454,-36.1449551214427,
122.020296381209)) ;
#107902 = CARTESIAN_POINT('Ctrl Pts',(-19.5332139354113,-36.1649004241238,
121.886365238136)) ;
#107903 = CARTESIAN_POINT('Ctrl Pts',(-19.0067003117622,-36.1847957311827,
121.935446627592)) ;
#107904 = CARTESIAN_POINT('Ctrl Pts',(-18.528185304181,-36.2046890013503,
122.160367750237)) ;
#107905 = CARTESIAN_POINT('Ctrl Pts',(-18.153899886363,-36.2246545940308,
122.536490933432)) ;
#107906 = CARTESIAN_POINT('Ctrl Pts',(-17.9310800836286,-36.2445299177156,
123.015484089359)) ;
#107907 = CARTESIAN_POINT('Ctrl Pts',(-17.8843234008794,-36.2645049802905,
123.544349544099)) ;
#107908 = CARTESIAN_POINT('Ctrl Pts',(-18.0214642489446,-36.2844573899217,
124.056610899457)) ;
#107909 = CARTESIAN_POINT('Ctrl Pts',(-18.3225697130406,-36.3042934441578,
124.489372589314)) ;
#107910 = CARTESIAN_POINT('Ctrl Pts',(-18.7560217521226,-36.3242713555753,
124.796062315731)) ;
#107911 = CARTESIAN_POINT('Ctrl Pts',(-19.2667087137698,-36.3441894050788,
124.935393803099)) ;
#107912 = CARTESIAN_POINT('Ctrl Pts',(-19.7932215456907,-36.3640575488469,
124.893573225547)) ;
#107913 = CARTESIAN_POINT('Ctrl Pts',(-20.2777203069031,-36.3841084054342,
124.671934669039)) ;
#107914 = CARTESIAN_POINT('Ctrl Pts',(-20.6529715193524,-36.4038888418901,
124.303513156347)) ;
#107915 = CARTESIAN_POINT('Ctrl Pts',(-20.8834919669097,-36.4239188975679,
123.823777378833)) ;
#107916 = CARTESIAN_POINT('Ctrl Pts',(-20.9351946084238,-36.4438000027427,
123.297815458133)) ;
#107917 = CARTESIAN_POINT('Ctrl Pts',(-20.805795972203,-36.4636804651105,
122.785569836397)) ;
#107918 = CARTESIAN_POINT('Ctrl Pts',(-20.5076408598673,-36.4836656122549,
122.345949379548)) ;
#107919 = CARTESIAN_POINT('Ctrl Pts',(-20.0793293333916,-36.5035561907912,
122.036043896619)) ;
#107920 = CARTESIAN_POINT('Ctrl Pts',(-19.5711616761895,-36.5234502106656,
121.889982105805)) ;
#107921 = CARTESIAN_POINT('Ctrl Pts',(-19.0429949662243,-36.543371655392,
121.926004249393)) ;
#107922 = CARTESIAN_POINT('Ctrl Pts',(-18.5587989821738,-36.5632697934474,
122.139082068904)) ;
#107923 = CARTESIAN_POINT('Ctrl Pts',(-18.1739452502748,-36.5833405486635,
122.508343006404)) ;
#107924 = CARTESIAN_POINT('Ctrl Pts',(-17.9412347696197,-36.6031260987147,
122.980047031886)) ;
#107925 = CARTESIAN_POINT('Ctrl Pts',(-17.8816250601364,-36.6231091735921,
123.507711042693)) ;
#107926 = CARTESIAN_POINT('Ctrl Pts',(-18.0060238701936,-36.643018256238,
124.02203763036)) ;
#107927 = CARTESIAN_POINT('Ctrl Pts',(-18.2964921624861,-36.6628768153608,
124.46281239647)) ;
#107928 = CARTESIAN_POINT('Ctrl Pts',(-18.7241093152604,-36.6829202591995,
124.780336057724)) ;
#107929 = CARTESIAN_POINT('Ctrl Pts',(-19.1443370740696,-36.6994203239287,
124.906201446965)) ;
#107930 = CARTESIAN_POINT('Ctrl Pts',(-19.4959912524148,-36.7128100637776,
124.916825364665)) ;
#107931 = CARTESIAN_POINT('Ctrl Pts',(-19.7523753879943,-36.722666964986,
124.879659208056)) ;
#107932 = CARTESIAN_POINT('Ctrl Pts',(-20.0018654730257,-36.7326584908325,
124.797967905292)) ;
#107933 = CARTESIAN_POINT('Ctrl Pts',(-20.2319502039447,-36.7425831712835,
124.675071044301)) ;
#107934 = CARTESIAN_POINT('Ctrl Pts',(-20.4389774416339,-36.7525937613279,
124.512826396115)) ;
#107935 = CARTESIAN_POINT('Ctrl Pts',(-20.6721055369594,-36.7658530220315,
124.253740187377)) ;
#107936 = CARTESIAN_POINT('Ctrl Pts',(-20.8329407184448,-36.7792040971818,
123.937561551758)) ;
#107937 = CARTESIAN_POINT('Ctrl Pts',(-20.9051385764094,-36.7924104064166,
123.598034123751)) ;
#107938 = CARTESIAN_POINT('Ctrl Pts',(-20.9148485286139,-36.8023972400069,
123.335815354596)) ;
#107939 = CARTESIAN_POINT('Ctrl Pts',(-20.8791206018551,-36.812349967503,
123.076674163905)) ;
#107940 = CARTESIAN_POINT('Ctrl Pts',(-20.7979834514624,-36.8223980643446,
122.82542587721)) ;
#107941 = CARTESIAN_POINT('Ctrl Pts',(-20.6772389440555,-36.8322395212164,
122.596690972918)) ;
#107942 = CARTESIAN_POINT('Ctrl Pts',(-20.5167636139699,-36.8422257881299,
122.389100234004)) ;
#107943 = CARTESIAN_POINT('Ctrl Pts',(-20.3236708136036,-36.8521623890303,
122.213249918781)) ;
#107944 = CARTESIAN_POINT('Ctrl Pts',(-20.1004488354142,-36.8622123318174,
122.072155044208)) ;
#107945 = CARTESIAN_POINT('Ctrl Pts',(-19.8610080268969,-36.8720625315031,
121.973756839385)) ;
#107946 = CARTESIAN_POINT('Ctrl Pts',(-19.6051634992664,-36.8820354364352,
121.917073652596)) ;
#107947 = CARTESIAN_POINT('Ctrl Pts',(-19.3426292753776,-36.8920338109148,
121.905727253449)) ;
#107948 = CARTESIAN_POINT('Ctrl Pts',(-19.0816097097037,-36.9020539847848,
121.940395605371)) ;
#107949 = CARTESIAN_POINT('Ctrl Pts',(-18.8334770246781,-36.9119550287268,
122.018703957336)) ;
#107950 = CARTESIAN_POINT('Ctrl Pts',(-18.6004816712349,-36.9219438324511,
122.139601545774)) ;
#107951 = CARTESIAN_POINT('Ctrl Pts',(-18.3926262261631,-36.9319092992829,
122.298887280516)) ;
#107952 = CARTESIAN_POINT('Ctrl Pts',(-18.2161960419998,-36.9418128615559,
122.490246883237)) ;
#107953 = CARTESIAN_POINT('Ctrl Pts',(-18.0736583691123,-36.9518735394339,
122.71287674179)) ;
#107954 = CARTESIAN_POINT('Ctrl Pts',(-17.9738349551272,-36.9617138373834,
122.951466470919)) ;
#107955 = CARTESIAN_POINT('Ctrl Pts',(-17.9153712422102,-36.9717768322928,
123.209332478486)) ;
#107956 = CARTESIAN_POINT('Ctrl Pts',(-17.9029963259701,-36.9816711264399,
123.469077685749)) ;
#107957 = CARTESIAN_POINT('Ctrl Pts',(-17.9353566103363,-36.9916129241368,
123.728293552518)) ;
#107958 = CARTESIAN_POINT('Ctrl Pts',(-18.0126312483315,-37.0016155016659,
123.979571905711)) ;
#107959 = CARTESIAN_POINT('Ctrl Pts',(-18.1330836135204,-37.011649965587,
124.214133981755)) ;
#107960 = CARTESIAN_POINT('Ctrl Pts',(-18.2891332508582,-37.0214961041081,
124.420537477893)) ;
#107961 = CARTESIAN_POINT('Ctrl Pts',(-18.4808302087652,-37.0314772773451,
124.599534219672)) ;
#107962 = CARTESIAN_POINT('Ctrl Pts',(-18.7001169445162,-37.0414295713023,
124.742077120558)) ;
#107963 = CARTESIAN_POINT('Ctrl Pts',(-18.9418253000939,-37.0514283664369,
124.845176341214)) ;
#107964 = CARTESIAN_POINT('Ctrl Pts',(-19.1988750598665,-37.0614674746977,
124.904479146326)) ;
#107965 = CARTESIAN_POINT('Ctrl Pts',(-19.4566988811573,-37.0712924161369,
124.918510704658)) ;
#107966 = CARTESIAN_POINT('Ctrl Pts',(-19.7190563874513,-37.0813471032113,
124.887274074788)) ;
#107967 = CARTESIAN_POINT('Ctrl Pts',(-19.969084030359,-37.0912899081514,
124.811372573199)) ;
#107968 = CARTESIAN_POINT('Ctrl Pts',(-20.2015786291338,-37.1011936941479,
124.694388313774)) ;
#107969 = CARTESIAN_POINT('Ctrl Pts',(-20.4131234868588,-37.1112405107127,
124.536454481788)) ;
#107970 = CARTESIAN_POINT('Ctrl Pts',(-20.5915236174634,-37.1211360301914,
124.347197240255)) ;
#107971 = CARTESIAN_POINT('Ctrl Pts',(-20.7367129157612,-37.1311981155158,
124.126248181755)) ;
#107972 = CARTESIAN_POINT('Ctrl Pts',(-20.8392138555914,-37.1410408264737,
123.888736566478)) ;
#107973 = CARTESIAN_POINT('Ctrl Pts',(-20.9004065395447,-37.1510315437798,
123.633455653351)) ;
#107974 = CARTESIAN_POINT('Ctrl Pts',(-20.9162024817298,-37.1609596268764,
123.373022214613)) ;
#107975 = CARTESIAN_POINT('Ctrl Pts',(-20.8868147103716,-37.1709475569881,
123.112189441755)) ;
#107976 = CARTESIAN_POINT('Ctrl Pts',(-20.8118080923206,-37.1809833831154,
122.859358313321)) ;
#107977 = CARTESIAN_POINT('Ctrl Pts',(-20.6965192508004,-37.190838720229,
122.627429700826)) ;
#107978 = CARTESIAN_POINT('Ctrl Pts',(-20.5408489070488,-37.2008364550792,
122.415819448535)) ;
#107979 = CARTESIAN_POINT('Ctrl Pts',(-20.3525399698651,-37.2107443590637,
122.235991135141)) ;
#107980 = CARTESIAN_POINT('Ctrl Pts',(-20.1338594498065,-37.2207554336121,
122.08972321814)) ;
#107981 = CARTESIAN_POINT('Ctrl Pts',(-19.8924886139935,-37.2307832891477,
121.98396490072)) ;
#107982 = CARTESIAN_POINT('Ctrl Pts',(-19.640883973354,-37.240640883053,121.922329058917)) ;
#107983 = CARTESIAN_POINT('Ctrl Pts',(-19.3779934736836,-37.2506675698911,
121.904487880375)) ;
#107984 = CARTESIAN_POINT('Ctrl Pts',(-19.1160127976239,-37.2606962390448,
121.933223522823)) ;
#107985 = CARTESIAN_POINT('Ctrl Pts',(-18.8675153981344,-37.2705414473262,
122.00519292378)) ;
#107986 = CARTESIAN_POINT('Ctrl Pts',(-18.6315296424855,-37.2805321362893,
122.120275185745)) ;
#107987 = CARTESIAN_POINT('Ctrl Pts',(-18.4184607715103,-37.2905700125716,
122.275783232046)) ;
#107988 = CARTESIAN_POINT('Ctrl Pts',(-18.2388199959597,-37.3004143902138,
122.46195567079)) ;
#107989 = CARTESIAN_POINT('Ctrl Pts',(-18.0917661888766,-37.3103991946052,
122.67922397644)) ;
#107990 = CARTESIAN_POINT('Ctrl Pts',(-17.9850247084905,-37.3203387248238,
122.917657976795)) ;
#107991 = CARTESIAN_POINT('Ctrl Pts',(-17.9207357281408,-37.3303784128607,
123.173516578115)) ;
#107992 = CARTESIAN_POINT('Ctrl Pts',(-17.9020031979114,-37.340266702229,
123.432709689292)) ;
#107993 = CARTESIAN_POINT('Ctrl Pts',(-17.9283346512609,-37.3502558259138,
123.693880259981)) ;
#107994 = CARTESIAN_POINT('Ctrl Pts',(-17.9996040811772,-37.3602158355884,
123.945724561577)) ;
#107995 = CARTESIAN_POINT('Ctrl Pts',(-18.1122851368062,-37.3701162652927,
124.180239595587)) ;
#107996 = CARTESIAN_POINT('Ctrl Pts',(-18.2661582318279,-37.3801593466994,
124.394649731977)) ;
#107997 = CARTESIAN_POINT('Ctrl Pts',(-18.4523869695707,-37.390066740607,
124.576615327164)) ;
#107998 = CARTESIAN_POINT('Ctrl Pts',(-18.6693614592825,-37.4000784715962,
124.725422533845)) ;
#107999 = CARTESIAN_POINT('Ctrl Pts',(-18.9095896394235,-37.410110689311,
124.834045138727)) ;
#108000 = CARTESIAN_POINT('Ctrl Pts',(-19.1603449861125,-37.4199631985572,
124.898470131179)) ;
#108001 = CARTESIAN_POINT('Ctrl Pts',(-19.4211984555545,-37.4299211351002,
124.919402923825)) ;
#108002 = CARTESIAN_POINT('Ctrl Pts',(-19.6837710962987,-37.4399600051085,
124.894054750711)) ;
#108003 = CARTESIAN_POINT('Ctrl Pts',(-19.9339449292123,-37.4498331602667,
124.825117088921)) ;
#108004 = CARTESIAN_POINT('Ctrl Pts',(-20.1729772826254,-37.4599064351164,
124.711500299774)) ;
#108005 = CARTESIAN_POINT('Ctrl Pts',(-20.3835223993662,-37.4697267522938,
124.562169109503)) ;
#108006 = CARTESIAN_POINT('Ctrl Pts',(-20.5697990348495,-37.4798054380873,
124.373977558108)) ;
#108007 = CARTESIAN_POINT('Ctrl Pts',(-20.7173197608685,-37.4896569494704,
124.16115630228)) ;
#108008 = CARTESIAN_POINT('Ctrl Pts',(-20.8282432976094,-37.499730395777,
123.920852463059)) ;
#108009 = CARTESIAN_POINT('Ctrl Pts',(-20.8942031840611,-37.5095716709017,
123.670756297551)) ;
#108010 = CARTESIAN_POINT('Ctrl Pts',(-20.9168622044648,-37.5195567705585,
123.409363382907)) ;
#108011 = CARTESIAN_POINT('Ctrl Pts',(-20.8933700263742,-37.5295642466928,
123.147408998468)) ;
#108012 = CARTESIAN_POINT('Ctrl Pts',(-20.8255717865833,-37.5394868344017,
122.895635106772)) ;
#108013 = CARTESIAN_POINT('Ctrl Pts',(-20.7147447437026,-37.5494734386751,
122.657720062072)) ;
#108014 = CARTESIAN_POINT('Ctrl Pts',(-20.5631062336304,-37.5595135670092,
122.441830793233)) ;
#108015 = CARTESIAN_POINT('Ctrl Pts',(-20.3803844725439,-37.5693530015426,
122.258841212078)) ;
#108016 = CARTESIAN_POINT('Ctrl Pts',(-20.1640074372698,-37.5794170560336,
122.106822876259)) ;
#108017 = CARTESIAN_POINT('Ctrl Pts',(-19.9285377911858,-37.5893079752708,
121.996693203954)) ;
#108018 = CARTESIAN_POINT('Ctrl Pts',(-19.6751435403959,-37.5992999685768,
121.927901435656)) ;
#108019 = CARTESIAN_POINT('Ctrl Pts',(-19.4143879012816,-37.6092628325361,
121.904463322897)) ;
#108020 = CARTESIAN_POINT('Ctrl Pts',(-19.1549736893451,-37.6191670923539,
121.925872135699)) ;
#108021 = CARTESIAN_POINT('Ctrl Pts',(-18.8993583114686,-37.6292275829253,
121.993249334213)) ;
#108022 = CARTESIAN_POINT('Ctrl Pts',(-18.6643727563373,-37.6390679325563,
122.101285905373)) ;
#108023 = CARTESIAN_POINT('Ctrl Pts',(-18.4467827532205,-37.6491309080463,
122.251509215231)) ;
#108024 = CARTESIAN_POINT('Ctrl Pts',(-18.2618415785691,-37.6590252281897,
122.434315181423)) ;
#108025 = CARTESIAN_POINT('Ctrl Pts',(-18.1101921979794,-37.6689669413213,
122.647012356503)) ;
#108026 = CARTESIAN_POINT('Ctrl Pts',(-17.9969505425752,-37.6789698311154,
122.884279729018)) ;
#108027 = CARTESIAN_POINT('Ctrl Pts',(-17.9268499593331,-37.6890096882759,
123.138607114906)) ;
#108028 = CARTESIAN_POINT('Ctrl Pts',(-17.9019179207587,-37.6988338691135,
123.395591251844)) ;
#108029 = CARTESIAN_POINT('Ctrl Pts',(-17.9220940157087,-37.7088908426167,
123.659084863121)) ;
#108030 = CARTESIAN_POINT('Ctrl Pts',(-17.9872042427552,-37.7188189668038,
123.911746027591)) ;
#108031 = CARTESIAN_POINT('Ctrl Pts',(-18.0948316129578,-37.7287726618772,
124.1501526263)) ;
#108032 = CARTESIAN_POINT('Ctrl Pts',(-18.2438973494036,-37.7388188554525,
124.368042069497)) ;
#108033 = CARTESIAN_POINT('Ctrl Pts',(-18.4247143523808,-37.7486669578124,
124.55319376787)) ;
#108034 = CARTESIAN_POINT('Ctrl Pts',(-18.6368737321832,-37.75862854604,124.706527900158)) ;
#108035 = CARTESIAN_POINT('Ctrl Pts',(-18.8741889123257,-37.7686572161963,
124.82117776678)) ;
#108036 = CARTESIAN_POINT('Ctrl Pts',(-19.1247639980567,-37.778567519078,
124.892107534021)) ;
#108037 = CARTESIAN_POINT('Ctrl Pts',(-19.3844408619282,-37.7885024028859,
124.919199981509)) ;
#108038 = CARTESIAN_POINT('Ctrl Pts',(-19.6476287569967,-37.7985435445765,
124.900351524568)) ;
#108039 = CARTESIAN_POINT('Ctrl Pts',(-19.8996880891423,-37.8084306657405,
124.837248718803)) ;
#108040 = CARTESIAN_POINT('Ctrl Pts',(-20.1396351561268,-37.818423008589,
124.730624721644)) ;
#108041 = CARTESIAN_POINT('Ctrl Pts',(-20.3564483081695,-37.828371309813,
124.584525305613)) ;
#108042 = CARTESIAN_POINT('Ctrl Pts',(-20.5446407648115,-37.8383088874951,
124.403488389917)) ;
#108043 = CARTESIAN_POINT('Ctrl Pts',(-20.6995353445836,-37.8482954619457,
124.19161538296)) ;
#108044 = CARTESIAN_POINT('Ctrl Pts',(-20.8154970734678,-37.8583242718541,
123.954954138649)) ;
#108045 = CARTESIAN_POINT('Ctrl Pts',(-20.8877508953249,-37.8682025931609,
123.705622620261)) ;
#108046 = CARTESIAN_POINT('Ctrl Pts',(-20.9165491642619,-37.8781942405083,
123.444627694951)) ;
#108047 = CARTESIAN_POINT('Ctrl Pts',(-20.8989830904194,-37.8882287639461,
123.181528801038)) ;
#108048 = CARTESIAN_POINT('Ctrl Pts',(-20.8375900725936,-37.8980921208247,
122.929677120428)) ;
#108049 = CARTESIAN_POINT('Ctrl Pts',(-20.7312850440034,-37.908162347505,
122.687363711049)) ;
#108050 = CARTESIAN_POINT('Ctrl Pts',(-20.5878097989603,-37.9180046556397,
122.472146620804)) ;
#108051 = CARTESIAN_POINT('Ctrl Pts',(-20.4077072811251,-37.9279653876631,
122.282207293624)) ;
#108052 = CARTESIAN_POINT('Ctrl Pts',(-20.1954236191509,-37.9380032768612,
122.125639435878)) ;
#108053 = CARTESIAN_POINT('Ctrl Pts',(-19.9632067506179,-37.94787755978,122.009773260868)) ;
#108054 = CARTESIAN_POINT('Ctrl Pts',(-19.7095351983791,-37.9579473043975,
121.934560773782)) ;
#108055 = CARTESIAN_POINT('Ctrl Pts',(-19.4527900585432,-37.9677806147431,
121.905097719252)) ;
#108056 = CARTESIAN_POINT('Ctrl Pts',(-19.1896456423422,-37.9778108580958,
121.920221120939)) ;
#108057 = CARTESIAN_POINT('Ctrl Pts',(-18.9332428132667,-37.9878431460742,
121.981587866224)) ;
#108058 = CARTESIAN_POINT('Ctrl Pts',(-18.6960940925784,-37.9976703225423,
122.083833011387)) ;
#108059 = CARTESIAN_POINT('Ctrl Pts',(-18.4761183695582,-38.0076757054092,
122.227800110012)) ;
#108060 = CARTESIAN_POINT('Ctrl Pts',(-18.2849162844405,-38.0176583444019,
122.40748589956)) ;
#108061 = CARTESIAN_POINT('Ctrl Pts',(-18.12715679948,-38.0277024115385,122.619066068581)) ;
#108062 = CARTESIAN_POINT('Ctrl Pts',(-18.0107464436038,-38.0375236303425,
122.849423615457)) ;
#108063 = CARTESIAN_POINT('Ctrl Pts',(-17.9338217319753,-38.0475604692805,
123.101709933647)) ;
#108064 = CARTESIAN_POINT('Ctrl Pts',(-17.90265430105,-38.0575848813783,123.363299617885)) ;
#108065 = CARTESIAN_POINT('Ctrl Pts',(-17.9165551681965,-38.0674369657836,
123.621833332223)) ;
#108066 = CARTESIAN_POINT('Ctrl Pts',(-17.9755624279843,-38.0774278625268,
123.877634519735)) ;
#108067 = CARTESIAN_POINT('Ctrl Pts',(-18.0772087987277,-38.0873458544277,
124.117665217245)) ;
#108068 = CARTESIAN_POINT('Ctrl Pts',(-18.2204811522142,-38.0973739698847,
124.33881969572)) ;
#108069 = CARTESIAN_POINT('Ctrl Pts',(-18.3973561188024,-38.1072591458268,
124.529083160064)) ;
#108070 = CARTESIAN_POINT('Ctrl Pts',(-18.6063780250938,-38.1172485042337,
124.687904172725)) ;
#108071 = CARTESIAN_POINT('Ctrl Pts',(-18.8412609312879,-38.127289651814,
124.808143474274)) ;
#108072 = CARTESIAN_POINT('Ctrl Pts',(-19.0880878425469,-38.1371222748204,
124.884569704916)) ;
#108073 = CARTESIAN_POINT('Ctrl Pts',(-19.3485474897113,-38.1471163459312,
124.918245536733)) ;
#108074 = CARTESIAN_POINT('Ctrl Pts',(-19.6118018432702,-38.1571450035721,
124.905623026337)) ;
#108075 = CARTESIAN_POINT('Ctrl Pts',(-19.8652033688323,-38.1670293297649,
124.848603449057)) ;
#108076 = CARTESIAN_POINT('Ctrl Pts',(-20.1070976067128,-38.1769950732555,
124.748213951497)) ;
#108077 = CARTESIAN_POINT('Ctrl Pts',(-20.3290517854793,-38.1870234523867,
124.606153348801)) ;
#108078 = CARTESIAN_POINT('Ctrl Pts',(-20.5208025509905,-38.1969242985936,
124.430241432871)) ;
#108079 = CARTESIAN_POINT('Ctrl Pts',(-20.6815171132775,-38.2069829560107,
124.220431994097)) ;
#108080 = CARTESIAN_POINT('Ctrl Pts',(-20.8012070122064,-38.2168405187926,
123.990641916311)) ;
#108081 = CARTESIAN_POINT('Ctrl Pts',(-20.880986737264,-38.2269089213458,
123.738410661885)) ;
#108082 = CARTESIAN_POINT('Ctrl Pts',(-20.9150057915804,-38.2367643200854,
123.48164244073)) ;
#108083 = CARTESIAN_POINT('Ctrl Pts',(-20.9045577592598,-38.2467591871593,
123.219204450533)) ;
#108084 = CARTESIAN_POINT('Ctrl Pts',(-20.847938397475,-38.2567904821428,
122.961739544388)) ;
#108085 = CARTESIAN_POINT('Ctrl Pts',(-20.749506310943,-38.2666570068693,
122.721858258568)) ;
#108086 = CARTESIAN_POINT('Ctrl Pts',(-20.6095975475329,-38.276644477565,
122.499835152768)) ;
#108087 = CARTESIAN_POINT('Ctrl Pts',(-20.4340771525001,-38.2865892371289,
122.306157365648)) ;
#108088 = CARTESIAN_POINT('Ctrl Pts',(-20.2254558520578,-38.2966347930777,
122.144445923788)) ;
#108089 = CARTESIAN_POINT('Ctrl Pts',(-19.9963237905782,-38.3064943814529,
122.023421108531)) ;
#108090 = CARTESIAN_POINT('Ctrl Pts',(-19.7463143416056,-38.3164953365889,
121.942527032134)) ;
#108091 = CARTESIAN_POINT('Ctrl Pts',(-19.488519326872,-38.3263995638665,
121.906409654677)) ;
#108092 = CARTESIAN_POINT('Ctrl Pts',(-19.2248216455674,-38.3364416407616,
121.915654492875)) ;
#108093 = CARTESIAN_POINT('Ctrl Pts',(-18.9700831262293,-38.3463492534478,
121.96970219596)) ;
#108094 = CARTESIAN_POINT('Ctrl Pts',(-18.725090400626,-38.3564037840635,
122.06855506497)) ;
#108095 = CARTESIAN_POINT('Ctrl Pts',(-18.5051609091542,-38.3662645706124,
122.205658540537)) ;
#108096 = CARTESIAN_POINT('Ctrl Pts',(-18.309510262844,-38.3762583256834,
122.38078922624)) ;
#108097 = CARTESIAN_POINT('Ctrl Pts',(-18.1481992555944,-38.3861836859234,
122.585804588426)) ;
#108098 = CARTESIAN_POINT('Ctrl Pts',(-18.0236898301112,-38.3962116153187,
122.818019304383)) ;
#108099 = CARTESIAN_POINT('Ctrl Pts',(-17.9422763014649,-38.406097882118,
123.064775411848)) ;
#108100 = CARTESIAN_POINT('Ctrl Pts',(-17.9042719720946,-38.4161296510163,
123.325601599264)) ;
#108101 = CARTESIAN_POINT('Ctrl Pts',(-17.9117644560896,-38.4260112468599,
123.585218113154)) ;
#108102 = CARTESIAN_POINT('Ctrl Pts',(-17.9650952399222,-38.4360731323278,
123.844159329746)) ;
#108103 = CARTESIAN_POINT('Ctrl Pts',(-18.0605428012265,-38.4459305663467,
124.085012614075)) ;
#108104 = CARTESIAN_POINT('Ctrl Pts',(-18.1977237107639,-38.4559238093887,
124.308906706103)) ;
#108105 = CARTESIAN_POINT('Ctrl Pts',(-18.3706274266826,-38.465854570275,
124.504401204195)) ;
#108106 = CARTESIAN_POINT('Ctrl Pts',(-18.6449345264328,-38.4792035624722,
124.723116581102)) ;
#108107 = CARTESIAN_POINT('Ctrl Pts',(-18.9682302464026,-38.4924719352886,
124.863914087516)) ;
#108108 = CARTESIAN_POINT('Ctrl Pts',(-19.3133620154976,-38.505754876673,
124.916356944705)) ;
#108109 = CARTESIAN_POINT('Ctrl Pts',(-19.5771786980068,-38.5157976625152,
124.909903565302)) ;
#108110 = CARTESIAN_POINT('Ctrl Pts',(-19.8309832614376,-38.5256476050673,
124.859016008072)) ;
#108111 = CARTESIAN_POINT('Ctrl Pts',(-20.0759219776748,-38.5356448379863,
124.764044983854)) ;
#108112 = CARTESIAN_POINT('Ctrl Pts',(-20.3008573210295,-38.5456597333208,
124.627383085711)) ;
#108113 = CARTESIAN_POINT('Ctrl Pts',(-20.5625428004282,-38.558899409959,
124.398103758951)) ;
#108114 = CARTESIAN_POINT('Ctrl Pts',(-20.807908613215,-38.5754466343643,
124.033145256858)) ;
#108115 = CARTESIAN_POINT('Ctrl Pts',(-20.9148745686964,-38.5920940714954,
123.603813235972)) ;
#108116 = CARTESIAN_POINT('Ctrl Pts',(-20.9084002065562,-38.6053835689736,
123.254614227225)) ;
#108117 = CARTESIAN_POINT('Ctrl Pts',(-20.8593805891934,-38.615256976796,
122.999823493722)) ;
#108118 = CARTESIAN_POINT('Ctrl Pts',(-20.7652368411073,-38.6253093543887,
122.753014839041)) ;
#108119 = CARTESIAN_POINT('Ctrl Pts',(-20.6315634106382,-38.6352130079296,
122.529686605686)) ;
#108120 = CARTESIAN_POINT('Ctrl Pts',(-20.4609554845938,-38.6451572769249,
122.33178149402)) ;
#108121 = CARTESIAN_POINT('Ctrl Pts',(-20.1896720233983,-38.6584882852576,
122.110006814825)) ;
#108122 = CARTESIAN_POINT('Ctrl Pts',(-19.7868146270394,-38.6751098657819,
121.928869257225)) ;
#108123 = CARTESIAN_POINT('Ctrl Pts',(-19.3484026500655,-38.6916525364803,
121.895341800195)) ;
#108124 = CARTESIAN_POINT('Ctrl Pts',(-19.0036115337529,-38.7050016960432,
121.959975648739)) ;
#108125 = CARTESIAN_POINT('Ctrl Pts',(-18.6780675299039,-38.7182298462027,
122.081998336567)) ;
#108126 = CARTESIAN_POINT('Ctrl Pts',(-18.318189296983,-38.7348605233402,
122.338529958053)) ;
#108127 = CARTESIAN_POINT('Ctrl Pts',(-18.0180618486451,-38.7547634626283,
122.774214527966)) ;
#108128 = CARTESIAN_POINT('Ctrl Pts',(-17.8841363367089,-38.7746663292316,
123.285862111396)) ;
#108129 = CARTESIAN_POINT('Ctrl Pts',(-17.9320867719657,-38.7945794943364,
123.813063123829)) ;
#108130 = CARTESIAN_POINT('Ctrl Pts',(-18.1591211464769,-38.8146153234777,
124.29467830062)) ;
#108131 = CARTESIAN_POINT('Ctrl Pts',(-18.5326984939295,-38.8344338983558,
124.666208169951)) ;
#108132 = CARTESIAN_POINT('Ctrl Pts',(-19.0136620305705,-38.8544041993978,
124.890287109403)) ;
#108133 = CARTESIAN_POINT('Ctrl Pts',(-19.5404886042975,-38.8742957317623,
124.936806064682)) ;
#108134 = CARTESIAN_POINT('Ctrl Pts',(-20.0545416964585,-38.8943188295789,
124.79955145257)) ;
#108135 = CARTESIAN_POINT('Ctrl Pts',(-20.4863312832862,-38.9141155824988,
124.498762007318)) ;
#108136 = CARTESIAN_POINT('Ctrl Pts',(-20.7931734977669,-38.9340766709876,
124.066022444128)) ;
#108137 = CARTESIAN_POINT('Ctrl Pts',(-20.9330014112939,-38.9540549399198,
123.553728971444)) ;
#108138 = CARTESIAN_POINT('Ctrl Pts',(-20.8907327724234,-38.9738749547108,
123.02869475274)) ;
#108139 = CARTESIAN_POINT('Ctrl Pts',(-20.671741885746,-38.9938133639626,
122.546100539438)) ;
#108140 = CARTESIAN_POINT('Ctrl Pts',(-20.2983058535929,-39.013860481355,
122.165949512377)) ;
#108141 = CARTESIAN_POINT('Ctrl Pts',(-19.8223852491387,-39.0337067271889,
121.938630866729)) ;
#108142 = CARTESIAN_POINT('Ctrl Pts',(-19.2975107818307,-39.0535556957009,
121.88528017714)) ;
#108143 = CARTESIAN_POINT('Ctrl Pts',(-18.7809909805652,-39.0736059980122,
122.016192548372)) ;
#108144 = CARTESIAN_POINT('Ctrl Pts',(-18.3447992174342,-39.0934409204434,
122.312485774824)) ;
#108145 = CARTESIAN_POINT('Ctrl Pts',(-18.0337712867575,-39.1133713216693,
122.741023909243)) ;
#108146 = CARTESIAN_POINT('Ctrl Pts',(-17.8872243556571,-39.1332562670282,
123.249020163311)) ;
#108147 = CARTESIAN_POINT('Ctrl Pts',(-17.9240100369502,-39.1533288751795,
123.781146880013)) ;
#108148 = CARTESIAN_POINT('Ctrl Pts',(-18.1371362656377,-39.1731201915077,
124.262143080741)) ;
#108149 = CARTESIAN_POINT('Ctrl Pts',(-18.5035341697257,-39.1930849812749,
124.645907690736)) ;
#108150 = CARTESIAN_POINT('Ctrl Pts',(-18.9799661770289,-39.2130679370252,
124.880649319702)) ;
#108151 = CARTESIAN_POINT('Ctrl Pts',(-19.5032134048626,-39.2328764590014,
124.939294610312)) ;
#108152 = CARTESIAN_POINT('Ctrl Pts',(-20.0196253121338,-39.2528620337372,
124.815383030727)) ;
#108153 = CARTESIAN_POINT('Ctrl Pts',(-20.4606098925301,-39.2727446738056,
124.523969753369)) ;
#108154 = CARTESIAN_POINT('Ctrl Pts',(-20.7770307675651,-39.2926999859375,
124.098449337436)) ;
#108155 = CARTESIAN_POINT('Ctrl Pts',(-20.9290125086487,-39.3125743425453,
123.592464133645)) ;
#108156 = CARTESIAN_POINT('Ctrl Pts',(-20.8993955940314,-39.3325565494064,
123.062255599716)) ;
#108157 = CARTESIAN_POINT('Ctrl Pts',(-20.6908311188949,-39.3524876273563,
122.575184100747)) ;
#108158 = CARTESIAN_POINT('Ctrl Pts',(-20.3288513423794,-39.3724146022113,
122.188711260408)) ;
#108159 = CARTESIAN_POINT('Ctrl Pts',(-19.8592740611879,-39.3922470611602,
121.949092111192)) ;
#108160 = CARTESIAN_POINT('Ctrl Pts',(-19.4200714383122,-39.4089047453354,
121.894176350712)) ;
#108161 = CARTESIAN_POINT('Ctrl Pts',(-19.0750845374092,-39.4221539692425,
121.941823263879)) ;
#108162 = CARTESIAN_POINT('Ctrl Pts',(-18.8237314955638,-39.4322029906937,
122.022704050237)) ;
#108163 = CARTESIAN_POINT('Ctrl Pts',(-18.5945719587257,-39.4420629989242,
122.143637046641)) ;
#108164 = CARTESIAN_POINT('Ctrl Pts',(-18.3180933172419,-39.4553465121488,
122.356805711671)) ;
#108165 = CARTESIAN_POINT('Ctrl Pts',(-18.0500122798187,-39.4719924311496,
122.708686652931)) ;
#108166 = CARTESIAN_POINT('Ctrl Pts',(-17.9182229494711,-39.4885464089657,
123.128502561202)) ;
#108167 = CARTESIAN_POINT('Ctrl Pts',(-17.9033037209562,-39.5019061379373,
123.479260538537)) ;
#108168 = CARTESIAN_POINT('Ctrl Pts',(-17.9373243166265,-39.511799189734,
123.73702185097)) ;
#108169 = CARTESIAN_POINT('Ctrl Pts',(-18.0159991395794,-39.521789155015,
123.987450031677)) ;
#108170 = CARTESIAN_POINT('Ctrl Pts',(-18.1363948183346,-39.5317410358759,
124.219660059973)) ;
#108171 = CARTESIAN_POINT('Ctrl Pts',(-18.2969567303426,-39.5417893875677,
124.429261495582)) ;
#108172 = CARTESIAN_POINT('Ctrl Pts',(-18.4872968694705,-39.5516306716739,
124.604383387252)) ;
#108173 = CARTESIAN_POINT('Ctrl Pts',(-18.7080132350859,-39.5616173747996,
124.746280915969)) ;
#108174 = CARTESIAN_POINT('Ctrl Pts',(-18.9487894622265,-39.571552403617,
124.847360989506)) ;
#108175 = CARTESIAN_POINT('Ctrl Pts',(-19.2065140511912,-39.5816081985239,
124.905565796026)) ;
#108176 = CARTESIAN_POINT('Ctrl Pts',(-19.4645174692471,-39.5914365618132,
124.918256133084)) ;
#108177 = CARTESIAN_POINT('Ctrl Pts',(-19.7268451727224,-39.6014975317111,
124.885572668199)) ;
#108178 = CARTESIAN_POINT('Ctrl Pts',(-19.975826615135,-39.6114118106009,
124.808745771758)) ;
#108179 = CARTESIAN_POINT('Ctrl Pts',(-20.2101147526998,-39.6214208050691,
124.689190878813)) ;
#108180 = CARTESIAN_POINT('Ctrl Pts',(-20.4201917083197,-39.6314506396329,
124.530016381586)) ;
#108181 = CARTESIAN_POINT('Ctrl Pts',(-20.5967480738789,-39.6413088697051,
124.340408988415)) ;
#108182 = CARTESIAN_POINT('Ctrl Pts',(-20.7399416116488,-39.6513075754475,
124.120151495225)) ;
#108183 = CARTESIAN_POINT('Ctrl Pts',(-20.8419667401955,-39.6612022313663,
123.880930605465)) ;
#108184 = CARTESIAN_POINT('Ctrl Pts',(-20.9018070177436,-39.6712652957503,
123.623389631562)) ;
#108185 = CARTESIAN_POINT('Ctrl Pts',(-20.9159959456146,-39.6811049540302,
123.365160498217)) ;
#108186 = CARTESIAN_POINT('Ctrl Pts',(-20.8847744321172,-39.691168121112,
123.102597212556)) ;
#108187 = CARTESIAN_POINT('Ctrl Pts',(-20.809489673972,-39.7010623662391,
122.85369436539)) ;
#108188 = CARTESIAN_POINT('Ctrl Pts',(-20.6922282780621,-39.7110041878437,
122.620263504091)) ;
#108189 = CARTESIAN_POINT('Ctrl Pts',(-20.5353015269347,-39.7210067187618,
122.409347149382)) ;
#108190 = CARTESIAN_POINT('Ctrl Pts',(-20.3432781213976,-39.7310413452193,
122.228634378221)) ;
#108191 = CARTESIAN_POINT('Ctrl Pts',(-20.1271560894029,-39.7408868802057,
122.086376137188)) ;
#108192 = CARTESIAN_POINT('Ctrl Pts',(-19.8865438462401,-39.7508703050448,
121.98185816591)) ;
#108193 = CARTESIAN_POINT('Ctrl Pts',(-19.6322426627051,-39.7608206954098,
121.920952858451)) ;
#108194 = CARTESIAN_POINT('Ctrl Pts',(-19.3699963296536,-39.7708183357069,
121.904697658829)) ;
#108195 = CARTESIAN_POINT('Ctrl Pts',(-19.1079263014732,-39.7808574162701,
121.934869440675)) ;
#108196 = CARTESIAN_POINT('Ctrl Pts',(-18.860246320499,-39.7906835670392,
122.007945708083)) ;
#108197 = CARTESIAN_POINT('Ctrl Pts',(-18.6234343625826,-39.8007401419683,
122.125222897049)) ;
#108198 = CARTESIAN_POINT('Ctrl Pts',(-18.4132900657496,-39.8106806813486,
122.280411411779)) ;
#108199 = CARTESIAN_POINT('Ctrl Pts',(-18.2333513169746,-39.820585074325,
122.468477752401)) ;
#108200 = CARTESIAN_POINT('Ctrl Pts',(-18.0868790875031,-39.8306317285299,
122.688109809972)) ;
#108201 = CARTESIAN_POINT('Ctrl Pts',(-17.9821196213691,-39.8405272904683,
122.926166157976)) ;
#108202 = CARTESIAN_POINT('Ctrl Pts',(-17.919264861442,-39.8505893683139,
123.182968808)) ;
#108203 = CARTESIAN_POINT('Ctrl Pts',(-17.902179100725,-39.8604320667276,
123.441089403448)) ;
#108204 = CARTESIAN_POINT('Ctrl Pts',(-17.9299684986018,-39.8704228416891,
123.702127740088)) ;
#108205 = CARTESIAN_POINT('Ctrl Pts',(-18.0022538608553,-39.8803507067082,
123.952822926741)) ;
#108206 = CARTESIAN_POINT('Ctrl Pts',(-18.1172750648444,-39.8903394514744,
124.18878013499)) ;
#108207 = CARTESIAN_POINT('Ctrl Pts',(-18.2725120158301,-39.9003722370613,
124.401889306387)) ;
#108208 = CARTESIAN_POINT('Ctrl Pts',(-18.4590581539121,-39.910238921682,
124.581959456617)) ;
#108209 = CARTESIAN_POINT('Ctrl Pts',(-18.6756999438248,-39.9202008138451,
124.728934492756)) ;
#108210 = CARTESIAN_POINT('Ctrl Pts',(-18.9164434449401,-39.9302342907577,
124.836443452761)) ;
#108211 = CARTESIAN_POINT('Ctrl Pts',(-19.1683377738206,-39.940118632006,
124.899975771883)) ;
#108212 = CARTESIAN_POINT('Ctrl Pts',(-19.4320522241906,-39.9501815741271,
124.919144828217)) ;
#108213 = CARTESIAN_POINT('Ctrl Pts',(-19.6895996842893,-39.9600319757467,
124.89292120347)) ;
#108214 = CARTESIAN_POINT('Ctrl Pts',(-19.9432985792622,-39.9700588645364,
124.821762394978)) ;
#108215 = CARTESIAN_POINT('Ctrl Pts',(-20.1805473148166,-39.9800874794926,
124.706983894137)) ;
#108216 = CARTESIAN_POINT('Ctrl Pts',(-20.3906194099252,-39.9899327026126,
124.555988101706)) ;
#108217 = CARTESIAN_POINT('Ctrl Pts',(-20.5744702495279,-39.9999233864186,
124.368552094175)) ;
#108218 = CARTESIAN_POINT('Ctrl Pts',(-20.7231943261795,-40.009961268491,
124.150693894303)) ;
#108219 = CARTESIAN_POINT('Ctrl Pts',(-20.8301547375358,-40.0198056281299,
123.915129884966)) ;
#108220 = CARTESIAN_POINT('Ctrl Pts',(-20.8959976047034,-40.0297904987446,
123.661170320315)) ;
#108221 = CARTESIAN_POINT('Ctrl Pts',(-20.9167748834998,-40.0397297820733,
123.400765241907)) ;
#108222 = CARTESIAN_POINT('Ctrl Pts',(-20.8916933004371,-40.0497703914464,
123.138130792356)) ;
#108223 = CARTESIAN_POINT('Ctrl Pts',(-20.8226519350043,-40.0596552423596,
122.887678558748)) ;
#108224 = CARTESIAN_POINT('Ctrl Pts',(-20.7101676316189,-40.0696571985284,
122.650166731446)) ;
#108225 = CARTESIAN_POINT('Ctrl Pts',(-20.5595427373319,-40.0795757952489,
122.437393424481)) ;
#108226 = CARTESIAN_POINT('Ctrl Pts',(-20.3718862888207,-40.0896226173247,
122.251727314683)) ;
#108227 = CARTESIAN_POINT('Ctrl Pts',(-20.1586418375335,-40.0994968984374,
122.103798399595)) ;
#108228 = CARTESIAN_POINT('Ctrl Pts',(-19.9188066374815,-40.109551098482,
121.993056383595)) ;
#108229 = CARTESIAN_POINT('Ctrl Pts',(-19.6673552313463,-40.1194465281173,
121.926576698577)) ;
#108230 = CARTESIAN_POINT('Ctrl Pts',(-19.403915213379,-40.1295081564346,
121.904345230977)) ;
#108231 = CARTESIAN_POINT('Ctrl Pts',(-19.1462503218584,-40.1393527852645,
121.927649389564)) ;
#108232 = CARTESIAN_POINT('Ctrl Pts',(-18.8933867189319,-40.1493128328701,
121.995219488322)) ;
#108233 = CARTESIAN_POINT('Ctrl Pts',(-18.6544595208045,-40.1593511390442,
122.107002406275)) ;
#108234 = CARTESIAN_POINT('Ctrl Pts',(-18.4417892571476,-40.1692244384768,
122.255702785229)) ;
#108235 = CARTESIAN_POINT('Ctrl Pts',(-18.2545782722109,-40.1792977000631,
122.44277820839)) ;
#108236 = CARTESIAN_POINT('Ctrl Pts',(-18.1061634154911,-40.1891179260198,
122.653968585527)) ;
#108237 = CARTESIAN_POINT('Ctrl Pts',(-17.9936299888844,-40.1991969899593,
122.893665938314)) ;
#108238 = CARTESIAN_POINT('Ctrl Pts',(-17.9258431923376,-40.2090470799791,
123.143555897094)) ;
#108239 = CARTESIAN_POINT('Ctrl Pts',(-17.9018083217025,-40.2191258335929,
123.407254879522)) ;
#108240 = CARTESIAN_POINT('Ctrl Pts',(-17.92317260739,-40.2289473008524,123.664525748583)) ;
#108241 = CARTESIAN_POINT('Ctrl Pts',(-17.9900923585646,-40.23901289921,123.920371717973)) ;
#108242 = CARTESIAN_POINT('Ctrl Pts',(-18.0987485022891,-40.2489155549847,
124.156904978574)) ;
#108243 = CARTESIAN_POINT('Ctrl Pts',(-18.248904465991,-40.2589663808143,
124.374130409106)) ;
#108244 = CARTESIAN_POINT('Ctrl Pts',(-18.4311339191493,-40.2688405851532,
124.558938498704)) ;
#108245 = CARTESIAN_POINT('Ctrl Pts',(-18.64682823792,-40.2789130351923,124.71226441453)) ;
#108246 = CARTESIAN_POINT('Ctrl Pts',(-18.8800799546237,-40.2887420519658,
124.823334593116)) ;
#108247 = CARTESIAN_POINT('Ctrl Pts',(-19.1349090565034,-40.2988088978806,
124.894208967306)) ;
#108248 = CARTESIAN_POINT('Ctrl Pts',(-19.3936461150515,-40.3086990691824,
124.919152044099)) ;
#108249 = CARTESIAN_POINT('Ctrl Pts',(-19.6554532124092,-40.3186912628062,
124.899160184907)) ;
#108250 = CARTESIAN_POINT('Ctrl Pts',(-19.9090113028745,-40.3286540734297,
124.833961970796)) ;
#108251 = CARTESIAN_POINT('Ctrl Pts',(-20.146294812703,-40.3385583462731,
124.72695427471)) ;
#108252 = CARTESIAN_POINT('Ctrl Pts',(-20.3646113413137,-40.3486188380777,
124.577901009706)) ;
#108253 = CARTESIAN_POINT('Ctrl Pts',(-20.5498777891069,-40.3584591697501,
124.39744010255)) ;
#108254 = CARTESIAN_POINT('Ctrl Pts',(-20.7046324746843,-40.3685222158418,
124.183046356769)) ;
#108255 = CARTESIAN_POINT('Ctrl Pts',(-20.8177094322231,-40.3784162715369,
123.948887583133)) ;
#108256 = CARTESIAN_POINT('Ctrl Pts',(-20.889431383718,-40.3883589718599,
123.697670525039)) ;
#108257 = CARTESIAN_POINT('Ctrl Pts',(-20.9166730793873,-40.3983647127875,
123.436117530858)) ;
#108258 = CARTESIAN_POINT('Ctrl Pts',(-20.8977644606213,-40.408385623303,
123.173464560564)) ;
#108259 = CARTESIAN_POINT('Ctrl Pts',(-20.8346596888786,-40.418276358753,
122.921314553624)) ;
#108260 = CARTESIAN_POINT('Ctrl Pts',(-20.7280148134984,-40.4282678994818,
122.681391753882)) ;
#108261 = CARTESIAN_POINT('Ctrl Pts',(-20.5819059977354,-40.4382157599035,
122.464616950572)) ;
#108262 = CARTESIAN_POINT('Ctrl Pts',(-20.4007589940039,-40.4481624290898,
122.276156866354)) ;
#108263 = CARTESIAN_POINT('Ctrl Pts',(-20.1873379860688,-40.4582105052254,
122.120688929112)) ;
#108264 = CARTESIAN_POINT('Ctrl Pts',(-19.9549808379891,-40.468058103231,
122.006755225708)) ;
#108265 = CARTESIAN_POINT('Ctrl Pts',(-19.7037329672669,-40.4780198263155,
121.933279690208)) ;
#108266 = CARTESIAN_POINT('Ctrl Pts',(-19.4417310980554,-40.4880484613985,
121.904681422218)) ;
#108267 = CARTESIAN_POINT('Ctrl Pts',(-19.1818683091589,-40.4979587697165,
121.921718478784)) ;
#108268 = CARTESIAN_POINT('Ctrl Pts',(-18.9281025160491,-40.5078936668524,
121.983111466972)) ;
#108269 = CARTESIAN_POINT('Ctrl Pts',(-18.6864066527644,-40.517934749795,
122.088968537774)) ;
#108270 = CARTESIAN_POINT('Ctrl Pts',(-18.4700085972782,-40.5278220926232,
122.232808818307)) ;
#108271 = CARTESIAN_POINT('Ctrl Pts',(-18.2795999896644,-40.5378136075626,
122.413579933739)) ;
#108272 = CARTESIAN_POINT('Ctrl Pts',(-18.1241747121208,-40.5477649987591,
122.6239004086)) ;
#108273 = CARTESIAN_POINT('Ctrl Pts',(-18.0074485776265,-40.5576975320917,
122.857361394326)) ;
#108274 = CARTESIAN_POINT('Ctrl Pts',(-17.9324508010301,-40.5676946899911,
123.10913336402)) ;
#108275 = CARTESIAN_POINT('Ctrl Pts',(-17.9022406529459,-40.5776797001546,
123.369825342602)) ;
#108276 = CARTESIAN_POINT('Ctrl Pts',(-17.9182261140399,-40.5877225267244,
123.633219631623)) ;
#108277 = CARTESIAN_POINT('Ctrl Pts',(-17.9778420179096,-40.5975527610294,
123.884617651115)) ;
#108278 = CARTESIAN_POINT('Ctrl Pts',(-18.082615365187,-40.607628786264,124.127734830538)) ;
#108279 = CARTESIAN_POINT('Ctrl Pts',(-18.2247286077959,-40.6174810227549,
124.344219676141)) ;
#108280 = CARTESIAN_POINT('Ctrl Pts',(-18.4060222671009,-40.627554229189,
124.537048390398)) ;
#108281 = CARTESIAN_POINT('Ctrl Pts',(-18.6132579836576,-40.6373957386962,
124.691803922634)) ;
#108282 = CARTESIAN_POINT('Ctrl Pts',(-18.8465505513508,-40.647356685476,
124.810505779796)) ;
#108283 = CARTESIAN_POINT('Ctrl Pts',(-19.0989962736122,-40.657394514276,
124.886982239754)) ;
#108284 = CARTESIAN_POINT('Ctrl Pts',(-19.3566017243631,-40.6672688240305,
124.918434301797)) ;
#108285 = CARTESIAN_POINT('Ctrl Pts',(-19.6208150027249,-40.6773385217037,
124.904396748732)) ;
#108286 = CARTESIAN_POINT('Ctrl Pts',(-19.8726147197196,-40.6871719929911,
124.846216573453)) ;
#108287 = CARTESIAN_POINT('Ctrl Pts',(-20.1155053857362,-40.697201639521,
124.743893434288)) ;
#108288 = CARTESIAN_POINT('Ctrl Pts',(-20.3366189670899,-40.7072361538484,
124.600200710188)) ;
#108289 = CARTESIAN_POINT('Ctrl Pts',(-20.525825198918,-40.7170614393193,
124.424506374465)) ;
#108290 = CARTESIAN_POINT('Ctrl Pts',(-20.68491390274,-40.7270656808678,124.215241512207)) ;
#108291 = CARTESIAN_POINT('Ctrl Pts',(-20.8049296705375,-40.7370483259469,
123.981914452977)) ;
#108292 = CARTESIAN_POINT('Ctrl Pts',(-20.8827863098033,-40.7470935230384,
123.729709556929)) ;
#108293 = CARTESIAN_POINT('Ctrl Pts',(-20.915379084268,-40.7569166387985,
123.473623942466)) ;
#108294 = CARTESIAN_POINT('Ctrl Pts',(-20.9034107635186,-40.7669512505988,
123.210200309604)) ;
#108295 = CARTESIAN_POINT('Ctrl Pts',(-20.8452197947678,-40.776976259372,
122.953252483694)) ;
#108296 = CARTESIAN_POINT('Ctrl Pts',(-20.7455808245074,-40.7868281842135,
122.714289948241)) ;
#108297 = CARTESIAN_POINT('Ctrl Pts',(-20.6043528530783,-40.7968191225363,
122.492995525235)) ;
#108298 = CARTESIAN_POINT('Ctrl Pts',(-20.4282240529534,-40.8067371076827,
122.300836023741)) ;
#108299 = CARTESIAN_POINT('Ctrl Pts',(-20.219189537808,-40.8167652085782,
122.140396675837)) ;
#108300 = CARTESIAN_POINT('Ctrl Pts',(-19.9888292012109,-40.8266504495208,
122.02031551487)) ;
#108301 = CARTESIAN_POINT('Ctrl Pts',(-19.7387079643851,-40.8366395624874,
121.940619087225)) ;
#108302 = CARTESIAN_POINT('Ctrl Pts',(-19.4771067125699,-40.8466816268282,
121.90595198204)) ;
#108303 = CARTESIAN_POINT('Ctrl Pts',(-19.2190107936235,-40.8565108282327,
121.916506045072)) ;
#108304 = CARTESIAN_POINT('Ctrl Pts',(-18.9620250651059,-40.8665176689909,
121.972140998041)) ;
#108305 = CARTESIAN_POINT('Ctrl Pts',(-18.7190636625384,-40.8765051931828,
122.071533195608)) ;
#108306 = CARTESIAN_POINT('Ctrl Pts',(-18.4962689240686,-40.8865348389914,
122.212311168412)) ;
#108307 = CARTESIAN_POINT('Ctrl Pts',(-18.3040798981206,-40.8964088697302,
122.386686890598)) ;
#108308 = CARTESIAN_POINT('Ctrl Pts',(-18.1428560506009,-40.9064081925943,
122.594132528104)) ;
#108309 = CARTESIAN_POINT('Ctrl Pts',(-18.0209192869641,-40.9163190281699,
122.824322396063)) ;
#108310 = CARTESIAN_POINT('Ctrl Pts',(-17.939762056432,-40.9263732761439,
123.075720211064)) ;
#108311 = CARTESIAN_POINT('Ctrl Pts',(-17.9038796152349,-40.9362320204066,
123.332346566764)) ;
#108312 = CARTESIAN_POINT('Ctrl Pts',(-17.9131359934758,-40.9463001064796,
123.59672475981)) ;
#108313 = CARTESIAN_POINT('Ctrl Pts',(-17.9670267901645,-40.9561555896591,
123.850070178166)) ;
#108314 = CARTESIAN_POINT('Ctrl Pts',(-18.0647187939215,-40.9661504354533,
124.09387118481)) ;
#108315 = CARTESIAN_POINT('Ctrl Pts',(-18.2042534659946,-40.9761817311159,
124.317531681712)) ;
#108316 = CARTESIAN_POINT('Ctrl Pts',(-18.3773037920473,-40.9860482744057,
124.510626572137)) ;
#108317 = CARTESIAN_POINT('Ctrl Pts',(-18.5834579512395,-40.9960356701691,
124.673010282947)) ;
#108318 = CARTESIAN_POINT('Ctrl Pts',(-18.8136905659678,-41.0059807108991,
124.796762194156)) ;
#108319 = CARTESIAN_POINT('Ctrl Pts',(-19.0643800763501,-41.0160252171158,
124.879316585335)) ;
#108320 = CARTESIAN_POINT('Ctrl Pts',(-19.3209063355399,-41.0258887232531,
124.916648200667)) ;
#108321 = CARTESIAN_POINT('Ctrl Pts',(-19.5833652350963,-41.0358815840892,
124.909236656653)) ;
#108322 = CARTESIAN_POINT('Ctrl Pts',(-19.838933260049,-41.0458077778081,
124.856823666464)) ;
#108323 = CARTESIAN_POINT('Ctrl Pts',(-20.08373963909,-41.0558267038407,124.760006771853)) ;
#108324 = CARTESIAN_POINT('Ctrl Pts',(-20.3058788547958,-41.0657417032083,
124.623756791964)) ;
#108325 = CARTESIAN_POINT('Ctrl Pts',(-20.5036454816884,-41.0757964747656,
124.448577731493)) ;
#108326 = CARTESIAN_POINT('Ctrl Pts',(-20.6649615792407,-41.0856554370632,
124.245802378159)) ;
#108327 = CARTESIAN_POINT('Ctrl Pts',(-20.7907129716142,-41.095649680901,
124.015274099518)) ;
#108328 = CARTESIAN_POINT('Ctrl Pts',(-20.8740909164821,-41.1055749103252,
123.768092059042)) ;
#108329 = CARTESIAN_POINT('Ctrl Pts',(-20.9136888180014,-41.1156028742167,
123.507595045891)) ;
#108330 = CARTESIAN_POINT('Ctrl Pts',(-20.9078085172522,-41.1254891338471,
123.247821927504)) ;
#108331 = CARTESIAN_POINT('Ctrl Pts',(-20.8563139433764,-41.1355208969249,
122.989320648716)) ;
#108332 = CARTESIAN_POINT('Ctrl Pts',(-20.7623509133108,-41.1454025232191,
122.747188328021)) ;
#108333 = CARTESIAN_POINT('Ctrl Pts',(-20.6254238376886,-41.1554642927052,
122.521036729548)) ;
#108334 = CARTESIAN_POINT('Ctrl Pts',(-20.4548494543705,-41.1653221602007,
122.326024259616)) ;
#108335 = CARTESIAN_POINT('Ctrl Pts',(-20.2506808427215,-41.1753137853181,
122.160974102844)) ;
#108336 = CARTESIAN_POINT('Ctrl Pts',(-20.0221515737594,-41.1852505844263,
122.034598195036)) ;
#108337 = CARTESIAN_POINT('Ctrl Pts',(-19.7739435190989,-41.1952414139836,
121.949006315307)) ;
#108338 = CARTESIAN_POINT('Ctrl Pts',(-19.5137514171269,-41.2052646496968,
121.907979672832)) ;
#108339 = CARTESIAN_POINT('Ctrl Pts',(-19.2537296731998,-41.215160997726,
121.912474207258)) ;
#108340 = CARTESIAN_POINT('Ctrl Pts',(-18.9959084829037,-41.2251505602285,
121.9619692281)) ;
#108341 = CARTESIAN_POINT('Ctrl Pts',(-18.7495657819261,-41.235190867913,
122.056441570099)) ;
#108342 = CARTESIAN_POINT('Ctrl Pts',(-18.5275452867294,-41.2450331712602,
122.189166374381)) ;
#108343 = CARTESIAN_POINT('Ctrl Pts',(-18.3281548287422,-41.2550568795393,
122.361237377681)) ;
#108344 = CARTESIAN_POINT('Ctrl Pts',(-18.1083697767218,-41.268279057007,
122.630432167841)) ;
#108345 = CARTESIAN_POINT('Ctrl Pts',(-17.9628107520037,-41.2815716420663,
122.952236618744)) ;
#108346 = CARTESIAN_POINT('Ctrl Pts',(-17.906179171894,-41.2948564979879,
123.296802175274)) ;
#108347 = CARTESIAN_POINT('Ctrl Pts',(-17.9090306066105,-41.3048287251607,
123.558807567158)) ;
#108348 = CARTESIAN_POINT('Ctrl Pts',(-17.956592126779,-41.3147373415997,
123.814847983363)) ;
#108349 = CARTESIAN_POINT('Ctrl Pts',(-18.0492993140407,-41.3247905469834,
124.062207468228)) ;
#108350 = CARTESIAN_POINT('Ctrl Pts',(-18.1809181516501,-41.3346556807437,
124.285582948487)) ;
#108351 = CARTESIAN_POINT('Ctrl Pts',(-18.4080967270928,-41.34799473837,124.552513462829)) ;
#108352 = CARTESIAN_POINT('Ctrl Pts',(-18.770623265762,-41.3645639257032,
124.802648338429)) ;
#108353 = CARTESIAN_POINT('Ctrl Pts',(-19.1984831391044,-41.3812090655542,
124.914853897133)) ;
#108354 = CARTESIAN_POINT('Ctrl Pts',(-19.5473217004566,-41.3944813680276,
124.912961520179)) ;
#108355 = CARTESIAN_POINT('Ctrl Pts',(-19.8054060000368,-41.4044623314752,
124.866340893151)) ;
#108356 = CARTESIAN_POINT('Ctrl Pts',(-20.0506155228347,-41.4144041635445,
124.776102300555)) ;
#108357 = CARTESIAN_POINT('Ctrl Pts',(-20.3531550397601,-41.42772373276,124.600157011431)) ;
#108358 = CARTESIAN_POINT('Ctrl Pts',(-20.6634973166793,-41.4442538876927,
124.289018525257)) ;
#108359 = CARTESIAN_POINT('Ctrl Pts',(-20.8878936866745,-41.4642756131848,
123.806648609792)) ;
#108360 = CARTESIAN_POINT('Ctrl Pts',(-20.9340514789459,-41.4840870097916,
123.281992417524)) ;
#108361 = CARTESIAN_POINT('Ctrl Pts',(-20.7981312719008,-41.5040722585005,
122.768629034436)) ;
#108362 = CARTESIAN_POINT('Ctrl Pts',(-20.4961530601248,-41.5239663211364,
122.334489849304)) ;
#108363 = CARTESIAN_POINT('Ctrl Pts',(-20.0638683825088,-41.54389800031,122.028293719276)) ;
#108364 = CARTESIAN_POINT('Ctrl Pts',(-19.5521109509209,-41.563862054782,
121.888097482406)) ;
#108365 = CARTESIAN_POINT('Ctrl Pts',(-19.0253800918483,-41.5837429565449,
121.930378296614)) ;
#108366 = CARTESIAN_POINT('Ctrl Pts',(-18.5431404788178,-41.6036816181533,
122.150032410846)) ;
#108367 = CARTESIAN_POINT('Ctrl Pts',(-18.1655334411876,-41.6235781434086,
122.52023469084)) ;
#108368 = CARTESIAN_POINT('Ctrl Pts',(-17.9361452856179,-41.6434731818629,
122.996685523952)) ;
#108369 = CARTESIAN_POINT('Ctrl Pts',(-17.8830117703529,-41.663437005169,
123.524584694649)) ;
#108370 = CARTESIAN_POINT('Ctrl Pts',(-18.0122651695746,-41.6833111292981,
124.03678760612)) ;
#108371 = CARTESIAN_POINT('Ctrl Pts',(-18.3096364829872,-41.7032862050253,
124.47662297454)) ;
#108372 = CARTESIAN_POINT('Ctrl Pts',(-18.7392073244081,-41.7232397743819,
124.78761036798)) ;
#108373 = CARTESIAN_POINT('Ctrl Pts',(-19.2458943339169,-41.7430776845698,
124.933458741482)) ;
#108374 = CARTESIAN_POINT('Ctrl Pts',(-19.7756310784011,-41.7630535131407,
124.897960696145)) ;
#108375 = CARTESIAN_POINT('Ctrl Pts',(-20.2597826091099,-41.782971557851,
124.683924222372)) ;
#108376 = CARTESIAN_POINT('Ctrl Pts',(-20.6419494519346,-41.8028418036386,
124.31927167099)) ;
#108377 = CARTESIAN_POINT('Ctrl Pts',(-20.8780338315248,-41.8228908067382,
123.841704887354)) ;
#108378 = CARTESIAN_POINT('Ctrl Pts',(-20.9367994539904,-41.842670047979,
123.319145032248)) ;
#108379 = CARTESIAN_POINT('Ctrl Pts',(-20.8130020447445,-41.8627001116879,
122.801495938331)) ;
#108380 = CARTESIAN_POINT('Ctrl Pts',(-20.5213260449873,-41.8825823965899,
122.360747751626)) ;
#108381 = CARTESIAN_POINT('Ctrl Pts',(-20.0977332665932,-41.9024646974829,
122.044888722237)) ;
#108382 = CARTESIAN_POINT('Ctrl Pts',(-19.5891103850463,-41.9224478071012,
121.891915834153)) ;
#108383 = CARTESIAN_POINT('Ctrl Pts',(-19.0612570378797,-41.9423382024791,
121.921619505175)) ;
#108384 = CARTESIAN_POINT('Ctrl Pts',(-18.5748533541873,-41.9622349925134,
122.12896396189)) ;
#108385 = CARTESIAN_POINT('Ctrl Pts',(-18.1875398551015,-41.982152046455,
122.489857562728)) ;
#108386 = CARTESIAN_POINT('Ctrl Pts',(-17.9457214835328,-42.0021555946585,
122.963422399835)) ;
#108387 = CARTESIAN_POINT('Ctrl Pts',(-17.8810265727572,-42.0220938883111,
123.489360284753)) ;
#108388 = CARTESIAN_POINT('Ctrl Pts',(-17.9977456916004,-42.041915375744,
124.003097477831)) ;
#108389 = CARTESIAN_POINT('Ctrl Pts',(-18.2845368526884,-42.0618937687349,
124.44990914885)) ;
#108390 = CARTESIAN_POINT('Ctrl Pts',(-18.7052001843518,-42.0817921503486,
124.770575674907)) ;
#108391 = CARTESIAN_POINT('Ctrl Pts',(-19.1255759866277,-42.0983750810785,
124.902691008963)) ;
#108392 = CARTESIAN_POINT('Ctrl Pts',(-19.4741352236223,-42.1116493166673,
124.918003242186)) ;
#108393 = CARTESIAN_POINT('Ctrl Pts',(-19.7358481841753,-42.1216957341235,
124.883486155696)) ;
#108394 = CARTESIAN_POINT('Ctrl Pts',(-19.9826831156594,-42.1315409593428,
124.805898248086)) ;
#108395 = CARTESIAN_POINT('Ctrl Pts',(-20.293988571428,-42.1448759303822,
124.64504920141)) ;
#108396 = CARTESIAN_POINT('Ctrl Pts',(-20.6198940492843,-42.1614587871748,
124.348199125728)) ;
#108397 = CARTESIAN_POINT('Ctrl Pts',(-20.8257028894447,-42.1781017895242,
123.956759520653)) ;
#108398 = CARTESIAN_POINT('Ctrl Pts',(-20.9027397201207,-42.1913455205559,
123.617281377377)) ;
#108399 = CARTESIAN_POINT('Ctrl Pts',(-20.9155836796199,-42.2013999152305,
123.353425803393)) ;
#108400 = CARTESIAN_POINT('Ctrl Pts',(-20.8834418745023,-42.2112409766191,
123.096770719865)) ;
#108401 = CARTESIAN_POINT('Ctrl Pts',(-20.8057549628219,-42.2213072009756,
122.843952261428)) ;
#108402 = CARTESIAN_POINT('Ctrl Pts',(-20.6874624206494,-42.2311878138952,
122.612764298362)) ;
#108403 = CARTESIAN_POINT('Ctrl Pts',(-20.5294874690542,-42.2411811070548,
122.403032653655)) ;
#108404 = CARTESIAN_POINT('Ctrl Pts',(-20.3383117523044,-42.2511321152785,
122.224541202617)) ;
#108405 = CARTESIAN_POINT('Ctrl Pts',(-20.1168527899179,-42.2611806296404,
122.080769292945)) ;
#108406 = CARTESIAN_POINT('Ctrl Pts',(-19.8788671687555,-42.2710221357031,
121.979466983407)) ;
#108407 = CARTESIAN_POINT('Ctrl Pts',(-19.6234113043599,-42.2810077883328,
121.919624716556)) ;
#108408 = CARTESIAN_POINT('Ctrl Pts',(-19.3625935822749,-42.2909467971777,
121.905011062528)) ;
#108409 = CARTESIAN_POINT('Ctrl Pts',(-19.1006128120326,-42.3009877224707,
121.936283706494)) ;
#108410 = CARTESIAN_POINT('Ctrl Pts',(-18.8517403555237,-42.3108780442256,
122.011291662105)) ;
#108411 = CARTESIAN_POINT('Ctrl Pts',(-18.617058468293,-42.320874017559,122.129257065168)) ;
#108412 = CARTESIAN_POINT('Ctrl Pts',(-18.4077464929747,-42.3308054171411,
122.285168774027)) ;
#108413 = CARTESIAN_POINT('Ctrl Pts',(-18.2270758492578,-42.3408109576181,
122.476218167005)) ;
#108414 = CARTESIAN_POINT('Ctrl Pts',(-18.0823406849302,-42.3508439415494,
122.696584921019)) ;
#108415 = CARTESIAN_POINT('Ctrl Pts',(-17.9794776416119,-42.3606995723763,
122.934300246061)) ;
#108416 = CARTESIAN_POINT('Ctrl Pts',(-17.9182607268367,-42.3706989745694,
123.18979755983)) ;
#108417 = CARTESIAN_POINT('Ctrl Pts',(-17.902198858114,-42.3805934439305,
123.449365848482)) ;
#108418 = CARTESIAN_POINT('Ctrl Pts',(-17.932016938791,-42.3906565580947,
123.712081637151)) ;
#108419 = CARTESIAN_POINT('Ctrl Pts',(-18.0050842699126,-42.4004962038111,
123.960163628557)) ;
#108420 = CARTESIAN_POINT('Ctrl Pts',(-18.12239287798,-42.4105593713669,124.197129769659)) ;
#108421 = CARTESIAN_POINT('Ctrl Pts',(-18.2766507483452,-42.4204536271617,
124.406474059086)) ;
#108422 = CARTESIAN_POINT('Ctrl Pts',(-18.4652833345317,-42.4303954056214,
124.587187892246)) ;
#108423 = CARTESIAN_POINT('Ctrl Pts',(-18.6837622031099,-42.4403980984516,
124.733409125687)) ;
#108424 = CARTESIAN_POINT('Ctrl Pts',(-18.9251828526098,-42.4504321204054,
124.839419707781)) ;
#108425 = CARTESIAN_POINT('Ctrl Pts',(-19.1765152614719,-42.4602799114944,
124.901132876178)) ;
#108426 = CARTESIAN_POINT('Ctrl Pts',(-19.4381823082108,-42.4702614360435,
124.919076853109)) ;
#108427 = CARTESIAN_POINT('Ctrl Pts',(-19.6981732583165,-42.4802106595344,
124.891361524154)) ;
#108428 = CARTESIAN_POINT('Ctrl Pts',(-19.9507299142993,-42.490208315751,
124.818885956961)) ;
#108429 = CARTESIAN_POINT('Ctrl Pts',(-20.1876133040232,-42.500248528806,
124.70273061815)) ;
#108430 = CARTESIAN_POINT('Ctrl Pts',(-20.3965851121659,-42.5100765760823,
124.550933160528)) ;
#108431 = CARTESIAN_POINT('Ctrl Pts',(-20.5804323450624,-42.5201309231147,
124.361187474538)) ;
#108432 = CARTESIAN_POINT('Ctrl Pts',(-20.7265203102694,-42.5300720594432,
124.14459996954)) ;
#108433 = CARTESIAN_POINT('Ctrl Pts',(-20.8331238061989,-42.5399762925229,
123.907153791526)) ;
#108434 = CARTESIAN_POINT('Ctrl Pts',(-20.8976296265304,-42.5500229893665,
123.651161969945)) ;
#108435 = CARTESIAN_POINT('Ctrl Pts',(-20.9166605708197,-42.5599185406468,
123.39177211738)) ;
#108436 = CARTESIAN_POINT('Ctrl Pts',(-20.8899295673934,-42.5699806184863,
123.128744028995)) ;
#108437 = CARTESIAN_POINT('Ctrl Pts',(-20.8196282304126,-42.5798233275824,
122.87979426522)) ;
#108438 = CARTESIAN_POINT('Ctrl Pts',(-20.7060650961516,-42.5898140598208,
122.643116802018)) ;
#108439 = CARTESIAN_POINT('Ctrl Pts',(-20.5540301203929,-42.5997420850496,
122.431077814992)) ;
#108440 = CARTESIAN_POINT('Ctrl Pts',(-20.3666760452894,-42.6097302317001,
122.247240006)) ;
#108441 = CARTESIAN_POINT('Ctrl Pts',(-20.1490062279118,-42.6197652495401,
122.098362587121)) ;
#108442 = CARTESIAN_POINT('Ctrl Pts',(-19.9129916906241,-42.6296300466453,
121.991144549183)) ;
#108443 = CARTESIAN_POINT('Ctrl Pts',(-19.6596809800496,-42.6395907790014,
121.925159819885)) ;
#108444 = CARTESIAN_POINT('Ctrl Pts',(-19.3968379506002,-42.6496242413984,
121.904448248065)) ;
#108445 = CARTESIAN_POINT('Ctrl Pts',(-19.1381776310196,-42.6595097756098,
121.928888325179)) ;
#108446 = CARTESIAN_POINT('Ctrl Pts',(-18.8832107613372,-42.6695746162898,
121.999112842521)) ;
#108447 = CARTESIAN_POINT('Ctrl Pts',(-18.6493558817514,-42.6794227480187,
122.11001697531)) ;
#108448 = CARTESIAN_POINT('Ctrl Pts',(-18.4340956755043,-42.6894502450088,
122.26199628503)) ;
#108449 = CARTESIAN_POINT('Ctrl Pts',(-18.2489571690901,-42.6994786970539,
122.449567162524)) ;
#108450 = CARTESIAN_POINT('Ctrl Pts',(-18.1015454019537,-42.709323963618,
122.662170651268)) ;
#108451 = CARTESIAN_POINT('Ctrl Pts',(-17.9910414028632,-42.7193146365589,
122.900334782034)) ;
#108452 = CARTESIAN_POINT('Ctrl Pts',(-17.9238206505132,-42.7293525186474,
123.155408137514)) ;
#108453 = CARTESIAN_POINT('Ctrl Pts',(-17.9018814338395,-42.739196889087,
123.41318653434)) ;
#108454 = CARTESIAN_POINT('Ctrl Pts',(-17.924844360066,-42.7491817164824,
123.674534933171)) ;
#108455 = CARTESIAN_POINT('Ctrl Pts',(-17.9924345358582,-42.7591211618877,
123.926875989498)) ;
#108456 = CARTESIAN_POINT('Ctrl Pts',(-18.1039701355728,-42.7691611661736,
124.165953010271)) ;
#108457 = CARTESIAN_POINT('Ctrl Pts',(-18.2529049853571,-42.7790482753592,
124.378889495216)) ;
#108458 = CARTESIAN_POINT('Ctrl Pts',(-18.4383679788379,-42.7890483352617,
124.565011599206)) ;
#108459 = CARTESIAN_POINT('Ctrl Pts',(-18.6514946875924,-42.7989657511764,
124.715085242335)) ;
#108460 = CARTESIAN_POINT('Ctrl Pts',(-18.8904787338854,-42.8090125659172,
124.827216311811)) ;
#108461 = CARTESIAN_POINT('Ctrl Pts',(-19.1409637043585,-42.8188880431139,
124.89525183759)) ;
#108462 = CARTESIAN_POINT('Ctrl Pts',(-19.4040830147248,-42.8289441388351,
124.919328928823)) ;
#108463 = CARTESIAN_POINT('Ctrl Pts',(-19.6632223451092,-42.8388373008502,
124.897799579971)) ;
#108464 = CARTESIAN_POINT('Ctrl Pts',(-19.9189229517029,-42.8488995368728,
124.830568230373)) ;
#108465 = CARTESIAN_POINT('Ctrl Pts',(-20.1539191213786,-42.8587440025017,
124.722359394121)) ;
#108466 = CARTESIAN_POINT('Ctrl Pts',(-20.3695791509415,-42.8687040952058,
124.574045748429)) ;
#108467 = CARTESIAN_POINT('Ctrl Pts',(-20.5573059185515,-42.8787423841869,
124.388734758303)) ;
#108468 = CARTESIAN_POINT('Ctrl Pts',(-20.7079330225329,-42.8886157072931,
124.177424425734)) ;
#108469 = CARTESIAN_POINT('Ctrl Pts',(-20.8217253254102,-42.8986888913782,
123.938476998425)) ;
#108470 = CARTESIAN_POINT('Ctrl Pts',(-20.8908827499387,-42.9085094036661,
123.689783809996)) ;
#108471 = CARTESIAN_POINT('Ctrl Pts',(-20.9167041508658,-42.9185873997819,
123.426269445096)) ;
#108472 = CARTESIAN_POINT('Ctrl Pts',(-20.8968822449302,-42.9284414747652,
123.168014102348)) ;
#108473 = CARTESIAN_POINT('Ctrl Pts',(-20.8314569368461,-42.9385053563489,
122.911818705928)) ;
#108474 = CARTESIAN_POINT('Ctrl Pts',(-20.7244115567648,-42.9483887823227,
122.675128176596)) ;
#108475 = CARTESIAN_POINT('Ctrl Pts',(-20.5765556238842,-42.9583893862437,
122.45791601346)) ;
#108476 = CARTESIAN_POINT('Ctrl Pts',(-20.3947650338374,-42.9683091705816,
122.271014843434)) ;
#108477 = CARTESIAN_POINT('Ctrl Pts',(-20.1806024800397,-42.9783565209384,
122.116660959539)) ;
#108478 = CARTESIAN_POINT('Ctrl Pts',(-19.9469622159444,-42.9882338631727,
122.003462045273)) ;
#108479 = CARTESIAN_POINT('Ctrl Pts',(-19.6924449489111,-42.9983037442474,
121.931213874839)) ;
#108480 = CARTESIAN_POINT('Ctrl Pts',(-19.4354546046545,-43.008133449449,
121.904618856356)) ;
#108481 = CARTESIAN_POINT('Ctrl Pts',(-19.1716059344272,-43.0182001106154,
121.923134771065)) ;
#108482 = CARTESIAN_POINT('Ctrl Pts',(-18.9194441886432,-43.0280903324827,
121.986237501983)) ;
#108483 = CARTESIAN_POINT('Ctrl Pts',(-18.6794320360846,-43.0380825085929,
122.092711334672)) ;
#108484 = CARTESIAN_POINT('Ctrl Pts',(-18.4623247536949,-43.0480453387055,
122.239022821817)) ;
#108485 = CARTESIAN_POINT('Ctrl Pts',(-18.2745479615962,-43.0579495511058,
122.419282436697)) ;
#108486 = CARTESIAN_POINT('Ctrl Pts',(-18.1187192118051,-43.0680102651937,
122.632820549184)) ;
#108487 = CARTESIAN_POINT('Ctrl Pts',(-18.0045425253802,-43.0778497681765,
122.864864491798)) ;
#108488 = CARTESIAN_POINT('Ctrl Pts',(-17.9304931125037,-43.0879159067429,
123.118771690062)) ;
#108489 = CARTESIAN_POINT('Ctrl Pts',(-17.9022688621809,-43.0977984212289,
123.376975393947)) ;
#108490 = CARTESIAN_POINT('Ctrl Pts',(-17.9189748412503,-43.1077907205845,
123.638990434993)) ;
#108491 = CARTESIAN_POINT('Ctrl Pts',(-17.980632945577,-43.1177437875379,
123.89321577407)) ;
#108492 = CARTESIAN_POINT('Ctrl Pts',(-18.0864334578628,-43.1277784957431,
124.134740590676)) ;
#108493 = CARTESIAN_POINT('Ctrl Pts',(-18.2302918456432,-43.1376667166473,
124.35115739606)) ;
#108494 = CARTESIAN_POINT('Ctrl Pts',(-18.4111337778499,-43.1476611396777,
124.54160421321)) ;
#108495 = CARTESIAN_POINT('Ctrl Pts',(-18.6213333522746,-43.1576064791239,
124.696916870791)) ;
#108496 = CARTESIAN_POINT('Ctrl Pts',(-18.8551254938992,-43.1675538237352,
124.813883031266)) ;
#108497 = CARTESIAN_POINT('Ctrl Pts',(-19.1082720190948,-43.1776017191462,
124.888940157989)) ;
#108498 = CARTESIAN_POINT('Ctrl Pts',(-19.3653633267677,-43.1874493646256,
124.918525063394)) ;
#108499 = CARTESIAN_POINT('Ctrl Pts',(-19.6267119617915,-43.1974110785396,
124.903661025087)) ;
#108500 = CARTESIAN_POINT('Ctrl Pts',(-19.8831726151699,-43.2074397028305,
124.842909625161)) ;
#108501 = CARTESIAN_POINT('Ctrl Pts',(-20.1223420758362,-43.2173500634872,
124.739869624029)) ;
#108502 = CARTESIAN_POINT('Ctrl Pts',(-20.3409183277363,-43.2272847620605,
124.597079858644)) ;
#108503 = CARTESIAN_POINT('Ctrl Pts',(-20.5332396283574,-43.2373265869147,
124.416406754811)) ;
#108504 = CARTESIAN_POINT('Ctrl Pts',(-20.6889998581201,-43.2472111606591,
124.20850068406)) ;
#108505 = CARTESIAN_POINT('Ctrl Pts',(-20.8079393724832,-43.2572130100223,
123.974153556956)) ;
#108506 = CARTESIAN_POINT('Ctrl Pts',(-20.8839549135246,-43.2671323115963,
123.724778206695)) ;
#108507 = CARTESIAN_POINT('Ctrl Pts',(-20.9159120162296,-43.2771764199416,
123.462793249305)) ;
#108508 = CARTESIAN_POINT('Ctrl Pts',(-20.9021938783438,-43.2870608433839,
123.203391169595)) ;
#108509 = CARTESIAN_POINT('Ctrl Pts',(-20.8434325546442,-43.2970772052933,
122.946804609188)) ;
#108510 = CARTESIAN_POINT('Ctrl Pts',(-20.7401748840849,-43.3071138607987,
122.704120206209)) ;
#108511 = CARTESIAN_POINT('Ctrl Pts',(-20.5998726346924,-43.316943990988,
122.487178184028)) ;
#108512 = CARTESIAN_POINT('Ctrl Pts',(-20.4197573959054,-43.3270200440779,
122.293157016589)) ;
#108513 = CARTESIAN_POINT('Ctrl Pts',(-20.2133796379951,-43.3368722732637,
122.136730156183)) ;
#108514 = CARTESIAN_POINT('Ctrl Pts',(-19.9779977934411,-43.346945481063,
122.015709849871)) ;
#108515 = CARTESIAN_POINT('Ctrl Pts',(-19.7309152909117,-43.3567869924144,
121.939250075785)) ;
#108516 = CARTESIAN_POINT('Ctrl Pts',(-19.4713473599111,-43.3667479304519,
121.905485975715)) ;
#108517 = CARTESIAN_POINT('Ctrl Pts',(-19.2078648410812,-43.3767857923769,
121.917923560275)) ;
#108518 = CARTESIAN_POINT('Ctrl Pts',(-18.9545933568594,-43.386659978374,
121.974511790238)) ;
#108519 = CARTESIAN_POINT('Ctrl Pts',(-18.7103144862265,-43.3967301379519,
122.076190688667)) ;
#108520 = CARTESIAN_POINT('Ctrl Pts',(-18.4925372665596,-43.4065618853777,
122.215260760015)) ;
#108521 = CARTESIAN_POINT('Ctrl Pts',(-18.2978258112365,-43.416597965449,
122.393131044889)) ;
#108522 = CARTESIAN_POINT('Ctrl Pts',(-18.1377717670256,-43.4266150123015,
122.602137878926)) ;
#108523 = CARTESIAN_POINT('Ctrl Pts',(-18.0176420342896,-43.4364972704681,
122.832383191886)) ;
#108524 = CARTESIAN_POINT('Ctrl Pts',(-17.9382017148114,-43.4464849532645,
123.082509715295)) ;
#108525 = CARTESIAN_POINT('Ctrl Pts',(-17.9033225321258,-43.4564316099812,
123.341600746611)) ;
#108526 = CARTESIAN_POINT('Ctrl Pts',(-17.9143468061501,-43.4664886680613,
123.605630312253)) ;
#108527 = CARTESIAN_POINT('Ctrl Pts',(-17.9693606834189,-43.4763068476108,
123.857723199161)) ;
#108528 = CARTESIAN_POINT('Ctrl Pts',(-18.068813138395,-43.4863427820498,
124.101979443464)) ;
#108529 = CARTESIAN_POINT('Ctrl Pts',(-18.2096563573265,-43.4963674364788,
124.324617133283)) ;
#108530 = CARTESIAN_POINT('Ctrl Pts',(-18.3835357390967,-43.5062194560583,
124.516444902272)) ;
#108531 = CARTESIAN_POINT('Ctrl Pts',(-18.5906910966535,-43.5162103697732,
124.677699425909)) ;
#108532 = CARTESIAN_POINT('Ctrl Pts',(-18.8209814559814,-43.5261283586128,
124.799818206441)) ;
#108533 = CARTESIAN_POINT('Ctrl Pts',(-19.0716619099763,-43.5361564693436,
124.881031637692)) ;
#108534 = CARTESIAN_POINT('Ctrl Pts',(-19.3289275583956,-43.546041667252,
124.91707739968)) ;
#108535 = CARTESIAN_POINT('Ctrl Pts',(-19.5913007390015,-43.55603094252,124.90845061953)) ;
#108536 = CARTESIAN_POINT('Ctrl Pts',(-19.8494016769146,-43.5660724006895,
124.853560006416)) ;
#108537 = CARTESIAN_POINT('Ctrl Pts',(-20.089126965417,-43.5759038644778,
124.757190574389)) ;
#108538 = CARTESIAN_POINT('Ctrl Pts',(-20.3126215899426,-43.5859087967817,
124.618769996767)) ;
#108539 = CARTESIAN_POINT('Ctrl Pts',(-20.5082846379011,-43.5958951606764,
124.443812980393)) ;
#108540 = CARTESIAN_POINT('Ctrl Pts',(-20.6710952998736,-43.6059247895623,
124.236573038023)) ;
#108541 = CARTESIAN_POINT('Ctrl Pts',(-20.7938534841655,-43.6158000116707,
124.007904553605)) ;
#108542 = CARTESIAN_POINT('Ctrl Pts',(-20.8763533612149,-43.6258012240678,
123.758410827057)) ;
#108543 = CARTESIAN_POINT('Ctrl Pts',(-20.914185635291,-43.6357098033033,
123.500740267426)) ;
#108544 = CARTESIAN_POINT('Ctrl Pts',(-20.9065152821478,-43.6457646558593,
123.236663666246)) ;
#108545 = CARTESIAN_POINT('Ctrl Pts',(-20.8544254443002,-43.6556232381341,
122.982834271091)) ;
#108546 = CARTESIAN_POINT('Ctrl Pts',(-20.7572075900671,-43.6656913675768,
122.736804469327)) ;
#108547 = CARTESIAN_POINT('Ctrl Pts',(-20.6216226854685,-43.6755468392659,
122.516112932406)) ;
#108548 = CARTESIAN_POINT('Ctrl Pts',(-20.4479582876326,-43.6855416876521,
122.319076542541)) ;
#108549 = CARTESIAN_POINT('Ctrl Pts',(-20.2416064978002,-43.6955729844366,
122.155024885299)) ;
#108550 = CARTESIAN_POINT('Ctrl Pts',(-20.0139042025043,-43.7054395206467,
122.030994761445)) ;
#108551 = CARTESIAN_POINT('Ctrl Pts',(-19.7652860328304,-43.7154269436075,
121.946983535015)) ;
#108552 = CARTESIAN_POINT('Ctrl Pts',(-19.5069160345804,-43.7253718826273,
121.907441269783)) ;
#108553 = CARTESIAN_POINT('Ctrl Pts',(-19.2430357316301,-43.7354167684873,
121.913545634588)) ;
#108554 = CARTESIAN_POINT('Ctrl Pts',(-18.9887149200403,-43.7452853035735,
121.964332757131)) ;
#108555 = CARTESIAN_POINT('Ctrl Pts',(-18.7444455097126,-43.7552511715802,
122.05874888763)) ;
#108556 = CARTESIAN_POINT('Ctrl Pts',(-18.5191315338864,-43.7652738190327,
122.195184429335)) ;
#108557 = CARTESIAN_POINT('Ctrl Pts',(-18.3228637036449,-43.7751974580403,
122.366880554806)) ;
#108558 = CARTESIAN_POINT('Ctrl Pts',(-18.1585688776028,-43.785140183046,
122.570066593669)) ;
#108559 = CARTESIAN_POINT('Ctrl Pts',(-18.0310320495463,-43.7951857890979,
122.801185890142)) ;
#108560 = CARTESIAN_POINT('Ctrl Pts',(-17.9468480696797,-43.805047211619,
123.046302545055)) ;
#108561 = CARTESIAN_POINT('Ctrl Pts',(-17.9055287972533,-43.8150407800682,
123.305614180194)) ;
#108562 = CARTESIAN_POINT('Ctrl Pts',(-17.9096981897941,-43.8249662508235,
123.566450318182)) ;
#108563 = CARTESIAN_POINT('Ctrl Pts',(-17.959577021804,-43.8349939247794,
123.825170364264)) ;
#108564 = CARTESIAN_POINT('Ctrl Pts',(-18.0520913255646,-43.8448811028211,
124.068003666983)) ;
#108565 = CARTESIAN_POINT('Ctrl Pts',(-18.1870726266539,-43.8549094821892,
124.29430476118)) ;
#108566 = CARTESIAN_POINT('Ctrl Pts',(-18.356931127565,-43.8648037249107,
124.491207973471)) ;
#108567 = CARTESIAN_POINT('Ctrl Pts',(-18.6285761936577,-43.8781566415616,
124.713286249922)) ;
#108568 = CARTESIAN_POINT('Ctrl Pts',(-18.948383164132,-43.8913591593083,
124.857812283669)) ;
#108569 = CARTESIAN_POINT('Ctrl Pts',(-19.2946498883519,-43.9047150645893,
124.914940485275)) ;
#108570 = CARTESIAN_POINT('Ctrl Pts',(-19.5547438289061,-43.9146117132271,
124.912309586641)) ;
#108571 = CARTESIAN_POINT('Ctrl Pts',(-19.8143049394651,-43.9246598512796,
124.863922492952)) ;
#108572 = CARTESIAN_POINT('Ctrl Pts',(-20.0576815747362,-43.9345508114574,
124.77263287154)) ;
#108573 = CARTESIAN_POINT('Ctrl Pts',(-20.2841489081808,-43.9445436473341,
124.639680505844)) ;
#108574 = CARTESIAN_POINT('Ctrl Pts',(-20.4846062456997,-43.9545827423357,
124.468189074761)) ;
#108575 = CARTESIAN_POINT('Ctrl Pts',(-20.6493647056431,-43.9644200981869,
124.268942295104)) ;
#108576 = CARTESIAN_POINT('Ctrl Pts',(-20.8232997802523,-43.9778130461176,
123.96303203667)) ;
#108577 = CARTESIAN_POINT('Ctrl Pts',(-20.9119483564918,-43.9909797225445,
123.624406077728)) ;
#108578 = CARTESIAN_POINT('Ctrl Pts',(-20.910325463326,-44.0043645039513,
123.272727081459)) ;
#108579 = CARTESIAN_POINT('Ctrl Pts',(-20.864238880758,-44.0142262865952,
123.01765838927)) ;
#108580 = CARTESIAN_POINT('Ctrl Pts',(-20.7737497681902,-44.0242254345482,
122.771019118975)) ;
#108581 = CARTESIAN_POINT('Ctrl Pts',(-20.6432368005239,-44.0341282271653,
122.545814143778)) ;
#108582 = CARTESIAN_POINT('Ctrl Pts',(-20.4731399955561,-44.0441778070562,
122.343878608251)) ;
#108583 = CARTESIAN_POINT('Ctrl Pts',(-20.2076059725452,-44.0573648808657,
122.121012079082)) ;
#108584 = CARTESIAN_POINT('Ctrl Pts',(-19.8041322252334,-44.0741176708369,
121.933097855495)) ;
#108585 = CARTESIAN_POINT('Ctrl Pts',(-19.3673869325287,-44.0906063229316,
121.894835933027)) ;
#108586 = CARTESIAN_POINT('Ctrl Pts',(-19.0216674963533,-44.103963149115,
121.955027343524)) ;
#108587 = CARTESIAN_POINT('Ctrl Pts',(-18.7770005207847,-44.1138595339929,
122.043352858125)) ;
#108588 = CARTESIAN_POINT('Ctrl Pts',(-18.5489164371702,-44.1238660485134,
122.17407896693)) ;
#108589 = CARTESIAN_POINT('Ctrl Pts',(-18.2820370334625,-44.1370561720298,
122.395456324411)) ;
#108590 = CARTESIAN_POINT('Ctrl Pts',(-18.0248472685587,-44.1538227331793,
122.759183838279)) ;
#108591 = CARTESIAN_POINT('Ctrl Pts',(-17.886054152953,-44.1736072218874,
123.266528761718)) ;
#108592 = CARTESIAN_POINT('Ctrl Pts',(-17.9274102999763,-44.1935526694839,
123.794897481469)) ;
#108593 = CARTESIAN_POINT('Ctrl Pts',(-18.1467356431328,-44.2134643316398,
124.276542042476)) ;
#108594 = CARTESIAN_POINT('Ctrl Pts',(-18.5161061142021,-44.2333565236587,
124.654929487936)) ;
#108595 = CARTESIAN_POINT('Ctrl Pts',(-18.9962004191449,-44.2533976542133,
124.885489162055)) ;
#108596 = CARTESIAN_POINT('Ctrl Pts',(-19.5204345314535,-44.2732159888289,
124.938089811446)) ;
#108597 = CARTESIAN_POINT('Ctrl Pts',(-20.0350360289523,-44.2931885540485,
124.808536609141)) ;
#108598 = CARTESIAN_POINT('Ctrl Pts',(-20.473093222117,-44.3130777702201,
124.512295701165)) ;
#108599 = CARTESIAN_POINT('Ctrl Pts',(-20.7853732663462,-44.3331013445428,
124.08151681092)) ;
#108600 = CARTESIAN_POINT('Ctrl Pts',(-20.9306784904965,-44.352898507631,
123.575705617938)) ;
#108601 = CARTESIAN_POINT('Ctrl Pts',(-20.8956409075036,-44.3728640014548,
123.046325488981)) ;
#108602 = CARTESIAN_POINT('Ctrl Pts',(-20.681482209836,-44.3928177091962,
122.560997313909)) ;
#108603 = CARTESIAN_POINT('Ctrl Pts',(-20.3156124672634,-44.4127250859228,
122.178943118097)) ;
#108604 = CARTESIAN_POINT('Ctrl Pts',(-19.8430851406969,-44.4325772974714,
121.94396651336)) ;
#108605 = CARTESIAN_POINT('Ctrl Pts',(-19.3129697699881,-44.4526496844171,
121.88421408573)) ;
#108606 = CARTESIAN_POINT('Ctrl Pts',(-18.8004875339095,-44.4724875540574,
122.008175589583)) ;
#108607 = CARTESIAN_POINT('Ctrl Pts',(-18.3595296194666,-44.4923382086105,
122.297851154628)) ;
#108608 = CARTESIAN_POINT('Ctrl Pts',(-18.0413388756731,-44.512390142951,
122.725336395254)) ;
#108609 = CARTESIAN_POINT('Ctrl Pts',(-17.8898208181151,-44.532223330517,
123.23034909197)) ;
#108610 = CARTESIAN_POINT('Ctrl Pts',(-17.9188074653872,-44.5521525427477,
123.759044469505)) ;
#108611 = CARTESIAN_POINT('Ctrl Pts',(-18.1255875324458,-44.5720375079621,
124.245643141328)) ;
#108612 = CARTESIAN_POINT('Ctrl Pts',(-18.4898169288741,-44.5921112491067,
124.635352509745)) ;
#108613 = CARTESIAN_POINT('Ctrl Pts',(-18.9586647938728,-44.6119044308871,
124.874137361605)) ;
#108614 = CARTESIAN_POINT('Ctrl Pts',(-19.4850008685489,-44.6318671388898,
124.940732867098)) ;
#108615 = CARTESIAN_POINT('Ctrl Pts',(-20.0027588463674,-44.6518500906322,
124.822336742244)) ;
#108616 = CARTESIAN_POINT('Ctrl Pts',(-20.4457804417171,-44.6716607104044,
124.537702205694)) ;
#108617 = CARTESIAN_POINT('Ctrl Pts',(-20.7682682433341,-44.6916444264373,
124.115825296363)) ;
#108618 = CARTESIAN_POINT('Ctrl Pts',(-20.9266119031138,-44.7115258903346,
123.611552263103)) ;
#108619 = CARTESIAN_POINT('Ctrl Pts',(-20.9036659950878,-44.731481220179,
123.08177562687)) ;
#108620 = CARTESIAN_POINT('Ctrl Pts',(-20.7024070889565,-44.7513566809845,
122.593268939263)) ;
#108621 = CARTESIAN_POINT('Ctrl Pts',(-20.3449059579803,-44.771341001036,
122.200518916191)) ;
#108622 = CARTESIAN_POINT('Ctrl Pts',(-19.8758735906964,-44.7912690338256,
121.954214849087)) ;
#108623 = CARTESIAN_POINT('Ctrl Pts',(-19.438578805638,-44.8078777957654,
121.894601445144)) ;
#108624 = CARTESIAN_POINT('Ctrl Pts',(-19.0946773195498,-44.8210654344555,
121.9376322726)) ;
#108625 = CARTESIAN_POINT('Ctrl Pts',(-18.8437209444758,-44.8310518688156,
122.014347849568)) ;
#108626 = CARTESIAN_POINT('Ctrl Pts',(-18.6094583387565,-44.841061242775,
122.133996670007)) ;
#108627 = CARTESIAN_POINT('Ctrl Pts',(-18.3305913715183,-44.8543512763403,
122.344268776071)) ;
#108628 = CARTESIAN_POINT('Ctrl Pts',(-18.0587975390607,-44.8709452640027,
122.691629909638)) ;
#108629 = CARTESIAN_POINT('Ctrl Pts',(-17.9215519402964,-44.8875775192782,
123.111821893515)) ;
#108630 = CARTESIAN_POINT('Ctrl Pts',(-17.9026701922283,-44.9008199029461,
123.459315264525)) ;
#108631 = CARTESIAN_POINT('Ctrl Pts',(-17.9331210763156,-44.9107341111735,
123.718074029776)) ;
#108632 = CARTESIAN_POINT('Ctrl Pts',(-18.0093944626743,-44.9207907504452,
123.971085550191)) ;
#108633 = CARTESIAN_POINT('Ctrl Pts',(-18.1256855379854,-44.9306365568653,
124.202241165926)) ;
#108634 = CARTESIAN_POINT('Ctrl Pts',(-18.2830906349234,-44.9406815564985,
124.414133633977)) ;
#108635 = CARTESIAN_POINT('Ctrl Pts',(-18.5370488897799,-44.9539625788713,
124.653520523732)) ;
#108636 = CARTESIAN_POINT('Ctrl Pts',(-18.8452706151881,-44.9671600253959,
124.820978374713)) ;
#108637 = CARTESIAN_POINT('Ctrl Pts',(-19.1881208578501,-44.9805743232029,
124.903002035483)) ;
#108638 = CARTESIAN_POINT('Ctrl Pts',(-19.4462158275204,-44.9904133886056,
124.918740428839)) ;
#108639 = CARTESIAN_POINT('Ctrl Pts',(-19.7069222802875,-45.0003965948833,
124.889687530317)) ;
#108640 = CARTESIAN_POINT('Ctrl Pts',(-19.9578337616693,-45.0103478297961,
124.815948358153)) ;
#108641 = CARTESIAN_POINT('Ctrl Pts',(-20.1934407068406,-45.0203488294977,
124.699467451423)) ;
#108642 = CARTESIAN_POINT('Ctrl Pts',(-20.4056291656955,-45.0303801752851,
124.543050170843)) ;
#108643 = CARTESIAN_POINT('Ctrl Pts',(-20.5844817934518,-45.0402339399901,
124.355784465079)) ;
#108644 = CARTESIAN_POINT('Ctrl Pts',(-20.730306116653,-45.0502045936584,
124.138128056574)) ;
#108645 = CARTESIAN_POINT('Ctrl Pts',(-20.8364235167749,-45.0602018373156,
123.897752942443)) ;
#108646 = CARTESIAN_POINT('Ctrl Pts',(-20.8990754352481,-45.0702352932598,
123.641658311866)) ;
#108647 = CARTESIAN_POINT('Ctrl Pts',(-20.9164257862816,-45.0800907975602,
123.383222452894)) ;
#108648 = CARTESIAN_POINT('Ctrl Pts',(-20.8885903520797,-45.0900902338463,
123.121973185214)) ;
#108649 = CARTESIAN_POINT('Ctrl Pts',(-20.8168393384412,-45.0999846933622,
122.872001936455)) ;
#108650 = CARTESIAN_POINT('Ctrl Pts',(-20.7008020992867,-45.1100478128138,
122.634422440595)) ;
#108651 = CARTESIAN_POINT('Ctrl Pts',(-20.5489090568532,-45.1198874472258,
122.425109333317)) ;
#108652 = CARTESIAN_POINT('Ctrl Pts',(-20.3590464678608,-45.1299506547116,
122.241080148602)) ;
#108653 = CARTESIAN_POINT('Ctrl Pts',(-20.143616765248,-45.1398447620908,
122.095446265196)) ;
#108654 = CARTESIAN_POINT('Ctrl Pts',(-19.90536102435,-45.1497870942832,121.988302155594)) ;
#108655 = CARTESIAN_POINT('Ctrl Pts',(-19.6505929754798,-45.1597877205982,
121.923634229427)) ;
#108656 = CARTESIAN_POINT('Ctrl Pts',(-19.3874182812413,-45.1698294548801,
121.904600717031)) ;
#108657 = CARTESIAN_POINT('Ctrl Pts',(-19.1304894002943,-45.1796548808292,
121.930404916149)) ;
#108658 = CARTESIAN_POINT('Ctrl Pts',(-18.8760225613039,-45.1897117073569,
122.001688985524)) ;
#108659 = CARTESIAN_POINT('Ctrl Pts',(-18.6409922371268,-45.1996391404784,
122.114947366633)) ;
#108660 = CARTESIAN_POINT('Ctrl Pts',(-18.428283078681,-45.2095891328847,
122.267030398883)) ;
#108661 = CARTESIAN_POINT('Ctrl Pts',(-18.2436293548006,-45.2196443339587,
122.456017242193)) ;
#108662 = CARTESIAN_POINT('Ctrl Pts',(-18.0976408516097,-45.229466608011,
122.66891028545)) ;
#108663 = CARTESIAN_POINT('Ctrl Pts',(-17.9878817132479,-45.2395225019702,
122.909275777523)) ;
#108664 = CARTESIAN_POINT('Ctrl Pts',(-17.9227281996274,-45.2494632238153,
123.162262403673)) ;
#108665 = CARTESIAN_POINT('Ctrl Pts',(-17.9017528415054,-45.2593675679019,
123.421696578876)) ;
#108666 = CARTESIAN_POINT('Ctrl Pts',(-17.9266573662769,-45.2694142352014,
123.684512768429)) ;
#108667 = CARTESIAN_POINT('Ctrl Pts',(-17.9955501165954,-45.2793097936513,
123.935309673887)) ;
#108668 = CARTESIAN_POINT('Ctrl Pts',(-18.1087830964484,-45.289371872356,
124.174216936959)) ;
#108669 = CARTESIAN_POINT('Ctrl Pts',(-18.258360118383,-45.2992145708218,
124.385273109242)) ;
#108670 = CARTESIAN_POINT('Ctrl Pts',(-18.4445967016622,-45.3092053447163,
124.570285917934)) ;
#108671 = CARTESIAN_POINT('Ctrl Pts',(-18.6588336632447,-45.3191332139512,
124.719195960976)) ;
#108672 = CARTESIAN_POINT('Ctrl Pts',(-18.8969306208894,-45.329121942921,
124.829738528518)) ;
#108673 = CARTESIAN_POINT('Ctrl Pts',(-19.1519909533467,-45.3391613449048,
124.89712446642)) ;
#108674 = CARTESIAN_POINT('Ctrl Pts',(-19.4096451598501,-45.3490015126416,
124.919272539632)) ;
#108675 = CARTESIAN_POINT('Ctrl Pts',(-19.6726846522424,-45.3590497230161,
124.896250057788)) ;
#108676 = CARTESIAN_POINT('Ctrl Pts',(-19.9250744800764,-45.3689968933038,
124.828188273529)) ;
#108677 = CARTESIAN_POINT('Ctrl Pts',(-20.161282054125,-45.3789077415589,
124.718447480095)) ;
#108678 = CARTESIAN_POINT('Ctrl Pts',(-20.3778191542026,-45.3889640692367,
124.566982119744)) ;
#108679 = CARTESIAN_POINT('Ctrl Pts',(-20.561118268851,-45.3988144820052,
124.384182606979)) ;
#108680 = CARTESIAN_POINT('Ctrl Pts',(-20.7130730814684,-45.4088413678389,
124.168919868791)) ;
#108681 = CARTESIAN_POINT('Ctrl Pts',(-20.8247497780107,-45.4188699834697,
123.930196528526)) ;
#108682 = CARTESIAN_POINT('Ctrl Pts',(-20.8924915813861,-45.4287152068472,
123.680514258014)) ;
#108683 = CARTESIAN_POINT('Ctrl Pts',(-20.9169002130611,-45.4387058889488,
123.419099763425)) ;
#108684 = CARTESIAN_POINT('Ctrl Pts',(-20.8948617738519,-45.4487437775813,
123.156239641148)) ;
#108685 = CARTESIAN_POINT('Ctrl Pts',(-20.8292495192011,-45.4585881126844,
122.905988466619)) ;
#108686 = CARTESIAN_POINT('Ctrl Pts',(-20.7201268218568,-45.4685730748819,
122.667400439687)) ;
#108687 = CARTESIAN_POINT('Ctrl Pts',(-20.5719794951113,-45.4785120164153,
122.45224941859)) ;
#108688 = CARTESIAN_POINT('Ctrl Pts',(-20.3868125283129,-45.4885539013867,
122.264265761858)) ;
#108689 = CARTESIAN_POINT('Ctrl Pts',(-20.1751991039344,-45.498440449295,
122.11348960682)) ;
#108690 = CARTESIAN_POINT('Ctrl Pts',(-19.9382932298207,-45.508434374795,
122.000209516617)) ;
#108691 = CARTESIAN_POINT('Ctrl Pts',(-19.6867430666025,-45.5183704659215,
121.930054267057)) ;
#108692 = CARTESIAN_POINT('Ctrl Pts',(-19.4244653461354,-45.5283997349014,
121.904461919994)) ;
#108693 = CARTESIAN_POINT('Ctrl Pts',(-19.1654769790705,-45.5382821174607,
121.924176829305)) ;
#108694 = CARTESIAN_POINT('Ctrl Pts',(-18.9095701072339,-45.5483346345486,
121.989564875615)) ;
#108695 = CARTESIAN_POINT('Ctrl Pts',(-18.6725611805939,-45.5582287553725,
122.096593974873)) ;
#108696 = CARTESIAN_POINT('Ctrl Pts',(-18.454122249887,-45.5682907347929,
122.245538250937)) ;
#108697 = CARTESIAN_POINT('Ctrl Pts',(-18.2689013297403,-45.5781352680218,
122.426165536045)) ;
#108698 = CARTESIAN_POINT('Ctrl Pts',(-18.1153278593355,-45.5880953469281,
122.638111849472)) ;
#108699 = CARTESIAN_POINT('Ctrl Pts',(-18.0004594417563,-45.5981336235007,
122.875570696473)) ;
#108700 = CARTESIAN_POINT('Ctrl Pts',(-17.9292550530874,-45.6080070100386,
123.125112116281)) ;
#108701 = CARTESIAN_POINT('Ctrl Pts',(-17.9020057930579,-45.6180799528056,
123.388361038033)) ;
#108702 = CARTESIAN_POINT('Ctrl Pts',(-17.9201003440477,-45.6279013669339,
123.645873411878)) ;
#108703 = CARTESIAN_POINT('Ctrl Pts',(-17.9839117490165,-45.6379759970062,
123.902769129534)) ;
#108704 = CARTESIAN_POINT('Ctrl Pts',(-18.0892730735631,-45.6478426343231,
124.139717934225)) ;
#108705 = CARTESIAN_POINT('Ctrl Pts',(-18.2358937929281,-45.6578661796949,
124.358532526418)) ;
#108706 = CARTESIAN_POINT('Ctrl Pts',(-18.4187982736359,-45.6678919312121,
124.548186844112)) ;
#108707 = CARTESIAN_POINT('Ctrl Pts',(-18.6279179687575,-45.6777455182215,
124.70087294293)) ;
#108708 = CARTESIAN_POINT('Ctrl Pts',(-18.8629921401903,-45.6877224784494,
124.816991235765)) ;
#108709 = CARTESIAN_POINT('Ctrl Pts',(-19.1158783884608,-45.6977436214779,
124.89042196862)) ;
#108710 = CARTESIAN_POINT('Ctrl Pts',(-19.3740455309343,-45.7076262274978,
124.918960029226)) ;
#108711 = CARTESIAN_POINT('Ctrl Pts',(-19.6380339189301,-45.7176946981305,
124.901825038415)) ;
#108712 = CARTESIAN_POINT('Ctrl Pts',(-19.8891097184639,-45.7275247813142,
124.840868485324)) ;
#108713 = CARTESIAN_POINT('Ctrl Pts',(-20.1315378133277,-45.7375913409946,
124.735100678908)) ;
#108714 = CARTESIAN_POINT('Ctrl Pts',(-20.3480312971626,-45.7474815908238,
124.591231930884)) ;
#108715 = CARTESIAN_POINT('Ctrl Pts',(-20.5385576486232,-45.7574737565726,
124.410560471012)) ;
#108716 = CARTESIAN_POINT('Ctrl Pts',(-20.6941656126137,-45.7674366001687,
124.200016201695)) ;
#108717 = CARTESIAN_POINT('Ctrl Pts',(-20.8107718164535,-45.7773407689965,
123.967301371836)) ;
#108718 = CARTESIAN_POINT('Ctrl Pts',(-20.8861323700367,-45.7874016438908,
123.713916570777)) ;
#108719 = CARTESIAN_POINT('Ctrl Pts',(-20.9160536921598,-45.7972405472202,
123.457055277836)) ;
#108720 = CARTESIAN_POINT('Ctrl Pts',(-20.9008271947572,-45.8073089235941,
123.192950934259)) ;
#108721 = CARTESIAN_POINT('Ctrl Pts',(-20.8410053145688,-45.8171895402267,
122.940244040831)) ;
#108722 = CARTESIAN_POINT('Ctrl Pts',(-20.7375809204795,-45.8271807004557,
122.698956739296)) ;
#108723 = CARTESIAN_POINT('Ctrl Pts',(-20.5943728761297,-45.8371337738878,
122.48004171132)) ;
#108724 = CARTESIAN_POINT('Ctrl Pts',(-20.4138196588889,-45.8471696095005,
122.287835517682)) ;
#108725 = CARTESIAN_POINT('Ctrl Pts',(-20.2057772654205,-45.8570597362306,
122.132027016977)) ;
#108726 = CARTESIAN_POINT('Ctrl Pts',(-19.9716662871303,-45.8670519179999,
122.013135288899)) ;
#108727 = CARTESIAN_POINT('Ctrl Pts',(-19.7215916075349,-45.8769978579744,
121.937133118513)) ;
#108728 = CARTESIAN_POINT('Ctrl Pts',(-19.4621372390162,-45.8869450417339,
121.905174548949)) ;
#108729 = CARTESIAN_POINT('Ctrl Pts',(-19.1984689476946,-45.8969929800242,
121.919182730932)) ;
#108730 = CARTESIAN_POINT('Ctrl Pts',(-18.9463055895591,-45.9068406148377,
121.977361332279)) ;
#108731 = CARTESIAN_POINT('Ctrl Pts',(-18.7050086728077,-45.9168023285357,
122.078849493128)) ;
#108732 = CARTESIAN_POINT('Ctrl Pts',(-18.4836777713451,-45.9268309643569,
122.22194223654)) ;
#108733 = CARTESIAN_POINT('Ctrl Pts',(-18.2927960619033,-45.9367412791087,
122.399094647672)) ;
#108734 = CARTESIAN_POINT('Ctrl Pts',(-18.1346245699497,-45.9466761497713,
122.606816266762)) ;
#108735 = CARTESIAN_POINT('Ctrl Pts',(-18.0138763110192,-45.9567173321731,
122.841426333629)) ;
#108736 = CARTESIAN_POINT('Ctrl Pts',(-17.9366880133725,-45.9666043036378,
123.089539209515)) ;
#108737 = CARTESIAN_POINT('Ctrl Pts',(-17.903054057272,-45.9766037359004,
123.350118250912)) ;
#108738 = CARTESIAN_POINT('Ctrl Pts',(-17.9149071079887,-45.986523801157,
123.61056930821)) ;
#108739 = CARTESIAN_POINT('Ctrl Pts',(-17.9724111669176,-45.9965606537412,
123.867967455661)) ;
#108740 = CARTESIAN_POINT('Ctrl Pts',(-18.0724951338109,-46.0064733130812,
124.108473552812)) ;
#108741 = CARTESIAN_POINT('Ctrl Pts',(-18.2134549140274,-46.0164645249961,
124.33000369932)) ;
#108742 = CARTESIAN_POINT('Ctrl Pts',(-18.392045730638,-46.0265061663992,
124.5242428558)) ;
#108743 = CARTESIAN_POINT('Ctrl Pts',(-18.5968569497117,-46.0363349606062,
124.681674981038)) ;
#108744 = CARTESIAN_POINT('Ctrl Pts',(-18.8315310091888,-46.0464113717275,
124.804221895689)) ;
#108745 = CARTESIAN_POINT('Ctrl Pts',(-19.0783635224015,-46.05626350477,124.882541551475)) ;
#108746 = CARTESIAN_POINT('Ctrl Pts',(-19.3406766420535,-46.0663367391113,
124.917791398394)) ;
#108747 = CARTESIAN_POINT('Ctrl Pts',(-19.5990992068201,-46.0761782404379,
124.907133995908)) ;
#108748 = CARTESIAN_POINT('Ctrl Pts',(-19.8549956383658,-46.0861391920327,
124.852064477482)) ;
#108749 = CARTESIAN_POINT('Ctrl Pts',(-20.0991149474506,-46.0961770097533,
124.752149387544)) ;
#108750 = CARTESIAN_POINT('Ctrl Pts',(-20.3188362146847,-46.1060513590104,
124.614043715742)) ;
#108751 = CARTESIAN_POINT('Ctrl Pts',(-20.5149807322072,-46.1161209097526,
124.436476561148)) ;
#108752 = CARTESIAN_POINT('Ctrl Pts',(-20.6736722161345,-46.1259549292612,
124.232479163217)) ;
#108753 = CARTESIAN_POINT('Ctrl Pts',(-20.7975880198892,-46.1359890838408,
123.999738628895)) ;
#108754 = CARTESIAN_POINT('Ctrl Pts',(-20.8784509574842,-46.1460050096632,
123.749243628566)) ;
#108755 = CARTESIAN_POINT('Ctrl Pts',(-20.914569442512,-46.1558872648575,
123.492067690217)) ;
#108756 = CARTESIAN_POINT('Ctrl Pts',(-20.9057131906475,-46.1658760713684,
123.229750694541)) ;
#108757 = CARTESIAN_POINT('Ctrl Pts',(-20.8518432319464,-46.1758246386311,
122.973880767554)) ;
#108758 = CARTESIAN_POINT('Ctrl Pts',(-20.7530881949105,-46.1858794439331,
122.728830454846)) ;
#108759 = CARTESIAN_POINT('Ctrl Pts',(-20.616861039315,-46.1956982271967,
122.509679270386)) ;
#108760 = CARTESIAN_POINT('Ctrl Pts',(-20.4413862067466,-46.2057339995573,
122.312807403627)) ;
#108761 = CARTESIAN_POINT('Ctrl Pts',(-20.2341435625144,-46.2157586985859,
122.150156536869)) ;
#108762 = CARTESIAN_POINT('Ctrl Pts',(-20.0060839751312,-46.225610701845,
122.027597836043)) ;
#108763 = CARTESIAN_POINT('Ctrl Pts',(-19.7569013276047,-46.2356016362422,
121.944987272963)) ;
#108764 = CARTESIAN_POINT('Ctrl Pts',(-19.4990198248001,-46.2455195586733,
121.906997442967)) ;
#108765 = CARTESIAN_POINT('Ctrl Pts',(-19.2356109355224,-46.2555479143556,
121.91438415743)) ;
#108766 = CARTESIAN_POINT('Ctrl Pts',(-18.9811375988693,-46.2654321988662,
121.9665159898)) ;
#108767 = CARTESIAN_POINT('Ctrl Pts',(-18.7367232904005,-46.2754248827741,
122.062532371143)) ;
#108768 = CARTESIAN_POINT('Ctrl Pts',(-18.5121245339067,-46.2854536197818,
122.200417548312)) ;
#108769 = CARTESIAN_POINT('Ctrl Pts',(-18.3174648059646,-46.2953390164107,
122.372455585845)) ;
#108770 = CARTESIAN_POINT('Ctrl Pts',(-18.1536854309232,-46.3053269018246,
122.577525230124)) ;
#108771 = CARTESIAN_POINT('Ctrl Pts',(-18.0283328197363,-46.3152776044852,
122.807058543816)) ;
#108772 = CARTESIAN_POINT('Ctrl Pts',(-17.9441425252922,-46.3253179225826,
123.057086661871)) ;
#108773 = CARTESIAN_POINT('Ctrl Pts',(-17.9050337144746,-46.3351924879158,
123.313645809229)) ;
#108774 = CARTESIAN_POINT('Ctrl Pts',(-17.9108065541753,-46.3451921479769,
123.576320024146)) ;
#108775 = CARTESIAN_POINT('Ctrl Pts',(-17.9614072155006,-46.3551011431446,
123.831801481986)) ;
#108776 = CARTESIAN_POINT('Ctrl Pts',(-18.0570299497226,-46.3651558843079,
124.078073850991)) ;
#108777 = CARTESIAN_POINT('Ctrl Pts',(-18.1910796797002,-46.3750144962217,
124.299825387159)) ;
#108778 = CARTESIAN_POINT('Ctrl Pts',(-18.3650434011911,-46.385082618501,
124.499120432854)) ;
#108779 = CARTESIAN_POINT('Ctrl Pts',(-18.5666792864394,-46.3949380892042,
124.661696531821)) ;
#108780 = CARTESIAN_POINT('Ctrl Pts',(-18.7962802236369,-46.4049329486976,
124.789235436467)) ;
#108781 = CARTESIAN_POINT('Ctrl Pts',(-19.0456405246855,-46.4149642020395,
124.874751408958)) ;
#108782 = CARTESIAN_POINT('Ctrl Pts',(-19.3017283009167,-46.4248309009126,
124.91540592978)) ;
#108783 = CARTESIAN_POINT('Ctrl Pts',(-19.5641107930564,-46.4348177166638,
124.911356078805)) ;
#108784 = CARTESIAN_POINT('Ctrl Pts',(-19.8208682713964,-46.4447649218593,
124.86211148328)) ;
#108785 = CARTESIAN_POINT('Ctrl Pts',(-20.0674353060267,-46.4548079099855,
124.768047551192)) ;
#108786 = CARTESIAN_POINT('Ctrl Pts',(-20.2900663287834,-46.464675264607,
124.6350864802)) ;
#108787 = CARTESIAN_POINT('Ctrl Pts',(-20.4886338862107,-46.4746411579051,
124.464343377395)) ;
#108788 = CARTESIAN_POINT('Ctrl Pts',(-20.6553083272588,-46.4846649352812,
124.260344882409)) ;
#108789 = CARTESIAN_POINT('Ctrl Pts',(-20.7828063712465,-46.4945904832129,
124.032811453884)) ;
#108790 = CARTESIAN_POINT('Ctrl Pts',(-20.8695819126354,-46.5045309596339,
123.786403623247)) ;
#108791 = CARTESIAN_POINT('Ctrl Pts',(-20.9124062871689,-46.5145771692968,
123.525912277354)) ;
#108792 = CARTESIAN_POINT('Ctrl Pts',(-20.9096836689865,-46.5244384259586,
123.266760258342)) ;
#108793 = CARTESIAN_POINT('Ctrl Pts',(-20.8618196513803,-46.5344320542339,
123.00857542062)) ;
#108794 = CARTESIAN_POINT('Ctrl Pts',(-20.7705820075892,-46.5443574515441,
122.76418240708)) ;
#108795 = CARTESIAN_POINT('Ctrl Pts',(-20.6369729547702,-46.5543853594543,
122.537081187664)) ;
#108796 = CARTESIAN_POINT('Ctrl Pts',(-20.4685329267532,-46.5642716751235,
122.339230363842)) ;
#108797 = CARTESIAN_POINT('Ctrl Pts',(-20.2655078356452,-46.5743032700273,
122.171141137268)) ;
#108798 = CARTESIAN_POINT('Ctrl Pts',(-20.039837488491,-46.584185512979,122.042547711301)) ;
#108799 = CARTESIAN_POINT('Ctrl Pts',(-19.790986603335,-46.5942449840088,
121.953442353936)) ;
#108800 = CARTESIAN_POINT('Ctrl Pts',(-19.5353950516732,-46.604111428672,
121.909781009716)) ;
#108801 = CARTESIAN_POINT('Ctrl Pts',(-19.2735030852152,-46.6140775531207,
121.910349350795)) ;
#108802 = CARTESIAN_POINT('Ctrl Pts',(-19.0140998320504,-46.6241077965118,
121.957095565601)) ;
#108803 = CARTESIAN_POINT('Ctrl Pts',(-18.7699834924998,-46.6340008314649,
122.046588137892)) ;
#108804 = CARTESIAN_POINT('Ctrl Pts',(-18.5415305597084,-46.6440517457017,
122.179105067727)) ;
#108805 = CARTESIAN_POINT('Ctrl Pts',(-18.342750038039,-46.6539415719263,
122.346547562767)) ;
#108806 = CARTESIAN_POINT('Ctrl Pts',(-18.1174517400336,-46.6672763869732,
122.614995956526)) ;
#108807 = CARTESIAN_POINT('Ctrl Pts',(-17.9686392139361,-46.6805534781447,
122.934913128643)) ;
#108808 = CARTESIAN_POINT('Ctrl Pts',(-17.9076787941137,-46.693801766743,
123.277725883847)) ;
#108809 = CARTESIAN_POINT('Ctrl Pts',(-17.9074679543351,-46.7038566082371,
123.541916040785)) ;
#108810 = CARTESIAN_POINT('Ctrl Pts',(-17.9516976277524,-46.7136875975446,
123.796495795355)) ;
#108811 = CARTESIAN_POINT('Ctrl Pts',(-18.0414367212003,-46.7237641618679,
124.045580065804)) ;
#108812 = CARTESIAN_POINT('Ctrl Pts',(-18.17013546342,-46.7336134870018,124.27017655509)) ;
#108813 = CARTESIAN_POINT('Ctrl Pts',(-18.3940809637255,-46.7469614866391,
124.540176759679)) ;
#108814 = CARTESIAN_POINT('Ctrl Pts',(-18.7539781559382,-46.7635462461757,
124.794640265119)) ;
#108815 = CARTESIAN_POINT('Ctrl Pts',(-19.178401102146,-46.7801147975237,
124.911971266093)) ;
#108816 = CARTESIAN_POINT('Ctrl Pts',(-19.5295056773098,-46.7934746223427,
124.914512890267)) ;
#108817 = CARTESIAN_POINT('Ctrl Pts',(-19.786214189388,-46.8033800311734,
124.871368392262)) ;
#108818 = CARTESIAN_POINT('Ctrl Pts',(-20.0329826854452,-46.8133400577574,
124.784198105326)) ;
#108819 = CARTESIAN_POINT('Ctrl Pts',(-20.3365985781968,-46.8265976419427,
124.613256266791)) ;
#108820 = CARTESIAN_POINT('Ctrl Pts',(-20.6530444857131,-46.8432488534374,
124.303863399263)) ;
#108821 = CARTESIAN_POINT('Ctrl Pts',(-20.8822282307178,-46.8631670675477,
123.826681959305)) ;
#108822 = CARTESIAN_POINT('Ctrl Pts',(-20.935851847913,-46.8830448307685,
123.301015754195)) ;
#108823 = CARTESIAN_POINT('Ctrl Pts',(-20.8055768749785,-46.9030574985557,
122.785411934825)) ;
#108824 = CARTESIAN_POINT('Ctrl Pts',(-20.5104582098003,-46.9228700212223,
122.349177441695)) ;
#108825 = CARTESIAN_POINT('Ctrl Pts',(-20.0811735104229,-46.9428533212222,
122.03661245177)) ;
#108826 = CARTESIAN_POINT('Ctrl Pts',(-19.5729864649457,-46.9627475983235,
121.890277286916)) ;
#108827 = CARTESIAN_POINT('Ctrl Pts',(-19.0443848766618,-46.9826803600813,
121.925379962756)) ;
#108828 = CARTESIAN_POINT('Ctrl Pts',(-18.5588179767112,-47.002646365846,
122.139461236973)) ;
#108829 = CARTESIAN_POINT('Ctrl Pts',(-18.1768456454212,-47.0225248980109,
122.504529177378)) ;
#108830 = CARTESIAN_POINT('Ctrl Pts',(-17.9412439125184,-47.0424645646712,
122.979181644419)) ;
#108831 = CARTESIAN_POINT('Ctrl Pts',(-17.8817257735614,-47.0623594393166,
123.504649624854)) ;
#108832 = CARTESIAN_POINT('Ctrl Pts',(-18.0046212015472,-47.0822665786099,
124.019152970604)) ;
#108833 = CARTESIAN_POINT('Ctrl Pts',(-18.2951649063741,-47.1021771266884,
124.461654024879)) ;
#108834 = CARTESIAN_POINT('Ctrl Pts',(-18.7231345570902,-47.1222457120455,
124.779809750388)) ;
#108835 = CARTESIAN_POINT('Ctrl Pts',(-19.226804714384,-47.1420275093603,
124.931228062656)) ;
#108836 = CARTESIAN_POINT('Ctrl Pts',(-19.7575681893512,-47.1620350563049,
124.902143874691)) ;
#108837 = CARTESIAN_POINT('Ctrl Pts',(-20.2423345965883,-47.1818567946077,
124.695505400649)) ;
#108838 = CARTESIAN_POINT('Ctrl Pts',(-20.6310620977836,-47.2018368145119,
124.333831088968)) ;
#108839 = CARTESIAN_POINT('Ctrl Pts',(-20.87170569344,-47.2217542657741,123.862294488323)) ;
#108840 = CARTESIAN_POINT('Ctrl Pts',(-20.9380824059377,-47.2416291869468,
123.338204944686)) ;
#108841 = CARTESIAN_POINT('Ctrl Pts',(-20.8204345579771,-47.2616535554976,
122.819191362508)) ;
#108842 = CARTESIAN_POINT('Ctrl Pts',(-20.5348082570627,-47.2815202398711,
122.37498839788)) ;
#108843 = CARTESIAN_POINT('Ctrl Pts',(-20.1137434665979,-47.3014640617173,
122.053088573225)) ;
#108844 = CARTESIAN_POINT('Ctrl Pts',(-19.6089193112748,-47.3213714309688,
121.894637053931)) ;
#108845 = CARTESIAN_POINT('Ctrl Pts',(-19.0811597470671,-47.3412461287155,
121.916943088499)) ;
#108846 = CARTESIAN_POINT('Ctrl Pts',(-18.5899719411168,-47.3612280712373,
122.118985961882)) ;
#108847 = CARTESIAN_POINT('Ctrl Pts',(-18.1991382375035,-47.3811307381481,
122.475368348256)) ;
#108848 = CARTESIAN_POINT('Ctrl Pts',(-17.9525186514706,-47.4009860956868,
122.942006158882)) ;
#108849 = CARTESIAN_POINT('Ctrl Pts',(-17.8797909685168,-47.4210501344028,
123.470209837654)) ;
#108850 = CARTESIAN_POINT('Ctrl Pts',(-17.9907794764626,-47.4409053141279,
123.986324657528)) ;
#108851 = CARTESIAN_POINT('Ctrl Pts',(-18.2724218178292,-47.4608854187923,
124.436282396569)) ;
#108852 = CARTESIAN_POINT('Ctrl Pts',(-18.6870135330641,-47.4806945239621,
124.761041750837)) ;
#108853 = CARTESIAN_POINT('Ctrl Pts',(-19.1917055879886,-47.5006871443028,
124.926757544361)) ;
#108854 = CARTESIAN_POINT('Ctrl Pts',(-19.6312174551831,-47.5172266268069,
124.913212879468)) ;
#108855 = CARTESIAN_POINT('Ctrl Pts',(-19.9675049947243,-47.5305909448711,
124.812128857147)) ;
#108856 = CARTESIAN_POINT('Ctrl Pts',(-20.277984697308,-47.5438085473726,
124.656243961923)) ;
#108857 = CARTESIAN_POINT('Ctrl Pts',(-20.6088670104154,-47.5604661416504,
124.362251795255)) ;
#108858 = CARTESIAN_POINT('Ctrl Pts',(-20.8603828060034,-47.5803318436921,
123.897898755475)) ;
#108859 = CARTESIAN_POINT('Ctrl Pts',(-20.9262201830231,-47.5969615703822,
123.460927621038)) ;
#108860 = CARTESIAN_POINT('Ctrl Pts',(-20.8869884578192,-47.61025068552,123.113852351726)) ;
#108861 = CARTESIAN_POINT('Ctrl Pts',(-20.8131428594769,-47.6202150324971,
122.86264462755)) ;
#108862 = CARTESIAN_POINT('Ctrl Pts',(-20.6973777337453,-47.6301434004986,
122.628839141613)) ;
#108863 = CARTESIAN_POINT('Ctrl Pts',(-20.4910418838649,-47.6434268335873,
122.347219669949)) ;
#108864 = CARTESIAN_POINT('Ctrl Pts',(-20.1458317228279,-47.6600789113277,
122.070296589039)) ;
#108865 = CARTESIAN_POINT('Ctrl Pts',(-19.7294313556018,-47.6766302806285,
121.928443166844)) ;
#108866 = CARTESIAN_POINT('Ctrl Pts',(-19.3810509337029,-47.6899177087775,
121.904509175098)) ;
#108867 = CARTESIAN_POINT('Ctrl Pts',(-19.1186147780108,-47.6999622484776,
121.932674760528)) ;
#108868 = CARTESIAN_POINT('Ctrl Pts',(-18.8700289913605,-47.7098050903014,
122.004211514632)) ;
#108869 = CARTESIAN_POINT('Ctrl Pts',(-18.6340718128688,-47.7197893745484,
122.118894210686)) ;
#108870 = CARTESIAN_POINT('Ctrl Pts',(-18.4223500836401,-47.7297390199475,
122.272337242117)) ;
#108871 = CARTESIAN_POINT('Ctrl Pts',(-18.2393375261666,-47.7397387816359,
122.460934913689)) ;
#108872 = CARTESIAN_POINT('Ctrl Pts',(-18.0917561865663,-47.7497701275948,
122.67936089865)) ;
#108873 = CARTESIAN_POINT('Ctrl Pts',(-17.9858813511188,-47.7596250820719,
122.915713531507)) ;
#108874 = CARTESIAN_POINT('Ctrl Pts',(-17.921313983943,-47.7695976200724,
123.169675068302)) ;
#108875 = CARTESIAN_POINT('Ctrl Pts',(-17.9017937695438,-47.7795926138074,
123.431647087822)) ;
#108876 = CARTESIAN_POINT('Ctrl Pts',(-17.928475189429,-47.7896266726015,
123.693955509307)) ;
#108877 = CARTESIAN_POINT('Ctrl Pts',(-17.9986334721321,-47.7994820154245,
123.943286670898)) ;
#108878 = CARTESIAN_POINT('Ctrl Pts',(-18.1123113435393,-47.8094814947701,
124.180149064765)) ;
#108879 = CARTESIAN_POINT('Ctrl Pts',(-18.2635967217222,-47.8193759435254,
124.39168267558)) ;
#108880 = CARTESIAN_POINT('Ctrl Pts',(-18.4524654950994,-47.8294390629599,
124.576715764561)) ;
#108881 = CARTESIAN_POINT('Ctrl Pts',(-18.6656604141753,-47.8392787082011,
124.723110773571)) ;
#108882 = CARTESIAN_POINT('Ctrl Pts',(-18.9061698010973,-47.8493418723872,
124.832971195248)) ;
#108883 = CARTESIAN_POINT('Ctrl Pts',(-19.1579245355548,-47.859236142136,
124.898091649154)) ;
#108884 = CARTESIAN_POINT('Ctrl Pts',(-19.418285236118,-47.8691778681498,
124.919307392181)) ;
#108885 = CARTESIAN_POINT('Ctrl Pts',(-19.6800605824406,-47.8791807568092,
124.894950207823)) ;
#108886 = CARTESIAN_POINT('Ctrl Pts',(-19.9343759736803,-47.8892206056032,
124.824805409366)) ;
#108887 = CARTESIAN_POINT('Ctrl Pts',(-20.1678242012441,-47.8990448210641,
124.714511643013)) ;
#108888 = CARTESIAN_POINT('Ctrl Pts',(-20.3837446801702,-47.9091016645576,
124.562152333181)) ;
#108889 = CARTESIAN_POINT('Ctrl Pts',(-20.5673352422377,-47.9190302739536,
124.376743540514)) ;
#108890 = CARTESIAN_POINT('Ctrl Pts',(-20.7168951714096,-47.9289821579915,
124.162191214488)) ;
#108891 = CARTESIAN_POINT('Ctrl Pts',(-20.82760319258,-47.9390351107991,123.92234566536)) ;
#108892 = CARTESIAN_POINT('Ctrl Pts',(-20.8939170780824,-47.9488579872653,
123.672853622298)) ;
#108893 = CARTESIAN_POINT('Ctrl Pts',(-20.9168841773058,-47.9589137198354,
123.409617614338)) ;
#108894 = CARTESIAN_POINT('Ctrl Pts',(-20.8935971778619,-47.9688544848231,
123.149415027689)) ;
#108895 = CARTESIAN_POINT('Ctrl Pts',(-20.8265214718633,-47.9787588177287,
122.897925847122)) ;
#108896 = CARTESIAN_POINT('Ctrl Pts',(-20.7150807429793,-47.9888054866094,
122.658606916278)) ;
#108897 = CARTESIAN_POINT('Ctrl Pts',(-20.5662122954325,-47.9987010499152,
122.445338160024)) ;
#108898 = CARTESIAN_POINT('Ctrl Pts',(-20.3795420640069,-48.0087631076155,
122.258115625074)) ;
#108899 = CARTESIAN_POINT('Ctrl Pts',(-20.1679441914161,-48.018605885243,
122.109301615718)) ;
#108900 = CARTESIAN_POINT('Ctrl Pts',(-19.9305295366812,-48.0285963634949,
121.997305134393)) ;
#108901 = CARTESIAN_POINT('Ctrl Pts',(-19.6787754200259,-48.0385253361384,
121.928681255677)) ;
#108902 = CARTESIAN_POINT('Ctrl Pts',(-19.4173556033698,-48.048516473018,
121.904257464178)) ;
#108903 = CARTESIAN_POINT('Ctrl Pts',(-19.154877813197,-48.0585385905069,
121.925978978752)) ;
#108904 = CARTESIAN_POINT('Ctrl Pts',(-18.9031878540514,-48.0684391009091,
121.991894698316)) ;
#108905 = CARTESIAN_POINT('Ctrl Pts',(-18.6644862196403,-48.0784280936552,
122.101106808281)) ;
#108906 = CARTESIAN_POINT('Ctrl Pts',(-18.4489980875861,-48.0883933377058,
122.24989675199)) ;
#108907 = CARTESIAN_POINT('Ctrl Pts',(-18.2633058629821,-48.098297602219,
122.432301210842)) ;
#108908 = CARTESIAN_POINT('Ctrl Pts',(-18.1099186316045,-48.1083556939172,
122.647530199542)) ;
#108909 = CARTESIAN_POINT('Ctrl Pts',(-17.9983934158616,-48.1182056343456,
122.881135521714)) ;
#108910 = CARTESIAN_POINT('Ctrl Pts',(-17.9272566245635,-48.1282326455192,
123.134845982042)) ;
#108911 = CARTESIAN_POINT('Ctrl Pts',(-17.9019314072819,-48.1382612321312,
123.397179595128)) ;
#108912 = CARTESIAN_POINT('Ctrl Pts',(-17.9216733250897,-48.1481064462439,
123.655133881955)) ;
#108913 = CARTESIAN_POINT('Ctrl Pts',(-17.9861782975322,-48.1580971944235,
123.909638987768)) ;
#108914 = CARTESIAN_POINT('Ctrl Pts',(-18.0949265686973,-48.168134828009,
124.149957160556)) ;
#108915 = CARTESIAN_POINT('Ctrl Pts',(-18.2405451274193,-48.1779801172218,
124.363815242263)) ;
#108916 = CARTESIAN_POINT('Ctrl Pts',(-18.4231455792606,-48.1879615180277,
124.552092371215)) ;
#108917 = CARTESIAN_POINT('Ctrl Pts',(-18.6351018542138,-48.1979137510176,
124.705319799365)) ;
#108918 = CARTESIAN_POINT('Ctrl Pts',(-18.8714073387186,-48.2079125624742,
124.820264398588)) ;
#108919 = CARTESIAN_POINT('Ctrl Pts',(-19.1252041777286,-48.2179516664049,
124.892225670979)) ;
#108920 = CARTESIAN_POINT('Ctrl Pts',(-19.3820164657569,-48.2277766088242,
124.919009855094)) ;
#108921 = CARTESIAN_POINT('Ctrl Pts',(-19.645598927116,-48.2378312963002,
124.900805826221)) ;
#108922 = CARTESIAN_POINT('Ctrl Pts',(-19.8990789793834,-48.247774098657,
124.837381251023)) ;
#108923 = CARTESIAN_POINT('Ctrl Pts',(-20.1370819206861,-48.2576778945968,
124.732055560425)) ;
#108924 = CARTESIAN_POINT('Ctrl Pts',(-20.3561905129845,-48.2677246739718,
124.584794460895)) ;
#108925 = CARTESIAN_POINT('Ctrl Pts',(-20.5437409268307,-48.2776203322664,
124.404601015632)) ;
#108926 = CARTESIAN_POINT('Ctrl Pts',(-20.699711817272,-48.287681899517,124.19113144653)) ;
#108927 = CARTESIAN_POINT('Ctrl Pts',(-20.8137891111206,-48.2975265439543,
123.958924282819)) ;
#108928 = CARTESIAN_POINT('Ctrl Pts',(-20.8875575622636,-48.307486590197,
123.707798631624)) ;
#108929 = CARTESIAN_POINT('Ctrl Pts',(-20.9163145705718,-48.3175248862154,
123.445587612575)) ;
#108930 = CARTESIAN_POINT('Ctrl Pts',(-20.8998826835862,-48.3273982276337,
123.186607836747)) ;
#108931 = CARTESIAN_POINT('Ctrl Pts',(-20.8374393368674,-48.337471331433,
122.929420568722)) ;
#108932 = CARTESIAN_POINT('Ctrl Pts',(-20.7342018444484,-48.3472921465519,
122.692831515298)) ;
#108933 = CARTESIAN_POINT('Ctrl Pts',(-20.5880398528313,-48.3573690116299,
122.472072060764)) ;
#108934 = CARTESIAN_POINT('Ctrl Pts',(-20.4094765525404,-48.3672337512852,
122.284097068372)) ;
#108935 = CARTESIAN_POINT('Ctrl Pts',(-20.1980999492212,-48.3772561545265,
122.126990352241)) ;
#108936 = CARTESIAN_POINT('Ctrl Pts',(-19.9622589109079,-48.387281878815,
122.009510754625)) ;
#108937 = CARTESIAN_POINT('Ctrl Pts',(-19.7140688412835,-48.3971366618363,
121.935611134121)) ;
#108938 = CARTESIAN_POINT('Ctrl Pts',(-19.4536367372929,-48.4071155055596,
121.904873002265)) ;
#108939 = CARTESIAN_POINT('Ctrl Pts',(-19.1908180123101,-48.4171343977962,
121.920334070307)) ;
#108940 = CARTESIAN_POINT('Ctrl Pts',(-18.9379752442509,-48.4270176068372,
121.979857228131)) ;
#108941 = CARTESIAN_POINT('Ctrl Pts',(-18.6949553095141,-48.4370859161774,
122.084369573566)) ;
#108942 = CARTESIAN_POINT('Ctrl Pts',(-18.4787661619225,-48.4469160415101,
122.225852664431)) ;
#108943 = CARTESIAN_POINT('Ctrl Pts',(-18.2857271344628,-48.4569825938871,
122.406667621698)) ;
#108944 = CARTESIAN_POINT('Ctrl Pts',(-18.1298795565182,-48.4668728307808,
122.61470398107)) ;
#108945 = CARTESIAN_POINT('Ctrl Pts',(-18.0108214031935,-48.4768650555748,
122.848729665131)) ;
#108946 = CARTESIAN_POINT('Ctrl Pts',(-17.9346625480558,-48.4868276759257,
123.099210441547)) ;
#108947 = CARTESIAN_POINT('Ctrl Pts',(-17.9026921520471,-48.4967326786889,
123.357550683362)) ;
#108948 = CARTESIAN_POINT('Ctrl Pts',(-17.9164495946662,-48.506790441087,
123.621476523787)) ;
#108949 = CARTESIAN_POINT('Ctrl Pts',(-17.9744028993469,-48.5166409604658,
123.873788410068)) ;
#108950 = CARTESIAN_POINT('Ctrl Pts',(-18.0765915286139,-48.526672537464,
124.116777343657)) ;
#108951 = CARTESIAN_POINT('Ctrl Pts',(-18.2195583870351,-48.5366822725689,
124.337613358447)) ;
#108952 = CARTESIAN_POINT('Ctrl Pts',(-18.3967026397366,-48.5465918491952,
124.528462578557)) ;
#108953 = CARTESIAN_POINT('Ctrl Pts',(-18.6042899116757,-48.5565192350519,
124.686490326835)) ;
#108954 = CARTESIAN_POINT('Ctrl Pts',(-18.8389855979222,-48.5665641695422,
124.807288343278)) ;
#108955 = CARTESIAN_POINT('Ctrl Pts',(-19.0870807049156,-48.5764501017301,
124.88441804605)) ;
#108956 = CARTESIAN_POINT('Ctrl Pts',(-19.3475102915803,-48.5864434076831,
124.918100928947)) ;
#108957 = CARTESIAN_POINT('Ctrl Pts',(-19.6085921832354,-48.596389045465,
124.906007103596)) ;
#108958 = CARTESIAN_POINT('Ctrl Pts',(-19.8637789792283,-48.6063363138109,
124.849275357252)) ;
#108959 = CARTESIAN_POINT('Ctrl Pts',(-20.1075477045523,-48.616384215948,
124.74781718916)) ;
#108960 = CARTESIAN_POINT('Ctrl Pts',(-20.3256903200238,-48.6262319107882,
124.60858627602)) ;
#108961 = CARTESIAN_POINT('Ctrl Pts',(-20.5190970658779,-48.6361934205326,
124.432188062646)) ;
#108962 = CARTESIAN_POINT('Ctrl Pts',(-20.679759546878,-48.6462228121415,
124.223243847713)) ;
#108963 = CARTESIAN_POINT('Ctrl Pts',(-20.8003422433532,-48.6561303076962,
123.992489355231)) ;
#108964 = CARTESIAN_POINT('Ctrl Pts',(-20.8798178028071,-48.6660756993592,
123.743533785496)) ;
#108965 = CARTESIAN_POINT('Ctrl Pts',(-20.9152202636129,-48.6760776169566,
123.483053144482)) ;
#108966 = CARTESIAN_POINT('Ctrl Pts',(-20.9043330847647,-48.6861176845088,
123.219459711109)) ;
#108967 = CARTESIAN_POINT('Ctrl Pts',(-20.8496202639193,-48.6959419959486,
122.967128154732)) ;
#108968 = CARTESIAN_POINT('Ctrl Pts',(-20.7499746982012,-48.7059982371047,
122.722395397519)) ;
#108969 = CARTESIAN_POINT('Ctrl Pts',(-20.6108122326477,-48.7159291588403,
122.501585804045)) ;
#108970 = CARTESIAN_POINT('Ctrl Pts',(-20.4356439584125,-48.7258723949166,
122.307742246963)) ;
#108971 = CARTESIAN_POINT('Ctrl Pts',(-20.228787585752,-48.735853678929,122.146399919613)) ;
#108972 = CARTESIAN_POINT('Ctrl Pts',(-19.9954475040825,-48.7458979805547,
122.023085563198)) ;
#108973 = CARTESIAN_POINT('Ctrl Pts',(-19.7497625805735,-48.7557260617741,
121.943308130325)) ;
#108974 = CARTESIAN_POINT('Ctrl Pts',(-19.4876032964969,-48.7658026646233,
121.906379105152)) ;
#108975 = CARTESIAN_POINT('Ctrl Pts',(-19.22879428654,-48.7756547437418,121.915201234916)) ;
#108976 = CARTESIAN_POINT('Ctrl Pts',(-18.9698136227784,-48.7857280020508,
121.969789340118)) ;
#108977 = CARTESIAN_POINT('Ctrl Pts',(-18.7298662537344,-48.7955694614311,
122.066333319079)) ;
#108978 = CARTESIAN_POINT('Ctrl Pts',(-18.5071641353739,-48.8055305568434,
122.20388639306)) ;
#108979 = CARTESIAN_POINT('Ctrl Pts',(-18.3105756785114,-48.8155678412401,
122.379738566765)) ;
#108980 = CARTESIAN_POINT('Ctrl Pts',(-18.1497440179017,-48.8254441799754,
122.583476122298)) ;
#108981 = CARTESIAN_POINT('Ctrl Pts',(-18.0244030217807,-48.8355063061287,
122.8162654372)) ;
#108982 = CARTESIAN_POINT('Ctrl Pts',(-17.942905899043,-48.8453744801052,
123.062485485328)) ;
#108983 = CARTESIAN_POINT('Ctrl Pts',(-17.9043608091258,-48.855380028609,
123.322544901866)) ;
#108984 = CARTESIAN_POINT('Ctrl Pts',(-17.911631882069,-48.8653626605046,
123.584825264922)) ;
#108985 = CARTESIAN_POINT('Ctrl Pts',(-17.96491145671,-48.8754066029264,123.843313454049)) ;
#108986 = CARTESIAN_POINT('Ctrl Pts',(-18.0598585764052,-48.8852347509536,
124.083501852298)) ;
#108987 = CARTESIAN_POINT('Ctrl Pts',(-18.1965745857908,-48.8952246183279,
124.307617145225)) ;
#108988 = CARTESIAN_POINT('Ctrl Pts',(-18.37157698631,-48.9052683572834,124.505196859197)) ;
#108989 = CARTESIAN_POINT('Ctrl Pts',(-18.5733245027204,-48.9150901058214,
124.666180890081)) ;
#108990 = CARTESIAN_POINT('Ctrl Pts',(-18.804570190676,-48.9251250834311,
124.79293891988)) ;
#108991 = CARTESIAN_POINT('Ctrl Pts',(-19.0543037323984,-48.9351499961888,
124.876841632141)) ;
#108992 = CARTESIAN_POINT('Ctrl Pts',(-19.3102311694343,-48.9450019392826,
124.91599016344)) ;
#108993 = CARTESIAN_POINT('Ctrl Pts',(-19.5726920168574,-48.9549929006117,
124.910425982327)) ;
#108994 = CARTESIAN_POINT('Ctrl Pts',(-19.8284128705692,-48.9649107754802,
124.859903942216)) ;
#108995 = CARTESIAN_POINT('Ctrl Pts',(-20.074156743072,-48.9749392944814,
124.764768705151)) ;
#108996 = CARTESIAN_POINT('Ctrl Pts',(-20.2964901168158,-48.9848229732793,
124.630476227167)) ;
#108997 = CARTESIAN_POINT('Ctrl Pts',(-20.4947028792025,-48.994817916719,
124.458139223687)) ;
#108998 = CARTESIAN_POINT('Ctrl Pts',(-20.6601584139195,-49.0048447705414,
124.253066383284)) ;
#108999 = CARTESIAN_POINT('Ctrl Pts',(-20.7859988178692,-49.0147289348803,
124.025827024865)) ;
#109000 = CARTESIAN_POINT('Ctrl Pts',(-20.8716773612727,-49.0247170329227,
123.777755041357)) ;
#109001 = CARTESIAN_POINT('Ctrl Pts',(-20.9129810731439,-49.0346681393798,
123.51949960993)) ;
#109002 = CARTESIAN_POINT('Ctrl Pts',(-20.908629938218,-49.0447131905479,
123.25557749533)) ;
#109003 = CARTESIAN_POINT('Ctrl Pts',(-20.859571512365,-49.0545749509062,
123.001104813214)) ;
#109004 = CARTESIAN_POINT('Ctrl Pts',(-20.7668806910983,-49.0645377677367,
122.756248061331)) ;
#109005 = CARTESIAN_POINT('Ctrl Pts',(-20.6317353832147,-49.0745724490174,
122.529824314885)) ;
#109006 = CARTESIAN_POINT('Ctrl Pts',(-20.4622046891527,-49.0844574787982,
122.332954833504)) ;
#109007 = CARTESIAN_POINT('Ctrl Pts',(-20.2574156100896,-49.0945230721962,
122.165604849423)) ;
#109008 = CARTESIAN_POINT('Ctrl Pts',(-20.0319252978085,-49.1043622405577,
122.038994712386)) ;
#109009 = CARTESIAN_POINT('Ctrl Pts',(-19.7825239386548,-49.1144248382992,
121.951198971752)) ;
#109010 = CARTESIAN_POINT('Ctrl Pts',(-19.5258681356092,-49.1243218507061,
121.909018990511)) ;
#109011 = CARTESIAN_POINT('Ctrl Pts',(-19.2648981101993,-49.1342531725317,
121.911184944876)) ;
#109012 = CARTESIAN_POINT('Ctrl Pts',(-19.0054644614894,-49.1442949352862,
121.959440242708)) ;
#109013 = CARTESIAN_POINT('Ctrl Pts',(-18.7620464793974,-49.1541831341769,
122.050426042176)) ;
#109014 = CARTESIAN_POINT('Ctrl Pts',(-18.5355498526046,-49.1641770727768,
122.183327970392)) ;
#109015 = CARTESIAN_POINT('Ctrl Pts',(-18.3366151190307,-49.1741178938136,
122.352671265509)) ;
#109016 = CARTESIAN_POINT('Ctrl Pts',(-18.1695582708548,-49.1840772761019,
122.554123401537)) ;
#109017 = CARTESIAN_POINT('Ctrl Pts',(-18.0393609910467,-49.1940750357542,
122.78235492102)) ;
#109018 = CARTESIAN_POINT('Ctrl Pts',(-17.9507830524061,-49.2041111719565,
123.030767337162)) ;
#109019 = CARTESIAN_POINT('Ctrl Pts',(-17.9071961511575,-49.2139619694474,
123.285938131175)) ;
#109020 = CARTESIAN_POINT('Ctrl Pts',(-17.9078135555546,-49.2239228345237,
123.547689302551)) ;
#109021 = CARTESIAN_POINT('Ctrl Pts',(-17.9545028435727,-49.2339517021541,
123.807083872471)) ;
#109022 = CARTESIAN_POINT('Ctrl Pts',(-18.0443614900807,-49.2438619382905,
124.051509569397)) ;
#109023 = CARTESIAN_POINT('Ctrl Pts',(-18.1750394781189,-49.253796891605,
124.277540500382)) ;
#109024 = CARTESIAN_POINT('Ctrl Pts',(-18.3449458767919,-49.2638378220146,
124.479414892215)) ;
#109025 = CARTESIAN_POINT('Ctrl Pts',(-18.5441450587453,-49.2737257187962,
124.646279157345)) ;
#109026 = CARTESIAN_POINT('Ctrl Pts',(-18.7713454870044,-49.2837151704549,
124.777768598755)) ;
#109027 = CARTESIAN_POINT('Ctrl Pts',(-19.0172462602511,-49.2936742608203,
124.867340329081)) ;
#109028 = CARTESIAN_POINT('Ctrl Pts',(-19.2732737968385,-49.3035715731266,
124.913231451981)) ;
#109029 = CARTESIAN_POINT('Ctrl Pts',(-19.5375236712753,-49.3136279990268,
124.913856788478)) ;
#109030 = CARTESIAN_POINT('Ctrl Pts',(-19.7931094413585,-49.3234980016166,
124.869551884532)) ;
#109031 = CARTESIAN_POINT('Ctrl Pts',(-20.0405595157066,-49.3335019347938,
124.780858628891)) ;
#109032 = CARTESIAN_POINT('Ctrl Pts',(-20.268461346366,-49.3434891952577,
124.650609341134)) ;
#109033 = CARTESIAN_POINT('Ctrl Pts',(-20.470944358427,-49.3535162468434,
124.482019340126)) ;
#109034 = CARTESIAN_POINT('Ctrl Pts',(-20.6389945572842,-49.3634073366695,
124.283693917084)) ;
#109035 = CARTESIAN_POINT('Ctrl Pts',(-20.8155279114935,-49.3767050914506,
123.982169929469)) ;
#109036 = CARTESIAN_POINT('Ctrl Pts',(-20.9091683649831,-49.3899031510587,
123.644067313166)) ;
#109037 = CARTESIAN_POINT('Ctrl Pts',(-20.9119671066389,-49.4032998916279,
123.292047468722)) ;
#109038 = CARTESIAN_POINT('Ctrl Pts',(-20.86922905483,-49.4131708037013,123.036144564407)) ;
#109039 = CARTESIAN_POINT('Ctrl Pts',(-20.7809586057459,-49.4232443654695,
122.786633988022)) ;
#109040 = CARTESIAN_POINT('Ctrl Pts',(-20.65417958686,-49.4330657780578,122.561751573419)) ;
#109041 = CARTESIAN_POINT('Ctrl Pts',(-20.4863376664184,-49.4431397952888,
122.357107851664)) ;
#109042 = CARTESIAN_POINT('Ctrl Pts',(-20.2240643845596,-49.4562985822534,
122.131632384811)) ;
#109043 = CARTESIAN_POINT('Ctrl Pts',(-19.904402249654,-49.4696646853476,
121.976914104498)) ;
#109044 = CARTESIAN_POINT('Ctrl Pts',(-19.5604858538446,-49.4829786202367,
121.912034841933)) ;
#109045 = CARTESIAN_POINT('Ctrl Pts',(-19.3003871649201,-49.4928786596841,
121.908349652686)) ;
#109046 = CARTESIAN_POINT('Ctrl Pts',(-19.0418061619267,-49.5028430628186,
121.949723315538)) ;
#109047 = CARTESIAN_POINT('Ctrl Pts',(-18.7927980800568,-49.5128730299398,
122.036150682678)) ;
#109048 = CARTESIAN_POINT('Ctrl Pts',(-18.565468855254,-49.5227753065488,
122.162762109831)) ;
#109049 = CARTESIAN_POINT('Ctrl Pts',(-18.2943922464803,-49.536041235718,
122.382027616931)) ;
#109050 = CARTESIAN_POINT('Ctrl Pts',(-18.0346360175635,-49.5526627668244,
122.739267143311)) ;
#109051 = CARTESIAN_POINT('Ctrl Pts',(-17.8877054079863,-49.5725375954691,
123.246737253887)) ;
#109052 = CARTESIAN_POINT('Ctrl Pts',(-17.9170062305799,-49.5892108035709,
123.688865187622)) ;
#109053 = CARTESIAN_POINT('Ctrl Pts',(-18.0293993130542,-49.6024619285522,
124.018479147189)) ;
#109054 = CARTESIAN_POINT('Ctrl Pts',(-18.1961111258911,-49.615704247373,
124.32401157025)) ;
#109055 = CARTESIAN_POINT('Ctrl Pts',(-18.5033429645354,-49.6324374877125,
124.645464754067)) ;
#109056 = CARTESIAN_POINT('Ctrl Pts',(-18.975740249179,-49.6522666359005,
124.879352518781)) ;
#109057 = CARTESIAN_POINT('Ctrl Pts',(-19.5017593847413,-49.6721913310011,
124.939533147707)) ;
#109058 = CARTESIAN_POINT('Ctrl Pts',(-20.0168814997899,-49.6921145595845,
124.816509691594)) ;
#109059 = CARTESIAN_POINT('Ctrl Pts',(-20.4591559559091,-49.7120416987106,
124.52524484642)) ;
#109060 = CARTESIAN_POINT('Ctrl Pts',(-20.7752892855415,-49.7319181613263,
124.101950919271)) ;
#109061 = CARTESIAN_POINT('Ctrl Pts',(-20.9290303017219,-49.7518953899316,
123.593740830601)) ;
#109062 = CARTESIAN_POINT('Ctrl Pts',(-20.8997552792579,-49.7718302479053,
123.064668541065)) ;
#109063 = CARTESIAN_POINT('Ctrl Pts',(-20.6926247770607,-49.7917266968361,
122.578151319081)) ;
#109064 = CARTESIAN_POINT('Ctrl Pts',(-20.3318449657526,-49.8116479809027,
122.190587914378)) ;
#109065 = CARTESIAN_POINT('Ctrl Pts',(-19.8595490175129,-49.8316046305737,
121.949122369929)) ;
#109066 = CARTESIAN_POINT('Ctrl Pts',(-19.3354133917941,-49.8514819236853,
121.883428245473)) ;
#109067 = CARTESIAN_POINT('Ctrl Pts',(-18.8196514980791,-49.8713683959137,
121.999250184421)) ;
#109068 = CARTESIAN_POINT('Ctrl Pts',(-18.3709182764398,-49.8914299618377,
122.287287346707)) ;
#109069 = CARTESIAN_POINT('Ctrl Pts',(-18.0514065132604,-49.9112703693785,
122.706761226316)) ;
#109070 = CARTESIAN_POINT('Ctrl Pts',(-17.8920110217991,-49.9311216933514,
123.209742540466)) ;
#109071 = CARTESIAN_POINT('Ctrl Pts',(-17.9148505895717,-49.9511749633028,
123.742166975697)) ;
#109072 = CARTESIAN_POINT('Ctrl Pts',(-18.1156270801346,-49.9709956206862,
124.229362048374)) ;
#109073 = CARTESIAN_POINT('Ctrl Pts',(-18.4724553006617,-49.9909670420167,
124.622102771765)) ;
#109074 = CARTESIAN_POINT('Ctrl Pts',(-18.9403141167353,-50.0108605343804,
124.868821111013)) ;
#109075 = CARTESIAN_POINT('Ctrl Pts',(-19.4674698621008,-50.0308846206214,
124.941152365213)) ;
#109076 = CARTESIAN_POINT('Ctrl Pts',(-19.9821925019439,-50.0506894997343,
124.830721241803)) ;
#109077 = CARTESIAN_POINT('Ctrl Pts',(-20.4325069663933,-50.0706485154322,
124.550354233972)) ;
#109078 = CARTESIAN_POINT('Ctrl Pts',(-20.7595911996121,-50.0906345390612,
124.131812199693)) ;
#109079 = CARTESIAN_POINT('Ctrl Pts',(-20.9237526047702,-50.1104430348217,
123.631533408587)) ;
#109080 = CARTESIAN_POINT('Ctrl Pts',(-20.9078620156029,-50.1304256739273,
123.10077833293)) ;
#109081 = CARTESIAN_POINT('Ctrl Pts',(-20.7125831300337,-50.1503071217213,
122.609626261788)) ;
#109082 = CARTESIAN_POINT('Ctrl Pts',(-20.3605756213218,-50.1702635884589,
122.213009119955)) ;
#109083 = CARTESIAN_POINT('Ctrl Pts',(-19.8961971448971,-50.1901409854144,
121.960910506346)) ;
#109084 = CARTESIAN_POINT('Ctrl Pts',(-19.371100043134,-50.2101229315897,
121.881727304474)) ;
#109085 = CARTESIAN_POINT('Ctrl Pts',(-18.8517714383784,-50.2300520306265,
121.986501624577)) ;
#109086 = CARTESIAN_POINT('Ctrl Pts',(-18.3995164456027,-50.2499806538391,
122.262017321329)) ;
#109087 = CARTESIAN_POINT('Ctrl Pts',(-18.069133225432,-50.2698149779455,
122.672869051133)) ;
#109088 = CARTESIAN_POINT('Ctrl Pts',(-17.9257188048663,-50.2864672653289,
123.091488247469)) ;
#109089 = CARTESIAN_POINT('Ctrl Pts',(-17.9020768429416,-50.2997277663511,
123.439219687815)) ;
#109090 = CARTESIAN_POINT('Ctrl Pts',(-17.9295576940747,-50.3097292435524,
123.700602593401)) ;
#109091 = CARTESIAN_POINT('Ctrl Pts',(-18.002656042515,-50.3197612644119,
123.953904108933)) ;
#109092 = CARTESIAN_POINT('Ctrl Pts',(-18.116386829973,-50.3296248081375,
124.186815776923)) ;
#109093 = CARTESIAN_POINT('Ctrl Pts',(-18.2699017108944,-50.3395935218076,
124.399094862358)) ;
#109094 = CARTESIAN_POINT('Ctrl Pts',(-18.5219731604255,-50.3529392692113,
124.642904643336)) ;
#109095 = CARTESIAN_POINT('Ctrl Pts',(-18.8271317055665,-50.366089824284,
124.813386630416)) ;
#109096 = CARTESIAN_POINT('Ctrl Pts',(-19.1680474112168,-50.3794752048338,
124.899924395506)) ;
#109097 = CARTESIAN_POINT('Ctrl Pts',(-19.4272102985137,-50.3893631408267,
124.919149230218)) ;
#109098 = CARTESIAN_POINT('Ctrl Pts',(-19.6884530721006,-50.3993543306393,
124.893257415268)) ;
#109099 = CARTESIAN_POINT('Ctrl Pts',(-19.9403450283617,-50.4093064291776,
124.822764313045)) ;
#109100 = CARTESIAN_POINT('Ctrl Pts',(-20.1782748640547,-50.4193526856281,
124.708404581415)) ;
#109101 = CARTESIAN_POINT('Ctrl Pts',(-20.3886616952028,-50.4292021330222,
124.55762525938)) ;
#109102 = CARTESIAN_POINT('Ctrl Pts',(-20.5723317337679,-50.4391647855174,
124.371065949195)) ;
#109103 = CARTESIAN_POINT('Ctrl Pts',(-20.7214333851646,-50.4491878711595,
124.153934546895)) ;
#109104 = CARTESIAN_POINT('Ctrl Pts',(-20.8297858694376,-50.4591129869164,
123.916652445147)) ;
#109105 = CARTESIAN_POINT('Ctrl Pts',(-20.8960168696597,-50.4691654653163,
123.660946913908)) ;
#109106 = CARTESIAN_POINT('Ctrl Pts',(-20.9166037059943,-50.479016964019,
123.402860359197)) ;
#109107 = CARTESIAN_POINT('Ctrl Pts',(-20.8924513733458,-50.4889887032215,
123.141962294283)) ;
#109108 = CARTESIAN_POINT('Ctrl Pts',(-20.8231514064948,-50.4989839109872,
122.888561525086)) ;
#109109 = CARTESIAN_POINT('Ctrl Pts',(-20.7102071657759,-50.5090179124563,
122.650317770348)) ;
#109110 = CARTESIAN_POINT('Ctrl Pts',(-20.5606367267542,-50.5188732705486,
122.43885338085)) ;
#109111 = CARTESIAN_POINT('Ctrl Pts',(-20.3742312146974,-50.5288727461419,
122.253706506383)) ;
#109112 = CARTESIAN_POINT('Ctrl Pts',(-20.160865960504,-50.538767194637,122.10501554527)) ;
#109113 = CARTESIAN_POINT('Ctrl Pts',(-19.9209557482341,-50.5488303188647,
121.993876783106)) ;
#109114 = CARTESIAN_POINT('Ctrl Pts',(-19.6710568689781,-50.5586699451933,
121.927289939446)) ;
#109115 = CARTESIAN_POINT('Ctrl Pts',(-19.4076455171057,-50.5687331802363,
121.904273103064)) ;
#109116 = CARTESIAN_POINT('Ctrl Pts',(-19.1486245172378,-50.5786271854703,
121.927179702334)) ;
#109117 = CARTESIAN_POINT('Ctrl Pts',(-18.8961488717579,-50.5885698986861,
121.994338288272)) ;
#109118 = CARTESIAN_POINT('Ctrl Pts',(-18.6575937125495,-50.5985756384843,
122.10498927942)) ;
#109119 = CARTESIAN_POINT('Ctrl Pts',(-18.4417453764348,-50.6085965406307,
122.255832615603)) ;
#109120 = CARTESIAN_POINT('Ctrl Pts',(-18.2575664390002,-50.6184873106796,
122.439245530965)) ;
#109121 = CARTESIAN_POINT('Ctrl Pts',(-18.106199313767,-50.6284787214593,
122.653775573156)) ;
#109122 = CARTESIAN_POINT('Ctrl Pts',(-17.994939377062,-50.6384270671238,
122.890345311721)) ;
#109123 = CARTESIAN_POINT('Ctrl Pts',(-17.9259303257963,-50.648371925185,
123.142434021388)) ;
#109124 = CARTESIAN_POINT('Ctrl Pts',(-17.9018642723726,-50.6584267605779,
123.40554120748)) ;
#109125 = CARTESIAN_POINT('Ctrl Pts',(-17.9228963383738,-50.6682491326794,
123.662827558674)) ;
#109126 = CARTESIAN_POINT('Ctrl Pts',(-17.9893655669342,-50.6783050001231,
123.918569075764)) ;
#109127 = CARTESIAN_POINT('Ctrl Pts',(-18.0984078853654,-50.688245729981,
124.155965789907)) ;
#109128 = CARTESIAN_POINT('Ctrl Pts',(-18.2457954157067,-50.6981500685321,
124.370495273016)) ;
#109129 = CARTESIAN_POINT('Ctrl Pts',(-18.4309155957162,-50.7081967499607,
124.558705815909)) ;
#109130 = CARTESIAN_POINT('Ctrl Pts',(-18.6425827603139,-50.7180922574299,
124.709841133587)) ;
#109131 = CARTESIAN_POINT('Ctrl Pts',(-18.8811592255437,-50.7281545259285,
124.823777836074)) ;
#109132 = CARTESIAN_POINT('Ctrl Pts',(-19.1303439298088,-50.7379965161991,
124.893182940593)) ;
#109133 = CARTESIAN_POINT('Ctrl Pts',(-19.3916248824372,-50.7479899330801,
124.919232757977)) ;
#109134 = CARTESIAN_POINT('Ctrl Pts',(-19.6517236646734,-50.7579144209322,
124.899673740811)) ;
#109135 = CARTESIAN_POINT('Ctrl Pts',(-19.9064096763508,-50.7679140548407,
124.835042611516)) ;
#109136 = CARTESIAN_POINT('Ctrl Pts',(-20.1457402038609,-50.7779001650975,
124.727300269212)) ;
#109137 = CARTESIAN_POINT('Ctrl Pts',(-20.3636013964809,-50.7879361162846,
124.578709908681)) ;
#109138 = CARTESIAN_POINT('Ctrl Pts',(-20.5492892152705,-50.7977927546194,
124.398083228579)) ;
#109139 = CARTESIAN_POINT('Ctrl Pts',(-20.7032288955082,-50.8077917146974,
124.18519187754)) ;
#109140 = CARTESIAN_POINT('Ctrl Pts',(-20.8169684935158,-50.8176869450112,
123.95130100847)) ;
#109141 = CARTESIAN_POINT('Ctrl Pts',(-20.8895126689177,-50.8277474574798,
123.697104486411)) ;
#109142 = CARTESIAN_POINT('Ctrl Pts',(-20.9163960233827,-50.837596749026,
123.439654669857)) ;
#109143 = CARTESIAN_POINT('Ctrl Pts',(-20.8985077215947,-50.8476239349582,
123.176765287496)) ;
#109144 = CARTESIAN_POINT('Ctrl Pts',(-20.8345597388551,-50.8576524714175,
122.921088430059)) ;
#109145 = CARTESIAN_POINT('Ctrl Pts',(-20.7296110651712,-50.8674977113825,
122.684622614722)) ;
#109146 = CARTESIAN_POINT('Ctrl Pts',(-20.5836373894201,-50.8774884063057,
122.466391230492)) ;
#109147 = CARTESIAN_POINT('Ctrl Pts',(-20.4007156047811,-50.8875262270643,
122.276336681186)) ;
#109148 = CARTESIAN_POINT('Ctrl Pts',(-20.1919297062301,-50.8973708208412,
122.123562264612)) ;
#109149 = CARTESIAN_POINT('Ctrl Pts',(-19.9567750355557,-50.9073548162173,
122.007254388353)) ;
#109150 = CARTESIAN_POINT('Ctrl Pts',(-19.7058360968949,-50.9173038647787,
121.933818914546)) ;
#109151 = CARTESIAN_POINT('Ctrl Pts',(-19.4445977592879,-50.9273063037532,
121.904634485153)) ;
#109152 = CARTESIAN_POINT('Ctrl Pts',(-19.1817978691591,-50.9373275450496,
121.921640529881)) ;
#109153 = CARTESIAN_POINT('Ctrl Pts',(-18.9291516129592,-50.9472202234891,
121.982914385195)) ;
#109154 = CARTESIAN_POINT('Ctrl Pts',(-18.6884726742296,-50.9572102774367,
122.087763857683)) ;
#109155 = CARTESIAN_POINT('Ctrl Pts',(-18.4704576208751,-50.9671686385852,
122.232502141319)) ;
#109156 = CARTESIAN_POINT('Ctrl Pts',(-18.2815439794151,-50.97706826547,122.411385729391)) ;
#109157 = CARTESIAN_POINT('Ctrl Pts',(-18.1243401709287,-50.9871161622734,
122.623503415483)) ;
#109158 = CARTESIAN_POINT('Ctrl Pts',(-18.0079328095563,-50.9970115199094,
122.856078803486)) ;
#109159 = CARTESIAN_POINT('Ctrl Pts',(-17.9324125309766,-51.0070731723661,
123.109443165395)) ;
#109160 = CARTESIAN_POINT('Ctrl Pts',(-17.9026431920304,-51.016917776638,
123.366440022436)) ;
#109161 = CARTESIAN_POINT('Ctrl Pts',(-17.9171914556696,-51.026877898336,
123.627772544712)) ;
#109162 = CARTESIAN_POINT('Ctrl Pts',(-17.9778575855944,-51.0369159326985,
123.884480568244)) ;
#109163 = CARTESIAN_POINT('Ctrl Pts',(-18.0800533841894,-51.046790245285,
124.123030915168)) ;
#109164 = CARTESIAN_POINT('Ctrl Pts',(-18.2248973712066,-51.0568597260677,
124.344440963174)) ;
#109165 = CARTESIAN_POINT('Ctrl Pts',(-18.4016942575522,-51.0666940620848,
124.532971381553)) ;
#109166 = CARTESIAN_POINT('Ctrl Pts',(-18.6122597307479,-51.076727019813,
124.691628705257)) ;
#109167 = CARTESIAN_POINT('Ctrl Pts',(-18.8472201491043,-51.0867474183882,
124.810522126315)) ;
#109168 = CARTESIAN_POINT('Ctrl Pts',(-19.095186956978,-51.0966129921594,
124.886265732947)) ;
#109169 = CARTESIAN_POINT('Ctrl Pts',(-19.357793794437,-51.1066818668155,
124.918452072339)) ;
#109170 = CARTESIAN_POINT('Ctrl Pts',(-19.6161806221117,-51.116527297721,
124.904898127975)) ;
#109171 = CARTESIAN_POINT('Ctrl Pts',(-19.871892695951,-51.1265069225917,
124.846720906365)) ;
#109172 = CARTESIAN_POINT('Ctrl Pts',(-20.1143711448199,-51.1365256055058,
124.744169162022)) ;
#109173 = CARTESIAN_POINT('Ctrl Pts',(-20.3327050133308,-51.1464088706896,
124.603447512875)) ;
#109174 = CARTESIAN_POINT('Ctrl Pts',(-20.5267220753818,-51.156477164781,
124.423616988893)) ;
#109175 = CARTESIAN_POINT('Ctrl Pts',(-20.6830811763147,-51.1663072949663,
124.217930329721)) ;
#109176 = CARTESIAN_POINT('Ctrl Pts',(-20.8044599409609,-51.1763738431815,
123.982929680634)) ;
#109177 = CARTESIAN_POINT('Ctrl Pts',(-20.881680652614,-51.1862640918701,
123.734726833842)) ;
#109178 = CARTESIAN_POINT('Ctrl Pts',(-20.9155355018185,-51.1962562736461,
123.474349688364)) ;
#109179 = CARTESIAN_POINT('Ctrl Pts',(-20.9034548595314,-51.2062190542739,
123.212821923773)) ;
#109180 = CARTESIAN_POINT('Ctrl Pts',(-20.8471147183909,-51.2161234589477,
122.958696270811)) ;
#109181 = CARTESIAN_POINT('Ctrl Pts',(-20.7457750358566,-51.2261834534267,
122.714550697447)) ;
#109182 = CARTESIAN_POINT('Ctrl Pts',(-20.6067346798878,-51.2360320753965,
122.496235768435)) ;
#109183 = CARTESIAN_POINT('Ctrl Pts',(-20.4291331957846,-51.2460625148083,
122.301482009075)) ;
#109184 = CARTESIAN_POINT('Ctrl Pts',(-20.2204863343757,-51.2560722304431,
122.14124999381)) ;
#109185 = CARTESIAN_POINT('Ctrl Pts',(-19.9896575967978,-51.2659829831357,
122.020681381118)) ;
#109186 = CARTESIAN_POINT('Ctrl Pts',(-19.7411001533727,-51.2759122560821,
121.941241152723)) ;
#109187 = CARTESIAN_POINT('Ctrl Pts',(-19.4795647357375,-51.2859549474748,
121.905989503812)) ;
#109188 = CARTESIAN_POINT('Ctrl Pts',(-19.2199484999009,-51.2958414806923,
121.916349708964)) ;
#109189 = CARTESIAN_POINT('Ctrl Pts',(-18.9632715215848,-51.3058346256243,
121.971785234731)) ;
#109190 = CARTESIAN_POINT('Ctrl Pts',(-18.7212976545593,-51.3157803064608,
122.070573488031)) ;
#109191 = CARTESIAN_POINT('Ctrl Pts',(-18.49982192186,-51.3257275636094,122.209451826745)) ;
#109192 = CARTESIAN_POINT('Ctrl Pts',(-18.3040765935433,-51.3357754674813,
122.386654309068)) ;
#109193 = CARTESIAN_POINT('Ctrl Pts',(-18.1451228804641,-51.3456231665793,
122.590872919258)) ;
#109194 = CARTESIAN_POINT('Ctrl Pts',(-18.0219193554534,-51.355584657558,
122.821834110184)) ;
#109195 = CARTESIAN_POINT('Ctrl Pts',(-17.9404646597919,-51.3656141199719,
123.072506175138)) ;
#109196 = CARTESIAN_POINT('Ctrl Pts',(-17.9040809682296,-51.3755213510718,
123.330303605166)) ;
#109197 = CARTESIAN_POINT('Ctrl Pts',(-17.9125155161275,-51.3854677297493,
123.591532484831)) ;
#109198 = CARTESIAN_POINT('Ctrl Pts',(-17.9664112488074,-51.3954724985581,
123.848886998314)) ;
#109199 = CARTESIAN_POINT('Ctrl Pts',(-18.0646024092112,-51.4054936195783,
124.093235374132)) ;
#109200 = CARTESIAN_POINT('Ctrl Pts',(-18.2016748070809,-51.4153844854309,
124.314086593535)) ;
#109201 = CARTESIAN_POINT('Ctrl Pts',(-18.3764583415646,-51.4253752941902,
124.509980152437)) ;
#109202 = CARTESIAN_POINT('Ctrl Pts',(-18.5818247469521,-51.4353259523705,
124.671874876727)) ;
#109203 = CARTESIAN_POINT('Ctrl Pts',(-18.8116522149616,-51.4452621620126,
124.795765081185)) ;
#109204 = CARTESIAN_POINT('Ctrl Pts',(-19.0606147398016,-51.4552453287375,
124.87859535558)) ;
#109205 = CARTESIAN_POINT('Ctrl Pts',(-19.3217627463815,-51.4652891259478,
124.916679949028)) ;
#109206 = CARTESIAN_POINT('Ctrl Pts',(-19.5799813331497,-51.4751173421161,
124.909619362426)) ;
#109207 = CARTESIAN_POINT('Ctrl Pts',(-19.8393782432694,-51.4851939095853,
124.856664288692)) ;
#109208 = CARTESIAN_POINT('Ctrl Pts',(-20.0803045545237,-51.4950459952747,
124.761719728551)) ;
#109209 = CARTESIAN_POINT('Ctrl Pts',(-20.306073135477,-51.5051192626801,
124.623591191497)) ;
#109210 = CARTESIAN_POINT('Ctrl Pts',(-20.4998622506351,-51.5149606791037,
124.452299627734)) ;
#109211 = CARTESIAN_POINT('Ctrl Pts',(-20.6636747138412,-51.5249219372464,
124.24813177878)) ;
#109212 = CARTESIAN_POINT('Ctrl Pts',(-20.7900568456154,-51.5349586136784,
124.016635338935)) ;
#109213 = CARTESIAN_POINT('Ctrl Pts',(-20.8734225094882,-51.5448372215422,
123.770756105118)) ;
#109214 = CARTESIAN_POINT('Ctrl Pts',(-20.9136026213356,-51.554897450181,
123.509489974879)) ;
#109215 = CARTESIAN_POINT('Ctrl Pts',(-20.9079937843595,-51.5647644343418,
123.250223069463)) ;
#109216 = CARTESIAN_POINT('Ctrl Pts',(-20.8572543274689,-51.5747700005945,
122.992264994515)) ;
#109217 = CARTESIAN_POINT('Ctrl Pts',(-20.7626104316149,-51.5847537890091,
122.747517362774)) ;
#109218 = CARTESIAN_POINT('Ctrl Pts',(-20.6258531267802,-51.5947996458117,
122.521731422933)) ;
#109219 = CARTESIAN_POINT('Ctrl Pts',(-20.4560156427673,-51.6046255230277,
122.327231639573)) ;
#109220 = CARTESIAN_POINT('Ctrl Pts',(-20.2521594332448,-51.614615998869,
122.161794290385)) ;
#109221 = CARTESIAN_POINT('Ctrl Pts',(-20.0211183356917,-51.6246595747678,
122.034194822812)) ;
#109222 = CARTESIAN_POINT('Ctrl Pts',(-19.7771218627311,-51.6344813670658,
121.950027748403)) ;
#109223 = CARTESIAN_POINT('Ctrl Pts',(-19.5167861488625,-51.6445163326917,
121.907987506781)) ;
#109224 = CARTESIAN_POINT('Ctrl Pts',(-19.2533739592759,-51.6545412496248,
121.912518592309)) ;
#109225 = CARTESIAN_POINT('Ctrl Pts',(-18.9991057307771,-51.6643931880009,
121.961295351794)) ;
#109226 = CARTESIAN_POINT('Ctrl Pts',(-18.7536483063783,-51.6743841640256,
122.054393070436)) ;
#109227 = CARTESIAN_POINT('Ctrl Pts',(-18.5295887727591,-51.6843019848293,
122.187596659951)) ;
#109228 = CARTESIAN_POINT('Ctrl Pts',(-18.3298720780152,-51.6943307053939,
122.35950935101)) ;
#109229 = CARTESIAN_POINT('Ctrl Pts',(-18.1652929595481,-51.7042136320031,
122.560450226182)) ;
#109230 = CARTESIAN_POINT('Ctrl Pts',(-18.0362039840031,-51.7142179171226,
122.78944338197)) ;
#109231 = CARTESIAN_POINT('Ctrl Pts',(-17.9490199350489,-51.7242015983304,
123.03694165535)) ;
#109232 = CARTESIAN_POINT('Ctrl Pts',(-17.9061972167895,-51.7342425970603,
123.297290625367)) ;
#109233 = CARTESIAN_POINT('Ctrl Pts',(-17.908803361231,-51.7440750419275,
123.555667262023)) ;
#109234 = CARTESIAN_POINT('Ctrl Pts',(-17.9562536617095,-51.7540700403578,
123.813996341053)) ;
#109235 = CARTESIAN_POINT('Ctrl Pts',(-18.0487087052507,-51.7641015891074,
124.060885187494)) ;
#109236 = CARTESIAN_POINT('Ctrl Pts',(-18.1801140761451,-51.7739669674129,
124.284351123223)) ;
#109237 = CARTESIAN_POINT('Ctrl Pts',(-18.3494200817977,-51.7839288148732,
124.484031080375)) ;
#109238 = CARTESIAN_POINT('Ctrl Pts',(-18.5525603287765,-51.7939637556874,
124.65216255298)) ;
#109239 = CARTESIAN_POINT('Ctrl Pts',(-18.7782099405819,-51.8038487167046,
124.780926155321)) ;
#109240 = CARTESIAN_POINT('Ctrl Pts',(-19.0272027318683,-51.8139143256234,
124.870073403993)) ;
#109241 = CARTESIAN_POINT('Ctrl Pts',(-19.2820659565915,-51.8237535006651,
124.913900713737)) ;
#109242 = CARTESIAN_POINT('Ctrl Pts',(-19.5464673888862,-51.833816056165,
124.913150026589)) ;
#109243 = CARTESIAN_POINT('Ctrl Pts',(-19.8024397374806,-51.843713230858,
124.866983100272)) ;
#109244 = CARTESIAN_POINT('Ctrl Pts',(-20.0476185001334,-51.8536439457813,
124.777597590516)) ;
#109245 = CARTESIAN_POINT('Ctrl Pts',(-20.2759776925336,-51.8636879738589,
124.645246173051)) ;
#109246 = CARTESIAN_POINT('Ctrl Pts',(-20.4748636938545,-51.8735741757122,
124.47806599248)) ;
#109247 = CARTESIAN_POINT('Ctrl Pts',(-20.6437806069074,-51.8835673421791,
124.277027652235)) ;
#109248 = CARTESIAN_POINT('Ctrl Pts',(-20.7746158733982,-51.8935068131662,
124.050921132866)) ;
#109249 = CARTESIAN_POINT('Ctrl Pts',(-20.864926632437,-51.9035233275204,
123.803704134483)) ;
#109250 = CARTESIAN_POINT('Ctrl Pts',(-20.9107718686361,-51.9134533539972,
123.546775177275)) ;
#109251 = CARTESIAN_POINT('Ctrl Pts',(-20.9111996492547,-51.9235058895067,
123.282627938416)) ;
#109252 = CARTESIAN_POINT('Ctrl Pts',(-20.8668285985531,-51.9333522927264,
123.027698354872)) ;
#109253 = CARTESIAN_POINT('Ctrl Pts',(-20.7786383276928,-51.9433143355804,
122.781223584953)) ;
#109254 = CARTESIAN_POINT('Ctrl Pts',(-20.6478126513841,-51.9533428863711,
122.552428957357)) ;
#109255 = CARTESIAN_POINT('Ctrl Pts',(-20.4813210380991,-51.9632532120887,
122.352179823965)) ;
#109256 = CARTESIAN_POINT('Ctrl Pts',(-20.2825219245844,-51.9731881239183,
122.182930241448)) ;
#109257 = CARTESIAN_POINT('Ctrl Pts',(-20.0548415494281,-51.9832291306864,
122.049575194896)) ;
#109258 = CARTESIAN_POINT('Ctrl Pts',(-19.8112844642767,-51.9931167635186,
121.959011480888)) ;
#109259 = CARTESIAN_POINT('Ctrl Pts',(-19.5531552028146,-52.0031071946166,
121.911171970469)) ;
#109260 = CARTESIAN_POINT('Ctrl Pts',(-19.2915375054555,-52.0130626311739,
121.909027597134)) ;
#109261 = CARTESIAN_POINT('Ctrl Pts',(-19.034617991688,-52.0229735792732,
121.951673016826)) ;
#109262 = CARTESIAN_POINT('Ctrl Pts',(-18.7863603364124,-52.0329856553709,
122.038889445469)) ;
#109263 = CARTESIAN_POINT('Ctrl Pts',(-18.5569711609349,-52.0430129774459,
122.168521876009)) ;
#109264 = CARTESIAN_POINT('Ctrl Pts',(-18.3565229470281,-52.0528717524,122.332741737178)) ;
#109265 = CARTESIAN_POINT('Ctrl Pts',(-18.1268595349139,-52.0662979452124,
122.600459541872)) ;
#109266 = CARTESIAN_POINT('Ctrl Pts',(-17.9756578065929,-52.0793819609939,
122.913770905691)) ;
#109267 = CARTESIAN_POINT('Ctrl Pts',(-17.9092075693229,-52.0928554097491,
123.261476632465)) ;
#109268 = CARTESIAN_POINT('Ctrl Pts',(-17.9058669085398,-52.1026883675549,
123.519888511161)) ;
#109269 = CARTESIAN_POINT('Ctrl Pts',(-17.9468914650355,-52.1126516410056,
123.778461358619)) ;
#109270 = CARTESIAN_POINT('Ctrl Pts',(-18.0333653429648,-52.1226887148236,
124.027643619177)) ;
#109271 = CARTESIAN_POINT('Ctrl Pts',(-18.1593058164668,-52.1325637178352,
124.254574691994)) ;
#109272 = CARTESIAN_POINT('Ctrl Pts',(-18.3258898060172,-52.1426313974614,
124.460065581407)) ;
#109273 = CARTESIAN_POINT('Ctrl Pts',(-18.5210760121677,-52.1524722476791,
124.629759584367)) ;
#109274 = CARTESIAN_POINT('Ctrl Pts',(-18.821066323113,-52.1658084461551,
124.810893970577)) ;
#109275 = CARTESIAN_POINT('Ctrl Pts',(-19.1585367061457,-52.1790259699695,
124.908593466705)) ;
#109276 = CARTESIAN_POINT('Ctrl Pts',(-19.5088651508526,-52.1923608964608,
124.916062617369)) ;
#109277 = CARTESIAN_POINT('Ctrl Pts',(-19.7681923500913,-52.2023439970554,
124.87610822169)) ;
#109278 = CARTESIAN_POINT('Ctrl Pts',(-20.017988630059,-52.212388772955,124.790864379723)) ;
#109279 = CARTESIAN_POINT('Ctrl Pts',(-20.244250111229,-52.2222066961409,
124.6668494841)) ;
#109280 = CARTESIAN_POINT('Ctrl Pts',(-20.450605569741,-52.2322560100963,
124.502062270369)) ;
#109281 = CARTESIAN_POINT('Ctrl Pts',(-20.681220352099,-52.2455597507188,
124.239335951063)) ;
#109282 = CARTESIAN_POINT('Ctrl Pts',(-20.8766427398963,-52.2620499461955,
123.846935211259)) ;
#109283 = CARTESIAN_POINT('Ctrl Pts',(-20.9269324311696,-52.2787691111201,
123.40555050436)) ;
#109284 = CARTESIAN_POINT('Ctrl Pts',(-20.8757860399941,-52.2919301047903,
123.06342307163)) ;
#109285 = CARTESIAN_POINT('Ctrl Pts',(-20.7933342692634,-52.3019263268955,
122.814030291687)) ;
#109286 = CARTESIAN_POINT('Ctrl Pts',(-20.6679526627159,-52.3119501664292,
122.582364382692)) ;
#109287 = CARTESIAN_POINT('Ctrl Pts',(-20.4530759574167,-52.3251434884225,
122.310238877443)) ;
#109288 = CARTESIAN_POINT('Ctrl Pts',(-20.0984661627794,-52.3418026601998,
122.045166826132)) ;
#109289 = CARTESIAN_POINT('Ctrl Pts',(-19.5917771670296,-52.3617128356855,
121.892473324342)) ;
#109290 = CARTESIAN_POINT('Ctrl Pts',(-19.0638317581949,-52.3816028235299,
121.920720400418)) ;
#109291 = CARTESIAN_POINT('Ctrl Pts',(-18.5747188817248,-52.4016082715447,
122.129015928262)) ;
#109292 = CARTESIAN_POINT('Ctrl Pts',(-18.1887873835307,-52.421444665572,
122.488412492527)) ;
#109293 = CARTESIAN_POINT('Ctrl Pts',(-17.9465342575995,-52.4414524594687,
122.961640970763)) ;
#109294 = CARTESIAN_POINT('Ctrl Pts',(-17.8806979911709,-52.4612790957627,
123.484567234561)) ;
#109295 = CARTESIAN_POINT('Ctrl Pts',(-17.9971902184704,-52.4812580387165,
124.002618696318)) ;
#109296 = CARTESIAN_POINT('Ctrl Pts',(-18.283564362864,-52.5011898405856,
124.44821305183)) ;
#109297 = CARTESIAN_POINT('Ctrl Pts',(-18.7016410326483,-52.5210141410831,
124.769156799688)) ;
#109298 = CARTESIAN_POINT('Ctrl Pts',(-19.2109481937342,-52.5411101424229,
124.929334135715)) ;
#109299 = CARTESIAN_POINT('Ctrl Pts',(-19.7359311031487,-52.5608685585269,
124.907024725982)) ;
#109300 = CARTESIAN_POINT('Ctrl Pts',(-20.2295133744255,-52.580962251411,
124.703919481245)) ;
#109301 = CARTESIAN_POINT('Ctrl Pts',(-20.4872495056866,-52.5940732173177,
124.469072010777)) ;
#109302 = CARTESIAN_POINT('Ctrl Pts',(-20.5950554345716,-52.6007865921055,
124.330331920903)) ;
#109303 = CARTESIAN_POINT('Ctrl Pts',(-18.2740165434593,-11.6199309704797,
123.800453906728)) ;
#109304 = CARTESIAN_POINT('Ctrl Pts',(-18.3189584578479,-11.6265578212978,
123.931788727399)) ;
#109305 = CARTESIAN_POINT('Ctrl Pts',(-18.4545056342566,-11.6397884477788,
124.178258738967)) ;
#109306 = CARTESIAN_POINT('Ctrl Pts',(-18.7737315926305,-11.6597640690375,
124.458465178954)) ;
#109307 = CARTESIAN_POINT('Ctrl Pts',(-19.1683574117918,-11.6796814039394,
124.612093197678)) ;
#109308 = CARTESIAN_POINT('Ctrl Pts',(-19.5908278464546,-11.6995546806554,
124.622778355947)) ;
#109309 = CARTESIAN_POINT('Ctrl Pts',(-19.994464359519,-11.7195791708194,
124.487373578546)) ;
#109310 = CARTESIAN_POINT('Ctrl Pts',(-20.3250783731983,-11.7394470119701,
124.224300920966)) ;
#109311 = CARTESIAN_POINT('Ctrl Pts',(-20.5474461234229,-11.7593926628497,
123.863226231781)) ;
#109312 = CARTESIAN_POINT('Ctrl Pts',(-20.632926132733,-11.7792980634666,
123.448705424789)) ;
#109313 = CARTESIAN_POINT('Ctrl Pts',(-20.5727438758044,-11.799172291283,
123.030430585982)) ;
#109314 = CARTESIAN_POINT('Ctrl Pts',(-20.3723428011855,-11.8191580821606,
122.655687341884)) ;
#109315 = CARTESIAN_POINT('Ctrl Pts',(-20.0574083966758,-11.8390523248204,
122.37332944073)) ;
#109316 = CARTESIAN_POINT('Ctrl Pts',(-19.6656737478531,-11.8589310408924,
122.214453016222)) ;
#109317 = CARTESIAN_POINT('Ctrl Pts',(-19.2399036844466,-11.878970490737,
122.199179901226)) ;
#109318 = CARTESIAN_POINT('Ctrl Pts',(-18.83787455867,-11.8988336522749,122.329001393587)) ;
#109319 = CARTESIAN_POINT('Ctrl Pts',(-18.5023851512414,-11.9188130202891,
122.589387354643)) ;
#109320 = CARTESIAN_POINT('Ctrl Pts',(-18.277297372266,-11.9386236008119,
122.945534657321)) ;
#109321 = CARTESIAN_POINT('Ctrl Pts',(-18.1859011724605,-11.9586045290975,
123.360352267523)) ;
#109322 = CARTESIAN_POINT('Ctrl Pts',(-18.241593410712,-11.9784972009669,
123.779690572845)) ;
#109323 = CARTESIAN_POINT('Ctrl Pts',(-18.4366948796533,-11.9984235312541,
124.155782379027)) ;
#109324 = CARTESIAN_POINT('Ctrl Pts',(-18.7493816096207,-12.0183940853463,
124.443073287162)) ;
#109325 = CARTESIAN_POINT('Ctrl Pts',(-19.0736805607038,-12.034925924434,
124.578622068491)) ;
#109326 = CARTESIAN_POINT('Ctrl Pts',(-19.3515879174634,-12.0482656632615,
124.616550900402)) ;
#109327 = CARTESIAN_POINT('Ctrl Pts',(-19.5623144109736,-12.0582979054801,
124.608028974798)) ;
#109328 = CARTESIAN_POINT('Ctrl Pts',(-19.7648627604016,-12.0681556061236,
124.56413869026)) ;
#109329 = CARTESIAN_POINT('Ctrl Pts',(-19.9594469113079,-12.0781474707628,
124.485041784485)) ;
#109330 = CARTESIAN_POINT('Ctrl Pts',(-20.1360963420345,-12.088070020523,
124.374088349641)) ;
#109331 = CARTESIAN_POINT('Ctrl Pts',(-20.3435978570512,-12.1013477940164,
124.187361805922)) ;
#109332 = CARTESIAN_POINT('Ctrl Pts',(-20.4979415370848,-12.114695132957,
123.949247082496)) ;
#109333 = CARTESIAN_POINT('Ctrl Pts',(-20.5838258782589,-12.1279023647502,
123.685145349159)) ;
#109334 = CARTESIAN_POINT('Ctrl Pts',(-20.6134813207567,-12.1378894808399,
123.477327116893)) ;
#109335 = CARTESIAN_POINT('Ctrl Pts',(-20.6067609171746,-12.1478403864197,
123.268195447007)) ;
#109336 = CARTESIAN_POINT('Ctrl Pts',(-20.5631573475887,-12.1578954884271,
123.061381717874)) ;
#109337 = CARTESIAN_POINT('Ctrl Pts',(-20.4864536400712,-12.1677171617482,
122.86964880363)) ;
#109338 = CARTESIAN_POINT('Ctrl Pts',(-20.3753205112896,-12.1777756328231,
122.689772517419)) ;
#109339 = CARTESIAN_POINT('Ctrl Pts',(-20.236275475545,-12.1877002439996,
122.534182095984)) ;
#109340 = CARTESIAN_POINT('Ctrl Pts',(-20.0174291749034,-12.2009775829,122.360945032613)) ;
#109341 = CARTESIAN_POINT('Ctrl Pts',(-19.7578511133676,-12.2142764621376,
122.248868010914)) ;
#109342 = CARTESIAN_POINT('Ctrl Pts',(-19.4824869100244,-12.2275153343083,
122.208104901209)) ;
#109343 = CARTESIAN_POINT('Ctrl Pts',(-19.2721841990618,-12.2375219524449,
122.213537831831)) ;
#109344 = CARTESIAN_POINT('Ctrl Pts',(-19.0656057042357,-12.2475528975064,
122.255904229453)) ;
#109345 = CARTESIAN_POINT('Ctrl Pts',(-18.8727802787229,-12.2574090708583,
122.331796234193)) ;
#109346 = CARTESIAN_POINT('Ctrl Pts',(-18.6933999177951,-12.2674083418211,
122.441334300413)) ;
#109347 = CARTESIAN_POINT('Ctrl Pts',(-18.5371998957103,-12.2773027935785,
122.578764123913)) ;
#109348 = CARTESIAN_POINT('Ctrl Pts',(-18.4051179179187,-12.2873661093878,
122.743982953584)) ;
#109349 = CARTESIAN_POINT('Ctrl Pts',(-18.3057447497142,-12.2972049661274,
122.925434068836)) ;
#109350 = CARTESIAN_POINT('Ctrl Pts',(-18.2376547052044,-12.307271087945,
123.125766687681)) ;
#109351 = CARTESIAN_POINT('Ctrl Pts',(-18.2060559824782,-12.3171543156693,
123.331154387361)) ;
#109352 = CARTESIAN_POINT('Ctrl Pts',(-18.210187256947,-12.3271437769481,
123.541102643659)) ;
#109353 = CARTESIAN_POINT('Ctrl Pts',(-18.2506856957687,-12.3371074873745,
123.746629235204)) ;
#109354 = CARTESIAN_POINT('Ctrl Pts',(-18.3262879839171,-12.3471024901054,
123.942700680937)) ;
#109355 = CARTESIAN_POINT('Ctrl Pts',(-18.4355049106728,-12.3571388211157,
124.123217326522)) ;
#109356 = CARTESIAN_POINT('Ctrl Pts',(-18.5715338688606,-12.366985050458,
124.279261942)) ;
#109357 = CARTESIAN_POINT('Ctrl Pts',(-18.7345869263412,-12.3769705487333,
124.411432153521)) ;
#109358 = CARTESIAN_POINT('Ctrl Pts',(-18.9171714511557,-12.3869054517162,
124.512934466652)) ;
#109359 = CARTESIAN_POINT('Ctrl Pts',(-19.1170398194792,-12.3969629548115,
124.581832630242)) ;
#109360 = CARTESIAN_POINT('Ctrl Pts',(-19.3209400853266,-12.406784611182,
124.614524423737)) ;
#109361 = CARTESIAN_POINT('Ctrl Pts',(-19.5323133885806,-12.4168406738471,
124.611634485065)) ;
#109362 = CARTESIAN_POINT('Ctrl Pts',(-19.7375456386176,-12.4267813385503,
124.572166328423)) ;
#109363 = CARTESIAN_POINT('Ctrl Pts',(-19.9323214479051,-12.4366857424989,
124.498546480256)) ;
#109364 = CARTESIAN_POINT('Ctrl Pts',(-20.1138409023662,-12.4467322274924,
124.390597508146)) ;
#109365 = CARTESIAN_POINT('Ctrl Pts',(-20.2716172652124,-12.4566284553041,
124.254936806907)) ;
#109366 = CARTESIAN_POINT('Ctrl Pts',(-20.4056121610864,-12.4666880388676,
124.091347650261)) ;
#109367 = CARTESIAN_POINT('Ctrl Pts',(-20.507066141368,-12.4765400485364,
123.910765831866)) ;
#109368 = CARTESIAN_POINT('Ctrl Pts',(-20.5770507733856,-12.486502579976,
123.713371093661)) ;
#109369 = CARTESIAN_POINT('Ctrl Pts',(-20.611619329922,-12.4965341282154,
123.505321762573)) ;
#109370 = CARTESIAN_POINT('Ctrl Pts',(-20.6097667698455,-12.5064255394284,
123.297381642139)) ;
#109371 = CARTESIAN_POINT('Ctrl Pts',(-20.5717313917485,-12.5164417931364,
123.090264184129)) ;
#109372 = CARTESIAN_POINT('Ctrl Pts',(-20.4977853673084,-12.5264718959811,
122.892794265222)) ;
#109373 = CARTESIAN_POINT('Ctrl Pts',(-20.3928637205027,-12.5363283449348,
122.714092812673)) ;
#109374 = CARTESIAN_POINT('Ctrl Pts',(-20.2567958209577,-12.5463273557071,
122.553905492347)) ;
#109375 = CARTESIAN_POINT('Ctrl Pts',(-20.0967563412076,-12.5562225726251,
122.420949585091)) ;
#109376 = CARTESIAN_POINT('Ctrl Pts',(-19.9130848862306,-12.5662830879825,
122.316129329314)) ;
#109377 = CARTESIAN_POINT('Ctrl Pts',(-19.7181830382075,-12.5761323813695,
122.246165874868)) ;
#109378 = CARTESIAN_POINT('Ctrl Pts',(-19.5105194628057,-12.5861595570495,
122.209950449473)) ;
#109379 = CARTESIAN_POINT('Ctrl Pts',(-19.2996790125702,-12.5961881326767,
122.210897336968)) ;
#109380 = CARTESIAN_POINT('Ctrl Pts',(-19.0959517446353,-12.6060332262226,
122.247358522708)) ;
#109381 = CARTESIAN_POINT('Ctrl Pts',(-18.8985634765197,-12.6160244676544,
122.319182824595)) ;
#109382 = CARTESIAN_POINT('Ctrl Pts',(-18.7160505312803,-12.6260602487976,
122.425038804406)) ;
#109383 = CARTESIAN_POINT('Ctrl Pts',(-18.5574736340685,-12.6359124545273,
122.558270830057)) ;
#109384 = CARTESIAN_POINT('Ctrl Pts',(-18.42248512393,-12.6458745486443,122.718394030827)) ;
#109385 = CARTESIAN_POINT('Ctrl Pts',(-18.3169324777761,-12.6558971094714,
122.900755181411)) ;
#109386 = CARTESIAN_POINT('Ctrl Pts',(-18.245130469483,-12.665824881123,123.096749174047)) ;
#109387 = CARTESIAN_POINT('Ctrl Pts',(-18.2080549208433,-12.6758672652478,
123.304574961793)) ;
#109388 = CARTESIAN_POINT('Ctrl Pts',(-18.2075488189041,-12.6857564893184,
123.512488877524)) ;
#109389 = CARTESIAN_POINT('Ctrl Pts',(-18.2431194259335,-12.6957457374858,
123.719452863823)) ;
#109390 = CARTESIAN_POINT('Ctrl Pts',(-18.3140184092516,-12.7057043145277,
123.916437185084)) ;
#109391 = CARTESIAN_POINT('Ctrl Pts',(-18.4169896425226,-12.715603883619,
124.09731297473)) ;
#109392 = CARTESIAN_POINT('Ctrl Pts',(-18.5518287181094,-12.725651795703,
124.259889532206)) ;
#109393 = CARTESIAN_POINT('Ctrl Pts',(-18.7103384941657,-12.7355471500102,
124.394667760721)) ;
#109394 = CARTESIAN_POINT('Ctrl Pts',(-18.8927953986471,-12.7456088005014,
124.501642275432)) ;
#109395 = CARTESIAN_POINT('Ctrl Pts',(-19.0867950431812,-12.7554534159639,
124.57376207232)) ;
#109396 = CARTESIAN_POINT('Ctrl Pts',(-19.2926110827325,-12.7654134948653,
124.612276631945)) ;
#109397 = CARTESIAN_POINT('Ctrl Pts',(-19.5036297168892,-12.7754516892237,
124.614075938439)) ;
#109398 = CARTESIAN_POINT('Ctrl Pts',(-19.7084424248004,-12.7853254046233,
124.580155183645)) ;
#109399 = CARTESIAN_POINT('Ctrl Pts',(-19.9081211140356,-12.7953971141575,
124.509801894743)) ;
#109400 = CARTESIAN_POINT('Ctrl Pts',(-20.0882669500003,-12.80522955461,124.408397818278)) ;
#109401 = CARTESIAN_POINT('Ctrl Pts',(-20.2516658484131,-12.8152613755354,
124.275064631415)) ;
#109402 = CARTESIAN_POINT('Ctrl Pts',(-20.3888239935729,-12.825281745421,
124.115169890093)) ;
#109403 = CARTESIAN_POINT('Ctrl Pts',(-20.4949634387566,-12.8351485165548,
123.936935099136)) ;
#109404 = CARTESIAN_POINT('Ctrl Pts',(-20.570045410844,-12.8452192877441,
123.738998457386)) ;
#109405 = CARTESIAN_POINT('Ctrl Pts',(-20.608753720074,-12.8550624482657,
123.535705476425)) ;
#109406 = CARTESIAN_POINT('Ctrl Pts',(-20.6123036182305,-12.8650426814522,
123.325926427639)) ;
#109407 = CARTESIAN_POINT('Ctrl Pts',(-20.5788479016647,-12.8750612014873,
123.117985181259)) ;
#109408 = CARTESIAN_POINT('Ctrl Pts',(-20.511135136831,-12.884944509871,122.921523586511)) ;
#109409 = CARTESIAN_POINT('Ctrl Pts',(-20.4084000656426,-12.8950127940418,
122.736499728356)) ;
#109410 = CARTESIAN_POINT('Ctrl Pts',(-20.2783984392069,-12.9048429207095,
122.575806329427)) ;
#109411 = CARTESIAN_POINT('Ctrl Pts',(-20.1189512083603,-12.914909492916,
122.436701980208)) ;
#109412 = CARTESIAN_POINT('Ctrl Pts',(-19.9408318540833,-12.9247996491567,
122.329389688264)) ;
#109413 = CARTESIAN_POINT('Ctrl Pts',(-19.7449774725297,-12.9347921767331,
122.253452042558)) ;
#109414 = CARTESIAN_POINT('Ctrl Pts',(-19.539505250276,-12.9447536666074,
122.21297524759)) ;
#109415 = CARTESIAN_POINT('Ctrl Pts',(-19.331225266214,-12.9546628884946,
122.208333177104)) ;
#109416 = CARTESIAN_POINT('Ctrl Pts',(-19.1224390490768,-12.964711468305,
122.240442162136)) ;
#109417 = CARTESIAN_POINT('Ctrl Pts',(-18.9256507642036,-12.974594442775,
122.307133949875)) ;
#109418 = CARTESIAN_POINT('Ctrl Pts',(-18.7411652401406,-12.9845893539177,
122.407705181215)) ;
#109419 = CARTESIAN_POINT('Ctrl Pts',(-18.5766906054186,-12.9946097404913,
122.539355425286)) ;
#109420 = CARTESIAN_POINT('Ctrl Pts',(-18.4390337996483,-13.0045198443484,
122.695723658892)) ;
#109421 = CARTESIAN_POINT('Ctrl Pts',(-18.3299475201132,-13.0144475565583,
122.873667321745)) ;
#109422 = CARTESIAN_POINT('Ctrl Pts',(-18.2526965274327,-13.0244906663255,
123.070156663903)) ;
#109423 = CARTESIAN_POINT('Ctrl Pts',(-18.2112560704067,-13.0343770867811,
123.273838810306)) ;
#109424 = CARTESIAN_POINT('Ctrl Pts',(-18.2053955760994,-13.0443702643867,
123.483833528556)) ;
#109425 = CARTESIAN_POINT('Ctrl Pts',(-18.2360212287472,-13.0543159272906,
123.690667983363)) ;
#109426 = CARTESIAN_POINT('Ctrl Pts',(-18.3017033464336,-13.0642632234958,
123.889219184243)) ;
#109427 = CARTESIAN_POINT('Ctrl Pts',(-18.4020633773929,-13.0743109890737,
124.075084996336)) ;
#109428 = CARTESIAN_POINT('Ctrl Pts',(-18.5304401414482,-13.0841592022913,
124.237516085386)) ;
#109429 = CARTESIAN_POINT('Ctrl Pts',(-18.6863595357741,-13.0941187750854,
124.37726396631)) ;
#109430 = CARTESIAN_POINT('Ctrl Pts',(-18.8657414368651,-13.1041553961179,
124.488354075364)) ;
#109431 = CARTESIAN_POINT('Ctrl Pts',(-19.0585457144832,-13.1140359109283,
124.565704233545)) ;
#109432 = CARTESIAN_POINT('Ctrl Pts',(-19.2653263607109,-13.1240885622353,
124.609213639801)) ;
#109433 = CARTESIAN_POINT('Ctrl Pts',(-19.47327955198,-13.1339839605153,124.616136490492)) ;
#109434 = CARTESIAN_POINT('Ctrl Pts',(-19.6824477261472,-13.1440340822214,
124.586491930911)) ;
#109435 = CARTESIAN_POINT('Ctrl Pts',(-19.8800328919683,-13.1539183617633,
124.522077682984)) ;
#109436 = CARTESIAN_POINT('Ctrl Pts',(-20.0656316770812,-13.1639131430553,
124.423608811804)) ;
#109437 = CARTESIAN_POINT('Ctrl Pts',(-20.2305126031394,-13.173860988242,
124.294932526718)) ;
#109438 = CARTESIAN_POINT('Ctrl Pts',(-20.370596849486,-13.1837979516294,
124.139979613577)) ;
#109439 = CARTESIAN_POINT('Ctrl Pts',(-20.482409312778,-13.1937809163667,
123.962339150495)) ;
#109440 = CARTESIAN_POINT('Ctrl Pts',(-20.5617843343879,-13.2038247677823,
123.766698740416)) ;
#109441 = CARTESIAN_POINT('Ctrl Pts',(-20.6055237172871,-13.213652969117,
123.564729914202)) ;
#109442 = CARTESIAN_POINT('Ctrl Pts',(-20.6138303777182,-13.2237295417151,
123.35309488214)) ;
#109443 = CARTESIAN_POINT('Ctrl Pts',(-20.585992210631,-13.2335816217226,
123.147807214761)) ;
#109444 = CARTESIAN_POINT('Ctrl Pts',(-20.5217116640761,-13.2436549067267,
122.94606310907)) ;
#109445 = CARTESIAN_POINT('Ctrl Pts',(-20.4255714232564,-13.2534962584372,
122.762843217951)) ;
#109446 = CARTESIAN_POINT('Ctrl Pts',(-20.2981644274266,-13.2634577578337,
122.596651344732)) ;
#109447 = CARTESIAN_POINT('Ctrl Pts',(-20.1424206513092,-13.2734935339637,
122.454309695618)) ;
#109448 = CARTESIAN_POINT('Ctrl Pts',(-19.9670675915503,-13.2833819606013,
122.342655174242)) ;
#109449 = CARTESIAN_POINT('Ctrl Pts',(-19.7726690014556,-13.2933972826762,
122.261750155835)) ;
#109450 = CARTESIAN_POINT('Ctrl Pts',(-19.5667675522153,-13.3034276315764,
122.216240187996)) ;
#109451 = CARTESIAN_POINT('Ctrl Pts',(-19.3600430082934,-13.3132710071831,
122.206925909651)) ;
#109452 = CARTESIAN_POINT('Ctrl Pts',(-19.1508941864425,-13.3233004440802,
122.233686847796)) ;
#109453 = CARTESIAN_POINT('Ctrl Pts',(-18.9496884327327,-13.3333323220132,
122.296924041704)) ;
#109454 = CARTESIAN_POINT('Ctrl Pts',(-18.7661167576985,-13.3431619451186,
122.391793595031)) ;
#109455 = CARTESIAN_POINT('Ctrl Pts',(-18.5987378566732,-13.3531514162717,
122.518643637613)) ;
#109456 = CARTESIAN_POINT('Ctrl Pts',(-18.4555483071856,-13.3631952650341,
122.673826378174)) ;
#109457 = CARTESIAN_POINT('Ctrl Pts',(-18.3436412819602,-13.3730169705658,
122.847354026751)) ;
#109458 = CARTESIAN_POINT('Ctrl Pts',(-18.2613484113623,-13.3830520103936,
123.041609263974)) ;
#109459 = CARTESIAN_POINT('Ctrl Pts',(-18.2146498332486,-13.3930767172851,
123.247129031518)) ;
#109460 = CARTESIAN_POINT('Ctrl Pts',(-18.2040846946911,-13.4029294216258,
123.453993452439)) ;
#109461 = CARTESIAN_POINT('Ctrl Pts',(-18.2295836172356,-13.4129175438335,
123.662406065847)) ;
#109462 = CARTESIAN_POINT('Ctrl Pts',(-18.290511914422,-13.4228460139408,
123.862048515229)) ;
#109463 = CARTESIAN_POINT('Ctrl Pts',(-18.3854475960473,-13.432834991108,
124.049375415601)) ;
#109464 = CARTESIAN_POINT('Ctrl Pts',(-18.5123625293364,-13.4428727983877,
124.217964745205)) ;
#109465 = CARTESIAN_POINT('Ctrl Pts',(-18.6634533043367,-13.452719099251,
124.359461543734)) ;
#109466 = CARTESIAN_POINT('Ctrl Pts',(-18.8397204086707,-13.4627448426303,
124.475030607362)) ;
#109467 = CARTESIAN_POINT('Ctrl Pts',(-19.0336949652238,-13.4727757090693,
124.55777688439)) ;
#109468 = CARTESIAN_POINT('Ctrl Pts',(-19.2350194889933,-13.4826130678681,
124.605064267741)) ;
#109469 = CARTESIAN_POINT('Ctrl Pts',(-19.4447178166025,-13.4926050288019,
124.617421996608)) ;
#109470 = CARTESIAN_POINT('Ctrl Pts',(-19.6541798442006,-13.5026373913584,
124.592661530218)) ;
#109471 = CARTESIAN_POINT('Ctrl Pts',(-19.852848820897,-13.5125025519328,
124.533165503474)) ;
#109472 = CARTESIAN_POINT('Ctrl Pts',(-20.0402681725955,-13.5224644565105,
124.439690047021)) ;
#109473 = CARTESIAN_POINT('Ctrl Pts',(-20.2096246621819,-13.5324993865863,
124.313911734044)) ;
#109474 = CARTESIAN_POINT('Ctrl Pts',(-20.3526856519067,-13.5423843334399,
124.163140610676)) ;
#109475 = CARTESIAN_POINT('Ctrl Pts',(-20.4694160685004,-13.5524500097513,
123.986678417847)) ;
#109476 = CARTESIAN_POINT('Ctrl Pts',(-20.5520572395193,-13.5622889293862,
123.797021956805)) ;
#109477 = CARTESIAN_POINT('Ctrl Pts',(-20.6018696701795,-13.5723524391207,
123.59143381905)) ;
#109478 = CARTESIAN_POINT('Ctrl Pts',(-20.6148347992683,-13.5822460522824,
123.383819066269)) ;
#109479 = CARTESIAN_POINT('Ctrl Pts',(-20.5919920261303,-13.5921900590958,
123.176044950521)) ;
#109480 = CARTESIAN_POINT('Ctrl Pts',(-20.5331618969595,-13.6021910134501,
122.974158341515)) ;
#109481 = CARTESIAN_POINT('Ctrl Pts',(-20.4395047172235,-13.6122297711424,
122.785052585812)) ;
#109482 = CARTESIAN_POINT('Ctrl Pts',(-20.3174523845497,-13.6220539553124,
122.618417886786)) ;
#109483 = CARTESIAN_POINT('Ctrl Pts',(-20.1650112643966,-13.6321120209118,
122.471905241046)) ;
#109484 = CARTESIAN_POINT('Ctrl Pts',(-19.9915019526225,-13.6420420676865,
122.355797819438)) ;
#109485 = CARTESIAN_POINT('Ctrl Pts',(-19.8002891820888,-13.6519935100237,
122.270899225697)) ;
#109486 = CARTESIAN_POINT('Ctrl Pts',(-19.5952293664333,-13.6620403072029,
122.220289731585)) ;
#109487 = CARTESIAN_POINT('Ctrl Pts',(-19.3886786446187,-13.671888247883,
122.20614277272)) ;
#109488 = CARTESIAN_POINT('Ctrl Pts',(-19.1803731343022,-13.6818498792256,
122.227680223616)) ;
#109489 = CARTESIAN_POINT('Ctrl Pts',(-18.9776681132246,-13.6918785386015,
122.285706651592)) ;
#109490 = CARTESIAN_POINT('Ctrl Pts',(-18.7903445226106,-13.7017888414897,
122.376887794601)) ;
#109491 = CARTESIAN_POINT('Ctrl Pts',(-18.6209463456044,-13.7117237360519,
122.499078917062)) ;
#109492 = CARTESIAN_POINT('Ctrl Pts',(-18.4739308193675,-13.7217648347188,
122.650555081557)) ;
#109493 = CARTESIAN_POINT('Ctrl Pts',(-18.3571350633017,-13.7316521172232,
122.822514937511)) ;
#109494 = CARTESIAN_POINT('Ctrl Pts',(-18.2707571691785,-13.7416438577337,
123.013976715457)) ;
#109495 = CARTESIAN_POINT('Ctrl Pts',(-18.2192126419942,-13.7515944069691,
123.216729538834)) ;
#109496 = CARTESIAN_POINT('Ctrl Pts',(-18.203370025249,-13.7615300846039,
123.424994336609)) ;
#109497 = CARTESIAN_POINT('Ctrl Pts',(-18.2238119198968,-13.7715155023967,
123.633937897449)) ;
#109498 = CARTESIAN_POINT('Ctrl Pts',(-18.2807153147586,-13.7815442952672,
123.836949140356)) ;
#109499 = CARTESIAN_POINT('Ctrl Pts',(-18.3704450421191,-13.7914238064952,
124.024261873033)) ;
#109500 = CARTESIAN_POINT('Ctrl Pts',(-18.4923442691577,-13.8014173431681,
124.195388052739)) ;
#109501 = CARTESIAN_POINT('Ctrl Pts',(-18.6429808856488,-13.811449611432,
124.342995145723)) ;
#109502 = CARTESIAN_POINT('Ctrl Pts',(-18.8138140242509,-13.8213135734378,
124.460588169099)) ;
#109503 = CARTESIAN_POINT('Ctrl Pts',(-19.0063568997655,-13.8313836347827,
124.548546337891)) ;
#109504 = CARTESIAN_POINT('Ctrl Pts',(-19.2066469307211,-13.8412259991315,
124.600533457555)) ;
#109505 = CARTESIAN_POINT('Ctrl Pts',(-19.4153248704645,-13.8511866716339,
124.6179206199)) ;
#109506 = CARTESIAN_POINT('Ctrl Pts',(-19.6254284412312,-13.8612247427017,
124.598242788524)) ;
#109507 = CARTESIAN_POINT('Ctrl Pts',(-19.825733453416,-13.8710983576622,
124.543671242809)) ;
#109508 = CARTESIAN_POINT('Ctrl Pts',(-20.0172095782411,-13.8811705922434,
124.453349060342)) ;
#109509 = CARTESIAN_POINT('Ctrl Pts',(-20.1860361213038,-13.8909946106922,
124.334308781026)) ;
#109510 = CARTESIAN_POINT('Ctrl Pts',(-20.3353297963812,-13.9010595316682,
124.18442760228)) ;
#109511 = CARTESIAN_POINT('Ctrl Pts',(-20.4942348757896,-13.914269829963,
123.956571188702)) ;
#109512 = CARTESIAN_POINT('Ctrl Pts',(-20.5910379879505,-13.9275852766949,
123.690586163799)) ;
#109513 = CARTESIAN_POINT('Ctrl Pts',(-20.6153297489384,-13.9408755219622,
123.412198327519)) ;
#109514 = CARTESIAN_POINT('Ctrl Pts',(-20.5967516359263,-13.9509262715693,
123.201753172192)) ;
#109515 = CARTESIAN_POINT('Ctrl Pts',(-20.543590199386,-13.9607388785516,
123.002398163361)) ;
#109516 = CARTESIAN_POINT('Ctrl Pts',(-20.4546105244745,-13.9708099765458,
122.810305934191)) ;
#109517 = CARTESIAN_POINT('Ctrl Pts',(-20.3356145167532,-13.9806995493207,
122.639802315371)) ;
#109518 = CARTESIAN_POINT('Ctrl Pts',(-20.1392383449349,-13.993969656124,
122.441608051328)) ;
#109519 = CARTESIAN_POINT('Ctrl Pts',(-19.8341118265951,-14.0105863430465,
122.263579363717)) ;
#109520 = CARTESIAN_POINT('Ctrl Pts',(-19.4873914708568,-14.0271603863627,
122.200251214047)) ;
#109521 = CARTESIAN_POINT('Ctrl Pts',(-19.2087764199032,-14.0404569537945,
122.222571598976)) ;
#109522 = CARTESIAN_POINT('Ctrl Pts',(-19.004705588221,-14.0504870173719,
122.275708570567)) ;
#109523 = CARTESIAN_POINT('Ctrl Pts',(-18.8155858009188,-14.0603809092212,
122.362246602637)) ;
#109524 = CARTESIAN_POINT('Ctrl Pts',(-18.5855945815836,-14.0736336650067,
122.519619615386)) ;
#109525 = CARTESIAN_POINT('Ctrl Pts',(-18.3545276201767,-14.0903617699992,
122.789939168335)) ;
#109526 = CARTESIAN_POINT('Ctrl Pts',(-18.2063450814763,-14.1101926064777,
123.18478360627)) ;
#109527 = CARTESIAN_POINT('Ctrl Pts',(-18.2007419609984,-14.1301179983678,
123.60832004595)) ;
#109528 = CARTESIAN_POINT('Ctrl Pts',(-18.3401055535235,-14.1500432117198,
124.008477481292)) ;
#109529 = CARTESIAN_POINT('Ctrl Pts',(-18.6074981505326,-14.1699682252049,
124.337030896518)) ;
#109530 = CARTESIAN_POINT('Ctrl Pts',(-18.969837071854,-14.1898446969049,
124.554624389499)) ;
#109531 = CARTESIAN_POINT('Ctrl Pts',(-19.3867580229997,-14.2098240148138,
124.636106317606)) ;
#109532 = CARTESIAN_POINT('Ctrl Pts',(-19.8054748474026,-14.2297570183898,
124.570257107458)) ;
#109533 = CARTESIAN_POINT('Ctrl Pts',(-20.1760501306965,-14.2496522884175,
124.366285575119)) ;
#109534 = CARTESIAN_POINT('Ctrl Pts',(-20.4554968261467,-14.2695736263233,
124.047938307059)) ;
#109535 = CARTESIAN_POINT('Ctrl Pts',(-20.6097303117202,-14.2895312495895,
123.652583375934)) ;
#109536 = CARTESIAN_POINT('Ctrl Pts',(-20.6198476183914,-14.3094110815467,
123.230070591861)) ;
#109537 = CARTESIAN_POINT('Ctrl Pts',(-20.4862218373925,-14.3292929328436,
122.828917275061)) ;
#109538 = CARTESIAN_POINT('Ctrl Pts',(-20.2206792290437,-14.3493639499474,
122.494899503894)) ;
#109539 = CARTESIAN_POINT('Ctrl Pts',(-19.8617957217555,-14.3691711737005,
122.274354166508)) ;
#109540 = CARTESIAN_POINT('Ctrl Pts',(-19.4458882801742,-14.3891523092693,
122.187819071332)) ;
#109541 = CARTESIAN_POINT('Ctrl Pts',(-19.0266631682687,-14.4090798026085,
122.249061084022)) ;
#109542 = CARTESIAN_POINT('Ctrl Pts',(-18.6546849167205,-14.4289004639663,
122.447411997577)) ;
#109543 = CARTESIAN_POINT('Ctrl Pts',(-18.3694753213306,-14.4489976531881,
122.765412017463)) ;
#109544 = CARTESIAN_POINT('Ctrl Pts',(-18.212151874632,-14.4687613321965,
123.155302225518)) ;
#109545 = CARTESIAN_POINT('Ctrl Pts',(-18.1966217826831,-14.4888186108695,
123.581303929373)) ;
#109546 = CARTESIAN_POINT('Ctrl Pts',(-18.3260112271543,-14.5086140346169,
123.981947343732)) ;
#109547 = CARTESIAN_POINT('Ctrl Pts',(-18.5854072331343,-14.5285776793445,
124.31788876283)) ;
#109548 = CARTESIAN_POINT('Ctrl Pts',(-18.9448261731476,-14.5485611706186,
124.544527237678)) ;
#109549 = CARTESIAN_POINT('Ctrl Pts',(-19.3562025954833,-14.5683686657679,
124.634965613811)) ;
#109550 = CARTESIAN_POINT('Ctrl Pts',(-19.7773748585471,-14.588351256488,
124.579603795729)) ;
#109551 = CARTESIAN_POINT('Ctrl Pts',(-20.1526221909103,-14.6082339104793,
124.384671060941)) ;
#109552 = CARTESIAN_POINT('Ctrl Pts',(-20.4400220888075,-14.6281921553423,
124.072556437344)) ;
#109553 = CARTESIAN_POINT('Ctrl Pts',(-20.6032822459784,-14.6480677423839,
123.682687060369)) ;
#109554 = CARTESIAN_POINT('Ctrl Pts',(-20.6241041028713,-14.6680486305192,
123.258378223045)) ;
#109555 = CARTESIAN_POINT('Ctrl Pts',(-20.4988242553076,-14.6879837716302,
122.853380464122)) ;
#109556 = CARTESIAN_POINT('Ctrl Pts',(-20.2434601424034,-14.7078957896413,
122.515729216227)) ;
#109557 = CARTESIAN_POINT('Ctrl Pts',(-19.8888235692295,-14.7277840078848,
122.285352048189)) ;
#109558 = CARTESIAN_POINT('Ctrl Pts',(-19.5451529782308,-14.7443823117317,
122.205344181822)) ;
#109559 = CARTESIAN_POINT('Ctrl Pts',(-19.2662167204674,-14.7576549016346,
122.214362442295)) ;
#109560 = CARTESIAN_POINT('Ctrl Pts',(-19.0602783592496,-14.7676623165854,
122.257360680082)) ;
#109561 = CARTESIAN_POINT('Ctrl Pts',(-18.8649799519787,-14.777669663318,
122.335647470716)) ;
#109562 = CARTESIAN_POINT('Ctrl Pts',(-18.6279934117573,-14.7909360231196,
122.482611222919)) ;
#109563 = CARTESIAN_POINT('Ctrl Pts',(-18.3871462871547,-14.8074506807426,
122.738163547435)) ;
#109564 = CARTESIAN_POINT('Ctrl Pts',(-18.2465602928986,-14.8240481139852,
123.061779179124)) ;
#109565 = CARTESIAN_POINT('Ctrl Pts',(-18.205485799876,-14.8373961111302,
123.339439525527)) ;
#109566 = CARTESIAN_POINT('Ctrl Pts',(-18.2109597428705,-14.8472918654818,
123.547401713647)) ;
#109567 = CARTESIAN_POINT('Ctrl Pts',(-18.2525893133953,-14.8572798194132,
123.753197605181)) ;
#109568 = CARTESIAN_POINT('Ctrl Pts',(-18.329012459074,-14.8672370431179,
123.948107145997)) ;
#109569 = CARTESIAN_POINT('Ctrl Pts',(-18.4390392351625,-14.8772725896746,
124.128107227732)) ;
#109570 = CARTESIAN_POINT('Ctrl Pts',(-18.5764840627479,-14.8871597009507,
124.28405500871)) ;
#109571 = CARTESIAN_POINT('Ctrl Pts',(-18.7404042636375,-14.8971511060515,
124.415383899885)) ;
#109572 = CARTESIAN_POINT('Ctrl Pts',(-18.9238326319927,-14.9070967272663,
124.515742159357)) ;
#109573 = CARTESIAN_POINT('Ctrl Pts',(-19.1218477324172,-14.9170459755346,
124.583157249583)) ;
#109574 = CARTESIAN_POINT('Ctrl Pts',(-19.3305973942062,-14.9270924707032,
124.615231794087)) ;
#109575 = CARTESIAN_POINT('Ctrl Pts',(-19.5376679335332,-14.9369438134948,
124.610869422813)) ;
#109576 = CARTESIAN_POINT('Ctrl Pts',(-19.7433876347227,-14.9469155936221,
124.570653906068)) ;
#109577 = CARTESIAN_POINT('Ctrl Pts',(-19.9395052151487,-14.9569107935998,
124.49511099063)) ;
#109578 = CARTESIAN_POINT('Ctrl Pts',(-20.1200485399181,-14.9669447852959,
124.386048025066)) ;
#109579 = CARTESIAN_POINT('Ctrl Pts',(-20.2763298912303,-14.9768001902684,
124.249986086602)) ;
#109580 = CARTESIAN_POINT('Ctrl Pts',(-20.4087021703842,-14.9867994881141,
124.086727001076)) ;
#109581 = CARTESIAN_POINT('Ctrl Pts',(-20.5098840238839,-14.9966946007193,
123.904925282074)) ;
#109582 = CARTESIAN_POINT('Ctrl Pts',(-20.5790585403251,-15.0067552462543,
123.705079406197)) ;
#109583 = CARTESIAN_POINT('Ctrl Pts',(-20.6119035237145,-15.0166041232435,
123.500630488175)) ;
#109584 = CARTESIAN_POINT('Ctrl Pts',(-20.6092249525559,-15.0266328343371,
123.289815302828)) ;
#109585 = CARTESIAN_POINT('Ctrl Pts',(-20.5694153658592,-15.0366622355932,
123.082753754717)) ;
#109586 = CARTESIAN_POINT('Ctrl Pts',(-20.4961065186197,-15.0465024273892,
122.889303085356)) ;
#109587 = CARTESIAN_POINT('Ctrl Pts',(-20.3889142895165,-15.0565058565822,
122.708392615128)) ;
#109588 = CARTESIAN_POINT('Ctrl Pts',(-20.2520951560738,-15.0664913690484,
122.549129092495)) ;
#109589 = CARTESIAN_POINT('Ctrl Pts',(-20.0887057062844,-15.0765324654324,
122.415501229975)) ;
#109590 = CARTESIAN_POINT('Ctrl Pts',(-19.9083321929545,-15.0863756613834,
122.314037128764)) ;
#109591 = CARTESIAN_POINT('Ctrl Pts',(-19.7104324077991,-15.0963619724378,
122.244058195102)) ;
#109592 = CARTESIAN_POINT('Ctrl Pts',(-19.5044074815444,-15.1062966576955,
122.209531335176)) ;
#109593 = CARTESIAN_POINT('Ctrl Pts',(-19.2930056275921,-15.1163542189126,
122.211509097799)) ;
#109594 = CARTESIAN_POINT('Ctrl Pts',(-19.0899248969351,-15.1261758605212,
122.248955348946)) ;
#109595 = CARTESIAN_POINT('Ctrl Pts',(-18.8917123028811,-15.1362319241121,
122.322431823877)) ;
#109596 = CARTESIAN_POINT('Ctrl Pts',(-18.7115304275704,-15.1461725998739,
122.428321237791)) ;
#109597 = CARTESIAN_POINT('Ctrl Pts',(-18.5526336060153,-15.1560769586623,
122.562890931627)) ;
#109598 = CARTESIAN_POINT('Ctrl Pts',(-18.4177188484118,-15.1661236132381,
122.725376550707)) ;
#109599 = CARTESIAN_POINT('Ctrl Pts',(-18.3144558864749,-15.1760192078809,
122.906011128)) ;
#109600 = CARTESIAN_POINT('Ctrl Pts',(-18.2429422388871,-15.1860811545378,
123.10506462228)) ;
#109601 = CARTESIAN_POINT('Ctrl Pts',(-18.2077902938068,-15.19593077847,123.309140059312)) ;
#109602 = CARTESIAN_POINT('Ctrl Pts',(-18.2079234689505,-15.2058940174998,
123.518586344628)) ;
#109603 = CARTESIAN_POINT('Ctrl Pts',(-18.2449367997325,-15.2159185922756,
123.72607129154)) ;
#109604 = CARTESIAN_POINT('Ctrl Pts',(-18.3165154277315,-15.2258371549633,
123.921914349635)) ;
#109605 = CARTESIAN_POINT('Ctrl Pts',(-18.4214761496435,-15.2358293416873,
124.103894254705)) ;
#109606 = CARTESIAN_POINT('Ctrl Pts',(-18.5572936379027,-15.2458641402715,
124.265311511789)) ;
#109607 = CARTESIAN_POINT('Ctrl Pts',(-18.7159696842485,-15.2557193309452,
124.39855934559)) ;
#109608 = CARTESIAN_POINT('Ctrl Pts',(-18.8978107982486,-15.2657186790982,
124.503966261353)) ;
#109609 = CARTESIAN_POINT('Ctrl Pts',(-19.0931219941704,-15.2756138047733,
124.575680357032)) ;
#109610 = CARTESIAN_POINT('Ctrl Pts',(-19.301284967467,-15.2856743477214,
124.612973605937)) ;
#109611 = CARTESIAN_POINT('Ctrl Pts',(-19.5083624530517,-15.2955236219883,
124.613661374866)) ;
#109612 = CARTESIAN_POINT('Ctrl Pts',(-19.7161694212036,-15.3055508465582,
124.578275147989)) ;
#109613 = CARTESIAN_POINT('Ctrl Pts',(-19.9145290440196,-15.315579245746,
124.506811325148)) ;
#109614 = CARTESIAN_POINT('Ctrl Pts',(-20.0943037661105,-15.3254249961595,
124.404246523484)) ;
#109615 = CARTESIAN_POINT('Ctrl Pts',(-20.2562466963265,-15.3354137865603,
124.270541646777)) ;
#109616 = CARTESIAN_POINT('Ctrl Pts',(-20.3928604337104,-15.34545871496,124.109519099858)) ;
#109617 = CARTESIAN_POINT('Ctrl Pts',(-20.4975269072714,-15.3552831997489,
123.931448016533)) ;
#109618 = CARTESIAN_POINT('Ctrl Pts',(-20.5716719496347,-15.3653405972901,
123.733454645231)) ;
#109619 = CARTESIAN_POINT('Ctrl Pts',(-20.6095443605714,-15.3752666888763,
123.528227190291)) ;
#109620 = CARTESIAN_POINT('Ctrl Pts',(-20.6117538896396,-15.3852214740209,
123.318960224126)) ;
#109621 = CARTESIAN_POINT('Ctrl Pts',(-20.5770787989191,-15.3952588436785,
123.110812438723)) ;
#109622 = CARTESIAN_POINT('Ctrl Pts',(-20.5079786726466,-15.4051476538001,
122.914732712821)) ;
#109623 = CARTESIAN_POINT('Ctrl Pts',(-20.405177649876,-15.4151370128512,
122.731611771047)) ;
#109624 = CARTESIAN_POINT('Ctrl Pts',(-20.2724329769306,-15.4250955603073,
122.569723651607)) ;
#109625 = CARTESIAN_POINT('Ctrl Pts',(-20.1148565670666,-15.4349951368583,
122.433749523495)) ;
#109626 = CARTESIAN_POINT('Ctrl Pts',(-19.9333764119797,-15.445043048689,
122.325686463759)) ;
#109627 = CARTESIAN_POINT('Ctrl Pts',(-19.7388960303713,-15.4549383965496,
122.251741280354)) ;
#109628 = CARTESIAN_POINT('Ctrl Pts',(-19.5311562979992,-15.4650000730808,
122.212012300388)) ;
#109629 = CARTESIAN_POINT('Ctrl Pts',(-19.3242084203133,-15.4748445908299,
122.208989215033)) ;
#109630 = CARTESIAN_POINT('Ctrl Pts',(-19.117367979988,-15.4848050345447,
122.241595181987)) ;
#109631 = CARTESIAN_POINT('Ctrl Pts',(-18.9179393137022,-15.4948418673629,
122.310513546074)) ;
#109632 = CARTESIAN_POINT('Ctrl Pts',(-18.7362238394064,-15.5047206641097,
122.411112431195)) ;
#109633 = CARTESIAN_POINT('Ctrl Pts',(-18.5717749639837,-15.5147799802381,
122.544043445986)) ;
#109634 = CARTESIAN_POINT('Ctrl Pts',(-18.4354881036463,-15.5246504269913,
122.700537312276)) ;
#109635 = CARTESIAN_POINT('Ctrl Pts',(-18.3266377092423,-15.5346430652493,
122.880215394805)) ;
#109636 = CARTESIAN_POINT('Ctrl Pts',(-18.2507661865552,-15.5446750807973,
123.076992671836)) ;
#109637 = CARTESIAN_POINT('Ctrl Pts',(-18.21043784316,-15.5545409371038,123.28046627568)) ;
#109638 = CARTESIAN_POINT('Ctrl Pts',(-18.2059425079987,-15.564610226573,
123.492083404427)) ;
#109639 = CARTESIAN_POINT('Ctrl Pts',(-18.2375158608786,-15.5744537841243,
123.696615003604)) ;
#109640 = CARTESIAN_POINT('Ctrl Pts',(-18.3043904535385,-15.5844339109121,
123.89547847275)) ;
#109641 = CARTESIAN_POINT('Ctrl Pts',(-18.4055207883085,-15.594452459512,
124.080226249269)) ;
#109642 = CARTESIAN_POINT('Ctrl Pts',(-18.5350893882449,-15.6043357600352,
124.242688864533)) ;
#109643 = CARTESIAN_POINT('Ctrl Pts',(-18.693831401869,-15.6144040470834,
124.382650639135)) ;
#109644 = CARTESIAN_POINT('Ctrl Pts',(-18.8701228866772,-15.624234170102,
124.490558622862)) ;
#109645 = CARTESIAN_POINT('Ctrl Pts',(-19.0669347785616,-15.6343007540273,
124.568265952009)) ;
#109646 = CARTESIAN_POINT('Ctrl Pts',(-19.2706999932353,-15.6441908670418,
124.609767418512)) ;
#109647 = CARTESIAN_POINT('Ctrl Pts',(-19.4806745293458,-15.6541835558044,
124.615758781183)) ;
#109648 = CARTESIAN_POINT('Ctrl Pts',(-19.6878442224981,-15.6641444441602,
124.585148636479)) ;
#109649 = CARTESIAN_POINT('Ctrl Pts',(-19.8857864611817,-15.6740623890402,
124.519664701863)) ;
#109650 = CARTESIAN_POINT('Ctrl Pts',(-20.0711599418231,-15.6840701421364,
124.420109867317)) ;
#109651 = CARTESIAN_POINT('Ctrl Pts',(-20.2365270596388,-15.6941012360955,
124.289260695756)) ;
#109652 = CARTESIAN_POINT('Ctrl Pts',(-20.3744685474025,-15.7039492041234,
124.13485341131)) ;
#109653 = CARTESIAN_POINT('Ctrl Pts',(-20.4860139505825,-15.7140111602493,
123.955138461719)) ;
#109654 = CARTESIAN_POINT('Ctrl Pts',(-20.5632011545908,-15.7239083718504,
123.761905716471)) ;
#109655 = CARTESIAN_POINT('Ctrl Pts',(-20.6064813747011,-15.7338395385151,
123.55766057874)) ;
#109656 = CARTESIAN_POINT('Ctrl Pts',(-20.6134913371925,-15.7438817227192,
123.346661541518)) ;
#109657 = CARTESIAN_POINT('Ctrl Pts',(-20.584365940305,-15.7537683909724,
123.140853962353)) ;
#109658 = CARTESIAN_POINT('Ctrl Pts',(-20.5195954590546,-15.7637615029506,
122.941012421973)) ;
#109659 = CARTESIAN_POINT('Ctrl Pts',(-20.4215027390492,-15.7737071805665,
122.756360656231)) ;
#109660 = CARTESIAN_POINT('Ctrl Pts',(-20.293147873749,-15.7836544835514,
122.591249152608)) ;
#109661 = CARTESIAN_POINT('Ctrl Pts',(-20.1363629892381,-15.7937022072982,
122.449699021811)) ;
#109662 = CARTESIAN_POINT('Ctrl Pts',(-19.9610175850139,-15.8035505810607,
122.339609678665)) ;
#109663 = CARTESIAN_POINT('Ctrl Pts',(-19.7673272399029,-15.8135095535064,
122.260115101771)) ;
#109664 = CARTESIAN_POINT('Ctrl Pts',(-19.5610606250045,-15.8235484153876,
122.21547621934)) ;
#109665 = CARTESIAN_POINT('Ctrl Pts',(-19.3535277647716,-15.8334270195594,
122.207127938507)) ;
#109666 = CARTESIAN_POINT('Ctrl Pts',(-19.1441320257692,-15.8434785607627,
122.235331703317)) ;
#109667 = CARTESIAN_POINT('Ctrl Pts',(-18.9458603675138,-15.853373958743,
122.298425308939)) ;
#109668 = CARTESIAN_POINT('Ctrl Pts',(-18.7586572899383,-15.8634251912883,
122.396376389839)) ;
#109669 = CARTESIAN_POINT('Ctrl Pts',(-18.5939995653867,-15.8733113819126,
122.523238105459)) ;
#109670 = CARTESIAN_POINT('Ctrl Pts',(-18.4521054124113,-15.8833039212284,
122.678123503836)) ;
#109671 = CARTESIAN_POINT('Ctrl Pts',(-18.339797930543,-15.8932523671231,
122.854575553561)) ;
#109672 = CARTESIAN_POINT('Ctrl Pts',(-18.2596650284503,-15.903189169655,
123.047478343827)) ;
#109673 = CARTESIAN_POINT('Ctrl Pts',(-18.2137638368443,-15.9131721771063,
123.252299084448)) ;
#109674 = CARTESIAN_POINT('Ctrl Pts',(-18.2044549894889,-15.9232160185211,
123.463222876647)) ;
#109675 = CARTESIAN_POINT('Ctrl Pts',(-18.2308440132966,-15.933044217145,
123.668181783629)) ;
#109676 = CARTESIAN_POINT('Ctrl Pts',(-18.2938579700638,-15.9431208105873,
123.870388933677)) ;
#109677 = CARTESIAN_POINT('Ctrl Pts',(-18.3888049458856,-15.9529728099288,
124.05451547145)) ;
#109678 = CARTESIAN_POINT('Ctrl Pts',(-18.5169135938401,-15.9630463967527,
124.22310665089)) ;
#109679 = CARTESIAN_POINT('Ctrl Pts',(-18.6688147995286,-15.9728866218502,
124.363569489608)) ;
#109680 = CARTESIAN_POINT('Ctrl Pts',(-18.8445860569989,-15.9828523258788,
124.477551487822)) ;
#109681 = CARTESIAN_POINT('Ctrl Pts',(-19.03880433049,-15.9928789591854,124.559512208558)) ;
#109682 = CARTESIAN_POINT('Ctrl Pts',(-19.2419523507273,-16.0027932548972,
124.606112524962)) ;
#109683 = CARTESIAN_POINT('Ctrl Pts',(-19.4516578148718,-16.0127815435897,
124.617191579111)) ;
#109684 = CARTESIAN_POINT('Ctrl Pts',(-19.6610890758173,-16.022820276748,
124.591182852167)) ;
#109685 = CARTESIAN_POINT('Ctrl Pts',(-19.8590045265917,-16.0326636085756,
124.530744531439)) ;
#109686 = CARTESIAN_POINT('Ctrl Pts',(-20.0470963330464,-16.0426913344552,
124.435533965308)) ;
#109687 = CARTESIAN_POINT('Ctrl Pts',(-20.215536875697,-16.0527236708437,
124.308590608307)) ;
#109688 = CARTESIAN_POINT('Ctrl Pts',(-20.3567606119686,-16.0625531711444,
124.157747572652)) ;
#109689 = CARTESIAN_POINT('Ctrl Pts',(-20.4720239071908,-16.0725426750611,
123.982187731756)) ;
#109690 = CARTESIAN_POINT('Ctrl Pts',(-20.5550085516547,-16.0825865155735,
123.788026918096)) ;
#109691 = CARTESIAN_POINT('Ctrl Pts',(-20.6023748873939,-16.0924082213416,
123.587050657339)) ;
#109692 = CARTESIAN_POINT('Ctrl Pts',(-20.6148970318561,-16.102443268474,
123.376455155403)) ;
#109693 = CARTESIAN_POINT('Ctrl Pts',(-20.5901081076604,-16.1124679459109,
123.167160158255)) ;
#109694 = CARTESIAN_POINT('Ctrl Pts',(-20.530818219645,-16.1223207607653,
122.968690528632)) ;
#109695 = CARTESIAN_POINT('Ctrl Pts',(-20.4370333070013,-16.1323084703729,
122.780843369881)) ;
#109696 = CARTESIAN_POINT('Ctrl Pts',(-20.312772898458,-16.1422384803669,
122.613084101585)) ;
#109697 = CARTESIAN_POINT('Ctrl Pts',(-20.1605853193158,-16.1522282355861,
122.468351969424)) ;
#109698 = CARTESIAN_POINT('Ctrl Pts',(-19.9847834588494,-16.162254844269,
122.352041821434)) ;
#109699 = CARTESIAN_POINT('Ctrl Pts',(-19.7942943177276,-16.1721387842908,
122.269038890483)) ;
#109700 = CARTESIAN_POINT('Ctrl Pts',(-19.5902387741109,-16.1821280118293,
122.219375677544)) ;
#109701 = CARTESIAN_POINT('Ctrl Pts',(-19.3795149808787,-16.192170882353,
122.206262663968)) ;
#109702 = CARTESIAN_POINT('Ctrl Pts',(-19.1740770402837,-16.2020032691084,
122.229113777203)) ;
#109703 = CARTESIAN_POINT('Ctrl Pts',(-18.9723117812923,-16.21199656228,122.287656027766)) ;
#109704 = CARTESIAN_POINT('Ctrl Pts',(-18.7832283026932,-16.2220285679285,
122.381103263292)) ;
#109705 = CARTESIAN_POINT('Ctrl Pts',(-18.6159331201159,-16.2318938238974,
122.503667595544)) ;
#109706 = CARTESIAN_POINT('Ctrl Pts',(-18.4706150949567,-16.2418557038049,
122.654486124673)) ;
#109707 = CARTESIAN_POINT('Ctrl Pts',(-18.3531300321575,-16.2518906371668,
122.829697635981)) ;
#109708 = CARTESIAN_POINT('Ctrl Pts',(-18.268789814556,-16.2617755955461,
123.01965860588)) ;
#109709 = CARTESIAN_POINT('Ctrl Pts',(-18.21786016684,-16.2718412224688,123.225013794551)) ;
#109710 = CARTESIAN_POINT('Ctrl Pts',(-18.2034722692019,-16.2816803281331,
123.431395580838)) ;
#109711 = CARTESIAN_POINT('Ctrl Pts',(-18.2253430575851,-16.2917431431385,
123.641785442518)) ;
#109712 = CARTESIAN_POINT('Ctrl Pts',(-18.2826479362205,-16.3016393491872,
123.841809756648)) ;
#109713 = CARTESIAN_POINT('Ctrl Pts',(-18.3736809587007,-16.3115801722124,
124.029901937627)) ;
#109714 = CARTESIAN_POINT('Ctrl Pts',(-18.4967610913104,-16.3215847551911,
124.200486445331)) ;
#109715 = CARTESIAN_POINT('Ctrl Pts',(-18.6479949929191,-16.3316056496358,
124.347144067133)) ;
#109716 = CARTESIAN_POINT('Ctrl Pts',(-18.8200146134422,-16.3414975702252,
124.464013893667)) ;
#109717 = CARTESIAN_POINT('Ctrl Pts',(-19.0115256420876,-16.3514910025706,
124.550383163772)) ;
#109718 = CARTESIAN_POINT('Ctrl Pts',(-19.2141727649583,-16.3614366074705,
124.601876515713)) ;
#109719 = CARTESIAN_POINT('Ctrl Pts',(-19.4226977962018,-16.371383880952,
124.617828957429)) ;
#109720 = CARTESIAN_POINT('Ctrl Pts',(-19.6328892761154,-16.3814317954284,
124.596890598634)) ;
#109721 = CARTESIAN_POINT('Ctrl Pts',(-19.8322548104562,-16.3912794357757,
124.541079249358)) ;
#109722 = CARTESIAN_POINT('Ctrl Pts',(-20.021336048831,-16.4012411511523,
124.451058494016)) ;
#109723 = CARTESIAN_POINT('Ctrl Pts',(-20.1929241151113,-16.4112697747251,
124.328527644872)) ;
#109724 = CARTESIAN_POINT('Ctrl Pts',(-20.3389201939629,-16.4211801367915,
124.179902253825)) ;
#109725 = CARTESIAN_POINT('Ctrl Pts',(-20.4576462994869,-16.4311148304439,
124.00806090734)) ;
#109726 = CARTESIAN_POINT('Ctrl Pts',(-20.5454725666168,-16.4411566735718,
123.816097292323)) ;
#109727 = CARTESIAN_POINT('Ctrl Pts',(-20.5979873013168,-16.4510411791422,
123.615017248029)) ;
#109728 = CARTESIAN_POINT('Ctrl Pts',(-20.6152306651731,-16.4610432829274,
123.405480440774)) ;
#109729 = CARTESIAN_POINT('Ctrl Pts',(-20.5961578299073,-16.4709616343424,
123.197804681328)) ;
#109730 = CARTESIAN_POINT('Ctrl Pts',(-20.5405653157238,-16.4810092903633,
122.994052111286)) ;
#109731 = CARTESIAN_POINT('Ctrl Pts',(-20.4522004741177,-16.4908804833915,
122.806233780895)) ;
#109732 = CARTESIAN_POINT('Ctrl Pts',(-20.330289868064,-16.500946196535,122.633325395461)) ;
#109733 = CARTESIAN_POINT('Ctrl Pts',(-20.1834850003555,-16.5107986571077,
122.487125747477)) ;
#109734 = CARTESIAN_POINT('Ctrl Pts',(-19.9518929518622,-16.5242271198303,
122.325807099789)) ;
#109735 = CARTESIAN_POINT('Ctrl Pts',(-19.6903720511171,-16.5373080673473,
122.23069883505)) ;
#109736 = CARTESIAN_POINT('Ctrl Pts',(-19.4083019160809,-16.5507825655819,
122.20577313946)) ;
#109737 = CARTESIAN_POINT('Ctrl Pts',(-19.2023528996714,-16.5606146691914,
122.22388710309)) ;
#109738 = CARTESIAN_POINT('Ctrl Pts',(-18.9998124510311,-16.570580572318,
122.277379757565)) ;
#109739 = CARTESIAN_POINT('Ctrl Pts',(-18.8085486716716,-16.5806079816283,
122.366089498496)) ;
#109740 = CARTESIAN_POINT('Ctrl Pts',(-18.6376144382237,-16.5905190129948,
122.485181013786)) ;
#109741 = CARTESIAN_POINT('Ctrl Pts',(-18.4395800595996,-16.6037633206159,
122.681031779891)) ;
#109742 = CARTESIAN_POINT('Ctrl Pts',(-18.2607391091555,-16.620463803287,
122.987662510097)) ;
#109743 = CARTESIAN_POINT('Ctrl Pts',(-18.1977926181829,-16.6369706324428,
123.333078302726)) ;
#109744 = CARTESIAN_POINT('Ctrl Pts',(-18.2199698947145,-16.6502812606804,
123.611945037936)) ;
#109745 = CARTESIAN_POINT('Ctrl Pts',(-18.2726905127628,-16.6602738242205,
123.815342227813)) ;
#109746 = CARTESIAN_POINT('Ctrl Pts',(-18.3604559850895,-16.6703039072221,
124.00703819638)) ;
#109747 = CARTESIAN_POINT('Ctrl Pts',(-18.5172871477933,-16.6834775112198,
124.235392726718)) ;
#109748 = CARTESIAN_POINT('Ctrl Pts',(-18.785768928342,-16.7001152164512,
124.465519466713)) ;
#109749 = CARTESIAN_POINT('Ctrl Pts',(-19.1813867892304,-16.7199969790187,
124.614927194957)) ;
#109750 = CARTESIAN_POINT('Ctrl Pts',(-19.5363104610225,-16.7366933312352,
124.619236231308)) ;
#109751 = CARTESIAN_POINT('Ctrl Pts',(-19.804422300902,-16.7498503590243,
124.551190202698)) ;
#109752 = CARTESIAN_POINT('Ctrl Pts',(-20.0610845707717,-16.7632277136678,
124.436239275609)) ;
#109753 = CARTESIAN_POINT('Ctrl Pts',(-20.3337551615359,-16.7797585479266,
124.214393619657)) ;
#109754 = CARTESIAN_POINT('Ctrl Pts',(-20.552444510262,-16.7997232376697,
123.850597100039)) ;
#109755 = CARTESIAN_POINT('Ctrl Pts',(-20.6332803508242,-16.8196397310933,
123.434897045989)) ;
#109756 = CARTESIAN_POINT('Ctrl Pts',(-20.5683255306972,-16.8395294504429,
123.016962646405)) ;
#109757 = CARTESIAN_POINT('Ctrl Pts',(-20.3632005830819,-16.8595361800907,
122.644358668796)) ;
#109758 = CARTESIAN_POINT('Ctrl Pts',(-20.0460339159118,-16.8793742337376,
122.36614334468)) ;
#109759 = CARTESIAN_POINT('Ctrl Pts',(-19.6502010050201,-16.8993675719512,
122.211319428287)) ;
#109760 = CARTESIAN_POINT('Ctrl Pts',(-19.2274810542746,-16.9192503713578,
122.201182930586)) ;
#109761 = CARTESIAN_POINT('Ctrl Pts',(-18.8264482555766,-16.9391425522766,
122.335224690758)) ;
#109762 = CARTESIAN_POINT('Ctrl Pts',(-18.494427148148,-16.9590447307716,
122.597799365927)) ;
#109763 = CARTESIAN_POINT('Ctrl Pts',(-18.2711836802026,-16.9790820419754,
122.960542078026)) ;
#109764 = CARTESIAN_POINT('Ctrl Pts',(-18.1854522350004,-16.9988944835162,
123.373183055826)) ;
#109765 = CARTESIAN_POINT('Ctrl Pts',(-18.2465250718034,-17.0189597242511,
123.79522378749)) ;
#109766 = CARTESIAN_POINT('Ctrl Pts',(-18.4447588957949,-17.038716929107,
124.165833804144)) ;
#109767 = CARTESIAN_POINT('Ctrl Pts',(-18.7611994425061,-17.0587502017527,
124.450659047111)) ;
#109768 = CARTESIAN_POINT('Ctrl Pts',(-19.1518956101868,-17.0785631102065,
124.608746114223)) ;
#109769 = CARTESIAN_POINT('Ctrl Pts',(-19.576578104548,-17.0985592563339,
124.624711052112)) ;
#109770 = CARTESIAN_POINT('Ctrl Pts',(-19.9789206558073,-17.1184210095564,
124.495756780167)) ;
#109771 = CARTESIAN_POINT('Ctrl Pts',(-20.3161959933635,-17.1384895266845,
124.234517323645)) ;
#109772 = CARTESIAN_POINT('Ctrl Pts',(-20.5412459928412,-17.1583203996814,
123.877828498823)) ;
#109773 = CARTESIAN_POINT('Ctrl Pts',(-20.6325581588657,-17.178242310498,
123.46429421579)) ;
#109774 = CARTESIAN_POINT('Ctrl Pts',(-20.5771055559046,-17.1981717539333,
123.044114310957)) ;
#109775 = CARTESIAN_POINT('Ctrl Pts',(-20.3819897667865,-17.2180814240497,
122.66849870212)) ;
#109776 = CARTESIAN_POINT('Ctrl Pts',(-20.0714042523442,-17.2379547813126,
122.381902337516)) ;
#109777 = CARTESIAN_POINT('Ctrl Pts',(-19.6794131236805,-17.2579463159305,
122.217639339943)) ;
#109778 = CARTESIAN_POINT('Ctrl Pts',(-19.2574582496179,-17.2778119333413,
122.196951656448)) ;
#109779 = CARTESIAN_POINT('Ctrl Pts',(-18.851381119533,-17.2977928631695,
122.321792161299)) ;
#109780 = CARTESIAN_POINT('Ctrl Pts',(-18.5132667997909,-17.3177313252526,
122.577558583777)) ;
#109781 = CARTESIAN_POINT('Ctrl Pts',(-18.2826875736514,-17.3376235184743,
122.932201676895)) ;
#109782 = CARTESIAN_POINT('Ctrl Pts',(-18.1868226115156,-17.3575942335097,
123.345774563987)) ;
#109783 = CARTESIAN_POINT('Ctrl Pts',(-18.2367369984319,-17.3774039051758,
123.764115337837)) ;
#109784 = CARTESIAN_POINT('Ctrl Pts',(-18.4277722770693,-17.397397121867,
124.143708004475)) ;
#109785 = CARTESIAN_POINT('Ctrl Pts',(-18.734673676871,-17.4172480340634,
124.433730342498)) ;
#109786 = CARTESIAN_POINT('Ctrl Pts',(-19.1263242402619,-17.4373226403824,
124.603166614917)) ;
#109787 = CARTESIAN_POINT('Ctrl Pts',(-19.4769995887317,-17.4538392722657,
124.624023090722)) ;
#109788 = CARTESIAN_POINT('Ctrl Pts',(-19.7517472064442,-17.4671779799598,
124.568109819516)) ;
#109789 = CARTESIAN_POINT('Ctrl Pts',(-19.9444114368832,-17.4770203542681,
124.492567950153)) ;
#109790 = CARTESIAN_POINT('Ctrl Pts',(-20.1249106079122,-17.4870753742509,
124.382584061632)) ;
#109791 = CARTESIAN_POINT('Ctrl Pts',(-20.333714948593,-17.5003075309084,
124.198802225224)) ;
#109792 = CARTESIAN_POINT('Ctrl Pts',(-20.5299811986958,-17.5169224982536,
123.905006518527)) ;
#109793 = CARTESIAN_POINT('Ctrl Pts',(-20.6139220428232,-17.5335170852648,
123.562354960311)) ;
#109794 = CARTESIAN_POINT('Ctrl Pts',(-20.6085090189388,-17.5467506536201,
123.284145259763)) ;
#109795 = CARTESIAN_POINT('Ctrl Pts',(-20.5678477264908,-17.5567942714288,
123.076973055526)) ;
#109796 = CARTESIAN_POINT('Ctrl Pts',(-20.4930714529787,-17.5666811956636,
122.883014189482)) ;
#109797 = CARTESIAN_POINT('Ctrl Pts',(-20.3849668052257,-17.5766718501104,
122.702955328018)) ;
#109798 = CARTESIAN_POINT('Ctrl Pts',(-20.2475870389124,-17.5866336085644,
122.544870559864)) ;
#109799 = CARTESIAN_POINT('Ctrl Pts',(-20.0298559708887,-17.5999734736316,
122.368098973395)) ;
#109800 = CARTESIAN_POINT('Ctrl Pts',(-19.7713314498364,-17.6132822565449,
122.253061517512)) ;
#109801 = CARTESIAN_POINT('Ctrl Pts',(-19.4973909934278,-17.626478013989,
122.209165833035)) ;
#109802 = CARTESIAN_POINT('Ctrl Pts',(-19.2879780154188,-17.6364398976655,
122.211856720957)) ;
#109803 = CARTESIAN_POINT('Ctrl Pts',(-19.0806022855442,-17.6464830071801,
122.251525005738)) ;
#109804 = CARTESIAN_POINT('Ctrl Pts',(-18.8869188738672,-17.6563352571794,
122.324944171028)) ;
#109805 = CARTESIAN_POINT('Ctrl Pts',(-18.7065327529303,-17.6663067941298,
122.43170197551)) ;
#109806 = CARTESIAN_POINT('Ctrl Pts',(-18.5470138305895,-17.6763020596074,
122.56853355476)) ;
#109807 = CARTESIAN_POINT('Ctrl Pts',(-18.4133926360928,-17.686336032481,
122.73173870635)) ;
#109808 = CARTESIAN_POINT('Ctrl Pts',(-18.3116707785593,-17.6961914472433,
122.912264154203)) ;
#109809 = CARTESIAN_POINT('Ctrl Pts',(-18.2415826929153,-17.7061907247522,
123.110414104041)) ;
#109810 = CARTESIAN_POINT('Ctrl Pts',(-18.2070923132308,-17.7160859089151,
123.315598967219)) ;
#109811 = CARTESIAN_POINT('Ctrl Pts',(-18.2088036935271,-17.7261462885559,
123.527064333547)) ;
#109812 = CARTESIAN_POINT('Ctrl Pts',(-18.2462864758189,-17.735996157564,
123.730739677823)) ;
#109813 = CARTESIAN_POINT('Ctrl Pts',(-18.3194342459221,-17.7460277187719,
123.928528752531)) ;
#109814 = CARTESIAN_POINT('Ctrl Pts',(-18.4259724257454,-17.7560381676542,
124.110043085157)) ;
#109815 = CARTESIAN_POINT('Ctrl Pts',(-18.560803472063,-17.7659449070712,
124.268770678852)) ;
#109816 = CARTESIAN_POINT('Ctrl Pts',(-18.7213893175962,-17.7758829231397,
124.40240536805)) ;
#109817 = CARTESIAN_POINT('Ctrl Pts',(-18.9039272751764,-17.7858881695908,
124.506966406098)) ;
#109818 = CARTESIAN_POINT('Ctrl Pts',(-19.1025083345875,-17.7959222306471,
124.578100107171)) ;
#109819 = CARTESIAN_POINT('Ctrl Pts',(-19.3064701319047,-17.8057673117052,
124.613359511751)) ;
#109820 = CARTESIAN_POINT('Ctrl Pts',(-19.5163698561987,-17.8157531176587,
124.613051491082)) ;
#109821 = CARTESIAN_POINT('Ctrl Pts',(-19.7220693123888,-17.8256879382129,
124.576625318593)) ;
#109822 = CARTESIAN_POINT('Ctrl Pts',(-19.9206135227075,-17.8357454633451,
124.503998222477)) ;
#109823 = CARTESIAN_POINT('Ctrl Pts',(-20.0994449015553,-17.8455671139965,
124.400734677242)) ;
#109824 = CARTESIAN_POINT('Ctrl Pts',(-20.2616284131143,-17.8556231775012,
124.265148632997)) ;
#109825 = CARTESIAN_POINT('Ctrl Pts',(-20.3959713587119,-17.8655638445652,
124.105055282078)) ;
#109826 = CARTESIAN_POINT('Ctrl Pts',(-20.5006583406591,-17.8754682382312,
123.925059620168)) ;
#109827 = CARTESIAN_POINT('Ctrl Pts',(-20.5733969612248,-17.8855147619942,
123.726790717913)) ;
#109828 = CARTESIAN_POINT('Ctrl Pts',(-20.6102547689637,-17.8954108450105,
123.521996956588)) ;
#109829 = CARTESIAN_POINT('Ctrl Pts',(-20.6109546878426,-17.9054775442406,
123.310402217638)) ;
#109830 = CARTESIAN_POINT('Ctrl Pts',(-20.5759989907447,-17.9153011546416,
123.106826896567)) ;
#109831 = CARTESIAN_POINT('Ctrl Pts',(-20.5049473013342,-17.9253570148191,
122.907747148049)) ;
#109832 = CARTESIAN_POINT('Ctrl Pts',(-20.401424074172,-17.9352901611241,
122.726358499416)) ;
#109833 = CARTESIAN_POINT('Ctrl Pts',(-20.2681766257186,-17.9452354168947,
122.565269682228)) ;
#109834 = CARTESIAN_POINT('Ctrl Pts',(-20.108444657178,-17.9552187153331,
122.429084134722)) ;
#109835 = CARTESIAN_POINT('Ctrl Pts',(-19.9264068310443,-17.9652558954798,
122.322397286291)) ;
#109836 = CARTESIAN_POINT('Ctrl Pts',(-19.7322883144763,-17.9751104481892,
122.249961687769)) ;
#109837 = CARTESIAN_POINT('Ctrl Pts',(-19.5256522418297,-17.9851099666366,
122.211500201786)) ;
#109838 = CARTESIAN_POINT('Ctrl Pts',(-19.31760333372,-17.9950050490986,122.209300818148)) ;
#109839 = CARTESIAN_POINT('Ctrl Pts',(-19.1089652472923,-18.0050655946047,
122.243837242944)) ;
#109840 = CARTESIAN_POINT('Ctrl Pts',(-18.9136030264272,-18.0149149018527,
122.312505382335)) ;
#109841 = CARTESIAN_POINT('Ctrl Pts',(-18.7296291464669,-18.0249419919401,
122.41540712287)) ;
#109842 = CARTESIAN_POINT('Ctrl Pts',(-18.5666314649229,-18.034970896077,
122.549156073621)) ;
#109843 = CARTESIAN_POINT('Ctrl Pts',(-18.4315663761752,-18.0448147611763,
122.705941987549)) ;
#109844 = CARTESIAN_POINT('Ctrl Pts',(-18.3236932692591,-18.0548105878847,
122.886285402256)) ;
#109845 = CARTESIAN_POINT('Ctrl Pts',(-18.2489130679187,-18.0648358045337,
123.083339159257)) ;
#109846 = CARTESIAN_POINT('Ctrl Pts',(-18.209741487676,-18.0747256366913,
123.287534557043)) ;
#109847 = CARTESIAN_POINT('Ctrl Pts',(-18.2063008109459,-18.0847164927761,
123.497538629128)) ;
#109848 = CARTESIAN_POINT('Ctrl Pts',(-18.2392644666018,-18.0946615873689,
123.704000402072)) ;
#109849 = CARTESIAN_POINT('Ctrl Pts',(-18.3072547434837,-18.104613491137,
123.901873659629)) ;
#109850 = CARTESIAN_POINT('Ctrl Pts',(-18.4095849077262,-18.1146498906065,
124.086389068294)) ;
#109851 = CARTESIAN_POINT('Ctrl Pts',(-18.5403379264193,-18.1245389606951,
124.248032485405)) ;
#109852 = CARTESIAN_POINT('Ctrl Pts',(-18.6985038062607,-18.134528250066,
124.386177725035)) ;
#109853 = CARTESIAN_POINT('Ctrl Pts',(-18.8777803549785,-18.1444868162757,
124.494293549754)) ;
#109854 = CARTESIAN_POINT('Ctrl Pts',(-19.0717815031303,-18.1543863874925,
124.569677868707)) ;
#109855 = CARTESIAN_POINT('Ctrl Pts',(-19.2789648452525,-18.1644343019068,
124.610759938649)) ;
#109856 = CARTESIAN_POINT('Ctrl Pts',(-19.4869781861118,-18.1743296447674,
124.615340835286)) ;
#109857 = CARTESIAN_POINT('Ctrl Pts',(-19.6960324373929,-18.1843913387148,
124.583240349093)) ;
#109858 = CARTESIAN_POINT('Ctrl Pts',(-19.8920550329424,-18.194235791799,
124.516818987295)) ;
#109859 = CARTESIAN_POINT('Ctrl Pts',(-20.0760459040153,-18.2041964767574,
124.416850431597)) ;
#109860 = CARTESIAN_POINT('Ctrl Pts',(-20.2409137177354,-18.2142324092659,
124.285180340434)) ;
#109861 = CARTESIAN_POINT('Ctrl Pts',(-20.3785155657472,-18.224121024954,
124.129353411916)) ;
#109862 = CARTESIAN_POINT('Ctrl Pts',(-20.4887176363811,-18.2341354340964,
123.949948003391)) ;
#109863 = CARTESIAN_POINT('Ctrl Pts',(-20.5657247935329,-18.2441692430542,
123.753577916827)) ;
#109864 = CARTESIAN_POINT('Ctrl Pts',(-20.6071923944832,-18.2539996973104,
123.551089226015)) ;
#109865 = CARTESIAN_POINT('Ctrl Pts',(-20.6130809594151,-18.2640773648886,
123.339347426672)) ;
#109866 = CARTESIAN_POINT('Ctrl Pts',(-20.582902766514,-18.2739292330109,
123.134395564541)) ;
#109867 = CARTESIAN_POINT('Ctrl Pts',(-20.5163228220205,-18.2840022705762,
122.933405280998)) ;
#109868 = CARTESIAN_POINT('Ctrl Pts',(-20.4181024846832,-18.2938448239271,
122.75126135266)) ;
#109869 = CARTESIAN_POINT('Ctrl Pts',(-20.2885210943149,-18.3038252194205,
122.586249239326)) ;
#109870 = CARTESIAN_POINT('Ctrl Pts',(-20.1313832651528,-18.3138436973983,
122.446011951459)) ;
#109871 = CARTESIAN_POINT('Ctrl Pts',(-19.9549078155107,-18.3237270117044,
122.336291529541)) ;
#109872 = CARTESIAN_POINT('Ctrl Pts',(-19.7584730390354,-18.3337953142431,
122.257540027093)) ;
#109873 = CARTESIAN_POINT('Ctrl Pts',(-19.5562323023717,-18.3436253615166,
122.214866324967)) ;
#109874 = CARTESIAN_POINT('Ctrl Pts',(-19.3447577383104,-18.3536922329321,
122.20752427073)) ;
#109875 = CARTESIAN_POINT('Ctrl Pts',(-19.1388736768093,-18.3635812717311,
122.236610942261)) ;
#109876 = CARTESIAN_POINT('Ctrl Pts',(-18.9389373187673,-18.3735779698652,
122.301297559938)) ;
#109877 = CARTESIAN_POINT('Ctrl Pts',(-18.7541016364828,-18.3835303955772,
122.399376140261)) ;
#109878 = CARTESIAN_POINT('Ctrl Pts',(-18.5891329929658,-18.3934716978101,
122.527667417873)) ;
#109879 = CARTESIAN_POINT('Ctrl Pts',(-18.4481604349202,-18.4034549368941,
122.683186416303)) ;
#109880 = CARTESIAN_POINT('Ctrl Pts',(-18.3360106589202,-18.4134937384627,
122.861948238004)) ;
#109881 = CARTESIAN_POINT('Ctrl Pts',(-18.2577237798474,-18.4233418445843,
123.053634390363)) ;
#109882 = CARTESIAN_POINT('Ctrl Pts',(-18.2127798020352,-18.4334020401596,
123.260283053906)) ;
#109883 = CARTESIAN_POINT('Ctrl Pts',(-18.2047236219182,-18.4432997234711,
123.468215778861)) ;
#109884 = CARTESIAN_POINT('Ctrl Pts',(-18.2323081943826,-18.453230763845,
123.675163328835)) ;
#109885 = CARTESIAN_POINT('Ctrl Pts',(-18.2963305021331,-18.4632729815016,
123.876337724394)) ;
#109886 = CARTESIAN_POINT('Ctrl Pts',(-18.3926661921207,-18.4731596422356,
124.060523572342)) ;
#109887 = CARTESIAN_POINT('Ctrl Pts',(-18.5205934832174,-18.4831527508381,
124.227156275565)) ;
#109888 = CARTESIAN_POINT('Ctrl Pts',(-18.6748368398283,-18.4930984494763,
124.368321231404)) ;
#109889 = CARTESIAN_POINT('Ctrl Pts',(-18.8510537948634,-18.5030456717474,
124.480943969705)) ;
#109890 = CARTESIAN_POINT('Ctrl Pts',(-19.0461817391406,-18.5130936973275,
124.561846130438)) ;
#109891 = CARTESIAN_POINT('Ctrl Pts',(-19.2482396916346,-18.5229409444704,
124.60689682058)) ;
#109892 = CARTESIAN_POINT('Ctrl Pts',(-19.4574511064627,-18.5329041215612,
124.616949966226)) ;
#109893 = CARTESIAN_POINT('Ctrl Pts',(-19.6665802013189,-18.5429338425946,
124.590031811997)) ;
#109894 = CARTESIAN_POINT('Ctrl Pts',(-19.8654406918519,-18.5528383101275,
124.528232716691)) ;
#109895 = CARTESIAN_POINT('Ctrl Pts',(-20.0527877442865,-18.5628627959572,
124.431771240858)) ;
#109896 = CARTESIAN_POINT('Ctrl Pts',(-20.2186677362007,-18.5727666310811,
124.305885701411)) ;
#109897 = CARTESIAN_POINT('Ctrl Pts',(-20.3622738910286,-18.5828178217911,
124.150907477487)) ;
#109898 = CARTESIAN_POINT('Ctrl Pts',(-20.4749460893355,-18.5927022644494,
123.976278874356)) ;
#109899 = CARTESIAN_POINT('Ctrl Pts',(-20.5568157573217,-18.6026952723013,
123.782823463623)) ;
#109900 = CARTESIAN_POINT('Ctrl Pts',(-20.6035788944032,-18.6126435920176,
123.578959670149)) ;
#109901 = CARTESIAN_POINT('Ctrl Pts',(-20.6145188719353,-18.622580430727,
123.370361143146)) ;
#109902 = CARTESIAN_POINT('Ctrl Pts',(-20.5892122371831,-18.6325634196466,
123.161991400775)) ;
#109903 = CARTESIAN_POINT('Ctrl Pts',(-20.5273804714218,-18.6426072990107,
122.960118989388)) ;
#109904 = CARTESIAN_POINT('Ctrl Pts',(-20.4339102063426,-18.6524353643691,
122.775817017754)) ;
#109905 = CARTESIAN_POINT('Ctrl Pts',(-20.3068358770649,-18.6625124529241,
122.606366164904)) ;
#109906 = CARTESIAN_POINT('Ctrl Pts',(-20.1557713412269,-18.6723626050803,
122.464647202051)) ;
#109907 = CARTESIAN_POINT('Ctrl Pts',(-19.9784770985486,-18.6824430855327,
122.348647963324)) ;
#109908 = CARTESIAN_POINT('Ctrl Pts',(-19.788854501275,-18.6922575833015,
122.267192158884)) ;
#109909 = CARTESIAN_POINT('Ctrl Pts',(-19.5829445565809,-18.7023258793217,
122.218373128635)) ;
#109910 = CARTESIAN_POINT('Ctrl Pts',(-19.3751375244403,-18.7122247118044,
122.206308010974)) ;
#109911 = CARTESIAN_POINT('Ctrl Pts',(-19.165261647951,-18.722277591819,122.2308020183)) ;
#109912 = CARTESIAN_POINT('Ctrl Pts',(-18.9663763634325,-18.7321474073151,
122.290099661692)) ;
#109913 = CARTESIAN_POINT('Ctrl Pts',(-18.7770383472959,-18.7422200883979,
122.384851804193)) ;
#109914 = CARTESIAN_POINT('Ctrl Pts',(-18.6109895857822,-18.7520525669689,
122.507998056999)) ;
#109915 = CARTESIAN_POINT('Ctrl Pts',(-18.4655594817358,-18.762083200955,
122.660691091284)) ;
#109916 = CARTESIAN_POINT('Ctrl Pts',(-18.3493434065967,-18.7721147581741,
122.836690045224)) ;
#109917 = CARTESIAN_POINT('Ctrl Pts',(-18.2667541362467,-18.7819444670458,
123.026104585291)) ;
#109918 = CARTESIAN_POINT('Ctrl Pts',(-18.2169066002216,-18.7919339158479,
123.230119006716)) ;
#109919 = CARTESIAN_POINT('Ctrl Pts',(-18.2037005080579,-18.801977768248,
123.440856989541)) ;
#109920 = CARTESIAN_POINT('Ctrl Pts',(-18.2263400136645,-18.81179948158,123.646094755983)) ;
#109921 = CARTESIAN_POINT('Ctrl Pts',(-18.2850324744184,-18.8218344865687,
123.848732778897)) ;
#109922 = CARTESIAN_POINT('Ctrl Pts',(-18.3784519371622,-18.8318593250163,
124.037658528342)) ;
#109923 = CARTESIAN_POINT('Ctrl Pts',(-18.5007451800902,-18.8417115379715,
124.20482578886)) ;
#109924 = CARTESIAN_POINT('Ctrl Pts',(-18.6520376500026,-18.8517014941653,
124.350470469228)) ;
#109925 = CARTESIAN_POINT('Ctrl Pts',(-18.8252508888394,-18.8616296044486,
124.466935240053)) ;
#109926 = CARTESIAN_POINT('Ctrl Pts',(-19.0170807321666,-18.8716182045281,
124.552376204875)) ;
#109927 = CARTESIAN_POINT('Ctrl Pts',(-19.2216757039211,-18.8816447964556,
124.603121645647)) ;
#109928 = CARTESIAN_POINT('Ctrl Pts',(-19.4289827201006,-18.8915299245198,
124.617585298166)) ;
#109929 = CARTESIAN_POINT('Ctrl Pts',(-19.6379309761058,-18.9015210419933,
124.596074976164)) ;
#109930 = CARTESIAN_POINT('Ctrl Pts',(-19.8408408659986,-18.9115616578451,
124.537900613941)) ;
#109931 = CARTESIAN_POINT('Ctrl Pts',(-20.0267914773591,-18.9213946486988,
124.447599732227)) ;
#109932 = CARTESIAN_POINT('Ctrl Pts',(-20.1973182339844,-18.9313877801491,
124.324897683907)) ;
#109933 = CARTESIAN_POINT('Ctrl Pts',(-20.3442152864121,-18.9414198285845,
124.173548748272)) ;
#109934 = CARTESIAN_POINT('Ctrl Pts',(-20.460833320421,-18.9512850751269,
124.002055699851)) ;
#109935 = CARTESIAN_POINT('Ctrl Pts',(-20.5472848658807,-18.9612469499537,
123.811294918023)) ;
#109936 = CARTESIAN_POINT('Ctrl Pts',(-20.5993432778741,-18.971281913065,
123.606864315382)) ;
#109937 = CARTESIAN_POINT('Ctrl Pts',(-20.6152338874665,-18.9811667575274,
123.399631875823)) ;
#109938 = CARTESIAN_POINT('Ctrl Pts',(-20.5944804096342,-18.9912328103682,
123.189068842797)) ;
#109939 = CARTESIAN_POINT('Ctrl Pts',(-20.5389790659131,-19.0010703262771,
122.989799966108)) ;
#109940 = CARTESIAN_POINT('Ctrl Pts',(-20.4478587662562,-19.011139074386,
122.79877977841)) ;
#109941 = CARTESIAN_POINT('Ctrl Pts',(-20.3271508490702,-19.021019591417,
122.629693356427)) ;
#109942 = CARTESIAN_POINT('Ctrl Pts',(-20.1776005214533,-19.0310107783515,
122.482244401453)) ;
#109943 = CARTESIAN_POINT('Ctrl Pts',(-20.0053468791113,-19.0409638446264,
122.363394238246)) ;
#109944 = CARTESIAN_POINT('Ctrl Pts',(-19.8135070594326,-19.050999682159,
122.275616756344)) ;
#109945 = CARTESIAN_POINT('Ctrl Pts',(-19.6123108142453,-19.0608898083705,
122.223108777758)) ;
#109946 = CARTESIAN_POINT('Ctrl Pts',(-19.4029666575183,-19.0708819902784,
122.205825287622)) ;
#109947 = CARTESIAN_POINT('Ctrl Pts',(-19.1947651029536,-19.080827930217,
122.225135235062)) ;
#109948 = CARTESIAN_POINT('Ctrl Pts',(-18.9929315166685,-19.0907751139811,
122.279902905228)) ;
#109949 = CARTESIAN_POINT('Ctrl Pts',(-18.8018734248919,-19.1008230522886,
122.369991207827)) ;
#109950 = CARTESIAN_POINT('Ctrl Pts',(-18.6326906003464,-19.1106706870288,
122.489316995885)) ;
#109951 = CARTESIAN_POINT('Ctrl Pts',(-18.4846495676106,-19.1206324010027,
122.637436213505)) ;
#109952 = CARTESIAN_POINT('Ctrl Pts',(-18.3639748817887,-19.1306610357935,
122.810334905789)) ;
#109953 = CARTESIAN_POINT('Ctrl Pts',(-18.2761502313581,-19.1405713543906,
122.999255258084)) ;
#109954 = CARTESIAN_POINT('Ctrl Pts',(-18.221794679452,-19.1505062107021,
123.200928384173)) ;
#109955 = CARTESIAN_POINT('Ctrl Pts',(-18.2032878691283,-19.1605474466628,
123.411204173313)) ;
#109956 = CARTESIAN_POINT('Ctrl Pts',(-18.2211226527169,-19.1704342182428,
123.61830904749)) ;
#109957 = CARTESIAN_POINT('Ctrl Pts',(-18.275002203274,-19.180434396949,123.82149097982)) ;
#109958 = CARTESIAN_POINT('Ctrl Pts',(-18.362473813008,-19.1903516751586,
124.010785298937)) ;
#109959 = CARTESIAN_POINT('Ctrl Pts',(-18.4830604606472,-19.2003989215723,
124.184170492209)) ;
#109960 = CARTESIAN_POINT('Ctrl Pts',(-18.6292379918478,-19.2102728105536,
124.331599109654)) ;
#109961 = CARTESIAN_POINT('Ctrl Pts',(-18.8019088991085,-19.2203348281341,
124.453750377466)) ;
#109962 = CARTESIAN_POINT('Ctrl Pts',(-18.9895857425821,-19.2302058898684,
124.542341717898)) ;
#109963 = CARTESIAN_POINT('Ctrl Pts',(-19.1921191624894,-19.2401999532287,
124.598242968715)) ;
#109964 = CARTESIAN_POINT('Ctrl Pts',(-19.402117853516,-19.2502321112621,
124.617737811101)) ;
#109965 = CARTESIAN_POINT('Ctrl Pts',(-19.6088502595505,-19.2600959875023,
124.60121401046)) ;
#109966 = CARTESIAN_POINT('Ctrl Pts',(-19.8137388516603,-19.2701665021406,
124.547988022322)) ;
#109967 = CARTESIAN_POINT('Ctrl Pts',(-20.001923561908,-19.2800071390815,
124.462005142766)) ;
#109968 = CARTESIAN_POINT('Ctrl Pts',(-20.1748742487419,-19.2899742679217,
124.343734624428)) ;
#109969 = CARTESIAN_POINT('Ctrl Pts',(-20.3252319959921,-19.2999882410463,
124.196364047669)) ;
#109970 = CARTESIAN_POINT('Ctrl Pts',(-20.4877985477209,-19.3132729749095,
123.969234364874)) ;
#109971 = CARTESIAN_POINT('Ctrl Pts',(-20.5871267764397,-19.3264982396243,
123.706173914171)) ;
#109972 = CARTESIAN_POINT('Ctrl Pts',(-20.6152290370537,-19.3398087621792,
123.42777540713)) ;
#109973 = CARTESIAN_POINT('Ctrl Pts',(-20.599492811723,-19.3498374070813,
123.217527858378)) ;
#109974 = CARTESIAN_POINT('Ctrl Pts',(-20.5484314303572,-19.3597184394352,
123.016168149835)) ;
#109975 = CARTESIAN_POINT('Ctrl Pts',(-20.4627206437305,-19.3696994121153,
122.824640769478)) ;
#109976 = CARTESIAN_POINT('Ctrl Pts',(-20.3449158365693,-19.3796805397013,
122.651015461201)) ;
#109977 = CARTESIAN_POINT('Ctrl Pts',(-20.1513347577874,-19.3929237299627,
122.450805264359)) ;
#109978 = CARTESIAN_POINT('Ctrl Pts',(-19.8474851368482,-19.4095917253235,
122.268618378182)) ;
#109979 = CARTESIAN_POINT('Ctrl Pts',(-19.502594184235,-19.4261122253356,
122.201353744407)) ;
#109980 = CARTESIAN_POINT('Ctrl Pts',(-19.2234377981057,-19.4394252416516,
122.220278409184)) ;
#109981 = CARTESIAN_POINT('Ctrl Pts',(-19.0209390775846,-19.4493417998846,
122.270033904775)) ;
#109982 = CARTESIAN_POINT('Ctrl Pts',(-18.8281392830111,-19.4593694681874,
122.355168921347)) ;
#109983 = CARTESIAN_POINT('Ctrl Pts',(-18.5974710054624,-19.4725500579321,
122.508922302642)) ;
#109984 = CARTESIAN_POINT('Ctrl Pts',(-18.3626796542857,-19.4892981970515,
122.776419914561)) ;
#109985 = CARTESIAN_POINT('Ctrl Pts',(-18.2093485735078,-19.509092939562,
123.168602503809)) ;
#109986 = CARTESIAN_POINT('Ctrl Pts',(-18.1985006814529,-19.5291373323708,
123.594513815601)) ;
#109987 = CARTESIAN_POINT('Ctrl Pts',(-18.3326934843077,-19.5489765146695,
123.994555170299)) ;
#109988 = CARTESIAN_POINT('Ctrl Pts',(-18.595532066045,-19.5689018383624,
124.326702945903)) ;
#109989 = CARTESIAN_POINT('Ctrl Pts',(-18.9560824794692,-19.5888254764139,
124.549244809384)) ;
#109990 = CARTESIAN_POINT('Ctrl Pts',(-19.3708157304134,-19.6087503498795,
124.635502197578)) ;
#109991 = CARTESIAN_POINT('Ctrl Pts',(-19.7892668695317,-19.6286289569584,
124.575730747181)) ;
#109992 = CARTESIAN_POINT('Ctrl Pts',(-20.1641244036154,-19.6486063997904,
124.375961440855)) ;
#109993 = CARTESIAN_POINT('Ctrl Pts',(-20.4474719028058,-19.668538247875,
124.060750143978)) ;
#109994 = CARTESIAN_POINT('Ctrl Pts',(-20.6063139188946,-19.6884335162176,
123.668704683304)) ;
#109995 = CARTESIAN_POINT('Ctrl Pts',(-20.6223315797479,-19.7083560146297,
123.245390651494)) ;
#109996 = CARTESIAN_POINT('Ctrl Pts',(-20.4925827004531,-19.7283154965057,
122.841292698172)) ;
#109997 = CARTESIAN_POINT('Ctrl Pts',(-20.2339043279252,-19.7481932489651,
122.507125822127)) ;
#109998 = CARTESIAN_POINT('Ctrl Pts',(-19.8771665827689,-19.7680750396997,
122.280148989809)) ;
#109999 = CARTESIAN_POINT('Ctrl Pts',(-19.4603683091959,-19.7881483785506,
122.188512153594)) ;
#110000 = CARTESIAN_POINT('Ctrl Pts',(-19.0428239455345,-19.8079528457864,
122.243764244141)) ;
#110001 = CARTESIAN_POINT('Ctrl Pts',(-18.665519263309,-19.8279361861942,
122.439036410553)) ;
#110002 = CARTESIAN_POINT('Ctrl Pts',(-18.3789440648268,-19.8478511507922,
122.75077682738)) ;
#110003 = CARTESIAN_POINT('Ctrl Pts',(-18.2152094913907,-19.8677196855086,
123.140303318834)) ;
#110004 = CARTESIAN_POINT('Ctrl Pts',(-18.1947357277213,-19.8877720697203,
123.566054433339)) ;
#110005 = CARTESIAN_POINT('Ctrl Pts',(-18.3185728161467,-19.9075460335095,
123.968029365014)) ;
#110006 = CARTESIAN_POINT('Ctrl Pts',(-18.5752735623611,-19.9276004125309,
124.308301084886)) ;
#110007 = CARTESIAN_POINT('Ctrl Pts',(-18.9284269314398,-19.9473971501041,
124.537586399167)) ;
#110008 = CARTESIAN_POINT('Ctrl Pts',(-19.3416860710979,-19.9673649624556,
124.634515296765)) ;
#110009 = CARTESIAN_POINT('Ctrl Pts',(-19.7631262986473,-19.9873239385206,
124.583944361733)) ;
#110010 = CARTESIAN_POINT('Ctrl Pts',(-20.1408300394929,-20.007218856798,
124.393492146768)) ;
#110011 = CARTESIAN_POINT('Ctrl Pts',(-20.4312553648527,-20.0271151692483,
124.08593532179)) ;
#110012 = CARTESIAN_POINT('Ctrl Pts',(-20.5998519136099,-20.0470231026225,
123.697630502845)) ;
#110013 = CARTESIAN_POINT('Ctrl Pts',(-20.6258245023825,-20.0669729929109,
123.274274416115)) ;
#110014 = CARTESIAN_POINT('Ctrl Pts',(-20.5065978044724,-20.0868502234122,
122.868753310191)) ;
#110015 = CARTESIAN_POINT('Ctrl Pts',(-20.2550274980702,-20.1068328922832,
122.526375979373)) ;
#110016 = CARTESIAN_POINT('Ctrl Pts',(-19.902383481254,-20.1267657788636,
122.291183292636)) ;
#110017 = CARTESIAN_POINT('Ctrl Pts',(-19.4912069295135,-20.1466785248815,
122.190296741337)) ;
#110018 = CARTESIAN_POINT('Ctrl Pts',(-19.140915912058,-20.1632482462234,
122.227731091177)) ;
#110019 = CARTESIAN_POINT('Ctrl Pts',(-18.8799587483963,-20.1765482575283,
122.328242563752)) ;
#110020 = CARTESIAN_POINT('Ctrl Pts',(-18.6408171882554,-20.1898184452782,
122.471832138392)) ;
#110021 = CARTESIAN_POINT('Ctrl Pts',(-18.3949341584234,-20.2064458276436,
122.725969122882)) ;
#110022 = CARTESIAN_POINT('Ctrl Pts',(-18.2507664641424,-20.2230681173888,
123.048618088243)) ;
#110023 = CARTESIAN_POINT('Ctrl Pts',(-18.2066181119589,-20.2363133317834,
123.323576763355)) ;
#110024 = CARTESIAN_POINT('Ctrl Pts',(-18.2092019548847,-20.246225296744,
123.531950166732)) ;
#110025 = CARTESIAN_POINT('Ctrl Pts',(-18.2487326336713,-20.2562839199085,
123.739663902486)) ;
#110026 = CARTESIAN_POINT('Ctrl Pts',(-18.3218330387796,-20.2661240340243,
123.93322086653)) ;
#110027 = CARTESIAN_POINT('Ctrl Pts',(-18.4296381028311,-20.2761898189819,
124.115280112872)) ;
#110028 = CARTESIAN_POINT('Ctrl Pts',(-18.5650254182879,-20.2860731367698,
124.272929899984)) ;
#110029 = CARTESIAN_POINT('Ctrl Pts',(-18.7271272737552,-20.2960625746284,
124.406415194955)) ;
#110030 = CARTESIAN_POINT('Ctrl Pts',(-18.9095372947152,-20.3060262886811,
124.50941030472)) ;
#110031 = CARTESIAN_POINT('Ctrl Pts',(-19.107611837261,-20.3160213003403,
124.579597798303)) ;
#110032 = CARTESIAN_POINT('Ctrl Pts',(-19.3157493662386,-20.3260575920346,
124.614140465234)) ;
#110033 = CARTESIAN_POINT('Ctrl Pts',(-19.5227562334868,-20.335903969728,
124.612396669605)) ;
#110034 = CARTESIAN_POINT('Ctrl Pts',(-19.7292111974221,-20.3458889138787,
124.574608753497)) ;
#110035 = CARTESIAN_POINT('Ctrl Pts',(-19.925125471761,-20.3558258850087,
124.501991060372)) ;
#110036 = CARTESIAN_POINT('Ctrl Pts',(-20.1073988758858,-20.3658756696404,
124.395191781569)) ;
#110037 = CARTESIAN_POINT('Ctrl Pts',(-20.2652964459926,-20.3757261317179,
124.261176985786)) ;
#110038 = CARTESIAN_POINT('Ctrl Pts',(-20.3995514635693,-20.3856981452383,
124.10019644683)) ;
#110039 = CARTESIAN_POINT('Ctrl Pts',(-20.5040636035381,-20.3956932923577,
123.917862057501)) ;
#110040 = CARTESIAN_POINT('Ctrl Pts',(-20.5753478684209,-20.4057272620938,
123.719344993247)) ;
#110041 = CARTESIAN_POINT('Ctrl Pts',(-20.6107721861125,-20.4155828077644,
123.515181542803)) ;
#110042 = CARTESIAN_POINT('Ctrl Pts',(-20.6104965932581,-20.4255815647777,
123.305010267577)) ;
#110043 = CARTESIAN_POINT('Ctrl Pts',(-20.5742911155273,-20.4354787000148,
123.100083952129)) ;
#110044 = CARTESIAN_POINT('Ctrl Pts',(-20.5019849660785,-20.4455317958545,
122.901512699624)) ;
#110045 = CARTESIAN_POINT('Ctrl Pts',(-20.3980814572166,-20.4554153045851,
122.721558477132)) ;
#110046 = CARTESIAN_POINT('Ctrl Pts',(-20.2633955813558,-20.4654101772312,
122.560285333352)) ;
#110047 = CARTESIAN_POINT('Ctrl Pts',(-20.1021248406292,-20.4754301388669,
122.424747050314)) ;
#110048 = CARTESIAN_POINT('Ctrl Pts',(-19.9219560051143,-20.4853355026667,
122.320331596646)) ;
#110049 = CARTESIAN_POINT('Ctrl Pts',(-19.7258557561227,-20.4952760902742,
122.248133907373)) ;
#110050 = CARTESIAN_POINT('Ctrl Pts',(-19.5188945875135,-20.5052789083749,
122.210725270222)) ;
#110051 = CARTESIAN_POINT('Ctrl Pts',(-19.307945758579,-20.515313620099,122.210161246172)) ;
#110052 = CARTESIAN_POINT('Ctrl Pts',(-19.103950726785,-20.5251585268363,
122.245209737207)) ;
#110053 = CARTESIAN_POINT('Ctrl Pts',(-18.906261605579,-20.5351443794053,
122.315759737791)) ;
#110054 = CARTESIAN_POINT('Ctrl Pts',(-18.7246214853924,-20.5450791878184,
122.418938878416)) ;
#110055 = CARTESIAN_POINT('Ctrl Pts',(-18.561841158437,-20.5551367148994,
122.553835375352)) ;
#110056 = CARTESIAN_POINT('Ctrl Pts',(-18.4278915293731,-20.5649583698965,
122.711002697544)) ;
#110057 = CARTESIAN_POINT('Ctrl Pts',(-18.3204489250586,-20.5750144140696,
122.893054741665)) ;
#110058 = CARTESIAN_POINT('Ctrl Pts',(-18.2474436152524,-20.5849551541147,
123.088883550092)) ;
#110059 = CARTESIAN_POINT('Ctrl Pts',(-18.2090477921902,-20.5948592751876,
123.293531110936)) ;
#110060 = CARTESIAN_POINT('Ctrl Pts',(-18.2068652483625,-20.6049068163418,
123.504735999591)) ;
#110061 = CARTESIAN_POINT('Ctrl Pts',(-18.2407324430566,-20.6148055679422,
123.71009232921)) ;
#110062 = CARTESIAN_POINT('Ctrl Pts',(-18.3106819815042,-20.624854046908,
123.909401518237)) ;
#110063 = CARTESIAN_POINT('Ctrl Pts',(-18.412525450658,-20.6347415439918,
124.090634268722)) ;
#110064 = CARTESIAN_POINT('Ctrl Pts',(-18.5453697766947,-20.6447346342898,
124.253363728476)) ;
#110065 = CARTESIAN_POINT('Ctrl Pts',(-18.7038706478983,-20.6546868043501,
124.389958772071)) ;
#110066 = CARTESIAN_POINT('Ctrl Pts',(-18.8832629374876,-20.6646252242646,
124.497042469255)) ;
#110067 = CARTESIAN_POINT('Ctrl Pts',(-19.0793903057609,-20.6746103543502,
124.571934113888)) ;
#110068 = CARTESIAN_POINT('Ctrl Pts',(-19.286632008583,-20.6846470437643,
124.61152478451)) ;
#110069 = CARTESIAN_POINT('Ctrl Pts',(-19.4938007273838,-20.6945017277568,
124.614806296996)) ;
#110070 = CARTESIAN_POINT('Ctrl Pts',(-19.7013904956514,-20.7045012118047,
124.581880810184)) ;
#110071 = CARTESIAN_POINT('Ctrl Pts',(-19.898174089497,-20.7143963005816,
124.514312939417)) ;
#110072 = CARTESIAN_POINT('Ctrl Pts',(-20.0832161329182,-20.7244568552277,
124.411930707382)) ;
#110073 = CARTESIAN_POINT('Ctrl Pts',(-20.2443229888537,-20.7343061196006,
124.281830751314)) ;
#110074 = CARTESIAN_POINT('Ctrl Pts',(-20.3832402337961,-20.7443333720484,
124.123279778184)) ;
#110075 = CARTESIAN_POINT('Ctrl Pts',(-20.4920625617071,-20.7543616696186,
123.942698375458)) ;
#110076 = CARTESIAN_POINT('Ctrl Pts',(-20.5668644543846,-20.7642077986246,
123.749699501768)) ;
#110077 = CARTESIAN_POINT('Ctrl Pts',(-20.6081396022148,-20.7742017039867,
123.543691073586)) ;
#110078 = CARTESIAN_POINT('Ctrl Pts',(-20.6126551704961,-20.7842258016697,
123.33299569446)) ;
#110079 = CARTESIAN_POINT('Ctrl Pts',(-20.5812076461925,-20.7941156295238,
123.12746908366)) ;
#110080 = CARTESIAN_POINT('Ctrl Pts',(-20.5141570188128,-20.8041076109542,
122.928403469444)) ;
#110081 = CARTESIAN_POINT('Ctrl Pts',(-20.4139656629359,-20.81405461572,122.744850153781)) ;
#110082 = CARTESIAN_POINT('Ctrl Pts',(-20.2836859018006,-20.8240042671098,
122.581191696516)) ;
#110083 = CARTESIAN_POINT('Ctrl Pts',(-20.1254895016299,-20.8340412700872,
122.441562353211)) ;
#110084 = CARTESIAN_POINT('Ctrl Pts',(-19.9481736179752,-20.8439301785222,
122.333013783755)) ;
#110085 = CARTESIAN_POINT('Ctrl Pts',(-19.7528897368703,-20.8539195109997,
122.255780022746)) ;
#110086 = CARTESIAN_POINT('Ctrl Pts',(-19.5477653368239,-20.8638780664368,
122.21391083095)) ;
#110087 = CARTESIAN_POINT('Ctrl Pts',(-19.3397219215297,-20.8737776376373,
122.207813425612)) ;
#110088 = CARTESIAN_POINT('Ctrl Pts',(-19.1307386777796,-20.8838255628893,
122.238452327892)) ;
#110089 = CARTESIAN_POINT('Ctrl Pts',(-18.9331920275897,-20.8937208624153,
122.303763595035)) ;
#110090 = CARTESIAN_POINT('Ctrl Pts',(-18.7469406377159,-20.9037827188633,
122.403992340542)) ;
#110091 = CARTESIAN_POINT('Ctrl Pts',(-18.5844660473413,-20.9136265652799,
122.532186232912)) ;
#110092 = CARTESIAN_POINT('Ctrl Pts',(-18.4445263094676,-20.923589514408,
122.688016060404)) ;
#110093 = CARTESIAN_POINT('Ctrl Pts',(-18.3332651907842,-20.933623550836,
122.867242942341)) ;
#110094 = CARTESIAN_POINT('Ctrl Pts',(-18.255760896139,-20.943510977794,123.06011486023)) ;
#110095 = CARTESIAN_POINT('Ctrl Pts',(-18.2119773230723,-20.9535254121304,
123.266061465517)) ;
#110096 = CARTESIAN_POINT('Ctrl Pts',(-18.2051328147067,-20.9635603567653,
123.47690249234)) ;
#110097 = CARTESIAN_POINT('Ctrl Pts',(-18.2338429419005,-20.9733927067963,
123.681630881858)) ;
#110098 = CARTESIAN_POINT('Ctrl Pts',(-18.2991641108333,-20.9834681459136,
123.883082556279)) ;
#110099 = CARTESIAN_POINT('Ctrl Pts',(-18.3962071339679,-20.9933206111482,
124.066122319021)) ;
#110100 = CARTESIAN_POINT('Ctrl Pts',(-18.5262236801046,-21.003393488725,
124.233228390532)) ;
#110101 = CARTESIAN_POINT('Ctrl Pts',(-18.679747523657,-21.0132360849175,
124.371988478455)) ;
#110102 = CARTESIAN_POINT('Ctrl Pts',(-18.8570885901101,-21.0232164690328,
124.484106351703)) ;
#110103 = CARTESIAN_POINT('Ctrl Pts',(-19.0521035461318,-21.0332349496816,
124.563654847553)) ;
#110104 = CARTESIAN_POINT('Ctrl Pts',(-19.2551257459928,-21.043118264682,
124.607973941518)) ;
#110105 = CARTESIAN_POINT('Ctrl Pts',(-19.4665891466891,-21.0531865617724,
124.616429421318)) ;
#110106 = CARTESIAN_POINT('Ctrl Pts',(-19.6714489088965,-21.0630166301447,
124.588945550582)) ;
#110107 = CARTESIAN_POINT('Ctrl Pts',(-19.8731767946345,-21.0730834226131,
124.525074761715)) ;
#110108 = CARTESIAN_POINT('Ctrl Pts',(-20.0574667356914,-21.0829727561017,
124.428757633775)) ;
#110109 = CARTESIAN_POINT('Ctrl Pts',(-20.2242553261606,-21.0929748875177,
124.30076558423)) ;
#110110 = CARTESIAN_POINT('Ctrl Pts',(-20.3653246495057,-21.1028987571387,
124.147006904464)) ;
#110111 = CARTESIAN_POINT('Ctrl Pts',(-20.4788171883682,-21.1129422726559,
123.968992960858)) ;
#110112 = CARTESIAN_POINT('Ctrl Pts',(-20.5586276458722,-21.1228244855442,
123.777137772232)) ;
#110113 = CARTESIAN_POINT('Ctrl Pts',(-20.6047443149979,-21.1328925627636,
123.570599818979)) ;
#110114 = CARTESIAN_POINT('Ctrl Pts',(-20.6142702694296,-21.1427310674978,
123.363949210001)) ;
#110115 = CARTESIAN_POINT('Ctrl Pts',(-20.5874714905014,-21.1527938359272,
123.154128203089)) ;
#110116 = CARTESIAN_POINT('Ctrl Pts',(-20.5254554023326,-21.16269082921,122.955506873785)) ;
#110117 = CARTESIAN_POINT('Ctrl Pts',(-20.4301916692366,-21.1726220568447,
122.769727356986)) ;
#110118 = CARTESIAN_POINT('Ctrl Pts',(-20.3025228731175,-21.1826642154869,
122.601589191688)) ;
#110119 = CARTESIAN_POINT('Ctrl Pts',(-20.150091024587,-21.1925509250179,
122.460275067558)) ;
#110120 = CARTESIAN_POINT('Ctrl Pts',(-19.9737686440358,-21.2025438974465,
122.346075116871)) ;
#110121 = CARTESIAN_POINT('Ctrl Pts',(-19.7811612302228,-21.2124900919831,
122.264687827814)) ;
#110122 = CARTESIAN_POINT('Ctrl Pts',(-19.5774463989845,-21.2224354668346,
122.217531678167)) ;
#110123 = CARTESIAN_POINT('Ctrl Pts',(-19.3663628543856,-21.2324903861945,
122.20667048337)) ;
#110124 = CARTESIAN_POINT('Ctrl Pts',(-19.1613711774936,-21.242311905638,
122.231635670187)) ;
#110125 = CARTESIAN_POINT('Ctrl Pts',(-18.9589018519402,-21.2523776744049,
122.293046537382)) ;
#110126 = CARTESIAN_POINT('Ctrl Pts',(-18.7732094196885,-21.26227959606,122.387219888)) ;
#110127 = CARTESIAN_POINT('Ctrl Pts',(-18.6042493248549,-21.272322654881,
122.513802987668)) ;
#110128 = CARTESIAN_POINT('Ctrl Pts',(-18.4618698159621,-21.2822286489237,
122.66579181477)) ;
#110129 = CARTESIAN_POINT('Ctrl Pts',(-18.3471676797606,-21.2921664220055,
122.840411185076)) ;
#110130 = CARTESIAN_POINT('Ctrl Pts',(-18.2638835728241,-21.3022067857378,
123.034362272501)) ;
#110131 = CARTESIAN_POINT('Ctrl Pts',(-18.2161214621588,-21.3120941294613,
123.236674064325)) ;
#110132 = CARTESIAN_POINT('Ctrl Pts',(-18.2037418777044,-21.32208636003,123.446362842133)) ;
#110133 = CARTESIAN_POINT('Ctrl Pts',(-18.2279129348315,-21.3320348878136,
123.654122553603)) ;
#110134 = CARTESIAN_POINT('Ctrl Pts',(-18.2874294697548,-21.3419716715369,
123.854348898815)) ;
#110135 = CARTESIAN_POINT('Ctrl Pts',(-18.3810239530935,-21.3519546723339,
124.042227779057)) ;
#110136 = CARTESIAN_POINT('Ctrl Pts',(-18.5068622838946,-21.3619985591746,
124.211757758782)) ;
#110137 = CARTESIAN_POINT('Ctrl Pts',(-18.6566313912586,-21.3718265827492,
124.354140460403)) ;
#110138 = CARTESIAN_POINT('Ctrl Pts',(-18.8330992076541,-21.3819038309628,
124.47128066986)) ;
#110139 = CARTESIAN_POINT('Ctrl Pts',(-19.0228746278111,-21.3917533862681,
124.554257395901)) ;
#110140 = CARTESIAN_POINT('Ctrl Pts',(-19.2288169230001,-21.4018360944658,
124.60422215499)) ;
#110141 = CARTESIAN_POINT('Ctrl Pts',(-19.4347261166129,-21.4116486873923,
124.617503248292)) ;
#110142 = CARTESIAN_POINT('Ctrl Pts',(-19.6450785005177,-21.4217158796502,
124.594593802766)) ;
#110143 = CARTESIAN_POINT('Ctrl Pts',(-19.8449338607638,-21.4316147091128,
124.536394653996)) ;
#110144 = CARTESIAN_POINT('Ctrl Pts',(-20.0345279221101,-21.441668700303,
124.443060736217)) ;
#110145 = CARTESIAN_POINT('Ctrl Pts',(-20.202124046624,-21.4515404250862,
124.320586102632)) ;
#110146 = CARTESIAN_POINT('Ctrl Pts',(-20.3487851621691,-21.4616108672164,
124.167950398261)) ;
#110147 = CARTESIAN_POINT('Ctrl Pts',(-20.4640443699973,-21.4714439456467,
123.99631872576)) ;
#110148 = CARTESIAN_POINT('Ctrl Pts',(-20.549971147551,-21.4814744191481,
123.803755949194)) ;
#110149 = CARTESIAN_POINT('Ctrl Pts',(-20.6005714118923,-21.4915060184468,
123.599008016726)) ;
#110150 = CARTESIAN_POINT('Ctrl Pts',(-20.6149930382803,-21.501335719485,
123.392875020764)) ;
#110151 = CARTESIAN_POINT('Ctrl Pts',(-20.5936752493036,-21.5113251575414,
123.183943960164)) ;
#110152 = CARTESIAN_POINT('Ctrl Pts',(-20.5355777473698,-21.5213690607575,
122.980942002523)) ;
#110153 = CARTESIAN_POINT('Ctrl Pts',(-20.4455485430694,-21.531190581571,
122.795122750937)) ;
#110154 = CARTESIAN_POINT('Ctrl Pts',(-20.32239781883,-21.5412263058181,122.62381713844)) ;
#110155 = CARTESIAN_POINT('Ctrl Pts',(-20.1711825346155,-21.5512484597506,
122.477072730469)) ;
#110156 = CARTESIAN_POINT('Ctrl Pts',(-19.9997840107128,-21.5611106915079,
122.360437973378)) ;
#110157 = CARTESIAN_POINT('Ctrl Pts',(-19.8091030402244,-21.5710697619658,
122.273953553956)) ;
#110158 = CARTESIAN_POINT('Ctrl Pts',(-19.6046853272401,-21.581104934342,
122.221814065515)) ;
#110159 = CARTESIAN_POINT('Ctrl Pts',(-19.3975576732119,-21.5909853195003,
122.205891559411)) ;
#110160 = CARTESIAN_POINT('Ctrl Pts',(-19.187156505492,-21.6010420340942,
122.226451139715)) ;
#110161 = CARTESIAN_POINT('Ctrl Pts',(-18.9870882797625,-21.6109213026663,
122.282251997296)) ;
#110162 = CARTESIAN_POINT('Ctrl Pts',(-18.7973962302635,-21.6209122601519,
122.372443187601)) ;
#110163 = CARTESIAN_POINT('Ctrl Pts',(-18.6256636562524,-21.6309529187871,
122.495187407755)) ;
#110164 = CARTESIAN_POINT('Ctrl Pts',(-18.48066666662,-21.6407858984951,122.642521307591)) ;
#110165 = CARTESIAN_POINT('Ctrl Pts',(-18.361049228198,-21.6507790317448,
122.815226200601)) ;
#110166 = CARTESIAN_POINT('Ctrl Pts',(-18.2732875703771,-21.6608110841282,
123.007015407753)) ;
#110167 = CARTESIAN_POINT('Ctrl Pts',(-18.2208007009396,-21.6706763130795,
123.207651206908)) ;
#110168 = CARTESIAN_POINT('Ctrl Pts',(-18.2031911283783,-21.6806382543227,
123.416346478614)) ;
#110169 = CARTESIAN_POINT('Ctrl Pts',(-18.2225608620938,-21.6906729693595,
123.62640699923)) ;
#110170 = CARTESIAN_POINT('Ctrl Pts',(-18.2769704978014,-21.7005587397035,
123.827014417292)) ;
#110171 = CARTESIAN_POINT('Ctrl Pts',(-18.366948205142,-21.7106213370923,
124.018445066761)) ;
#110172 = CARTESIAN_POINT('Ctrl Pts',(-18.4861761449273,-21.7204717489275,
124.187785812144)) ;
#110173 = CARTESIAN_POINT('Ctrl Pts',(-18.6352321006929,-21.7304989182135,
124.336841760697)) ;
#110174 = CARTESIAN_POINT('Ctrl Pts',(-18.8082391470289,-21.7405263989276,
124.457313560108)) ;
#110175 = CARTESIAN_POINT('Ctrl Pts',(-18.9958335774974,-21.7503694515069,
124.54464010057)) ;
#110176 = CARTESIAN_POINT('Ctrl Pts',(-19.1986731078238,-21.7603633549455,
124.599405998781)) ;
#110177 = CARTESIAN_POINT('Ctrl Pts',(-19.40867613973,-21.7703904777219,124.617796950321)) ;
#110178 = CARTESIAN_POINT('Ctrl Pts',(-19.6158461362615,-21.780281182614,
124.599954845564)) ;
#110179 = CARTESIAN_POINT('Ctrl Pts',(-19.818898212955,-21.7902732094643,
124.546160262873)) ;
#110180 = CARTESIAN_POINT('Ctrl Pts',(-20.0086259642229,-21.8002191909528,
124.45827439386)) ;
#110181 = CARTESIAN_POINT('Ctrl Pts',(-20.1804838998877,-21.8101663635748,
124.339105459725)) ;
#110182 = CARTESIAN_POINT('Ctrl Pts',(-20.3303651061853,-21.8202143049009,
124.190260940552)) ;
#110183 = CARTESIAN_POINT('Ctrl Pts',(-20.44984618333,-21.8300619387087,124.021187754941)) ;
#110184 = CARTESIAN_POINT('Ctrl Pts',(-20.5397670979024,-21.8400236533937,
123.832058906243)) ;
#110185 = CARTESIAN_POINT('Ctrl Pts',(-20.595605471887,-21.8500522862723,
123.628740790415)) ;
#110186 = CARTESIAN_POINT('Ctrl Pts',(-20.6151272873564,-21.8599626118074,
123.421319755788)) ;
#110187 = CARTESIAN_POINT('Ctrl Pts',(-20.5988366246806,-21.8698974422791,
123.213090195066)) ;
#110188 = CARTESIAN_POINT('Ctrl Pts',(-20.5459055465969,-21.8799387746611,
123.008733750031)) ;
#110189 = CARTESIAN_POINT('Ctrl Pts',(-20.4596600267201,-21.8898316480999,
122.819481746608)) ;
#110190 = CARTESIAN_POINT('Ctrl Pts',(-20.3413884517558,-21.8998008139178,
122.646447100999)) ;
#110191 = CARTESIAN_POINT('Ctrl Pts',(-20.1937643496207,-21.9098295476343,
122.495946975075)) ;
#110192 = CARTESIAN_POINT('Ctrl Pts',(-19.9684091132724,-21.9230220664055,
122.334150782013)) ;
#110193 = CARTESIAN_POINT('Ctrl Pts',(-19.7027954997359,-21.9363819344482,
122.233654581358)) ;
#110194 = CARTESIAN_POINT('Ctrl Pts',(-19.4261136233799,-21.949607271597,
122.206049795975)) ;
#110195 = CARTESIAN_POINT('Ctrl Pts',(-19.2168214355543,-21.9595884974377,
122.221179697756)) ;
#110196 = CARTESIAN_POINT('Ctrl Pts',(-19.0123391542729,-21.9696240644205,
122.273098838906)) ;
#110197 = CARTESIAN_POINT('Ctrl Pts',(-18.8230823789941,-21.9794871423826,
122.35787277801)) ;
#110198 = CARTESIAN_POINT('Ctrl Pts',(-18.647826079591,-21.9895574411837,
122.476601262641)) ;
#110199 = CARTESIAN_POINT('Ctrl Pts',(-18.4992732563713,-21.9993997397515,
122.620651348207)) ;
#110200 = CARTESIAN_POINT('Ctrl Pts',(-18.3759120884647,-22.0093604379213,
122.789857776292)) ;
#110201 = CARTESIAN_POINT('Ctrl Pts',(-18.2834679404638,-22.0193984721008,
122.979555019762)) ;
#110202 = CARTESIAN_POINT('Ctrl Pts',(-18.2259320393072,-22.0292722089473,
123.179027482154)) ;
#110203 = CARTESIAN_POINT('Ctrl Pts',(-18.2034947861187,-22.0393439928725,
123.389545892511)) ;
#110204 = CARTESIAN_POINT('Ctrl Pts',(-18.2174847861371,-22.0491761140737,
123.595794504607)) ;
#110205 = CARTESIAN_POINT('Ctrl Pts',(-18.2675292236571,-22.0592091380992,
123.800687116202)) ;
#110206 = CARTESIAN_POINT('Ctrl Pts',(-18.3527474674148,-22.0692250182958,
123.993252228015)) ;
#110207 = CARTESIAN_POINT('Ctrl Pts',(-18.4682277219451,-22.07910853739,124.165989285002)) ;
#110208 = CARTESIAN_POINT('Ctrl Pts',(-18.6132948886826,-22.0890989497537,
124.317850175962)) ;
#110209 = CARTESIAN_POINT('Ctrl Pts',(-18.8379447204078,-22.1023621129571,
124.4830618042)) ;
#110210 = CARTESIAN_POINT('Ctrl Pts',(-19.1007522517418,-22.1156396832083,
124.586210092196)) ;
#110211 = CARTESIAN_POINT('Ctrl Pts',(-19.379236168064,-22.1289699857149,
124.617408838081)) ;
#110212 = CARTESIAN_POINT('Ctrl Pts',(-19.5869520547249,-22.1388686675313,
124.604630768228)) ;
#110213 = CARTESIAN_POINT('Ctrl Pts',(-19.7911927299696,-22.1488581825789,
124.555778247688)) ;
#110214 = CARTESIAN_POINT('Ctrl Pts',(-19.9830639463942,-22.1588062343539,
124.472536042139)) ;
#110215 = CARTESIAN_POINT('Ctrl Pts',(-20.1575732402841,-22.1687476376324,
124.357556089327)) ;
#110216 = CARTESIAN_POINT('Ctrl Pts',(-20.3608541530847,-22.1820343024133,
124.165920245841)) ;
#110217 = CARTESIAN_POINT('Ctrl Pts',(-20.5464540439784,-22.1986447240681,
123.865489281931)) ;
#110218 = CARTESIAN_POINT('Ctrl Pts',(-20.633019827343,-22.2185559863189,
123.451045815633)) ;
#110219 = CARTESIAN_POINT('Ctrl Pts',(-20.5730213815299,-22.2385001154838,
123.031223440757)) ;
#110220 = CARTESIAN_POINT('Ctrl Pts',(-20.3735529890649,-22.258423278089,
122.657547985206)) ;
#110221 = CARTESIAN_POINT('Ctrl Pts',(-20.0594592735491,-22.2783134004955,
122.374245995463)) ;
#110222 = CARTESIAN_POINT('Ctrl Pts',(-19.6652813669515,-22.2983183540956,
122.214565895303)) ;
#110223 = CARTESIAN_POINT('Ctrl Pts',(-19.2436812231406,-22.3181566111112,
122.198771686006)) ;
#110224 = CARTESIAN_POINT('Ctrl Pts',(-18.8388332464108,-22.3381509118978,
122.32835579748)) ;
#110225 = CARTESIAN_POINT('Ctrl Pts',(-18.504525172612,-22.3580361539422,
122.58723590079)) ;
#110226 = CARTESIAN_POINT('Ctrl Pts',(-18.2777439448493,-22.3779111004182,
122.943826523653)) ;
#110227 = CARTESIAN_POINT('Ctrl Pts',(-18.1858522059303,-22.3979441703592,
123.359795345687)) ;
#110228 = CARTESIAN_POINT('Ctrl Pts',(-18.2415379515437,-22.4178326772596,
123.778960157754)) ;
#110229 = CARTESIAN_POINT('Ctrl Pts',(-18.4353340344913,-22.4376875370409,
124.154091788582)) ;
#110230 = CARTESIAN_POINT('Ctrl Pts',(-18.7489215868885,-22.4577383708286,
124.442775285541)) ;
#110231 = CARTESIAN_POINT('Ctrl Pts',(-19.1366297245527,-22.4775043127179,
124.60529872623)) ;
#110232 = CARTESIAN_POINT('Ctrl Pts',(-19.56148346132,-22.4975170441772,124.626852836326)) ;
#110233 = CARTESIAN_POINT('Ctrl Pts',(-19.9658127678861,-22.5174098791208,
124.502264634216)) ;
#110234 = CARTESIAN_POINT('Ctrl Pts',(-20.3038468818721,-22.5373169024603,
124.247689032613)) ;
#110235 = CARTESIAN_POINT('Ctrl Pts',(-20.535324133174,-22.557232167361,123.892984573076)) ;
#110236 = CARTESIAN_POINT('Ctrl Pts',(-20.6318705197225,-22.5772638595207,
123.478178968152)) ;
#110237 = CARTESIAN_POINT('Ctrl Pts',(-20.5815656121697,-22.5971069060937,
123.059226546936)) ;
#110238 = CARTESIAN_POINT('Ctrl Pts',(-20.3915264450237,-22.6170234539935,
122.680851642089)) ;
#110239 = CARTESIAN_POINT('Ctrl Pts',(-20.0834094424047,-22.6369556969848,
122.389795960095)) ;
#110240 = CARTESIAN_POINT('Ctrl Pts',(-19.6951657708857,-22.6568595317941,
122.221411049338)) ;
#110241 = CARTESIAN_POINT('Ctrl Pts',(-19.2728522521722,-22.6767599319816,
122.195093377981)) ;
#110242 = CARTESIAN_POINT('Ctrl Pts',(-18.8658348488513,-22.6967096083609,
122.314600232637)) ;
#110243 = CARTESIAN_POINT('Ctrl Pts',(-18.5243859309268,-22.7166421325813,
122.565678762431)) ;
#110244 = CARTESIAN_POINT('Ctrl Pts',(-18.2889454703731,-22.7365621415675,
122.917803138735)) ;
#110245 = CARTESIAN_POINT('Ctrl Pts',(-18.187692847346,-22.7565190477437,
123.329839846167)) ;
#110246 = CARTESIAN_POINT('Ctrl Pts',(-18.2325926072875,-22.7764048872452,
123.750356723264)) ;
#110247 = CARTESIAN_POINT('Ctrl Pts',(-18.4190644171146,-22.796376059381,
124.131759994554)) ;
#110248 = CARTESIAN_POINT('Ctrl Pts',(-18.7218015732181,-22.8161902563654,
124.424850326707)) ;
#110249 = CARTESIAN_POINT('Ctrl Pts',(-19.1092637308384,-22.8361714423337,
124.598954233523)) ;
#110250 = CARTESIAN_POINT('Ctrl Pts',(-19.4607813361328,-22.8527469477229,
124.624835893571)) ;
#110251 = CARTESIAN_POINT('Ctrl Pts',(-19.7357495655615,-22.8660563955865,
124.572863160943)) ;
#110252 = CARTESIAN_POINT('Ctrl Pts',(-19.9985287739549,-22.8794240933631,
124.473365736425)) ;
#110253 = CARTESIAN_POINT('Ctrl Pts',(-20.2833779018832,-22.895914665029,
124.268814789731)) ;
#110254 = CARTESIAN_POINT('Ctrl Pts',(-20.5233279788086,-22.9158349373618,
123.919863210383)) ;
#110255 = CARTESIAN_POINT('Ctrl Pts',(-20.6120068716856,-22.9324519730828,
123.577849376162)) ;
#110256 = CARTESIAN_POINT('Ctrl Pts',(-20.6099216751847,-22.9457428233639,
123.298396601366)) ;
#110257 = CARTESIAN_POINT('Ctrl Pts',(-20.572087590818,-22.9557118685184,
123.092286569263)) ;
#110258 = CARTESIAN_POINT('Ctrl Pts',(-20.499891090419,-22.965615259152,122.89697650164)) ;
#110259 = CARTESIAN_POINT('Ctrl Pts',(-20.3931695810502,-22.9756730452647,
122.714468566167)) ;
#110260 = CARTESIAN_POINT('Ctrl Pts',(-20.2592801680963,-22.9855250819144,
122.556402868269)) ;
#110261 = CARTESIAN_POINT('Ctrl Pts',(-20.0435485813,-22.9988902060576,122.376462993025)) ;
#110262 = CARTESIAN_POINT('Ctrl Pts',(-19.7882388012344,-23.0121162690207,
122.258444297752)) ;
#110263 = CARTESIAN_POINT('Ctrl Pts',(-19.5127364334295,-23.0254199173029,
122.210272537815)) ;
#110264 = CARTESIAN_POINT('Ctrl Pts',(-19.302659680117,-23.0354114484659,
122.210467160808)) ;
#110265 = CARTESIAN_POINT('Ctrl Pts',(-19.0949024968935,-23.0454508962652,
122.247583999801)) ;
#110266 = CARTESIAN_POINT('Ctrl Pts',(-18.9004743134239,-23.0552946717791,
122.318513409327)) ;
#110267 = CARTESIAN_POINT('Ctrl Pts',(-18.7185635235317,-23.0652803131667,
122.423230018673)) ;
#110268 = CARTESIAN_POINT('Ctrl Pts',(-18.5582621672955,-23.0752170975285,
122.557236993689)) ;
#110269 = CARTESIAN_POINT('Ctrl Pts',(-18.4222515809406,-23.0852669319959,
122.718888205701)) ;
#110270 = CARTESIAN_POINT('Ctrl Pts',(-18.3183218889293,-23.095117381499,
122.898025477711)) ;
#110271 = CARTESIAN_POINT('Ctrl Pts',(-18.2456967820823,-23.1050893954811,
123.09465898779)) ;
#110272 = CARTESIAN_POINT('Ctrl Pts',(-18.2082468940344,-23.1150845533282,
123.301458861102)) ;
#110273 = CARTESIAN_POINT('Ctrl Pts',(-18.2075241696679,-23.1251184796919,
123.512384558567)) ;
#110274 = CARTESIAN_POINT('Ctrl Pts',(-18.2424855512265,-23.1349741881243,
123.716630820847)) ;
#110275 = CARTESIAN_POINT('Ctrl Pts',(-18.3130881296415,-23.144972337463,
123.914575875777)) ;
#110276 = CARTESIAN_POINT('Ctrl Pts',(-18.4158307681651,-23.1548717406366,
124.095598548209)) ;
#110277 = CARTESIAN_POINT('Ctrl Pts',(-18.5504085228041,-23.164922937525,
124.25848010614)) ;
#110278 = CARTESIAN_POINT('Ctrl Pts',(-18.7085302858223,-23.1748052613379,
124.393265861275)) ;
#110279 = CARTESIAN_POINT('Ctrl Pts',(-18.8894347437918,-23.1848001569945,
124.500144674728)) ;
#110280 = CARTESIAN_POINT('Ctrl Pts',(-19.0867888436961,-23.194821256377,
124.573899104479)) ;
#110281 = CARTESIAN_POINT('Ctrl Pts',(-19.2915556335797,-23.2047285242391,
124.611989875097)) ;
#110282 = CARTESIAN_POINT('Ctrl Pts',(-19.5004638216049,-23.2146668680644,
124.614373203452)) ;
#110283 = CARTESIAN_POINT('Ctrl Pts',(-19.7080204511455,-23.2246702873648,
124.580349653203)) ;
#110284 = CARTESIAN_POINT('Ctrl Pts',(-19.9069858163038,-23.2347048380719,
124.510269234869)) ;
#110285 = CARTESIAN_POINT('Ctrl Pts',(-20.0874821253585,-23.2445497876775,
124.408959105725)) ;
#110286 = CARTESIAN_POINT('Ctrl Pts',(-20.2501516550219,-23.2545356297904,
124.276305983329)) ;
#110287 = CARTESIAN_POINT('Ctrl Pts',(-20.3867763361912,-23.2644704371595,
124.118278247021)) ;
#110288 = CARTESIAN_POINT('Ctrl Pts',(-20.4950121083751,-23.2745279788728,
123.936675423566)) ;
#110289 = CARTESIAN_POINT('Ctrl Pts',(-20.5686262721724,-23.284349576385,
123.743738384957)) ;
#110290 = CARTESIAN_POINT('Ctrl Pts',(-20.6089302655981,-23.2944058358654,
123.536219936466)) ;
#110291 = CARTESIAN_POINT('Ctrl Pts',(-20.6121814567959,-23.3043457721658,
123.327265179517)) ;
#110292 = CARTESIAN_POINT('Ctrl Pts',(-20.5798325049275,-23.3142528929102,
123.121516391018)) ;
#110293 = CARTESIAN_POINT('Ctrl Pts',(-20.5112510750128,-23.3242957988355,
122.921836997744)) ;
#110294 = CARTESIAN_POINT('Ctrl Pts',(-20.4104455696014,-23.3342035799347,
122.73955294421)) ;
#110295 = CARTESIAN_POINT('Ctrl Pts',(-20.2784539158277,-23.3442139489371,
122.575631898684)) ;
#110296 = CARTESIAN_POINT('Ctrl Pts',(-20.1194051420233,-23.3542447875059,
122.43716482541)) ;
#110297 = CARTESIAN_POINT('Ctrl Pts',(-19.942123138102,-23.3640976271456,
122.330025521725)) ;
#110298 = CARTESIAN_POINT('Ctrl Pts',(-19.7464394046845,-23.3740856283106,
122.253919465106)) ;
#110299 = CARTESIAN_POINT('Ctrl Pts',(-19.5417130313355,-23.3840144472898,
122.213180879339)) ;
#110300 = CARTESIAN_POINT('Ctrl Pts',(-19.3317876298679,-23.3940021500121,
122.208227534681)) ;
#110301 = CARTESIAN_POINT('Ctrl Pts',(-19.1232603427964,-23.4040381498147,
122.240299687688)) ;
#110302 = CARTESIAN_POINT('Ctrl Pts',(-18.9269409432071,-23.4138930196162,
122.306551166819)) ;
#110303 = CARTESIAN_POINT('Ctrl Pts',(-18.7423483508961,-23.4238924500397,
122.407064735356)) ;
#110304 = CARTESIAN_POINT('Ctrl Pts',(-18.5795334617463,-23.433787567505,
122.536604730174)) ;
#110305 = CARTESIAN_POINT('Ctrl Pts',(-18.4394363745847,-23.4438480610219,
122.695019230009)) ;
#110306 = CARTESIAN_POINT('Ctrl Pts',(-18.3311723273328,-23.4536975412231,
122.871546085858)) ;
#110307 = CARTESIAN_POINT('Ctrl Pts',(-18.2533388588761,-23.4637239914869,
123.067434642298)) ;
#110308 = CARTESIAN_POINT('Ctrl Pts',(-18.2112477394473,-23.473755281965,
123.274085618954)) ;
#110309 = CARTESIAN_POINT('Ctrl Pts',(-18.2053327705776,-23.4835966696168,
123.480899299161)) ;
#110310 = CARTESIAN_POINT('Ctrl Pts',(-18.235505133088,-23.4936000705081,
123.689005373139)) ;
#110311 = CARTESIAN_POINT('Ctrl Pts',(-18.3013289225385,-23.5035844532992,
123.888359313208)) ;
#110312 = CARTESIAN_POINT('Ctrl Pts',(-18.4014615852489,-23.5136235433126,
124.074123169983)) ;
#110313 = CARTESIAN_POINT('Ctrl Pts',(-18.5296028532157,-23.5234693522218,
124.236698626146)) ;
#110314 = CARTESIAN_POINT('Ctrl Pts',(-18.6858817598592,-23.5334537750408,
124.376783929551)) ;
#110315 = CARTESIAN_POINT('Ctrl Pts',(-18.8633136513147,-23.543393400282,
124.487216451084)) ;
#110316 = CARTESIAN_POINT('Ctrl Pts',(-19.0591532249286,-23.5534330898006,
124.565884907563)) ;
#110317 = CARTESIAN_POINT('Ctrl Pts',(-19.2625668267101,-23.5633212782192,
124.608805756136)) ;
#110318 = CARTESIAN_POINT('Ctrl Pts',(-19.4724402524542,-23.5733108042213,
124.616219808974)) ;
#110319 = CARTESIAN_POINT('Ctrl Pts',(-19.6797460656949,-23.5832693055765,
124.587011177109)) ;
#110320 = CARTESIAN_POINT('Ctrl Pts',(-19.8778294184368,-23.5931688995801,
124.523118158871)) ;
#110321 = CARTESIAN_POINT('Ctrl Pts',(-20.0645009151981,-23.6032167877014,
124.424293933469)) ;
#110322 = CARTESIAN_POINT('Ctrl Pts',(-20.2287913693335,-23.613112212947,
124.296622733357)) ;
#110323 = CARTESIAN_POINT('Ctrl Pts',(-20.3707437807528,-23.6231736036475,
124.139840437194)) ;
#110324 = CARTESIAN_POINT('Ctrl Pts',(-20.4809539118127,-23.6330191873342,
123.964623075631)) ;
#110325 = CARTESIAN_POINT('Ctrl Pts',(-20.5606419765024,-23.6429821606434,
123.770937332769)) ;
#110326 = CARTESIAN_POINT('Ctrl Pts',(-20.6055037734853,-23.6530078274692,
123.56498225823)) ;
#110327 = CARTESIAN_POINT('Ctrl Pts',(-20.6139419352035,-23.6629223053355,
123.356726806991)) ;
#110328 = CARTESIAN_POINT('Ctrl Pts',(-20.5862956208339,-23.6729108200105,
123.14854744861)) ;
#110329 = CARTESIAN_POINT('Ctrl Pts',(-20.5221502827436,-23.6829549309259,
122.947387448466)) ;
#110330 = CARTESIAN_POINT('Ctrl Pts',(-20.4265837612512,-23.6927830685205,
122.764165574932)) ;
#110331 = CARTESIAN_POINT('Ctrl Pts',(-20.2975940227322,-23.7028596365794,
122.596176929257)) ;
#110332 = CARTESIAN_POINT('Ctrl Pts',(-20.1448810386907,-23.7127117984836,
122.456185671951)) ;
#110333 = CARTESIAN_POINT('Ctrl Pts',(-19.9664286165022,-23.7227847604404,
122.342238453517)) ;
#110334 = CARTESIAN_POINT('Ctrl Pts',(-19.7753138611136,-23.7326273224433,
122.26287251808)) ;
#110335 = CARTESIAN_POINT('Ctrl Pts',(-19.5706729532653,-23.7426077589371,
122.216584699147)) ;
#110336 = CARTESIAN_POINT('Ctrl Pts',(-19.3602825510398,-23.7526260642615,
122.206899947135)) ;
#110337 = CARTESIAN_POINT('Ctrl Pts',(-19.1541287161243,-23.762510028181,
122.233106229601)) ;
#110338 = CARTESIAN_POINT('Ctrl Pts',(-18.9520644866515,-23.7725759049195,
122.29588185769)) ;
#110339 = CARTESIAN_POINT('Ctrl Pts',(-18.7681068289641,-23.7824150057804,
122.390503386169)) ;
#110340 = CARTESIAN_POINT('Ctrl Pts',(-18.599825755944,-23.7924480886462,
122.517654550901)) ;
#110341 = CARTESIAN_POINT('Ctrl Pts',(-18.4567081464835,-23.8024697739216,
122.672293715682)) ;
#110342 = CARTESIAN_POINT('Ctrl Pts',(-18.3441156236053,-23.8123364690201,
122.846486737125)) ;
#110343 = CARTESIAN_POINT('Ctrl Pts',(-18.2621969240914,-23.8222963587547,
123.039195128774)) ;
#110344 = CARTESIAN_POINT('Ctrl Pts',(-18.2149476763688,-23.8323313465801,
123.244789425331)) ;
#110345 = CARTESIAN_POINT('Ctrl Pts',(-18.203926343966,-23.8422180506544,
123.452375693097)) ;
#110346 = CARTESIAN_POINT('Ctrl Pts',(-18.2296160957685,-23.8522831948873,
123.662377221486)) ;
#110347 = CARTESIAN_POINT('Ctrl Pts',(-18.2898091826048,-23.8621224856159,
123.860311225393)) ;
#110348 = CARTESIAN_POINT('Ctrl Pts',(-18.3852966084127,-23.8721850430543,
124.049053763556)) ;
#110349 = CARTESIAN_POINT('Ctrl Pts',(-18.5102198967292,-23.8820820943064,
124.215459659652)) ;
#110350 = CARTESIAN_POINT('Ctrl Pts',(-18.6621744689301,-23.8920133010547,
124.358634148045)) ;
#110351 = CARTESIAN_POINT('Ctrl Pts',(-18.8387600546237,-23.9020554852735,
124.474338026162)) ;
#110352 = CARTESIAN_POINT('Ctrl Pts',(-19.0296995508452,-23.9119421133844,
124.556477302136)) ;
#110353 = CARTESIAN_POINT('Ctrl Pts',(-19.2340821692286,-23.9219353859168,
124.605065390389)) ;
#110354 = CARTESIAN_POINT('Ctrl Pts',(-19.442801812465,-23.9318804614583,
124.617298377842)) ;
#110355 = CARTESIAN_POINT('Ctrl Pts',(-19.6506236910629,-23.9418300121866,
124.593497792637)) ;
#110356 = CARTESIAN_POINT('Ctrl Pts',(-19.8528899890465,-23.9518693470345,
124.533250027574)) ;
#110357 = CARTESIAN_POINT('Ctrl Pts',(-20.0388518149153,-23.9617554859785,
124.44039783482)) ;
#110358 = CARTESIAN_POINT('Ctrl Pts',(-20.2078844344468,-23.9717535989522,
124.315505613017)) ;
#110359 = CARTESIAN_POINT('Ctrl Pts',(-20.3516543828328,-23.9816733613046,
124.164406301395)) ;
#110360 = CARTESIAN_POINT('Ctrl Pts',(-20.4684314444969,-23.9917127569173,
123.988608412845)) ;
#110361 = CARTESIAN_POINT('Ctrl Pts',(-20.5517608746673,-24.0016219427055,
123.79767674532)) ;
#110362 = CARTESIAN_POINT('Ctrl Pts',(-20.6013705954172,-24.011557126863,
123.594783343307)) ;
#110363 = CARTESIAN_POINT('Ctrl Pts',(-20.6149354137884,-24.0215981842489,
123.384130130513)) ;
#110364 = CARTESIAN_POINT('Ctrl Pts',(-20.5922202938844,-24.0314853422822,
123.177504905946)) ;
#110365 = CARTESIAN_POINT('Ctrl Pts',(-20.5336967238571,-24.0414776219581,
122.975767602112)) ;
#110366 = CARTESIAN_POINT('Ctrl Pts',(-20.4413760381456,-24.0514261390032,
122.788083918421)) ;
#110367 = CARTESIAN_POINT('Ctrl Pts',(-20.3182709023201,-24.0613629165736,
122.619329904814)) ;
#110368 = CARTESIAN_POINT('Ctrl Pts',(-20.1671857819634,-24.0713459527205,
122.473618394258)) ;
#110369 = CARTESIAN_POINT('Ctrl Pts',(-19.9918622669936,-24.0813897043143,
122.355989336053)) ;
#110370 = CARTESIAN_POINT('Ctrl Pts',(-19.8030626681569,-24.0912182335268,
122.271955592122)) ;
#110371 = CARTESIAN_POINT('Ctrl Pts',(-19.5976019317903,-24.1012935944355,
122.22063139524)) ;
#110372 = CARTESIAN_POINT('Ctrl Pts',(-19.390857925714,-24.1111501933227,
122.206005511593)) ;
#110373 = CARTESIAN_POINT('Ctrl Pts',(-19.1804602082013,-24.1212131873406,
122.227722199197)) ;
#110374 = CARTESIAN_POINT('Ctrl Pts',(-18.9807008139895,-24.1310911216301,
122.284611091076)) ;
#110375 = CARTESIAN_POINT('Ctrl Pts',(-18.7914583071917,-24.1410917691882,
122.37612289784)) ;
#110376 = CARTESIAN_POINT('Ctrl Pts',(-18.6222389478431,-24.1510096156262,
122.498001096716)) ;
#110377 = CARTESIAN_POINT('Ctrl Pts',(-18.4748893231177,-24.1610607326319,
122.649408018513)) ;
#110378 = CARTESIAN_POINT('Ctrl Pts',(-18.3579656374133,-24.1709314679425,
122.820892393194)) ;
#110379 = CARTESIAN_POINT('Ctrl Pts',(-18.27085472596,-24.1810021751855,123.013821879065)) ;
#110380 = CARTESIAN_POINT('Ctrl Pts',(-18.2196956072974,-24.1908351826373,
123.214131850173)) ;
#110381 = CARTESIAN_POINT('Ctrl Pts',(-18.203182383299,-24.2008656749396,
123.424349246205)) ;
#110382 = CARTESIAN_POINT('Ctrl Pts',(-18.2240367900546,-24.210897270013,
123.634223367364)) ;
#110383 = CARTESIAN_POINT('Ctrl Pts',(-18.2794462997399,-24.2207269691513,
123.833292653055)) ;
#110384 = CARTESIAN_POINT('Ctrl Pts',(-18.369470470645,-24.2307164190328,
124.023035501007)) ;
#110385 = CARTESIAN_POINT('Ctrl Pts',(-18.4921668210782,-24.2407602768485,
124.194879674593)) ;
#110386 = CARTESIAN_POINT('Ctrl Pts',(-18.6392056274176,-24.2505819674387,
124.339844804999)) ;
#110387 = CARTESIAN_POINT('Ctrl Pts',(-18.8125807545781,-24.2606170579791,
124.460042933258)) ;
#110388 = CARTESIAN_POINT('Ctrl Pts',(-19.0042411114035,-24.2706415769618,
124.547716707311)) ;
#110389 = CARTESIAN_POINT('Ctrl Pts',(-19.204744921899,-24.280501422372,124.600243463678)) ;
#110390 = CARTESIAN_POINT('Ctrl Pts',(-19.4133882030251,-24.2904611986877,
124.617906639724)) ;
#110391 = CARTESIAN_POINT('Ctrl Pts',(-19.6233285317806,-24.3004893960023,
124.598654710765)) ;
#110392 = CARTESIAN_POINT('Ctrl Pts',(-19.8243735365458,-24.3103969382926,
124.544142550926)) ;
#110393 = CARTESIAN_POINT('Ctrl Pts',(-20.0152813405617,-24.3204295888565,
124.454510616187)) ;
#110394 = CARTESIAN_POINT('Ctrl Pts',(-20.1852235288111,-24.3303135452832,
124.334929781957)) ;
#110395 = CARTESIAN_POINT('Ctrl Pts',(-20.3337579658419,-24.340303246645,
124.186453407632)) ;
#110396 = CARTESIAN_POINT('Ctrl Pts',(-20.454504189754,-24.350344241921,124.01330338354)) ;
#110397 = CARTESIAN_POINT('Ctrl Pts',(-20.5418176551072,-24.3601771311894,
123.825934135748)) ;
#110398 = CARTESIAN_POINT('Ctrl Pts',(-20.5967254094152,-24.3701702895568,
123.623152066709)) ;
#110399 = CARTESIAN_POINT('Ctrl Pts',(-20.6152263746241,-24.3802023319089,
123.413049979044)) ;
#110400 = CARTESIAN_POINT('Ctrl Pts',(-20.597526063301,-24.3900675758674,
123.206418993137)) ;
#110401 = CARTESIAN_POINT('Ctrl Pts',(-20.5442637117006,-24.4000294671134,
123.003868682479)) ;
#110402 = CARTESIAN_POINT('Ctrl Pts',(-20.4556941373607,-24.4100643671318,
122.812407533436)) ;
#110403 = CARTESIAN_POINT('Ctrl Pts',(-20.3372857157704,-24.4199494475464,
122.641592449798)) ;
#110404 = CARTESIAN_POINT('Ctrl Pts',(-20.1883750406009,-24.4300146196713,
122.491295787956)) ;
#110405 = CARTESIAN_POINT('Ctrl Pts',(-20.0194007925051,-24.4398618543947,
122.371657218722)) ;
#110406 = CARTESIAN_POINT('Ctrl Pts',(-19.8289741759901,-24.4498926657125,
122.281093232715)) ;
#110407 = CARTESIAN_POINT('Ctrl Pts',(-19.6259933636175,-24.459902281626,
122.225493674487)) ;
#110408 = CARTESIAN_POINT('Ctrl Pts',(-19.4185733943728,-24.4698130610297,
122.205975379152)) ;
#110409 = CARTESIAN_POINT('Ctrl Pts',(-19.2104563499327,-24.4797423268187,
122.222280280898)) ;
#110410 = CARTESIAN_POINT('Ctrl Pts',(-19.0060856933986,-24.4897850201314,
122.275238157231)) ;
#110411 = CARTESIAN_POINT('Ctrl Pts',(-18.8169262806703,-24.4996715528261,
122.361399226204)) ;
#110412 = CARTESIAN_POINT('Ctrl Pts',(-18.6435709470347,-24.5096646979294,
122.480058099008)) ;
#110413 = CARTESIAN_POINT('Ctrl Pts',(-18.4942123914404,-24.5196103786034,
122.62638216693)) ;
#110414 = CARTESIAN_POINT('Ctrl Pts',(-18.372156381268,-24.5295576362302,
122.796203012087)) ;
#110415 = CARTESIAN_POINT('Ctrl Pts',(-18.2807444939529,-24.5396055383516,
122.986630967248)) ;
#110416 = CARTESIAN_POINT('Ctrl Pts',(-18.2247509265294,-24.5494532439733,
123.185945976272)) ;
#110417 = CARTESIAN_POINT('Ctrl Pts',(-18.2033210095578,-24.5594147106074,
123.394260452559)) ;
#110418 = CARTESIAN_POINT('Ctrl Pts',(-18.2187746637337,-24.5694442638756,
123.604554053366)) ;
#110419 = CARTESIAN_POINT('Ctrl Pts',(-18.2697576888872,-24.579351155903,
123.806494507573)) ;
#110420 = CARTESIAN_POINT('Ctrl Pts',(-18.3550027451092,-24.5892988000161,
123.997444662551)) ;
#110421 = CARTESIAN_POINT('Ctrl Pts',(-18.4726412751785,-24.5992988430449,
124.171715744092)) ;
#110422 = CARTESIAN_POINT('Ctrl Pts',(-18.6195572279532,-24.6093376090389,
124.323206672354)) ;
#110423 = CARTESIAN_POINT('Ctrl Pts',(-18.7866725870464,-24.6191626710612,
124.444626473713)) ;
#110424 = CARTESIAN_POINT('Ctrl Pts',(-18.9764902505804,-24.6292172183875,
124.537602583139)) ;
#110425 = CARTESIAN_POINT('Ctrl Pts',(-19.1774391836388,-24.6391604618367,
124.595216990383)) ;
#110426 = CARTESIAN_POINT('Ctrl Pts',(-19.3844082519006,-24.6490626334446,
124.617617851746)) ;
#110427 = CARTESIAN_POINT('Ctrl Pts',(-19.5952632025592,-24.6591154690548,
124.603401290191)) ;
#110428 = CARTESIAN_POINT('Ctrl Pts',(-19.7968137497714,-24.6689885267404,
124.553771093963)) ;
#110429 = CARTESIAN_POINT('Ctrl Pts',(-19.989234791442,-24.678983788266,124.46934100081)) ;
#110430 = CARTESIAN_POINT('Ctrl Pts',(-20.1643959320374,-24.6890091576865,
124.352113839791)) ;
#110431 = CARTESIAN_POINT('Ctrl Pts',(-20.3146769999965,-24.6988989902131,
124.208421467969)) ;
#110432 = CARTESIAN_POINT('Ctrl Pts',(-20.4803794017226,-24.7121969610225,
123.983284046882)) ;
#110433 = CARTESIAN_POINT('Ctrl Pts',(-20.583172824706,-24.7253953561317,
123.722088064228)) ;
#110434 = CARTESIAN_POINT('Ctrl Pts',(-20.6148627591486,-24.7387907984112,
123.442321742943)) ;
#110435 = CARTESIAN_POINT('Ctrl Pts',(-20.6022377853291,-24.7486666366501,
123.235043687605)) ;
#110436 = CARTESIAN_POINT('Ctrl Pts',(-20.5530156986825,-24.7587280392479,
123.02936454998)) ;
#110437 = CARTESIAN_POINT('Ctrl Pts',(-20.4705008278291,-24.768593096183,
122.839056333103)) ;
#110438 = CARTESIAN_POINT('Ctrl Pts',(-20.354842376879,-24.7786051921318,
122.663232317905)) ;
#110439 = CARTESIAN_POINT('Ctrl Pts',(-20.1632024974996,-24.7918825012772,
122.460204444533)) ;
#110440 = CARTESIAN_POINT('Ctrl Pts',(-19.8630432768577,-24.8084815267845,
122.274649337892)) ;
#110441 = CARTESIAN_POINT('Ctrl Pts',(-19.5174930616311,-24.8250805748176,
122.202608401859)) ;
#110442 = CARTESIAN_POINT('Ctrl Pts',(-19.2395187066018,-24.8383239868485,
122.217832443928)) ;
#110443 = CARTESIAN_POINT('Ctrl Pts',(-19.033997275374,-24.8483614145369,
122.265684107542)) ;
#110444 = CARTESIAN_POINT('Ctrl Pts',(-18.842496877025,-24.8582657164925,
122.347427319138)) ;
#110445 = CARTESIAN_POINT('Ctrl Pts',(-18.608465987776,-24.8715325564677,
122.499206192217)) ;
#110446 = CARTESIAN_POINT('Ctrl Pts',(-18.3717401678559,-24.8881587545576,
122.761724130708)) ;
#110447 = CARTESIAN_POINT('Ctrl Pts',(-18.212362203183,-24.9080778699411,
123.154130994214)) ;
#110448 = CARTESIAN_POINT('Ctrl Pts',(-18.1988264560947,-24.9246842930753,
123.507013414508)) ;
#110449 = CARTESIAN_POINT('Ctrl Pts',(-18.2607645224499,-24.937980513571,
123.779547310328)) ;
#110450 = CARTESIAN_POINT('Ctrl Pts',(-18.3683294666878,-24.9512493459124,
124.037013938642)) ;
#110451 = CARTESIAN_POINT('Ctrl Pts',(-18.5855216636615,-24.9679405939455,
124.317571827094)) ;
#110452 = CARTESIAN_POINT('Ctrl Pts',(-18.9413374717823,-24.9877503256183,
124.543094069177)) ;
#110453 = CARTESIAN_POINT('Ctrl Pts',(-19.3559853576268,-25.0077279329469,
124.635225003851)) ;
#110454 = CARTESIAN_POINT('Ctrl Pts',(-19.7759665018772,-25.0276542420047,
124.579702340069)) ;
#110455 = CARTESIAN_POINT('Ctrl Pts',(-20.1505529324183,-25.0474711021694,
124.386507876771)) ;
#110456 = CARTESIAN_POINT('Ctrl Pts',(-20.4401485253289,-25.0675709177634,
124.072406620765)) ;
#110457 = CARTESIAN_POINT('Ctrl Pts',(-20.6026714408021,-25.087327881646,
123.68484227443)) ;
#110458 = CARTESIAN_POINT('Ctrl Pts',(-20.6242932351504,-25.1073648077154,
123.259498088641)) ;
#110459 = CARTESIAN_POINT('Ctrl Pts',(-20.4998013082234,-25.127234390097,
122.855661485121)) ;
#110460 = CARTESIAN_POINT('Ctrl Pts',(-20.24549215291,-25.1471389618501,122.517464742249)) ;
#110461 = CARTESIAN_POINT('Ctrl Pts',(-19.8900326876619,-25.1670915640486,
122.285744324432)) ;
#110462 = CARTESIAN_POINT('Ctrl Pts',(-19.4778520384419,-25.1870010550189,
122.189613357775)) ;
#110463 = CARTESIAN_POINT('Ctrl Pts',(-19.0585077529647,-25.2068524237183,
122.238603659123)) ;
#110464 = CARTESIAN_POINT('Ctrl Pts',(-18.6771571783455,-25.2269326198543,
122.430408261582)) ;
#110465 = CARTESIAN_POINT('Ctrl Pts',(-18.3880842308716,-25.2467335634297,
122.736659447663)) ;
#110466 = CARTESIAN_POINT('Ctrl Pts',(-18.2185194959118,-25.2667175399392,
123.126200095586)) ;
#110467 = CARTESIAN_POINT('Ctrl Pts',(-18.1928057162493,-25.2866335029148,
123.548884616493)) ;
#110468 = CARTESIAN_POINT('Ctrl Pts',(-18.3115038619705,-25.3065039377368,
123.954453948555)) ;
#110469 = CARTESIAN_POINT('Ctrl Pts',(-18.5641908604236,-25.3265542229698,
124.297667067177)) ;
#110470 = CARTESIAN_POINT('Ctrl Pts',(-18.9138516524025,-25.3463281917291,
124.531454945539)) ;
#110471 = CARTESIAN_POINT('Ctrl Pts',(-19.3277338141013,-25.3663846498487,
124.633528228989)) ;
#110472 = CARTESIAN_POINT('Ctrl Pts',(-19.7463497564962,-25.3861795328397,
124.588652941236)) ;
#110473 = CARTESIAN_POINT('Ctrl Pts',(-20.1281401460027,-25.406146188142,
124.403184513832)) ;
#110474 = CARTESIAN_POINT('Ctrl Pts',(-20.4232242232993,-25.4261051582185,
124.098070449542)) ;
#110475 = CARTESIAN_POINT('Ctrl Pts',(-20.5961678544623,-25.4460012458087,
123.712015075938)) ;
#110476 = CARTESIAN_POINT('Ctrl Pts',(-20.6274946135136,-25.4658994157202,
123.290123175569)) ;
#110477 = CARTESIAN_POINT('Ctrl Pts',(-20.5133433762152,-25.4858052510873,
122.882522983055)) ;
#110478 = CARTESIAN_POINT('Ctrl Pts',(-20.2664372745077,-25.5057551760253,
122.53764350913)) ;
#110479 = CARTESIAN_POINT('Ctrl Pts',(-19.9180604263204,-25.5256343659356,
122.29819791607)) ;
#110480 = CARTESIAN_POINT('Ctrl Pts',(-19.5069178349822,-25.5456156902162,
122.191266262627)) ;
#110481 = CARTESIAN_POINT('Ctrl Pts',(-19.0849510432749,-25.5655454744246,
122.231183049216)) ;
#110482 = CARTESIAN_POINT('Ctrl Pts',(-18.7022565000659,-25.5854654638154,
122.412448802774)) ;
#110483 = CARTESIAN_POINT('Ctrl Pts',(-18.4045387398408,-25.6053206591694,
122.711916513803)) ;
#110484 = CARTESIAN_POINT('Ctrl Pts',(-18.225635629765,-25.6253666608287,
123.098678174589)) ;
#110485 = CARTESIAN_POINT('Ctrl Pts',(-18.195689723047,-25.6418664080385,
123.448307091214)) ;
#110486 = CARTESIAN_POINT('Ctrl Pts',(-18.244756749659,-25.6552550124866,
123.725454292906)) ;
#110487 = CARTESIAN_POINT('Ctrl Pts',(-18.3158066758108,-25.6651168408215,
123.920229417609)) ;
#110488 = CARTESIAN_POINT('Ctrl Pts',(-18.4201303421128,-25.6750829835791,
124.101948787489)) ;
#110489 = CARTESIAN_POINT('Ctrl Pts',(-18.6004853620919,-25.688444729704,
124.317180416273)) ;
#110490 = CARTESIAN_POINT('Ctrl Pts',(-18.8864936960802,-25.7048990586591,
124.519010382514)) ;
#110491 = CARTESIAN_POINT('Ctrl Pts',(-19.2302505976413,-25.7216663037074,
124.612811052732)) ;
#110492 = CARTESIAN_POINT('Ctrl Pts',(-19.5076063857434,-25.7348528689815,
124.613710719248)) ;
#110493 = CARTESIAN_POINT('Ctrl Pts',(-19.7145916605731,-25.7448423277261,
124.578551181133)) ;
#110494 = CARTESIAN_POINT('Ctrl Pts',(-19.91173393572,-25.7547961002072,124.508243089248)) ;
#110495 = CARTESIAN_POINT('Ctrl Pts',(-20.0952486511012,-25.7648439167398,
124.403684620192)) ;
#110496 = CARTESIAN_POINT('Ctrl Pts',(-20.2546739861016,-25.7746854498623,
124.271776251033)) ;
#110497 = CARTESIAN_POINT('Ctrl Pts',(-20.3910509367533,-25.784671692082,
124.112206188903)) ;
#110498 = CARTESIAN_POINT('Ctrl Pts',(-20.4972454477229,-25.7946083155069,
123.932272415258)) ;
#110499 = CARTESIAN_POINT('Ctrl Pts',(-20.5713011055568,-25.8046581928899,
123.734419022057)) ;
#110500 = CARTESIAN_POINT('Ctrl Pts',(-20.6092722385274,-25.8145086316675,
123.530827063093)) ;
#110501 = CARTESIAN_POINT('Ctrl Pts',(-20.6118885254664,-25.8244806456362,
123.321226640003)) ;
#110502 = CARTESIAN_POINT('Ctrl Pts',(-20.5779551204334,-25.8344758142623,
123.113820960216)) ;
#110503 = CARTESIAN_POINT('Ctrl Pts',(-20.5080341605627,-25.8445096975235,
122.914819867729)) ;
#110504 = CARTESIAN_POINT('Ctrl Pts',(-20.4067160569946,-25.8543655675869,
122.734062504968)) ;
#110505 = CARTESIAN_POINT('Ctrl Pts',(-20.2739494064753,-25.864363113504,
122.571154437494)) ;
#110506 = CARTESIAN_POINT('Ctrl Pts',(-20.1163559570364,-25.8742712404033,
122.434931525575)) ;
#110507 = CARTESIAN_POINT('Ctrl Pts',(-19.9358437787201,-25.8842816119255,
122.326724423727)) ;
#110508 = CARTESIAN_POINT('Ctrl Pts',(-19.7387398262382,-25.8943120546729,
122.251799641665)) ;
#110509 = CARTESIAN_POINT('Ctrl Pts',(-19.5354577915131,-25.9041600072262,
122.212477682683)) ;
#110510 = CARTESIAN_POINT('Ctrl Pts',(-19.3239607884795,-25.9142226762471,
122.208810515714)) ;
#110511 = CARTESIAN_POINT('Ctrl Pts',(-19.1185179458694,-25.9241170517111,
122.241520754432)) ;
#110512 = CARTESIAN_POINT('Ctrl Pts',(-18.9207930186115,-25.9340588500292,
122.309186599903)) ;
#110513 = CARTESIAN_POINT('Ctrl Pts',(-18.7366171869378,-25.9440613437565,
122.410727695288)) ;
#110514 = CARTESIAN_POINT('Ctrl Pts',(-18.572582561361,-25.9540961422634,
122.543364268059)) ;
#110515 = CARTESIAN_POINT('Ctrl Pts',(-18.4364115519052,-25.9639410262428,
122.699248360137)) ;
#110516 = CARTESIAN_POINT('Ctrl Pts',(-18.327528703322,-25.9739268830608,
122.878699708157)) ;
#110517 = CARTESIAN_POINT('Ctrl Pts',(-18.2516825622591,-25.9838616972356,
123.073344235732)) ;
#110518 = CARTESIAN_POINT('Ctrl Pts',(-18.210478331982,-25.9939191970209,
123.280700166032)) ;
#110519 = CARTESIAN_POINT('Ctrl Pts',(-18.2056945124196,-26.0037409554392,
123.487151328553)) ;
#110520 = CARTESIAN_POINT('Ctrl Pts',(-18.2371725213672,-26.0137966132232,
123.696178603444)) ;
#110521 = CARTESIAN_POINT('Ctrl Pts',(-18.3040751977876,-26.0237387954033,
123.894209457018)) ;
#110522 = CARTESIAN_POINT('Ctrl Pts',(-18.4034096181746,-26.033644004098,
124.077224976143)) ;
#110523 = CARTESIAN_POINT('Ctrl Pts',(-18.5348523658315,-26.0436857950604,
124.242418104981)) ;
#110524 = CARTESIAN_POINT('Ctrl Pts',(-18.6908648185278,-26.0535935695326,
124.380437265698)) ;
#110525 = CARTESIAN_POINT('Ctrl Pts',(-18.8701258377811,-26.0636050697602,
124.490740558356)) ;
#110526 = CARTESIAN_POINT('Ctrl Pts',(-19.0663873130377,-26.0736378301529,
124.56799590781)) ;
#110527 = CARTESIAN_POINT('Ctrl Pts',(-19.2692608469735,-26.0834883992878,
124.609595331971)) ;
#110528 = CARTESIAN_POINT('Ctrl Pts',(-19.4791433316891,-26.0934770088177,
124.615814187021)) ;
#110529 = CARTESIAN_POINT('Ctrl Pts',(-19.6856930401549,-26.1034056648418,
124.585673011114)) ;
#110530 = CARTESIAN_POINT('Ctrl Pts',(-19.8851674649268,-26.1133934110196,
124.520072236)) ;
#110531 = CARTESIAN_POINT('Ctrl Pts',(-20.0709297229496,-26.1234293999554,
124.420049383132)) ;
#110532 = CARTESIAN_POINT('Ctrl Pts',(-20.2337477185959,-26.133284269769,
124.291905458098)) ;
#110533 = CARTESIAN_POINT('Ctrl Pts',(-20.3740466529306,-26.1432837110107,
124.135400902693)) ;
#110534 = CARTESIAN_POINT('Ctrl Pts',(-20.4841082757415,-26.1531787851908,
123.958835208534)) ;
#110535 = CARTESIAN_POINT('Ctrl Pts',(-20.5630967932527,-26.1632394410305,
123.76266074657)) ;
#110536 = CARTESIAN_POINT('Ctrl Pts',(-20.6060280435003,-26.1730883152261,
123.560090363843)) ;
#110537 = CARTESIAN_POINT('Ctrl Pts',(-20.6137949078894,-26.1831170271894,
123.3494013289)) ;
#110538 = CARTESIAN_POINT('Ctrl Pts',(-20.5842903249999,-26.1931464277725,
123.140622176029)) ;
#110539 = CARTESIAN_POINT('Ctrl Pts',(-20.5206537069258,-26.2029866213893,
122.943778440767)) ;
#110540 = CARTESIAN_POINT('Ctrl Pts',(-20.4225541880432,-26.2129900439645,
122.757780638879)) ;
#110541 = CARTESIAN_POINT('Ctrl Pts',(-20.2937913153936,-26.2229755810576,
122.591935898754)) ;
#110542 = CARTESIAN_POINT('Ctrl Pts',(-20.1372232102672,-26.2330165855444,
122.450378641205)) ;
#110543 = CARTESIAN_POINT('Ctrl Pts',(-19.9620904051924,-26.2428601244856,
122.340106595476)) ;
#110544 = CARTESIAN_POINT('Ctrl Pts',(-19.767926137489,-26.2528451554764,
122.260405279376)) ;
#110545 = CARTESIAN_POINT('Ctrl Pts',(-19.5637669590693,-26.2627846179984,
122.215737642416)) ;
#110546 = CARTESIAN_POINT('Ctrl Pts',(-19.352891176795,-26.2728243502222,
122.207160407152)) ;
#110547 = CARTESIAN_POINT('Ctrl Pts',(-19.1468450178501,-26.2827125305394,
122.234804767052)) ;
#110548 = CARTESIAN_POINT('Ctrl Pts',(-18.9465967029927,-26.2927020462419,
122.298069403054)) ;
#110549 = CARTESIAN_POINT('Ctrl Pts',(-18.7610267246917,-26.3026605968966,
122.394986000667)) ;
#110550 = CARTESIAN_POINT('Ctrl Pts',(-18.5957571493347,-26.3125600040016,
122.521494169074)) ;
#110551 = CARTESIAN_POINT('Ctrl Pts',(-18.4529337021753,-26.3226085904179,
122.677116958264)) ;
#110552 = CARTESIAN_POINT('Ctrl Pts',(-18.3408562457463,-26.3325014093824,
122.852362383433)) ;
#110553 = CARTESIAN_POINT('Ctrl Pts',(-18.259572512269,-26.3425725269122,
123.04781837416)) ;
#110554 = CARTESIAN_POINT('Ctrl Pts',(-18.2143416859,-26.3523882208783,123.249196790386)) ;
#110555 = CARTESIAN_POINT('Ctrl Pts',(-18.2042182872028,-26.3624545983756,
123.460536622291)) ;
#110556 = CARTESIAN_POINT('Ctrl Pts',(-18.2305738200012,-26.3723535844574,
123.667020979689)) ;
#110557 = CARTESIAN_POINT('Ctrl Pts',(-18.293243398823,-26.3824077644509,
123.868839172699)) ;
#110558 = CARTESIAN_POINT('Ctrl Pts',(-18.3880999549811,-26.3922785773836,
124.053460786974)) ;
#110559 = CARTESIAN_POINT('Ctrl Pts',(-18.5160984531023,-26.4023524782374,
124.222127159959)) ;
#110560 = CARTESIAN_POINT('Ctrl Pts',(-18.6674236319948,-26.4121726336241,
124.362634461012)) ;
#110561 = CARTESIAN_POINT('Ctrl Pts',(-18.8452192562724,-26.4222513405763,
124.477797233596)) ;
#110562 = CARTESIAN_POINT('Ctrl Pts',(-19.0359780715653,-26.4321029291151,
124.558583780994)) ;
#110563 = CARTESIAN_POINT('Ctrl Pts',(-19.2422790855532,-26.4421760456401,
124.606227046759)) ;
#110564 = CARTESIAN_POINT('Ctrl Pts',(-19.4489350530524,-26.4520185627359,
124.617041701118)) ;
#110565 = CARTESIAN_POINT('Ctrl Pts',(-19.6572651507117,-26.4619990242899,
124.592159464658)) ;
#110566 = CARTESIAN_POINT('Ctrl Pts',(-19.8587601203264,-26.4720172742807,
124.530862060285)) ;
#110567 = CARTESIAN_POINT('Ctrl Pts',(-20.0442514543082,-26.4819014344744,
124.437157740887)) ;
#110568 = CARTESIAN_POINT('Ctrl Pts',(-20.2136392704106,-26.4919665814494,
124.310379327204)) ;
#110569 = CARTESIAN_POINT('Ctrl Pts',(-20.3553383843994,-26.5018084050902,
124.159590286957)) ;
#110570 = CARTESIAN_POINT('Ctrl Pts',(-20.4713283979345,-26.5118378775511,
123.983514422778)) ;
#110571 = CARTESIAN_POINT('Ctrl Pts',(-20.5544239986158,-26.5218647328131,
123.789782324486)) ;
#110572 = CARTESIAN_POINT('Ctrl Pts',(-20.6022185669702,-26.5317079829236,
123.588438568568)) ;
#110573 = CARTESIAN_POINT('Ctrl Pts',(-20.614866181552,-26.5417564225068,
123.377573522423)) ;
#110574 = CARTESIAN_POINT('Ctrl Pts',(-20.590616600736,-26.5517059167547,
123.169813415634)) ;
#110575 = CARTESIAN_POINT('Ctrl Pts',(-20.5315083998309,-26.5616137724807,
122.970069947374)) ;
#110576 = CARTESIAN_POINT('Ctrl Pts',(-20.4370085488783,-26.5716732491306,
122.780900554702)) ;
#110577 = CARTESIAN_POINT('Ctrl Pts',(-20.3140324029055,-26.5815140585393,
122.614501427793)) ;
#110578 = CARTESIAN_POINT('Ctrl Pts',(-20.1608753383716,-26.5915762088401,
122.468618002252)) ;
#110579 = CARTESIAN_POINT('Ctrl Pts',(-19.9874570374253,-26.6014733699627,
122.353625023571)) ;
#110580 = CARTESIAN_POINT('Ctrl Pts',(-19.7963432071235,-26.6114045443667,
122.269574389895)) ;
#110581 = CARTESIAN_POINT('Ctrl Pts',(-19.5912142635546,-26.6214467480918,
122.219653873535)) ;
#110582 = CARTESIAN_POINT('Ctrl Pts',(-19.3837955264011,-26.6313333305222,
122.206165966457)) ;
#110583 = CARTESIAN_POINT('Ctrl Pts',(-19.1749362828923,-26.6413267662705,
122.228796135027)) ;
#110584 = CARTESIAN_POINT('Ctrl Pts',(-18.9741725579041,-26.6512712346287,
122.287126420661)) ;
#110585 = CARTESIAN_POINT('Ctrl Pts',(-18.7862673362354,-26.6612230508743,
122.379146706221)) ;
#110586 = CARTESIAN_POINT('Ctrl Pts',(-18.6158690282792,-26.6712604869887,
122.50360047639)) ;
#110587 = CARTESIAN_POINT('Ctrl Pts',(-18.4717243590258,-26.6811454461651,
122.653319942849)) ;
#110588 = CARTESIAN_POINT('Ctrl Pts',(-18.3542552499905,-26.691143564377,
122.827593139812)) ;
#110589 = CARTESIAN_POINT('Ctrl Pts',(-18.2693381219175,-26.701064496889,
123.018117560052)) ;
#110590 = CARTESIAN_POINT('Ctrl Pts',(-18.2181333257309,-26.7111057971111,
123.222902884654)) ;
#110591 = CARTESIAN_POINT('Ctrl Pts',(-18.2035332631008,-26.721012715501,
123.430666924453)) ;
#110592 = CARTESIAN_POINT('Ctrl Pts',(-18.224697169119,-26.7309485072101,
123.638474499806)) ;
#110593 = CARTESIAN_POINT('Ctrl Pts',(-18.2824280222144,-26.740989401788,
123.84151309244)) ;
#110594 = CARTESIAN_POINT('Ctrl Pts',(-18.3729966082461,-26.7508766035018,
124.02861623182)) ;
#110595 = CARTESIAN_POINT('Ctrl Pts',(-18.4956721144685,-26.7608688712634,
124.199126068328)) ;
#110596 = CARTESIAN_POINT('Ctrl Pts',(-18.6454908270371,-26.7708173922852,
124.345080276502)) ;
#110597 = CARTESIAN_POINT('Ctrl Pts',(-18.8179817972822,-26.7807541658629,
124.462892356275)) ;
#110598 = CARTESIAN_POINT('Ctrl Pts',(-19.0091256152341,-26.790737214004,
124.549624767018)) ;
#110599 = CARTESIAN_POINT('Ctrl Pts',(-19.2137095159906,-26.800780921614,
124.601783721585)) ;
#110600 = CARTESIAN_POINT('Ctrl Pts',(-19.4197466591261,-26.8106096147673,
124.61776558967)) ;
#110601 = CARTESIAN_POINT('Ctrl Pts',(-19.6305350011526,-26.8206843638968,
124.597381006242)) ;
#110602 = CARTESIAN_POINT('Ctrl Pts',(-19.8303786028158,-26.8305496896923,
124.54182533887)) ;
#110603 = CARTESIAN_POINT('Ctrl Pts',(-20.0207211479435,-26.8405718640493,
124.451492563277)) ;
#110604 = CARTESIAN_POINT('Ctrl Pts',(-20.1922715292697,-26.8505979172562,
124.328999953253)) ;
#110605 = CARTESIAN_POINT('Ctrl Pts',(-20.337626616102,-26.8604516141025,
124.18142447709)) ;
#110606 = CARTESIAN_POINT('Ctrl Pts',(-20.4569429153724,-26.8704110188554,
124.009361455575)) ;
#110607 = CARTESIAN_POINT('Ctrl Pts',(-20.5449154129948,-26.8804492645603,
123.817549468856)) ;
#110608 = CARTESIAN_POINT('Ctrl Pts',(-20.5977454907655,-26.8903234487224,
123.61677021684)) ;
#110609 = CARTESIAN_POINT('Ctrl Pts',(-20.6152375327223,-26.9003932318603,
123.40582454301)) ;
#110610 = CARTESIAN_POINT('Ctrl Pts',(-20.5963991070301,-26.910226486881,
123.199941655379)) ;
#110611 = CARTESIAN_POINT('Ctrl Pts',(-20.5415922646434,-26.9202569130127,
122.996324418451)) ;
#110612 = CARTESIAN_POINT('Ctrl Pts',(-20.4516896121168,-26.9302885251997,
122.805537621311)) ;
#110613 = CARTESIAN_POINT('Ctrl Pts',(-20.3328415198314,-26.9401182220543,
122.636499269653)) ;
#110614 = CARTESIAN_POINT('Ctrl Pts',(-20.1844978187328,-26.9501076639568,
122.487836302709)) ;
#110615 = CARTESIAN_POINT('Ctrl Pts',(-20.0113567846103,-26.9601515559725,
122.366974395451)) ;
#110616 = CARTESIAN_POINT('Ctrl Pts',(-19.8242790287249,-26.9699731177417,
122.279594921611)) ;
#110617 = CARTESIAN_POINT('Ctrl Pts',(-19.6206587478616,-26.9800086893659,
122.224347832925)) ;
#110618 = CARTESIAN_POINT('Ctrl Pts',(-19.4106166081929,-26.9900379636477,
122.205937744305)) ;
#110619 = CARTESIAN_POINT('Ctrl Pts',(-19.2046087115135,-26.9998718007664,
122.223368190757)) ;
#110620 = CARTESIAN_POINT('Ctrl Pts',(-19.0002654705531,-27.0099241968545,
122.277228787039)) ;
#110621 = CARTESIAN_POINT('Ctrl Pts',(-18.8106801357417,-27.0198609638051,
122.364987697976)) ;
#110622 = CARTESIAN_POINT('Ctrl Pts',(-18.6389579167766,-27.0297951987843,
122.483850800831)) ;
#110623 = CARTESIAN_POINT('Ctrl Pts',(-18.4892353613386,-27.0398189621111,
122.63214087965)) ;
#110624 = CARTESIAN_POINT('Ctrl Pts',(-18.369078593146,-27.0497053034958,
122.801728542321)) ;
#110625 = CARTESIAN_POINT('Ctrl Pts',(-18.2788245133217,-27.0596943522627,
122.991353353766)) ;
#110626 = CARTESIAN_POINT('Ctrl Pts',(-18.2229994632625,-27.0697355729601,
123.19493528438)) ;
#110627 = CARTESIAN_POINT('Ctrl Pts',(-18.2034414898905,-27.079568213138,
123.400717189936)) ;
#110628 = CARTESIAN_POINT('Ctrl Pts',(-18.2195809984065,-27.089562142446,
123.610199097045)) ;
#110629 = CARTESIAN_POINT('Ctrl Pts',(-18.2724661111922,-27.0995913501265,
123.814306157545)) ;
#110630 = CARTESIAN_POINT('Ctrl Pts',(-18.3583452819723,-27.1094671618306,
124.003345460771)) ;
#110631 = CARTESIAN_POINT('Ctrl Pts',(-18.476997564272,-27.119466388802,124.176839727171)) ;
#110632 = CARTESIAN_POINT('Ctrl Pts',(-18.6225510070377,-27.1293758699577,
124.325929138969)) ;
#110633 = CARTESIAN_POINT('Ctrl Pts',(-18.7942080268238,-27.1394291002586,
124.449191144853)) ;
#110634 = CARTESIAN_POINT('Ctrl Pts',(-18.9811891278579,-27.1492997168097,
124.539217956625)) ;
#110635 = CARTESIAN_POINT('Ctrl Pts',(-19.1838754210547,-27.1593213785417,
124.596716114534)) ;
#110636 = CARTESIAN_POINT('Ctrl Pts',(-19.3935528106593,-27.1693441917228,
124.617671266922)) ;
#110637 = CARTESIAN_POINT('Ctrl Pts',(-19.600426039293,-27.1792113561828,
124.602494375536)) ;
#110638 = CARTESIAN_POINT('Ctrl Pts',(-19.8042281735719,-27.1892047984027,
124.551440542455)) ;
#110639 = CARTESIAN_POINT('Ctrl Pts',(-19.9966297545078,-27.199236472003,
124.465075195787)) ;
#110640 = CARTESIAN_POINT('Ctrl Pts',(-20.1684257326335,-27.209102907116,
124.348824213868)) ;
#110641 = CARTESIAN_POINT('Ctrl Pts',(-20.3194677009734,-27.2190903576491,
124.203009056851)) ;
#110642 = CARTESIAN_POINT('Ctrl Pts',(-20.4424950270544,-27.2290352874771,
124.033926303457)) ;
#110643 = CARTESIAN_POINT('Ctrl Pts',(-20.5350890868499,-27.2390801825322,
123.844155121471)) ;
#110644 = CARTESIAN_POINT('Ctrl Pts',(-20.5924512107683,-27.248942244218,
123.644900786293)) ;
#110645 = CARTESIAN_POINT('Ctrl Pts',(-20.6150474433533,-27.2589339670049,
123.4360788639)) ;
#110646 = CARTESIAN_POINT('Ctrl Pts',(-20.6010482061257,-27.2688661812449,
123.227739726593)) ;
#110647 = CARTESIAN_POINT('Ctrl Pts',(-20.5515184501192,-27.2788054998106,
123.024732970121)) ;
#110648 = CARTESIAN_POINT('Ctrl Pts',(-20.4664320868568,-27.2888496745865,
122.831477496338)) ;
#110649 = CARTESIAN_POINT('Ctrl Pts',(-20.351203413317,-27.2987202286514,
122.658901128913)) ;
#110650 = CARTESIAN_POINT('Ctrl Pts',(-20.2068261870264,-27.3086852110056,
122.507099670608)) ;
#110651 = CARTESIAN_POINT('Ctrl Pts',(-20.0369859907984,-27.3187159138954,
122.382116057125)) ;
#110652 = CARTESIAN_POINT('Ctrl Pts',(-19.8507376344476,-27.3286082539206,
122.289527171008)) ;
#110653 = CARTESIAN_POINT('Ctrl Pts',(-19.648056414902,-27.3386614870806,
122.229720320401)) ;
#110654 = CARTESIAN_POINT('Ctrl Pts',(-19.4416112658404,-27.3485427315573,
122.206286392451)) ;
#110655 = CARTESIAN_POINT('Ctrl Pts',(-19.2311109166751,-27.3585758524284,
122.219090242423)) ;
#110656 = CARTESIAN_POINT('Ctrl Pts',(-19.02901808018,-27.3684570627034,122.267342539582)) ;
#110657 = CARTESIAN_POINT('Ctrl Pts',(-18.8349279304701,-27.3785191384728,
122.351381964771)) ;
#110658 = CARTESIAN_POINT('Ctrl Pts',(-18.6618829526836,-27.3883761968545,
122.465445390156)) ;
#110659 = CARTESIAN_POINT('Ctrl Pts',(-18.5089263033684,-27.3983707521435,
122.609456672092)) ;
#110660 = CARTESIAN_POINT('Ctrl Pts',(-18.3840648307091,-27.408296639679,
122.776687456522)) ;
#110661 = CARTESIAN_POINT('Ctrl Pts',(-18.2891643409132,-27.4183216596743,
122.964852260548)) ;
#110662 = CARTESIAN_POINT('Ctrl Pts',(-18.2290739236376,-27.428219036778,
123.164066885729)) ;
#110663 = CARTESIAN_POINT('Ctrl Pts',(-18.203800317435,-27.4382092738588,
123.372572776699)) ;
#110664 = CARTESIAN_POINT('Ctrl Pts',(-18.2155715307985,-27.4482458866676,
123.583242432194)) ;
#110665 = CARTESIAN_POINT('Ctrl Pts',(-18.2625214370724,-27.4580957700856,
123.784933411613)) ;
#110666 = CARTESIAN_POINT('Ctrl Pts',(-18.3446461197677,-27.4680993869881,
123.978520605294)) ;
#110667 = CARTESIAN_POINT('Ctrl Pts',(-18.4591002816257,-27.4780887987532,
124.154640815134)) ;
#110668 = CARTESIAN_POINT('Ctrl Pts',(-18.602874195874,-27.4881075600981,
124.308533582263)) ;
#110669 = CARTESIAN_POINT('Ctrl Pts',(-18.8247600084296,-27.5013262354791,
124.475933882896)) ;
#110670 = CARTESIAN_POINT('Ctrl Pts',(-19.0869288411818,-27.5146365427238,
124.582416106165)) ;
#110671 = CARTESIAN_POINT('Ctrl Pts',(-19.3630784764609,-27.5278742089498,
124.616824793686)) ;
#110672 = CARTESIAN_POINT('Ctrl Pts',(-19.5713975017315,-27.5377939043605,
124.60695201127)) ;
#110673 = CARTESIAN_POINT('Ctrl Pts',(-19.7774918625085,-27.5478467713591,
124.560209602054)) ;
#110674 = CARTESIAN_POINT('Ctrl Pts',(-19.9686338251995,-27.5577021796884,
124.480202503589)) ;
#110675 = CARTESIAN_POINT('Ctrl Pts',(-20.1463794715423,-27.5677408113649,
124.366454939727)) ;
#110676 = CARTESIAN_POINT('Ctrl Pts',(-20.3519681993946,-27.581042993632,
124.176828926503)) ;
#110677 = CARTESIAN_POINT('Ctrl Pts',(-20.5406264713926,-27.5975880067148,
123.879925090862)) ;
#110678 = CARTESIAN_POINT('Ctrl Pts',(-20.6172144359266,-27.614240022791,
123.534231246347)) ;
#110679 = CARTESIAN_POINT('Ctrl Pts',(-20.6051273373897,-27.6274631136963,
123.256522981013)) ;
#110680 = CARTESIAN_POINT('Ctrl Pts',(-20.5603980530631,-27.6374240732556,
123.051937897148)) ;
#110681 = CARTESIAN_POINT('Ctrl Pts',(-20.4800781630855,-27.6474488700067,
122.857100247904)) ;
#110682 = CARTESIAN_POINT('Ctrl Pts',(-20.3314044135135,-27.6606733174025,
122.622123937831)) ;
#110683 = CARTESIAN_POINT('Ctrl Pts',(-20.0717196318595,-27.6773071021016,
122.382102116417)) ;
#110684 = CARTESIAN_POINT('Ctrl Pts',(-19.6815155154758,-27.6972097688266,
122.218215389868)) ;
#110685 = CARTESIAN_POINT('Ctrl Pts',(-19.2589566433352,-27.7171099966084,
122.196772525716)) ;
#110686 = CARTESIAN_POINT('Ctrl Pts',(-18.8539833359904,-27.7370274841399,
122.32064842801)) ;
#110687 = CARTESIAN_POINT('Ctrl Pts',(-18.5152100703713,-27.7569570099568,
122.575243993039)) ;
#110688 = CARTESIAN_POINT('Ctrl Pts',(-18.283337647524,-27.7769192778431,
122.930790683589)) ;
#110689 = CARTESIAN_POINT('Ctrl Pts',(-18.1870487801957,-27.7968094727953,
123.342544982765)) ;
#110690 = CARTESIAN_POINT('Ctrl Pts',(-18.2360062167125,-27.8166997175416,
123.76271600587)) ;
#110691 = CARTESIAN_POINT('Ctrl Pts',(-18.4278813702986,-27.836774090104,
124.143929279547)) ;
#110692 = CARTESIAN_POINT('Ctrl Pts',(-18.7338457780182,-27.8565594674643,
124.43274359205)) ;
#110693 = CARTESIAN_POINT('Ctrl Pts',(-19.1228314887895,-27.8765213415315,
124.602478439993)) ;
#110694 = CARTESIAN_POINT('Ctrl Pts',(-19.5468862353794,-27.896501317022,
124.62829701089)) ;
#110695 = CARTESIAN_POINT('Ctrl Pts',(-19.9511281685244,-27.9163137468999,
124.509652697272)) ;
#110696 = CARTESIAN_POINT('Ctrl Pts',(-20.2937312269528,-27.9362938549902,
124.258579137099)) ;
#110697 = CARTESIAN_POINT('Ctrl Pts',(-20.5290187527357,-27.9561882385874,
123.906931267207)) ;
#110698 = CARTESIAN_POINT('Ctrl Pts',(-20.6306760326366,-27.9761151665647,
123.495704172077)) ;
#110699 = CARTESIAN_POINT('Ctrl Pts',(-20.5865144561214,-27.9960100238659,
123.07489936553)) ;
#110700 = CARTESIAN_POINT('Ctrl Pts',(-20.3997370188874,-28.0160492174695,
122.691977689567)) ;
#110701 = CARTESIAN_POINT('Ctrl Pts',(-20.0964199669085,-28.0358891853803,
122.39872994005)) ;
#110702 = CARTESIAN_POINT('Ctrl Pts',(-19.7103073433732,-28.0558040023444,
122.224973259188)) ;
#110703 = CARTESIAN_POINT('Ctrl Pts',(-19.2874715894312,-28.0757462477406,
122.19365698923)) ;
#110704 = CARTESIAN_POINT('Ctrl Pts',(-18.8804519053716,-28.0956182958551,
122.307451334295)) ;
#110705 = CARTESIAN_POINT('Ctrl Pts',(-18.5346616873186,-28.1156293608092,
122.555147151279)) ;
#110706 = CARTESIAN_POINT('Ctrl Pts',(-18.2958175051763,-28.1354408851129,
122.902370223066)) ;
#110707 = CARTESIAN_POINT('Ctrl Pts',(-18.188623677032,-28.1555360970762,
123.315810290643)) ;
#110708 = CARTESIAN_POINT('Ctrl Pts',(-18.2284238750421,-28.175316820996,
123.734683554714)) ;
#110709 = CARTESIAN_POINT('Ctrl Pts',(-18.4096666886819,-28.1953078966388,
124.118996145647)) ;
#110710 = CARTESIAN_POINT('Ctrl Pts',(-18.7099298896078,-28.2151898356818,
124.416746694773)) ;
#110711 = CARTESIAN_POINT('Ctrl Pts',(-19.0947697828435,-28.2351424401851,
124.595141717737)) ;
#110712 = CARTESIAN_POINT('Ctrl Pts',(-19.5163602730384,-28.2550413089158,
124.63141064558)) ;
#110713 = CARTESIAN_POINT('Ctrl Pts',(-19.92492807576,-28.2749347087253,124.522202021035)) ;
#110714 = CARTESIAN_POINT('Ctrl Pts',(-20.2724837530038,-28.2948438395654,
124.280378861559)) ;
#110715 = CARTESIAN_POINT('Ctrl Pts',(-20.5176133990071,-28.3148759393289,
123.932100895011)) ;
#110716 = CARTESIAN_POINT('Ctrl Pts',(-20.6098155147677,-28.3314080124984,
123.592842983908)) ;
#110717 = CARTESIAN_POINT('Ctrl Pts',(-20.611096777598,-28.3447433531043,
123.312512297403)) ;
#110718 = CARTESIAN_POINT('Ctrl Pts',(-20.5764613049868,-28.3545859116441,
123.108490703106)) ;
#110719 = CARTESIAN_POINT('Ctrl Pts',(-20.5056644438528,-28.364637818494,
122.90939802792)) ;
#110720 = CARTESIAN_POINT('Ctrl Pts',(-20.3681581046119,-28.3778863328849,
122.667197630107)) ;
#110721 = CARTESIAN_POINT('Ctrl Pts',(-20.1207676706769,-28.3944855078326,
122.415435774505)) ;
#110722 = CARTESIAN_POINT('Ctrl Pts',(-19.8026289880667,-28.4110742936277,
122.263226023403)) ;
#110723 = CARTESIAN_POINT('Ctrl Pts',(-19.5282808196721,-28.4243501099696,
122.211756029638)) ;
#110724 = CARTESIAN_POINT('Ctrl Pts',(-19.3186094544046,-28.4343239607634,
122.209171007534)) ;
#110725 = CARTESIAN_POINT('Ctrl Pts',(-19.1105750538736,-28.4443529928558,
122.243437373191)) ;
#110726 = CARTESIAN_POINT('Ctrl Pts',(-18.9143171121521,-28.4542431183577,
122.312136733921)) ;
#110727 = CARTESIAN_POINT('Ctrl Pts',(-18.7309861690545,-28.4642355966292,
122.414657346976)) ;
#110728 = CARTESIAN_POINT('Ctrl Pts',(-18.5687975170022,-28.4741868117266,
122.546853414388)) ;
#110729 = CARTESIAN_POINT('Ctrl Pts',(-18.4308556464004,-28.4842353134817,
122.706820806781)) ;
#110730 = CARTESIAN_POINT('Ctrl Pts',(-18.3247843083646,-28.4940766630984,
122.884481270357)) ;
#110731 = CARTESIAN_POINT('Ctrl Pts',(-18.2496867518536,-28.5040629541187,
123.080496872413)) ;
#110732 = CARTESIAN_POINT('Ctrl Pts',(-18.2098480735606,-28.5139995658473,
123.285597343899)) ;
#110733 = CARTESIAN_POINT('Ctrl Pts',(-18.2062920964332,-28.5240494412148,
123.496826054513)) ;
#110734 = CARTESIAN_POINT('Ctrl Pts',(-18.2386605108681,-28.5338998997503,
123.701383802332)) ;
#110735 = CARTESIAN_POINT('Ctrl Pts',(-18.3063536198826,-28.543871836703,
123.899768176382)) ;
#110736 = CARTESIAN_POINT('Ctrl Pts',(-18.4077602679674,-28.5538672936351,
124.083853266906)) ;
#110737 = CARTESIAN_POINT('Ctrl Pts',(-18.5402393677939,-28.5639001006882,
124.247960463492)) ;
#110738 = CARTESIAN_POINT('Ctrl Pts',(-18.6962940205108,-28.5737599872782,
124.384411356347)) ;
#110739 = CARTESIAN_POINT('Ctrl Pts',(-18.8757659383011,-28.5837490678434,
124.493420420083)) ;
#110740 = CARTESIAN_POINT('Ctrl Pts',(-19.0703342091959,-28.5936805470526,
124.569178770303)) ;
#110741 = CARTESIAN_POINT('Ctrl Pts',(-19.2761626392862,-28.6036664064985,
124.61056752489)) ;
#110742 = CARTESIAN_POINT('Ctrl Pts',(-19.4871303851611,-28.6137045571457,
124.615242555406)) ;
#110743 = CARTESIAN_POINT('Ctrl Pts',(-19.691852735633,-28.6235526476501,
124.584234214769)) ;
#110744 = CARTESIAN_POINT('Ctrl Pts',(-19.8923396435699,-28.6336135561681,
124.516905024912)) ;
#110745 = CARTESIAN_POINT('Ctrl Pts',(-20.0749919675193,-28.6435084033261,
124.417310792677)) ;
#110746 = CARTESIAN_POINT('Ctrl Pts',(-20.2386582429069,-28.6534500753711,
124.287364241298)) ;
#110747 = CARTESIAN_POINT('Ctrl Pts',(-20.3782212827018,-28.6634526024966,
124.130031001371)) ;
#110748 = CARTESIAN_POINT('Ctrl Pts',(-20.4883954083524,-28.673487393684,
123.950138191648)) ;
#110749 = CARTESIAN_POINT('Ctrl Pts',(-20.5645319592197,-28.6833322735432,
123.757665821225)) ;
#110750 = CARTESIAN_POINT('Ctrl Pts',(-20.6070652574756,-28.6933181541616,
123.552119517391)) ;
#110751 = CARTESIAN_POINT('Ctrl Pts',(-20.6133837761091,-28.7032528772548,
123.343316499696)) ;
#110752 = CARTESIAN_POINT('Ctrl Pts',(-20.5827972090838,-28.713310717566,
123.134125176626)) ;
#110753 = CARTESIAN_POINT('Ctrl Pts',(-20.5182188073121,-28.7231312049625,
122.937999638884)) ;
#110754 = CARTESIAN_POINT('Ctrl Pts',(-20.4185157175339,-28.7331916063077,
122.751501960081)) ;
#110755 = CARTESIAN_POINT('Ctrl Pts',(-20.2893727294956,-28.7431225718606,
122.587425311953)) ;
#110756 = CARTESIAN_POINT('Ctrl Pts',(-20.133922757538,-28.753061434197,122.447837730162)) ;
#110757 = CARTESIAN_POINT('Ctrl Pts',(-19.9557965525416,-28.7630471651232,
122.336697470485)) ;
#110758 = CARTESIAN_POINT('Ctrl Pts',(-19.7602776861525,-28.7730715505507,
122.25809185253)) ;
#110759 = CARTESIAN_POINT('Ctrl Pts',(-19.5565956291653,-28.7829748349039,
122.214833769626)) ;
#110760 = CARTESIAN_POINT('Ctrl Pts',(-19.3452532269251,-28.7930348394819,
122.207556053065)) ;
#110761 = CARTESIAN_POINT('Ctrl Pts',(-19.1403035508003,-28.802878108551,
122.236311195689)) ;
#110762 = CARTESIAN_POINT('Ctrl Pts',(-18.9404078514478,-28.8128686741587,
122.300692951174)) ;
#110763 = CARTESIAN_POINT('Ctrl Pts',(-18.7558729417214,-28.8227968059375,
122.398237495578)) ;
#110764 = CARTESIAN_POINT('Ctrl Pts',(-18.5898613852116,-28.8327846930185,
122.526823544594)) ;
#110765 = CARTESIAN_POINT('Ctrl Pts',(-18.4482966997316,-28.8428206425871,
122.683257165934)) ;
#110766 = CARTESIAN_POINT('Ctrl Pts',(-18.337764772644,-28.852675528966,122.85850936285)) ;
#110767 = CARTESIAN_POINT('Ctrl Pts',(-18.257946305705,-28.8626749433138,
123.052947680852)) ;
#110768 = CARTESIAN_POINT('Ctrl Pts',(-18.2133359518162,-28.8725701085043,
123.256171138497)) ;
#110769 = CARTESIAN_POINT('Ctrl Pts',(-18.2045696957069,-28.8826304271963,
123.467461075091)) ;
#110770 = CARTESIAN_POINT('Ctrl Pts',(-18.2319223609867,-28.8924805589724,
123.672745679353)) ;
#110771 = CARTESIAN_POINT('Ctrl Pts',(-18.2951669413889,-28.9025111294226,
123.873902429767)) ;
#110772 = CARTESIAN_POINT('Ctrl Pts',(-18.3926450016252,-28.9125252800954,
124.060518201577)) ;
#110773 = CARTESIAN_POINT('Ctrl Pts',(-18.5192189735594,-28.9224182136408,
124.225552588671)) ;
#110774 = CARTESIAN_POINT('Ctrl Pts',(-18.67384301108,-28.9324077276311,124.367635535114)) ;
#110775 = CARTESIAN_POINT('Ctrl Pts',(-18.8501231974599,-28.9423614982835,
124.480451230367)) ;
#110776 = CARTESIAN_POINT('Ctrl Pts',(-19.0451644754906,-28.9524092669441,
124.561511122501)) ;
#110777 = CARTESIAN_POINT('Ctrl Pts',(-19.2470735250654,-28.9622509933839,
124.606778813278)) ;
#110778 = CARTESIAN_POINT('Ctrl Pts',(-19.4567244004309,-28.9722365102067,
124.616894986941)) ;
#110779 = CARTESIAN_POINT('Ctrl Pts',(-19.6640556831938,-28.9821758419022,
124.590645855405)) ;
#110780 = CARTESIAN_POINT('Ctrl Pts',(-19.8656384560267,-28.9922156115997,
124.528141800616)) ;
#110781 = CARTESIAN_POINT('Ctrl Pts',(-20.0505449265834,-29.0021037728485,
124.433122031589)) ;
#110782 = CARTESIAN_POINT('Ctrl Pts',(-20.2180648655832,-29.0120933273509,
124.306476704154)) ;
#110783 = CARTESIAN_POINT('Ctrl Pts',(-20.3604892062169,-29.0220517418745,
124.153037504906)) ;
#110784 = CARTESIAN_POINT('Ctrl Pts',(-20.4738773529589,-29.0319516547039,
123.978495713902)) ;
#110785 = CARTESIAN_POINT('Ctrl Pts',(-20.556374683759,-29.0419983543538,
123.784081738039)) ;
#110786 = CARTESIAN_POINT('Ctrl Pts',(-20.6033086922642,-29.0518982146594,
123.581284084144)) ;
#110787 = CARTESIAN_POINT('Ctrl Pts',(-20.614552088122,-29.0619496188649,
123.370300764834)) ;
#110788 = CARTESIAN_POINT('Ctrl Pts',(-20.5894921854852,-29.071830655786,
123.1640570945)) ;
#110789 = CARTESIAN_POINT('Ctrl Pts',(-20.5285675690555,-29.0818304879635,
122.962887021951)) ;
#110790 = CARTESIAN_POINT('Ctrl Pts',(-20.4345370713259,-29.0917484909484,
122.776744997018)) ;
#110791 = CARTESIAN_POINT('Ctrl Pts',(-20.3079234699645,-29.101799796823,
122.607612222485)) ;
#110792 = CARTESIAN_POINT('Ctrl Pts',(-20.1567634233035,-29.1116696202145,
122.46540431238)) ;
#110793 = CARTESIAN_POINT('Ctrl Pts',(-19.9796844708315,-29.1217437862648,
122.349309684017)) ;
#110794 = CARTESIAN_POINT('Ctrl Pts',(-19.790058128133,-29.1315638704064,
122.267561983645)) ;
#110795 = CARTESIAN_POINT('Ctrl Pts',(-19.5839698235328,-29.1416425971423,
122.218556199953)) ;
#110796 = CARTESIAN_POINT('Ctrl Pts',(-19.3771735392641,-29.1514941777918,
122.206283009837)) ;
#110797 = CARTESIAN_POINT('Ctrl Pts',(-19.1668255047857,-29.1615673060902,
122.230443832909)) ;
#110798 = CARTESIAN_POINT('Ctrl Pts',(-18.9684710698238,-29.1714097839817,
122.289426602626)) ;
#110799 = CARTESIAN_POINT('Ctrl Pts',(-18.7804867352061,-29.1813903905797,
122.382611081221)) ;
#110800 = CARTESIAN_POINT('Ctrl Pts',(-18.6111371054285,-29.1914080995985,
122.507808429459)) ;
#110801 = CARTESIAN_POINT('Ctrl Pts',(-18.4676985525238,-29.2012942786359,
122.658237444482)) ;
#110802 = CARTESIAN_POINT('Ctrl Pts',(-18.3505689202486,-29.2113518912083,
122.83425146942)) ;
#110803 = CARTESIAN_POINT('Ctrl Pts',(-18.2672768048722,-29.2212282845804,
123.024459025801)) ;
#110804 = CARTESIAN_POINT('Ctrl Pts',(-18.2171823153464,-29.2312233127309,
123.228521178178)) ;
#110805 = CARTESIAN_POINT('Ctrl Pts',(-18.2036038117194,-29.2412440595769,
123.438760145202)) ;
#110806 = CARTESIAN_POINT('Ctrl Pts',(-18.2262184883961,-29.2511461282432,
123.645698345896)) ;
#110807 = CARTESIAN_POINT('Ctrl Pts',(-18.2846455612304,-29.2611368680629,
123.847446251794)) ;
#110808 = CARTESIAN_POINT('Ctrl Pts',(-18.377093739046,-29.2711000642732,
124.035386718241)) ;
#110809 = CARTESIAN_POINT('Ctrl Pts',(-18.4996383434537,-29.2810042485733,
124.203746593179)) ;
#110810 = CARTESIAN_POINT('Ctrl Pts',(-18.6520116876082,-29.2910647089642,
124.350391619468)) ;
#110811 = CARTESIAN_POINT('Ctrl Pts',(-18.8235918172234,-29.300905254835,
124.466022281404)) ;
#110812 = CARTESIAN_POINT('Ctrl Pts',(-19.0167458852889,-29.3109674755468,
124.552225107633)) ;
#110813 = CARTESIAN_POINT('Ctrl Pts',(-19.2186519981554,-29.3208646185633,
124.602535484802)) ;
#110814 = CARTESIAN_POINT('Ctrl Pts',(-19.4268756397549,-29.3307957949805,
124.617765858331)) ;
#110815 = CARTESIAN_POINT('Ctrl Pts',(-19.6368811175299,-29.3408380087591,
124.596142981632)) ;
#110816 = CARTESIAN_POINT('Ctrl Pts',(-19.8368503844399,-29.3507245489619,
124.53942477153)) ;
#110817 = CARTESIAN_POINT('Ctrl Pts',(-20.0260825823634,-29.3607181435673,
124.44818222752)) ;
#110818 = CARTESIAN_POINT('Ctrl Pts',(-20.1957534857927,-29.3706620187248,
124.326037153957)) ;
#110819 = CARTESIAN_POINT('Ctrl Pts',(-20.3420619538255,-29.3806225548397,
124.176246087768)) ;
#110820 = CARTESIAN_POINT('Ctrl Pts',(-20.4606917415724,-29.3906191581624,
124.002742704819)) ;
#110821 = CARTESIAN_POINT('Ctrl Pts',(-20.5474262436801,-29.4006522411169,
123.810478861127)) ;
#110822 = CARTESIAN_POINT('Ctrl Pts',(-20.5987706230352,-29.4105034098184,
123.609845860846)) ;
#110823 = CARTESIAN_POINT('Ctrl Pts',(-20.6152927537207,-29.4204659005173,
123.401063314741)) ;
#110824 = CARTESIAN_POINT('Ctrl Pts',(-20.594918170003,-29.4304943289351,
123.191208760988)) ;
#110825 = CARTESIAN_POINT('Ctrl Pts',(-20.5391514970204,-29.4404046962996,
122.990473872677)) ;
#110826 = CARTESIAN_POINT('Ctrl Pts',(-20.4496430928384,-29.4503395639147,
122.801756711146)) ;
#110827 = CARTESIAN_POINT('Ctrl Pts',(-20.3272805436771,-29.4603807058938,
122.629750123816)) ;
#110828 = CARTESIAN_POINT('Ctrl Pts',(-20.179306753908,-29.4702678420969,
122.483757848448)) ;
#110829 = CARTESIAN_POINT('Ctrl Pts',(-20.0066330711629,-29.4802601245003,
122.364147157058)) ;
#110830 = CARTESIAN_POINT('Ctrl Pts',(-19.816601112119,-29.4902086524655,
122.276761842047)) ;
#110831 = CARTESIAN_POINT('Ctrl Pts',(-19.6146259436223,-29.5001453836277,
122.223483746351)) ;
#110832 = CARTESIAN_POINT('Ctrl Pts',(-19.4054733351576,-29.5101285944876,
122.205738011155)) ;
#110833 = CARTESIAN_POINT('Ctrl Pts',(-19.1952435624113,-29.5201716936375,
122.225063268743)) ;
#110834 = CARTESIAN_POINT('Ctrl Pts',(-18.9956988930366,-29.5300026579124,
122.278990709555)) ;
#110835 = CARTESIAN_POINT('Ctrl Pts',(-18.8039305285302,-29.5400755102984,
122.368740277853)) ;
#110836 = CARTESIAN_POINT('Ctrl Pts',(-18.6342252244993,-29.5499396380101,
122.487963358883)) ;
#110837 = CARTESIAN_POINT('Ctrl Pts',(-18.4851060196993,-29.559961840145,
122.636805516814)) ;
#110838 = CARTESIAN_POINT('Ctrl Pts',(-18.3644327138293,-29.5699890331134,
122.809667959652)) ;
#110839 = CARTESIAN_POINT('Ctrl Pts',(-18.2768442313984,-29.5798446270804,
122.997422270078)) ;
#110840 = CARTESIAN_POINT('Ctrl Pts',(-18.2220256417573,-29.5898017989457,
123.199455768176)) ;
#110841 = CARTESIAN_POINT('Ctrl Pts',(-18.2033282561175,-29.5998406429441,
123.409661433168)) ;
#110842 = CARTESIAN_POINT('Ctrl Pts',(-18.2207543970375,-29.6097146668197,
123.616539257195)) ;
#110843 = CARTESIAN_POINT('Ctrl Pts',(-18.2748812641831,-29.6197844928101,
123.821172162496)) ;
#110844 = CARTESIAN_POINT('Ctrl Pts',(-18.361548637412,-29.6296177367074,
124.00887233281)) ;
#110845 = CARTESIAN_POINT('Ctrl Pts',(-18.4813509732249,-29.6396481644804,
124.18239803893)) ;
#110846 = CARTESIAN_POINT('Ctrl Pts',(-18.6299300057852,-29.6496797812255,
124.332085748158)) ;
#110847 = CARTESIAN_POINT('Ctrl Pts',(-18.7985041884999,-29.6595094582063,
124.45159044379)) ;
#110848 = CARTESIAN_POINT('Ctrl Pts',(-18.9880545036046,-29.6694989750462,
124.542022840078)) ;
#110849 = CARTESIAN_POINT('Ctrl Pts',(-19.1916571487734,-29.679542587186,
124.597954392427)) ;
#110850 = CARTESIAN_POINT('Ctrl Pts',(-19.3972171202795,-29.6893651935213,
124.617681414701)) ;
#110851 = CARTESIAN_POINT('Ctrl Pts',(-19.6076268516394,-29.6994034234205,
124.601538956107)) ;
#110852 = CARTESIAN_POINT('Ctrl Pts',(-19.8113833174027,-29.7094144582124,
124.548770184925)) ;
#110853 = CARTESIAN_POINT('Ctrl Pts',(-20.0008354829509,-29.7193121891796,
124.462723139858)) ;
#110854 = CARTESIAN_POINT('Ctrl Pts',(-20.1742196158642,-29.72930181703,124.344221616664)) ;
#110855 = CARTESIAN_POINT('Ctrl Pts',(-20.3238339684053,-29.739257607476,
124.197860240491)) ;
#110856 = CARTESIAN_POINT('Ctrl Pts',(-20.4457452907353,-29.7491850060381,
124.028453482605)) ;
#110857 = CARTESIAN_POINT('Ctrl Pts',(-20.5372249530755,-29.759210601148,
123.838579289834)) ;
#110858 = CARTESIAN_POINT('Ctrl Pts',(-20.5936754529771,-29.7690964518175,
123.638560035978)) ;
#110859 = CARTESIAN_POINT('Ctrl Pts',(-20.6152518901214,-29.7790856316617,
123.429661569512)) ;
#110860 = CARTESIAN_POINT('Ctrl Pts',(-20.5997105873746,-29.7891268187653,
123.219137570526)) ;
#110861 = CARTESIAN_POINT('Ctrl Pts',(-20.5492588585748,-29.7989594622413,
123.018679750874)) ;
#110862 = CARTESIAN_POINT('Ctrl Pts',(-20.463929600502,-29.8089534119507,
122.826684501155)) ;
#110863 = CARTESIAN_POINT('Ctrl Pts',(-20.3457758880849,-29.8189825347273,
122.652054279035)) ;
#110864 = CARTESIAN_POINT('Ctrl Pts',(-20.2015667371248,-29.8288586656459,
122.502665469025)) ;
#110865 = CARTESIAN_POINT('Ctrl Pts',(-20.0317095853665,-29.838856700663,
122.378900046862)) ;
#110866 = CARTESIAN_POINT('Ctrl Pts',(-19.8445560518921,-29.8487706304217,
122.287118075451)) ;
#110867 = CARTESIAN_POINT('Ctrl Pts',(-19.6417509911196,-29.8588138181595,
122.228441087821)) ;
#110868 = CARTESIAN_POINT('Ctrl Pts',(-19.4348089155927,-29.8687136602998,
122.206175419326)) ;
#110869 = CARTESIAN_POINT('Ctrl Pts',(-19.2252055848282,-29.8787049271078,
122.219861949601)) ;
#110870 = CARTESIAN_POINT('Ctrl Pts',(-19.0204144320014,-29.8887370292398,
122.270293254083)) ;
#110871 = CARTESIAN_POINT('Ctrl Pts',(-18.8305639761779,-29.8986039101946,
122.353859507053)) ;
#110872 = CARTESIAN_POINT('Ctrl Pts',(-18.6556387109257,-29.9085957014827,
122.470167892145)) ;
#110873 = CARTESIAN_POINT('Ctrl Pts',(-18.5032370765788,-29.9186278173942,
122.615959251121)) ;
#110874 = CARTESIAN_POINT('Ctrl Pts',(-18.3802665479819,-29.9284941341943,
122.783008307461)) ;
#110875 = CARTESIAN_POINT('Ctrl Pts',(-18.2867460420855,-29.9384816156679,
122.970970810779)) ;
#110876 = CARTESIAN_POINT('Ctrl Pts',(-18.2274133413087,-29.9484265400468,
123.171480851248)) ;
#110877 = CARTESIAN_POINT('Ctrl Pts',(-18.2036829181316,-29.9584714259575,
123.381298888447)) ;
#110878 = CARTESIAN_POINT('Ctrl Pts',(-18.2163274034564,-29.96833352967,123.588260229601)) ;
#110879 = CARTESIAN_POINT('Ctrl Pts',(-18.264931028882,-29.9783250934945,
123.792598178663)) ;
#110880 = CARTESIAN_POINT('Ctrl Pts',(-18.3478715928108,-29.9882579015574,
123.984238297766)) ;
#110881 = CARTESIAN_POINT('Ctrl Pts',(-18.4624553674049,-29.9981950037937,
124.158935155883)) ;
#110882 = CARTESIAN_POINT('Ctrl Pts',(-18.6074774312528,-30.0082474500641,
124.312635708356)) ;
#110883 = CARTESIAN_POINT('Ctrl Pts',(-18.7733546015186,-30.0180935656457,
124.436489105787)) ;
#110884 = CARTESIAN_POINT('Ctrl Pts',(-18.9618306363196,-30.0281415853606,
124.531848067045)) ;
#110885 = CARTESIAN_POINT('Ctrl Pts',(-19.1619768486738,-30.0380835369896,
124.592115870425)) ;
#110886 = CARTESIAN_POINT('Ctrl Pts',(-19.3694102443087,-30.0480223179886,
124.617220922463)) ;
#110887 = CARTESIAN_POINT('Ctrl Pts',(-19.5798591505657,-30.0580483667147,
124.605669428812)) ;
#110888 = CARTESIAN_POINT('Ctrl Pts',(-19.7823544531391,-30.0679352271229,
124.558666002782)) ;
#110889 = CARTESIAN_POINT('Ctrl Pts',(-19.9763869209635,-30.0779665022547,
124.476138580313)) ;
#110890 = CARTESIAN_POINT('Ctrl Pts',(-20.1507108682372,-30.0878494795551,
124.363008690583)) ;
#110891 = CARTESIAN_POINT('Ctrl Pts',(-20.3053499867673,-30.0979063329623,
124.21890683899)) ;
#110892 = CARTESIAN_POINT('Ctrl Pts',(-20.472466062812,-30.1110745740382,
123.998074707083)) ;
#110893 = CARTESIAN_POINT('Ctrl Pts',(-20.5799188097016,-30.1244756032648,
123.734274564754)) ;
#110894 = CARTESIAN_POINT('Ctrl Pts',(-20.6142292717578,-30.1376885199956,
123.458583462747)) ;
#110895 = CARTESIAN_POINT('Ctrl Pts',(-20.6043586023796,-30.1476169144488,
123.250125810394)) ;
#110896 = CARTESIAN_POINT('Ctrl Pts',(-20.5583338851093,-30.157598414577,
123.045363360107)) ;
#110897 = CARTESIAN_POINT('Ctrl Pts',(-20.4767223139127,-30.1676389578471,
122.850706254228)) ;
#110898 = CARTESIAN_POINT('Ctrl Pts',(-20.3649484161175,-30.1774882896302,
122.676398430749)) ;
#110899 = CARTESIAN_POINT('Ctrl Pts',(-20.2229259158472,-30.1874836941018,
122.521525739695)) ;
#110900 = CARTESIAN_POINT('Ctrl Pts',(-20.0555905567354,-30.1975000215504,
122.393695498053)) ;
#110901 = CARTESIAN_POINT('Ctrl Pts',(-19.8088969552577,-30.210723678717,
122.265445425939)) ;
#110902 = CARTESIAN_POINT('Ctrl Pts',(-19.5330272008713,-30.2240179701063,
122.203984380507)) ;
#110903 = CARTESIAN_POINT('Ctrl Pts',(-19.2539915157893,-30.2373023210378,
122.215885126457)) ;
#110904 = CARTESIAN_POINT('Ctrl Pts',(-19.0492501087174,-30.2472747020996,
122.26089061953)) ;
#110905 = CARTESIAN_POINT('Ctrl Pts',(-18.8564975146907,-30.2571830817252,
122.339933494422)) ;
#110906 = CARTESIAN_POINT('Ctrl Pts',(-18.6778987788476,-30.2672370804733,
122.452935156648)) ;
#110907 = CARTESIAN_POINT('Ctrl Pts',(-18.5244772873896,-30.2770992775896,
122.592422355087)) ;
#110908 = CARTESIAN_POINT('Ctrl Pts',(-18.3524364415899,-30.2904464039637,
122.81409854329)) ;
#110909 = CARTESIAN_POINT('Ctrl Pts',(-18.2159932371191,-30.3069833696052,
123.138166619095)) ;
#110910 = CARTESIAN_POINT('Ctrl Pts',(-18.197670960025,-30.3236179737791,
123.491378902353)) ;
#110911 = CARTESIAN_POINT('Ctrl Pts',(-18.25605817187,-30.3369077670217,123.764606733069)) ;
#110912 = CARTESIAN_POINT('Ctrl Pts',(-18.3343798206414,-30.3468603982811,
123.958616619102)) ;
#110913 = CARTESIAN_POINT('Ctrl Pts',(-18.4450022895849,-30.3568123655858,
124.136223927861)) ;
#110914 = CARTESIAN_POINT('Ctrl Pts',(-18.6328487204077,-30.3701796240496,
124.345213791547)) ;
#110915 = CARTESIAN_POINT('Ctrl Pts',(-18.9269899088885,-30.3866964359988,
124.537244079557)) ;
#110916 = CARTESIAN_POINT('Ctrl Pts',(-19.3414672867283,-30.4067223310052,
124.634317537045)) ;
#110917 = CARTESIAN_POINT('Ctrl Pts',(-19.7598559365141,-30.4265330611353,
124.584765784642)) ;
#110918 = CARTESIAN_POINT('Ctrl Pts',(-20.1396861772112,-30.4465102772652,
124.394694797982)) ;
#110919 = CARTESIAN_POINT('Ctrl Pts',(-20.4305654759697,-30.4664371526604,
124.086654754617)) ;
#110920 = CARTESIAN_POINT('Ctrl Pts',(-20.5992561023151,-30.4862586141367,
123.700365779593)) ;
#110921 = CARTESIAN_POINT('Ctrl Pts',(-20.6260517162596,-30.506332931946,
123.274438520922)) ;
#110922 = CARTESIAN_POINT('Ctrl Pts',(-20.5068006738216,-30.5261809009539,
122.869494392848)) ;
#110923 = CARTESIAN_POINT('Ctrl Pts',(-20.2561000415122,-30.5461279350171,
122.527506972999)) ;
#110924 = CARTESIAN_POINT('Ctrl Pts',(-19.9044846617621,-30.5660238859893,
122.292221804116)) ;
#110925 = CARTESIAN_POINT('Ctrl Pts',(-19.4939183143729,-30.5859193656075,
122.190385250121)) ;
#110926 = CARTESIAN_POINT('Ctrl Pts',(-19.0718958107704,-30.6058754765723,
122.234812026665)) ;
#110927 = CARTESIAN_POINT('Ctrl Pts',(-18.6914879436141,-30.6257800246123,
122.420176934716)) ;
#110928 = CARTESIAN_POINT('Ctrl Pts',(-18.3967601738748,-30.6456541489314,
122.723120521545)) ;
#110929 = CARTESIAN_POINT('Ctrl Pts',(-18.2221440537837,-30.6657086789304,
123.112068385375)) ;
#110930 = CARTESIAN_POINT('Ctrl Pts',(-18.190987007323,-30.6855161926904,
123.532166336377)) ;
#110931 = CARTESIAN_POINT('Ctrl Pts',(-18.3051669303263,-30.7054995484582,
123.941376041176)) ;
#110932 = CARTESIAN_POINT('Ctrl Pts',(-18.5518825166987,-30.7254178510421,
124.285605662195)) ;
#110933 = CARTESIAN_POINT('Ctrl Pts',(-18.8998090253807,-30.7452860664878,
124.525367393536)) ;
#110934 = CARTESIAN_POINT('Ctrl Pts',(-19.3123807021432,-30.7653363832841,
124.632280078784)) ;
#110935 = CARTESIAN_POINT('Ctrl Pts',(-19.731211809009,-30.7851124451666,
124.593072886192)) ;
#110936 = CARTESIAN_POINT('Ctrl Pts',(-20.1167006845037,-30.8051670508591,
124.411195876899)) ;
#110937 = CARTESIAN_POINT('Ctrl Pts',(-20.4131995257569,-30.8249607400149,
124.112322445664)) ;
#110938 = CARTESIAN_POINT('Ctrl Pts',(-20.5924160652199,-30.8449274316093,
123.727557835573)) ;
#110939 = CARTESIAN_POINT('Ctrl Pts',(-20.6289177344259,-30.8648874773603,
123.304647397556)) ;
#110940 = CARTESIAN_POINT('Ctrl Pts',(-20.5195484909326,-30.8847857375105,
122.895963083405)) ;
#110941 = CARTESIAN_POINT('Ctrl Pts',(-20.2777396156655,-30.9046806530597,
122.548891927275)) ;
#110942 = CARTESIAN_POINT('Ctrl Pts',(-19.9319581954525,-30.9245908334733,
122.304652410846)) ;
#110943 = CARTESIAN_POINT('Ctrl Pts',(-19.5230956047795,-30.9445266325876,
122.192737630462)) ;
#110944 = CARTESIAN_POINT('Ctrl Pts',(-19.1005558990613,-30.9644644942417,
122.227039044501)) ;
#110945 = CARTESIAN_POINT('Ctrl Pts',(-18.7153141741338,-30.9843835408794,
122.403079277346)) ;
#110946 = CARTESIAN_POINT('Ctrl Pts',(-18.4127970947094,-31.0043324389335,
122.700396617679)) ;
#110947 = CARTESIAN_POINT('Ctrl Pts',(-18.2301812572521,-31.0242382663766,
123.082254315887)) ;
#110948 = CARTESIAN_POINT('Ctrl Pts',(-18.1953741322619,-31.0408209617419,
123.433044543302)) ;
#110949 = CARTESIAN_POINT('Ctrl Pts',(-18.2402816620071,-31.0540951754655,
123.70853874743)) ;
#110950 = CARTESIAN_POINT('Ctrl Pts',(-18.3100454270419,-31.0641418946649,
123.907868209197)) ;
#110951 = CARTESIAN_POINT('Ctrl Pts',(-18.4111023323004,-31.0739859293105,
124.088497890168)) ;
#110952 = CARTESIAN_POINT('Ctrl Pts',(-18.5878427173119,-31.0873203142151,
124.306014556575)) ;
#110953 = CARTESIAN_POINT('Ctrl Pts',(-18.8736729199836,-31.1039075315148,
124.512815858387)) ;
#110954 = CARTESIAN_POINT('Ctrl Pts',(-19.2135917359452,-31.1205407435527,
124.610143180137)) ;
#110955 = CARTESIAN_POINT('Ctrl Pts',(-19.4928520602652,-31.1338231858249,
124.614857716735)) ;
#110956 = CARTESIAN_POINT('Ctrl Pts',(-19.6985677773523,-31.1437290737391,
124.582580217435)) ;
#110957 = CARTESIAN_POINT('Ctrl Pts',(-19.8973118378281,-31.1537174918443,
124.514752467582)) ;
#110958 = CARTESIAN_POINT('Ctrl Pts',(-20.0817895040142,-31.163740919083,
124.412897157068)) ;
#110959 = CARTESIAN_POINT('Ctrl Pts',(-20.2438978809988,-31.1736453502,124.282224219338)) ;
#110960 = CARTESIAN_POINT('Ctrl Pts',(-20.4278530152037,-31.1869085028104,
124.072693688048)) ;
#110961 = CARTESIAN_POINT('Ctrl Pts',(-20.5532323701249,-31.2002334007143,
123.818652314628)) ;
#110962 = CARTESIAN_POINT('Ctrl Pts',(-20.6078115826222,-31.2134891443299,
123.545311844045)) ;
#110963 = CARTESIAN_POINT('Ctrl Pts',(-20.6128436190423,-31.2234485177772,
123.336025653533)) ;
#110964 = CARTESIAN_POINT('Ctrl Pts',(-20.5817628333554,-31.2333923417042,
123.129271563074)) ;
#110965 = CARTESIAN_POINT('Ctrl Pts',(-20.5144000187116,-31.2434402858515,
122.92907768263)) ;
#110966 = CARTESIAN_POINT('Ctrl Pts',(-20.4154292073334,-31.2532912570697,
122.747144528427)) ;
#110967 = CARTESIAN_POINT('Ctrl Pts',(-20.285234699123,-31.2632630745117,
122.582864770209)) ;
#110968 = CARTESIAN_POINT('Ctrl Pts',(-20.1280595915438,-31.2732584968038,
122.443347493676)) ;
#110969 = CARTESIAN_POINT('Ctrl Pts',(-19.9482881394493,-31.2832915619275,
122.333032433614)) ;
#110970 = CARTESIAN_POINT('Ctrl Pts',(-19.7554452935688,-31.2931568945927,
122.256713481666)) ;
#110971 = CARTESIAN_POINT('Ctrl Pts',(-19.5504347395914,-31.3031174371903,
122.214029832058)) ;
#110972 = CARTESIAN_POINT('Ctrl Pts',(-19.3395941650345,-31.313151122692,
122.20790061229)) ;
#110973 = CARTESIAN_POINT('Ctrl Pts',(-19.1338978544078,-31.3230359546823,
122.237668445641)) ;
#110974 = CARTESIAN_POINT('Ctrl Pts',(-18.9329243763462,-31.3331033814421,
122.303926600611)) ;
#110975 = CARTESIAN_POINT('Ctrl Pts',(-18.7505899823176,-31.342941870601,
122.401649387696)) ;
#110976 = CARTESIAN_POINT('Ctrl Pts',(-18.5841524487221,-31.3530053517911,
122.532210339757)) ;
#110977 = CARTESIAN_POINT('Ctrl Pts',(-18.4453883431229,-31.3628995096062,
122.687197158415)) ;
#110978 = CARTESIAN_POINT('Ctrl Pts',(-18.3346568422309,-31.3728413663505,
122.864432311163)) ;
#110979 = CARTESIAN_POINT('Ctrl Pts',(-18.2558101849589,-31.3828438440219,
123.059405613758)) ;
#110980 = CARTESIAN_POINT('Ctrl Pts',(-18.2122072175293,-31.3928786483262,
123.265799819206)) ;
#110981 = CARTESIAN_POINT('Ctrl Pts',(-18.2048893892992,-31.4027235251719,
123.472654534328)) ;
#110982 = CARTESIAN_POINT('Ctrl Pts',(-18.2336127202697,-31.4127094047274,
123.680580465293)) ;
#110983 = CARTESIAN_POINT('Ctrl Pts',(-18.2975511490545,-31.4226441350859,
123.879454712275)) ;
#110984 = CARTESIAN_POINT('Ctrl Pts',(-18.3963984163014,-31.4327019473988,
124.066335160558)) ;
#110985 = CARTESIAN_POINT('Ctrl Pts',(-18.5228930013536,-31.4425225395232,
124.229549268469)) ;
#110986 = CARTESIAN_POINT('Ctrl Pts',(-18.6794032644519,-31.452589125133,
124.371937466252)) ;
#110987 = CARTESIAN_POINT('Ctrl Pts',(-18.8553890889416,-31.4624887057148,
124.48312811206)) ;
#110988 = CARTESIAN_POINT('Ctrl Pts',(-19.050853581083,-31.472540305393,124.563325265324)) ;
#110989 = CARTESIAN_POINT('Ctrl Pts',(-19.2536732806486,-31.48241449181,124.607740482583)) ;
#110990 = CARTESIAN_POINT('Ctrl Pts',(-19.464869384007,-31.4924709676909,
124.616554888009)) ;
#110991 = CARTESIAN_POINT('Ctrl Pts',(-19.67107210323,-31.5023638989935,124.589086356959)) ;
#110992 = CARTESIAN_POINT('Ctrl Pts',(-19.8727150974772,-31.5124266777062,
124.525215234312)) ;
#110993 = CARTESIAN_POINT('Ctrl Pts',(-20.056201628323,-31.5222692032873,
124.429511938588)) ;
#110994 = CARTESIAN_POINT('Ctrl Pts',(-20.2230194275553,-31.5322599687122,
124.301933683297)) ;
#110995 = CARTESIAN_POINT('Ctrl Pts',(-20.3642568301366,-31.5421880447102,
124.148246211986)) ;
#110996 = CARTESIAN_POINT('Ctrl Pts',(-20.4776500938156,-31.5521759550973,
123.971508403461)) ;
#110997 = CARTESIAN_POINT('Ctrl Pts',(-20.5586853666361,-31.5622118672222,
123.776713289031)) ;
#110998 = CARTESIAN_POINT('Ctrl Pts',(-20.6041772588354,-31.5720668800699,
123.574569942644)) ;
#110999 = CARTESIAN_POINT('Ctrl Pts',(-20.6143116227714,-31.5820658259861,
123.364638894636)) ;
#111000 = CARTESIAN_POINT('Ctrl Pts',(-20.5883043288792,-31.5919627384341,
123.158174199298)) ;
#111001 = CARTESIAN_POINT('Ctrl Pts',(-20.5259098266886,-31.6020165365276,
122.956257926399)) ;
#111002 = CARTESIAN_POINT('Ctrl Pts',(-20.4310950457735,-31.6118974573543,
122.771404890897)) ;
#111003 = CARTESIAN_POINT('Ctrl Pts',(-20.3043856023873,-31.6219019833521,
122.603560424754)) ;
#111004 = CARTESIAN_POINT('Ctrl Pts',(-20.1506872029286,-31.6318859469695,
122.460566443654)) ;
#111005 = CARTESIAN_POINT('Ctrl Pts',(-19.9734467715761,-31.6419255875208,
122.345990374777)) ;
#111006 = CARTESIAN_POINT('Ctrl Pts',(-19.7828774660423,-31.6517696131355,
122.265288199531)) ;
#111007 = CARTESIAN_POINT('Ctrl Pts',(-19.5783150582492,-31.6617606189529,
122.217619085736)) ;
#111008 = CARTESIAN_POINT('Ctrl Pts',(-19.3675761229911,-31.6717984104851,
122.206620385186)) ;
#111009 = CARTESIAN_POINT('Ctrl Pts',(-19.1621125650746,-31.6816428102735,
122.23152300414)) ;
#111010 = CARTESIAN_POINT('Ctrl Pts',(-18.9611827679441,-31.6916276108302,
122.292174303081)) ;
#111011 = CARTESIAN_POINT('Ctrl Pts',(-18.7745945804999,-31.7015671342414,
122.386307698307)) ;
#111012 = CARTESIAN_POINT('Ctrl Pts',(-18.6055635122502,-31.7116068533424,
122.51268279667)) ;
#111013 = CARTESIAN_POINT('Ctrl Pts',(-18.4631294183271,-31.7214950252616,
122.664115130075)) ;
#111014 = CARTESIAN_POINT('Ctrl Pts',(-18.3476659224257,-31.7314845876786,
122.839529091556)) ;
#111015 = CARTESIAN_POINT('Ctrl Pts',(-18.2648166657048,-31.7414429598733,
123.031790588101)) ;
#111016 = CARTESIAN_POINT('Ctrl Pts',(-18.2164011291446,-31.751343034104,
123.234219310739)) ;
#111017 = CARTESIAN_POINT('Ctrl Pts',(-18.2037134576193,-31.7613891304776,
123.445028875281)) ;
#111018 = CARTESIAN_POINT('Ctrl Pts',(-18.2274818505537,-31.7712977144747,
123.65198756325)) ;
#111019 = CARTESIAN_POINT('Ctrl Pts',(-18.2870598082787,-31.7813082930656,
123.853835575894)) ;
#111020 = CARTESIAN_POINT('Ctrl Pts',(-18.3813381495651,-31.7913374511785,
124.042436313349)) ;
#111021 = CARTESIAN_POINT('Ctrl Pts',(-18.5044722824645,-31.8011903330165,
124.208985901477)) ;
#111022 = CARTESIAN_POINT('Ctrl Pts',(-18.6558495349648,-31.8111498941675,
124.353651361732)) ;
#111023 = CARTESIAN_POINT('Ctrl Pts',(-18.8316227813614,-31.8211883287566,
124.470423349805)) ;
#111024 = CARTESIAN_POINT('Ctrl Pts',(-19.0217047863666,-31.8310616009837,
124.55388930621)) ;
#111025 = CARTESIAN_POINT('Ctrl Pts',(-19.2274184196166,-31.8411348429773,
124.603996891665)) ;
#111026 = CARTESIAN_POINT('Ctrl Pts',(-19.4334723224669,-31.8509551745104,
124.617559154811)) ;
#111027 = CARTESIAN_POINT('Ctrl Pts',(-19.6440751231138,-31.8610338357371,
124.594752478478)) ;
#111028 = CARTESIAN_POINT('Ctrl Pts',(-19.8430504569168,-31.8708854310314,
124.537096738257)) ;
#111029 = CARTESIAN_POINT('Ctrl Pts',(-20.0331768412375,-31.8809585662602,
124.443919161582)) ;
#111030 = CARTESIAN_POINT('Ctrl Pts',(-20.2003452640676,-31.8908010017852,
124.321944272941)) ;
#111031 = CARTESIAN_POINT('Ctrl Pts',(-20.3462944552437,-31.9007817709186,
124.171207606797)) ;
#111032 = CARTESIAN_POINT('Ctrl Pts',(-20.4639641857985,-31.9107988721625,
123.996558181382)) ;
#111033 = CARTESIAN_POINT('Ctrl Pts',(-20.5487866675735,-31.9206873197643,
123.806747058626)) ;
#111034 = CARTESIAN_POINT('Ctrl Pts',(-20.6002315884477,-31.9307430339452,
123.60171887215)) ;
#111035 = CARTESIAN_POINT('Ctrl Pts',(-20.6150585311005,-31.940618240359,
123.394627414762)) ;
#111036 = CARTESIAN_POINT('Ctrl Pts',(-20.5939482942075,-31.9506132928317,
123.185569097398)) ;
#111037 = CARTESIAN_POINT('Ctrl Pts',(-20.5363734078417,-31.9606351767938,
122.982888547521)) ;
#111038 = CARTESIAN_POINT('Ctrl Pts',(-20.4457763136072,-31.9705391493231,
122.79542134903)) ;
#111039 = CARTESIAN_POINT('Ctrl Pts',(-20.3232089706056,-31.980527645984,
122.624911550368)) ;
#111040 = CARTESIAN_POINT('Ctrl Pts',(-20.1731785988359,-31.990491443232,
122.47874667217)) ;
#111041 = CARTESIAN_POINT('Ctrl Pts',(-20.0013492474168,-32.00039546654,122.361121541256)) ;
#111042 = CARTESIAN_POINT('Ctrl Pts',(-19.8086786426288,-32.0104559698617,
122.273939353814)) ;
#111043 = CARTESIAN_POINT('Ctrl Pts',(-19.6082912144808,-32.0202965050015,
122.222412597469)) ;
#111044 = CARTESIAN_POINT('Ctrl Pts',(-19.3974247205881,-32.0303587257061,
122.205837223768)) ;
#111045 = CARTESIAN_POINT('Ctrl Pts',(-19.1903252623623,-32.0402558794824,
122.226013703721)) ;
#111046 = CARTESIAN_POINT('Ctrl Pts',(-18.9890157586273,-32.0501870128678,
122.281360250581)) ;
#111047 = CARTESIAN_POINT('Ctrl Pts',(-18.7983606964968,-32.0602293880136,
122.372034096135)) ;
#111048 = CARTESIAN_POINT('Ctrl Pts',(-18.628919632478,-32.0701153257797,
122.492406079435)) ;
#111049 = CARTESIAN_POINT('Ctrl Pts',(-18.4811182502262,-32.0801111687645,
122.641766124136)) ;
#111050 = CARTESIAN_POINT('Ctrl Pts',(-18.362144460142,-32.0900531466432,
122.813626300764)) ;
#111051 = CARTESIAN_POINT('Ctrl Pts',(-18.2744163791547,-32.1000125211241,
123.003725424228)) ;
#111052 = CARTESIAN_POINT('Ctrl Pts',(-18.2207156442196,-32.1100091369579,
123.20693169086)) ;
#111053 = CARTESIAN_POINT('Ctrl Pts',(-18.2033294204649,-32.1200433555314,
123.417158833608)) ;
#111054 = CARTESIAN_POINT('Ctrl Pts',(-18.2221093830639,-32.129896422742,
123.623444961005)) ;
#111055 = CARTESIAN_POINT('Ctrl Pts',(-18.2764221133871,-32.1398566806196,
123.825667129567)) ;
#111056 = CARTESIAN_POINT('Ctrl Pts',(-18.3658675430293,-32.1498857073252,
124.016608439681)) ;
#111057 = CARTESIAN_POINT('Ctrl Pts',(-18.4856092719792,-32.1597959143596,
124.187093370292)) ;
#111058 = CARTESIAN_POINT('Ctrl Pts',(-18.6331239720399,-32.1697308250073,
124.334963670436)) ;
#111059 = CARTESIAN_POINT('Ctrl Pts',(-18.8060039080149,-32.1797719551865,
124.456088912158)) ;
#111060 = CARTESIAN_POINT('Ctrl Pts',(-18.994309857815,-32.1896590955564,
124.544127878436)) ;
#111061 = CARTESIAN_POINT('Ctrl Pts',(-19.1970601287714,-32.1996513730924,
124.599039382613)) ;
#111062 = CARTESIAN_POINT('Ctrl Pts',(-19.4053803118689,-32.2095999163607,
124.617773458022)) ;
#111063 = CARTESIAN_POINT('Ctrl Pts',(-19.6135385905514,-32.2195365911779,
124.600372594959)) ;
#111064 = CARTESIAN_POINT('Ctrl Pts',(-19.8165641321699,-32.2295200121143,
124.547077151019)) ;
#111065 = CARTESIAN_POINT('Ctrl Pts',(-20.0082045252136,-32.2395623273035,
124.458523898483)) ;
#111066 = CARTESIAN_POINT('Ctrl Pts',(-20.1782724858429,-32.2494026447427,
124.340732707119)) ;
#111067 = CARTESIAN_POINT('Ctrl Pts',(-20.3284823050766,-32.2594323488002,
124.192751787689)) ;
#111068 = CARTESIAN_POINT('Ctrl Pts',(-20.4501448268239,-32.2694533055227,
124.020761100757)) ;
#111069 = CARTESIAN_POINT('Ctrl Pts',(-20.5391965505084,-32.2793198478263,
123.833407718044)) ;
#111070 = CARTESIAN_POINT('Ctrl Pts',(-20.5955014894934,-32.2893909477715,
123.629325484045)) ;
#111071 = CARTESIAN_POINT('Ctrl Pts',(-20.6150581381533,-32.2992330219491,
123.42333293983)) ;
#111072 = CARTESIAN_POINT('Ctrl Pts',(-20.5991226989991,-32.3091938165361,
123.214537677283)) ;
#111073 = CARTESIAN_POINT('Ctrl Pts',(-20.5463695099126,-32.3192316894369,
123.010217358845)) ;
#111074 = CARTESIAN_POINT('Ctrl Pts',(-20.4607025302325,-32.329105974981,
122.821101903146)) ;
#111075 = CARTESIAN_POINT('Ctrl Pts',(-20.3412003434424,-32.3391757253949,
122.646392803246)) ;
#111076 = CARTESIAN_POINT('Ctrl Pts',(-20.1967030316238,-32.3490090099296,
122.498530545508)) ;
#111077 = CARTESIAN_POINT('Ctrl Pts',(-20.0257286909022,-32.3590393507296,
122.375116147167)) ;
#111078 = CARTESIAN_POINT('Ctrl Pts',(-19.8356093287975,-32.3690712747292,
122.283799559052)) ;
#111079 = CARTESIAN_POINT('Ctrl Pts',(-19.6367804005082,-32.3788998096651,
122.22760822429)) ;
#111080 = CARTESIAN_POINT('Ctrl Pts',(-19.4278088318512,-32.3888935874298,
122.20586949495)) ;
#111081 = CARTESIAN_POINT('Ctrl Pts',(-19.2175470747755,-32.3989212979154,
122.221210724145)) ;
#111082 = CARTESIAN_POINT('Ctrl Pts',(-19.0159240745563,-32.4088097087493,
122.271857869907)) ;
#111083 = CARTESIAN_POINT('Ctrl Pts',(-18.8243268225095,-32.4187865592849,
122.357161573968)) ;
#111084 = CARTESIAN_POINT('Ctrl Pts',(-18.6501429093091,-32.4287783558353,
122.474623948813)) ;
#111085 = CARTESIAN_POINT('Ctrl Pts',(-18.4985443009351,-32.438814361929,
122.621344322979)) ;
#111086 = CARTESIAN_POINT('Ctrl Pts',(-18.3767323453049,-32.4486650961918,
122.788842659603)) ;
#111087 = CARTESIAN_POINT('Ctrl Pts',(-18.2842520228874,-32.45865635472,122.977402613262)) ;
#111088 = CARTESIAN_POINT('Ctrl Pts',(-18.2262100848264,-32.4685742496232,
123.177694165123)) ;
#111089 = CARTESIAN_POINT('Ctrl Pts',(-18.2035294382131,-32.4786023912863,
123.387276598808)) ;
#111090 = CARTESIAN_POINT('Ctrl Pts',(-18.2172975833845,-32.4884875594021,
123.59464241443)) ;
#111091 = CARTESIAN_POINT('Ctrl Pts',(-18.2668882869775,-32.4984769229081,
123.798715457908)) ;
#111092 = CARTESIAN_POINT('Ctrl Pts',(-18.3520027631055,-32.5085180579182,
123.99189209642)) ;
#111093 = CARTESIAN_POINT('Ctrl Pts',(-18.4666437837428,-32.5183507261062,
124.16389862609)) ;
#111094 = CARTESIAN_POINT('Ctrl Pts',(-18.6113167569351,-32.5283446290607,
124.316255744136)) ;
#111095 = CARTESIAN_POINT('Ctrl Pts',(-18.7811122527559,-32.5383739141452,
124.44126274807)) ;
#111096 = CARTESIAN_POINT('Ctrl Pts',(-18.966995046856,-32.5482494425871,
124.53376094413)) ;
#111097 = CARTESIAN_POINT('Ctrl Pts',(-19.168529051928,-32.5582497252032,
124.593535705015)) ;
#111098 = CARTESIAN_POINT('Ctrl Pts',(-19.3755681293351,-32.5681617412602,
124.617371731371)) ;
#111099 = CARTESIAN_POINT('Ctrl Pts',(-19.5862937541998,-32.5782038165992,
124.604789768503)) ;
#111100 = CARTESIAN_POINT('Ctrl Pts',(-19.7887488454565,-32.5881036492553,
124.556492318562)) ;
#111101 = CARTESIAN_POINT('Ctrl Pts',(-19.9817040535824,-32.5980960498334,
124.473434533461)) ;
#111102 = CARTESIAN_POINT('Ctrl Pts',(-20.157834546487,-32.6081300715927,
124.357339411608)) ;
#111103 = CARTESIAN_POINT('Ctrl Pts',(-20.3087209608443,-32.6179946824339,
124.215071266553)) ;
#111104 = CARTESIAN_POINT('Ctrl Pts',(-20.4346339667854,-32.6279870818951,
124.046912168793)) ;
#111105 = CARTESIAN_POINT('Ctrl Pts',(-20.5294401855393,-32.638019035228,
123.858519229892)) ;
#111106 = CARTESIAN_POINT('Ctrl Pts',(-20.5894011242506,-32.6478853941696,
123.659944008041)) ;
#111107 = CARTESIAN_POINT('Ctrl Pts',(-20.614609393886,-32.6578728696554,
123.451520232646)) ;
#111108 = CARTESIAN_POINT('Ctrl Pts',(-20.6034027832421,-32.6678177758439,
123.242716459489)) ;
#111109 = CARTESIAN_POINT('Ctrl Pts',(-20.5555298751202,-32.6778627405042,
123.03705837456)) ;
#111110 = CARTESIAN_POINT('Ctrl Pts',(-20.4743442635801,-32.687724547409,
122.846269977045)) ;
#111111 = CARTESIAN_POINT('Ctrl Pts',(-20.360123579153,-32.6977172197148,
122.669983009096)) ;
#111112 = CARTESIAN_POINT('Ctrl Pts',(-20.2179031724518,-32.7076458906601,
122.517182290364)) ;
#111113 = CARTESIAN_POINT('Ctrl Pts',(-20.0511405476393,-32.7175984328854,
122.390837735781)) ;
#111114 = CARTESIAN_POINT('Ctrl Pts',(-19.8640787766569,-32.7275997888813,
122.294783715393)) ;
#111115 = CARTESIAN_POINT('Ctrl Pts',(-19.6625777664322,-32.737628401156,
122.232784379602)) ;
#111116 = CARTESIAN_POINT('Ctrl Pts',(-19.4568140049153,-32.7474927357055,
122.206836472349)) ;
#111117 = CARTESIAN_POINT('Ctrl Pts',(-19.2470090489067,-32.7574850597821,
122.216814039382)) ;
#111118 = CARTESIAN_POINT('Ctrl Pts',(-19.0433688140209,-32.767412552148,
122.262659371029)) ;
#111119 = CARTESIAN_POINT('Ctrl Pts',(-18.8489001005185,-32.7774399106988,
122.343962784584)) ;
#111120 = CARTESIAN_POINT('Ctrl Pts',(-18.673828414615,-32.7873263287499,
122.45604154194)) ;
#111121 = CARTESIAN_POINT('Ctrl Pts',(-18.5186048624772,-32.7973580634853,
122.598762072522)) ;
#111122 = CARTESIAN_POINT('Ctrl Pts',(-18.3922312739287,-32.8072396447286,
122.763692552986)) ;
#111123 = CARTESIAN_POINT('Ctrl Pts',(-18.2946528298106,-32.8173016227609,
122.95133975949)) ;
#111124 = CARTESIAN_POINT('Ctrl Pts',(-18.2323412981276,-32.8271587011226,
123.149007151983)) ;
#111125 = CARTESIAN_POINT('Ctrl Pts',(-18.204510096804,-32.8371532742286,
123.357239039164)) ;
#111126 = CARTESIAN_POINT('Ctrl Pts',(-18.2131241389225,-32.8470790705162,
123.565761767911)) ;
#111127 = CARTESIAN_POINT('Ctrl Pts',(-18.258197970899,-32.857104437686,123.771633144582)) ;
#111128 = CARTESIAN_POINT('Ctrl Pts',(-18.3372272405645,-32.8670005173398,
123.964094221634)) ;
#111129 = CARTESIAN_POINT('Ctrl Pts',(-18.4492248133132,-32.8769955970454,
124.141890841908)) ;
#111130 = CARTESIAN_POINT('Ctrl Pts',(-18.5910790932769,-32.8870206848612,
124.297761386933)) ;
#111131 = CARTESIAN_POINT('Ctrl Pts',(-18.8100939818751,-32.9002045072285,
124.467641769232)) ;
#111132 = CARTESIAN_POINT('Ctrl Pts',(-19.0709210204541,-32.9135266253744,
124.578154880978)) ;
#111133 = CARTESIAN_POINT('Ctrl Pts',(-19.3495998071121,-32.926905835002,
124.616255033073)) ;
#111134 = CARTESIAN_POINT('Ctrl Pts',(-19.5563151397081,-32.9367440722462,
124.608827321986)) ;
#111135 = CARTESIAN_POINT('Ctrl Pts',(-19.7634008442254,-32.946816995505,
124.564684835371)) ;
#111136 = CARTESIAN_POINT('Ctrl Pts',(-19.9554965109162,-32.9566736369601,
124.486920797758)) ;
#111137 = CARTESIAN_POINT('Ctrl Pts',(-20.1337364756346,-32.9666590124661,
124.376044330954)) ;
#111138 = CARTESIAN_POINT('Ctrl Pts',(-20.3414691605472,-32.9799430439266,
124.189421708892)) ;
#111139 = CARTESIAN_POINT('Ctrl Pts',(-20.5342413911385,-32.9964618357969,
123.895712172444)) ;
#111140 = CARTESIAN_POINT('Ctrl Pts',(-20.6157082340627,-33.0132475528035,
123.548262732575)) ;
#111141 = CARTESIAN_POINT('Ctrl Pts',(-20.6070708680724,-33.0263607013125,
123.272702591332)) ;
#111142 = CARTESIAN_POINT('Ctrl Pts',(-20.5647832210259,-33.0363962503927,
123.06602490063)) ;
#111143 = CARTESIAN_POINT('Ctrl Pts',(-20.48681950121,-33.0464123065721,122.870399065451)) ;
#111144 = CARTESIAN_POINT('Ctrl Pts',(-20.3416449321372,-33.0595903424381,
122.634464713355)) ;
#111145 = CARTESIAN_POINT('Ctrl Pts',(-20.0859211980473,-33.0761922196252,
122.391058402553)) ;
#111146 = CARTESIAN_POINT('Ctrl Pts',(-19.6946142274822,-33.0962553642411,
122.221193149357)) ;
#111147 = CARTESIAN_POINT('Ctrl Pts',(-19.274351500161,-33.1160562543248,
122.195138702217)) ;
#111148 = CARTESIAN_POINT('Ctrl Pts',(-18.8673399828958,-33.1359993796035,
122.313861160131)) ;
#111149 = CARTESIAN_POINT('Ctrl Pts',(-18.5261643559591,-33.1558974247231,
122.564047637345)) ;
#111150 = CARTESIAN_POINT('Ctrl Pts',(-18.2900746254247,-33.1757831843499,
122.914893048641)) ;
#111151 = CARTESIAN_POINT('Ctrl Pts',(-18.1876300251765,-33.1958483595298,
123.329014580289)) ;
#111152 = CARTESIAN_POINT('Ctrl Pts',(-18.2322759255964,-33.2156750026326,
123.748284718805)) ;
#111153 = CARTESIAN_POINT('Ctrl Pts',(-18.4169536795342,-33.2355837120809,
124.12906485576)) ;
#111154 = CARTESIAN_POINT('Ctrl Pts',(-18.721236864346,-33.2555355491127,
124.424840811136)) ;
#111155 = CARTESIAN_POINT('Ctrl Pts',(-19.1094164004183,-33.2755440238159,
124.598830114587)) ;
#111156 = CARTESIAN_POINT('Ctrl Pts',(-19.529298702979,-33.2953454825774,
124.630091367489)) ;
#111157 = CARTESIAN_POINT('Ctrl Pts',(-19.9381108978162,-33.3153023708133,
124.516363383193)) ;
#111158 = CARTESIAN_POINT('Ctrl Pts',(-20.2834684399108,-33.3352862082274,
124.268849046373)) ;
#111159 = CARTESIAN_POINT('Ctrl Pts',(-20.5222687847403,-33.3550946474483,
123.921840039079)) ;
#111160 = CARTESIAN_POINT('Ctrl Pts',(-20.6296448046269,-33.3750803568285,
123.510810582247)) ;
#111161 = CARTESIAN_POINT('Ctrl Pts',(-20.5906528432692,-33.3949498798438,
123.089960015209)) ;
#111162 = CARTESIAN_POINT('Ctrl Pts',(-20.4090010950481,-33.414970618961,
122.705145495629)) ;
#111163 = CARTESIAN_POINT('Ctrl Pts',(-20.1103611131004,-33.434774683938,
122.408051963855)) ;
#111164 = CARTESIAN_POINT('Ctrl Pts',(-19.7236069667395,-33.4548366476687,
122.228379429361)) ;
#111165 = CARTESIAN_POINT('Ctrl Pts',(-19.3033477231765,-33.4746698279572,
122.19228617749)) ;
#111166 = CARTESIAN_POINT('Ctrl Pts',(-18.894089623578,-33.4945890252833,
122.301053762642)) ;
#111167 = CARTESIAN_POINT('Ctrl Pts',(-18.5462823598986,-33.5145270503966,
122.543443961697)) ;
#111168 = CARTESIAN_POINT('Ctrl Pts',(-18.3022892801216,-33.5344050964527,
122.888617895256)) ;
#111169 = CARTESIAN_POINT('Ctrl Pts',(-18.1901238358899,-33.5543898307408,
123.29841976143)) ;
#111170 = CARTESIAN_POINT('Ctrl Pts',(-18.2243456643153,-33.5743006474192,
123.720514994806)) ;
#111171 = CARTESIAN_POINT('Ctrl Pts',(-18.4014895416104,-33.594299622938,
124.106981560946)) ;
#111172 = CARTESIAN_POINT('Ctrl Pts',(-18.6967362116398,-33.6141045435832,
124.407368145461)) ;
#111173 = CARTESIAN_POINT('Ctrl Pts',(-19.0797620543256,-33.6340885038744,
124.591098017542)) ;
#111174 = CARTESIAN_POINT('Ctrl Pts',(-19.5006266056499,-33.6539747075983,
124.632722196139)) ;
#111175 = CARTESIAN_POINT('Ctrl Pts',(-19.911731941663,-33.6739238859215,
124.528393098124)) ;
#111176 = CARTESIAN_POINT('Ctrl Pts',(-20.261690387992,-33.6938256851611,
124.290509068858)) ;
#111177 = CARTESIAN_POINT('Ctrl Pts',(-20.5099189608146,-33.7137042902134,
123.94837982416)) ;
#111178 = CARTESIAN_POINT('Ctrl Pts',(-20.6272087060775,-33.7337366499391,
123.538874173407)) ;
#111179 = CARTESIAN_POINT('Ctrl Pts',(-20.6022470734653,-33.7503183758952,
123.187197869442)) ;
#111180 = CARTESIAN_POINT('Ctrl Pts',(-20.5124584713011,-33.7635125461931,
122.924736823265)) ;
#111181 = CARTESIAN_POINT('Ctrl Pts',(-20.3777000671248,-33.7768247242863,
122.679516465303)) ;
#111182 = CARTESIAN_POINT('Ctrl Pts',(-20.1339983690097,-33.7933909038797,
122.425063683071)) ;
#111183 = CARTESIAN_POINT('Ctrl Pts',(-19.8172247792237,-33.8100190987398,
122.268242034196)) ;
#111184 = CARTESIAN_POINT('Ctrl Pts',(-19.5432355209233,-33.8233076804496,
122.213312671982)) ;
#111185 = CARTESIAN_POINT('Ctrl Pts',(-19.3337564759155,-33.8332759285532,
122.208248783748)) ;
#111186 = CARTESIAN_POINT('Ctrl Pts',(-19.1276245549163,-33.8431906848093,
122.239209963793)) ;
#111187 = CARTESIAN_POINT('Ctrl Pts',(-18.9279613092715,-33.8532038354605,
122.30593018381)) ;
#111188 = CARTESIAN_POINT('Ctrl Pts',(-18.7430898166205,-33.8632165426625,
122.406594889193)) ;
#111189 = CARTESIAN_POINT('Ctrl Pts',(-18.5254733609243,-33.8764358313538,
122.579427031468)) ;
#111190 = CARTESIAN_POINT('Ctrl Pts',(-18.3148416700841,-33.8930545123519,
122.863105264753)) ;
#111191 = CARTESIAN_POINT('Ctrl Pts',(-18.2135484225965,-33.9096194201253,
123.200460683676)) ;
#111192 = CARTESIAN_POINT('Ctrl Pts',(-18.2053484474901,-33.9230178917362,
123.482045141024)) ;
#111193 = CARTESIAN_POINT('Ctrl Pts',(-18.2351320382913,-33.9328591472231,
123.686795125231)) ;
#111194 = CARTESIAN_POINT('Ctrl Pts',(-18.3005160780668,-33.9428454628113,
123.886263768473)) ;
#111195 = CARTESIAN_POINT('Ctrl Pts',(-18.3989921231265,-33.9527820703977,
124.070534261)) ;
#111196 = CARTESIAN_POINT('Ctrl Pts',(-18.5294851402055,-33.962831937766,
124.236671820662)) ;
#111197 = CARTESIAN_POINT('Ctrl Pts',(-18.6836450057974,-33.9726824324408,
124.374971489095)) ;
#111198 = CARTESIAN_POINT('Ctrl Pts',(-18.8613157630865,-33.9826542328353,
124.486192409667)) ;
#111199 = CARTESIAN_POINT('Ctrl Pts',(-19.0561371062447,-33.9926501998612,
124.565067005719)) ;
#111200 = CARTESIAN_POINT('Ctrl Pts',(-19.2625528780155,-34.0026876592423,
124.608805121776)) ;
#111201 = CARTESIAN_POINT('Ctrl Pts',(-19.4693150818045,-34.0125283601431,
124.616289159939)) ;
#111202 = CARTESIAN_POINT('Ctrl Pts',(-19.6785718860248,-34.0225763814104,
124.587470375843)) ;
#111203 = CARTESIAN_POINT('Ctrl Pts',(-19.8775406913797,-34.0325237744931,
124.523081359573)) ;
#111204 = CARTESIAN_POINT('Ctrl Pts',(-20.0619206158677,-34.0424339205395,
124.426049034927)) ;
#111205 = CARTESIAN_POINT('Ctrl Pts',(-20.2289520631335,-34.0524928343891,
124.296392276593)) ;
#111206 = CARTESIAN_POINT('Ctrl Pts',(-20.3681027880477,-34.0623336046784,
124.143259875445)) ;
#111207 = CARTESIAN_POINT('Ctrl Pts',(-20.4812240140718,-34.0723964742571,
123.964522289183)) ;
#111208 = CARTESIAN_POINT('Ctrl Pts',(-20.5601075070064,-34.0822907973875,
123.772026359654)) ;
#111209 = CARTESIAN_POINT('Ctrl Pts',(-20.6051242676879,-34.092232604482,
123.567950255567)) ;
#111210 = CARTESIAN_POINT('Ctrl Pts',(-20.6141585892128,-34.1022351154374,
123.357831532396)) ;
#111211 = CARTESIAN_POINT('Ctrl Pts',(-20.586160972297,-34.1122698362557,
123.148748981869)) ;
#111212 = CARTESIAN_POINT('Ctrl Pts',(-20.5238102195263,-34.1221150137615,
122.951374645537)) ;
#111213 = CARTESIAN_POINT('Ctrl Pts',(-20.4271652846039,-34.1320997741625,
122.765068487965)) ;
#111214 = CARTESIAN_POINT('Ctrl Pts',(-20.3002677681671,-34.1420386804789,
122.599029198552)) ;
#111215 = CARTESIAN_POINT('Ctrl Pts',(-20.144858671582,-34.1520809081147,
122.456164531375)) ;
#111216 = CARTESIAN_POINT('Ctrl Pts',(-19.969828377326,-34.161966119699,122.344082055439)) ;
#111217 = CARTESIAN_POINT('Ctrl Pts',(-19.7759430930242,-34.171965049901,
122.262943911718)) ;
#111218 = CARTESIAN_POINT('Ctrl Pts',(-19.5725573403791,-34.1818824728114,
122.216910572559)) ;
#111219 = CARTESIAN_POINT('Ctrl Pts',(-19.3615911403277,-34.1919304048901,
122.206803419125)) ;
#111220 = CARTESIAN_POINT('Ctrl Pts',(-19.1555400792907,-34.2018077806995,
122.23283367733)) ;
#111221 = CARTESIAN_POINT('Ctrl Pts',(-18.9536299337116,-34.2118616738674,
122.29521910007)) ;
#111222 = CARTESIAN_POINT('Ctrl Pts',(-18.7685026689917,-34.2217552971207,
122.390126408204)) ;
#111223 = CARTESIAN_POINT('Ctrl Pts',(-18.5998752959417,-34.2318178907437,
122.517809167733)) ;
#111224 = CARTESIAN_POINT('Ctrl Pts',(-18.4590073721732,-34.2416604647328,
122.669410488933)) ;
#111225 = CARTESIAN_POINT('Ctrl Pts',(-18.3445175761883,-34.2516512216157,
122.845468473704)) ;
#111226 = CARTESIAN_POINT('Ctrl Pts',(-18.2628714138679,-34.2615792833737,
123.037566658329)) ;
#111227 = CARTESIAN_POINT('Ctrl Pts',(-18.2151802603476,-34.2715672592628,
123.242066313336)) ;
#111228 = CARTESIAN_POINT('Ctrl Pts',(-18.2040198515877,-34.2816029236193,
123.452746057416)) ;
#111229 = CARTESIAN_POINT('Ctrl Pts',(-18.2288306331781,-34.2914588620389,
123.658468698724)) ;
#111230 = CARTESIAN_POINT('Ctrl Pts',(-18.2894970662497,-34.3014543534358,
123.859634562195)) ;
#111231 = CARTESIAN_POINT('Ctrl Pts',(-18.3833175267175,-34.3113641583893,
124.045659980296)) ;
#111232 = CARTESIAN_POINT('Ctrl Pts',(-18.5090245348309,-34.321376380656,
124.214494784121)) ;
#111233 = CARTESIAN_POINT('Ctrl Pts',(-18.6626570593713,-34.3314042613489,
124.358861992873)) ;
#111234 = CARTESIAN_POINT('Ctrl Pts',(-18.8358100465464,-34.3412606573315,
124.472679095895)) ;
#111235 = CARTESIAN_POINT('Ctrl Pts',(-19.0291759498572,-34.3512854545114,
124.55651008144)) ;
#111236 = CARTESIAN_POINT('Ctrl Pts',(-19.2344095278912,-34.3613163844952,
124.605019584198)) ;
#111237 = CARTESIAN_POINT('Ctrl Pts',(-19.4409992862381,-34.3711609870039,
124.617302775841)) ;
#111238 = CARTESIAN_POINT('Ctrl Pts',(-19.6497175181962,-34.381151838228,
124.593741483947)) ;
#111239 = CARTESIAN_POINT('Ctrl Pts',(-19.8519812717914,-34.3911896712392,
124.533566543043)) ;
#111240 = CARTESIAN_POINT('Ctrl Pts',(-20.0372566388389,-34.4010340597047,
124.44132477663)) ;
#111241 = CARTESIAN_POINT('Ctrl Pts',(-20.2062935579755,-34.4110188640742,
124.316914757588)) ;
#111242 = CARTESIAN_POINT('Ctrl Pts',(-20.3506086836628,-34.4209583835571,
124.165754613573)) ;
#111243 = CARTESIAN_POINT('Ctrl Pts',(-20.4675870896656,-34.4309981145584,
123.990089351953)) ;
#111244 = CARTESIAN_POINT('Ctrl Pts',(-20.5511156753519,-34.4408862428047,
123.799716285732)) ;
#111245 = CARTESIAN_POINT('Ctrl Pts',(-20.6012008940428,-34.4508759680132,
123.595768743447)) ;
#111246 = CARTESIAN_POINT('Ctrl Pts',(-20.6149183330863,-34.4608337327147,
123.386878194724)) ;
#111247 = CARTESIAN_POINT('Ctrl Pts',(-20.5927684673275,-34.4707360741267,
123.179874670469)) ;
#111248 = CARTESIAN_POINT('Ctrl Pts',(-20.5341702978408,-34.4807802698331,
122.977018193298)) ;
#111249 = CARTESIAN_POINT('Ctrl Pts',(-20.4425166301804,-34.4906876705924,
122.78997097188)) ;
#111250 = CARTESIAN_POINT('Ctrl Pts',(-20.3188031174288,-34.5006982704667,
122.619714411063)) ;
#111251 = CARTESIAN_POINT('Ctrl Pts',(-20.1668235411832,-34.5107285663789,
122.473528441037)) ;
#111252 = CARTESIAN_POINT('Ctrl Pts',(-19.9950092007968,-34.5205833460286,
122.357781229142)) ;
#111253 = CARTESIAN_POINT('Ctrl Pts',(-19.8039794053567,-34.5305406742461,
122.272158018811)) ;
#111254 = CARTESIAN_POINT('Ctrl Pts',(-19.5992481195288,-34.540579707153,
122.220952089567)) ;
#111255 = CARTESIAN_POINT('Ctrl Pts',(-19.3921953913607,-34.5504528190423,
122.205929381447)) ;
#111256 = CARTESIAN_POINT('Ctrl Pts',(-19.1815753178159,-34.5605261040694,
122.227570733735)) ;
#111257 = CARTESIAN_POINT('Ctrl Pts',(-18.9828684301485,-34.5703464238062,
122.283763766445)) ;
#111258 = CARTESIAN_POINT('Ctrl Pts',(-18.7920486869385,-34.5804250891846,
122.37575024978)) ;
#111259 = CARTESIAN_POINT('Ctrl Pts',(-18.62385065284,-34.5902766796684,122.496683357487)) ;
#111260 = CARTESIAN_POINT('Ctrl Pts',(-18.4758820061033,-34.6003498299873,
122.648127424558)) ;
#111261 = CARTESIAN_POINT('Ctrl Pts',(-18.3591839794984,-34.6101922099624,
122.819021731713)) ;
#111262 = CARTESIAN_POINT('Ctrl Pts',(-18.2721174003429,-34.6201731862054,
123.009919983954)) ;
#111263 = CARTESIAN_POINT('Ctrl Pts',(-18.2196704611977,-34.6301895145607,
123.213870251278)) ;
#111264 = CARTESIAN_POINT('Ctrl Pts',(-18.2033629295152,-34.6400873115519,
123.421305021254)) ;
#111265 = CARTESIAN_POINT('Ctrl Pts',(-18.2231956668317,-34.6500998682839,
123.63087967846)) ;
#111266 = CARTESIAN_POINT('Ctrl Pts',(-18.2796995522642,-34.6601319031304,
123.834064442886)) ;
#111267 = CARTESIAN_POINT('Ctrl Pts',(-18.3684247329062,-34.6699713039459,
124.020942950508)) ;
#111268 = CARTESIAN_POINT('Ctrl Pts',(-18.4908530383524,-34.6800370895974,
124.19351681441)) ;
#111269 = CARTESIAN_POINT('Ctrl Pts',(-18.6388650570813,-34.689927544712,
124.339584143233)) ;
#111270 = CARTESIAN_POINT('Ctrl Pts',(-18.8114664666422,-34.6999196633478,
124.459300233467)) ;
#111271 = CARTESIAN_POINT('Ctrl Pts',(-19.0017602372872,-34.7098824901109,
124.546794762991)) ;
#111272 = CARTESIAN_POINT('Ctrl Pts',(-19.2030523352962,-34.7197867733837,
124.60012274474)) ;
#111273 = CARTESIAN_POINT('Ctrl Pts',(-19.4137905275479,-34.7298472073308,
124.617781357666)) ;
#111274 = CARTESIAN_POINT('Ctrl Pts',(-19.6198660615148,-34.739687760004,
124.599260033499)) ;
#111275 = CARTESIAN_POINT('Ctrl Pts',(-19.824116758414,-34.7497499799497,
124.544295335213)) ;
#111276 = CARTESIAN_POINT('Ctrl Pts',(-20.0125152682012,-34.7596471192283,
124.455960258011)) ;
#111277 = CARTESIAN_POINT('Ctrl Pts',(-20.1836871158852,-34.7695783113634,
124.336420819834)) ;
#111278 = CARTESIAN_POINT('Ctrl Pts',(-20.3329870852971,-34.7796204660084,
124.187162803798)) ;
#111279 = CARTESIAN_POINT('Ctrl Pts',(-20.4523816066316,-34.7895072270277,
124.017004336229)) ;
#111280 = CARTESIAN_POINT('Ctrl Pts',(-20.5416439250666,-34.799506528745,
123.826710791505)) ;
#111281 = CARTESIAN_POINT('Ctrl Pts',(-20.5962295758391,-34.8094273269117,
123.625384524441)) ;
#111282 = CARTESIAN_POINT('Ctrl Pts',(-20.6152613604502,-34.8194613805084,
123.415320824013)) ;
#111283 = CARTESIAN_POINT('Ctrl Pts',(-20.5978472517342,-34.8293844980748,
123.20740189344)) ;
#111284 = CARTESIAN_POINT('Ctrl Pts',(-20.5438513344793,-34.839440621574,
123.003024081087)) ;
#111285 = CARTESIAN_POINT('Ctrl Pts',(-20.4571161714757,-34.8492860632288,
122.815082617948)) ;
#111286 = CARTESIAN_POINT('Ctrl Pts',(-20.3382431442323,-34.8592483643529,
122.642663692333)) ;
#111287 = CARTESIAN_POINT('Ctrl Pts',(-20.1900442363744,-34.8692768436281,
122.492688745898)) ;
#111288 = CARTESIAN_POINT('Ctrl Pts',(-20.020143034041,-34.8791871971377,
122.372116826232)) ;
#111289 = CARTESIAN_POINT('Ctrl Pts',(-19.8316411016788,-34.8891220693149,
122.282155355649)) ;
#111290 = CARTESIAN_POINT('Ctrl Pts',(-19.6281895716657,-34.8991632069006,
122.225885570986)) ;
#111291 = CARTESIAN_POINT('Ctrl Pts',(-19.4212767291133,-34.9090503561152,
122.205957500959)) ;
#111292 = CARTESIAN_POINT('Ctrl Pts',(-19.2118424556958,-34.9190425908663,
122.222079971605)) ;
#111293 = CARTESIAN_POINT('Ctrl Pts',(-19.0092661997009,-34.9289912964292,
122.274160394646)) ;
#111294 = CARTESIAN_POINT('Ctrl Pts',(-18.8189496627,-34.9389273648529,122.360225751965)) ;
#111295 = CARTESIAN_POINT('Ctrl Pts',(-18.6454413921216,-34.9489130490687,
122.478439150244)) ;
#111296 = CARTESIAN_POINT('Ctrl Pts',(-18.494526960012,-34.9589534756374,
122.626004432111)) ;
#111297 = CARTESIAN_POINT('Ctrl Pts',(-18.3737039740162,-34.9687925891011,
122.793902583486)) ;
#111298 = CARTESIAN_POINT('Ctrl Pts',(-18.2817008900092,-34.9788223232769,
122.983631407706)) ;
#111299 = CARTESIAN_POINT('Ctrl Pts',(-18.2246114593742,-34.9888444227828,
123.18644384283)) ;
#111300 = CARTESIAN_POINT('Ctrl Pts',(-18.2034063943752,-34.9987128626763,
123.392838308102)) ;
#111301 = CARTESIAN_POINT('Ctrl Pts',(-18.2186669876198,-35.0087817273619,
123.603947850047)) ;
#111302 = CARTESIAN_POINT('Ctrl Pts',(-18.2691895098107,-35.0186244004605,
123.804616201168)) ;
#111303 = CARTESIAN_POINT('Ctrl Pts',(-18.3540964494701,-35.0285850346229,
123.996029309736)) ;
#111304 = CARTESIAN_POINT('Ctrl Pts',(-18.4721989122427,-35.0386229503011,
124.170905820594)) ;
#111305 = CARTESIAN_POINT('Ctrl Pts',(-18.6162270642338,-35.0484972251605,
124.320436137073)) ;
#111306 = CARTESIAN_POINT('Ctrl Pts',(-18.7873162126898,-35.0585669755356,
124.445065769784)) ;
#111307 = CARTESIAN_POINT('Ctrl Pts',(-18.9729724040706,-35.0684002709101,
124.536030391313)) ;
#111308 = CARTESIAN_POINT('Ctrl Pts',(-19.1753937077913,-35.0784305683898,
124.595095249358)) ;
#111309 = CARTESIAN_POINT('Ctrl Pts',(-19.3851154487914,-35.0884626548312,
124.617503718348)) ;
#111310 = CARTESIAN_POINT('Ctrl Pts',(-19.5912719153366,-35.0982905833201,
124.603904305506)) ;
#111311 = CARTESIAN_POINT('Ctrl Pts',(-19.7955090552236,-35.1082866244309,
124.554420478054)) ;
#111312 = CARTESIAN_POINT('Ctrl Pts',(-19.9884689771848,-35.1183124365321,
124.469598741811)) ;
#111313 = CARTESIAN_POINT('Ctrl Pts',(-20.1614939021767,-35.1281996714269,
124.354404799942)) ;
#111314 = CARTESIAN_POINT('Ctrl Pts',(-20.3134788784359,-35.138176537638,
124.209881679991)) ;
#111315 = CARTESIAN_POINT('Ctrl Pts',(-20.4383178055652,-35.1481694815098,
124.04087805112)) ;
#111316 = CARTESIAN_POINT('Ctrl Pts',(-20.532077004532,-35.1582074041811,
123.851839699254)) ;
#111317 = CARTESIAN_POINT('Ctrl Pts',(-20.5907738467583,-35.1680558684428,
123.653272389979)) ;
#111318 = CARTESIAN_POINT('Ctrl Pts',(-20.6148079463407,-35.1780477351868,
123.444622192885)) ;
#111319 = CARTESIAN_POINT('Ctrl Pts',(-20.6024561591228,-35.187965467228,
123.236459374795)) ;
#111320 = CARTESIAN_POINT('Ctrl Pts',(-20.5536749365443,-35.1979936521233,
123.031374270941)) ;
#111321 = CARTESIAN_POINT('Ctrl Pts',(-20.4712889430407,-35.2078788101721,
122.840579545261)) ;
#111322 = CARTESIAN_POINT('Ctrl Pts',(-20.3562493607325,-35.2178681707138,
122.664878277586)) ;
#111323 = CARTESIAN_POINT('Ctrl Pts',(-20.2113820099639,-35.2279093276482,
122.511335986107)) ;
#111324 = CARTESIAN_POINT('Ctrl Pts',(-20.0457798750078,-35.2377419111033,
122.38762552669)) ;
#111325 = CARTESIAN_POINT('Ctrl Pts',(-19.8584474655071,-35.2477361310653,
122.292485495827)) ;
#111326 = CARTESIAN_POINT('Ctrl Pts',(-19.6566267408171,-35.2577642328526,
122.231520181329)) ;
#111327 = CARTESIAN_POINT('Ctrl Pts',(-19.450416436115,-35.2676441774757,
122.206599298197)) ;
#111328 = CARTESIAN_POINT('Ctrl Pts',(-19.2406925010912,-35.2776345040327,
122.217663247814)) ;
#111329 = CARTESIAN_POINT('Ctrl Pts',(-19.037070040132,-35.287575435687,122.264742809954)) ;
#111330 = CARTESIAN_POINT('Ctrl Pts',(-18.8436947821256,-35.2975625541899,
122.346570403201)) ;
#111331 = CARTESIAN_POINT('Ctrl Pts',(-18.6668553018261,-35.3075958870871,
122.461522490985)) ;
#111332 = CARTESIAN_POINT('Ctrl Pts',(-18.5149265051629,-35.3174619915319,
122.602763665917)) ;
#111333 = CARTESIAN_POINT('Ctrl Pts',(-18.3872831444672,-35.3275281054122,
122.77152549007)) ;
#111334 = CARTESIAN_POINT('Ctrl Pts',(-18.2928656067779,-35.3373841171806,
122.955984013624)) ;
#111335 = CARTESIAN_POINT('Ctrl Pts',(-18.230465961538,-35.3473788208119,
123.156618928905)) ;
#111336 = CARTESIAN_POINT('Ctrl Pts',(-18.2042001744746,-35.3574101565368,
123.365870947332)) ;
#111337 = CARTESIAN_POINT('Ctrl Pts',(-18.2141648932899,-35.3672766817405,
123.573063985548)) ;
#111338 = CARTESIAN_POINT('Ctrl Pts',(-18.2601775539436,-35.3772641097863,
123.77790193493)) ;
#111339 = CARTESIAN_POINT('Ctrl Pts',(-18.3406310032263,-35.3872090394727,
123.970909548811)) ;
#111340 = CARTESIAN_POINT('Ctrl Pts',(-18.4545817808251,-35.3972539575812,
124.148679017072)) ;
#111341 = CARTESIAN_POINT('Ctrl Pts',(-18.59495026283,-35.4071159271951,124.301287123249)) ;
#111342 = CARTESIAN_POINT('Ctrl Pts',(-18.7615786815796,-35.4171079952163,
124.429167522647)) ;
#111343 = CARTESIAN_POINT('Ctrl Pts',(-18.9467874257851,-35.4270389205909,
124.525562443922)) ;
#111344 = CARTESIAN_POINT('Ctrl Pts',(-19.1461828867164,-35.4369895488143,
124.58878520872)) ;
#111345 = CARTESIAN_POINT('Ctrl Pts',(-19.3545825069938,-35.4469897878734,
124.616689033974)) ;
#111346 = CARTESIAN_POINT('Ctrl Pts',(-19.5652104007088,-35.4570182432426,
124.607656602288)) ;
#111347 = CARTESIAN_POINT('Ctrl Pts',(-19.7678210459839,-35.4668842778259,
124.563227768607)) ;
#111348 = CARTESIAN_POINT('Ctrl Pts',(-19.9621986440151,-35.4768765995733,
124.483614782916)) ;
#111349 = CARTESIAN_POINT('Ctrl Pts',(-20.1387827535857,-35.4868088892503,
124.372143287744)) ;
#111350 = CARTESIAN_POINT('Ctrl Pts',(-20.2945277553807,-35.4968105342211,
124.230893520391)) ;
#111351 = CARTESIAN_POINT('Ctrl Pts',(-20.4659698004387,-35.5101231676371,
124.009636120394)) ;
#111352 = CARTESIAN_POINT('Ctrl Pts',(-20.5752600415281,-35.5233549170187,
123.750378115547)) ;
#111353 = CARTESIAN_POINT('Ctrl Pts',(-20.61365827496,-35.5366781818358,123.472967009072)) ;
#111354 = CARTESIAN_POINT('Ctrl Pts',(-20.606300706745,-35.5465538880534,
123.265462332407)) ;
#111355 = CARTESIAN_POINT('Ctrl Pts',(-20.5627998349141,-35.5565434791535,
123.060029415646)) ;
#111356 = CARTESIAN_POINT('Ctrl Pts',(-20.4848914604262,-35.5664705756089,
122.86639032806)) ;
#111357 = CARTESIAN_POINT('Ctrl Pts',(-20.3734990076902,-35.5764957241134,
122.687494701056)) ;
#111358 = CARTESIAN_POINT('Ctrl Pts',(-20.2346261347806,-35.5863913782601,
122.532570025056)) ;
#111359 = CARTESIAN_POINT('Ctrl Pts',(-20.069392983769,-35.5963949126383,
122.40250052827)) ;
#111360 = CARTESIAN_POINT('Ctrl Pts',(-19.8843701761844,-35.6063800510784,
122.303273447116)) ;
#111361 = CARTESIAN_POINT('Ctrl Pts',(-19.6838893863715,-35.6164159756738,
122.237560806524)) ;
#111362 = CARTESIAN_POINT('Ctrl Pts',(-19.4789119228008,-35.6262672511014,
122.207961790604)) ;
#111363 = CARTESIAN_POINT('Ctrl Pts',(-19.2689199019656,-35.6362595122628,
122.213895904953)) ;
#111364 = CARTESIAN_POINT('Ctrl Pts',(-19.0622933373956,-35.6462993962804,
122.256922553656)) ;
#111365 = CARTESIAN_POINT('Ctrl Pts',(-18.8700530340583,-35.6561341707828,
122.333100099704)) ;
#111366 = CARTESIAN_POINT('Ctrl Pts',(-18.6896438171072,-35.6662105518031,
122.444065459644)) ;
#111367 = CARTESIAN_POINT('Ctrl Pts',(-18.5347774515829,-35.6760568249538,
122.581455503724)) ;
#111368 = CARTESIAN_POINT('Ctrl Pts',(-18.3597507997684,-35.689421346239,
122.801250462498)) ;
#111369 = CARTESIAN_POINT('Ctrl Pts',(-18.2477902793086,-35.7026275906734,
123.05879644847)) ;
#111370 = CARTESIAN_POINT('Ctrl Pts',(-18.205714641466,-35.7158925453506,
123.334416907952)) ;
#111371 = CARTESIAN_POINT('Ctrl Pts',(-18.2106623110942,-35.7259248259023,
123.545283524578)) ;
#111372 = CARTESIAN_POINT('Ctrl Pts',(-18.2516205902962,-35.7358335594202,
123.749523566181)) ;
#111373 = CARTESIAN_POINT('Ctrl Pts',(-18.3271374520613,-35.7457711102877,
123.944325473825)) ;
#111374 = CARTESIAN_POINT('Ctrl Pts',(-18.4364698117058,-35.7558009578817,
124.124598503643)) ;
#111375 = CARTESIAN_POINT('Ctrl Pts',(-18.6196409824421,-35.7690360978021,
124.334155609205)) ;
#111376 = CARTESIAN_POINT('Ctrl Pts',(-18.91389130429,-35.7857045621733,124.531485319361)) ;
#111377 = CARTESIAN_POINT('Ctrl Pts',(-19.3240838980477,-35.8055755740472,
124.633322926257)) ;
#111378 = CARTESIAN_POINT('Ctrl Pts',(-19.6773099932291,-35.8222826584301,
124.596016932901)) ;
#111379 = CARTESIAN_POINT('Ctrl Pts',(-19.9358939662199,-35.8354599397407,
124.496620570408)) ;
#111380 = CARTESIAN_POINT('Ctrl Pts',(-20.1754328411166,-35.8487274002548,
124.35371542067)) ;
#111381 = CARTESIAN_POINT('Ctrl Pts',(-20.4216852858064,-35.865341290942,
124.100451035231)) ;
#111382 = CARTESIAN_POINT('Ctrl Pts',(-20.5958971094138,-35.8852900903694,
123.7136635781)) ;
#111383 = CARTESIAN_POINT('Ctrl Pts',(-20.6275338812049,-35.9052112019003,
123.291329293392)) ;
#111384 = CARTESIAN_POINT('Ctrl Pts',(-20.5142789827827,-35.9250776500732,
122.884311703603)) ;
#111385 = CARTESIAN_POINT('Ctrl Pts',(-20.2668111895115,-35.9451039966903,
122.537847342949)) ;
#111386 = CARTESIAN_POINT('Ctrl Pts',(-19.9187011974883,-35.9649660410798,
122.29860611084)) ;
#111387 = CARTESIAN_POINT('Ctrl Pts',(-19.5084301973606,-35.984911343761,
122.191459288078)) ;
#111388 = CARTESIAN_POINT('Ctrl Pts',(-19.0872180869834,-36.0048066508198,
122.230722818326)) ;
#111389 = CARTESIAN_POINT('Ctrl Pts',(-18.7044045266393,-36.0246999209875,
122.410659196091)) ;
#111390 = CARTESIAN_POINT('Ctrl Pts',(-18.4049751985419,-36.0446655136679,
122.711557332103)) ;
#111391 = CARTESIAN_POINT('Ctrl Pts',(-18.2267181486412,-36.0645408373527,
123.094752957051)) ;
#111392 = CARTESIAN_POINT('Ctrl Pts',(-18.1893125835567,-36.0845158999277,
123.517845578166)) ;
#111393 = CARTESIAN_POINT('Ctrl Pts',(-18.2990250608244,-36.1044683095588,
123.927655337161)) ;
#111394 = CARTESIAN_POINT('Ctrl Pts',(-18.5399109172271,-36.1243043637949,
124.273866236982)) ;
#111395 = CARTESIAN_POINT('Ctrl Pts',(-18.8866732207326,-36.1442822752124,
124.519217496431)) ;
#111396 = CARTESIAN_POINT('Ctrl Pts',(-19.2952239326377,-36.1642003247159,
124.63068224588)) ;
#111397 = CARTESIAN_POINT('Ctrl Pts',(-19.7164354601563,-36.184068468484,
124.597224185815)) ;
#111398 = CARTESIAN_POINT('Ctrl Pts',(-20.1040334649446,-36.2041193250713,
124.419912317543)) ;
#111399 = CARTESIAN_POINT('Ctrl Pts',(-20.4042347842874,-36.2238997615272,
124.125172356029)) ;
#111400 = CARTESIAN_POINT('Ctrl Pts',(-20.5886490222637,-36.243929817205,
123.741383064753)) ;
#111401 = CARTESIAN_POINT('Ctrl Pts',(-20.6300092332548,-36.2638109223798,
123.320612273952)) ;
#111402 = CARTESIAN_POINT('Ctrl Pts',(-20.5264874980267,-36.2836913847476,
122.91081547106)) ;
#111403 = CARTESIAN_POINT('Ctrl Pts',(-20.2879610963858,-36.303676531892,
122.559120563189)) ;
#111404 = CARTESIAN_POINT('Ctrl Pts',(-19.9453095601295,-36.3235671104283,
122.31119799223)) ;
#111405 = CARTESIAN_POINT('Ctrl Pts',(-19.5387738824579,-36.3434611303027,
122.194351442702)) ;
#111406 = CARTESIAN_POINT('Ctrl Pts',(-19.116240251417,-36.3633825750291,
122.223172528786)) ;
#111407 = CARTESIAN_POINT('Ctrl Pts',(-18.7288844738135,-36.3832807130846,
122.393638320056)) ;
#111408 = CARTESIAN_POINT('Ctrl Pts',(-18.421004213588,-36.4033514683006,
122.689049307375)) ;
#111409 = CARTESIAN_POINT('Ctrl Pts',(-18.2348386703719,-36.4231370183519,
123.066415114148)) ;
#111410 = CARTESIAN_POINT('Ctrl Pts',(-18.1871546931954,-36.4431200932292,
123.488546741973)) ;
#111411 = CARTESIAN_POINT('Ctrl Pts',(-18.2866782259088,-36.4630291758752,
123.900007586698)) ;
#111412 = CARTESIAN_POINT('Ctrl Pts',(-18.5190543274305,-36.4828877349979,
124.252624939886)) ;
#111413 = CARTESIAN_POINT('Ctrl Pts',(-18.8611588618101,-36.5029311788366,
124.506642312783)) ;
#111414 = CARTESIAN_POINT('Ctrl Pts',(-19.1973161146736,-36.5194312435658,
124.607325426955)) ;
#111415 = CARTESIAN_POINT('Ctrl Pts',(-19.4786627604574,-36.5328209834147,
124.615826937265)) ;
#111416 = CARTESIAN_POINT('Ctrl Pts',(-19.6837652848018,-36.5426778846231,
124.586090935942)) ;
#111417 = CARTESIAN_POINT('Ctrl Pts',(-19.8833582941557,-36.5526694104696,
124.520735560093)) ;
#111418 = CARTESIAN_POINT('Ctrl Pts',(-20.0674233220451,-36.5625940909206,
124.422418051402)) ;
#111419 = CARTESIAN_POINT('Ctrl Pts',(-20.2330492966152,-36.572604680965,
124.292613071805)) ;
#111420 = CARTESIAN_POINT('Ctrl Pts',(-20.4195222062165,-36.5858639416687,
124.085379818857)) ;
#111421 = CARTESIAN_POINT('Ctrl Pts',(-20.5482092582577,-36.5992150168189,
123.83241540766)) ;
#111422 = CARTESIAN_POINT('Ctrl Pts',(-20.6059663778409,-36.6124213260537,
123.560779051882)) ;
#111423 = CARTESIAN_POINT('Ctrl Pts',(-20.6137317458316,-36.622408159644,
123.351006750326)) ;
#111424 = CARTESIAN_POINT('Ctrl Pts',(-20.5851472722717,-36.6323608871401,
123.143693383766)) ;
#111425 = CARTESIAN_POINT('Ctrl Pts',(-20.5202354143856,-36.6424089839817,
122.942695716871)) ;
#111426 = CARTESIAN_POINT('Ctrl Pts',(-20.4236378085152,-36.6522504408535,
122.759708760837)) ;
#111427 = CARTESIAN_POINT('Ctrl Pts',(-20.2952557917833,-36.662236707767,
122.593637620156)) ;
#111428 = CARTESIAN_POINT('Ctrl Pts',(-20.1407800757662,-36.6721733086674,
122.452959070845)) ;
#111429 = CARTESIAN_POINT('Ctrl Pts',(-19.9622013251309,-36.6822232514545,
122.340085108477)) ;
#111430 = CARTESIAN_POINT('Ctrl Pts',(-19.770647907417,-36.6920734511402,
122.261368668836)) ;
#111431 = CARTESIAN_POINT('Ctrl Pts',(-19.5659718905042,-36.7020463560723,
122.216024336144)) ;
#111432 = CARTESIAN_POINT('Ctrl Pts',(-19.3559444745547,-36.712044730552,
122.206949462971)) ;
#111433 = CARTESIAN_POINT('Ctrl Pts',(-19.1471291615711,-36.7220649044219,
122.234686372883)) ;
#111434 = CARTESIAN_POINT('Ctrl Pts',(-18.9486238237768,-36.7319659483639,
122.297335154375)) ;
#111435 = CARTESIAN_POINT('Ctrl Pts',(-18.7622286417222,-36.7419547520882,
122.394055169228)) ;
#111436 = CARTESIAN_POINT('Ctrl Pts',(-18.5959457277222,-36.7519202189201,
122.521485476503)) ;
#111437 = CARTESIAN_POINT('Ctrl Pts',(-18.4548033425623,-36.761823781193,
122.674574505268)) ;
#111438 = CARTESIAN_POINT('Ctrl Pts',(-18.3407750617073,-36.771884459071,
122.852679614005)) ;
#111439 = CARTESIAN_POINT('Ctrl Pts',(-18.2609184875223,-36.7817247570205,
123.043551941228)) ;
#111440 = CARTESIAN_POINT('Ctrl Pts',(-18.214149636979,-36.7917877519299,
123.249845265548)) ;
#111441 = CARTESIAN_POINT('Ctrl Pts',(-18.2042519096971,-36.8016820460771,
123.45764127111)) ;
#111442 = CARTESIAN_POINT('Ctrl Pts',(-18.230142237402,-36.8116238437739,
123.665013488537)) ;
#111443 = CARTESIAN_POINT('Ctrl Pts',(-18.29196396426,-36.821626421303,123.866035481059)) ;
#111444 = CARTESIAN_POINT('Ctrl Pts',(-18.3883277917964,-36.8316608852241,
124.053684162638)) ;
#111445 = CARTESIAN_POINT('Ctrl Pts',(-18.513168929447,-36.8415070237452,
124.218805314199)) ;
#111446 = CARTESIAN_POINT('Ctrl Pts',(-18.6665278100136,-36.8514881969822,
124.362001094646)) ;
#111447 = CARTESIAN_POINT('Ctrl Pts',(-18.8419581496268,-36.8614404909394,
124.476033554616)) ;
#111448 = CARTESIAN_POINT('Ctrl Pts',(-19.0353255574773,-36.871439286074,
124.558511020834)) ;
#111449 = CARTESIAN_POINT('Ctrl Pts',(-19.2409658848742,-36.8814783943348,
124.605951228771)) ;
#111450 = CARTESIAN_POINT('Ctrl Pts',(-19.4472244351549,-36.891303335774,
124.617174411097)) ;
#111451 = CARTESIAN_POINT('Ctrl Pts',(-19.6571102913545,-36.9013580228484,
124.592183126847)) ;
#111452 = CARTESIAN_POINT('Ctrl Pts',(-19.8571315570534,-36.9113008277885,
124.531460050326)) ;
#111453 = CARTESIAN_POINT('Ctrl Pts',(-20.0431259850148,-36.921204613785,
124.4378711065)) ;
#111454 = CARTESIAN_POINT('Ctrl Pts',(-20.2123607667977,-36.9312514303498,
124.311522422747)) ;
#111455 = CARTESIAN_POINT('Ctrl Pts',(-20.3550791520104,-36.9411469498285,
124.160115650287)) ;
#111456 = CARTESIAN_POINT('Ctrl Pts',(-20.4712290614694,-36.951209035153,
123.983355223544)) ;
#111457 = CARTESIAN_POINT('Ctrl Pts',(-20.5532277916522,-36.9610517461109,
123.793345814573)) ;
#111458 = CARTESIAN_POINT('Ctrl Pts',(-20.6021801450132,-36.9710424634169,
123.589120798251)) ;
#111459 = CARTESIAN_POINT('Ctrl Pts',(-20.6148150633814,-36.9809705465135,
123.380774327372)) ;
#111460 = CARTESIAN_POINT('Ctrl Pts',(-20.5913031319495,-36.9909584766253,
123.1721084492)) ;
#111461 = CARTESIAN_POINT('Ctrl Pts',(-20.5312960773604,-37.0009943027526,
122.969843996497)) ;
#111462 = CARTESIAN_POINT('Ctrl Pts',(-20.4390637669857,-37.0108496398662,
122.784302539848)) ;
#111463 = CARTESIAN_POINT('Ctrl Pts',(-20.3145262149137,-37.0208473747163,
122.61501542878)) ;
#111464 = CARTESIAN_POINT('Ctrl Pts',(-20.1638783038931,-37.0307552787008,
122.471154341589)) ;
#111465 = CARTESIAN_POINT('Ctrl Pts',(-19.9889330421426,-37.0407663532492,
122.354141342379)) ;
#111466 = CARTESIAN_POINT('Ctrl Pts',(-19.7958356533357,-37.0507942087849,
122.269536203962)) ;
#111467 = CARTESIAN_POINT('Ctrl Pts',(-19.5945523380126,-37.0606518026901,
122.220229267546)) ;
#111468 = CARTESIAN_POINT('Ctrl Pts',(-19.3842398152168,-37.0706784895282,
122.205957811028)) ;
#111469 = CARTESIAN_POINT('Ctrl Pts',(-19.1746553930291,-37.0807071586819,
122.228947936959)) ;
#111470 = CARTESIAN_POINT('Ctrl Pts',(-18.9758587583279,-37.0905523669633,
122.286524671456)) ;
#111471 = CARTESIAN_POINT('Ctrl Pts',(-18.7870709003769,-37.1005430559265,
122.378591654802)) ;
#111472 = CARTESIAN_POINT('Ctrl Pts',(-18.6166166019702,-37.1105809322087,
122.502999367113)) ;
#111473 = CARTESIAN_POINT('Ctrl Pts',(-18.4729056470409,-37.120425309851,
122.65193762026)) ;
#111474 = CARTESIAN_POINT('Ctrl Pts',(-18.3552637914304,-37.1304101142424,
122.825752828987)) ;
#111475 = CARTESIAN_POINT('Ctrl Pts',(-18.269871949298,-37.1403496444609,
123.016500152582)) ;
#111476 = CARTESIAN_POINT('Ctrl Pts',(-18.2184419882713,-37.1503893324978,
123.221187462413)) ;
#111477 = CARTESIAN_POINT('Ctrl Pts',(-18.2034572766474,-37.1602776218661,
123.428541305545)) ;
#111478 = CARTESIAN_POINT('Ctrl Pts',(-18.2245235721972,-37.1702667455509,
123.637477475914)) ;
#111479 = CARTESIAN_POINT('Ctrl Pts',(-18.2815401762124,-37.1802267552255,
123.838952255662)) ;
#111480 = CARTESIAN_POINT('Ctrl Pts',(-18.3716856726904,-37.1901271849298,
124.026563193576)) ;
#111481 = CARTESIAN_POINT('Ctrl Pts',(-18.494785105519,-37.2001702663365,
124.198090808399)) ;
#111482 = CARTESIAN_POINT('Ctrl Pts',(-18.6437683697007,-37.2100776602442,
124.34366206687)) ;
#111483 = CARTESIAN_POINT('Ctrl Pts',(-18.817348470021,-37.2200893912333,
124.462707024047)) ;
#111484 = CARTESIAN_POINT('Ctrl Pts',(-19.0095315322514,-37.2301216089481,
124.549604161805)) ;
#111485 = CARTESIAN_POINT('Ctrl Pts',(-19.2101350754558,-37.2399741181943,
124.601142942869)) ;
#111486 = CARTESIAN_POINT('Ctrl Pts',(-19.4188175397486,-37.2499320547373,
124.617888348396)) ;
#111487 = CARTESIAN_POINT('Ctrl Pts',(-19.6288756964164,-37.2599709247456,
124.597608888052)) ;
#111488 = CARTESIAN_POINT('Ctrl Pts',(-19.8290136826369,-37.2698440799038,
124.542458230366)) ;
#111489 = CARTESIAN_POINT('Ctrl Pts',(-20.0202395233851,-37.2799173547535,
124.451563913773)) ;
#111490 = CARTESIAN_POINT('Ctrl Pts',(-20.188674177373,-37.2897376719309,
124.33209908352)) ;
#111491 = CARTESIAN_POINT('Ctrl Pts',(-20.337695270437,-37.2998163577244,
124.181545098102)) ;
#111492 = CARTESIAN_POINT('Ctrl Pts',(-20.4557107130966,-37.3096678691075,
124.011288589486)) ;
#111493 = CARTESIAN_POINT('Ctrl Pts',(-20.5444491455552,-37.3197413154142,
123.819044947763)) ;
#111494 = CARTESIAN_POINT('Ctrl Pts',(-20.5972161790664,-37.3295825905389,
123.618968960944)) ;
#111495 = CARTESIAN_POINT('Ctrl Pts',(-20.6153429771361,-37.3395676901956,
123.409854825953)) ;
#111496 = CARTESIAN_POINT('Ctrl Pts',(-20.5965487503626,-37.3495751663299,
123.200291419129)) ;
#111497 = CARTESIAN_POINT('Ctrl Pts',(-20.5423098994705,-37.3594977540389,
122.998873017778)) ;
#111498 = CARTESIAN_POINT('Ctrl Pts',(-20.4536480500816,-37.3694843583122,
122.808541290812)) ;
#111499 = CARTESIAN_POINT('Ctrl Pts',(-20.3323367844917,-37.3795244866463,
122.635830014515)) ;
#111500 = CARTESIAN_POINT('Ctrl Pts',(-20.1861599955276,-37.3893639211797,
122.489439408705)) ;
#111501 = CARTESIAN_POINT('Ctrl Pts',(-20.0130579706787,-37.3994279756707,
122.367824770233)) ;
#111502 = CARTESIAN_POINT('Ctrl Pts',(-19.8246828907098,-37.4093188949079,
122.279721644593)) ;
#111503 = CARTESIAN_POINT('Ctrl Pts',(-19.6219676186005,-37.4193108882139,
122.224688412414)) ;
#111504 = CARTESIAN_POINT('Ctrl Pts',(-19.4133634522417,-37.4292737521732,
122.205938159795)) ;
#111505 = CARTESIAN_POINT('Ctrl Pts',(-19.2058328347879,-37.439178011991,
122.223065184596)) ;
#111506 = CARTESIAN_POINT('Ctrl Pts',(-19.001340283221,-37.4492385025624,
122.276967108069)) ;
#111507 = CARTESIAN_POINT('Ctrl Pts',(-18.8133529124744,-37.4590788521934,
122.363395881225)) ;
#111508 = CARTESIAN_POINT('Ctrl Pts',(-18.6392806231424,-37.4691418276835,
122.483574640577)) ;
#111509 = CARTESIAN_POINT('Ctrl Pts',(-18.4913282540789,-37.4790361478268,
122.629818827626)) ;
#111510 = CARTESIAN_POINT('Ctrl Pts',(-18.370008887463,-37.4889778609584,
122.799976038917)) ;
#111511 = CARTESIAN_POINT('Ctrl Pts',(-18.2794154013326,-37.4989807507526,
122.989789752726)) ;
#111512 = CARTESIAN_POINT('Ctrl Pts',(-18.2233347975645,-37.509020607913,
123.193251775107)) ;
#111513 = CARTESIAN_POINT('Ctrl Pts',(-18.2033890405656,-37.5188447887507,
123.398837791463)) ;
#111514 = CARTESIAN_POINT('Ctrl Pts',(-18.2195295932789,-37.5289017622539,
123.609632975167)) ;
#111515 = CARTESIAN_POINT('Ctrl Pts',(-18.2716173802949,-37.5388298864409,
123.811761400771)) ;
#111516 = CARTESIAN_POINT('Ctrl Pts',(-18.3577187041589,-37.5487835815143,
124.002486464945)) ;
#111517 = CARTESIAN_POINT('Ctrl Pts',(-18.4769711218395,-37.5588297750896,
124.176798371199)) ;
#111518 = CARTESIAN_POINT('Ctrl Pts',(-18.6216236556792,-37.5686778774495,
124.32491921087)) ;
#111519 = CARTESIAN_POINT('Ctrl Pts',(-18.7913505096594,-37.5786394656771,
124.447586794052)) ;
#111520 = CARTESIAN_POINT('Ctrl Pts',(-18.9812024966382,-37.5886681358334,
124.539307190478)) ;
#111521 = CARTESIAN_POINT('Ctrl Pts',(-19.1816617431546,-37.5985784387151,
124.596051335293)) ;
#111522 = CARTESIAN_POINT('Ctrl Pts',(-19.3894026350066,-37.608513322523,
124.617725946101)) ;
#111523 = CARTESIAN_POINT('Ctrl Pts',(-19.5999531467853,-37.6185544642137,
124.602647818621)) ;
#111524 = CARTESIAN_POINT('Ctrl Pts',(-19.8015999748702,-37.6284415853776,
124.552166449768)) ;
#111525 = CARTESIAN_POINT('Ctrl Pts',(-19.9935578049216,-37.6384339282262,
124.466868050426)) ;
#111526 = CARTESIAN_POINT('Ctrl Pts',(-20.167008404191,-37.6483822294501,
124.349989406633)) ;
#111527 = CARTESIAN_POINT('Ctrl Pts',(-20.3175626051093,-37.6583198071322,
124.205160860977)) ;
#111528 = CARTESIAN_POINT('Ctrl Pts',(-20.4414789151916,-37.6683063815828,
124.035663158613)) ;
#111529 = CARTESIAN_POINT('Ctrl Pts',(-20.5342491047195,-37.6783351914913,
123.846334475287)) ;
#111530 = CARTESIAN_POINT('Ctrl Pts',(-20.5920528123341,-37.6882135127981,
123.646870336206)) ;
#111531 = CARTESIAN_POINT('Ctrl Pts',(-20.6150924684944,-37.6982051601455,
123.43807466397)) ;
#111532 = CARTESIAN_POINT('Ctrl Pts',(-20.6010405408264,-37.7082396835832,
123.227595402001)) ;
#111533 = CARTESIAN_POINT('Ctrl Pts',(-20.5519273803559,-37.7181030404618,
123.026114699529)) ;
#111534 = CARTESIAN_POINT('Ctrl Pts',(-20.4668842211972,-37.7281732671421,
122.832263260374)) ;
#111535 = CARTESIAN_POINT('Ctrl Pts',(-20.3521054942186,-37.7380155752768,
122.660089856857)) ;
#111536 = CARTESIAN_POINT('Ctrl Pts',(-20.2080246387661,-37.7479763073002,
122.508137744132)) ;
#111537 = CARTESIAN_POINT('Ctrl Pts',(-20.0381983196995,-37.7580141964983,
122.382882450839)) ;
#111538 = CARTESIAN_POINT('Ctrl Pts',(-19.8524261195439,-37.7678884794172,
122.290188729038)) ;
#111539 = CARTESIAN_POINT('Ctrl Pts',(-19.6494889728013,-37.7779582240346,
122.230017437484)) ;
#111540 = CARTESIAN_POINT('Ctrl Pts',(-19.4440940258962,-37.7877915343803,
122.206445815944)) ;
#111541 = CARTESIAN_POINT('Ctrl Pts',(-19.233578340546,-37.7978217777329,
122.218543083299)) ;
#111542 = CARTESIAN_POINT('Ctrl Pts',(-19.0284557077842,-37.8078540657113,
122.267635236295)) ;
#111543 = CARTESIAN_POINT('Ctrl Pts',(-18.8387371145789,-37.8176812421794,
122.349429635045)) ;
#111544 = CARTESIAN_POINT('Ctrl Pts',(-18.6627557536767,-37.8276866250463,
122.464601992116)) ;
#111545 = CARTESIAN_POINT('Ctrl Pts',(-18.5097931762662,-37.837669264039,
122.608349404732)) ;
#111546 = CARTESIAN_POINT('Ctrl Pts',(-18.3835843507206,-37.8477133311756,
122.777612770899)) ;
#111547 = CARTESIAN_POINT('Ctrl Pts',(-18.2904551442728,-37.8575345499796,
122.961897225357)) ;
#111548 = CARTESIAN_POINT('Ctrl Pts',(-18.2289137583434,-37.8675713889177,
123.163725874887)) ;
#111549 = CARTESIAN_POINT('Ctrl Pts',(-18.2039782976807,-37.8775958010154,
123.372997461474)) ;
#111550 = CARTESIAN_POINT('Ctrl Pts',(-18.215097319495,-37.8874478854207,
123.579823715194)) ;
#111551 = CARTESIAN_POINT('Ctrl Pts',(-18.2623014355616,-37.8974387821639,
123.784464914976)) ;
#111552 = CARTESIAN_POINT('Ctrl Pts',(-18.3436167608932,-37.9073567740648,
123.976489726983)) ;
#111553 = CARTESIAN_POINT('Ctrl Pts',(-18.4582331962466,-37.9173848895218,
124.153414280329)) ;
#111554 = CARTESIAN_POINT('Ctrl Pts',(-18.5997314801908,-37.927270065464,
124.305625819282)) ;
#111555 = CARTESIAN_POINT('Ctrl Pts',(-18.7669477783445,-37.9372594238708,
124.432684036662)) ;
#111556 = CARTESIAN_POINT('Ctrl Pts',(-18.9548533599214,-37.9473005714511,
124.528877089993)) ;
#111557 = CARTESIAN_POINT('Ctrl Pts',(-19.1523136142343,-37.9571331944576,
124.590019608605)) ;
#111558 = CARTESIAN_POINT('Ctrl Pts',(-19.3606809866643,-37.9671272655683,
124.616962197826)) ;
#111559 = CARTESIAN_POINT('Ctrl Pts',(-19.5712845702679,-37.9771559232092,
124.606866062767)) ;
#111560 = CARTESIAN_POINT('Ctrl Pts',(-19.7740057109294,-37.987040249402,
124.56125238552)) ;
#111561 = CARTESIAN_POINT('Ctrl Pts',(-19.9675216950022,-37.9970059928926,
124.48094271042)) ;
#111562 = CARTESIAN_POINT('Ctrl Pts',(-20.1450861017954,-38.0070343720238,
124.367295867457)) ;
#111563 = CARTESIAN_POINT('Ctrl Pts',(-20.2984877679681,-38.0169352182307,
124.226568085961)) ;
#111564 = CARTESIAN_POINT('Ctrl Pts',(-20.4270610609682,-38.0269938756478,
124.058721673059)) ;
#111565 = CARTESIAN_POINT('Ctrl Pts',(-20.5228145375505,-38.0368514384297,
123.874891009865)) ;
#111566 = CARTESIAN_POINT('Ctrl Pts',(-20.5866403096007,-38.0469198409829,
123.673106507591)) ;
#111567 = CARTESIAN_POINT('Ctrl Pts',(-20.6138575148914,-38.0567752397225,
123.467692694179)) ;
#111568 = CARTESIAN_POINT('Ctrl Pts',(-20.6055012210604,-38.0667701067964,
123.257742296648)) ;
#111569 = CARTESIAN_POINT('Ctrl Pts',(-20.5602077541318,-38.0768014017799,
123.051769928458)) ;
#111570 = CARTESIAN_POINT('Ctrl Pts',(-20.4814641956645,-38.0866679265065,
122.859864478831)) ;
#111571 = CARTESIAN_POINT('Ctrl Pts',(-20.3695390587959,-38.0966553972022,
122.682244929332)) ;
#111572 = CARTESIAN_POINT('Ctrl Pts',(-20.2291244692025,-38.106600156766,
122.527301387467)) ;
#111573 = CARTESIAN_POINT('Ctrl Pts',(-20.0622287341448,-38.1166457127149,
122.397930524766)) ;
#111574 = CARTESIAN_POINT('Ctrl Pts',(-19.8789244007381,-38.12650530109,122.301108914779)) ;
#111575 = CARTESIAN_POINT('Ctrl Pts',(-19.6789175845978,-38.136506256226,
122.236391579469)) ;
#111576 = CARTESIAN_POINT('Ctrl Pts',(-19.4726820864949,-38.1464104835036,
122.207495519726)) ;
#111577 = CARTESIAN_POINT('Ctrl Pts',(-19.2617238715247,-38.1564525603987,
122.214889176616)) ;
#111578 = CARTESIAN_POINT('Ctrl Pts',(-19.0579327738821,-38.1663601730849,
122.258125131166)) ;
#111579 = CARTESIAN_POINT('Ctrl Pts',(-18.8619377657771,-38.1764147037006,
122.337205363752)) ;
#111580 = CARTESIAN_POINT('Ctrl Pts',(-18.6859931771413,-38.1862754902495,
122.446886140875)) ;
#111581 = CARTESIAN_POINT('Ctrl Pts',(-18.5294712055464,-38.1962692453206,
122.586988973454)) ;
#111582 = CARTESIAN_POINT('Ctrl Pts',(-18.4004207000116,-38.2061946055606,
122.750999792233)) ;
#111583 = CARTESIAN_POINT('Ctrl Pts',(-18.3008112005479,-38.2162225349558,
122.936770457195)) ;
#111584 = CARTESIAN_POINT('Ctrl Pts',(-18.2356782692147,-38.2261088017551,
123.134174548358)) ;
#111585 = CARTESIAN_POINT('Ctrl Pts',(-18.2052725837904,-38.2361405706534,
123.34283512174)) ;
#111586 = CARTESIAN_POINT('Ctrl Pts',(-18.2112643073026,-38.246022166497,
123.550528336752)) ;
#111587 = CARTESIAN_POINT('Ctrl Pts',(-18.2539267545677,-38.256084051965,
123.757681737281)) ;
#111588 = CARTESIAN_POINT('Ctrl Pts',(-18.3302825444125,-38.2659414859838,
123.950365039774)) ;
#111589 = CARTESIAN_POINT('Ctrl Pts',(-18.4400259469316,-38.2759347290258,
124.129482006284)) ;
#111590 = CARTESIAN_POINT('Ctrl Pts',(-18.5783449699185,-38.2858654899121,
124.285877034331)) ;
#111591 = CARTESIAN_POINT('Ctrl Pts',(-18.797800066847,-38.2992144821093,
124.460861868792)) ;
#111592 = CARTESIAN_POINT('Ctrl Pts',(-19.0564633169718,-38.3124828549258,
124.573503677827)) ;
#111593 = CARTESIAN_POINT('Ctrl Pts',(-19.3325238155901,-38.3257657963101,
124.6154494148)) ;
#111594 = CARTESIAN_POINT('Ctrl Pts',(-19.5435860924634,-38.3358085821523,
124.61029115832)) ;
#111595 = CARTESIAN_POINT('Ctrl Pts',(-19.7466277481613,-38.3456585247044,
124.569582978898)) ;
#111596 = CARTESIAN_POINT('Ctrl Pts',(-19.942581001548,-38.3556557576234,
124.493607027395)) ;
#111597 = CARTESIAN_POINT('Ctrl Pts',(-20.1225268951548,-38.3656706529579,
124.384284337573)) ;
#111598 = CARTESIAN_POINT('Ctrl Pts',(-20.3318936737294,-38.3789103295961,
124.200838329891)) ;
#111599 = CARTESIAN_POINT('Ctrl Pts',(-20.5281689110061,-38.3954575540015,
123.90891594944)) ;
#111600 = CARTESIAN_POINT('Ctrl Pts',(-20.6137584736085,-38.4121049911325,
123.565384315522)) ;
#111601 = CARTESIAN_POINT('Ctrl Pts',(-20.6085739408093,-38.4253944886108,
123.286078404833)) ;
#111602 = CARTESIAN_POINT('Ctrl Pts',(-20.5693616431059,-38.4352678964331,
123.082234242801)) ;
#111603 = CARTESIAN_POINT('Ctrl Pts',(-20.4940484563953,-38.4453202740258,
122.884789812796)) ;
#111604 = CARTESIAN_POINT('Ctrl Pts',(-20.3871103204177,-38.4552239275667,
122.706124714209)) ;
#111605 = CARTESIAN_POINT('Ctrl Pts',(-20.2506291861779,-38.465168196562,
122.547800904937)) ;
#111606 = CARTESIAN_POINT('Ctrl Pts',(-20.033584489698,-38.4784992048947,
122.370371715302)) ;
#111607 = CARTESIAN_POINT('Ctrl Pts',(-19.7113358816903,-38.495120785419,
122.225466397032)) ;
#111608 = CARTESIAN_POINT('Ctrl Pts',(-19.3605438529147,-38.5116634561174,
122.198641645534)) ;
#111609 = CARTESIAN_POINT('Ctrl Pts',(-19.0847618328719,-38.5250126156803,
122.250343354559)) ;
#111610 = CARTESIAN_POINT('Ctrl Pts',(-18.8243063208859,-38.5382407658398,
122.3479663699)) ;
#111611 = CARTESIAN_POINT('Ctrl Pts',(-18.536415594409,-38.5548714429773,
122.553181981053)) ;
#111612 = CARTESIAN_POINT('Ctrl Pts',(-18.2963062234918,-38.5747743822654,
122.901730686515)) ;
#111613 = CARTESIAN_POINT('Ctrl Pts',(-18.1891638869259,-38.5946772488687,
123.311048037197)) ;
#111614 = CARTESIAN_POINT('Ctrl Pts',(-18.2275213426716,-38.6145904139735,
123.732809891453)) ;
#111615 = CARTESIAN_POINT('Ctrl Pts',(-18.4091462603593,-38.6346262431149,
124.118102875856)) ;
#111616 = CARTESIAN_POINT('Ctrl Pts',(-18.7080073643682,-38.6544448179929,
124.415329627801)) ;
#111617 = CARTESIAN_POINT('Ctrl Pts',(-19.0927775776593,-38.6744151190349,
124.594594867999)) ;
#111618 = CARTESIAN_POINT('Ctrl Pts',(-19.5142396463623,-38.6943066513995,
124.631812025782)) ;
#111619 = CARTESIAN_POINT('Ctrl Pts',(-19.9254823846201,-38.714329749216,
124.522010261592)) ;
#111620 = CARTESIAN_POINT('Ctrl Pts',(-20.2709167165201,-38.7341265021359,
124.281378827604)) ;
#111621 = CARTESIAN_POINT('Ctrl Pts',(-20.5163914718187,-38.7540875906247,
123.935187258332)) ;
#111622 = CARTESIAN_POINT('Ctrl Pts',(-20.6282549540396,-38.7740658595569,
123.525352612121)) ;
#111623 = CARTESIAN_POINT('Ctrl Pts',(-20.5944404953484,-38.7938858743479,
123.105322954346)) ;
#111624 = CARTESIAN_POINT('Ctrl Pts',(-20.4192472238477,-38.8138242835997,
122.719246962933)) ;
#111625 = CARTESIAN_POINT('Ctrl Pts',(-20.1204989908082,-38.8338714009922,
122.415126542636)) ;
#111626 = CARTESIAN_POINT('Ctrl Pts',(-19.7397606456982,-38.853717646826,
122.233270693111)) ;
#111627 = CARTESIAN_POINT('Ctrl Pts',(-19.319859218339,-38.873566615338,122.190591115551)) ;
#111628 = CARTESIAN_POINT('Ctrl Pts',(-18.9066441971448,-38.8936169176493,
122.295321844005)) ;
#111629 = CARTESIAN_POINT('Ctrl Pts',(-18.5576899317708,-38.9134518400806,
122.532358389631)) ;
#111630 = CARTESIAN_POINT('Ctrl Pts',(-18.3088685698943,-38.9333822413064,
122.875190550138)) ;
#111631 = CARTESIAN_POINT('Ctrl Pts',(-18.1916327898511,-38.9532671866653,
123.281589103572)) ;
#111632 = CARTESIAN_POINT('Ctrl Pts',(-18.2210632664517,-38.9733397948167,
123.70728965681)) ;
#111633 = CARTESIAN_POINT('Ctrl Pts',(-18.3915669690608,-38.9931311111448,
124.092087452181)) ;
#111634 = CARTESIAN_POINT('Ctrl Pts',(-18.6846875143043,-39.0130959009121,
124.399097364144)) ;
#111635 = CARTESIAN_POINT('Ctrl Pts',(-19.0658343612412,-39.0330788566624,
124.586888443645)) ;
#111636 = CARTESIAN_POINT('Ctrl Pts',(-19.4844338519567,-39.0528873786385,
124.633801864858)) ;
#111637 = CARTESIAN_POINT('Ctrl Pts',(-19.8975626919081,-39.0728729533743,
124.534669398346)) ;
#111638 = CARTESIAN_POINT('Ctrl Pts',(-20.2503490912173,-39.0927555934427,
124.301535626291)) ;
#111639 = CARTESIAN_POINT('Ctrl Pts',(-20.5034831073176,-39.1127109055746,
123.961116997629)) ;
#111640 = CARTESIAN_POINT('Ctrl Pts',(-20.6250651046642,-39.1325852621824,
123.556327194031)) ;
#111641 = CARTESIAN_POINT('Ctrl Pts',(-20.6013679066506,-39.1525674690435,
123.132160553473)) ;
#111642 = CARTESIAN_POINT('Ctrl Pts',(-20.4345120841467,-39.1724985469935,
122.742504595562)) ;
#111643 = CARTESIAN_POINT('Ctrl Pts',(-20.1449274430582,-39.1924255218484,
122.433328925818)) ;
#111644 = CARTESIAN_POINT('Ctrl Pts',(-19.7692548084333,-39.2122579807973,
122.2416366517)) ;
#111645 = CARTESIAN_POINT('Ctrl Pts',(-19.4179185607593,-39.2289156649725,
122.197708876693)) ;
#111646 = CARTESIAN_POINT('Ctrl Pts',(-19.1419055899965,-39.2421648888796,
122.235828477247)) ;
#111647 = CARTESIAN_POINT('Ctrl Pts',(-18.9408305539058,-39.2522139103308,
122.300533219516)) ;
#111648 = CARTESIAN_POINT('Ctrl Pts',(-18.7574950088905,-39.2620739185613,
122.397289650164)) ;
#111649 = CARTESIAN_POINT('Ctrl Pts',(-18.5363510917662,-39.2753574317859,
122.567786744329)) ;
#111650 = CARTESIAN_POINT('Ctrl Pts',(-18.3218449965654,-39.2920033507868,
122.849347672533)) ;
#111651 = CARTESIAN_POINT('Ctrl Pts',(-18.2164382230536,-39.3085573286028,
123.185154868491)) ;
#111652 = CARTESIAN_POINT('Ctrl Pts',(-18.2044962088326,-39.3219170575744,
123.465792895425)) ;
#111653 = CARTESIAN_POINT('Ctrl Pts',(-18.2317168356426,-39.3318101093711,
123.671995379416)) ;
#111654 = CARTESIAN_POINT('Ctrl Pts',(-18.2946583082233,-39.3418000746522,
123.872338908844)) ;
#111655 = CARTESIAN_POINT('Ctrl Pts',(-18.3909769779386,-39.351751955513,
124.058105426171)) ;
#111656 = CARTESIAN_POINT('Ctrl Pts',(-18.5194282052934,-39.3618003072048,
124.225785268847)) ;
#111657 = CARTESIAN_POINT('Ctrl Pts',(-18.6717018757687,-39.371641591311,
124.36588111631)) ;
#111658 = CARTESIAN_POINT('Ctrl Pts',(-18.848276134984,-39.3816282944367,
124.479397208524)) ;
#111659 = CARTESIAN_POINT('Ctrl Pts',(-19.0408979361627,-39.3915633232541,
124.560259162815)) ;
#111660 = CARTESIAN_POINT('Ctrl Pts',(-19.2470780633845,-39.401619118161,
124.606820792536)) ;
#111661 = CARTESIAN_POINT('Ctrl Pts',(-19.4534807990528,-39.4114474814503,
124.616970804252)) ;
#111662 = CARTESIAN_POINT('Ctrl Pts',(-19.6633426444756,-39.4215084513482,
124.590821801667)) ;
#111663 = CARTESIAN_POINT('Ctrl Pts',(-19.8625270331918,-39.431422730238,
124.529358162085)) ;
#111664 = CARTESIAN_POINT('Ctrl Pts',(-20.0499564697624,-39.4414317247063,
124.433712278389)) ;
#111665 = CARTESIAN_POINT('Ctrl Pts',(-20.2180166461141,-39.45146155927,124.306370899416)) ;
#111666 = CARTESIAN_POINT('Ctrl Pts',(-20.3592599691175,-39.4613197893422,
124.154683595042)) ;
#111667 = CARTESIAN_POINT('Ctrl Pts',(-20.473812887028,-39.4713184950847,
123.978476443416)) ;
#111668 = CARTESIAN_POINT('Ctrl Pts',(-20.5554308726724,-39.4812131510035,
123.787099057776)) ;
#111669 = CARTESIAN_POINT('Ctrl Pts',(-20.6033009369879,-39.4912762153874,
123.581065747596)) ;
#111670 = CARTESIAN_POINT('Ctrl Pts',(-20.6146498642187,-39.5011158736673,
123.374482650769)) ;
#111671 = CARTESIAN_POINT('Ctrl Pts',(-20.5896704825479,-39.5111790407491,
123.164432243332)) ;
#111672 = CARTESIAN_POINT('Ctrl Pts',(-20.529440651171,-39.5210732858762,
122.965310854951)) ;
#111673 = CARTESIAN_POINT('Ctrl Pts',(-20.4356297147218,-39.5310151074809,
122.778567317446)) ;
#111674 = CARTESIAN_POINT('Ctrl Pts',(-20.3100866446553,-39.5410176383989,
122.609835558872)) ;
#111675 = CARTESIAN_POINT('Ctrl Pts',(-20.1564664242704,-39.5510522648564,
122.465266912577)) ;
#111676 = CARTESIAN_POINT('Ctrl Pts',(-19.9835680040262,-39.5608977998429,
122.351462347985)) ;
#111677 = CARTESIAN_POINT('Ctrl Pts',(-19.7910775109186,-39.5708812246819,
122.267849931277)) ;
#111678 = CARTESIAN_POINT('Ctrl Pts',(-19.5876362908515,-39.580831615047,
122.21912775665)) ;
#111679 = CARTESIAN_POINT('Ctrl Pts',(-19.3778391821031,-39.590829255344,
122.206125638961)) ;
#111680 = CARTESIAN_POINT('Ctrl Pts',(-19.1681833516847,-39.6008683359072,
122.230265157014)) ;
#111681 = CARTESIAN_POINT('Ctrl Pts',(-18.9700405352401,-39.6106944866763,
122.28872794687)) ;
#111682 = CARTESIAN_POINT('Ctrl Pts',(-18.7805917723038,-39.6207510616055,
122.382551514656)) ;
#111683 = CARTESIAN_POINT('Ctrl Pts',(-18.6124777620064,-39.6306916009857,
122.506703809047)) ;
#111684 = CARTESIAN_POINT('Ctrl Pts',(-18.4685284561753,-39.6405959939621,
122.657157910547)) ;
#111685 = CARTESIAN_POINT('Ctrl Pts',(-18.3513522549235,-39.650642648167,
122.832864711716)) ;
#111686 = CARTESIAN_POINT('Ctrl Pts',(-18.2675466298892,-39.6605382101054,
123.023310137376)) ;
#111687 = CARTESIAN_POINT('Ctrl Pts',(-18.2172646578921,-39.670600287951,
123.228752857409)) ;
#111688 = CARTESIAN_POINT('Ctrl Pts',(-18.2035979933994,-39.6804429863648,
123.435248767042)) ;
#111689 = CARTESIAN_POINT('Ctrl Pts',(-18.2258312979083,-39.6904337613262,
123.644079105315)) ;
#111690 = CARTESIAN_POINT('Ctrl Pts',(-18.2836612226647,-39.7003616263453,
123.84463437606)) ;
#111691 = CARTESIAN_POINT('Ctrl Pts',(-18.3756796903981,-39.7103503711115,
124.033399249309)) ;
#111692 = CARTESIAN_POINT('Ctrl Pts',(-18.4998707481865,-39.7203831566985,
124.203885569467)) ;
#111693 = CARTESIAN_POINT('Ctrl Pts',(-18.6491083855865,-39.7302498413191,
124.347939938678)) ;
#111694 = CARTESIAN_POINT('Ctrl Pts',(-18.8224225034986,-39.7402117334822,
124.465518459762)) ;
#111695 = CARTESIAN_POINT('Ctrl Pts',(-19.0150180665771,-39.7502452103948,
124.551524096966)) ;
#111696 = CARTESIAN_POINT('Ctrl Pts',(-19.2165333116674,-39.7601295516431,
124.602348214556)) ;
#111697 = CARTESIAN_POINT('Ctrl Pts',(-19.4275051954898,-39.7701924937642,
124.617681843137)) ;
#111698 = CARTESIAN_POINT('Ctrl Pts',(-19.6335421669846,-39.7800428953838,
124.596701425017)) ;
#111699 = CARTESIAN_POINT('Ctrl Pts',(-19.8365009125244,-39.7900697841735,
124.539772940591)) ;
#111700 = CARTESIAN_POINT('Ctrl Pts',(-20.0262992465954,-39.8000983991297,
124.447948659546)) ;
#111701 = CARTESIAN_POINT('Ctrl Pts',(-20.1943553064354,-39.8099436222498,
124.327151312276)) ;
#111702 = CARTESIAN_POINT('Ctrl Pts',(-20.3414348815078,-39.8199343060557,
124.177201650013)) ;
#111703 = CARTESIAN_POINT('Ctrl Pts',(-20.4604129636766,-39.8299721881281,
124.002914155658)) ;
#111704 = CARTESIAN_POINT('Ctrl Pts',(-20.5459796222407,-39.839816547767,
123.814463221015)) ;
#111705 = CARTESIAN_POINT('Ctrl Pts',(-20.5986526054623,-39.8498014183817,
123.611295435785)) ;
#111706 = CARTESIAN_POINT('Ctrl Pts',(-20.6152731234148,-39.8597407017104,
123.402971706879)) ;
#111707 = CARTESIAN_POINT('Ctrl Pts',(-20.5952065572316,-39.8697813110835,
123.192864149865)) ;
#111708 = CARTESIAN_POINT('Ctrl Pts',(-20.5399724573556,-39.8796661619968,
122.99250342132)) ;
#111709 = CARTESIAN_POINT('Ctrl Pts',(-20.4499839938859,-39.8896681181656,
122.802494569433)) ;
#111710 = CARTESIAN_POINT('Ctrl Pts',(-20.32948348358,-39.899586714886,122.632277048077)) ;
#111711 = CARTESIAN_POINT('Ctrl Pts',(-20.1793573936441,-39.9096335369618,
122.483744858883)) ;
#111712 = CARTESIAN_POINT('Ctrl Pts',(-20.0087618982145,-39.9195078180745,
122.365403102179)) ;
#111713 = CARTESIAN_POINT('Ctrl Pts',(-19.8168931041751,-39.9295620181191,
122.276810365965)) ;
#111714 = CARTESIAN_POINT('Ctrl Pts',(-19.6157324287139,-39.9394574477544,
122.223627808536)) ;
#111715 = CARTESIAN_POINT('Ctrl Pts',(-19.4049800665042,-39.9495190760717,
122.205843629942)) ;
#111716 = CARTESIAN_POINT('Ctrl Pts',(-19.1988492983228,-39.9593637049016,
122.224487872626)) ;
#111717 = CARTESIAN_POINT('Ctrl Pts',(-18.9965589739824,-39.9693237525072,
122.278544623241)) ;
#111718 = CARTESIAN_POINT('Ctrl Pts',(-18.8054174859207,-39.9793620586813,
122.36797184238)) ;
#111719 = CARTESIAN_POINT('Ctrl Pts',(-18.635282468693,-39.989235358114,122.48693228137)) ;
#111720 = CARTESIAN_POINT('Ctrl Pts',(-18.4855140169504,-39.9993086197002,
122.636593440334)) ;
#111721 = CARTESIAN_POINT('Ctrl Pts',(-18.3667834467825,-40.0091288456569,
122.805545144584)) ;
#111722 = CARTESIAN_POINT('Ctrl Pts',(-18.2767571585724,-40.0192079095964,
122.997303658689)) ;
#111723 = CARTESIAN_POINT('Ctrl Pts',(-18.2225286239996,-40.0290579996162,
123.197214767681)) ;
#111724 = CARTESIAN_POINT('Ctrl Pts',(-18.2033013065767,-40.03913675323,123.408174394108)) ;
#111725 = CARTESIAN_POINT('Ctrl Pts',(-18.2203931909953,-40.0489582204895,
123.613989771213)) ;
#111726 = CARTESIAN_POINT('Ctrl Pts',(-18.2739295174187,-40.0590238188471,
123.818666721539)) ;
#111727 = CARTESIAN_POINT('Ctrl Pts',(-18.3608545685295,-40.0689264746218,
124.007892465016)) ;
#111728 = CARTESIAN_POINT('Ctrl Pts',(-18.4809798438393,-40.0789773004515,
124.181672724413)) ;
#111729 = CARTESIAN_POINT('Ctrl Pts',(-18.6267630396012,-40.0888515047903,
124.329518251049)) ;
#111730 = CARTESIAN_POINT('Ctrl Pts',(-18.7993190041685,-40.0989239548294,
124.452178855583)) ;
#111731 = CARTESIAN_POINT('Ctrl Pts',(-18.985919405343,-40.1087529716029,
124.541034166242)) ;
#111732 = CARTESIAN_POINT('Ctrl Pts',(-19.1897830594759,-40.1188198175177,
124.59773351556)) ;
#111733 = CARTESIAN_POINT('Ctrl Pts',(-19.3967718988251,-40.1287099888195,
124.617687610302)) ;
#111734 = CARTESIAN_POINT('Ctrl Pts',(-19.6062173951724,-40.1387021824434,
124.601693994836)) ;
#111735 = CARTESIAN_POINT('Ctrl Pts',(-19.8090634628098,-40.1486649930668,
124.549535314913)) ;
#111736 = CARTESIAN_POINT('Ctrl Pts',(-19.9988895705213,-40.1585692659102,
124.463929433814)) ;
#111737 = CARTESIAN_POINT('Ctrl Pts',(-20.1735429731809,-40.1686297577149,
124.344686583238)) ;
#111738 = CARTESIAN_POINT('Ctrl Pts',(-20.3217552818586,-40.1784700893872,
124.200318672514)) ;
#111739 = CARTESIAN_POINT('Ctrl Pts',(-20.4455592635018,-40.1885331354789,
124.028803475415)) ;
#111740 = CARTESIAN_POINT('Ctrl Pts',(-20.5360204871642,-40.198427191174,
123.841477197477)) ;
#111741 = CARTESIAN_POINT('Ctrl Pts',(-20.5933980982579,-40.208369891497,
123.640504103453)) ;
#111742 = CARTESIAN_POINT('Ctrl Pts',(-20.6151916585932,-40.2183756324246,
123.431261797586)) ;
#111743 = CARTESIAN_POINT('Ctrl Pts',(-20.6000648932316,-40.2283965429401,
123.221139380091)) ;
#111744 = CARTESIAN_POINT('Ctrl Pts',(-20.5495814837081,-40.2382872783901,
123.019420132795)) ;
#111745 = CARTESIAN_POINT('Ctrl Pts',(-20.4642659333143,-40.2482788191189,
122.827481925444)) ;
#111746 = CARTESIAN_POINT('Ctrl Pts',(-20.3473793834705,-40.2582266795406,
122.654062315484)) ;
#111747 = CARTESIAN_POINT('Ctrl Pts',(-20.2024624018767,-40.2681733487269,
122.503294288896)) ;
#111748 = CARTESIAN_POINT('Ctrl Pts',(-20.0317256366531,-40.2782214248625,
122.37891954227)) ;
#111749 = CARTESIAN_POINT('Ctrl Pts',(-19.8458410995588,-40.2880690228682,
122.287772713109)) ;
#111750 = CARTESIAN_POINT('Ctrl Pts',(-19.6448433223198,-40.2980307459526,
122.228991805251)) ;
#111751 = CARTESIAN_POINT('Ctrl Pts',(-19.435241806661,-40.3080593810356,
122.206112664313)) ;
#111752 = CARTESIAN_POINT('Ctrl Pts',(-19.2273522393713,-40.3179696893537,
122.219741722418)) ;
#111753 = CARTESIAN_POINT('Ctrl Pts',(-19.0243399510485,-40.3279045864895,
122.268855297259)) ;
#111754 = CARTESIAN_POINT('Ctrl Pts',(-18.830982862391,-40.3379456694321,
122.353540418053)) ;
#111755 = CARTESIAN_POINT('Ctrl Pts',(-18.6578647257515,-40.3478330122603,
122.46861160416)) ;
#111756 = CARTESIAN_POINT('Ctrl Pts',(-18.5055374059641,-40.3578245271997,
122.613227801925)) ;
#111757 = CARTESIAN_POINT('Ctrl Pts',(-18.381196813808,-40.3677759183962,
122.781483374974)) ;
#111758 = CARTESIAN_POINT('Ctrl Pts',(-18.2878153511664,-40.3777084517288,
122.968251293523)) ;
#111759 = CARTESIAN_POINT('Ctrl Pts',(-18.227816296101,-40.3877056096282,
123.169668494202)) ;
#111760 = CARTESIAN_POINT('Ctrl Pts',(-18.2036472741279,-40.3976906197917,
123.378221787086)) ;
#111761 = CARTESIAN_POINT('Ctrl Pts',(-18.2164348161517,-40.4077334463615,
123.588937413733)) ;
#111762 = CARTESIAN_POINT('Ctrl Pts',(-18.2641263224755,-40.4175636806665,
123.790054933994)) ;
#111763 = CARTESIAN_POINT('Ctrl Pts',(-18.3479442111075,-40.4276397059012,
123.984549393256)) ;
#111764 = CARTESIAN_POINT('Ctrl Pts',(-18.4616333982887,-40.437491942392,
124.157737013279)) ;
#111765 = CARTESIAN_POINT('Ctrl Pts',(-18.6066677528805,-40.4475651488262,
124.312000963464)) ;
#111766 = CARTESIAN_POINT('Ctrl Pts',(-18.7724548511225,-40.4574066583333,
124.435805622703)) ;
#111767 = CARTESIAN_POINT('Ctrl Pts',(-18.9590880314163,-40.4673676051131,
124.530768111123)) ;
#111768 = CARTESIAN_POINT('Ctrl Pts',(-19.1610443709841,-40.4774054339132,
124.591950432081)) ;
#111769 = CARTESIAN_POINT('Ctrl Pts',(-19.3671277733051,-40.4872797436676,
124.617113251877)) ;
#111770 = CARTESIAN_POINT('Ctrl Pts',(-19.5784987422063,-40.4973494413408,
124.605884467991)) ;
#111771 = CARTESIAN_POINT('Ctrl Pts',(-19.779937812333,-40.5071829126282,
124.559341827718)) ;
#111772 = CARTESIAN_POINT('Ctrl Pts',(-19.9742509754254,-40.5172125591581,
124.47748463539)) ;
#111773 = CARTESIAN_POINT('Ctrl Pts',(-20.1511426049087,-40.5272470734855,
124.362531504326)) ;
#111774 = CARTESIAN_POINT('Ctrl Pts',(-20.3025078038996,-40.5370723589564,
124.221977782079)) ;
#111775 = CARTESIAN_POINT('Ctrl Pts',(-20.429779946649,-40.5470766005049,
124.054566875836)) ;
#111776 = CARTESIAN_POINT('Ctrl Pts',(-20.5257938258127,-40.557059245584,
123.867906072683)) ;
#111777 = CARTESIAN_POINT('Ctrl Pts',(-20.5880805609529,-40.5671044426755,
123.66614246652)) ;
#111778 = CARTESIAN_POINT('Ctrl Pts',(-20.6141561792752,-40.5769275584357,
123.461275158254)) ;
#111779 = CARTESIAN_POINT('Ctrl Pts',(-20.6045831812981,-40.5869621702359,
123.250536092246)) ;
#111780 = CARTESIAN_POINT('Ctrl Pts',(-20.5580318886837,-40.5969871790091,
123.044977475681)) ;
#111781 = CARTESIAN_POINT('Ctrl Pts',(-20.4783225281622,-40.6068391038507,
122.85380756401)) ;
#111782 = CARTESIAN_POINT('Ctrl Pts',(-20.3653416615926,-40.6168300421734,
122.676771223956)) ;
#111783 = CARTESIAN_POINT('Ctrl Pts',(-20.2244402055431,-40.6267480273198,
122.523042790523)) ;
#111784 = CARTESIAN_POINT('Ctrl Pts',(-20.0572136325295,-40.6367761282153,
122.394689913089)) ;
#111785 = CARTESIAN_POINT('Ctrl Pts',(-19.8729266980651,-40.6466613691579,
122.298623695754)) ;
#111786 = CARTESIAN_POINT('Ctrl Pts',(-19.6728303942634,-40.6566504821245,
122.234864816463)) ;
#111787 = CARTESIAN_POINT('Ctrl Pts',(-19.4635495514283,-40.6666925464653,
122.207129365987)) ;
#111788 = CARTESIAN_POINT('Ctrl Pts',(-19.2570735123544,-40.6765217478698,
122.215570738154)) ;
#111789 = CARTESIAN_POINT('Ctrl Pts',(-19.0514845795026,-40.686528588628,
122.260076794459)) ;
#111790 = CARTESIAN_POINT('Ctrl Pts',(-18.8571148525317,-40.6965161128199,
122.339588736615)) ;
#111791 = CARTESIAN_POINT('Ctrl Pts',(-18.6788780360965,-40.7065457586286,
122.452209534781)) ;
#111792 = CARTESIAN_POINT('Ctrl Pts',(-18.5251259193675,-40.7164197893673,
122.591708322353)) ;
#111793 = CARTESIAN_POINT('Ctrl Pts',(-18.3961453373296,-40.7264191122314,
122.75766355134)) ;
#111794 = CARTESIAN_POINT('Ctrl Pts',(-18.2985943342903,-40.736329947807,
122.941814172693)) ;
#111795 = CARTESIAN_POINT('Ctrl Pts',(-18.2336666242668,-40.746384195781,
123.142931895919)) ;
#111796 = CARTESIAN_POINT('Ctrl Pts',(-18.2049587344076,-40.7562429400437,
123.348232185171)) ;
#111797 = CARTESIAN_POINT('Ctrl Pts',(-18.2123617923871,-40.7663110261167,
123.55973493359)) ;
#111798 = CARTESIAN_POINT('Ctrl Pts',(-18.2554723254281,-40.7761665092963,
123.762411205619)) ;
#111799 = CARTESIAN_POINT('Ctrl Pts',(-18.3336239212163,-40.7861613550904,
123.957452729622)) ;
#111800 = CARTESIAN_POINT('Ctrl Pts',(-18.4452499014164,-40.796192650753,
124.13638222185)) ;
#111801 = CARTESIAN_POINT('Ctrl Pts',(-18.5836883141878,-40.8060591940429,
124.290859237411)) ;
#111802 = CARTESIAN_POINT('Ctrl Pts',(-18.7486102321774,-40.8160465898062,
124.420767836735)) ;
#111803 = CARTESIAN_POINT('Ctrl Pts',(-18.9327951365055,-40.8259916305362,
124.519771180057)) ;
#111804 = CARTESIAN_POINT('Ctrl Pts',(-19.1333460863393,-40.8360361367529,
124.585816740584)) ;
#111805 = CARTESIAN_POINT('Ctrl Pts',(-19.3385664444487,-40.8458996428903,
124.615684129492)) ;
#111806 = CARTESIAN_POINT('Ctrl Pts',(-19.5485335498232,-40.8558925037263,
124.609757099615)) ;
#111807 = CARTESIAN_POINT('Ctrl Pts',(-19.7529882392803,-40.8658186974453,
124.567828903137)) ;
#111808 = CARTESIAN_POINT('Ctrl Pts',(-19.9488341180264,-40.8758376234778,
124.49037745935)) ;
#111809 = CARTESIAN_POINT('Ctrl Pts',(-20.1265465040341,-40.8857526228454,
124.38137945927)) ;
#111810 = CARTESIAN_POINT('Ctrl Pts',(-20.2847612738675,-40.8958073944027,
124.241237878504)) ;
#111811 = CARTESIAN_POINT('Ctrl Pts',(-20.4138157607911,-40.9056663567003,
124.079019149827)) ;
#111812 = CARTESIAN_POINT('Ctrl Pts',(-20.5144188196696,-40.9156606005381,
123.894597657184)) ;
#111813 = CARTESIAN_POINT('Ctrl Pts',(-20.5811232695722,-40.9255858299624,
123.696852841891)) ;
#111814 = CARTESIAN_POINT('Ctrl Pts',(-20.6128038079446,-40.9356137938538,
123.48845561963)) ;
#111815 = CARTESIAN_POINT('Ctrl Pts',(-20.6081018191365,-40.9455000534842,
123.280637167687)) ;
#111816 = CARTESIAN_POINT('Ctrl Pts',(-20.566908383739,-40.9555318165621,
123.073835757362)) ;
#111817 = CARTESIAN_POINT('Ctrl Pts',(-20.4917400768975,-40.9654134428562,
122.880129133333)) ;
#111818 = CARTESIAN_POINT('Ctrl Pts',(-20.3822003818654,-40.9754752123424,
122.699206744954)) ;
#111819 = CARTESIAN_POINT('Ctrl Pts',(-20.2457425750103,-40.9853330798378,
122.543195292142)) ;
#111820 = CARTESIAN_POINT('Ctrl Pts',(-20.0824091257493,-40.9953247049552,
122.411153443483)) ;
#111821 = CARTESIAN_POINT('Ctrl Pts',(-19.8995867943335,-41.0052615040634,
122.310050755017)) ;
#111822 = CARTESIAN_POINT('Ctrl Pts',(-19.7010211124057,-41.0152523336208,
122.241575154726)) ;
#111823 = CARTESIAN_POINT('Ctrl Pts',(-19.4928678585313,-41.025275569334,
122.208751641588)) ;
#111824 = CARTESIAN_POINT('Ctrl Pts',(-19.2848503632379,-41.0351719173631,
122.212345030709)) ;
#111825 = CARTESIAN_POINT('Ctrl Pts',(-19.07859298932,-41.0451614798656,122.251938903219)) ;
#111826 = CARTESIAN_POINT('Ctrl Pts',(-18.8815182468336,-41.0552017875502,
122.327514551695)) ;
#111827 = CARTESIAN_POINT('Ctrl Pts',(-18.7039001242788,-41.0650440908974,
122.433692972669)) ;
#111828 = CARTESIAN_POINT('Ctrl Pts',(-18.544387928971,-41.0750677991764,
122.571346729459)) ;
#111829 = CARTESIAN_POINT('Ctrl Pts',(-18.3685498844597,-41.0882899766441,
122.786707534414)) ;
#111830 = CARTESIAN_POINT('Ctrl Pts',(-18.2520956580198,-41.1015825617034,
123.044183223302)) ;
#111831 = CARTESIAN_POINT('Ctrl Pts',(-18.2068004018191,-41.114867417625,
123.319789093301)) ;
#111832 = CARTESIAN_POINT('Ctrl Pts',(-18.2090769320335,-41.1248396447978,
123.529402799935)) ;
#111833 = CARTESIAN_POINT('Ctrl Pts',(-18.2471245872075,-41.1347482612368,
123.734233106963)) ;
#111834 = CARTESIAN_POINT('Ctrl Pts',(-18.3212891930769,-41.1448014666205,
123.932122543222)) ;
#111835 = CARTESIAN_POINT('Ctrl Pts',(-18.4265788315876,-41.1546666003808,
124.110821692057)) ;
#111836 = CARTESIAN_POINT('Ctrl Pts',(-18.6083393135342,-41.1680056580072,
124.324380236434)) ;
#111837 = CARTESIAN_POINT('Ctrl Pts',(-18.8983224768309,-41.1845748453403,
124.524474984768)) ;
#111838 = CARTESIAN_POINT('Ctrl Pts',(-19.2406726079015,-41.2012199851913,
124.614254619646)) ;
#111839 = CARTESIAN_POINT('Ctrl Pts',(-19.5196924195731,-41.2144922876647,
124.612735689302)) ;
#111840 = CARTESIAN_POINT('Ctrl Pts',(-19.7261710268642,-41.2244732511124,
124.575442063407)) ;
#111841 = CARTESIAN_POINT('Ctrl Pts',(-19.9223349265476,-41.2344150831817,
124.503254224524)) ;
#111842 = CARTESIAN_POINT('Ctrl Pts',(-20.1643779768538,-41.2477346523971,
124.362491046623)) ;
#111843 = CARTESIAN_POINT('Ctrl Pts',(-20.4126434461924,-41.2642648073298,
124.113592004093)) ;
#111844 = CARTESIAN_POINT('Ctrl Pts',(-20.5921670689411,-41.2842865328219,
123.72769435448)) ;
#111845 = CARTESIAN_POINT('Ctrl Pts',(-20.6290956635991,-41.3040979294287,
123.307969336178)) ;
#111846 = CARTESIAN_POINT('Ctrl Pts',(-20.5203624950541,-41.3240831781376,
122.897277537584)) ;
#111847 = CARTESIAN_POINT('Ctrl Pts',(-20.2787817615362,-41.3439772407735,
122.549964002153)) ;
#111848 = CARTESIAN_POINT('Ctrl Pts',(-19.9329550212592,-41.3639089199471,
122.305004739995)) ;
#111849 = CARTESIAN_POINT('Ctrl Pts',(-19.5235494591319,-41.3838729744191,
122.192845305889)) ;
#111850 = CARTESIAN_POINT('Ctrl Pts',(-19.102163510832,-41.403753876182,122.226667859758)) ;
#111851 = CARTESIAN_POINT('Ctrl Pts',(-18.7163705084351,-41.4236925377904,
122.402389708857)) ;
#111852 = CARTESIAN_POINT('Ctrl Pts',(-18.4142829500388,-41.4435890630457,
122.698551075891)) ;
#111853 = CARTESIAN_POINT('Ctrl Pts',(-18.2307708887597,-41.4634841015001,
123.079712317658)) ;
#111854 = CARTESIAN_POINT('Ctrl Pts',(-18.1882630471687,-41.4834479248061,
123.502031962921)) ;
#111855 = CARTESIAN_POINT('Ctrl Pts',(-18.2916655233516,-41.5033220489352,
123.911795907653)) ;
#111856 = CARTESIAN_POINT('Ctrl Pts',(-18.5295625666408,-41.5232971246625,
124.263664540088)) ;
#111857 = CARTESIAN_POINT('Ctrl Pts',(-18.8732195093216,-41.5432506940191,
124.512455105266)) ;
#111858 = CARTESIAN_POINT('Ctrl Pts',(-19.278571245914,-41.5630886042069,
124.62913406829)) ;
#111859 = CARTESIAN_POINT('Ctrl Pts',(-19.7023608337579,-41.5830644327778,
124.600734803121)) ;
#111860 = CARTESIAN_POINT('Ctrl Pts',(-20.0896826671183,-41.6029824774881,
124.42950456159)) ;
#111861 = CARTESIAN_POINT('Ctrl Pts',(-20.3954161122859,-41.6228527232758,
124.137780484374)) ;
#111862 = CARTESIAN_POINT('Ctrl Pts',(-20.5842821915269,-41.6429017263753,
123.755726897361)) ;
#111863 = CARTESIAN_POINT('Ctrl Pts',(-20.631293225079,-41.6626809676162,
123.337676657674)) ;
#111864 = CARTESIAN_POINT('Ctrl Pts',(-20.5322532304651,-41.682711031325,
122.923558200882)) ;
#111865 = CARTESIAN_POINT('Ctrl Pts',(-20.298910163309,-41.702593316227,122.570959878373)) ;
#111866 = CARTESIAN_POINT('Ctrl Pts',(-19.9600335550022,-41.72247561712,122.318274201022)) ;
#111867 = CARTESIAN_POINT('Ctrl Pts',(-19.5531343747822,-41.7424587267384,
122.19589847905)) ;
#111868 = CARTESIAN_POINT('Ctrl Pts',(-19.1308510498446,-41.7623491221162,
122.219664287497)) ;
#111869 = CARTESIAN_POINT('Ctrl Pts',(-18.7417287028976,-41.7822459121505,
122.385543059357)) ;
#111870 = CARTESIAN_POINT('Ctrl Pts',(-18.4318798816301,-41.8021629660921,
122.674260758328)) ;
#111871 = CARTESIAN_POINT('Ctrl Pts',(-18.2384283480196,-41.8221665142956,
123.053114122942)) ;
#111872 = CARTESIAN_POINT('Ctrl Pts',(-18.1866756004169,-41.8421048079482,
123.473865156741)) ;
#111873 = CARTESIAN_POINT('Ctrl Pts',(-18.2800552935238,-41.8619262953812,
123.884855074471)) ;
#111874 = CARTESIAN_POINT('Ctrl Pts',(-18.5094895263513,-41.881904688372,
124.242301840394)) ;
#111875 = CARTESIAN_POINT('Ctrl Pts',(-18.8460304484914,-41.9018030699857,
124.498833972733)) ;
#111876 = CARTESIAN_POINT('Ctrl Pts',(-19.1823088449987,-41.9183860007156,
124.604517397028)) ;
#111877 = CARTESIAN_POINT('Ctrl Pts',(-19.461177798175,-41.9316602363045,
124.616769086704)) ;
#111878 = CARTESIAN_POINT('Ctrl Pts',(-19.6705412714561,-41.9417066537607,
124.589154093643)) ;
#111879 = CARTESIAN_POINT('Ctrl Pts',(-19.8680188194388,-41.9515518789799,
124.527075358096)) ;
#111880 = CARTESIAN_POINT('Ctrl Pts',(-20.117018044822,-41.9648868500193,
124.39842617402)) ;
#111881 = CARTESIAN_POINT('Ctrl Pts',(-20.3777930102394,-41.981469706812,
124.160899063277)) ;
#111882 = CARTESIAN_POINT('Ctrl Pts',(-20.5424084430053,-41.9981127091614,
123.847785516672)) ;
#111883 = CARTESIAN_POINT('Ctrl Pts',(-20.6040494652692,-42.011356440193,
123.576174911359)) ;
#111884 = CARTESIAN_POINT('Ctrl Pts',(-20.6143195417858,-42.0214108348676,
123.365095967157)) ;
#111885 = CARTESIAN_POINT('Ctrl Pts',(-20.588604650163,-42.0312518962562,
123.159770506357)) ;
#111886 = CARTESIAN_POINT('Ctrl Pts',(-20.5264528198864,-42.0413181206127,
122.957516925225)) ;
#111887 = CARTESIAN_POINT('Ctrl Pts',(-20.431816816729,-42.0511987335323,
122.772567374822)) ;
#111888 = CARTESIAN_POINT('Ctrl Pts',(-20.3054350733916,-42.061192026692,
122.6047834817)) ;
#111889 = CARTESIAN_POINT('Ctrl Pts',(-20.1524929814204,-42.0711430349156,
122.461991966139)) ;
#111890 = CARTESIAN_POINT('Ctrl Pts',(-19.9753246537659,-42.0811915492776,
122.346976367142)) ;
#111891 = CARTESIAN_POINT('Ctrl Pts',(-19.7849352437681,-42.0910330553402,
122.265936576408)) ;
#111892 = CARTESIAN_POINT('Ctrl Pts',(-19.580570099987,-42.1010187079699,
122.218064982014)) ;
#111893 = CARTESIAN_POINT('Ctrl Pts',(-19.3719158525698,-42.1109577168148,
122.206376314343)) ;
#111894 = CARTESIAN_POINT('Ctrl Pts',(-19.1623315554076,-42.1209986421078,
122.231396668231)) ;
#111895 = CARTESIAN_POINT('Ctrl Pts',(-18.9632343186275,-42.1308889638627,
122.291405170605)) ;
#111896 = CARTESIAN_POINT('Ctrl Pts',(-18.7754898804389,-42.1408849371962,
122.385779478317)) ;
#111897 = CARTESIAN_POINT('Ctrl Pts',(-18.6080417247803,-42.1508163367782,
122.510510591969)) ;
#111898 = CARTESIAN_POINT('Ctrl Pts',(-18.463506882559,-42.1608218772553,
122.663351602255)) ;
#111899 = CARTESIAN_POINT('Ctrl Pts',(-18.3477206552532,-42.1708548611866,
122.839646219681)) ;
#111900 = CARTESIAN_POINT('Ctrl Pts',(-18.2654323528944,-42.1807104920134,
123.02981919676)) ;
#111901 = CARTESIAN_POINT('Ctrl Pts',(-18.2164610104545,-42.1907098942066,
123.234217498079)) ;
#111902 = CARTESIAN_POINT('Ctrl Pts',(-18.2036137360674,-42.2006043635676,
123.441872055247)) ;
#111903 = CARTESIAN_POINT('Ctrl Pts',(-18.227470411628,-42.2106674777319,
123.652044464352)) ;
#111904 = CARTESIAN_POINT('Ctrl Pts',(-18.2859262935667,-42.2205071234482,
123.850509118278)) ;
#111905 = CARTESIAN_POINT('Ctrl Pts',(-18.3797751516572,-42.230570291004,
124.040081096163)) ;
#111906 = CARTESIAN_POINT('Ctrl Pts',(-18.5031830583083,-42.2404645467989,
124.207555011868)) ;
#111907 = CARTESIAN_POINT('Ctrl Pts',(-18.6540904565505,-42.2504063252585,
124.352124384181)) ;
#111908 = CARTESIAN_POINT('Ctrl Pts',(-18.8288746807045,-42.2604090180887,
124.46909956343)) ;
#111909 = CARTESIAN_POINT('Ctrl Pts',(-19.0220120842227,-42.2704430400425,
124.553906048458)) ;
#111910 = CARTESIAN_POINT('Ctrl Pts',(-19.2230780812026,-42.2802908311316,
124.603274405477)) ;
#111911 = CARTESIAN_POINT('Ctrl Pts',(-19.4324117207057,-42.2902723556806,
124.617627506357)) ;
#111912 = CARTESIAN_POINT('Ctrl Pts',(-19.640404045017,-42.3002215791715,
124.595453200088)) ;
#111913 = CARTESIAN_POINT('Ctrl Pts',(-19.8424487261026,-42.3102192353881,
124.537470807969)) ;
#111914 = CARTESIAN_POINT('Ctrl Pts',(-20.0319545563167,-42.3202594484432,
124.44454462917)) ;
#111915 = CARTESIAN_POINT('Ctrl Pts',(-20.1991303071474,-42.3300874957194,
124.323105380383)) ;
#111916 = CARTESIAN_POINT('Ctrl Pts',(-20.3462067287079,-42.3401418427518,
124.171307388996)) ;
#111917 = CARTESIAN_POINT('Ctrl Pts',(-20.463075259657,-42.3500829790803,
123.998036465554)) ;
#111918 = CARTESIAN_POINT('Ctrl Pts',(-20.5483561164731,-42.3599872121601,
123.808079120287)) ;
#111919 = CARTESIAN_POINT('Ctrl Pts',(-20.5999588950317,-42.3700339090037,
123.603285104193)) ;
#111920 = CARTESIAN_POINT('Ctrl Pts',(-20.6151816987204,-42.3799294602839,
123.395773546933)) ;
#111921 = CARTESIAN_POINT('Ctrl Pts',(-20.5937949650998,-42.3899915381234,
123.185351125372)) ;
#111922 = CARTESIAN_POINT('Ctrl Pts',(-20.5375522532826,-42.3998342472195,
122.986192499132)) ;
#111923 = CARTESIAN_POINT('Ctrl Pts',(-20.4467001735165,-42.4098249794579,
122.796851438406)) ;
#111924 = CARTESIAN_POINT('Ctrl Pts',(-20.3250709463571,-42.4197530046867,
122.627221623983)) ;
#111925 = CARTESIAN_POINT('Ctrl Pts',(-20.1751865675631,-42.4297411513373,
122.480152722109)) ;
#111926 = CARTESIAN_POINT('Ctrl Pts',(-20.0010496434023,-42.4397761691772,
122.361052246818)) ;
#111927 = CARTESIAN_POINT('Ctrl Pts',(-19.8122379147055,-42.4496409662824,
122.275279709418)) ;
#111928 = CARTESIAN_POINT('Ctrl Pts',(-19.6095892045483,-42.4596016986385,
122.222493576233)) ;
#111929 = CARTESIAN_POINT('Ctrl Pts',(-19.3993145753135,-42.4696351610355,
122.205926016389)) ;
#111930 = CARTESIAN_POINT('Ctrl Pts',(-19.1923871065186,-42.4795206952469,
122.225479642791)) ;
#111931 = CARTESIAN_POINT('Ctrl Pts',(-18.9884138471623,-42.4895855359269,
122.281660888493)) ;
#111932 = CARTESIAN_POINT('Ctrl Pts',(-18.8013313907338,-42.4994336676558,
122.370385291505)) ;
#111933 = CARTESIAN_POINT('Ctrl Pts',(-18.6291240560497,-42.5094611646459,
122.491969970082)) ;
#111934 = CARTESIAN_POINT('Ctrl Pts',(-18.4810143630638,-42.519489616691,
122.642027847986)) ;
#111935 = CARTESIAN_POINT('Ctrl Pts',(-18.3630867111402,-42.5293348832551,
122.812110770155)) ;
#111936 = CARTESIAN_POINT('Ctrl Pts',(-18.2746848318278,-42.539325556196,
123.002642514541)) ;
#111937 = CARTESIAN_POINT('Ctrl Pts',(-18.2209096538713,-42.5493634382845,
123.206701684777)) ;
#111938 = CARTESIAN_POINT('Ctrl Pts',(-18.2033597633638,-42.5592078087242,
123.412923585972)) ;
#111939 = CARTESIAN_POINT('Ctrl Pts',(-18.2217313839453,-42.5691926361195,
123.622001992178)) ;
#111940 = CARTESIAN_POINT('Ctrl Pts',(-18.2758046426485,-42.5791320815248,
123.823874085808)) ;
#111941 = CARTESIAN_POINT('Ctrl Pts',(-18.3650343462559,-42.5891720858107,
124.015135264948)) ;
#111942 = CARTESIAN_POINT('Ctrl Pts',(-18.4841828213854,-42.5990591949964,
124.185483118143)) ;
#111943 = CARTESIAN_POINT('Ctrl Pts',(-18.6325539737966,-42.6090592548988,
124.334379885104)) ;
#111944 = CARTESIAN_POINT('Ctrl Pts',(-18.8030555249044,-42.6189766708135,
124.454437541171)) ;
#111945 = CARTESIAN_POINT('Ctrl Pts',(-18.9942434053939,-42.6290234855543,
124.544141426732)) ;
#111946 = CARTESIAN_POINT('Ctrl Pts',(-19.1946308598923,-42.638898962751,
124.598568573232)) ;
#111947 = CARTESIAN_POINT('Ctrl Pts',(-19.4051266120994,-42.6489550584722,
124.617829207744)) ;
#111948 = CARTESIAN_POINT('Ctrl Pts',(-19.612437254331,-42.6588482204873,
124.600604757448)) ;
#111949 = CARTESIAN_POINT('Ctrl Pts',(-19.8169977341629,-42.6689104565099,
124.546818623211)) ;
#111950 = CARTESIAN_POINT('Ctrl Pts',(-20.0049932843688,-42.6787549221389,
124.460251074525)) ;
#111951 = CARTESIAN_POINT('Ctrl Pts',(-20.1775205573937,-42.688715014843,
124.341599711872)) ;
#111952 = CARTESIAN_POINT('Ctrl Pts',(-20.3277014204995,-42.698753303824,
124.193350176597)) ;
#111953 = CARTESIAN_POINT('Ctrl Pts',(-20.4482019333063,-42.7086266269302,
124.024302181984)) ;
#111954 = CARTESIAN_POINT('Ctrl Pts',(-20.5392351844517,-42.7186998110153,
123.833143580073)) ;
#111955 = CARTESIAN_POINT('Ctrl Pts',(-20.5945600836748,-42.7285203233033,
123.634190030685)) ;
#111956 = CARTESIAN_POINT('Ctrl Pts',(-20.6152165698879,-42.7385983194191,
123.423378102018)) ;
#111957 = CARTESIAN_POINT('Ctrl Pts',(-20.5993584671312,-42.7484523944023,
123.216774912312)) ;
#111958 = CARTESIAN_POINT('Ctrl Pts',(-20.5470175821238,-42.758516275986,
123.011818471691)) ;
#111959 = CARTESIAN_POINT('Ctrl Pts',(-20.4613810858779,-42.7683997019598,
122.822467078789)) ;
#111960 = CARTESIAN_POINT('Ctrl Pts',(-20.3430959897355,-42.7784003058808,
122.64869772331)) ;
#111961 = CARTESIAN_POINT('Ctrl Pts',(-20.1976636242682,-42.7883200902187,
122.499177550356)) ;
#111962 = CARTESIAN_POINT('Ctrl Pts',(-20.0263331492517,-42.7983674405756,
122.375694718542)) ;
#111963 = CARTESIAN_POINT('Ctrl Pts',(-19.8394215960014,-42.8082447828098,
122.285136347955)) ;
#111964 = CARTESIAN_POINT('Ctrl Pts',(-19.6358073460402,-42.8183146638845,
122.227338104629)) ;
#111965 = CARTESIAN_POINT('Ctrl Pts',(-19.430216265058,-42.8281443690862,
122.206062548162)) ;
#111966 = CARTESIAN_POINT('Ctrl Pts',(-19.2191370280308,-42.8382110302526,
122.22087554616)) ;
#111967 = CARTESIAN_POINT('Ctrl Pts',(-19.0174085150384,-42.8481012521199,
122.271357806117)) ;
#111968 = CARTESIAN_POINT('Ctrl Pts',(-18.8253990069409,-42.85809342823,122.356536932198)) ;
#111969 = CARTESIAN_POINT('Ctrl Pts',(-18.6517135987976,-42.8680562583427,
122.473586088928)) ;
#111970 = CARTESIAN_POINT('Ctrl Pts',(-18.5014927325004,-42.877960470743,
122.617793286138)) ;
#111971 = CARTESIAN_POINT('Ctrl Pts',(-18.3768296433921,-42.8880211848308,
122.788624062866)) ;
#111972 = CARTESIAN_POINT('Ctrl Pts',(-18.2854888209971,-42.8978606878136,
122.974258158057)) ;
#111973 = CARTESIAN_POINT('Ctrl Pts',(-18.226249141792,-42.90792682638,123.177384208037)) ;
#111974 = CARTESIAN_POINT('Ctrl Pts',(-18.2036698022387,-42.9178093408661,
123.383946267231)) ;
#111975 = CARTESIAN_POINT('Ctrl Pts',(-18.2170344052626,-42.9278016402216,
123.593558136021)) ;
#111976 = CARTESIAN_POINT('Ctrl Pts',(-18.2663606150584,-42.937754707175,
123.796938051307)) ;
#111977 = CARTESIAN_POINT('Ctrl Pts',(-18.3510009303235,-42.9477894153802,
123.99015807792)) ;
#111978 = CARTESIAN_POINT('Ctrl Pts',(-18.4660869987782,-42.9576776362844,
124.163290919993)) ;
#111979 = CARTESIAN_POINT('Ctrl Pts',(-18.6107602048254,-42.9676720593148,
124.315648466723)) ;
#111980 = CARTESIAN_POINT('Ctrl Pts',(-18.7789193125409,-42.977617398761,
124.43989854007)) ;
#111981 = CARTESIAN_POINT('Ctrl Pts',(-18.9659524266887,-42.9875647433723,
124.533471638483)) ;
#111982 = CARTESIAN_POINT('Ctrl Pts',(-19.1684697409131,-42.9976126387833,
124.593517727441)) ;
#111983 = CARTESIAN_POINT('Ctrl Pts',(-19.3741416291269,-43.0074602842627,
124.617185921389)) ;
#111984 = CARTESIAN_POINT('Ctrl Pts',(-19.5832202082557,-43.0174219981767,
124.605295316354)) ;
#111985 = CARTESIAN_POINT('Ctrl Pts',(-19.7883889263271,-43.0274506224676,
124.556694685865)) ;
#111986 = CARTESIAN_POINT('Ctrl Pts',(-19.9797240658731,-43.0373609831244,
124.474263460181)) ;
#111987 = CARTESIAN_POINT('Ctrl Pts',(-20.1545850142046,-43.0472956816976,
124.360032533365)) ;
#111988 = CARTESIAN_POINT('Ctrl Pts',(-20.3084426092712,-43.0573375065518,
124.215494418398)) ;
#111989 = CARTESIAN_POINT('Ctrl Pts',(-20.4330508501372,-43.0672220802963,
124.049170656684)) ;
#111990 = CARTESIAN_POINT('Ctrl Pts',(-20.5282031046947,-43.0772239296594,
123.861693414148)) ;
#111991 = CARTESIAN_POINT('Ctrl Pts',(-20.5890161497155,-43.0871432312335,
123.662193958205)) ;
#111992 = CARTESIAN_POINT('Ctrl Pts',(-20.6145826704146,-43.0971873395787,
123.452605924384)) ;
#111993 = CARTESIAN_POINT('Ctrl Pts',(-20.6036090469699,-43.107071763021,
123.245085036931)) ;
#111994 = CARTESIAN_POINT('Ctrl Pts',(-20.5566009430782,-43.1170881249304,
123.039815571423)) ;
#111995 = CARTESIAN_POINT('Ctrl Pts',(-20.4739955187747,-43.1271247804358,
122.845667638388)) ;
#111996 = CARTESIAN_POINT('Ctrl Pts',(-20.3617551658394,-43.1369549106252,
122.672114443644)) ;
#111997 = CARTESIAN_POINT('Ctrl Pts',(-20.2176634788176,-43.147030963715,
122.516896574677)) ;
#111998 = CARTESIAN_POINT('Ctrl Pts',(-20.0525626841022,-43.1568831929008,
122.39175485612)) ;
#111999 = CARTESIAN_POINT('Ctrl Pts',(-19.8642574206319,-43.1669564007001,
122.294937497257)) ;
#112000 = CARTESIAN_POINT('Ctrl Pts',(-19.6665927303785,-43.1767979120515,
122.233768964213)) ;
#112001 = CARTESIAN_POINT('Ctrl Pts',(-19.4589388734095,-43.1867588500891,
122.206756446791)) ;
#112002 = CARTESIAN_POINT('Ctrl Pts',(-19.2481526968511,-43.196796712014,
122.216705348309)) ;
#112003 = CARTESIAN_POINT('Ctrl Pts',(-19.0455360209674,-43.2066708980111,
122.261974508476)) ;
#112004 = CARTESIAN_POINT('Ctrl Pts',(-18.8501121762515,-43.216741057589,
122.343316558559)) ;
#112005 = CARTESIAN_POINT('Ctrl Pts',(-18.675890563891,-43.2265728050148,
122.454570961457)) ;
#112006 = CARTESIAN_POINT('Ctrl Pts',(-18.5201203546228,-43.2366088850861,
122.596866177134)) ;
#112007 = CARTESIAN_POINT('Ctrl Pts',(-18.3920760831414,-43.2466259319386,
122.76407083837)) ;
#112008 = CARTESIAN_POINT('Ctrl Pts',(-18.2959713810654,-43.2565081901052,
122.948265792227)) ;
#112009 = CARTESIAN_POINT('Ctrl Pts',(-18.2324177679235,-43.2664958729016,
123.148366411114)) ;
#112010 = CARTESIAN_POINT('Ctrl Pts',(-18.2045129717693,-43.2764425296183,
123.355638672475)) ;
#112011 = CARTESIAN_POINT('Ctrl Pts',(-18.2133309385032,-43.2864995876985,
123.566862560092)) ;
#112012 = CARTESIAN_POINT('Ctrl Pts',(-18.2573403282676,-43.2963177672479,
123.768536209006)) ;
#112013 = CARTESIAN_POINT('Ctrl Pts',(-18.3369007822062,-43.3063537016869,
123.963941913838)) ;
#112014 = CARTESIAN_POINT('Ctrl Pts',(-18.4495740797396,-43.3163783561159,
124.142052896215)) ;
#112015 = CARTESIAN_POINT('Ctrl Pts',(-18.5886758351092,-43.3262303756954,
124.29551560948)) ;
#112016 = CARTESIAN_POINT('Ctrl Pts',(-18.7543989660692,-43.3362212894104,
124.424520489361)) ;
#112017 = CARTESIAN_POINT('Ctrl Pts',(-18.9386300394327,-43.3461392782499,
124.522216828266)) ;
#112018 = CARTESIAN_POINT('Ctrl Pts',(-19.1391738917971,-43.3561673889807,
124.587189239485)) ;
#112019 = CARTESIAN_POINT('Ctrl Pts',(-19.3449855840381,-43.3660525868891,
124.616027510103)) ;
#112020 = CARTESIAN_POINT('Ctrl Pts',(-19.554884063921,-43.3760418621571,
124.609127952486)) ;
#112021 = CARTESIAN_POINT('Ctrl Pts',(-19.7613652559724,-43.3860833203266,
124.56521717942)) ;
#112022 = CARTESIAN_POINT('Ctrl Pts',(-19.9531454597752,-43.395914784115,
124.488123637092)) ;
#112023 = CARTESIAN_POINT('Ctrl Pts',(-20.1319421270881,-43.4059197164188,
124.377388853606)) ;
#112024 = CARTESIAN_POINT('Ctrl Pts',(-20.2884737430992,-43.4159060803136,
124.23742474908)) ;
#112025 = CARTESIAN_POINT('Ctrl Pts',(-20.4187237680991,-43.4259357091994,
124.071633940788)) ;
#112026 = CARTESIAN_POINT('Ctrl Pts',(-20.5169317592403,-43.4358109313078,
123.888700540312)) ;
#112027 = CARTESIAN_POINT('Ctrl Pts',(-20.5829335072602,-43.4458121437049,
123.68910626295)) ;
#112028 = CARTESIAN_POINT('Ctrl Pts',(-20.6132012525155,-43.4557207229405,
123.482970481711)) ;
#112029 = CARTESIAN_POINT('Ctrl Pts',(-20.6070669616249,-43.4657755754965,
123.271709054527)) ;
#112030 = CARTESIAN_POINT('Ctrl Pts',(-20.5653971827007,-43.4756341577712,
123.068645639476)) ;
#112031 = CARTESIAN_POINT('Ctrl Pts',(-20.4876247610563,-43.4857022872139,
122.87182093088)) ;
#112032 = CARTESIAN_POINT('Ctrl Pts',(-20.3791588412689,-43.495557758903,
122.695267056003)) ;
#112033 = CARTESIAN_POINT('Ctrl Pts',(-20.2402289738578,-43.5055526072893,
122.537636595006)) ;
#112034 = CARTESIAN_POINT('Ctrl Pts',(-20.0751488316468,-43.5155839040738,
122.406393649367)) ;
#112035 = CARTESIAN_POINT('Ctrl Pts',(-19.8929883675451,-43.5254504402838,
122.307167892137)) ;
#112036 = CARTESIAN_POINT('Ctrl Pts',(-19.6940946141925,-43.5354378632447,
122.239956902472)) ;
#112037 = CARTESIAN_POINT('Ctrl Pts',(-19.4873991266177,-43.5453828022644,
122.208320983698)) ;
#112038 = CARTESIAN_POINT('Ctrl Pts',(-19.2762948216171,-43.5554276881244,
122.213202323494)) ;
#112039 = CARTESIAN_POINT('Ctrl Pts',(-19.072838073808,-43.5652962232107,
122.253829835183)) ;
#112040 = CARTESIAN_POINT('Ctrl Pts',(-18.8774218528688,-43.5752620912173,
122.329360633563)) ;
#112041 = CARTESIAN_POINT('Ctrl Pts',(-18.6971695641427,-43.5852847386698,
122.438507175185)) ;
#112042 = CARTESIAN_POINT('Ctrl Pts',(-18.5401539946423,-43.5952083776774,
122.575862295527)) ;
#112043 = CARTESIAN_POINT('Ctrl Pts',(-18.4087164825012,-43.6051511026832,
122.738409619408)) ;
#112044 = CARTESIAN_POINT('Ctrl Pts',(-18.3066850874188,-43.615196708735,
122.923303971004)) ;
#112045 = CARTESIAN_POINT('Ctrl Pts',(-18.2393358638878,-43.6250581312561,
123.119396369836)) ;
#112046 = CARTESIAN_POINT('Ctrl Pts',(-18.2062782392345,-43.6350516997053,
123.326845266776)) ;
#112047 = CARTESIAN_POINT('Ctrl Pts',(-18.2096114923245,-43.6449771704606,
123.53551409604)) ;
#112048 = CARTESIAN_POINT('Ctrl Pts',(-18.249512391208,-43.6550048444165,
123.742490554767)) ;
#112049 = CARTESIAN_POINT('Ctrl Pts',(-18.3235215022522,-43.6648920224582,
123.936757740212)) ;
#112050 = CARTESIAN_POINT('Ctrl Pts',(-18.4315053078655,-43.6749204018264,
124.11780036)) ;
#112051 = CARTESIAN_POINT('Ctrl Pts',(-18.5673876440628,-43.6848146445478,
124.275321991375)) ;
#112052 = CARTESIAN_POINT('Ctrl Pts',(-18.7847152892274,-43.6981675611987,
124.452998678916)) ;
#112053 = CARTESIAN_POINT('Ctrl Pts',(-19.0405842553741,-43.7113700789455,
124.568622037401)) ;
#112054 = CARTESIAN_POINT('Ctrl Pts',(-19.3175542136474,-43.7247259842264,
124.614316021264)) ;
#112055 = CARTESIAN_POINT('Ctrl Pts',(-19.5256380473388,-43.7346226328643,
124.612215852115)) ;
#112056 = CARTESIAN_POINT('Ctrl Pts',(-19.73328492877,-43.7446707709167,124.57350778193)) ;
#112057 = CARTESIAN_POINT('Ctrl Pts',(-19.9279877373747,-43.7545617310945,
124.500478282354)) ;
#112058 = CARTESIAN_POINT('Ctrl Pts',(-20.1091624315112,-43.7645545669713,
124.394118393869)) ;
#112059 = CARTESIAN_POINT('Ctrl Pts',(-20.2695300895979,-43.7745936619728,
124.25692653165)) ;
#112060 = CARTESIAN_POINT('Ctrl Pts',(-20.4013372670491,-43.784431017824,
124.097532222068)) ;
#112061 = CARTESIAN_POINT('Ctrl Pts',(-20.5404948427755,-43.7978239657547,
123.852796202382)) ;
#112062 = CARTESIAN_POINT('Ctrl Pts',(-20.6114147034954,-43.8109906421817,
123.581864059881)) ;
#112063 = CARTESIAN_POINT('Ctrl Pts',(-20.6101144842842,-43.8243754235884,
123.300568261177)) ;
#112064 = CARTESIAN_POINT('Ctrl Pts',(-20.5732481420028,-43.8342372062323,
123.09650308057)) ;
#112065 = CARTESIAN_POINT('Ctrl Pts',(-20.5008588905469,-43.8442363541853,
122.899193642545)) ;
#112066 = CARTESIAN_POINT('Ctrl Pts',(-20.3964490350757,-43.8541391468024,
122.719027204123)) ;
#112067 = CARTESIAN_POINT('Ctrl Pts',(-20.2603777403452,-43.8641887266934,
122.557479655234)) ;
#112068 = CARTESIAN_POINT('Ctrl Pts',(-20.0479297146214,-43.8773758005028,
122.379174658217)) ;
#112069 = CARTESIAN_POINT('Ctrl Pts',(-19.7251920374131,-43.894128590474,
122.228850599484)) ;
#112070 = CARTESIAN_POINT('Ctrl Pts',(-19.375730609699,-43.9106172425687,
122.198236073225)) ;
#112071 = CARTESIAN_POINT('Ctrl Pts',(-19.0992070500844,-43.9239740687521,
122.246385626479)) ;
#112072 = CARTESIAN_POINT('Ctrl Pts',(-18.9034615109419,-43.9338704536301,
122.317045147132)) ;
#112073 = CARTESIAN_POINT('Ctrl Pts',(-18.7209976848891,-43.9438769681505,
122.421622210258)) ;
#112074 = CARTESIAN_POINT('Ctrl Pts',(-18.5074835665858,-43.9570670916669,
122.598733350696)) ;
#112075 = CARTESIAN_POINT('Ctrl Pts',(-18.3017386622612,-43.9738336528165,
122.88970118387)) ;
#112076 = CARTESIAN_POINT('Ctrl Pts',(-18.1906974881969,-43.9936181415245,
123.295581178581)) ;
#112077 = CARTESIAN_POINT('Ctrl Pts',(-18.2237801253929,-44.013563589121,
123.718275771807)) ;
#112078 = CARTESIAN_POINT('Ctrl Pts',(-18.399237608955,-44.0334752512769,
124.103593520298)) ;
#112079 = CARTESIAN_POINT('Ctrl Pts',(-18.6947326988886,-44.0533674432958,
124.406305831262)) ;
#112080 = CARTESIAN_POINT('Ctrl Pts',(-19.0788065914813,-44.0734085738504,
124.590755928571)) ;
#112081 = CARTESIAN_POINT('Ctrl Pts',(-19.4981951038131,-44.093226908466,
124.632839132586)) ;
#112082 = CARTESIAN_POINT('Ctrl Pts',(-19.9098771362282,-44.1131994736856,
124.529198585816)) ;
#112083 = CARTESIAN_POINT('Ctrl Pts',(-20.2603247768381,-44.1330886898572,
124.29220689285)) ;
#112084 = CARTESIAN_POINT('Ctrl Pts',(-20.5101502363749,-44.1531122641799,
123.947585111656)) ;
#112085 = CARTESIAN_POINT('Ctrl Pts',(-20.6263965415741,-44.1729094272682,
123.542934559649)) ;
#112086 = CARTESIAN_POINT('Ctrl Pts',(-20.5983673539183,-44.1928749210919,
123.1194299464)) ;
#112087 = CARTESIAN_POINT('Ctrl Pts',(-20.4270411323208,-44.2128286288334,
122.731166605694)) ;
#112088 = CARTESIAN_POINT('Ctrl Pts',(-20.1343451456775,-44.23273600556,122.425521852271)) ;
#112089 = CARTESIAN_POINT('Ctrl Pts',(-19.7563215601734,-44.2525882171085,
122.237539781473)) ;
#112090 = CARTESIAN_POINT('Ctrl Pts',(-19.3322302168017,-44.2726606040542,
122.189737953661)) ;
#112091 = CARTESIAN_POINT('Ctrl Pts',(-18.9222423305636,-44.2924984736945,
122.288907559817)) ;
#112092 = CARTESIAN_POINT('Ctrl Pts',(-18.5694751926027,-44.3123491282477,
122.520649949583)) ;
#112093 = CARTESIAN_POINT('Ctrl Pts',(-18.3149237536485,-44.3324010625881,
122.862638266878)) ;
#112094 = CARTESIAN_POINT('Ctrl Pts',(-18.1937098847275,-44.3522342501541,
123.266650488517)) ;
#112095 = CARTESIAN_POINT('Ctrl Pts',(-18.2169010073165,-44.3721634623848,
123.689607452994)) ;
#112096 = CARTESIAN_POINT('Ctrl Pts',(-18.3823274082541,-44.3920484275992,
124.078886479811)) ;
#112097 = CARTESIAN_POINT('Ctrl Pts',(-18.6737119070075,-44.4121221687438,
124.390652119878)) ;
#112098 = CARTESIAN_POINT('Ctrl Pts',(-19.0487928360358,-44.4319153505242,
124.58167893321)) ;
#112099 = CARTESIAN_POINT('Ctrl Pts',(-19.4698622989597,-44.4518780585269,
124.634952557951)) ;
#112100 = CARTESIAN_POINT('Ctrl Pts',(-19.8840682422003,-44.4718610102694,
124.540233149876)) ;
#112101 = CARTESIAN_POINT('Ctrl Pts',(-20.2384850678646,-44.4916716300415,
124.312522261016)) ;
#112102 = CARTESIAN_POINT('Ctrl Pts',(-20.496472765814,-44.5116553460744,
123.975018682566)) ;
#112103 = CARTESIAN_POINT('Ctrl Pts',(-20.6231446911847,-44.5315368099717,
123.571598605078)) ;
#112104 = CARTESIAN_POINT('Ctrl Pts',(-20.6047845603425,-44.5514921398161,
123.147777224827)) ;
#112105 = CARTESIAN_POINT('Ctrl Pts',(-20.4437732938135,-44.5713676006216,
122.756972680874)) ;
#112106 = CARTESIAN_POINT('Ctrl Pts',(-20.1577714229677,-44.5913519206731,
122.442775355077)) ;
#112107 = CARTESIAN_POINT('Ctrl Pts',(-19.7825364475005,-44.6112799534628,
122.245734864262)) ;
#112108 = CARTESIAN_POINT('Ctrl Pts',(-19.4327219006692,-44.6278887154025,
122.198048980151)) ;
#112109 = CARTESIAN_POINT('Ctrl Pts',(-19.157580718328,-44.6410763540926,
122.232475357399)) ;
#112110 = CARTESIAN_POINT('Ctrl Pts',(-18.9568220789536,-44.6510627884528,
122.29384808022)) ;
#112111 = CARTESIAN_POINT('Ctrl Pts',(-18.7694045001361,-44.6610721624121,
122.389576711822)) ;
#112112 = CARTESIAN_POINT('Ctrl Pts',(-18.5463500482097,-44.6743621959774,
122.557757582452)) ;
#112113 = CARTESIAN_POINT('Ctrl Pts',(-18.3288731895613,-44.6909561836399,
122.835700482128)) ;
#112114 = CARTESIAN_POINT('Ctrl Pts',(-18.2191010631187,-44.7075884389154,
123.171813055935)) ;
#112115 = CARTESIAN_POINT('Ctrl Pts',(-18.203989244122,-44.7208308225832,
123.449835880554)) ;
#112116 = CARTESIAN_POINT('Ctrl Pts',(-18.2283538978317,-44.7307450308107,
123.656837058028)) ;
#112117 = CARTESIAN_POINT('Ctrl Pts',(-18.289374685234,-44.7408016700823,
123.859247402958)) ;
#112118 = CARTESIAN_POINT('Ctrl Pts',(-18.3824078062696,-44.7506474765025,
124.044169184027)) ;
#112119 = CARTESIAN_POINT('Ctrl Pts',(-18.5083408075851,-44.7606924761356,
124.213687403652)) ;
#112120 = CARTESIAN_POINT('Ctrl Pts',(-18.7114734667272,-44.7739734985084,
124.40516701968)) ;
#112121 = CARTESIAN_POINT('Ctrl Pts',(-18.9580690734197,-44.787170945033,
124.539151428102)) ;
#112122 = CARTESIAN_POINT('Ctrl Pts',(-19.2323659465609,-44.80058524284,124.604770452948)) ;
#112123 = CARTESIAN_POINT('Ctrl Pts',(-19.4388388617706,-44.8104243082428,
124.617358313457)) ;
#112124 = CARTESIAN_POINT('Ctrl Pts',(-19.6474045731059,-44.8204075145204,
124.5941139162)) ;
#112125 = CARTESIAN_POINT('Ctrl Pts',(-19.8481328383631,-44.8303587494332,
124.535120383893)) ;
#112126 = CARTESIAN_POINT('Ctrl Pts',(-20.036617400384,-44.8403597491349,
124.441933673575)) ;
#112127 = CARTESIAN_POINT('Ctrl Pts',(-20.2063667732729,-44.8503910949222,
124.316798054001)) ;
#112128 = CARTESIAN_POINT('Ctrl Pts',(-20.3494471813072,-44.8602448596272,
124.166983999628)) ;
#112129 = CARTESIAN_POINT('Ctrl Pts',(-20.4661047179767,-44.8702155132955,
123.992857697695)) ;
#112130 = CARTESIAN_POINT('Ctrl Pts',(-20.5509965592624,-44.8802127569528,
123.80055675814)) ;
#112131 = CARTESIAN_POINT('Ctrl Pts',(-20.6011158941463,-44.8902462128969,
123.595680546654)) ;
#112132 = CARTESIAN_POINT('Ctrl Pts',(-20.6149939254353,-44.9001017171973,
123.388931897605)) ;
#112133 = CARTESIAN_POINT('Ctrl Pts',(-20.5927233643213,-44.9101011534834,
123.179932791972)) ;
#112134 = CARTESIAN_POINT('Ctrl Pts',(-20.5353204855905,-44.9199956129993,
122.979956605771)) ;
#112135 = CARTESIAN_POINT('Ctrl Pts',(-20.4424886850467,-44.930058732451,
122.789893958215)) ;
#112136 = CARTESIAN_POINT('Ctrl Pts',(-20.3209726648125,-44.939898366863,
122.622445032574)) ;
#112137 = CARTESIAN_POINT('Ctrl Pts',(-20.1690810486208,-44.9499615743488,
122.475223225858)) ;
#112138 = CARTESIAN_POINT('Ctrl Pts',(-19.9967362767347,-44.9598556817279,
122.358718086467)) ;
#112139 = CARTESIAN_POINT('Ctrl Pts',(-19.8061309975113,-44.9697980139203,
122.273004840585)) ;
#112140 = CARTESIAN_POINT('Ctrl Pts',(-19.6023161030383,-44.9797986402353,
122.221272579548)) ;
#112141 = CARTESIAN_POINT('Ctrl Pts',(-19.3917761637449,-44.9898403745172,
122.20604793693)) ;
#112142 = CARTESIAN_POINT('Ctrl Pts',(-19.1862337746417,-44.9996658004663,
122.226693354258)) ;
#112143 = CARTESIAN_POINT('Ctrl Pts',(-18.982660801087,-45.009722626994,122.283722634516)) ;
#112144 = CARTESIAN_POINT('Ctrl Pts',(-18.7946376983317,-45.0196500601156,
122.374331134874)) ;
#112145 = CARTESIAN_POINT('Ctrl Pts',(-18.6244717451029,-45.0296000525218,
122.495999087954)) ;
#112146 = CARTESIAN_POINT('Ctrl Pts',(-18.4767502039697,-45.0396552535958,
122.647190087996)) ;
#112147 = CARTESIAN_POINT('Ctrl Pts',(-18.3599614367754,-45.0494775276481,
122.817505157329)) ;
#112148 = CARTESIAN_POINT('Ctrl Pts',(-18.2721558928169,-45.0595334216073,
123.009798455244)) ;
#112149 = CARTESIAN_POINT('Ctrl Pts',(-18.2200351252746,-45.0694741434525,
123.212188005796)) ;
#112150 = CARTESIAN_POINT('Ctrl Pts',(-18.2032568014897,-45.079378487539,
123.419735076342)) ;
#112151 = CARTESIAN_POINT('Ctrl Pts',(-18.2231823777921,-45.0894251548385,
123.629987926016)) ;
#112152 = CARTESIAN_POINT('Ctrl Pts',(-18.2782983084812,-45.0993207132885,
123.830624491024)) ;
#112153 = CARTESIAN_POINT('Ctrl Pts',(-18.3688864953703,-45.1093827919931,
124.021749608845)) ;
#112154 = CARTESIAN_POINT('Ctrl Pts',(-18.4885492639764,-45.1192254904589,
124.190592880512)) ;
#112155 = CARTESIAN_POINT('Ctrl Pts',(-18.63753970716,-45.1292162643534,124.338601743866)) ;
#112156 = CARTESIAN_POINT('Ctrl Pts',(-18.8089299927722,-45.1391441335883,
124.457728064916)) ;
#112157 = CARTESIAN_POINT('Ctrl Pts',(-18.9994081551835,-45.1491328625582,
124.546160477723)) ;
#112158 = CARTESIAN_POINT('Ctrl Pts',(-19.2034569695943,-45.1591722645419,
124.600067489495)) ;
#112159 = CARTESIAN_POINT('Ctrl Pts',(-19.4095796875665,-45.1690124322787,
124.617784150228)) ;
#112160 = CARTESIAN_POINT('Ctrl Pts',(-19.6200112606756,-45.1790606426532,
124.599364491927)) ;
#112161 = CARTESIAN_POINT('Ctrl Pts',(-19.8219223505373,-45.189007812941,
124.544913466163)) ;
#112162 = CARTESIAN_POINT('Ctrl Pts',(-20.0108872509035,-45.198918661196,
124.457119601259)) ;
#112163 = CARTESIAN_POINT('Ctrl Pts',(-20.1841161337091,-45.2089749888738,
124.335945859741)) ;
#112164 = CARTESIAN_POINT('Ctrl Pts',(-20.3307537021234,-45.2188254016423,
124.189705699026)) ;
#112165 = CARTESIAN_POINT('Ctrl Pts',(-20.4523163557832,-45.228852287476,
124.01749462699)) ;
#112166 = CARTESIAN_POINT('Ctrl Pts',(-20.5416562719571,-45.2388809031068,
123.826515218872)) ;
#112167 = CARTESIAN_POINT('Ctrl Pts',(-20.5958480104501,-45.2487261264844,
123.626769868609)) ;
#112168 = CARTESIAN_POINT('Ctrl Pts',(-20.6153735248044,-45.2587168085859,
123.417638300358)) ;
#112169 = CARTESIAN_POINT('Ctrl Pts',(-20.5977412690247,-45.2687546972184,
123.20735022135)) ;
#112170 = CARTESIAN_POINT('Ctrl Pts',(-20.545250341206,-45.2785990323215,
123.007150547242)) ;
#112171 = CARTESIAN_POINT('Ctrl Pts',(-20.4579510824147,-45.2885839945191,
122.816280848881)) ;
#112172 = CARTESIAN_POINT('Ctrl Pts',(-20.3394324184313,-45.2985229360524,
122.644161114151)) ;
#112173 = CARTESIAN_POINT('Ctrl Pts',(-20.1912978402225,-45.3085648210239,
122.493775011373)) ;
#112174 = CARTESIAN_POINT('Ctrl Pts',(-20.0220069788937,-45.3184513689321,
122.373155542679)) ;
#112175 = CARTESIAN_POINT('Ctrl Pts',(-19.8324819011337,-45.3284452944321,
122.282532592719)) ;
#112176 = CARTESIAN_POINT('Ctrl Pts',(-19.6312419105329,-45.3383813855586,
122.226409620381)) ;
#112177 = CARTESIAN_POINT('Ctrl Pts',(-19.4214195604293,-45.3484106545385,
122.205936892489)) ;
#112178 = CARTESIAN_POINT('Ctrl Pts',(-19.2142297562444,-45.3582930370979,
122.22170984067)) ;
#112179 = CARTESIAN_POINT('Ctrl Pts',(-19.0095043275591,-45.3683455541857,
122.274021359231)) ;
#112180 = CARTESIAN_POINT('Ctrl Pts',(-18.819898283972,-45.3782396750096,
122.359645278325)) ;
#112181 = CARTESIAN_POINT('Ctrl Pts',(-18.6451474980736,-45.38830165443,122.478801691166)) ;
#112182 = CARTESIAN_POINT('Ctrl Pts',(-18.4969722279792,-45.398146187659,
122.623303507455)) ;
#112183 = CARTESIAN_POINT('Ctrl Pts',(-18.3741143083612,-45.4081062665652,
122.792860727327)) ;
#112184 = CARTESIAN_POINT('Ctrl Pts',(-18.2822203421796,-45.4181445431378,
122.982828320738)) ;
#112185 = CARTESIAN_POINT('Ctrl Pts',(-18.2252578435109,-45.4280179296757,
123.182460809263)) ;
#112186 = CARTESIAN_POINT('Ctrl Pts',(-18.2034592125122,-45.4380908724427,
123.393060369931)) ;
#112187 = CARTESIAN_POINT('Ctrl Pts',(-18.2179355021344,-45.4479122865711,
123.599068980304)) ;
#112188 = CARTESIAN_POINT('Ctrl Pts',(-18.2689853566682,-45.4579869166434,
123.804585741856)) ;
#112189 = CARTESIAN_POINT('Ctrl Pts',(-18.3532746485599,-45.4678535539602,
123.994143613972)) ;
#112190 = CARTESIAN_POINT('Ctrl Pts',(-18.4705716785323,-45.477877099332,
124.169195026815)) ;
#112191 = CARTESIAN_POINT('Ctrl Pts',(-18.616895802998,-45.4879028508492,
124.320918056513)) ;
#112192 = CARTESIAN_POINT('Ctrl Pts',(-18.7841910377941,-45.4977564378586,
124.443065845683)) ;
#112193 = CARTESIAN_POINT('Ctrl Pts',(-18.9722503153279,-45.5077333980865,
124.535960002031)) ;
#112194 = CARTESIAN_POINT('Ctrl Pts',(-19.1745594692366,-45.517754541115,
124.594704097951)) ;
#112195 = CARTESIAN_POINT('Ctrl Pts',(-19.3810923511896,-45.5276371471349,
124.617534072969)) ;
#112196 = CARTESIAN_POINT('Ctrl Pts',(-19.5922833632214,-45.5377056177676,
124.603825651929)) ;
#112197 = CARTESIAN_POINT('Ctrl Pts',(-19.7931427269805,-45.5475357009513,
124.555060379054)) ;
#112198 = CARTESIAN_POINT('Ctrl Pts',(-19.9870853964243,-45.5576022606317,
124.470445781898)) ;
#112199 = CARTESIAN_POINT('Ctrl Pts',(-20.160279325872,-45.5674925104609,
124.355351008496)) ;
#112200 = CARTESIAN_POINT('Ctrl Pts',(-20.3127001853136,-45.5774846762097,
124.21081385571)) ;
#112201 = CARTESIAN_POINT('Ctrl Pts',(-20.4371861738948,-45.5874475198058,
124.042378611189)) ;
#112202 = CARTESIAN_POINT('Ctrl Pts',(-20.5304707678996,-45.5973516886336,
123.856207403373)) ;
#112203 = CARTESIAN_POINT('Ctrl Pts',(-20.590759198916,-45.6074125635279,
123.653499262459)) ;
#112204 = CARTESIAN_POINT('Ctrl Pts',(-20.6146961146888,-45.6172514668573,
123.448011402192)) ;
#112205 = CARTESIAN_POINT('Ctrl Pts',(-20.6025149596037,-45.6273198432312,
123.236727603107)) ;
#112206 = CARTESIAN_POINT('Ctrl Pts',(-20.5546577007811,-45.6372004598639,
123.034562960351)) ;
#112207 = CARTESIAN_POINT('Ctrl Pts',(-20.4719184101995,-45.6471916200928,
122.841533213297)) ;
#112208 = CARTESIAN_POINT('Ctrl Pts',(-20.357352351717,-45.6571446935249,
122.666401434716)) ;
#112209 = CARTESIAN_POINT('Ctrl Pts',(-20.2129098091589,-45.6671805291376,
122.512636284954)) ;
#112210 = CARTESIAN_POINT('Ctrl Pts',(-20.0464767007912,-45.6770706558677,
122.387989837056)) ;
#112211 = CARTESIAN_POINT('Ctrl Pts',(-19.8591882069865,-45.6870628376371,
122.292876253175)) ;
#112212 = CARTESIAN_POINT('Ctrl Pts',(-19.6591290009908,-45.6970087776115,
122.232074381846)) ;
#112213 = CARTESIAN_POINT('Ctrl Pts',(-19.4515660138375,-45.706955961371,
122.20650716541)) ;
#112214 = CARTESIAN_POINT('Ctrl Pts',(-19.2406311624066,-45.7170038996613,
122.217713377264)) ;
#112215 = CARTESIAN_POINT('Ctrl Pts',(-19.0389014767737,-45.7268515344749,
122.264255616678)) ;
#112216 = CARTESIAN_POINT('Ctrl Pts',(-18.8458640438782,-45.7368132481728,
122.345445445744)) ;
#112217 = CARTESIAN_POINT('Ctrl Pts',(-18.6687989747755,-45.746841883994,
122.459919244656)) ;
#112218 = CARTESIAN_POINT('Ctrl Pts',(-18.5160937519667,-45.7567521987458,
122.601640299451)) ;
#112219 = CARTESIAN_POINT('Ctrl Pts',(-18.3895563121381,-45.7666870694084,
122.767816742559)) ;
#112220 = CARTESIAN_POINT('Ctrl Pts',(-18.2929570591405,-45.7767282518102,
122.955504634634)) ;
#112221 = CARTESIAN_POINT('Ctrl Pts',(-18.2312060009898,-45.7866152232749,
123.153993923407)) ;
#112222 = CARTESIAN_POINT('Ctrl Pts',(-18.2042980751124,-45.7966146555375,
123.362456936392)) ;
#112223 = CARTESIAN_POINT('Ctrl Pts',(-18.21377966855,-45.8065347207942,123.570817220911)) ;
#112224 = CARTESIAN_POINT('Ctrl Pts',(-18.2597821274748,-45.8165715733783,
123.776736043751)) ;
#112225 = CARTESIAN_POINT('Ctrl Pts',(-18.3398482828159,-45.8264842327183,
123.969140635487)) ;
#112226 = CARTESIAN_POINT('Ctrl Pts',(-18.4526152021124,-45.8364754446332,
124.146365128544)) ;
#112227 = CARTESIAN_POINT('Ctrl Pts',(-18.5954873427342,-45.8465170860363,
124.301757118765)) ;
#112228 = CARTESIAN_POINT('Ctrl Pts',(-18.7593348076605,-45.8563458802434,
124.427702893936)) ;
#112229 = CARTESIAN_POINT('Ctrl Pts',(-18.9470738947917,-45.8664222913646,
124.525741478292)) ;
#112230 = CARTESIAN_POINT('Ctrl Pts',(-19.1445386518432,-45.8762744244071,
124.588397891619)) ;
#112231 = CARTESIAN_POINT('Ctrl Pts',(-19.3543893205684,-45.8863476587484,
124.616598889941)) ;
#112232 = CARTESIAN_POINT('Ctrl Pts',(-19.5611263751771,-45.896189160075,
124.608074079589)) ;
#112233 = CARTESIAN_POINT('Ctrl Pts',(-19.7658434749185,-45.9061501116698,
124.564019794142)) ;
#112234 = CARTESIAN_POINT('Ctrl Pts',(-19.9611394646978,-45.9161879293905,
124.484088766988)) ;
#112235 = CARTESIAN_POINT('Ctrl Pts',(-20.136916473112,-45.9260622786475,
124.373605742439)) ;
#112236 = CARTESIAN_POINT('Ctrl Pts',(-20.2938331498129,-45.9361318293897,
124.231552775294)) ;
#112237 = CARTESIAN_POINT('Ctrl Pts',(-20.4207867370096,-45.9459658488983,
124.068356470516)) ;
#112238 = CARTESIAN_POINT('Ctrl Pts',(-20.5199207033217,-45.9560000034779,
123.882164647022)) ;
#112239 = CARTESIAN_POINT('Ctrl Pts',(-20.5846122993623,-45.9660159293003,
123.681769059258)) ;
#112240 = CARTESIAN_POINT('Ctrl Pts',(-20.6135083844529,-45.9758981844946,
123.476029223684)) ;
#112241 = CARTESIAN_POINT('Ctrl Pts',(-20.6064248631113,-45.9858869910055,
123.266175738193)) ;
#112242 = CARTESIAN_POINT('Ctrl Pts',(-20.5633304515029,-45.9958355582682,
123.061479842369)) ;
#112243 = CARTESIAN_POINT('Ctrl Pts',(-20.4843277115197,-46.0058903635702,
122.865438884472)) ;
#112244 = CARTESIAN_POINT('Ctrl Pts',(-20.3753478215545,-46.0157091468338,
122.69011798633)) ;
#112245 = CARTESIAN_POINT('Ctrl Pts',(-20.2349691409533,-46.0257449191944,
122.532619318995)) ;
#112246 = CARTESIAN_POINT('Ctrl Pts',(-20.0691759514788,-46.035769618223,
122.402497415323)) ;
#112247 = CARTESIAN_POINT('Ctrl Pts',(-19.886729763957,-46.0456216214821,
122.304449399509)) ;
#112248 = CARTESIAN_POINT('Ctrl Pts',(-19.6873843122432,-46.0556125558793,
122.238359374228)) ;
#112249 = CARTESIAN_POINT('Ctrl Pts',(-19.4810798142807,-46.0655304783104,
122.20796586497)) ;
#112250 = CARTESIAN_POINT('Ctrl Pts',(-19.2703526256733,-46.0755588339928,
122.213873496241)) ;
#112251 = CARTESIAN_POINT('Ctrl Pts',(-19.0667741821998,-46.0854431185033,
122.255577117318)) ;
#112252 = CARTESIAN_POINT('Ctrl Pts',(-18.871242160211,-46.0954358024112,
122.332388452974)) ;
#112253 = CARTESIAN_POINT('Ctrl Pts',(-18.6915622061126,-46.1054645394189,
122.442695083021)) ;
#112254 = CARTESIAN_POINT('Ctrl Pts',(-18.5358336205684,-46.1153499360478,
122.580323768878)) ;
#112255 = CARTESIAN_POINT('Ctrl Pts',(-18.4048087210755,-46.1253378214617,
122.744378200816)) ;
#112256 = CARTESIAN_POINT('Ctrl Pts',(-18.3045250816927,-46.1352885241223,
122.928003704835)) ;
#112257 = CARTESIAN_POINT('Ctrl Pts',(-18.2371710361434,-46.1453288422197,
123.128025652158)) ;
#112258 = CARTESIAN_POINT('Ctrl Pts',(-18.2058821670197,-46.155203407553,
123.33327213757)) ;
#112259 = CARTESIAN_POINT('Ctrl Pts',(-18.2104984624826,-46.165203067614,
123.543411466745)) ;
#112260 = CARTESIAN_POINT('Ctrl Pts',(-18.2509769537846,-46.1751120627818,
123.747796649027)) ;
#112261 = CARTESIAN_POINT('Ctrl Pts',(-18.3274733133207,-46.185166803945,
123.944815348873)) ;
#112262 = CARTESIAN_POINT('Ctrl Pts',(-18.4347110927751,-46.1950254158588,
124.122217182559)) ;
#112263 = CARTESIAN_POINT('Ctrl Pts',(-18.5738806058935,-46.2050935381382,
124.281654659473)) ;
#112264 = CARTESIAN_POINT('Ctrl Pts',(-18.7351876418152,-46.2149490088413,
124.411716817521)) ;
#112265 = CARTESIAN_POINT('Ctrl Pts',(-18.9188672875366,-46.2249438683347,
124.513749765115)) ;
#112266 = CARTESIAN_POINT('Ctrl Pts',(-19.1183548553274,-46.2349751216766,
124.58216450119)) ;
#112267 = CARTESIAN_POINT('Ctrl Pts',(-19.3232243383772,-46.2448418205497,
124.614690139671)) ;
#112268 = CARTESIAN_POINT('Ctrl Pts',(-19.533130267108,-46.2548286363009,
124.611452413315)) ;
#112269 = CARTESIAN_POINT('Ctrl Pts',(-19.738536473541,-46.2647758414964,
124.572058893479)) ;
#112270 = CARTESIAN_POINT('Ctrl Pts',(-19.9357908805247,-46.2748188296227,
124.496809754335)) ;
#112271 = CARTESIAN_POINT('Ctrl Pts',(-20.113896523159,-46.2846861842441,
124.390442924641)) ;
#112272 = CARTESIAN_POINT('Ctrl Pts',(-20.2727519268867,-46.2946520775422,
124.253850194985)) ;
#112273 = CARTESIAN_POINT('Ctrl Pts',(-20.4060931571765,-46.3046758549183,
124.090652810968)) ;
#112274 = CARTESIAN_POINT('Ctrl Pts',(-20.5080934186025,-46.31460140285,123.908627308799)) ;
#112275 = CARTESIAN_POINT('Ctrl Pts',(-20.577515911766,-46.324541879271,123.711501911497)) ;
#112276 = CARTESIAN_POINT('Ctrl Pts',(-20.6117775963673,-46.3345880889339,
123.503109211031)) ;
#112277 = CARTESIAN_POINT('Ctrl Pts',(-20.6096017321849,-46.3444493455957,
123.295787784314)) ;
#112278 = CARTESIAN_POINT('Ctrl Pts',(-20.5713127397986,-46.354442973871,
123.089239564761)) ;
#112279 = CARTESIAN_POINT('Ctrl Pts',(-20.498324765104,-46.3643683711812,
122.893724466756)) ;
#112280 = CARTESIAN_POINT('Ctrl Pts',(-20.3914394880559,-46.3743962790915,
122.712042393839)) ;
#112281 = CARTESIAN_POINT('Ctrl Pts',(-20.256689239832,-46.3842825947606,
122.553760347426)) ;
#112282 = CARTESIAN_POINT('Ctrl Pts',(-20.0942706479515,-46.3943141896644,
122.41928726284)) ;
#112283 = CARTESIAN_POINT('Ctrl Pts',(-19.9137355290625,-46.4041964326161,
122.316410590995)) ;
#112284 = CARTESIAN_POINT('Ctrl Pts',(-19.7146556451297,-46.414255903646,
122.245124204062)) ;
#112285 = CARTESIAN_POINT('Ctrl Pts',(-19.5101827941688,-46.4241223483091,
122.210192911167)) ;
#112286 = CARTESIAN_POINT('Ctrl Pts',(-19.300669239508,-46.4340884727578,
122.210645334395)) ;
#112287 = CARTESIAN_POINT('Ctrl Pts',(-19.0931462837476,-46.444118716149,
122.248040115787)) ;
#112288 = CARTESIAN_POINT('Ctrl Pts',(-18.8978525388153,-46.454011751102,
122.319631950706)) ;
#112289 = CARTESIAN_POINT('Ctrl Pts',(-18.7150886406695,-46.4640626653389,
122.425644026029)) ;
#112290 = CARTESIAN_POINT('Ctrl Pts',(-18.5560646605381,-46.4739524915634,
122.559594432222)) ;
#112291 = CARTESIAN_POINT('Ctrl Pts',(-18.3758141645687,-46.4872873066104,
122.774360823759)) ;
#112292 = CARTESIAN_POINT('Ctrl Pts',(-18.2567586677251,-46.5005643977818,
123.030323044475)) ;
#112293 = CARTESIAN_POINT('Ctrl Pts',(-18.2080003376662,-46.5138126863801,
123.304527883005)) ;
#112294 = CARTESIAN_POINT('Ctrl Pts',(-18.2078269549903,-46.5238675278742,
123.515888932731)) ;
#112295 = CARTESIAN_POINT('Ctrl Pts',(-18.2432089965828,-46.5336985171818,
123.71955079902)) ;
#112296 = CARTESIAN_POINT('Ctrl Pts',(-18.3149991934965,-46.543775081505,
123.9188202)) ;
#112297 = CARTESIAN_POINT('Ctrl Pts',(-18.4179520511202,-46.5536244066389,
124.098495528479)) ;
#112298 = CARTESIAN_POINT('Ctrl Pts',(-18.5971286629228,-46.5669724062762,
124.314512720931)) ;
#112299 = CARTESIAN_POINT('Ctrl Pts',(-18.8850046434392,-46.5835571658128,
124.518066925778)) ;
#112300 = CARTESIAN_POINT('Ctrl Pts',(-19.2246076001695,-46.6001257171609,
124.611949255393)) ;
#112301 = CARTESIAN_POINT('Ctrl Pts',(-19.505438469017,-46.6134855419799,
124.613976513588)) ;
#112302 = CARTESIAN_POINT('Ctrl Pts',(-19.7108170957817,-46.6233909508105,
124.579464047361)) ;
#112303 = CARTESIAN_POINT('Ctrl Pts',(-19.9082275521811,-46.6333509773946,
124.509731266276)) ;
#112304 = CARTESIAN_POINT('Ctrl Pts',(-20.151134320981,-46.6466085615799,
124.372969265967)) ;
#112305 = CARTESIAN_POINT('Ctrl Pts',(-20.4042796970229,-46.6632597730745,
124.125469202742)) ;
#112306 = CARTESIAN_POINT('Ctrl Pts',(-20.5876345968214,-46.6831779871848,
123.743721464506)) ;
#112307 = CARTESIAN_POINT('Ctrl Pts',(-20.6305357814613,-46.7030557504057,
123.323189204303)) ;
#112308 = CARTESIAN_POINT('Ctrl Pts',(-20.5263194692478,-46.7230684181928,
122.910705134848)) ;
#112309 = CARTESIAN_POINT('Ctrl Pts',(-20.2902264123703,-46.7428809408594,
122.561714812587)) ;
#112310 = CARTESIAN_POINT('Ctrl Pts',(-19.946800266929,-46.7628642408593,
122.311660401265)) ;
#112311 = CARTESIAN_POINT('Ctrl Pts',(-19.5402506810294,-46.7827585179606,
122.194589328653)) ;
#112312 = CARTESIAN_POINT('Ctrl Pts',(-19.1173686987748,-46.8026912797184,
122.222669030425)) ;
#112313 = CARTESIAN_POINT('Ctrl Pts',(-18.7289139334426,-46.8226572854831,
122.393931904574)) ;
#112314 = CARTESIAN_POINT('Ctrl Pts',(-18.4233337697194,-46.842535817648,
122.685985428324)) ;
#112315 = CARTESIAN_POINT('Ctrl Pts',(-18.2348504446286,-46.8624754843083,
123.06570710446)) ;
#112316 = CARTESIAN_POINT('Ctrl Pts',(-18.1872341898074,-46.8823703589537,
123.486082371583)) ;
#112317 = CARTESIAN_POINT('Ctrl Pts',(-18.2855495501073,-46.902277498247,
123.897686387017)) ;
#112318 = CARTESIAN_POINT('Ctrl Pts',(-18.5179844798223,-46.9221880463255,
124.251688406246)) ;
#112319 = CARTESIAN_POINT('Ctrl Pts',(-18.8603589045177,-46.9422566316827,
124.506213322785)) ;
#112320 = CARTESIAN_POINT('Ctrl Pts',(-19.263297363643,-46.9620384289975,
124.627349310008)) ;
#112321 = CARTESIAN_POINT('Ctrl Pts',(-19.6879081938475,-46.982045975942,
124.604082007723)) ;
#112322 = CARTESIAN_POINT('Ctrl Pts',(-20.0757232899352,-47.0018677142448,
124.438770166374)) ;
#112323 = CARTESIAN_POINT('Ctrl Pts',(-20.3867048793228,-47.021847734149,
124.149429935307)) ;
#112324 = CARTESIAN_POINT('Ctrl Pts',(-20.579219557561,-47.0417651854112,
123.772199439542)) ;
#112325 = CARTESIAN_POINT('Ctrl Pts',(-20.6323196594387,-47.0616401065839,
123.352926287067)) ;
#112326 = CARTESIAN_POINT('Ctrl Pts',(-20.5382000199075,-47.0816644751348,
122.937716026895)) ;
#112327 = CARTESIAN_POINT('Ctrl Pts',(-20.3096969385905,-47.1015311595082,
122.582353383261)) ;
#112328 = CARTESIAN_POINT('Ctrl Pts',(-19.9728434364968,-47.1214749813544,
122.324834830175)) ;
#112329 = CARTESIAN_POINT('Ctrl Pts',(-19.5689826518041,-47.141382350606,
122.198075391916)) ;
#112330 = CARTESIAN_POINT('Ctrl Pts',(-19.1467740833316,-47.1612570483527,
122.215922873727)) ;
#112331 = CARTESIAN_POINT('Ctrl Pts',(-18.753824803381,-47.1812389908744,
122.377559763358)) ;
#112332 = CARTESIAN_POINT('Ctrl Pts',(-18.4411591482481,-47.2011416577852,
122.662668237289)) ;
#112333 = CARTESIAN_POINT('Ctrl Pts',(-18.2438659642917,-47.2209970153239,
123.035980851795)) ;
#112334 = CARTESIAN_POINT('Ctrl Pts',(-18.1856871451721,-47.2410610540399,
123.458543778335)) ;
#112335 = CARTESIAN_POINT('Ctrl Pts',(-18.2744811982601,-47.260916233765,
123.871435782825)) ;
#112336 = CARTESIAN_POINT('Ctrl Pts',(-18.4997986820405,-47.2808963384294,
124.23140012887)) ;
#112337 = CARTESIAN_POINT('Ctrl Pts',(-18.8314729834885,-47.3007054435992,
124.491205586576)) ;
#112338 = CARTESIAN_POINT('Ctrl Pts',(-19.2352356788639,-47.3206980639399,
124.623773316543)) ;
#112339 = CARTESIAN_POINT('Ctrl Pts',(-19.5868211815082,-47.337237546444,
124.612937929343)) ;
#112340 = CARTESIAN_POINT('Ctrl Pts',(-19.8558775477887,-47.3506018645082,
124.532060972348)) ;
#112341 = CARTESIAN_POINT('Ctrl Pts',(-20.104215075308,-47.3638194670097,
124.407379079751)) ;
#112342 = CARTESIAN_POINT('Ctrl Pts',(-20.3689671537126,-47.3804770612875,
124.172152277024)) ;
#112343 = CARTESIAN_POINT('Ctrl Pts',(-20.5701609304998,-47.4003427633293,
123.800669027524)) ;
#112344 = CARTESIAN_POINT('Ctrl Pts',(-20.6228296445874,-47.4169724900193,
123.45111703364)) ;
#112345 = CARTESIAN_POINT('Ctrl Pts',(-20.5914417493191,-47.4302616051571,
123.173432206332)) ;
#112346 = CARTESIAN_POINT('Ctrl Pts',(-20.5323650698409,-47.4402259521342,
122.972473478572)) ;
#112347 = CARTESIAN_POINT('Ctrl Pts',(-20.4397431155912,-47.4501543201357,
122.785421120555)) ;
#112348 = CARTESIAN_POINT('Ctrl Pts',(-20.2747113607622,-47.4634377532245,
122.560165348541)) ;
#112349 = CARTESIAN_POINT('Ctrl Pts',(-19.9984875586522,-47.4800898309648,
122.338584385767)) ;
#112350 = CARTESIAN_POINT('Ctrl Pts',(-19.6654140137925,-47.4966412002656,
122.225127778742)) ;
#112351 = CARTESIAN_POINT('Ctrl Pts',(-19.3866765503919,-47.5099286284146,
122.205972916037)) ;
#112352 = CARTESIAN_POINT('Ctrl Pts',(-19.1767345637303,-47.5199731681147,
122.228509751238)) ;
#112353 = CARTESIAN_POINT('Ctrl Pts',(-18.9778647497344,-47.5298160099385,
122.285740753146)) ;
#112354 = CARTESIAN_POINT('Ctrl Pts',(-18.7891005316615,-47.5398002941855,
122.377489070515)) ;
#112355 = CARTESIAN_POINT('Ctrl Pts',(-18.6197243887218,-47.5497499395846,
122.500245250624)) ;
#112356 = CARTESIAN_POINT('Ctrl Pts',(-18.4733160403355,-47.559749701273,
122.651124926742)) ;
#112357 = CARTESIAN_POINT('Ctrl Pts',(-18.3552528574441,-47.5697810472319,
122.825866939157)) ;
#112358 = CARTESIAN_POINT('Ctrl Pts',(-18.2705550913228,-47.5796360017091,
123.014949882465)) ;
#112359 = CARTESIAN_POINT('Ctrl Pts',(-18.2189034005309,-47.5896085397096,
123.218119575981)) ;
#112360 = CARTESIAN_POINT('Ctrl Pts',(-18.2032894718372,-47.5996035334445,
123.427697294973)) ;
#112361 = CARTESIAN_POINT('Ctrl Pts',(-18.2246368504535,-47.6096375922386,
123.637543773587)) ;
#112362 = CARTESIAN_POINT('Ctrl Pts',(-18.2807655836226,-47.6194929350616,
123.837007913932)) ;
#112363 = CARTESIAN_POINT('Ctrl Pts',(-18.3717098635288,-47.6294924144072,
124.026496797301)) ;
#112364 = CARTESIAN_POINT('Ctrl Pts',(-18.4927398425373,-47.6393868631625,
124.195722227869)) ;
#112365 = CARTESIAN_POINT('Ctrl Pts',(-18.6438364368498,-47.649449982597,
124.343747132124)) ;
#112366 = CARTESIAN_POINT('Ctrl Pts',(-18.8143933446472,-47.6592896278382,
124.460861138169)) ;
#112367 = CARTESIAN_POINT('Ctrl Pts',(-19.0068017942194,-47.6693527920243,
124.548747506202)) ;
#112368 = CARTESIAN_POINT('Ctrl Pts',(-19.2082058747896,-47.6792470617731,
124.600841677437)) ;
#112369 = CARTESIAN_POINT('Ctrl Pts',(-19.4164943987263,-47.689188787787,
124.617812118174)) ;
#112370 = CARTESIAN_POINT('Ctrl Pts',(-19.6259144085407,-47.6991916764463,
124.598324257875)) ;
#112371 = CARTESIAN_POINT('Ctrl Pts',(-19.8293661695385,-47.7092315252403,
124.542206315651)) ;
#112372 = CARTESIAN_POINT('Ctrl Pts',(-20.0161233883961,-47.7190557407012,
124.453969603024)) ;
#112373 = CARTESIAN_POINT('Ctrl Pts',(-20.1888586248246,-47.7291125841947,
124.332080413821)) ;
#112374 = CARTESIAN_POINT('Ctrl Pts',(-20.3357293835601,-47.7390411935907,
124.183752074677)) ;
#112375 = CARTESIAN_POINT('Ctrl Pts',(-20.4553755209974,-47.7489930776286,
124.012109234267)) ;
#112376 = CARTESIAN_POINT('Ctrl Pts',(-20.5439400727336,-47.7590460304362,
123.82023183912)) ;
#112377 = CARTESIAN_POINT('Ctrl Pts',(-20.5969890506143,-47.7688689069024,
123.620638287797)) ;
#112378 = CARTESIAN_POINT('Ctrl Pts',(-20.6153607625257,-47.7789246394725,
123.410049220734)) ;
#112379 = CARTESIAN_POINT('Ctrl Pts',(-20.5967291539221,-47.7888654044602,
123.201887600154)) ;
#112380 = CARTESIAN_POINT('Ctrl Pts',(-20.5430668298858,-47.7987697373658,
123.000697166747)) ;
#112381 = CARTESIAN_POINT('Ctrl Pts',(-20.4539124372812,-47.8088164062465,
122.809242773058)) ;
#112382 = CARTESIAN_POINT('Ctrl Pts',(-20.3348163697857,-47.8187119695523,
122.638629251295)) ;
#112383 = CARTESIAN_POINT('Ctrl Pts',(-20.1854787174004,-47.8287740272526,
122.488852479566)) ;
#112384 = CARTESIAN_POINT('Ctrl Pts',(-20.0161998927408,-47.8386168048801,
122.369803227324)) ;
#112385 = CARTESIAN_POINT('Ctrl Pts',(-19.8262675220778,-47.848607283132,
122.280207740246)) ;
#112386 = CARTESIAN_POINT('Ctrl Pts',(-19.6248641321868,-47.8585362557755,
122.225310490238)) ;
#112387 = CARTESIAN_POINT('Ctrl Pts',(-19.4157282479092,-47.8685273926551,
122.205773209419)) ;
#112388 = CARTESIAN_POINT('Ctrl Pts',(-19.2057461496962,-47.878549510144,
122.223152218182)) ;
#112389 = CARTESIAN_POINT('Ctrl Pts',(-19.0043951364117,-47.8884500205462,
122.275886363127)) ;
#112390 = CARTESIAN_POINT('Ctrl Pts',(-18.8134346663008,-47.8984390132923,
122.363257528798)) ;
#112391 = CARTESIAN_POINT('Ctrl Pts',(-18.6410453546976,-47.9084042573429,
122.482290756221)) ;
#112392 = CARTESIAN_POINT('Ctrl Pts',(-18.49249309703,-47.9183085218561,122.628215087707)) ;
#112393 = CARTESIAN_POINT('Ctrl Pts',(-18.3697845447552,-47.9283666135544,
122.800399383047)) ;
#112394 = CARTESIAN_POINT('Ctrl Pts',(-18.2805661816345,-47.9382165539828,
122.987283582192)) ;
#112395 = CARTESIAN_POINT('Ctrl Pts',(-18.2236581707164,-47.9482435651563,
123.190252380736)) ;
#112396 = CARTESIAN_POINT('Ctrl Pts',(-18.2033996012696,-47.9582721517683,
123.40011948226)) ;
#112397 = CARTESIAN_POINT('Ctrl Pts',(-18.2191945852685,-47.968117365881,
123.606481902007)) ;
#112398 = CARTESIAN_POINT('Ctrl Pts',(-18.2707998651141,-47.9781081140606,
123.810085495265)) ;
#112399 = CARTESIAN_POINT('Ctrl Pts',(-18.3577998921847,-47.9881457476461,
124.002339511984)) ;
#112400 = CARTESIAN_POINT('Ctrl Pts',(-18.474295379249,-47.9979910368589,
124.173424409346)) ;
#112401 = CARTESIAN_POINT('Ctrl Pts',(-18.6203765194803,-48.0079724376648,
124.324045059621)) ;
#112402 = CARTESIAN_POINT('Ctrl Pts',(-18.7899419953663,-48.0179246706548,
124.44662572462)) ;
#112403 = CARTESIAN_POINT('Ctrl Pts',(-18.9789868238322,-48.0279234821114,
124.538580251259)) ;
#112404 = CARTESIAN_POINT('Ctrl Pts',(-19.1820247834595,-48.0379625860421,
124.596148012077)) ;
#112405 = CARTESIAN_POINT('Ctrl Pts',(-19.3874736460319,-48.0477875284614,
124.617574034173)) ;
#112406 = CARTESIAN_POINT('Ctrl Pts',(-19.5983397427853,-48.0578422159373,
124.603009673274)) ;
#112407 = CARTESIAN_POINT('Ctrl Pts',(-19.8011230555925,-48.0677850182941,
124.552268930693)) ;
#112408 = CARTESIAN_POINT('Ctrl Pts',(-19.9915243649244,-48.0776888142339,
124.468007698445)) ;
#112409 = CARTESIAN_POINT('Ctrl Pts',(-20.1668107754577,-48.0877355936089,
124.350197826916)) ;
#112410 = CARTESIAN_POINT('Ctrl Pts',(-20.3168498677824,-48.0976312519035,
124.206042834238)) ;
#112411 = CARTESIAN_POINT('Ctrl Pts',(-20.4416259074893,-48.1076928191541,
124.035266364549)) ;
#112412 = CARTESIAN_POINT('Ctrl Pts',(-20.5328863657658,-48.1175374635914,
123.849501135341)) ;
#112413 = CARTESIAN_POINT('Ctrl Pts',(-20.5919002625934,-48.1274975098341,
123.6486007418)) ;
#112414 = CARTESIAN_POINT('Ctrl Pts',(-20.6149049730474,-48.1375358058525,
123.438831697536)) ;
#112415 = CARTESIAN_POINT('Ctrl Pts',(-20.6017587262513,-48.1474091472708,
123.231648825688)) ;
#112416 = CARTESIAN_POINT('Ctrl Pts',(-20.5518031750003,-48.1574822510701,
123.025898872531)) ;
#112417 = CARTESIAN_POINT('Ctrl Pts',(-20.4692130010252,-48.167303066189,
122.836629061271)) ;
#112418 = CARTESIAN_POINT('Ctrl Pts',(-20.3522826566052,-48.177379931267,
122.660021565818)) ;
#112419 = CARTESIAN_POINT('Ctrl Pts',(-20.2094321897144,-48.1872446709223,
122.509642753544)) ;
#112420 = CARTESIAN_POINT('Ctrl Pts',(-20.0403305661027,-48.1972670741636,
122.383957778473)) ;
#112421 = CARTESIAN_POINT('Ctrl Pts',(-19.8516573689572,-48.2072927984521,
122.289974681153)) ;
#112422 = CARTESIAN_POINT('Ctrl Pts',(-19.6531061690027,-48.2171475814734,
122.230855837251)) ;
#112423 = CARTESIAN_POINT('Ctrl Pts',(-19.4447607021445,-48.2271264251967,
122.2062657623)) ;
#112424 = CARTESIAN_POINT('Ctrl Pts',(-19.2345057398771,-48.2371453174333,
122.218635130679)) ;
#112425 = CARTESIAN_POINT('Ctrl Pts',(-19.0322324679663,-48.2470285264743,
122.266253824616)) ;
#112426 = CARTESIAN_POINT('Ctrl Pts',(-18.8378163793331,-48.2570968358145,
122.349864205604)) ;
#112427 = CARTESIAN_POINT('Ctrl Pts',(-18.6648662737018,-48.2669269611472,
122.463050279867)) ;
#112428 = CARTESIAN_POINT('Ctrl Pts',(-18.5104349871933,-48.2769935135242,
122.607702642203)) ;
#112429 = CARTESIAN_POINT('Ctrl Pts',(-18.3857576576127,-48.2868837504179,
122.774131230521)) ;
#112430 = CARTESIAN_POINT('Ctrl Pts',(-18.2905113390233,-48.2968759752119,
122.961351689572)) ;
#112431 = CARTESIAN_POINT('Ctrl Pts',(-18.2295845575195,-48.3068385955629,
123.16173602059)) ;
#112432 = CARTESIAN_POINT('Ctrl Pts',(-18.2040083715551,-48.316743598326,
123.368407475898)) ;
#112433 = CARTESIAN_POINT('Ctrl Pts',(-18.2150144272805,-48.3268013607242,
123.579548413525)) ;
#112434 = CARTESIAN_POINT('Ctrl Pts',(-18.2613768489998,-48.336651880103,
123.78139681908)) ;
#112435 = CARTESIAN_POINT('Ctrl Pts',(-18.3431276815469,-48.3466834571011,
123.975788097822)) ;
#112436 = CARTESIAN_POINT('Ctrl Pts',(-18.4575011644632,-48.3566931922061,
124.152456872072)) ;
#112437 = CARTESIAN_POINT('Ctrl Pts',(-18.5992160450194,-48.3666027688323,
124.305135751122)) ;
#112438 = CARTESIAN_POINT('Ctrl Pts',(-18.7652852593955,-48.376530154689,
124.431557757183)) ;
#112439 = CARTESIAN_POINT('Ctrl Pts',(-18.9530418886853,-48.3865750891793,
124.528196388258)) ;
#112440 = CARTESIAN_POINT('Ctrl Pts',(-19.1515170844124,-48.3964610213672,
124.589900081657)) ;
#112441 = CARTESIAN_POINT('Ctrl Pts',(-19.359860552196,-48.4064543273203,
124.616846676175)) ;
#112442 = CARTESIAN_POINT('Ctrl Pts',(-19.5687256031965,-48.4163999651021,
124.60717192265)) ;
#112443 = CARTESIAN_POINT('Ctrl Pts',(-19.7728746826063,-48.426347233448,
124.561787035575)) ;
#112444 = CARTESIAN_POINT('Ctrl Pts',(-19.9678899803052,-48.4363951355851,
124.480620742549)) ;
#112445 = CARTESIAN_POINT('Ctrl Pts',(-20.1424033442942,-48.4462428304253,
124.369236951358)) ;
#112446 = CARTESIAN_POINT('Ctrl Pts',(-20.2971288806409,-48.4562043401698,
124.228119074902)) ;
#112447 = CARTESIAN_POINT('Ctrl Pts',(-20.4256593250759,-48.4662337317786,
124.060963954446)) ;
#112448 = CARTESIAN_POINT('Ctrl Pts',(-20.5221256411427,-48.4761412273334,
123.876361251367)) ;
#112449 = CARTESIAN_POINT('Ctrl Pts',(-20.5857065959764,-48.4860866189964,
123.677197446102)) ;
#112450 = CARTESIAN_POINT('Ctrl Pts',(-20.6140292647029,-48.4960885365937,
123.46881313064)) ;
#112451 = CARTESIAN_POINT('Ctrl Pts',(-20.6053201167629,-48.5061286041459,
123.257938221129)) ;
#112452 = CARTESIAN_POINT('Ctrl Pts',(-20.5615508444086,-48.5159529155857,
123.056074010608)) ;
#112453 = CARTESIAN_POINT('Ctrl Pts',(-20.481835069034,-48.5260091567418,
122.860287259344)) ;
#112454 = CARTESIAN_POINT('Ctrl Pts',(-20.3705060228585,-48.5359400784775,
122.683639640191)) ;
#112455 = CARTESIAN_POINT('Ctrl Pts',(-20.2303723823661,-48.5458833145537,
122.528564560664)) ;
#112456 = CARTESIAN_POINT('Ctrl Pts',(-20.0648880313581,-48.5558645985662,
122.399490085288)) ;
#112457 = CARTESIAN_POINT('Ctrl Pts',(-19.8782162210794,-48.5659089001918,
122.300837790204)) ;
#112458 = CARTESIAN_POINT('Ctrl Pts',(-19.6816696818352,-48.5757369814113,
122.237015270821)) ;
#112459 = CARTESIAN_POINT('Ctrl Pts',(-19.4719420530272,-48.5858135842604,
122.20747100423)) ;
#112460 = CARTESIAN_POINT('Ctrl Pts',(-19.2648957958491,-48.595665663379,
122.214527639684)) ;
#112461 = CARTESIAN_POINT('Ctrl Pts',(-19.0577107266058,-48.6057389216879,
122.258197125633)) ;
#112462 = CARTESIAN_POINT('Ctrl Pts',(-18.8657533990305,-48.6155803810682,
122.335430927247)) ;
#112463 = CARTESIAN_POINT('Ctrl Pts',(-18.687591301979,-48.6255414764805,
122.445472119578)) ;
#112464 = CARTESIAN_POINT('Ctrl Pts',(-18.5303196765728,-48.6355787608773,
122.586153051913)) ;
#112465 = CARTESIAN_POINT('Ctrl Pts',(-18.4016538429066,-48.6454550996125,
122.74914168273)) ;
#112466 = CARTESIAN_POINT('Ctrl Pts',(-18.3013798056818,-48.6555172257658,
122.935372725944)) ;
#112467 = CARTESIAN_POINT('Ctrl Pts',(-18.2361811364486,-48.6653853997423,
123.132347569418)) ;
#112468 = CARTESIAN_POINT('Ctrl Pts',(-18.2053436827784,-48.6753909482461,
123.340394829146)) ;
#112469 = CARTESIAN_POINT('Ctrl Pts',(-18.2111591489872,-48.6853735801417,
123.550218979142)) ;
#112470 = CARTESIAN_POINT('Ctrl Pts',(-18.2537815324817,-48.6954175225635,
123.75700992454)) ;
#112471 = CARTESIAN_POINT('Ctrl Pts',(-18.3297375461676,-48.7052456705907,
123.949160200971)) ;
#112472 = CARTESIAN_POINT('Ctrl Pts',(-18.4391089400008,-48.7152355379651,
124.12845313594)) ;
#112473 = CARTESIAN_POINT('Ctrl Pts',(-18.5791098640398,-48.7252792769206,
124.28651794592)) ;
#112474 = CARTESIAN_POINT('Ctrl Pts',(-18.7405061367694,-48.7351010254585,
124.415305754142)) ;
#112475 = CARTESIAN_POINT('Ctrl Pts',(-18.9255019617217,-48.7451360030682,
124.516713676706)) ;
#112476 = CARTESIAN_POINT('Ctrl Pts',(-19.1252883280624,-48.7551609158259,
124.583837298046)) ;
#112477 = CARTESIAN_POINT('Ctrl Pts',(-19.3300292339202,-48.7650128589198,
124.615157613263)) ;
#112478 = CARTESIAN_POINT('Ctrl Pts',(-19.5399978111561,-48.7750038202489,
124.610707975462)) ;
#112479 = CARTESIAN_POINT('Ctrl Pts',(-19.7445743811808,-48.7849216951173,
124.570292129443)) ;
#112480 = CARTESIAN_POINT('Ctrl Pts',(-19.9411701344729,-48.7949502141185,
124.494185553889)) ;
#112481 = CARTESIAN_POINT('Ctrl Pts',(-20.1190372380851,-48.8048338929164,
124.38675338542)) ;
#112482 = CARTESIAN_POINT('Ctrl Pts',(-20.277608582612,-48.8148288363561,
124.248885257726)) ;
#112483 = CARTESIAN_POINT('Ctrl Pts',(-20.4099744103347,-48.8248556901785,
124.084828091915)) ;
#112484 = CARTESIAN_POINT('Ctrl Pts',(-20.5106480738825,-48.8347398545175,
123.903037980162)) ;
#112485 = CARTESIAN_POINT('Ctrl Pts',(-20.5791926570833,-48.8447279525599,
123.704581133387)) ;
#112486 = CARTESIAN_POINT('Ctrl Pts',(-20.6122374714526,-48.8546790590169,
123.49797735337)) ;
#112487 = CARTESIAN_POINT('Ctrl Pts',(-20.6087584533805,-48.864724110185,
123.286839559356)) ;
#112488 = CARTESIAN_POINT('Ctrl Pts',(-20.5695137034719,-48.8745858705433,
123.083261633698)) ;
#112489 = CARTESIAN_POINT('Ctrl Pts',(-20.4953630075865,-48.8845486873738,
122.887375702559)) ;
#112490 = CARTESIAN_POINT('Ctrl Pts',(-20.3872484320562,-48.8945833686545,
122.706235677299)) ;
#112491 = CARTESIAN_POINT('Ctrl Pts',(-20.2516256994326,-48.9044683984353,
122.548739117609)) ;
#112492 = CARTESIAN_POINT('Ctrl Pts',(-20.0877956177476,-48.9145339918333,
122.414857497145)) ;
#112493 = CARTESIAN_POINT('Ctrl Pts',(-19.9074048588428,-48.9243731601948,
122.313567884926)) ;
#112494 = CARTESIAN_POINT('Ctrl Pts',(-19.7078843640748,-48.9344357579363,
122.243329292492)) ;
#112495 = CARTESIAN_POINT('Ctrl Pts',(-19.502560422072,-48.9443327703432,
122.209583343813)) ;
#112496 = CARTESIAN_POINT('Ctrl Pts',(-19.2937846243021,-48.9542640921688,
122.211313963836)) ;
#112497 = CARTESIAN_POINT('Ctrl Pts',(-19.0862372956741,-48.9643058549233,
122.249916130738)) ;
#112498 = CARTESIAN_POINT('Ctrl Pts',(-18.8915024825037,-48.974194053814,
122.322702656119)) ;
#112499 = CARTESIAN_POINT('Ctrl Pts',(-18.7103041550708,-48.9841879924139,
122.429022288737)) ;
#112500 = CARTESIAN_POINT('Ctrl Pts',(-18.5511551114689,-48.9941288134508,
122.564495155954)) ;
#112501 = CARTESIAN_POINT('Ctrl Pts',(-18.417508038418,-49.004088195739,122.725655359385)) ;
#112502 = CARTESIAN_POINT('Ctrl Pts',(-18.3133483409578,-49.0140859553913,
122.908239426834)) ;
#112503 = CARTESIAN_POINT('Ctrl Pts',(-18.2424839484345,-49.0241220915936,
123.106968613935)) ;
#112504 = CARTESIAN_POINT('Ctrl Pts',(-18.2076123164538,-49.0339728890845,
123.311104572595)) ;
#112505 = CARTESIAN_POINT('Ctrl Pts',(-18.208104001698,-49.0439337541608,
123.520505414161)) ;
#112506 = CARTESIAN_POINT('Ctrl Pts',(-18.2454532427305,-49.0539626217912,
123.728021428883)) ;
#112507 = CARTESIAN_POINT('Ctrl Pts',(-18.3173380129022,-49.0638728579276,
123.923562596765)) ;
#112508 = CARTESIAN_POINT('Ctrl Pts',(-18.4218784036675,-49.0738078112422,
124.104388376332)) ;
#112509 = CARTESIAN_POINT('Ctrl Pts',(-18.5578017840032,-49.0838487416517,
124.265889304236)) ;
#112510 = CARTESIAN_POINT('Ctrl Pts',(-18.7171595894999,-49.0937366384333,
124.399382355885)) ;
#112511 = CARTESIAN_POINT('Ctrl Pts',(-18.8989187555445,-49.103726090092,
124.504575833043)) ;
#112512 = CARTESIAN_POINT('Ctrl Pts',(-19.0956385312897,-49.1136851804574,
124.576235307926)) ;
#112513 = CARTESIAN_POINT('Ctrl Pts',(-19.3004601226159,-49.1235824927637,
124.612950417777)) ;
#112514 = CARTESIAN_POINT('Ctrl Pts',(-19.5118599483828,-49.133638918664,
124.613452938736)) ;
#112515 = CARTESIAN_POINT('Ctrl Pts',(-19.7163289331552,-49.1435089212537,
124.578011247484)) ;
#112516 = CARTESIAN_POINT('Ctrl Pts',(-19.9142897379415,-49.1535128544309,
124.507058726721)) ;
#112517 = CARTESIAN_POINT('Ctrl Pts',(-20.096612158011,-49.1635001148948,
124.40286143459)) ;
#112518 = CARTESIAN_POINT('Ctrl Pts',(-20.2586003862197,-49.1735271664805,
124.267990590128)) ;
#112519 = CARTESIAN_POINT('Ctrl Pts',(-20.3930406526253,-49.1834182563066,
124.109333994006)) ;
#112520 = CARTESIAN_POINT('Ctrl Pts',(-20.5342779951206,-49.1967160110877,
123.868104780252)) ;
#112521 = CARTESIAN_POINT('Ctrl Pts',(-20.609190819642,-49.2099140706958,
123.597594078994)) ;
#112522 = CARTESIAN_POINT('Ctrl Pts',(-20.6114275516929,-49.223310811265,
123.316024719013)) ;
#112523 = CARTESIAN_POINT('Ctrl Pts',(-20.5772402615923,-49.2331817233385,
123.111292507867)) ;
#112524 = CARTESIAN_POINT('Ctrl Pts',(-20.5066258182633,-49.2432552851066,
122.911686089534)) ;
#112525 = CARTESIAN_POINT('Ctrl Pts',(-20.405204144403,-49.2530766976949,
122.731777766255)) ;
#112526 = CARTESIAN_POINT('Ctrl Pts',(-20.2709332612198,-49.263150714926,
122.568063068129)) ;
#112527 = CARTESIAN_POINT('Ctrl Pts',(-20.0611118100133,-49.2763095018905,
122.387673800966)) ;
#112528 = CARTESIAN_POINT('Ctrl Pts',(-19.8053480766044,-49.2896756049847,
122.263890150075)) ;
#112529 = CARTESIAN_POINT('Ctrl Pts',(-19.5302618500152,-49.3029895398738,
122.211998231694)) ;
#112530 = CARTESIAN_POINT('Ctrl Pts',(-19.322173258648,-49.3128895793212,
122.209045193887)) ;
#112531 = CARTESIAN_POINT('Ctrl Pts',(-19.1153106938718,-49.3228539824558,
122.242142770257)) ;
#112532 = CARTESIAN_POINT('Ctrl Pts',(-18.9161024640866,-49.3328839495769,
122.311283145719)) ;
#112533 = CARTESIAN_POINT('Ctrl Pts',(-18.7342401363849,-49.342786226186,
122.412568319475)) ;
#112534 = CARTESIAN_POINT('Ctrl Pts',(-18.517366176944,-49.3560521553551,
122.587991055439)) ;
#112535 = CARTESIAN_POINT('Ctrl Pts',(-18.30957142216,-49.3726736864615,122.873770741006)) ;
#112536 = CARTESIAN_POINT('Ctrl Pts',(-18.192015813889,-49.3925485151062,
123.279733855682)) ;
#112537 = CARTESIAN_POINT('Ctrl Pts',(-18.2154654165058,-49.4092217232081,
123.633488353052)) ;
#112538 = CARTESIAN_POINT('Ctrl Pts',(-18.3053671473419,-49.4224728481893,
123.897133270708)) ;
#112539 = CARTESIAN_POINT('Ctrl Pts',(-18.4387434440384,-49.4357151670102,
124.141576453899)) ;
#112540 = CARTESIAN_POINT('Ctrl Pts',(-18.6845184576895,-49.4524484073496,
124.398730072478)) ;
#112541 = CARTESIAN_POINT('Ctrl Pts',(-19.0624384269411,-49.4722775555376,
124.58584708309)) ;
#112542 = CARTESIAN_POINT('Ctrl Pts',(-19.4832532966315,-49.4922022506382,
124.633993538889)) ;
#112543 = CARTESIAN_POINT('Ctrl Pts',(-19.8953523493917,-49.5121254792217,
124.53557750034)) ;
#112544 = CARTESIAN_POINT('Ctrl Pts',(-20.2491737763079,-49.5320526183478,
124.302567324585)) ;
#112545 = CARTESIAN_POINT('Ctrl Pts',(-20.5020828345387,-49.5519290809634,
123.96393258443)) ;
#112546 = CARTESIAN_POINT('Ctrl Pts',(-20.6250775151487,-49.5719063095687,
123.557364863011)) ;
#112547 = CARTESIAN_POINT('Ctrl Pts',(-20.6016593496557,-49.5918411675424,
123.13410630739)) ;
#112548 = CARTESIAN_POINT('Ctrl Pts',(-20.4359559222623,-49.6117376164732,
122.744890921738)) ;
#112549 = CARTESIAN_POINT('Ctrl Pts',(-20.147332301622,-49.6316589005398,
122.434838812771)) ;
#112550 = CARTESIAN_POINT('Ctrl Pts',(-19.7694955938687,-49.6516155502108,
122.241665286729)) ;
#112551 = CARTESIAN_POINT('Ctrl Pts',(-19.3501856822976,-49.6714928433224,
122.189109044763)) ;
#112552 = CARTESIAN_POINT('Ctrl Pts',(-18.9375747380152,-49.6913793155508,
122.281767052859)) ;
#112553 = CARTESIAN_POINT('Ctrl Pts',(-18.578588864441,-49.7114408814748,
122.512196275813)) ;
#112554 = CARTESIAN_POINT('Ctrl Pts',(-18.3229781081925,-49.7312812890156,
122.847777012305)) ;
#112555 = CARTESIAN_POINT('Ctrl Pts',(-18.1954623101242,-49.7511326129885,
123.250164082328)) ;
#112556 = CARTESIAN_POINT('Ctrl Pts',(-18.213734919431,-49.77118588294,123.676102974948)) ;
#112557 = CARTESIAN_POINT('Ctrl Pts',(-18.3743579456915,-49.7910065403233,
124.065860356479)) ;
#112558 = CARTESIAN_POINT('Ctrl Pts',(-18.6598220255199,-49.8109779616538,
124.380051991554)) ;
#112559 = CARTESIAN_POINT('Ctrl Pts',(-19.0341108196759,-49.8308714540175,
124.577425425163)) ;
#112560 = CARTESIAN_POINT('Ctrl Pts',(-19.4558354955313,-49.8508955402586,
124.635288468776)) ;
#112561 = CARTESIAN_POINT('Ctrl Pts',(-19.8676148488999,-49.8707004193714,
124.546941051481)) ;
#112562 = CARTESIAN_POINT('Ctrl Pts',(-20.227865170192,-49.8906594350693,
124.322644914943)) ;
#112563 = CARTESIAN_POINT('Ctrl Pts',(-20.489530623628,-49.9106454586984,
123.987809616561)) ;
#112564 = CARTESIAN_POINT('Ctrl Pts',(-20.6208573466702,-49.9304539544589,
123.58758433816)) ;
#112565 = CARTESIAN_POINT('Ctrl Pts',(-20.6081415997644,-49.9504365935644,
123.16298029532)) ;
#112566 = CARTESIAN_POINT('Ctrl Pts',(-20.4519151495861,-49.9703180413585,
122.770059233808)) ;
#112567 = CARTESIAN_POINT('Ctrl Pts',(-20.1703063471457,-49.990274508096,
122.45276767941)) ;
#112568 = CARTESIAN_POINT('Ctrl Pts',(-19.7988012664467,-50.0101519050516,
122.251091777802)) ;
#112569 = CARTESIAN_POINT('Ctrl Pts',(-19.3787230205005,-50.0301338512269,
122.187748844902)) ;
#112570 = CARTESIAN_POINT('Ctrl Pts',(-18.9632604830043,-50.0500629502636,
122.271572702089)) ;
#112571 = CARTESIAN_POINT('Ctrl Pts',(-18.6014588807801,-50.0699915734762,
122.491986611948)) ;
#112572 = CARTESIAN_POINT('Ctrl Pts',(-18.3371530370209,-50.0898258975826,
122.820679133444)) ;
#112573 = CARTESIAN_POINT('Ctrl Pts',(-18.2224316437084,-50.106478184966,
123.155550365973)) ;
#112574 = CARTESIAN_POINT('Ctrl Pts',(-18.2035148971638,-50.1197386859883,
123.43375828852)) ;
#112575 = CARTESIAN_POINT('Ctrl Pts',(-18.2255027776912,-50.1297401631895,
123.642859724866)) ;
#112576 = CARTESIAN_POINT('Ctrl Pts',(-18.2839836536651,-50.139772184049,
123.845501863548)) ;
#112577 = CARTESIAN_POINT('Ctrl Pts',(-18.3749684505038,-50.1496357277746,
124.031828661224)) ;
#112578 = CARTESIAN_POINT('Ctrl Pts',(-18.4977895113647,-50.1596044414447,
124.201656540985)) ;
#112579 = CARTESIAN_POINT('Ctrl Pts',(-18.6994118624443,-50.1729501888484,
124.39667330037)) ;
#112580 = CARTESIAN_POINT('Ctrl Pts',(-18.9435598837211,-50.1861007439211,
124.533078881535)) ;
#112581 = CARTESIAN_POINT('Ctrl Pts',(-19.2163066269421,-50.199486124471,
124.602308382208)) ;
#112582 = CARTESIAN_POINT('Ctrl Pts',(-19.4236344602334,-50.2093740604638,
124.617685592478)) ;
#112583 = CARTESIAN_POINT('Ctrl Pts',(-19.6326291408661,-50.2193652502764,
124.596970025646)) ;
#112584 = CARTESIAN_POINT('Ctrl Pts',(-19.834141889102,-50.2293173488147,
124.540573351786)) ;
#112585 = CARTESIAN_POINT('Ctrl Pts',(-20.0244847661262,-50.2393636052652,
124.449083585329)) ;
#112586 = CARTESIAN_POINT('Ctrl Pts',(-20.1927929341777,-50.2492130526593,
124.328458274937)) ;
#112587 = CARTESIAN_POINT('Ctrl Pts',(-20.3397273084912,-50.2591757051545,
124.179209288041)) ;
#112588 = CARTESIAN_POINT('Ctrl Pts',(-20.4590067387522,-50.2691987907966,
124.00550293132)) ;
#112589 = CARTESIAN_POINT('Ctrl Pts',(-20.5456866474962,-50.2791239065536,
123.815676367226)) ;
#112590 = CARTESIAN_POINT('Ctrl Pts',(-20.5986692480775,-50.2891763849534,
123.611111420755)) ;
#112591 = CARTESIAN_POINT('Ctrl Pts',(-20.6151364581576,-50.2990278836561,
123.404642091851)) ;
#112592 = CARTESIAN_POINT('Ctrl Pts',(-20.5958123606465,-50.3089996228586,
123.195923940047)) ;
#112593 = CARTESIAN_POINT('Ctrl Pts',(-20.5403702391664,-50.3189948306243,
122.993203978011)) ;
#112594 = CARTESIAN_POINT('Ctrl Pts',(-20.4500128197971,-50.3290288320934,
122.802609968587)) ;
#112595 = CARTESIAN_POINT('Ctrl Pts',(-20.3303547472016,-50.3388841901857,
122.633439905687)) ;
#112596 = CARTESIAN_POINT('Ctrl Pts',(-20.181228814507,-50.348883665779,122.485324042021)) ;
#112597 = CARTESIAN_POINT('Ctrl Pts',(-20.0105355194634,-50.3587781142741,
122.366373208271)) ;
#112598 = CARTESIAN_POINT('Ctrl Pts',(-19.8186063894417,-50.3688412385019,
122.277464202475)) ;
#112599 = CARTESIAN_POINT('Ctrl Pts',(-19.6186870394102,-50.3786808648305,
122.224196938849)) ;
#112600 = CARTESIAN_POINT('Ctrl Pts',(-19.4079577314643,-50.3887440998734,
122.205785639959)) ;
#112601 = CARTESIAN_POINT('Ctrl Pts',(-19.2007413885338,-50.3986381051075,
122.22411308346)) ;
#112602 = CARTESIAN_POINT('Ctrl Pts',(-18.9987616298135,-50.4085808183232,
122.277841967342)) ;
#112603 = CARTESIAN_POINT('Ctrl Pts',(-18.8079184533537,-50.4185865581214,
122.366364670794)) ;
#112604 = CARTESIAN_POINT('Ctrl Pts',(-18.6352410382406,-50.4286074602678,
122.487041101726)) ;
#112605 = CARTESIAN_POINT('Ctrl Pts',(-18.4878996305112,-50.4384982303167,
122.633772710933)) ;
#112606 = CARTESIAN_POINT('Ctrl Pts',(-18.3668077052516,-50.4484896410964,
122.805397870104)) ;
#112607 = CARTESIAN_POINT('Ctrl Pts',(-18.2778017566575,-50.4584379867609,
122.994654360126)) ;
#112608 = CARTESIAN_POINT('Ctrl Pts',(-18.2225965528002,-50.4683828448221,
123.196325636834)) ;
#112609 = CARTESIAN_POINT('Ctrl Pts',(-18.2033457855982,-50.478437680215,
123.406811664647)) ;
#112610 = CARTESIAN_POINT('Ctrl Pts',(-18.2201734187332,-50.4882600523165,
123.612639953426)) ;
#112611 = CARTESIAN_POINT('Ctrl Pts',(-18.2733507426702,-50.4983159197602,
123.817232754366)) ;
#112612 = CARTESIAN_POINT('Ctrl Pts',(-18.3605863404009,-50.5082566496181,
124.007149030284)) ;
#112613 = CARTESIAN_POINT('Ctrl Pts',(-18.4784977174571,-50.5181609881693,
124.178771169424)) ;
#112614 = CARTESIAN_POINT('Ctrl Pts',(-18.6265953152141,-50.5282076695977,
124.329338290363)) ;
#112615 = CARTESIAN_POINT('Ctrl Pts',(-18.7959297842799,-50.538103177067,
124.450244708555)) ;
#112616 = CARTESIAN_POINT('Ctrl Pts',(-18.98679191873,-50.5481654455656,124.541392395481)) ;
#112617 = CARTESIAN_POINT('Ctrl Pts',(-19.1861395232659,-50.5580074358362,
124.596914461004)) ;
#112618 = CARTESIAN_POINT('Ctrl Pts',(-19.3951643288124,-50.5680008527172,
124.617752496017)) ;
#112619 = CARTESIAN_POINT('Ctrl Pts',(-19.6032428165905,-50.5779253405694,
124.602103511439)) ;
#112620 = CARTESIAN_POINT('Ctrl Pts',(-19.8069911016793,-50.5879249744778,
124.550396919584)) ;
#112621 = CARTESIAN_POINT('Ctrl Pts',(-19.9984546726886,-50.5979110847346,
124.464201497683)) ;
#112622 = CARTESIAN_POINT('Ctrl Pts',(-20.1727426618484,-50.6079470359217,
124.34532767475)) ;
#112623 = CARTESIAN_POINT('Ctrl Pts',(-20.3212911735649,-50.6178036742565,
124.200825593126)) ;
#112624 = CARTESIAN_POINT('Ctrl Pts',(-20.4444414900303,-50.6278026343345,
124.030511612747)) ;
#112625 = CARTESIAN_POINT('Ctrl Pts',(-20.5354314452942,-50.6376978646483,
123.843398733492)) ;
#112626 = CARTESIAN_POINT('Ctrl Pts',(-20.5934652630922,-50.647758377117,
123.640040880647)) ;
#112627 = CARTESIAN_POINT('Ctrl Pts',(-20.6149702588124,-50.6576076686631,
123.434081690231)) ;
#112628 = CARTESIAN_POINT('Ctrl Pts',(-20.600658133905,-50.6676348545953,
123.223770254395)) ;
#112629 = CARTESIAN_POINT('Ctrl Pts',(-20.5494981650714,-50.6776633910547,
123.01922910674)) ;
#112630 = CARTESIAN_POINT('Ctrl Pts',(-20.4655381980224,-50.6875086310196,
122.830057891183)) ;
#112631 = CARTESIAN_POINT('Ctrl Pts',(-20.3487581951403,-50.6974993259428,
122.655473682621)) ;
#112632 = CARTESIAN_POINT('Ctrl Pts',(-20.2024196130709,-50.7075371467014,
122.503431006686)) ;
#112633 = CARTESIAN_POINT('Ctrl Pts',(-20.0353908164329,-50.7173817404784,
122.381213164985)) ;
#112634 = CARTESIAN_POINT('Ctrl Pts',(-19.8472666966091,-50.7273657358544,
122.288168117737)) ;
#112635 = CARTESIAN_POINT('Ctrl Pts',(-19.6465155507219,-50.7373147844158,
122.229421092525)) ;
#112636 = CARTESIAN_POINT('Ctrl Pts',(-19.4375248247999,-50.7473172233904,
122.206074791464)) ;
#112637 = CARTESIAN_POINT('Ctrl Pts',(-19.2272849712098,-50.7573384646867,
122.219680942423)) ;
#112638 = CARTESIAN_POINT('Ctrl Pts',(-19.0251689568679,-50.7672311431262,
122.268701074215)) ;
#112639 = CARTESIAN_POINT('Ctrl Pts',(-18.8326264313164,-50.7772211970739,
122.352581644759)) ;
#112640 = CARTESIAN_POINT('Ctrl Pts',(-18.6582153400934,-50.7871795582223,
122.468373080214)) ;
#112641 = CARTESIAN_POINT('Ctrl Pts',(-18.5070856641764,-50.7970791851072,
122.611480233133)) ;
#112642 = CARTESIAN_POINT('Ctrl Pts',(-18.3813233789678,-50.8071270819105,
122.781175163949)) ;
#112643 = CARTESIAN_POINT('Ctrl Pts',(-18.2881987381908,-50.8170224395465,
122.967235281899)) ;
#112644 = CARTESIAN_POINT('Ctrl Pts',(-18.2277834212995,-50.8270840920032,
123.169927313875)) ;
#112645 = CARTESIAN_POINT('Ctrl Pts',(-18.2039690796087,-50.8369286962752,
123.375523865749)) ;
#112646 = CARTESIAN_POINT('Ctrl Pts',(-18.2156084624216,-50.8468888179732,
123.58458947442)) ;
#112647 = CARTESIAN_POINT('Ctrl Pts',(-18.2641422862322,-50.8569268523357,
123.789955808551)) ;
#112648 = CARTESIAN_POINT('Ctrl Pts',(-18.3458993070211,-50.8668011649221,
123.980794947183)) ;
#112649 = CARTESIAN_POINT('Ctrl Pts',(-18.4617753485035,-50.8768706457048,
124.157922816574)) ;
#112650 = CARTESIAN_POINT('Ctrl Pts',(-18.6032126153864,-50.8867049817219,
124.308745769103)) ;
#112651 = CARTESIAN_POINT('Ctrl Pts',(-18.7716654279813,-50.8967379394501,
124.435671211385)) ;
#112652 = CARTESIAN_POINT('Ctrl Pts',(-18.9596341405767,-50.9067583380253,
124.530785270448)) ;
#112653 = CARTESIAN_POINT('Ctrl Pts',(-19.1580068381129,-50.9166239117966,
124.591379289052)) ;
#112654 = CARTESIAN_POINT('Ctrl Pts',(-19.3680927099143,-50.9266927864526,
124.61712779175)) ;
#112655 = CARTESIAN_POINT('Ctrl Pts',(-19.5748010130013,-50.9365382173581,
124.606284092173)) ;
#112656 = CARTESIAN_POINT('Ctrl Pts',(-19.7793703423323,-50.9465178422288,
124.559741988982)) ;
#112657 = CARTESIAN_POINT('Ctrl Pts',(-19.9733529078127,-50.9565365251429,
124.477700113164)) ;
#112658 = CARTESIAN_POINT('Ctrl Pts',(-20.1480190596379,-50.9664197903268,
124.365122951867)) ;
#112659 = CARTESIAN_POINT('Ctrl Pts',(-20.3032326727282,-50.9764880844181,
124.221258009866)) ;
#112660 = CARTESIAN_POINT('Ctrl Pts',(-20.4283189444348,-50.9863182146035,
124.056709463853)) ;
#112661 = CARTESIAN_POINT('Ctrl Pts',(-20.5254218842155,-50.9963847628186,
123.868708549322)) ;
#112662 = CARTESIAN_POINT('Ctrl Pts',(-20.5871979301326,-51.0062750115072,
123.670146987558)) ;
#112663 = CARTESIAN_POINT('Ctrl Pts',(-20.6142816467168,-51.0162671932833,
123.461845422591)) ;
#112664 = CARTESIAN_POINT('Ctrl Pts',(-20.6046169448565,-51.0262299739111,
123.252623585603)) ;
#112665 = CARTESIAN_POINT('Ctrl Pts',(-20.5595449556983,-51.0361343785848,
123.049323802543)) ;
#112666 = CARTESIAN_POINT('Ctrl Pts',(-20.4784730252217,-51.0461943730639,
122.854007128078)) ;
#112667 = CARTESIAN_POINT('Ctrl Pts',(-20.3672413189656,-51.0560429950336,
122.679356150277)) ;
#112668 = CARTESIAN_POINT('Ctrl Pts',(-20.2251601542649,-51.0660734344455,
122.523552994694)) ;
#112669 = CARTESIAN_POINT('Ctrl Pts',(-20.0582426814132,-51.0760831500802,
122.395367416698)) ;
#112670 = CARTESIAN_POINT('Ctrl Pts',(-19.8735803491217,-51.0859939027728,
122.298912820241)) ;
#112671 = CARTESIAN_POINT('Ctrl Pts',(-19.674735027393,-51.0959231757192,
122.235360617119)) ;
#112672 = CARTESIAN_POINT('Ctrl Pts',(-19.4655065445213,-51.1059658671119,
122.207159119509)) ;
#112673 = CARTESIAN_POINT('Ctrl Pts',(-19.2578144174641,-51.1158524003294,
122.215447050614)) ;
#112674 = CARTESIAN_POINT('Ctrl Pts',(-19.0524729282517,-51.1258455452615,
122.259795132188)) ;
#112675 = CARTESIAN_POINT('Ctrl Pts',(-18.8588941676076,-51.1357912260979,
122.338825291014)) ;
#112676 = CARTESIAN_POINT('Ctrl Pts',(-18.6817137475003,-51.1457384832465,
122.449927361774)) ;
#112677 = CARTESIAN_POINT('Ctrl Pts',(-18.5251171049062,-51.1557863871185,
122.591689226379)) ;
#112678 = CARTESIAN_POINT('Ctrl Pts',(-18.3979545063662,-51.1656340862164,
122.755062985549)) ;
#112679 = CARTESIAN_POINT('Ctrl Pts',(-18.299391322462,-51.1755955771951,
122.93983133097)) ;
#112680 = CARTESIAN_POINT('Ctrl Pts',(-18.2342270482721,-51.1856250396091,
123.14036889934)) ;
#112681 = CARTESIAN_POINT('Ctrl Pts',(-18.2051196484244,-51.195532270709,
123.346606058763)) ;
#112682 = CARTESIAN_POINT('Ctrl Pts',(-18.2118665859905,-51.2054786493864,
123.555588712844)) ;
#112683 = CARTESIAN_POINT('Ctrl Pts',(-18.2549824645526,-51.2154834181952,
123.761472396139)) ;
#112684 = CARTESIAN_POINT('Ctrl Pts',(-18.3335348192412,-51.2255045392154,
123.956951359182)) ;
#112685 = CARTESIAN_POINT('Ctrl Pts',(-18.4431917157819,-51.2353954050681,
124.133632026721)) ;
#112686 = CARTESIAN_POINT('Ctrl Pts',(-18.5830178355526,-51.2453862138273,
124.290347276985)) ;
#112687 = CARTESIAN_POINT('Ctrl Pts',(-18.747310135802,-51.2553368720076,
124.419863404542)) ;
#112688 = CARTESIAN_POINT('Ctrl Pts',(-18.9311712481617,-51.2652730816497,
124.518976091854)) ;
#112689 = CARTESIAN_POINT('Ctrl Pts',(-19.1303407741657,-51.2752562483746,
124.585241146071)) ;
#112690 = CARTESIAN_POINT('Ctrl Pts',(-19.3392592089175,-51.285300045585,
124.615709667689)) ;
#112691 = CARTESIAN_POINT('Ctrl Pts',(-19.5458329516792,-51.2951282617532,
124.610062207379)) ;
#112692 = CARTESIAN_POINT('Ctrl Pts',(-19.7533510198841,-51.3052048292224,
124.567699066889)) ;
#112693 = CARTESIAN_POINT('Ctrl Pts',(-19.9460915305853,-51.3150569149118,
124.491744743796)) ;
#112694 = CARTESIAN_POINT('Ctrl Pts',(-20.1267072366614,-51.3251301823172,
124.381242674608)) ;
#112695 = CARTESIAN_POINT('Ctrl Pts',(-20.2817384563211,-51.3349715987408,
124.244210915471)) ;
#112696 = CARTESIAN_POINT('Ctrl Pts',(-20.4127892301149,-51.3449328568836,
124.080877695399)) ;
#112697 = CARTESIAN_POINT('Ctrl Pts',(-20.5138960157704,-51.3549695333155,
123.89568101577)) ;
#112698 = CARTESIAN_POINT('Ctrl Pts',(-20.5805894963791,-51.3648481411793,
123.698978791711)) ;
#112699 = CARTESIAN_POINT('Ctrl Pts',(-20.6127348911985,-51.3749083698181,
123.489965857339)) ;
#112700 = CARTESIAN_POINT('Ctrl Pts',(-20.6082491364838,-51.3847753539789,
123.282553134315)) ;
#112701 = CARTESIAN_POINT('Ctrl Pts',(-20.5676589645604,-51.3947809202316,
123.076186469411)) ;
#112702 = CARTESIAN_POINT('Ctrl Pts',(-20.4919452068756,-51.4047647086462,
122.880388030383)) ;
#112703 = CARTESIAN_POINT('Ctrl Pts',(-20.3825404339122,-51.4148105654489,
122.699758479817)) ;
#112704 = CARTESIAN_POINT('Ctrl Pts',(-20.2466721794999,-51.4246364426648,
122.544158506925)) ;
#112705 = CARTESIAN_POINT('Ctrl Pts',(-20.0835883095508,-51.4346269185061,
122.411807494114)) ;
#112706 = CARTESIAN_POINT('Ctrl Pts',(-19.8987560226693,-51.4446704944049,
122.309726607672)) ;
#112707 = CARTESIAN_POINT('Ctrl Pts',(-19.7035602889854,-51.454492286703,
122.242391815721)) ;
#112708 = CARTESIAN_POINT('Ctrl Pts',(-19.4952918997847,-51.4645272523288,
122.208757967334)) ;
#112709 = CARTESIAN_POINT('Ctrl Pts',(-19.2845621023363,-51.4745521692619,
122.212381311644)) ;
#112710 = CARTESIAN_POINT('Ctrl Pts',(-19.0811480042896,-51.484404107638,
122.25140096557)) ;
#112711 = CARTESIAN_POINT('Ctrl Pts',(-18.8847815882352,-51.4943950836628,
122.3258774984)) ;
#112712 = CARTESIAN_POINT('Ctrl Pts',(-18.7055334699572,-51.5043129044664,
122.432438648279)) ;
#112713 = CARTESIAN_POINT('Ctrl Pts',(-18.5457589562265,-51.514341625031,
122.569967502804)) ;
#112714 = CARTESIAN_POINT('Ctrl Pts',(-18.4140946735869,-51.5242245516402,
122.73071861672)) ;
#112715 = CARTESIAN_POINT('Ctrl Pts',(-18.3108219270137,-51.5342288367597,
122.913912176719)) ;
#112716 = CARTESIAN_POINT('Ctrl Pts',(-18.2410730116051,-51.5442125179675,
123.111910051885)) ;
#112717 = CARTESIAN_POINT('Ctrl Pts',(-18.2068130647051,-51.5542535166975,
123.320189013492)) ;
#112718 = CARTESIAN_POINT('Ctrl Pts',(-18.2088961336951,-51.5640859615646,
123.52688957825)) ;
#112719 = CARTESIAN_POINT('Ctrl Pts',(-18.2468544329822,-51.5740809599949,
123.733553095855)) ;
#112720 = CARTESIAN_POINT('Ctrl Pts',(-18.3208167251711,-51.5841125087445,
123.931064856642)) ;
#112721 = CARTESIAN_POINT('Ctrl Pts',(-18.4259390712428,-51.59397788705,124.109838076423)) ;
#112722 = CARTESIAN_POINT('Ctrl Pts',(-18.5613822053359,-51.6039397345103,
124.269583194417)) ;
#112723 = CARTESIAN_POINT('Ctrl Pts',(-18.7238931725869,-51.6139746753246,
124.404089901432)) ;
#112724 = CARTESIAN_POINT('Ctrl Pts',(-18.9044114707914,-51.6238596363417,
124.507102311526)) ;
#112725 = CARTESIAN_POINT('Ctrl Pts',(-19.1036051370934,-51.6339252452606,
124.578422045019)) ;
#112726 = CARTESIAN_POINT('Ctrl Pts',(-19.3074948149248,-51.6437644203022,
124.613485807768)) ;
#112727 = CARTESIAN_POINT('Ctrl Pts',(-19.5190160718242,-51.6538269758022,
124.612887340952)) ;
#112728 = CARTESIAN_POINT('Ctrl Pts',(-19.7237939479907,-51.6637241504951,
124.575955884788)) ;
#112729 = CARTESIAN_POINT('Ctrl Pts',(-19.919937465841,-51.6736548654184,
124.504449571205)) ;
#112730 = CARTESIAN_POINT('Ctrl Pts',(-20.1026258992887,-51.683698893496,
124.398570252338)) ;
#112731 = CARTESIAN_POINT('Ctrl Pts',(-20.261735811042,-51.6935850953493,
124.264827956889)) ;
#112732 = CARTESIAN_POINT('Ctrl Pts',(-20.3968709458919,-51.7035782618161,
124.103998740106)) ;
#112733 = CARTESIAN_POINT('Ctrl Pts',(-20.5015409411099,-51.7135177328034,
123.923114773742)) ;
#112734 = CARTESIAN_POINT('Ctrl Pts',(-20.5737915755205,-51.7235342471575,
123.725341959794)) ;
#112735 = CARTESIAN_POINT('Ctrl Pts',(-20.6104698830179,-51.7334642736344,
123.519799372944)) ;
#112736 = CARTESIAN_POINT('Ctrl Pts',(-20.6108142890113,-51.7435168091438,
123.308481567904)) ;
#112737 = CARTESIAN_POINT('Ctrl Pts',(-20.5753196619724,-51.7533632123635,
123.104537840915)) ;
#112738 = CARTESIAN_POINT('Ctrl Pts',(-20.5047695869921,-51.7633252552176,
122.907357363388)) ;
#112739 = CARTESIAN_POINT('Ctrl Pts',(-20.4001109887819,-51.7733538060082,
122.724320591003)) ;
#112740 = CARTESIAN_POINT('Ctrl Pts',(-20.2669195170586,-51.7832641317259,
122.56411999032)) ;
#112741 = CARTESIAN_POINT('Ctrl Pts',(-20.107881764231,-51.7931990435554,
122.428718679853)) ;
#112742 = CARTESIAN_POINT('Ctrl Pts',(-19.9257386287471,-51.8032400503235,
122.322032728023)) ;
#112743 = CARTESIAN_POINT('Ctrl Pts',(-19.7308938638371,-51.8131276831557,
122.249579695475)) ;
#112744 = CARTESIAN_POINT('Ctrl Pts',(-19.5243909163584,-51.8231181142538,
122.211305883517)) ;
#112745 = CARTESIAN_POINT('Ctrl Pts',(-19.3150968639725,-51.833073550811,
122.209588120564)) ;
#112746 = CARTESIAN_POINT('Ctrl Pts',(-19.1095608840621,-51.8429844989103,
122.243702271056)) ;
#112747 = CARTESIAN_POINT('Ctrl Pts',(-18.9109542294438,-51.852996575008,
122.313473096882)) ;
#112748 = CARTESIAN_POINT('Ctrl Pts',(-18.727441220938,-51.863023897083,122.417177700006)) ;
#112749 = CARTESIAN_POINT('Ctrl Pts',(-18.5670835351562,-51.8728826720372,
122.548549395356)) ;
#112750 = CARTESIAN_POINT('Ctrl Pts',(-18.3833391042562,-51.8863088648496,
122.762733815895)) ;
#112751 = CARTESIAN_POINT('Ctrl Pts',(-18.2623737700174,-51.899392880631,
123.013407995106)) ;
#112752 = CARTESIAN_POINT('Ctrl Pts',(-18.2092236013382,-51.9128663293862,
123.291528365553)) ;
#112753 = CARTESIAN_POINT('Ctrl Pts',(-18.2065462379793,-51.9226992871921,
123.4982667153)) ;
#112754 = CARTESIAN_POINT('Ctrl Pts',(-18.2393644183496,-51.9326625606427,
123.705123027563)) ;
#112755 = CARTESIAN_POINT('Ctrl Pts',(-18.3085412245122,-51.9426996344607,
123.904470097435)) ;
#112756 = CARTESIAN_POINT('Ctrl Pts',(-18.4092917461789,-51.9525746374723,
124.086015929885)) ;
#112757 = CARTESIAN_POINT('Ctrl Pts',(-18.5425574544622,-51.9626423170985,
124.250410246371)) ;
#112758 = CARTESIAN_POINT('Ctrl Pts',(-18.6987039415357,-51.9724831673162,
124.386166061986)) ;
#112759 = CARTESIAN_POINT('Ctrl Pts',(-18.9387011299791,-51.9858193657922,
124.531082053001)) ;
#112760 = CARTESIAN_POINT('Ctrl Pts',(-19.2087116420615,-51.9990368896066,
124.60924459251)) ;
#112761 = CARTESIAN_POINT('Ctrl Pts',(-19.4889265757665,-52.0123718160979,
124.615216455318)) ;
#112762 = CARTESIAN_POINT('Ctrl Pts',(-19.6963982872269,-52.0223549166925,
124.583256147023)) ;
#112763 = CARTESIAN_POINT('Ctrl Pts',(-19.8962330924119,-52.0323996925921,
124.515063107923)) ;
#112764 = CARTESIAN_POINT('Ctrl Pts',(-20.0772449980274,-52.042217615778,
124.415851635224)) ;
#112765 = CARTESIAN_POINT('Ctrl Pts',(-20.2423283485584,-52.0522669297334,
124.28402776922)) ;
#112766 = CARTESIAN_POINT('Ctrl Pts',(-20.4268317901234,-52.0655706703559,
124.073827263991)) ;
#112767 = CARTESIAN_POINT('Ctrl Pts',(-20.5831621926118,-52.0820608658326,
123.759945685997)) ;
#112768 = CARTESIAN_POINT('Ctrl Pts',(-20.6234000138412,-52.0987800307572,
123.406774916073)) ;
#112769 = CARTESIAN_POINT('Ctrl Pts',(-20.582485071963,-52.1119410244274,
123.133123245053)) ;
#112770 = CARTESIAN_POINT('Ctrl Pts',(-20.5165248713095,-52.1219372465326,
122.933597826454)) ;
#112771 = CARTESIAN_POINT('Ctrl Pts',(-20.4162229703339,-52.1319610860664,
122.748268378229)) ;
#112772 = CARTESIAN_POINT('Ctrl Pts',(-20.2443143446357,-52.1451544080596,
122.530558883224)) ;
#112773 = CARTESIAN_POINT('Ctrl Pts',(-19.960637766521,-52.1618135798369,
122.318506411865)) ;
#112774 = CARTESIAN_POINT('Ctrl Pts',(-19.5552838947998,-52.1817237553226,
122.196345924405)) ;
#112775 = CARTESIAN_POINT('Ctrl Pts',(-19.1329274788629,-52.201613743167,
122.21894138524)) ;
#112776 = CARTESIAN_POINT('Ctrl Pts',(-18.7416358730448,-52.2216191911818,
122.385574926501)) ;
#112777 = CARTESIAN_POINT('Ctrl Pts',(-18.4328880060854,-52.2414555852091,
122.67309119488)) ;
#112778 = CARTESIAN_POINT('Ctrl Pts',(-18.2390833517027,-52.2614633791058,
123.051672805991)) ;
#112779 = CARTESIAN_POINT('Ctrl Pts',(-18.1864119564092,-52.2812900153998,
123.470015081427)) ;
#112780 = CARTESIAN_POINT('Ctrl Pts',(-18.2796040947721,-52.3012689583536,
123.88445686926)) ;
#112781 = CARTESIAN_POINT('Ctrl Pts',(-18.508702238209,-52.3212007602227,
124.240933892213)) ;
#112782 = CARTESIAN_POINT('Ctrl Pts',(-18.843164123141,-52.3410250607202,
124.497691120367)) ;
#112783 = CARTESIAN_POINT('Ctrl Pts',(-19.2506096488724,-52.3611210620601,
124.625832867507)) ;
#112784 = CARTESIAN_POINT('Ctrl Pts',(-19.6705945477707,-52.380879478164,
124.607989808831)) ;
#112785 = CARTESIAN_POINT('Ctrl Pts',(-20.0654778420062,-52.4009731710481,
124.445491756973)) ;
#112786 = CARTESIAN_POINT('Ctrl Pts',(-20.2716335866836,-52.4140841369548,
124.257641708504)) ;
#112787 = CARTESIAN_POINT('Ctrl Pts',(-20.3578982754669,-52.4207975117427,
124.146632267721)) ;
#112788 = CARTESIAN_POINT('',(-20.1427547090972,-13.6718523192586,122.386342110905)) ;
#112789 = CARTESIAN_POINT('Ctrl Pts',(-19.0974359578004,-13.6947924667252,
122.237608099407)) ;
#112790 = CARTESIAN_POINT('Ctrl Pts',(-19.2120769631286,-13.6922154699035,
122.201830774592)) ;
#112791 = CARTESIAN_POINT('Ctrl Pts',(-19.3314507352027,-13.6896773479743,
122.183356159395)) ;
#112792 = CARTESIAN_POINT('Ctrl Pts',(-19.5995429421847,-13.6839804037597,
122.180997175628)) ;
#112793 = CARTESIAN_POINT('Ctrl Pts',(-19.721803047479,-13.6814287159781,
122.206768959723)) ;
#112794 = CARTESIAN_POINT('Ctrl Pts',(-19.8865306638505,-13.6778224757203,
122.254908008027)) ;
#112795 = CARTESIAN_POINT('Ctrl Pts',(-19.9620984847369,-13.6761482722936,
122.285342576564)) ;
#112796 = CARTESIAN_POINT('Ctrl Pts',(-20.0723681059987,-13.6735665071745,
122.342645278353)) ;
#112797 = CARTESIAN_POINT('Ctrl Pts',(-20.1085870938132,-13.6726943420558,
122.363974125483)) ;
#112798 = CARTESIAN_POINT('Ctrl Pts',(-20.1427547090971,-13.6718523192586,
122.386342110905)) ;
#112799 = CARTESIAN_POINT('Ctrl Pts',(-20.1427547090971,-13.6718523192586,
122.386342110905)) ;
#112800 = CARTESIAN_POINT('Ctrl Pts',(-20.2533086992448,-13.6691278393892,
122.458716785562)) ;
#112801 = CARTESIAN_POINT('Ctrl Pts',(-20.3424059519751,-13.6666598154076,
122.541938102797)) ;
#112802 = CARTESIAN_POINT('Ctrl Pts',(-20.52065809351,-13.6610234961052,122.750520764435)) ;
#112803 = CARTESIAN_POINT('Ctrl Pts',(-20.6032494586061,-13.6577012237831,
122.897899282716)) ;
#112804 = CARTESIAN_POINT('Ctrl Pts',(-20.681889270313,-13.6526511564228,
123.137033239163)) ;
#112805 = CARTESIAN_POINT('Ctrl Pts',(-20.7003452000579,-13.6509739277555,
123.219679921959)) ;
#112806 = CARTESIAN_POINT('Ctrl Pts',(-20.721135241652,-13.6475919378546,
123.387953197661)) ;
#112807 = CARTESIAN_POINT('Ctrl Pts',(-20.7233363536002,-13.6458822226044,
123.473399226477)) ;
#112808 = CARTESIAN_POINT('Ctrl Pts',(-20.7110403730629,-13.6425352830905,
123.643193427743)) ;
#112809 = CARTESIAN_POINT('Ctrl Pts',(-20.6965740866421,-13.6408892425586,
123.727436908383)) ;
#112810 = CARTESIAN_POINT('Ctrl Pts',(-20.6515138209952,-13.637458664297,
123.893871600147)) ;
#112811 = CARTESIAN_POINT('Ctrl Pts',(-20.6203597889817,-13.6357466098998,
123.975677850441)) ;
#112812 = CARTESIAN_POINT('Ctrl Pts',(-20.5428030701302,-13.6324211081288,
124.130955369702)) ;
#112813 = CARTESIAN_POINT('Ctrl Pts',(-20.4970550450635,-13.6307370012978,
124.204192372236)) ;
#112814 = CARTESIAN_POINT('Ctrl Pts',(-20.3909174270119,-13.627327030588,
124.34259237775)) ;
#112815 = CARTESIAN_POINT('Ctrl Pts',(-20.3303019140264,-13.625657631967,
124.407138812779)) ;
#112816 = CARTESIAN_POINT('Ctrl Pts',(-20.1966757307745,-13.6222674503412,
124.524262641715)) ;
#112817 = CARTESIAN_POINT('Ctrl Pts',(-20.1239933631889,-13.6205446496782,
124.576366759863)) ;
#112818 = CARTESIAN_POINT('Ctrl Pts',(-19.9689329053457,-13.6171441040426,
124.665720042683)) ;
#112819 = CARTESIAN_POINT('Ctrl Pts',(-19.8873263669662,-13.6154427854306,
124.702675859603)) ;
#112820 = CARTESIAN_POINT('Ctrl Pts',(-19.6330384003724,-13.6103641080695,
124.789104028508)) ;
#112821 = CARTESIAN_POINT('Ctrl Pts',(-19.4536584152726,-13.6070536493634,
124.813121692777)) ;
#112822 = CARTESIAN_POINT('Ctrl Pts',(-19.1827744651566,-13.6019893485611,
124.796942766395)) ;
#112823 = CARTESIAN_POINT('Ctrl Pts',(-19.0924943493097,-13.6002817418405,
124.782641282948)) ;
#112824 = CARTESIAN_POINT('Ctrl Pts',(-18.824850920792,-13.5952033913341,
124.712722188967)) ;
#112825 = CARTESIAN_POINT('Ctrl Pts',(-18.6565129639246,-13.5918390838892,
124.630996767531)) ;
#112826 = CARTESIAN_POINT('Ctrl Pts',(-18.3602350620407,-13.5850157442234,
124.407701004899)) ;
#112827 = CARTESIAN_POINT('Ctrl Pts',(-18.2352659715359,-13.5817118196255,
124.267794979268)) ;
#112828 = CARTESIAN_POINT('Ctrl Pts',(-18.092056886489,-13.5766954025593,
124.027929221237)) ;
#112829 = CARTESIAN_POINT('Ctrl Pts',(-18.0516931671806,-13.5750061219964,
123.942337834033)) ;
#112830 = CARTESIAN_POINT('Ctrl Pts',(-17.9880845644536,-13.5716296807247,
123.764555003539)) ;
#112831 = CARTESIAN_POINT('Ctrl Pts',(-17.9650672998151,-13.5699752678031,
123.672811723789)) ;
#112832 = CARTESIAN_POINT('Ctrl Pts',(-17.9283249417299,-13.5656129119573,
123.429645434397)) ;
#112833 = CARTESIAN_POINT('Ctrl Pts',(-17.9289880100393,-13.5629586805205,
123.277778063909)) ;
#112834 = CARTESIAN_POINT('Ctrl Pts',(-17.9646728459758,-13.5589725221897,
123.052964478894)) ;
#112835 = CARTESIAN_POINT('Ctrl Pts',(-17.982347914987,-13.5576281988937,
122.978706457618)) ;
#112836 = CARTESIAN_POINT('Ctrl Pts',(-18.0291931228724,-13.5549754839852,
122.833074777741)) ;
#112837 = CARTESIAN_POINT('Ctrl Pts',(-18.0583348684619,-13.5536392537495,
122.761805861894)) ;
#112838 = CARTESIAN_POINT('Ctrl Pts',(-18.0926293799299,-13.5522956097346,
122.693350211338)) ;
#112839 = CARTESIAN_POINT('Origin',(-19.4092696390352,-14.2022556137854,123.411833654994)) ;
#112840 = CARTESIAN_POINT('',(-19.9937457018646,-13.7999200508426,122.59467283657)) ;
#112841 = CARTESIAN_POINT('',(-19.5256213580744,-14.2022556137854,123.249161354104)) ;
#112842 = CARTESIAN_POINT('Origin',(-19.4092696390352,-13.7999200508426,123.411833654994)) ;
#112843 = CARTESIAN_POINT('Origin',(-20.3808792107508,-13.7999200508426,126.250138578738)) ;
#112844 = CARTESIAN_POINT('',(-18.7566932181803,-13.7999200508426,122.842497185995)) ;
#112845 = CARTESIAN_POINT('',(-19.5760412740645,-13.7999200508426,122.56201766211)) ;
#112846 = CARTESIAN_POINT('',(-18.7566932181803,-13.7999200508426,122.842497185995)) ;
#112847 = CARTESIAN_POINT('',(-20.2286176949323,-13.7999200508426,123.131354131104)) ;
#112848 = CARTESIAN_POINT('',(-19.5760412740645,-13.7999200508426,122.56201766211)) ;
#112849 = CARTESIAN_POINT('',(-20.0618460599159,-13.7999200508426,123.981170123984)) ;
#112850 = CARTESIAN_POINT('',(-20.2286176949323,-13.7999200508426,123.131354131104)) ;
#112851 = CARTESIAN_POINT('',(-19.2424980040317,-13.7999200508426,124.261649647869)) ;
#112852 = CARTESIAN_POINT('',(-20.0618460599159,-13.7999200508426,123.981170123984)) ;
#112853 = CARTESIAN_POINT('',(-18.5899215831638,-13.7999200508426,123.692313178874)) ;
#112854 = CARTESIAN_POINT('',(-19.2424980040317,-13.7999200508426,124.261649647869)) ;
#112855 = CARTESIAN_POINT('',(-18.5899215831638,-13.7999200508426,123.692313178874)) ;
#112856 = CARTESIAN_POINT('Origin',(-18.7566932181803,-15.3022556137854,122.842497185995)) ;
#112857 = CARTESIAN_POINT('',(-18.7566932181803,-12.9245228503138,122.842497185995)) ;
#112858 = CARTESIAN_POINT('',(-18.7566932181803,-13.7999200508426,122.842497185995)) ;
#112859 = CARTESIAN_POINT('',(-19.5760412740645,-12.9245228503138,122.56201766211)) ;
#112860 = CARTESIAN_POINT('',(-18.7566932181803,-12.9245228503138,122.842497185995)) ;
#112861 = CARTESIAN_POINT('',(-19.5760412740645,-13.7999200508426,122.56201766211)) ;
#112862 = CARTESIAN_POINT('Origin',(-19.5760412740645,-15.3022556137854,122.56201766211)) ;
#112863 = CARTESIAN_POINT('',(-20.2286176949323,-12.9245228503138,123.131354131104)) ;
#112864 = CARTESIAN_POINT('',(-19.5760412740645,-12.9245228503138,122.56201766211)) ;
#112865 = CARTESIAN_POINT('',(-20.2286176949323,-13.7999200508426,123.131354131104)) ;
#112866 = CARTESIAN_POINT('Origin',(-20.2286176949323,-15.3022556137854,123.131354131104)) ;
#112867 = CARTESIAN_POINT('',(-20.0618460599159,-12.9245228503138,123.981170123984)) ;
#112868 = CARTESIAN_POINT('',(-20.2286176949323,-12.9245228503138,123.131354131104)) ;
#112869 = CARTESIAN_POINT('',(-20.0618460599159,-13.7999200508426,123.981170123984)) ;
#112870 = CARTESIAN_POINT('Origin',(-20.0618460599159,-15.3022556137854,123.981170123984)) ;
#112871 = CARTESIAN_POINT('',(-19.2424980040316,-12.9245228503138,124.261649647869)) ;
#112872 = CARTESIAN_POINT('',(-20.0618460599159,-12.9245228503138,123.981170123984)) ;
#112873 = CARTESIAN_POINT('',(-19.2424980040317,-13.7999200508426,124.261649647869)) ;
#112874 = CARTESIAN_POINT('Origin',(-19.2424980040316,-15.3022556137854,124.261649647869)) ;
#112875 = CARTESIAN_POINT('',(-18.5899215831638,-12.9245228503138,123.692313178874)) ;
#112876 = CARTESIAN_POINT('',(-19.2424980040316,-12.9245228503138,124.261649647869)) ;
#112877 = CARTESIAN_POINT('',(-18.5899215831638,-13.7999200508426,123.692313178874)) ;
#112878 = CARTESIAN_POINT('Origin',(-18.5899215831638,-15.3022556137854,123.692313178874)) ;
#112879 = CARTESIAN_POINT('',(-18.5899215831638,-12.9245228503138,123.692313178874)) ;
#112880 = CARTESIAN_POINT('Origin',(-18.7566932181803,-12.9245228503138,122.842497185995)) ;
#112881 = CARTESIAN_POINT('Origin',(-32.7369214287712,6.20000000004959,159.065417425017)) ;
#112882 = CARTESIAN_POINT('',(-29.8935702991225,6.2000000000496,130.4656735525)) ;
#112883 = CARTESIAN_POINT('',(-11.2264641357304,6.2000000000496,140.004194424792)) ;
#112884 = CARTESIAN_POINT('Origin',(-32.7369214287712,6.20000000004961,159.065417425018)) ;
#112885 = CARTESIAN_POINT('',(-11.2264641357304,9.2000000000496,140.004194424792)) ;
#112886 = CARTESIAN_POINT('',(-11.2264641357304,6.2000000000496,140.004194424792)) ;
#112887 = CARTESIAN_POINT('',(-29.8935702991225,9.2000000000496,130.4656735525)) ;
#112888 = CARTESIAN_POINT('Origin',(-32.7369214287712,9.2000000000496,159.065417425018)) ;
#112889 = CARTESIAN_POINT('',(-29.8935702991225,6.2000000000496,130.4656735525)) ;
#112890 = CARTESIAN_POINT('Origin',(-1.22124532708767E-13,6.2000000000496,
130.056003483261)) ;
#112891 = CARTESIAN_POINT('',(-2.77488334235139,6.2000000000496,115.314903713015)) ;
#112892 = CARTESIAN_POINT('Origin',(-1.17683640610267E-13,6.2000000000496,
130.056003483261)) ;
#112893 = CARTESIAN_POINT('',(-2.77488334235139,9.2000000000496,115.314903713015)) ;
#112894 = CARTESIAN_POINT('',(-2.77488334235139,6.2000000000496,115.314903713015)) ;
#112895 = CARTESIAN_POINT('Origin',(-1.17683640610267E-13,9.2000000000496,
130.056003483261)) ;
#112896 = CARTESIAN_POINT('Origin',(-8.09169626799619,6.2000000000496,87.0702317281284)) ;
#112897 = CARTESIAN_POINT('',(-23.3714287291853,6.2000000000496,111.412782357317)) ;
#112898 = CARTESIAN_POINT('Origin',(-8.09169626799633,6.2000000000496,87.0702317281289)) ;
#112899 = CARTESIAN_POINT('',(-23.3714287291853,9.2000000000496,111.412782357317)) ;
#112900 = CARTESIAN_POINT('',(-23.3714287291853,6.2000000000496,111.412782357317)) ;
#112901 = CARTESIAN_POINT('Origin',(-8.09169626799633,9.20000000004958,87.0702317281289)) ;
#112902 = CARTESIAN_POINT('Origin',(-28.8703041205684,6.2000000000496,120.173187866852)) ;
#112903 = CARTESIAN_POINT('Origin',(-28.8703041205685,6.2000000000496,120.173187866852)) ;
#112904 = CARTESIAN_POINT('Origin',(-28.8703041205685,9.2000000000496,120.173187866852)) ;
#112905 = CARTESIAN_POINT('Origin',(-10.6619859316946,6.2000000000496,134.537724339802)) ;
#112906 = CARTESIAN_POINT('',(-9.66208462629207,9.2000000000496,134.523675159956)) ;
#112907 = CARTESIAN_POINT('Origin',(-10.6619859316946,9.2000000000496,134.537724339801)) ;
#112908 = CARTESIAN_POINT('',(-9.66208462629207,6.2000000000496,134.523675159956)) ;
#112909 = CARTESIAN_POINT('',(-9.66208462629206,6.2000000000496,134.523675159956)) ;
#112910 = CARTESIAN_POINT('Origin',(-10.6619859316946,6.2000000000496,134.537724339801)) ;
#112911 = CARTESIAN_POINT('Origin',(-27.0022936957715,6.2000000000496,119.45866911073)) ;
#112912 = CARTESIAN_POINT('',(-27.0022936957715,6.2000000000496,119.45866911073)) ;
#112913 = CARTESIAN_POINT('Origin',(-28.8703041205685,6.2000000000496,120.173187866852)) ;
#112914 = CARTESIAN_POINT('',(-22.3968667215,6.2000000000496,124.757886585629)) ;
#112915 = CARTESIAN_POINT('',(-20.9452555485298,6.2000000000496,120.517347833308)) ;
#112916 = CARTESIAN_POINT('Origin',(-4.6047610169353E-11,6.20000000004936,
130.056003483247)) ;
#112917 = CARTESIAN_POINT('',(-17.5311532747538,6.2000000000496,125.908900336264)) ;
#112918 = CARTESIAN_POINT('Origin',(-19.9640098891908,6.2000000000496,125.333393000437)) ;
#112919 = CARTESIAN_POINT('',(-16.3949039990916,6.2000000000496,122.589617308188)) ;
#112920 = CARTESIAN_POINT('Origin',(-5.43787237461402E-12,6.20000000004983,
130.056003483259)) ;
#112921 = CARTESIAN_POINT('Origin',(-18.6700795113902,6.2000000000496,121.553481994517)) ;
#112922 = CARTESIAN_POINT('',(5.47072336176247,6.2000000000496,134.423060375387)) ;
#112923 = CARTESIAN_POINT('Origin',(-1.33226762955019E-14,6.2000000000496,
130.056003483261)) ;
#112924 = CARTESIAN_POINT('',(-33.0324919366153,6.2000000000496,125.387266520802)) ;
#112925 = CARTESIAN_POINT('',(-34.9040877475781,6.2000000000496,127.731862247231)) ;
#112926 = CARTESIAN_POINT('Origin',(-33.9682898421302,6.2000000000496,126.55956438399)) ;
#112927 = CARTESIAN_POINT('',(-34.557234512772,6.2000000000496,123.661632554657)) ;
#112928 = CARTESIAN_POINT('Origin',(-28.8703041205576,6.20000000004974,120.173187866839)) ;
#112929 = CARTESIAN_POINT('',(-37.1144548939429,6.2000000000496,125.23027015529)) ;
#112930 = CARTESIAN_POINT('Origin',(-35.8358444062484,6.2000000000496,124.445951839326)) ;
#112931 = CARTESIAN_POINT('Origin',(-28.8703041205676,6.20000000004974,120.173187866851)) ;
#112932 = CARTESIAN_POINT('Origin',(-27.0022936957715,9.2000000000496,119.45866911073)) ;
#112933 = CARTESIAN_POINT('',(5.58795314825178,9.2000000000496,134.516640166064)) ;
#112934 = CARTESIAN_POINT('Ctrl Pts',(5.58795314825178,9.2000000000496,134.516640166064)) ;
#112935 = CARTESIAN_POINT('Ctrl Pts',(5.02776600408638,9.2000000000496,135.218925186777)) ;
#112936 = CARTESIAN_POINT('Ctrl Pts',(3.58102682874936,9.20000000004958,136.459065126737)) ;
#112937 = CARTESIAN_POINT('Ctrl Pts',(0.819706526786835,9.2000000000496,137.362239934218)) ;
#112938 = CARTESIAN_POINT('Ctrl Pts',(-2.07329727026273,9.20000000004959,
137.093448346514)) ;
#112939 = CARTESIAN_POINT('Ctrl Pts',(-4.56753011885253,9.20000000004959,
135.777900274175)) ;
#112940 = CARTESIAN_POINT('Ctrl Pts',(-6.40313455515177,9.2000000000496,133.637111179546)) ;
#112941 = CARTESIAN_POINT('Ctrl Pts',(-7.30617826165478,9.20000000004959,
130.875683925058)) ;
#112942 = CARTESIAN_POINT('Ctrl Pts',(-7.03751608684004,9.20000000004958,
127.982693648484)) ;
#112943 = CARTESIAN_POINT('Ctrl Pts',(-5.72184342923753,9.2000000000496,125.488474550351)) ;
#112944 = CARTESIAN_POINT('Ctrl Pts',(-3.5811627186061,9.20000000004957,123.652885698944)) ;
#112945 = CARTESIAN_POINT('Ctrl Pts',(-0.819600541308432,9.2000000000496,
122.749780638574)) ;
#112946 = CARTESIAN_POINT('Ctrl Pts',(2.07323217291338,9.20000000004958,123.018548271325)) ;
#112947 = CARTESIAN_POINT('Ctrl Pts',(4.56757555136914,9.20000000004958,124.334122518572)) ;
#112948 = CARTESIAN_POINT('Ctrl Pts',(6.4030863521721,9.20000000004959,126.474865718472)) ;
#112949 = CARTESIAN_POINT('Ctrl Pts',(7.30625034559879,9.20000000004959,129.236381983343)) ;
#112950 = CARTESIAN_POINT('Ctrl Pts',(7.03738575174059,9.2000000000496,132.129195828704)) ;
#112951 = CARTESIAN_POINT('Ctrl Pts',(6.14865293878678,9.20000000004959,133.814761812278)) ;
#112952 = CARTESIAN_POINT('Ctrl Pts',(5.58795314825178,9.2000000000496,134.516640166064)) ;
#112953 = CARTESIAN_POINT('',(-21.0817660968248,9.2000000000496,120.455179752781)) ;
#112954 = CARTESIAN_POINT('',(-16.2583934682522,9.2000000000496,122.651785427042)) ;
#112955 = CARTESIAN_POINT('Ctrl Pts',(-21.0817660968248,9.2000000000496,120.455179752781)) ;
#112956 = CARTESIAN_POINT('Ctrl Pts',(-20.9381930117988,9.2000000000496,120.13944913774)) ;
#112957 = CARTESIAN_POINT('Ctrl Pts',(-20.5249581888851,9.2000000000496,119.56540103953)) ;
#112958 = CARTESIAN_POINT('Ctrl Pts',(-19.6230264687625,9.20000000004958,
119.006828830265)) ;
#112959 = CARTESIAN_POINT('Ctrl Pts',(-18.5758907605794,9.2000000000496,118.83604139381)) ;
#112960 = CARTESIAN_POINT('Ctrl Pts',(-17.5431612788873,9.20000000004959,
119.078919711506)) ;
#112961 = CARTESIAN_POINT('Ctrl Pts',(-16.6819548364584,9.20000000004959,
119.698549065317)) ;
#112962 = CARTESIAN_POINT('Ctrl Pts',(-16.123420065397,9.2000000000496,120.60057414181)) ;
#112963 = CARTESIAN_POINT('Ctrl Pts',(-15.9526858401603,9.20000000004958,
121.647648458748)) ;
#112964 = CARTESIAN_POINT('Ctrl Pts',(-16.1144562107074,9.2000000000496,122.336195813076)) ;
#112965 = CARTESIAN_POINT('Ctrl Pts',(-16.2583934681596,9.2000000000496,122.651785427097)) ;
#112966 = CARTESIAN_POINT('',(-17.3851818756338,9.19999999991291,125.943430776977)) ;
#112967 = CARTESIAN_POINT('Origin',(-4.21641852046444,9.2000000000496,128.61264886444)) ;
#112968 = CARTESIAN_POINT('',(-22.5428381268374,9.2000000000496,124.723356175805)) ;
#112969 = CARTESIAN_POINT('Ctrl Pts',(-17.3851818731081,9.2000000000496,125.943430777582)) ;
#112970 = CARTESIAN_POINT('Ctrl Pts',(-17.4648341623564,9.20000000004959,
126.281003578961)) ;
#112971 = CARTESIAN_POINT('Ctrl Pts',(-17.7589736989414,9.20000000004959,
126.924250687851)) ;
#112972 = CARTESIAN_POINT('Ctrl Pts',(-18.5355338243201,9.2000000000496,127.647054501784)) ;
#112973 = CARTESIAN_POINT('Ctrl Pts',(-19.5297170934661,9.2000000000496,128.017558118363)) ;
#112974 = CARTESIAN_POINT('Ctrl Pts',(-20.5899333565814,9.2000000000496,127.979449233406)) ;
#112975 = CARTESIAN_POINT('Ctrl Pts',(-21.5549025420905,9.2000000000496,127.538495083066)) ;
#112976 = CARTESIAN_POINT('Ctrl Pts',(-22.2776843192047,9.2000000000496,126.761830817273)) ;
#112977 = CARTESIAN_POINT('Ctrl Pts',(-22.6481211896443,9.20000000004961,
125.767700230883)) ;
#112978 = CARTESIAN_POINT('Ctrl Pts',(-22.6228797294498,9.2000000000496,125.06085865435)) ;
#112979 = CARTESIAN_POINT('Ctrl Pts',(-22.5428381268374,9.2000000000496,124.723356175805)) ;
#112980 = CARTESIAN_POINT('Origin',(-5.46730784800664,9.2000000000496,128.184450336603)) ;
#112981 = CARTESIAN_POINT('',(-34.9976674182864,9.2000000000496,127.849092131696)) ;
#112982 = CARTESIAN_POINT('',(-37.2423156796051,9.2000000000496,125.308702418377)) ;
#112983 = CARTESIAN_POINT('Origin',(-30.6977563686737,9.2000000000496,121.787893254627)) ;
#112984 = CARTESIAN_POINT('',(-34.4293734856409,9.2000000000496,123.583200684669)) ;
#112985 = CARTESIAN_POINT('Ctrl Pts',(-37.2423156796052,9.2000000000496,125.308702418377)) ;
#112986 = CARTESIAN_POINT('Ctrl Pts',(-37.3035108477935,9.2000000000496,125.210394441041)) ;
#112987 = CARTESIAN_POINT('Ctrl Pts',(-37.3534324664497,9.20000000004957,
125.1053745779)) ;
#112988 = CARTESIAN_POINT('Ctrl Pts',(-37.4300532165178,9.20000000004957,
124.886985389158)) ;
#112989 = CARTESIAN_POINT('Ctrl Pts',(-37.4567166242111,9.20000000004957,
124.773812893931)) ;
#112990 = CARTESIAN_POINT('Ctrl Pts',(-37.4967079950417,9.20000000004957,
124.464620592181)) ;
#112991 = CARTESIAN_POINT('Ctrl Pts',(-37.489671697536,9.20000000004957,124.252609113297)) ;
#112992 = CARTESIAN_POINT('Ctrl Pts',(-37.3824674523358,9.20000000004957,
123.831470024454)) ;
#112993 = CARTESIAN_POINT('Ctrl Pts',(-37.2886173018908,9.20000000004956,
123.634993007773)) ;
#112994 = CARTESIAN_POINT('Ctrl Pts',(-37.035690031635,9.20000000004956,123.294197445114)) ;
#112995 = CARTESIAN_POINT('Ctrl Pts',(-36.8780104418293,9.20000000004958,
123.149398131845)) ;
#112996 = CARTESIAN_POINT('Ctrl Pts',(-36.5193687649608,9.20000000004958,
122.929404397955)) ;
#112997 = CARTESIAN_POINT('Ctrl Pts',(-36.3186607801125,9.20000000004958,
122.854370983339)) ;
#112998 = CARTESIAN_POINT('Ctrl Pts',(-35.9005416749946,9.20000000004958,
122.78339315007)) ;
#112999 = CARTESIAN_POINT('Ctrl Pts',(-35.6833683383588,9.20000000004958,
122.788791264233)) ;
#113000 = CARTESIAN_POINT('Ctrl Pts',(-35.2593825552086,9.20000000004958,
122.883888816214)) ;
#113001 = CARTESIAN_POINT('Ctrl Pts',(-35.0667355944975,9.20000000004958,
122.973751721585)) ;
#113002 = CARTESIAN_POINT('Ctrl Pts',(-34.8088104674519,9.20000000004958,
123.149773346661)) ;
#113003 = CARTESIAN_POINT('Ctrl Pts',(-34.7200310044914,9.20000000004958,
123.224791694348)) ;
#113004 = CARTESIAN_POINT('Ctrl Pts',(-34.5601404915692,9.20000000004958,
123.392015869226)) ;
#113005 = CARTESIAN_POINT('Ctrl Pts',(-34.4891960629546,9.2000000000496,123.484094170402)) ;
#113006 = CARTESIAN_POINT('Ctrl Pts',(-34.4293734856409,9.2000000000496,123.583200684669)) ;
#113007 = CARTESIAN_POINT('',(-32.9389121458628,9.2000000000496,125.270036734223)) ;
#113008 = CARTESIAN_POINT('Origin',(-30.0837635005368,9.20000000004981,121.24538010296)) ;
#113009 = CARTESIAN_POINT('Ctrl Pts',(-32.9389121456355,9.2000000000496,125.270036733944)) ;
#113010 = CARTESIAN_POINT('Ctrl Pts',(-32.5987066128391,9.2000000000496,125.537972355178)) ;
#113011 = CARTESIAN_POINT('Ctrl Pts',(-32.2656287248248,9.2000000000496,126.150548345613)) ;
#113012 = CARTESIAN_POINT('Ctrl Pts',(-32.3422999176508,9.2000000000496,127.029372379786)) ;
#113013 = CARTESIAN_POINT('Ctrl Pts',(-32.6448691671967,9.2000000000496,127.615804974768)) ;
#113014 = CARTESIAN_POINT('Ctrl Pts',(-33.1500786747586,9.2000000000496,128.041286812588)) ;
#113015 = CARTESIAN_POINT('Ctrl Pts',(-33.9896462617629,9.2000000000496,128.310218608482)) ;
#113016 = CARTESIAN_POINT('Ctrl Pts',(-34.6611211806255,9.20000000004961,
128.121705182437)) ;
#113017 = CARTESIAN_POINT('Ctrl Pts',(-34.9976674182864,9.2000000000496,127.849092131696)) ;
#113018 = CARTESIAN_POINT('',(-26.8621929121386,9.2000000000496,119.40508020332)) ;
#113019 = CARTESIAN_POINT('Ctrl Pts',(-26.8621929121386,9.2000000000496,119.40508020332)) ;
#113020 = CARTESIAN_POINT('Ctrl Pts',(-26.7615104285989,9.20000000004959,
119.667852759595)) ;
#113021 = CARTESIAN_POINT('Ctrl Pts',(-26.6651414372152,9.2000000000496,120.233557031884)) ;
#113022 = CARTESIAN_POINT('Ctrl Pts',(-26.8560141325428,9.2000000000496,121.072849900875)) ;
#113023 = CARTESIAN_POINT('Ctrl Pts',(-27.3536755345133,9.2000000000496,121.775201700263)) ;
#113024 = CARTESIAN_POINT('Ctrl Pts',(-28.0821610405967,9.2000000000496,122.233641256589)) ;
#113025 = CARTESIAN_POINT('Ctrl Pts',(-28.9306655937973,9.20000000004959,
122.378411352712)) ;
#113026 = CARTESIAN_POINT('Ctrl Pts',(-29.769968345177,9.20000000004959,122.187446863389)) ;
#113027 = CARTESIAN_POINT('Ctrl Pts',(-30.4723169970674,9.20000000004959,
121.689833204347)) ;
#113028 = CARTESIAN_POINT('Ctrl Pts',(-30.9307580101565,9.20000000004961,
120.961321719305)) ;
#113029 = CARTESIAN_POINT('Ctrl Pts',(-31.0755273221357,9.20000000004959,
120.112831708247)) ;
#113030 = CARTESIAN_POINT('Ctrl Pts',(-30.8845632771364,9.20000000004961,
119.27352063753)) ;
#113031 = CARTESIAN_POINT('Ctrl Pts',(-30.3869493696082,9.20000000004959,
118.571176652922)) ;
#113032 = CARTESIAN_POINT('Ctrl Pts',(-29.6584380217711,9.20000000004961,
118.112733056803)) ;
#113033 = CARTESIAN_POINT('Ctrl Pts',(-28.8099464114727,9.2000000000496,117.967965846063)) ;
#113034 = CARTESIAN_POINT('Ctrl Pts',(-27.9706124163009,9.20000000004959,
118.15891731463)) ;
#113035 = CARTESIAN_POINT('Ctrl Pts',(-27.2683350105885,9.2000000000496,118.656574828484)) ;
#113036 = CARTESIAN_POINT('Ctrl Pts',(-26.9625809346018,9.2000000000496,119.142176892536)) ;
#113037 = CARTESIAN_POINT('Ctrl Pts',(-26.8621929121386,9.2000000000496,119.40508020332)) ;
#113038 = CARTESIAN_POINT('Origin',(-28.8703041205685,6.2000000000496,120.173187866852)) ;
#113039 = CARTESIAN_POINT('',(-27.0022936957715,9.05000000004959,119.45866911073)) ;
#113040 = CARTESIAN_POINT('Origin',(-28.8703041205685,9.05000000004959,120.173187866852)) ;
#113041 = CARTESIAN_POINT('',(-27.0022936957716,6.2000000000496,119.45866911073)) ;
#113042 = CARTESIAN_POINT('Origin',(-18.6700795113902,6.2000000000496,121.553481994517)) ;
#113043 = CARTESIAN_POINT('',(-20.9452555485298,9.05000000004959,120.517347833308)) ;
#113044 = CARTESIAN_POINT('',(-20.9452555485298,6.2000000000496,120.517347833308)) ;
#113045 = CARTESIAN_POINT('',(-16.3949039990916,9.05000000004959,122.589617308188)) ;
#113046 = CARTESIAN_POINT('',(-16.3949039990916,6.2000000000496,122.589617308188)) ;
#113047 = CARTESIAN_POINT('Ctrl Pts',(-20.9452555485298,9.05000000004959,
120.517347833308)) ;
#113048 = CARTESIAN_POINT('Ctrl Pts',(-20.8098092259609,9.05000000004959,
120.219488731387)) ;
#113049 = CARTESIAN_POINT('Ctrl Pts',(-20.4199650586345,9.0500000000496,119.677933924817)) ;
#113050 = CARTESIAN_POINT('Ctrl Pts',(-19.5690860737905,9.05000000004958,
119.150979010872)) ;
#113051 = CARTESIAN_POINT('Ctrl Pts',(-18.5812221993204,9.05000000004961,
118.989858785028)) ;
#113052 = CARTESIAN_POINT('Ctrl Pts',(-17.606949105008,9.05000000004959,119.218989276765)) ;
#113053 = CARTESIAN_POINT('Ctrl Pts',(-16.7944901933067,9.05000000004959,
119.803545268697)) ;
#113054 = CARTESIAN_POINT('Ctrl Pts',(-16.2675706030868,9.05000000004959,
120.65451232145)) ;
#113055 = CARTESIAN_POINT('Ctrl Pts',(-16.1065005744166,9.05000000004958,
121.642318285021)) ;
#113056 = CARTESIAN_POINT('Ctrl Pts',(-16.2591141342633,9.0500000000496,122.291891253157)) ;
#113057 = CARTESIAN_POINT('Ctrl Pts',(-16.3949039990916,9.05000000004959,
122.589617308188)) ;
#113058 = CARTESIAN_POINT('Origin',(-4.34985381048136E-12,6.20000000004959,
130.056003483259)) ;
#113059 = CARTESIAN_POINT('',(-17.5311532747538,9.05000000004959,125.908900336264)) ;
#113060 = CARTESIAN_POINT('',(-17.5311532747538,6.2000000000496,125.908900336264)) ;
#113061 = CARTESIAN_POINT('Origin',(-6.26387830493513E-12,9.05000000005006,
130.056003483259)) ;
#113062 = CARTESIAN_POINT('Origin',(-19.9640098891908,6.2000000000496,125.333393000437)) ;
#113063 = CARTESIAN_POINT('',(-22.3968667215,9.05000000004959,124.757886585629)) ;
#113064 = CARTESIAN_POINT('',(-22.3968667215,6.2000000000496,124.757886585629)) ;
#113065 = CARTESIAN_POINT('Ctrl Pts',(-17.5311532747538,9.05000000004959,
125.908900336264)) ;
#113066 = CARTESIAN_POINT('Ctrl Pts',(-17.6062969361899,9.05000000004959,
126.227365244915)) ;
#113067 = CARTESIAN_POINT('Ctrl Pts',(-17.8837870704631,9.05000000004959,
126.834202139267)) ;
#113068 = CARTESIAN_POINT('Ctrl Pts',(-18.6163909589713,9.05000000004961,
127.516092529978)) ;
#113069 = CARTESIAN_POINT('Ctrl Pts',(-19.5542997048764,9.0500000000496,127.865624243821)) ;
#113070 = CARTESIAN_POINT('Ctrl Pts',(-20.5545037267052,9.0500000000496,127.829672465207)) ;
#113071 = CARTESIAN_POINT('Ctrl Pts',(-21.4648520142714,9.0500000000496,127.413677984308)) ;
#113072 = CARTESIAN_POINT('Ctrl Pts',(-22.1467216161347,9.05000000004959,
126.680975846054)) ;
#113073 = CARTESIAN_POINT('Ctrl Pts',(-22.4961903603291,9.05000000004961,
125.743116803329)) ;
#113074 = CARTESIAN_POINT('Ctrl Pts',(-22.4723776645545,9.05000000004959,
125.076285126214)) ;
#113075 = CARTESIAN_POINT('Ctrl Pts',(-22.3968667215,9.05000000004959,124.757886585629)) ;
#113076 = CARTESIAN_POINT('Origin',(-4.80682160741708E-11,6.2000000000496,
130.056003483246)) ;
#113077 = CARTESIAN_POINT('Ctrl Pts',(-22.3968667215,9.05000000004959,124.757886585629)) ;
#113078 = CARTESIAN_POINT('Ctrl Pts',(-22.2245939589431,9.049950612143,124.029633476594)) ;
#113079 = CARTESIAN_POINT('Ctrl Pts',(-22.0169038912293,9.05001239481549,
123.310215297127)) ;
#113080 = CARTESIAN_POINT('Ctrl Pts',(-21.5321687944225,9.05001239481544,
121.894176346136)) ;
#113081 = CARTESIAN_POINT('Ctrl Pts',(-21.2554130236569,9.04995061214263,
121.198400574409)) ;
#113082 = CARTESIAN_POINT('Ctrl Pts',(-20.9452555485298,9.05000000004959,
120.517347833308)) ;
#113083 = CARTESIAN_POINT('Origin',(-4.21884749357559E-14,6.2000000000496,
130.056003483261)) ;
#113084 = CARTESIAN_POINT('',(5.47072336176247,9.05000000004959,134.423060375387)) ;
#113085 = CARTESIAN_POINT('Origin',(-1.4432899320127E-14,9.05000000004959,
130.056003483261)) ;
#113086 = CARTESIAN_POINT('',(5.47072336176241,6.2000000000496,134.423060375387)) ;
#113087 = CARTESIAN_POINT('Origin',(-28.8703041205676,6.20000000004959,120.173187866851)) ;
#113088 = CARTESIAN_POINT('',(-34.9040876899405,9.04999999949199,127.731862293537)) ;
#113089 = CARTESIAN_POINT('',(-34.9040877475781,6.2000000000496,127.731862247231)) ;
#113090 = CARTESIAN_POINT('',(-37.1144547230141,9.04999999990636,125.230270433971)) ;
#113091 = CARTESIAN_POINT('',(-37.1144548939429,6.2000000000496,125.23027015529)) ;
#113092 = CARTESIAN_POINT('Ctrl Pts',(-34.9040876897959,9.04999999901832,
127.731862293356)) ;
#113093 = CARTESIAN_POINT('Ctrl Pts',(-35.3413645465505,9.04979412705185,
127.382801894057)) ;
#113094 = CARTESIAN_POINT('Ctrl Pts',(-35.7475313924077,9.05005211409003,
126.996450959224)) ;
#113095 = CARTESIAN_POINT('Ctrl Pts',(-36.4885024120155,9.05005211928734,
126.157853987428)) ;
#113096 = CARTESIAN_POINT('Ctrl Pts',(-36.8218973505677,9.04979413761622,
125.707202917238)) ;
#113097 = CARTESIAN_POINT('Ctrl Pts',(-37.1144546376467,9.0499999998019,125.230270573109)) ;
#113098 = CARTESIAN_POINT('Origin',(-35.8358444062483,6.2000000000496,124.445951839326)) ;
#113099 = CARTESIAN_POINT('',(-34.557234512772,9.05000000004959,123.661632554657)) ;
#113100 = CARTESIAN_POINT('',(-34.557234512772,6.2000000000496,123.661632554657)) ;
#113101 = CARTESIAN_POINT('Origin',(-35.8358444062484,9.05000000004959,124.445951839326)) ;
#113102 = CARTESIAN_POINT('Origin',(-28.8703041205587,6.20000000004959,120.17318786684)) ;
#113103 = CARTESIAN_POINT('',(-33.0324919366153,9.05000000004959,125.387266520802)) ;
#113104 = CARTESIAN_POINT('',(-33.0324919366153,6.2000000000496,125.387266520802)) ;
#113105 = CARTESIAN_POINT('Origin',(-28.8703041205587,9.05000000004948,120.17318786684)) ;
#113106 = CARTESIAN_POINT('Origin',(-33.9682898421302,6.2000000000496,126.55956438399)) ;
#113107 = CARTESIAN_POINT('Ctrl Pts',(-33.0324919366153,9.05000000004959,
125.387266520802)) ;
#113108 = CARTESIAN_POINT('Ctrl Pts',(-32.7232141786532,9.05000000004961,
125.630844357595)) ;
#113109 = CARTESIAN_POINT('Ctrl Pts',(-32.4204161032166,9.05000000004959,
126.187731618834)) ;
#113110 = CARTESIAN_POINT('Ctrl Pts',(-32.4901171977394,9.0500000000496,126.986662550358)) ;
#113111 = CARTESIAN_POINT('Ctrl Pts',(-32.7651801608489,9.0500000000496,127.519783083619)) ;
#113112 = CARTESIAN_POINT('Ctrl Pts',(-33.2244615410704,9.0500000000496,127.906584747446)) ;
#113113 = CARTESIAN_POINT('Ctrl Pts',(-33.98770481185,9.0500000000496,128.151068188889)) ;
#113114 = CARTESIAN_POINT('Ctrl Pts',(-34.5981365609726,9.0500000000496,127.979692345601)) ;
#113115 = CARTESIAN_POINT('Ctrl Pts',(-34.9040876850543,9.05000000004959,
127.731862297877)) ;
#113116 = CARTESIAN_POINT('Ctrl Pts',(-27.0096412809262,9.04213325052386,
119.46147958081)) ;
#113117 = CARTESIAN_POINT('Ctrl Pts',(-26.8621929121386,9.2000000000496,119.40508020332)) ;
#113118 = CARTESIAN_POINT('Ctrl Pts',(-26.9163515465784,9.04213325052386,
119.704957694364)) ;
#113119 = CARTESIAN_POINT('Ctrl Pts',(-26.7615104285989,9.20000000004959,
119.667852759595)) ;
#113120 = CARTESIAN_POINT('Ctrl Pts',(-26.8270585844507,9.04213325052387,
120.22912434222)) ;
#113121 = CARTESIAN_POINT('Ctrl Pts',(-26.6651414372152,9.2000000000496,120.233557031884)) ;
#113122 = CARTESIAN_POINT('Ctrl Pts',(-27.0039161850776,9.04213325052386,
121.006790961142)) ;
#113123 = CARTESIAN_POINT('Ctrl Pts',(-26.8560141325428,9.2000000000496,121.072849900875)) ;
#113124 = CARTESIAN_POINT('Ctrl Pts',(-27.4650361038947,9.04213325052387,
121.657571599361)) ;
#113125 = CARTESIAN_POINT('Ctrl Pts',(-27.3536755345133,9.2000000000496,121.775201700263)) ;
#113126 = CARTESIAN_POINT('Ctrl Pts',(-28.1400315464981,9.04213325052387,
122.082349592043)) ;
#113127 = CARTESIAN_POINT('Ctrl Pts',(-28.0821610405967,9.2000000000496,122.233641256589)) ;
#113128 = CARTESIAN_POINT('Ctrl Pts',(-28.9262334681465,9.04213325052386,
122.216489741491)) ;
#113129 = CARTESIAN_POINT('Ctrl Pts',(-28.9306655937973,9.20000000004959,
122.378411352712)) ;
#113130 = CARTESIAN_POINT('Ctrl Pts',(-29.7039092450077,9.04213325052386,
122.03954708619)) ;
#113131 = CARTESIAN_POINT('Ctrl Pts',(-29.769968345177,9.20000000004959,122.187446863389)) ;
#113132 = CARTESIAN_POINT('Ctrl Pts',(-30.3546869661086,9.04213325052386,
121.578471404859)) ;
#113133 = CARTESIAN_POINT('Ctrl Pts',(-30.4723169970674,9.20000000004959,
121.689833204347)) ;
#113134 = CARTESIAN_POINT('Ctrl Pts',(-30.7794663090683,9.04213325052388,
120.903451890977)) ;
#113135 = CARTESIAN_POINT('Ctrl Pts',(-30.9307580101565,9.20000000004961,
120.961321719305)) ;
#113136 = CARTESIAN_POINT('Ctrl Pts',(-30.9136057317632,9.04213325052386,
120.117263443625)) ;
#113137 = CARTESIAN_POINT('Ctrl Pts',(-31.0755273221357,9.20000000004959,
120.112831708247)) ;
#113138 = CARTESIAN_POINT('Ctrl Pts',(-30.7366634886015,9.04213325052388,
119.33957995907)) ;
#113139 = CARTESIAN_POINT('Ctrl Pts',(-30.8845632771364,9.20000000004961,
119.27352063753)) ;
#113140 = CARTESIAN_POINT('Ctrl Pts',(-30.2755875763735,9.04213325052386,
118.688806561695)) ;
#113141 = CARTESIAN_POINT('Ctrl Pts',(-30.3869493696082,9.20000000004959,
118.571176652922)) ;
#113142 = CARTESIAN_POINT('Ctrl Pts',(-29.6005681904104,9.04213325052388,
118.264024825605)) ;
#113143 = CARTESIAN_POINT('Ctrl Pts',(-29.6584380217711,9.20000000004961,
118.112733056803)) ;
#113144 = CARTESIAN_POINT('Ctrl Pts',(-28.8143782605279,9.04213325052386,
118.129887349728)) ;
#113145 = CARTESIAN_POINT('Ctrl Pts',(-28.8099464114727,9.2000000000496,117.967965846063)) ;
#113146 = CARTESIAN_POINT('Ctrl Pts',(-28.0366735347411,9.04213325052387,
118.306817939836)) ;
#113147 = CARTESIAN_POINT('Ctrl Pts',(-27.9706124163009,9.20000000004959,
118.15891731463)) ;
#113148 = CARTESIAN_POINT('Ctrl Pts',(-27.385961828654,9.04213325052387,118.7679342568)) ;
#113149 = CARTESIAN_POINT('Ctrl Pts',(-27.2683350105885,9.2000000000496,118.656574828484)) ;
#113150 = CARTESIAN_POINT('Ctrl Pts',(-27.1026581693672,9.04213325052387,
119.217880311326)) ;
#113151 = CARTESIAN_POINT('Ctrl Pts',(-26.9625809346018,9.2000000000496,119.142176892536)) ;
#113152 = CARTESIAN_POINT('Ctrl Pts',(-27.0096412809262,9.04213325052386,
119.46147958081)) ;
#113153 = CARTESIAN_POINT('Ctrl Pts',(-26.8621929121386,9.2000000000496,119.40508020332)) ;
#113154 = CARTESIAN_POINT('',(-27.0022936957715,9.05000000004959,119.45866911073)) ;
#113155 = CARTESIAN_POINT('Ctrl Pts',(-20.9452555485298,9.05000000004959,
120.517347833308)) ;
#113156 = CARTESIAN_POINT('Ctrl Pts',(-21.0817660968248,9.2000000000496,120.455179752781)) ;
#113157 = CARTESIAN_POINT('Ctrl Pts',(-20.8098092259609,9.05000000004959,
120.219488731387)) ;
#113158 = CARTESIAN_POINT('Ctrl Pts',(-20.9381930117988,9.2000000000496,120.13944913774)) ;
#113159 = CARTESIAN_POINT('Ctrl Pts',(-20.4199650586345,9.0500000000496,119.677933924817)) ;
#113160 = CARTESIAN_POINT('Ctrl Pts',(-20.5249581888851,9.2000000000496,119.56540103953)) ;
#113161 = CARTESIAN_POINT('Ctrl Pts',(-19.5690860737905,9.05000000004958,
119.150979010872)) ;
#113162 = CARTESIAN_POINT('Ctrl Pts',(-19.6230264687625,9.20000000004958,
119.006828830265)) ;
#113163 = CARTESIAN_POINT('Ctrl Pts',(-18.5812221993204,9.05000000004961,
118.989858785028)) ;
#113164 = CARTESIAN_POINT('Ctrl Pts',(-18.5758907605794,9.2000000000496,118.83604139381)) ;
#113165 = CARTESIAN_POINT('Ctrl Pts',(-17.606949105008,9.05000000004959,119.218989276765)) ;
#113166 = CARTESIAN_POINT('Ctrl Pts',(-17.5431612788873,9.20000000004959,
119.078919711506)) ;
#113167 = CARTESIAN_POINT('Ctrl Pts',(-16.7944901933067,9.05000000004959,
119.803545268697)) ;
#113168 = CARTESIAN_POINT('Ctrl Pts',(-16.6819548364584,9.20000000004959,
119.698549065317)) ;
#113169 = CARTESIAN_POINT('Ctrl Pts',(-16.2675706030868,9.05000000004959,
120.65451232145)) ;
#113170 = CARTESIAN_POINT('Ctrl Pts',(-16.123420065397,9.2000000000496,120.60057414181)) ;
#113171 = CARTESIAN_POINT('Ctrl Pts',(-16.1065005744166,9.05000000004958,
121.642318285021)) ;
#113172 = CARTESIAN_POINT('Ctrl Pts',(-15.9526858401603,9.20000000004958,
121.647648458748)) ;
#113173 = CARTESIAN_POINT('Ctrl Pts',(-16.2591141342633,9.0500000000496,122.291891253157)) ;
#113174 = CARTESIAN_POINT('Ctrl Pts',(-16.1144562107074,9.2000000000496,122.336195813076)) ;
#113175 = CARTESIAN_POINT('Ctrl Pts',(-16.3949039990916,9.05000000004959,
122.589617308188)) ;
#113176 = CARTESIAN_POINT('Ctrl Pts',(-16.2583934681596,9.2000000000496,122.651785427097)) ;
#113177 = CARTESIAN_POINT('',(-16.3949039990916,9.05000000004959,122.589617308188)) ;
#113178 = CARTESIAN_POINT('',(-21.0817660968248,9.2000000000496,120.455179752781)) ;
#113179 = CARTESIAN_POINT('Ctrl Pts',(-16.3949039990916,9.05000000004959,
122.589617308188)) ;
#113180 = CARTESIAN_POINT('Ctrl Pts',(-16.2583934683448,9.2000000000496,122.651785426988)) ;
#113181 = CARTESIAN_POINT('Ctrl Pts',(-16.8804331897068,9.0500000000496,123.655569656133)) ;
#113182 = CARTESIAN_POINT('Ctrl Pts',(-16.7398799486352,9.20000000004959,
123.708862229139)) ;
#113183 = CARTESIAN_POINT('Ctrl Pts',(-17.2615869582204,9.05000000004959,
124.769020077632)) ;
#113184 = CARTESIAN_POINT('Ctrl Pts',(-17.1178600783809,9.2000000000496,124.813041616962)) ;
#113185 = CARTESIAN_POINT('Ctrl Pts',(-17.5311532747538,9.05000000004959,
125.908900336264)) ;
#113186 = CARTESIAN_POINT('Ctrl Pts',(-17.3851818778934,9.2000000000496,125.943430776435)) ;
#113187 = CARTESIAN_POINT('',(-17.3851818755008,9.2000000000496,125.943430777009)) ;
#113188 = CARTESIAN_POINT('Ctrl Pts',(-17.5311532747538,9.05000000004959,
125.908900336264)) ;
#113189 = CARTESIAN_POINT('Ctrl Pts',(-17.3851818731081,9.2000000000496,125.943430777582)) ;
#113190 = CARTESIAN_POINT('Ctrl Pts',(-17.6062969361899,9.05000000004959,
126.227365244915)) ;
#113191 = CARTESIAN_POINT('Ctrl Pts',(-17.4648341623564,9.20000000004959,
126.281003578961)) ;
#113192 = CARTESIAN_POINT('Ctrl Pts',(-17.8837870704631,9.05000000004959,
126.834202139267)) ;
#113193 = CARTESIAN_POINT('Ctrl Pts',(-17.7589736989414,9.20000000004959,
126.924250687851)) ;
#113194 = CARTESIAN_POINT('Ctrl Pts',(-18.6163909589713,9.05000000004961,
127.516092529978)) ;
#113195 = CARTESIAN_POINT('Ctrl Pts',(-18.5355338243201,9.2000000000496,127.647054501784)) ;
#113196 = CARTESIAN_POINT('Ctrl Pts',(-19.5542997048764,9.0500000000496,127.865624243821)) ;
#113197 = CARTESIAN_POINT('Ctrl Pts',(-19.5297170934661,9.2000000000496,128.017558118363)) ;
#113198 = CARTESIAN_POINT('Ctrl Pts',(-20.5545037267052,9.0500000000496,127.829672465207)) ;
#113199 = CARTESIAN_POINT('Ctrl Pts',(-20.5899333565814,9.2000000000496,127.979449233406)) ;
#113200 = CARTESIAN_POINT('Ctrl Pts',(-21.4648520142714,9.0500000000496,127.413677984308)) ;
#113201 = CARTESIAN_POINT('Ctrl Pts',(-21.5549025420905,9.2000000000496,127.538495083066)) ;
#113202 = CARTESIAN_POINT('Ctrl Pts',(-22.1467216161347,9.05000000004959,
126.680975846054)) ;
#113203 = CARTESIAN_POINT('Ctrl Pts',(-22.2776843192047,9.2000000000496,126.761830817273)) ;
#113204 = CARTESIAN_POINT('Ctrl Pts',(-22.4961903603291,9.05000000004961,
125.743116803329)) ;
#113205 = CARTESIAN_POINT('Ctrl Pts',(-22.6481211896443,9.20000000004961,
125.767700230883)) ;
#113206 = CARTESIAN_POINT('Ctrl Pts',(-22.4723776645545,9.05000000004959,
125.076285126214)) ;
#113207 = CARTESIAN_POINT('Ctrl Pts',(-22.6228797294498,9.2000000000496,125.06085865435)) ;
#113208 = CARTESIAN_POINT('Ctrl Pts',(-22.3968667215,9.05000000004959,124.757886585629)) ;
#113209 = CARTESIAN_POINT('Ctrl Pts',(-22.5428381268374,9.2000000000496,124.723356175805)) ;
#113210 = CARTESIAN_POINT('',(-22.3968667215,9.05000000004959,124.757886585629)) ;
#113211 = CARTESIAN_POINT('Ctrl Pts',(-22.3968186600187,9.04995061214263,
124.75789795486)) ;
#113212 = CARTESIAN_POINT('Ctrl Pts',(-22.5428381268374,9.2000000000496,124.723356175805)) ;
#113213 = CARTESIAN_POINT('Ctrl Pts',(-22.0524359330944,9.04995061214263,
123.301650939299)) ;
#113214 = CARTESIAN_POINT('Ctrl Pts',(-22.1962101373909,9.2000000000496,123.257614912411)) ;
#113215 = CARTESIAN_POINT('Ctrl Pts',(-21.5654953531972,9.04995061214263,
121.879169191031)) ;
#113216 = CARTESIAN_POINT('Ctrl Pts',(-21.7060948744266,9.2000000000496,121.82585907834)) ;
#113217 = CARTESIAN_POINT('Ctrl Pts',(-20.9452106020614,9.04995061214263,
120.517368302317)) ;
#113218 = CARTESIAN_POINT('Ctrl Pts',(-21.0817660968248,9.2000000000496,120.455179752781)) ;
#113219 = CARTESIAN_POINT('Ctrl Pts',(5.45900038311354,9.0350000000496,134.413702396319)) ;
#113220 = CARTESIAN_POINT('Ctrl Pts',(5.58795314825178,9.2000000000496,134.516640166064)) ;
#113221 = CARTESIAN_POINT('Ctrl Pts',(4.91174063504482,9.0350000000496,135.099780839932)) ;
#113222 = CARTESIAN_POINT('Ctrl Pts',(5.02776600408638,9.2000000000496,135.218925186777)) ;
#113223 = CARTESIAN_POINT('Ctrl Pts',(3.49838774780947,9.03500000004959,136.311302165659)) ;
#113224 = CARTESIAN_POINT('Ctrl Pts',(3.58102682874936,9.20000000004958,136.459065126737)) ;
#113225 = CARTESIAN_POINT('Ctrl Pts',(0.800790222613687,9.03500000004959,
137.193634477665)) ;
#113226 = CARTESIAN_POINT('Ctrl Pts',(0.819706526786835,9.2000000000496,137.362239934218)) ;
#113227 = CARTESIAN_POINT('Ctrl Pts',(-2.02545194877293,9.03500000004959,
136.931045772719)) ;
#113228 = CARTESIAN_POINT('Ctrl Pts',(-2.07329727026273,9.20000000004959,
137.093448346514)) ;
#113229 = CARTESIAN_POINT('Ctrl Pts',(-4.46212557757601,9.0350000000496,135.645856502129)) ;
#113230 = CARTESIAN_POINT('Ctrl Pts',(-4.56753011885253,9.20000000004959,
135.777900274175)) ;
#113231 = CARTESIAN_POINT('Ctrl Pts',(-6.25536991162766,9.0350000000496,133.554470232605)) ;
#113232 = CARTESIAN_POINT('Ctrl Pts',(-6.40313455515177,9.2000000000496,133.637111179546)) ;
#113233 = CARTESIAN_POINT('Ctrl Pts',(-7.13757414785378,9.0350000000496,130.856768222766)) ;
#113234 = CARTESIAN_POINT('Ctrl Pts',(-7.30617826165478,9.20000000004959,
130.875683925058)) ;
#113235 = CARTESIAN_POINT('Ctrl Pts',(-6.87511186948821,9.03500000004958,
128.030539259957)) ;
#113236 = CARTESIAN_POINT('Ctrl Pts',(-7.03751608684004,9.20000000004958,
127.982693648484)) ;
#113237 = CARTESIAN_POINT('Ctrl Pts',(-5.58980088850994,9.03500000004961,
125.593879064238)) ;
#113238 = CARTESIAN_POINT('Ctrl Pts',(-5.72184342923753,9.2000000000496,125.488474550351)) ;
#113239 = CARTESIAN_POINT('Ctrl Pts',(-3.49852050212872,9.03500000004958,
123.800649955475)) ;
#113240 = CARTESIAN_POINT('Ctrl Pts',(-3.5811627186061,9.20000000004957,123.652885698944)) ;
#113241 = CARTESIAN_POINT('Ctrl Pts',(-0.800686682415543,9.03500000004961,
122.918385781163)) ;
#113242 = CARTESIAN_POINT('Ctrl Pts',(-0.819600541308432,9.2000000000496,
122.749780638574)) ;
#113243 = CARTESIAN_POINT('Ctrl Pts',(2.0253883534138,9.03500000004958,123.180951083883)) ;
#113244 = CARTESIAN_POINT('Ctrl Pts',(2.07323217291338,9.20000000004958,123.018548271325)) ;
#113245 = CARTESIAN_POINT('Ctrl Pts',(4.46216996178487,9.03500000004959,124.466165925497)) ;
#113246 = CARTESIAN_POINT('Ctrl Pts',(4.56757555136914,9.20000000004958,124.334122518572)) ;
#113247 = CARTESIAN_POINT('Ctrl Pts',(6.25532282093323,9.03500000004959,126.557507359097)) ;
#113248 = CARTESIAN_POINT('Ctrl Pts',(6.4030863521721,9.20000000004959,126.474865718472)) ;
#113249 = CARTESIAN_POINT('Ctrl Pts',(7.13764456841352,9.0350000000496,129.255296325887)) ;
#113250 = CARTESIAN_POINT('Ctrl Pts',(7.30625034559879,9.20000000004959,129.236381983343)) ;
#113251 = CARTESIAN_POINT('Ctrl Pts',(6.87498454206566,9.0350000000496,132.081352928266)) ;
#113252 = CARTESIAN_POINT('Ctrl Pts',(7.03738575174059,9.2000000000496,132.129195828704)) ;
#113253 = CARTESIAN_POINT('Ctrl Pts',(6.00676094790199,9.0350000000496,133.728021235528)) ;
#113254 = CARTESIAN_POINT('Ctrl Pts',(6.14865293878678,9.20000000004959,133.814761812278)) ;
#113255 = CARTESIAN_POINT('Ctrl Pts',(5.45900038311354,9.0350000000496,134.413702396319)) ;
#113256 = CARTESIAN_POINT('Ctrl Pts',(5.58795314825178,9.2000000000496,134.516640166064)) ;
#113257 = CARTESIAN_POINT('',(5.47072336176247,9.05000000004959,134.423060375387)) ;
#113258 = CARTESIAN_POINT('Ctrl Pts',(-34.9039592011489,9.04979412703026,
127.731701439515)) ;
#113259 = CARTESIAN_POINT('Ctrl Pts',(-34.9976674182864,9.2000000000496,127.849092131696)) ;
#113260 = CARTESIAN_POINT('Ctrl Pts',(-35.7782611147991,9.04979412703026,
127.03430818834)) ;
#113261 = CARTESIAN_POINT('Ctrl Pts',(-35.885548055222,9.2000000000496,127.140867712464)) ;
#113262 = CARTESIAN_POINT('Ctrl Pts',(-36.5298554822976,9.04979412703025,
126.183688247106)) ;
#113263 = CARTESIAN_POINT('Ctrl Pts',(-36.648815376531,9.20000000004959,126.277036858917)) ;
#113264 = CARTESIAN_POINT('Ctrl Pts',(-37.1142791502663,9.04979412703026,
125.230162926567)) ;
#113265 = CARTESIAN_POINT('Ctrl Pts',(-37.2423156796051,9.2000000000496,125.308702418377)) ;
#113266 = CARTESIAN_POINT('',(-37.1144546378578,9.05000000004959,125.230270573239)) ;
#113267 = CARTESIAN_POINT('',(-34.9976674182864,9.2000000000496,127.849092131696)) ;
#113268 = CARTESIAN_POINT('Ctrl Pts',(-37.1082337249472,9.04599943216395,
125.232675075925)) ;
#113269 = CARTESIAN_POINT('Ctrl Pts',(-37.2392155304809,9.2000000000496,125.313661591374)) ;
#113270 = CARTESIAN_POINT('Ctrl Pts',(-37.3179597355144,9.04599943216395,
124.898605624879)) ;
#113271 = CARTESIAN_POINT('Ctrl Pts',(-37.470531050067,9.2000000000496,124.945202526875)) ;
#113272 = CARTESIAN_POINT('Ctrl Pts',(-37.4144690154477,9.04599943216395,
124.271498541862)) ;
#113273 = CARTESIAN_POINT('Ctrl Pts',(-37.576975151988,9.20000000004958,124.253540041622)) ;
#113274 = CARTESIAN_POINT('Ctrl Pts',(-37.0774440110852,9.04599943216397,
123.544161120042)) ;
#113275 = CARTESIAN_POINT('Ctrl Pts',(-37.2052562543511,9.20000000004962,
123.451329344491)) ;
#113276 = CARTESIAN_POINT('Ctrl Pts',(-36.6386902271357,9.04599943216393,
123.13739949304)) ;
#113277 = CARTESIAN_POINT('Ctrl Pts',(-36.7213364569814,9.20000000004957,
123.002695027438)) ;
#113278 = CARTESIAN_POINT('Ctrl Pts',(-36.0767657044606,9.04599943216394,
122.930336957724)) ;
#113279 = CARTESIAN_POINT('Ctrl Pts',(-36.1015665274975,9.20000000004959,
122.774317144308)) ;
#113280 = CARTESIAN_POINT('Ctrl Pts',(-35.276205492832,9.04599943216394,122.95988896865)) ;
#113281 = CARTESIAN_POINT('Ctrl Pts',(-35.2185953694054,9.20000000004958,
122.806911285417)) ;
#113282 = CARTESIAN_POINT('Ctrl Pts',(-34.7604852661333,9.04599943216395,
123.329749691522)) ;
#113283 = CARTESIAN_POINT('Ctrl Pts',(-34.6497860829949,9.20000000004959,
123.214846063503)) ;
#113284 = CARTESIAN_POINT('Ctrl Pts',(-34.5579126235981,9.04599943216395,
123.668270050405)) ;
#113285 = CARTESIAN_POINT('Ctrl Pts',(-34.426360247948,9.2000000000496,123.588214307529)) ;
#113286 = CARTESIAN_POINT('',(-34.557234512772,9.05000000004959,123.661632554657)) ;
#113287 = CARTESIAN_POINT('Ctrl Pts',(-34.557234512772,9.05000000004959,123.661632554657)) ;
#113288 = CARTESIAN_POINT('Ctrl Pts',(-34.4293734856409,9.2000000000496,123.583200684669)) ;
#113289 = CARTESIAN_POINT('Ctrl Pts',(-34.1540823463917,9.05000000004959,
124.319401976811)) ;
#113290 = CARTESIAN_POINT('Ctrl Pts',(-34.0352854825652,9.20000000004958,
124.226181328024)) ;
#113291 = CARTESIAN_POINT('Ctrl Pts',(-33.6356107525321,9.0500000000496,124.906184432313)) ;
#113292 = CARTESIAN_POINT('Ctrl Pts',(-33.528470849969,9.2000000000496,124.799770967498)) ;
#113293 = CARTESIAN_POINT('Ctrl Pts',(-33.0324919366153,9.05000000004959,
125.387266520802)) ;
#113294 = CARTESIAN_POINT('Ctrl Pts',(-32.9389121460902,9.2000000000496,125.270036734502)) ;
#113295 = CARTESIAN_POINT('',(-32.9389121458628,9.2000000000496,125.270036734223)) ;
#113296 = CARTESIAN_POINT('Ctrl Pts',(-33.0324919366153,9.05000000004959,
125.387266520802)) ;
#113297 = CARTESIAN_POINT('Ctrl Pts',(-32.9389121456355,9.2000000000496,125.270036733944)) ;
#113298 = CARTESIAN_POINT('Ctrl Pts',(-32.7232141786936,9.05000000004961,
125.630844357562)) ;
#113299 = CARTESIAN_POINT('Ctrl Pts',(-32.5987066128391,9.2000000000496,125.537972355178)) ;
#113300 = CARTESIAN_POINT('Ctrl Pts',(-32.4204160994068,9.05000000004959,
126.18773162192)) ;
#113301 = CARTESIAN_POINT('Ctrl Pts',(-32.2656287248248,9.2000000000496,126.150548345613)) ;
#113302 = CARTESIAN_POINT('Ctrl Pts',(-32.4901171834901,9.0500000000496,126.9866625619)) ;
#113303 = CARTESIAN_POINT('Ctrl Pts',(-32.3422999176508,9.2000000000496,127.029372379786)) ;
#113304 = CARTESIAN_POINT('Ctrl Pts',(-32.7651801374046,9.0500000000496,127.51978310261)) ;
#113305 = CARTESIAN_POINT('Ctrl Pts',(-32.6448691671967,9.2000000000496,127.615804974768)) ;
#113306 = CARTESIAN_POINT('Ctrl Pts',(-33.2244615084222,9.0500000000496,127.906584773892)) ;
#113307 = CARTESIAN_POINT('Ctrl Pts',(-33.1500786747586,9.2000000000496,128.041286812588)) ;
#113308 = CARTESIAN_POINT('Ctrl Pts',(-33.9877047687723,9.0500000000496,128.151068223783)) ;
#113309 = CARTESIAN_POINT('Ctrl Pts',(-33.9896462617629,9.2000000000496,128.310218608482)) ;
#113310 = CARTESIAN_POINT('Ctrl Pts',(-34.5981365140358,9.0500000000496,127.979692383621)) ;
#113311 = CARTESIAN_POINT('Ctrl Pts',(-34.6611211806255,9.20000000004961,
128.121705182437)) ;
#113312 = CARTESIAN_POINT('Ctrl Pts',(-34.9040876381615,9.05000000004959,
127.731862335862)) ;
#113313 = CARTESIAN_POINT('Ctrl Pts',(-34.9976674182864,9.2000000000496,127.849092131696)) ;
#113314 = CARTESIAN_POINT('Origin',(-8.09169626799648,-6.19999999995041,87.0702317281296)) ;
#113315 = CARTESIAN_POINT('',(-23.3714287291853,-6.19999999995041,111.412782357318)) ;
#113316 = CARTESIAN_POINT('',(-2.77488334235144,-6.19999999995041,115.314903713015)) ;
#113317 = CARTESIAN_POINT('Origin',(-8.09169626799648,-6.19999999995041,87.0702317281297)) ;
#113318 = CARTESIAN_POINT('',(-2.77488334235144,-9.1999999999504,115.314903713015)) ;
#113319 = CARTESIAN_POINT('',(-2.77488334235144,-6.19999999995041,115.314903713015)) ;
#113320 = CARTESIAN_POINT('',(-23.3714287291853,-9.1999999999504,111.412782357318)) ;
#113321 = CARTESIAN_POINT('Origin',(-8.09169626799648,-9.19999999995042,87.0702317281297)) ;
#113322 = CARTESIAN_POINT('',(-23.3714287291853,-6.19999999995041,111.412782357318)) ;
#113323 = CARTESIAN_POINT('Origin',(-3.99680288865056E-14,-6.19999999995041,
130.056003483261)) ;
#113324 = CARTESIAN_POINT('',(-11.2264641357303,-6.19999999995041,140.004194424792)) ;
#113325 = CARTESIAN_POINT('Origin',(-8.32667268468867E-14,-6.19999999995041,
130.056003483261)) ;
#113326 = CARTESIAN_POINT('',(-11.2264641357303,-9.1999999999504,140.004194424792)) ;
#113327 = CARTESIAN_POINT('',(-11.2264641357303,-6.19999999995041,140.004194424792)) ;
#113328 = CARTESIAN_POINT('Origin',(-8.32667268468867E-14,-9.1999999999504,
130.056003483261)) ;
#113329 = CARTESIAN_POINT('Origin',(-32.7369214287718,-6.19999999995041,159.065417425019)) ;
#113330 = CARTESIAN_POINT('',(-29.8935702991225,-6.19999999995041,130.4656735525)) ;
#113331 = CARTESIAN_POINT('Origin',(-32.7369214287721,-6.19999999995039,159.06541742502)) ;
#113332 = CARTESIAN_POINT('',(-29.8935702991225,-9.1999999999504,130.4656735525)) ;
#113333 = CARTESIAN_POINT('',(-29.8935702991225,-6.19999999995041,130.4656735525)) ;
#113334 = CARTESIAN_POINT('Origin',(-32.7369214287721,-9.19999999995039,159.06541742502)) ;
#113335 = CARTESIAN_POINT('Origin',(-28.8703041205684,-6.19999999995041,120.173187866852)) ;
#113336 = CARTESIAN_POINT('Origin',(-28.8703041205685,-6.19999999995041,120.173187866852)) ;
#113337 = CARTESIAN_POINT('Origin',(-28.8703041205685,-9.1999999999504,120.173187866852)) ;
#113338 = CARTESIAN_POINT('Origin',(-27.8320398342445,-6.19999999995041,121.882575848483)) ;
#113339 = CARTESIAN_POINT('',(-27.8320398342445,-6.19999999995041,121.882575848483)) ;
#113340 = CARTESIAN_POINT('Origin',(-28.8703041205685,-6.19999999995041,120.173187866852)) ;
#113341 = CARTESIAN_POINT('',(-20.9452546314344,-6.19999999995041,120.517345819523)) ;
#113342 = CARTESIAN_POINT('',(-22.3968662121113,-6.19999999995041,124.757884432279)) ;
#113343 = CARTESIAN_POINT('Origin',(-4.52793358363124E-11,-6.19999999995017,
130.056003483244)) ;
#113344 = CARTESIAN_POINT('',(-16.3949039990916,-6.19999999995041,122.589617308188)) ;
#113345 = CARTESIAN_POINT('Origin',(-18.6700795113902,-6.19999999995041,121.553481994517)) ;
#113346 = CARTESIAN_POINT('',(-17.5311532747538,-6.19999999995041,125.908900336264)) ;
#113347 = CARTESIAN_POINT('Origin',(-5.38680211548126E-12,-6.19999999995041,
130.056003483259)) ;
#113348 = CARTESIAN_POINT('Origin',(-19.9640098891907,-6.19999999995041,125.333393000438)) ;
#113349 = CARTESIAN_POINT('',(6.99930913781763,-6.19999999995041,129.957659224341)) ;
#113350 = CARTESIAN_POINT('Origin',(-1.22124532708767E-14,-6.19999999995041,
130.056003483261)) ;
#113351 = CARTESIAN_POINT('',(-28.9640348151852,-6.19999999995041,113.502233048948)) ;
#113352 = CARTESIAN_POINT('',(-29.0061823547883,-6.19999999995041,110.502529132742)) ;
#113353 = CARTESIAN_POINT('Origin',(-28.9851085850295,-6.19999999995041,112.002381090846)) ;
#113354 = CARTESIAN_POINT('',(-31.2264258318076,-6.19999999995041,113.931464218094)) ;
#113355 = CARTESIAN_POINT('Origin',(-28.8703041205684,-6.19999999995041,120.173187866868)) ;
#113356 = CARTESIAN_POINT('',(-32.2858929448779,-6.19999999995041,111.124770534002)) ;
#113357 = CARTESIAN_POINT('Origin',(-31.7561588567387,-6.19999999995041,112.528117175379)) ;
#113358 = CARTESIAN_POINT('Origin',(-28.8703041205686,-6.19999999995048,120.173187866852)) ;
#113359 = CARTESIAN_POINT('',(-4.72036737313531,-6.19999999995041,119.695237805925)) ;
#113360 = CARTESIAN_POINT('Origin',(-5.67880467459402,-6.19999999995041,119.980541046657)) ;
#113361 = CARTESIAN_POINT('Origin',(-27.8320398342445,-9.1999999999504,121.882575848483)) ;
#113362 = CARTESIAN_POINT('',(7.14929433383964,-9.19999999995041,129.955551847362)) ;
#113363 = CARTESIAN_POINT('Ctrl Pts',(7.14929433383963,-9.1999999999504,129.955551847362)) ;
#113364 = CARTESIAN_POINT('Ctrl Pts',(7.1370004751631,-9.19999999995042,129.057296456148)) ;
#113365 = CARTESIAN_POINT('Ctrl Pts',(6.75374615451857,-9.1999999999504,127.19071738259)) ;
#113366 = CARTESIAN_POINT('Ctrl Pts',(5.12518384136061,-9.1999999999504,124.784808129301)) ;
#113367 = CARTESIAN_POINT('Ctrl Pts',(2.67435373485517,-9.19999999995041,
123.224310876368)) ;
#113368 = CARTESIAN_POINT('Ctrl Pts',(-0.102837066898579,-9.19999999995041,
122.735357418181)) ;
#113369 = CARTESIAN_POINT('Ctrl Pts',(-2.86529415935288,-9.19999999995041,
123.302148743622)) ;
#113370 = CARTESIAN_POINT('Ctrl Pts',(-5.27116535713755,-9.1999999999504,
124.93087591456)) ;
#113371 = CARTESIAN_POINT('Ctrl Pts',(-6.83175658899844,-9.19999999995038,
127.38161602962)) ;
#113372 = CARTESIAN_POINT('Ctrl Pts',(-7.32060317086497,-9.19999999995042,
130.158872314311)) ;
#113373 = CARTESIAN_POINT('Ctrl Pts',(-6.75388794178746,-9.19999999995039,
132.921250670983)) ;
#113374 = CARTESIAN_POINT('Ctrl Pts',(-5.12509175131467,-9.1999999999504,
135.327253035705)) ;
#113375 = CARTESIAN_POINT('Ctrl Pts',(-2.67441151797393,-9.1999999999504,
136.887664374679)) ;
#113376 = CARTESIAN_POINT('Ctrl Pts',(0.102882667250271,-9.19999999995039,
137.376664884276)) ;
#113377 = CARTESIAN_POINT('Ctrl Pts',(2.8652376417193,-9.19999999995039,136.809852443687)) ;
#113378 = CARTESIAN_POINT('Ctrl Pts',(5.27125844026773,-9.19999999995041,
135.181128649693)) ;
#113379 = CARTESIAN_POINT('Ctrl Pts',(6.83158159539024,-9.19999999995041,
132.73040390682)) ;
#113380 = CARTESIAN_POINT('Ctrl Pts',(7.16224251088857,-9.19999999995039,
130.853800044315)) ;
#113381 = CARTESIAN_POINT('Ctrl Pts',(7.14929433383963,-9.1999999999504,129.955551847362)) ;
#113382 = CARTESIAN_POINT('',(-22.5428375993846,-9.1999999999504,124.72335395111)) ;
#113383 = CARTESIAN_POINT('',(-17.3851818777868,-9.1999999999504,125.943430776449)) ;
#113384 = CARTESIAN_POINT('Ctrl Pts',(-22.5428375993846,-9.1999999999504,
124.72335395111)) ;
#113385 = CARTESIAN_POINT('Ctrl Pts',(-22.6228705779793,-9.19999999995041,
125.060835468167)) ;
#113386 = CARTESIAN_POINT('Ctrl Pts',(-22.6481146793898,-9.19999999995039,
125.767699651254)) ;
#113387 = CARTESIAN_POINT('Ctrl Pts',(-22.2776969349358,-9.19999999995041,
126.761819581242)) ;
#113388 = CARTESIAN_POINT('Ctrl Pts',(-21.5548924132103,-9.19999999995038,
127.538488856445)) ;
#113389 = CARTESIAN_POINT('Ctrl Pts',(-20.5899677472564,-9.19999999995041,
127.979442878113)) ;
#113390 = CARTESIAN_POINT('Ctrl Pts',(-19.5297019368864,-9.19999999995041,
128.017567454019)) ;
#113391 = CARTESIAN_POINT('Ctrl Pts',(-18.5355543800929,-9.1999999999504,
127.64705299455)) ;
#113392 = CARTESIAN_POINT('Ctrl Pts',(-17.7589647755576,-9.19999999995041,
126.924264376153)) ;
#113393 = CARTESIAN_POINT('Ctrl Pts',(-17.4648406712947,-9.1999999999504,
126.281024045295)) ;
#113394 = CARTESIAN_POINT('Ctrl Pts',(-17.3851818776801,-9.1999999999504,
125.943430776462)) ;
#113395 = CARTESIAN_POINT('',(-16.2583934662271,-9.19999999981371,122.651785427944)) ;
#113396 = CARTESIAN_POINT('Origin',(-4.21641852199826,-9.1999999999504,128.612648863915)) ;
#113397 = CARTESIAN_POINT('',(-21.081765150282,-9.1999999999504,120.455177671548)) ;
#113398 = CARTESIAN_POINT('Ctrl Pts',(-16.2583934638605,-9.1999999999504,
122.651785429014)) ;
#113399 = CARTESIAN_POINT('Ctrl Pts',(-16.1144636094565,-9.1999999999504,
122.336215974813)) ;
#113400 = CARTESIAN_POINT('Ctrl Pts',(-15.9527012801464,-9.19999999995041,
121.647653807036)) ;
#113401 = CARTESIAN_POINT('Ctrl Pts',(-16.123402898105,-9.1999999999504,120.600585547852)) ;
#113402 = CARTESIAN_POINT('Ctrl Pts',(-16.6819725346811,-9.1999999999504,
119.698547154189)) ;
#113403 = CARTESIAN_POINT('Ctrl Pts',(-17.5431302078255,-9.19999999995039,
119.078935764952)) ;
#113404 = CARTESIAN_POINT('Ctrl Pts',(-18.5758949488641,-9.1999999999504,
118.836030266143)) ;
#113405 = CARTESIAN_POINT('Ctrl Pts',(-19.6230096138486,-9.19999999995042,
119.006827682583)) ;
#113406 = CARTESIAN_POINT('Ctrl Pts',(-20.524962978159,-9.19999999995041,
119.565396591838)) ;
#113407 = CARTESIAN_POINT('Ctrl Pts',(-20.9381860344248,-9.19999999995041,
120.139425207325)) ;
#113408 = CARTESIAN_POINT('Ctrl Pts',(-21.081765150282,-9.1999999999504,120.455177671548)) ;
#113409 = CARTESIAN_POINT('Origin',(-5.46730600432587,-9.19999999995093,128.184444950592)) ;
#113410 = CARTESIAN_POINT('',(-4.57660177482253,-9.19999999995041,119.652442318957)) ;
#113411 = CARTESIAN_POINT('Ctrl Pts',(-4.57660177482253,-9.1999999999504,
119.652442318957)) ;
#113412 = CARTESIAN_POINT('Ctrl Pts',(-4.66090400079055,-9.19999999995039,
119.363676940337)) ;
#113413 = CARTESIAN_POINT('Ctrl Pts',(-5.07231914777193,-9.19999999995039,
118.859385893862)) ;
#113414 = CARTESIAN_POINT('Ctrl Pts',(-6.04236399869572,-9.19999999995039,
118.758213536859)) ;
#113415 = CARTESIAN_POINT('Ctrl Pts',(-6.80048159967586,-9.19999999995041,
119.373645566077)) ;
#113416 = CARTESIAN_POINT('Ctrl Pts',(-6.90081901473353,-9.1999999999504,
120.344304696983)) ;
#113417 = CARTESIAN_POINT('Ctrl Pts',(-6.28597182491173,-9.19999999995039,
121.102070939682)) ;
#113418 = CARTESIAN_POINT('Ctrl Pts',(-5.31469869100537,-9.19999999995039,
121.202705829313)) ;
#113419 = CARTESIAN_POINT('Ctrl Pts',(-4.55790335108104,-9.1999999999504,
120.587495567235)) ;
#113420 = CARTESIAN_POINT('Ctrl Pts',(-4.48925688934139,-9.19999999995039,
119.940301972492)) ;
#113421 = CARTESIAN_POINT('Ctrl Pts',(-4.57660177482253,-9.1999999999504,
119.652442318957)) ;
#113422 = CARTESIAN_POINT('',(-29.0082897317938,-9.19999999985937,110.352543935372)) ;
#113423 = CARTESIAN_POINT('',(-32.3388659738659,-9.1999999999504,110.984435725954)) ;
#113424 = CARTESIAN_POINT('Origin',(-29.3248670281959,-9.1999999999504,117.777304321592)) ;
#113425 = CARTESIAN_POINT('',(-31.1734524639126,-9.1999999999504,114.071798898544)) ;
#113426 = CARTESIAN_POINT('Ctrl Pts',(-32.3388659738659,-9.1999999999504,
110.984435725954)) ;
#113427 = CARTESIAN_POINT('Ctrl Pts',(-32.7450041950327,-9.1999999999504,
111.13470650637)) ;
#113428 = CARTESIAN_POINT('Ctrl Pts',(-33.250393360795,-9.1999999999504,111.615093587184)) ;
#113429 = CARTESIAN_POINT('Ctrl Pts',(-33.4478232528979,-9.1999999999504,
112.474879142272)) ;
#113430 = CARTESIAN_POINT('Ctrl Pts',(-33.3403541520526,-9.1999999999504,
113.125956337085)) ;
#113431 = CARTESIAN_POINT('Ctrl Pts',(-32.9905552298659,-9.19999999995041,
113.686234783214)) ;
#113432 = CARTESIAN_POINT('Ctrl Pts',(-32.2744514960019,-9.1999999999504,
114.200426654396)) ;
#113433 = CARTESIAN_POINT('Ctrl Pts',(-31.5775476849482,-9.1999999999504,
114.227645696731)) ;
#113434 = CARTESIAN_POINT('Ctrl Pts',(-31.1734524639126,-9.1999999999504,
114.071798898544)) ;
#113435 = CARTESIAN_POINT('',(-28.9619274381839,-9.19999999988973,113.652218245759)) ;
#113436 = CARTESIAN_POINT('Origin',(-29.1721385651905,-9.1999999999503,118.58228377673)) ;
#113437 = CARTESIAN_POINT('Ctrl Pts',(-28.9619274381555,-9.1999999999504,
113.652218246912)) ;
#113438 = CARTESIAN_POINT('Ctrl Pts',(-28.5288930381478,-9.19999999995042,
113.648976325215)) ;
#113439 = CARTESIAN_POINT('Ctrl Pts',(-27.8902872163334,-9.1999999999504,
113.369024853141)) ;
#113440 = CARTESIAN_POINT('Ctrl Pts',(-27.4123099953964,-9.19999999995041,
112.627574967391)) ;
#113441 = CARTESIAN_POINT('Ctrl Pts',(-27.2920262774471,-9.1999999999504,
111.978742812502)) ;
#113442 = CARTESIAN_POINT('Ctrl Pts',(-27.4305073144874,-9.1999999999504,
111.332914318425)) ;
#113443 = CARTESIAN_POINT('Ctrl Pts',(-27.9291423031889,-9.1999999999504,
110.605892050379)) ;
#113444 = CARTESIAN_POINT('Ctrl Pts',(-28.5752805886998,-9.1999999999504,
110.343363232169)) ;
#113445 = CARTESIAN_POINT('Ctrl Pts',(-29.0082897318249,-9.1999999999504,
110.352543933643)) ;
#113446 = CARTESIAN_POINT('',(-27.7541700117984,-9.19999999995041,122.010779948746)) ;
#113447 = CARTESIAN_POINT('Ctrl Pts',(-27.7541700117984,-9.1999999999504,
122.010779948746)) ;
#113448 = CARTESIAN_POINT('Ctrl Pts',(-27.5135754621942,-9.19999999995041,
121.864832555746)) ;
#113449 = CARTESIAN_POINT('Ctrl Pts',(-27.0907457483677,-9.19999999995038,
121.476859181283)) ;
#113450 = CARTESIAN_POINT('Ctrl Pts',(-26.7272384292546,-9.1999999999504,
120.696662196726)) ;
#113451 = CARTESIAN_POINT('Ctrl Pts',(-26.6900822991809,-9.1999999999504,
119.836671299616)) ;
#113452 = CARTESIAN_POINT('Ctrl Pts',(-26.9848031252087,-9.19999999995041,
119.027970122367)) ;
#113453 = CARTESIAN_POINT('Ctrl Pts',(-27.5665894666998,-9.1999999999504,
118.393586161041)) ;
#113454 = CARTESIAN_POINT('Ctrl Pts',(-28.3468505140607,-9.19999999995041,
118.030145323177)) ;
#113455 = CARTESIAN_POINT('Ctrl Pts',(-29.2068096659533,-9.19999999995039,
117.992953394567)) ;
#113456 = CARTESIAN_POINT('Ctrl Pts',(-30.0155279148894,-9.19999999995041,
118.287693856939)) ;
#113457 = CARTESIAN_POINT('Ctrl Pts',(-30.6499023447983,-9.1999999999504,
118.869469187485)) ;
#113458 = CARTESIAN_POINT('Ctrl Pts',(-31.0133486320491,-9.1999999999504,
119.649736536709)) ;
#113459 = CARTESIAN_POINT('Ctrl Pts',(-31.0505375041286,-9.1999999999504,
120.50969215252)) ;
#113460 = CARTESIAN_POINT('Ctrl Pts',(-30.755798733008,-9.19999999995039,
121.318412358944)) ;
#113461 = CARTESIAN_POINT('Ctrl Pts',(-30.1740208511346,-9.19999999995042,
121.95278610807)) ;
#113462 = CARTESIAN_POINT('Ctrl Pts',(-29.3937430936942,-9.1999999999504,
122.316256382307)) ;
#113463 = CARTESIAN_POINT('Ctrl Pts',(-28.5338133666822,-9.19999999995043,
122.353369994526)) ;
#113464 = CARTESIAN_POINT('Ctrl Pts',(-27.9946120019688,-9.1999999999504,
122.1570111193)) ;
#113465 = CARTESIAN_POINT('Ctrl Pts',(-27.7541700117984,-9.1999999999504,
122.010779948746)) ;
#113466 = CARTESIAN_POINT('Origin',(-28.8703041205685,-6.19999999995041,120.173187866852)) ;
#113467 = CARTESIAN_POINT('',(-27.8320398342445,-9.0499999999504,121.882575848483)) ;
#113468 = CARTESIAN_POINT('Origin',(-28.8703041205684,-9.0499999999504,120.173187866852)) ;
#113469 = CARTESIAN_POINT('',(-27.8320398342445,-6.19999999995041,121.882575848483)) ;
#113470 = CARTESIAN_POINT('Origin',(-19.9640098891909,-6.19999999995041,125.333393000438)) ;
#113471 = CARTESIAN_POINT('',(-22.3968662121113,-9.0499999999504,124.757884432279)) ;
#113472 = CARTESIAN_POINT('',(-22.3968662121113,-6.19999999995041,124.757884432279)) ;
#113473 = CARTESIAN_POINT('',(-17.5311532747538,-9.0499999999504,125.908900336264)) ;
#113474 = CARTESIAN_POINT('',(-17.5311532747538,-6.19999999995041,125.908900336264)) ;
#113475 = CARTESIAN_POINT('Ctrl Pts',(-22.3968662121113,-9.0499999999504,
124.757884432279)) ;
#113476 = CARTESIAN_POINT('Ctrl Pts',(-22.4723690285854,-9.04999999995042,
125.076263256322)) ;
#113477 = CARTESIAN_POINT('Ctrl Pts',(-22.4961842209104,-9.04999999995039,
125.743116253558)) ;
#113478 = CARTESIAN_POINT('Ctrl Pts',(-22.1467335154594,-9.04999999995042,
126.680965246019)) ;
#113479 = CARTESIAN_POINT('Ctrl Pts',(-21.4648424596514,-9.04999999995038,
127.4136721109)) ;
#113480 = CARTESIAN_POINT('Ctrl Pts',(-20.5545361708193,-9.04999999995042,
127.829666467211)) ;
#113481 = CARTESIAN_POINT('Ctrl Pts',(-19.5542854041389,-9.04999999995041,
127.865633052449)) ;
#113482 = CARTESIAN_POINT('Ctrl Pts',(-18.6164103552122,-9.04999999995039,
127.516091106774)) ;
#113483 = CARTESIAN_POINT('Ctrl Pts',(-17.8837786462394,-9.04999999995041,
126.834215051392)) ;
#113484 = CARTESIAN_POINT('Ctrl Pts',(-17.6063030831261,-9.0499999999504,
126.227384554924)) ;
#113485 = CARTESIAN_POINT('Ctrl Pts',(-17.5311532747538,-9.0499999999504,
125.908900336264)) ;
#113486 = CARTESIAN_POINT('Origin',(-5.63105118089879E-12,-6.19999999995041,
130.056003483259)) ;
#113487 = CARTESIAN_POINT('',(-16.3949039990916,-9.0499999999504,122.589617308188)) ;
#113488 = CARTESIAN_POINT('',(-16.3949039990916,-6.19999999995041,122.589617308188)) ;
#113489 = CARTESIAN_POINT('Origin',(-5.79536418854332E-12,-9.04999999995087,
130.056003483259)) ;
#113490 = CARTESIAN_POINT('Origin',(-18.6700795113902,-6.19999999995041,121.553481994517)) ;
#113491 = CARTESIAN_POINT('',(-20.9452546314344,-9.0499999999504,120.517345819523)) ;
#113492 = CARTESIAN_POINT('',(-20.9452546314344,-6.19999999995041,120.517345819523)) ;
#113493 = CARTESIAN_POINT('Ctrl Pts',(-16.3949039990916,-9.0499999999504,
122.589617308188)) ;
#113494 = CARTESIAN_POINT('Ctrl Pts',(-16.2591211104845,-9.0499999999504,
122.291910279286)) ;
#113495 = CARTESIAN_POINT('Ctrl Pts',(-16.1065151442268,-9.0499999999504,
121.642323325885)) ;
#113496 = CARTESIAN_POINT('Ctrl Pts',(-16.2675544036708,-9.04999999995041,
120.654523083266)) ;
#113497 = CARTESIAN_POINT('Ctrl Pts',(-16.7945068920798,-9.0499999999504,
119.803543465656)) ;
#113498 = CARTESIAN_POINT('Ctrl Pts',(-17.6069197915061,-9.04999999995039,
119.219004419472)) ;
#113499 = CARTESIAN_POINT('Ctrl Pts',(-18.5812261501238,-9.0499999999504,
118.989848288481)) ;
#113500 = CARTESIAN_POINT('Ctrl Pts',(-19.5690701747728,-9.04999999995041,
119.150977926698)) ;
#113501 = CARTESIAN_POINT('Ctrl Pts',(-20.419969573241,-9.04999999995041,
119.677929727982)) ;
#113502 = CARTESIAN_POINT('Ctrl Pts',(-20.8098026478821,-9.04999999995041,
120.219466157043)) ;
#113503 = CARTESIAN_POINT('Ctrl Pts',(-20.9452546314344,-9.0499999999504,
120.517345819523)) ;
#113504 = CARTESIAN_POINT('Origin',(-4.50262049866978E-11,-6.19999999995041,
130.056003483244)) ;
#113505 = CARTESIAN_POINT('Ctrl Pts',(-20.9452546314344,-9.0499999999504,
120.517345819523)) ;
#113506 = CARTESIAN_POINT('Ctrl Pts',(-21.2554121720413,-9.04995061204382,
121.198398530804)) ;
#113507 = CARTESIAN_POINT('Ctrl Pts',(-21.5321680097022,-9.05001239471631,
121.894174275922)) ;
#113508 = CARTESIAN_POINT('Ctrl Pts',(-22.0169032426545,-9.05001239471625,
123.310213180309)) ;
#113509 = CARTESIAN_POINT('Ctrl Pts',(-22.2245933795366,-9.04995061204343,
124.029631339807)) ;
#113510 = CARTESIAN_POINT('Ctrl Pts',(-22.3968662121113,-9.04999999995041,
124.757884432279)) ;
#113511 = CARTESIAN_POINT('Origin',(-3.33066907387547E-14,-6.19999999995041,
130.056003483261)) ;
#113512 = CARTESIAN_POINT('',(6.99930913781763,-9.0499999999504,129.957659224341)) ;
#113513 = CARTESIAN_POINT('Origin',(-8.88178419700125E-15,-9.0499999999504,
130.056003483261)) ;
#113514 = CARTESIAN_POINT('',(6.99930913781758,-6.19999999995041,129.957659224341)) ;
#113515 = CARTESIAN_POINT('Origin',(-28.8703041205686,-6.1999999999504,120.173187866852)) ;
#113516 = CARTESIAN_POINT('',(-29.0061823547883,-9.0499999999504,110.502529132742)) ;
#113517 = CARTESIAN_POINT('',(-29.0061823547883,-6.19999999995041,110.502529132742)) ;
#113518 = CARTESIAN_POINT('',(-32.2858926954066,-9.04999999991833,111.124770439505)) ;
#113519 = CARTESIAN_POINT('',(-32.2858929448779,-6.19999999995041,111.124770534002)) ;
#113520 = CARTESIAN_POINT('Ctrl Pts',(-29.0061823547883,-9.04999999995044,
110.502529132742)) ;
#113521 = CARTESIAN_POINT('Ctrl Pts',(-29.5656395665731,-9.04979411927751,
110.510389823533)) ;
#113522 = CARTESIAN_POINT('Ctrl Pts',(-30.1233656337281,-9.05005210980387,
110.566783181888)) ;
#113523 = CARTESIAN_POINT('Ctrl Pts',(-31.2228076802224,-9.0500521214643,
110.775374244021)) ;
#113524 = CARTESIAN_POINT('Ctrl Pts',(-31.7624325937661,-9.04979414280626,
110.927175193771)) ;
#113525 = CARTESIAN_POINT('Ctrl Pts',(-32.2858925706799,-9.04999999980325,
111.124770392751)) ;
#113526 = CARTESIAN_POINT('Origin',(-31.7561588567387,-6.19999999995041,112.528117175379)) ;
#113527 = CARTESIAN_POINT('',(-31.2264258318076,-9.0499999999504,113.931464218094)) ;
#113528 = CARTESIAN_POINT('',(-31.2264258318076,-6.19999999995041,113.931464218094)) ;
#113529 = CARTESIAN_POINT('Ctrl Pts',(-32.2858926956549,-9.0499999999504,
111.124770438834)) ;
#113530 = CARTESIAN_POINT('Ctrl Pts',(-32.655109233656,-9.0499999999504,111.261380268983)) ;
#113531 = CARTESIAN_POINT('Ctrl Pts',(-33.1145538702893,-9.04999999995041,
111.6980957759)) ;
#113532 = CARTESIAN_POINT('Ctrl Pts',(-33.2940355805978,-9.0499999999504,
112.479718963136)) ;
#113533 = CARTESIAN_POINT('Ctrl Pts',(-33.1963363978295,-9.0499999999504,
113.071607322719)) ;
#113534 = CARTESIAN_POINT('Ctrl Pts',(-32.878337377691,-9.04999999995041,
113.580951364404)) ;
#113535 = CARTESIAN_POINT('Ctrl Pts',(-32.2273339833429,-9.04999999995041,
114.048398519428)) ;
#113536 = CARTESIAN_POINT('Ctrl Pts',(-31.5937850640421,-9.0499999999504,
114.073143104941)) ;
#113537 = CARTESIAN_POINT('Ctrl Pts',(-31.2264258318076,-9.0499999999504,
113.931464218094)) ;
#113538 = CARTESIAN_POINT('Origin',(-28.8703041205683,-6.19999999995041,120.173187866869)) ;
#113539 = CARTESIAN_POINT('',(-28.9640348151852,-9.0499999999504,113.502233048948)) ;
#113540 = CARTESIAN_POINT('',(-28.9640348151852,-6.19999999995041,113.502233048948)) ;
#113541 = CARTESIAN_POINT('Origin',(-28.8703041205685,-9.04999999995033,120.173187866868)) ;
#113542 = CARTESIAN_POINT('Origin',(-28.9851085850296,-6.19999999995041,112.002381090846)) ;
#113543 = CARTESIAN_POINT('Ctrl Pts',(-28.9640348151852,-9.0499999999504,
113.502233048948)) ;
#113544 = CARTESIAN_POINT('Ctrl Pts',(-28.5703671785535,-9.04999999995041,
113.49928585092)) ;
#113545 = CARTESIAN_POINT('Ctrl Pts',(-27.9898164318432,-9.0499999999504,
113.244784510051)) ;
#113546 = CARTESIAN_POINT('Ctrl Pts',(-27.5552916853933,-9.0499999999504,
112.570739161072)) ;
#113547 = CARTESIAN_POINT('Ctrl Pts',(-27.4459428508496,-9.0499999999504,
111.980891746487)) ;
#113548 = CARTESIAN_POINT('Ctrl Pts',(-27.5718347027607,-9.04999999995039,
111.393774933819)) ;
#113549 = CARTESIAN_POINT('Ctrl Pts',(-28.0251392380631,-9.04999999995041,
110.732845600627)) ;
#113550 = CARTESIAN_POINT('Ctrl Pts',(-28.612537679088,-9.0499999999504,110.494183035205)) ;
#113551 = CARTESIAN_POINT('Ctrl Pts',(-29.0061823547883,-9.0499999999504,
110.502529132742)) ;
#113552 = CARTESIAN_POINT('Origin',(-5.67880467459403,-6.19999999995041,119.980541046657)) ;
#113553 = CARTESIAN_POINT('',(-4.72036737313531,-9.0499999999504,119.695237805925)) ;
#113554 = CARTESIAN_POINT('Ctrl Pts',(-4.72036737313531,-9.0499999999504,
119.695237805925)) ;
#113555 = CARTESIAN_POINT('Ctrl Pts',(-4.79367365129389,-9.04999999995039,
119.444137474753)) ;
#113556 = CARTESIAN_POINT('Ctrl Pts',(-5.15142595671263,-9.04999999995038,
119.005623523177)) ;
#113557 = CARTESIAN_POINT('Ctrl Pts',(-5.99494321694567,-9.04999999995039,
118.917647559852)) ;
#113558 = CARTESIAN_POINT('Ctrl Pts',(-6.65417591390635,-9.04999999995041,
119.452805846097)) ;
#113559 = CARTESIAN_POINT('Ctrl Pts',(-6.74142583978821,-9.0499999999504,
120.296857264431)) ;
#113560 = CARTESIAN_POINT('Ctrl Pts',(-6.2067761094534,-9.04999999995039,
120.955784431796)) ;
#113561 = CARTESIAN_POINT('Ctrl Pts',(-5.36219077623412,-9.04999999995039,
121.043293031702)) ;
#113562 = CARTESIAN_POINT('Ctrl Pts',(-4.70410787109404,-9.04999999995041,
120.508327585707)) ;
#113563 = CARTESIAN_POINT('Ctrl Pts',(-4.64441529656359,-9.0499999999504,
119.945550548028)) ;
#113564 = CARTESIAN_POINT('Ctrl Pts',(-4.72036737313531,-9.0499999999504,
119.695237805925)) ;
#113565 = CARTESIAN_POINT('',(-4.72036737313532,-6.19999999995041,119.695237805925)) ;
#113566 = CARTESIAN_POINT('Ctrl Pts',(-27.8361237168375,-9.04213325042268,
121.875852184848)) ;
#113567 = CARTESIAN_POINT('Ctrl Pts',(-27.7541700117984,-9.1999999999504,
122.010779948746)) ;
#113568 = CARTESIAN_POINT('Ctrl Pts',(-27.6131951563421,-9.04213325042269,
121.740621185333)) ;
#113569 = CARTESIAN_POINT('Ctrl Pts',(-27.5135754621942,-9.19999999995041,
121.864832555746)) ;
#113570 = CARTESIAN_POINT('Ctrl Pts',(-27.2214123048267,-9.04213325042267,
121.381135295391)) ;
#113571 = CARTESIAN_POINT('Ctrl Pts',(-27.0907457483677,-9.19999999995038,
121.476859181283)) ;
#113572 = CARTESIAN_POINT('Ctrl Pts',(-26.8845960173112,-9.04213325042268,
120.658225363553)) ;
#113573 = CARTESIAN_POINT('Ctrl Pts',(-26.7272384292546,-9.1999999999504,
120.696662196726)) ;
#113574 = CARTESIAN_POINT('Ctrl Pts',(-26.8501681278626,-9.04213325042268,
119.861380498453)) ;
#113575 = CARTESIAN_POINT('Ctrl Pts',(-26.6900822991809,-9.1999999999504,
119.836671299616)) ;
#113576 = CARTESIAN_POINT('Ctrl Pts',(-27.1232486667411,-9.04213325042269,
119.112059332406)) ;
#113577 = CARTESIAN_POINT('Ctrl Pts',(-26.9848031252087,-9.19999999995041,
119.027970122367)) ;
#113578 = CARTESIAN_POINT('Ctrl Pts',(-27.6623165339235,-9.04213325042267,
118.524255899387)) ;
#113579 = CARTESIAN_POINT('Ctrl Pts',(-27.5665894666998,-9.1999999999504,
118.393586161041)) ;
#113580 = CARTESIAN_POINT('Ctrl Pts',(-28.3852858260732,-9.04213325042269,
118.187501211538)) ;
#113581 = CARTESIAN_POINT('Ctrl Pts',(-28.3468505140607,-9.19999999995041,
118.030145323177)) ;
#113582 = CARTESIAN_POINT('Ctrl Pts',(-29.182101276225,-9.04213325042267,
118.15304015244)) ;
#113583 = CARTESIAN_POINT('Ctrl Pts',(-29.2068096659533,-9.19999999995039,
117.992953394567)) ;
#113584 = CARTESIAN_POINT('Ctrl Pts',(-29.9314382607409,-9.04213325042269,
118.426138885432)) ;
#113585 = CARTESIAN_POINT('Ctrl Pts',(-30.0155279148894,-9.19999999995041,
118.287693856939)) ;
#113586 = CARTESIAN_POINT('Ctrl Pts',(-30.5192328620952,-9.04213325042268,
118.965196550334)) ;
#113587 = CARTESIAN_POINT('Ctrl Pts',(-30.6499023447983,-9.1999999999504,
118.869469187485)) ;
#113588 = CARTESIAN_POINT('Ctrl Pts',(-30.8559925991121,-9.04213325042268,
119.688171680639)) ;
#113589 = CARTESIAN_POINT('Ctrl Pts',(-31.0133486320491,-9.1999999999504,
119.649736536709)) ;
#113590 = CARTESIAN_POINT('Ctrl Pts',(-30.8904508259688,-9.04213325042268,
120.484983855758)) ;
#113591 = CARTESIAN_POINT('Ctrl Pts',(-31.0505375041286,-9.1999999999504,
120.50969215252)) ;
#113592 = CARTESIAN_POINT('Ctrl Pts',(-30.61735366085,-9.04213325042268,121.23432265262)) ;
#113593 = CARTESIAN_POINT('Ctrl Pts',(-30.755798733008,-9.19999999995039,
121.318412358944)) ;
#113594 = CARTESIAN_POINT('Ctrl Pts',(-30.0782936311612,-9.04213325042269,
121.82211662443)) ;
#113595 = CARTESIAN_POINT('Ctrl Pts',(-30.1740208511346,-9.19999999995042,
121.95278610807)) ;
#113596 = CARTESIAN_POINT('Ctrl Pts',(-29.3553088569288,-9.04213325042268,
122.158898586878)) ;
#113597 = CARTESIAN_POINT('Ctrl Pts',(-29.3937430936942,-9.1999999999504,
122.316256382307)) ;
#113598 = CARTESIAN_POINT('Ctrl Pts',(-28.5585206705951,-9.0421332504227,
122.193287079418)) ;
#113599 = CARTESIAN_POINT('Ctrl Pts',(-28.5338133666822,-9.19999999995043,
122.353369994526)) ;
#113600 = CARTESIAN_POINT('Ctrl Pts',(-28.0589109164076,-9.04213325042268,
122.011346130603)) ;
#113601 = CARTESIAN_POINT('Ctrl Pts',(-27.9946120019688,-9.1999999999504,
122.1570111193)) ;
#113602 = CARTESIAN_POINT('Ctrl Pts',(-27.8361237168375,-9.04213325042268,
121.875852184848)) ;
#113603 = CARTESIAN_POINT('Ctrl Pts',(-27.7541700117984,-9.1999999999504,
122.010779948746)) ;
#113604 = CARTESIAN_POINT('',(-27.8320398342445,-9.0499999999504,121.882575848483)) ;
#113605 = CARTESIAN_POINT('Ctrl Pts',(-22.3968662121113,-9.0499999999504,
124.757884432279)) ;
#113606 = CARTESIAN_POINT('Ctrl Pts',(-22.5428375993846,-9.1999999999504,
124.72335395111)) ;
#113607 = CARTESIAN_POINT('Ctrl Pts',(-22.4723690285854,-9.04999999995042,
125.076263256322)) ;
#113608 = CARTESIAN_POINT('Ctrl Pts',(-22.6228705779793,-9.19999999995041,
125.060835468167)) ;
#113609 = CARTESIAN_POINT('Ctrl Pts',(-22.4961842209104,-9.04999999995039,
125.743116253558)) ;
#113610 = CARTESIAN_POINT('Ctrl Pts',(-22.6481146793898,-9.19999999995039,
125.767699651254)) ;
#113611 = CARTESIAN_POINT('Ctrl Pts',(-22.1467335154594,-9.04999999995042,
126.680965246019)) ;
#113612 = CARTESIAN_POINT('Ctrl Pts',(-22.2776969349358,-9.19999999995041,
126.761819581242)) ;
#113613 = CARTESIAN_POINT('Ctrl Pts',(-21.4648424596514,-9.04999999995038,
127.4136721109)) ;
#113614 = CARTESIAN_POINT('Ctrl Pts',(-21.5548924132103,-9.19999999995038,
127.538488856445)) ;
#113615 = CARTESIAN_POINT('Ctrl Pts',(-20.5545361708193,-9.04999999995042,
127.829666467211)) ;
#113616 = CARTESIAN_POINT('Ctrl Pts',(-20.5899677472564,-9.19999999995041,
127.979442878113)) ;
#113617 = CARTESIAN_POINT('Ctrl Pts',(-19.5542854041389,-9.04999999995041,
127.865633052449)) ;
#113618 = CARTESIAN_POINT('Ctrl Pts',(-19.5297019368864,-9.19999999995041,
128.017567454019)) ;
#113619 = CARTESIAN_POINT('Ctrl Pts',(-18.6164103552122,-9.04999999995039,
127.516091106774)) ;
#113620 = CARTESIAN_POINT('Ctrl Pts',(-18.5355543800929,-9.1999999999504,
127.64705299455)) ;
#113621 = CARTESIAN_POINT('Ctrl Pts',(-17.8837786462394,-9.04999999995041,
126.834215051392)) ;
#113622 = CARTESIAN_POINT('Ctrl Pts',(-17.7589647755576,-9.19999999995041,
126.924264376153)) ;
#113623 = CARTESIAN_POINT('Ctrl Pts',(-17.6063030831261,-9.0499999999504,
126.227384554924)) ;
#113624 = CARTESIAN_POINT('Ctrl Pts',(-17.4648406712947,-9.1999999999504,
126.281024045295)) ;
#113625 = CARTESIAN_POINT('Ctrl Pts',(-17.5311532747538,-9.0499999999504,
125.908900336264)) ;
#113626 = CARTESIAN_POINT('Ctrl Pts',(-17.3851818776801,-9.1999999999504,
125.943430776462)) ;
#113627 = CARTESIAN_POINT('',(-17.5311532747538,-9.0499999999504,125.908900336264)) ;
#113628 = CARTESIAN_POINT('',(-22.5428375993846,-9.1999999999504,124.72335395111)) ;
#113629 = CARTESIAN_POINT('Ctrl Pts',(-17.5311532747538,-9.0499999999504,
125.908900336264)) ;
#113630 = CARTESIAN_POINT('Ctrl Pts',(-17.3851818778934,-9.1999999999504,
125.943430776435)) ;
#113631 = CARTESIAN_POINT('Ctrl Pts',(-17.2615869582204,-9.0499999999504,
124.769020077632)) ;
#113632 = CARTESIAN_POINT('Ctrl Pts',(-17.1178600783809,-9.19999999995041,
124.813041616962)) ;
#113633 = CARTESIAN_POINT('Ctrl Pts',(-16.8804331897069,-9.04999999995041,
123.655569656133)) ;
#113634 = CARTESIAN_POINT('Ctrl Pts',(-16.7398799486353,-9.1999999999504,
123.708862229139)) ;
#113635 = CARTESIAN_POINT('Ctrl Pts',(-16.3949039990916,-9.0499999999504,
122.589617308188)) ;
#113636 = CARTESIAN_POINT('Ctrl Pts',(-16.2583934683448,-9.1999999999504,
122.651785426988)) ;
#113637 = CARTESIAN_POINT('',(-16.3949039990916,-9.0499999999504,122.589617308188)) ;
#113638 = CARTESIAN_POINT('Ctrl Pts',(-16.3949039990916,-9.0499999999504,
122.589617308188)) ;
#113639 = CARTESIAN_POINT('Ctrl Pts',(-16.2583934638605,-9.1999999999504,
122.651785429014)) ;
#113640 = CARTESIAN_POINT('Ctrl Pts',(-16.2591211104845,-9.0499999999504,
122.291910279286)) ;
#113641 = CARTESIAN_POINT('Ctrl Pts',(-16.1144636094565,-9.1999999999504,
122.336215974813)) ;
#113642 = CARTESIAN_POINT('Ctrl Pts',(-16.1065151442268,-9.0499999999504,
121.642323325885)) ;
#113643 = CARTESIAN_POINT('Ctrl Pts',(-15.9527012801464,-9.19999999995041,
121.647653807036)) ;
#113644 = CARTESIAN_POINT('Ctrl Pts',(-16.2675544036708,-9.04999999995041,
120.654523083266)) ;
#113645 = CARTESIAN_POINT('Ctrl Pts',(-16.123402898105,-9.1999999999504,120.600585547852)) ;
#113646 = CARTESIAN_POINT('Ctrl Pts',(-16.7945068920798,-9.0499999999504,
119.803543465656)) ;
#113647 = CARTESIAN_POINT('Ctrl Pts',(-16.6819725346811,-9.1999999999504,
119.698547154189)) ;
#113648 = CARTESIAN_POINT('Ctrl Pts',(-17.6069197915061,-9.04999999995039,
119.219004419472)) ;
#113649 = CARTESIAN_POINT('Ctrl Pts',(-17.5431302078255,-9.19999999995039,
119.078935764952)) ;
#113650 = CARTESIAN_POINT('Ctrl Pts',(-18.5812261501238,-9.0499999999504,
118.989848288481)) ;
#113651 = CARTESIAN_POINT('Ctrl Pts',(-18.5758949488641,-9.1999999999504,
118.836030266143)) ;
#113652 = CARTESIAN_POINT('Ctrl Pts',(-19.5690701747728,-9.04999999995041,
119.150977926698)) ;
#113653 = CARTESIAN_POINT('Ctrl Pts',(-19.6230096138486,-9.19999999995042,
119.006827682583)) ;
#113654 = CARTESIAN_POINT('Ctrl Pts',(-20.419969573241,-9.04999999995041,
119.677929727982)) ;
#113655 = CARTESIAN_POINT('Ctrl Pts',(-20.524962978159,-9.19999999995041,
119.565396591838)) ;
#113656 = CARTESIAN_POINT('Ctrl Pts',(-20.8098026478821,-9.04999999995041,
120.219466157043)) ;
#113657 = CARTESIAN_POINT('Ctrl Pts',(-20.9381860344248,-9.19999999995041,
120.139425207325)) ;
#113658 = CARTESIAN_POINT('Ctrl Pts',(-20.9452546314344,-9.0499999999504,
120.517345819523)) ;
#113659 = CARTESIAN_POINT('Ctrl Pts',(-21.081765150282,-9.1999999999504,120.455177671548)) ;
#113660 = CARTESIAN_POINT('',(-20.9452546314344,-9.0499999999504,120.517345819523)) ;
#113661 = CARTESIAN_POINT('Ctrl Pts',(-20.9452096849757,-9.04995061204342,
120.517366288554)) ;
#113662 = CARTESIAN_POINT('Ctrl Pts',(-21.081765150282,-9.1999999999504,120.455177671548)) ;
#113663 = CARTESIAN_POINT('Ctrl Pts',(-21.5654945670341,-9.04995061204342,
121.879167117613)) ;
#113664 = CARTESIAN_POINT('Ctrl Pts',(-21.706094083138,-9.1999999999504,121.825856991404)) ;
#113665 = CARTESIAN_POINT('Ctrl Pts',(-22.0524352836959,-9.04995061204342,
123.301648819064)) ;
#113666 = CARTESIAN_POINT('Ctrl Pts',(-22.1962094837586,-9.1999999999504,
123.257612778353)) ;
#113667 = CARTESIAN_POINT('Ctrl Pts',(-22.396818150636,-9.04995061204342,
124.757895801533)) ;
#113668 = CARTESIAN_POINT('Ctrl Pts',(-22.5428375993846,-9.1999999999504,
124.72335395111)) ;
#113669 = CARTESIAN_POINT('Ctrl Pts',(6.98431061821543,-9.0349999999504,129.957869962039)) ;
#113670 = CARTESIAN_POINT('Ctrl Pts',(7.14929433383963,-9.1999999999504,129.955551847362)) ;
#113671 = CARTESIAN_POINT('Ctrl Pts',(6.97230046451942,-9.03499999995042,
129.080343541437)) ;
#113672 = CARTESIAN_POINT('Ctrl Pts',(7.1370004751631,-9.19999999995042,129.057296456148)) ;
#113673 = CARTESIAN_POINT('Ctrl Pts',(6.59789047376578,-9.0349999999504,127.256839369418)) ;
#113674 = CARTESIAN_POINT('Ctrl Pts',(6.75374615451857,-9.1999999999504,127.19071738259)) ;
#113675 = CARTESIAN_POINT('Ctrl Pts',(5.00691036833316,-9.03499999995039,
124.90645109918)) ;
#113676 = CARTESIAN_POINT('Ctrl Pts',(5.12518384136061,-9.1999999999504,124.784808129301)) ;
#113677 = CARTESIAN_POINT('Ctrl Pts',(2.61263787931452,-9.03499999995041,
123.381965321084)) ;
#113678 = CARTESIAN_POINT('Ctrl Pts',(2.67435373485517,-9.19999999995041,
123.224310876368)) ;
#113679 = CARTESIAN_POINT('Ctrl Pts',(-0.100463903727752,-9.0349999999504,
122.904295404302)) ;
#113680 = CARTESIAN_POINT('Ctrl Pts',(-0.102837066898579,-9.19999999995041,
122.735357418181)) ;
#113681 = CARTESIAN_POINT('Ctrl Pts',(-2.7991719865524,-9.0349999999504,123.458006929968)) ;
#113682 = CARTESIAN_POINT('Ctrl Pts',(-2.86529415935288,-9.19999999995041,
123.302148743622)) ;
#113683 = CARTESIAN_POINT('Ctrl Pts',(-5.14952307947999,-9.03499999995039,
125.049148089099)) ;
#113684 = CARTESIAN_POINT('Ctrl Pts',(-5.27116535713755,-9.1999999999504,
124.93087591456)) ;
#113685 = CARTESIAN_POINT('Ctrl Pts',(-6.67410066780377,-9.03499999995039,
127.443332663221)) ;
#113686 = CARTESIAN_POINT('Ctrl Pts',(-6.83175658899844,-9.19999999995038,
127.38161602962)) ;
#113687 = CARTESIAN_POINT('Ctrl Pts',(-7.15166617454153,-9.03499999995041,
130.156498418203)) ;
#113688 = CARTESIAN_POINT('Ctrl Pts',(-7.32060317086497,-9.19999999995042,
130.158872314311)) ;
#113689 = CARTESIAN_POINT('Ctrl Pts',(-6.59802898938665,-9.03499999995039,
132.855129581994)) ;
#113690 = CARTESIAN_POINT('Ctrl Pts',(-6.75388794178746,-9.19999999995039,
132.921250670983)) ;
#113691 = CARTESIAN_POINT('Ctrl Pts',(-5.00682040300008,-9.0349999999504,
135.2056088154)) ;
#113692 = CARTESIAN_POINT('Ctrl Pts',(-5.12509175131467,-9.1999999999504,
135.327253035705)) ;
#113693 = CARTESIAN_POINT('Ctrl Pts',(-2.61269432921154,-9.0349999999504,
136.730010661744)) ;
#113694 = CARTESIAN_POINT('Ctrl Pts',(-2.67441151797393,-9.1999999999504,
136.887664374679)) ;
#113695 = CARTESIAN_POINT('Ctrl Pts',(0.100508451930804,-9.03499999995039,
137.207726544253)) ;
#113696 = CARTESIAN_POINT('Ctrl Pts',(0.102882667250271,-9.19999999995039,
137.376664884276)) ;
#113697 = CARTESIAN_POINT('Ctrl Pts',(2.79911677297535,-9.0349999999504,136.653994390812)) ;
#113698 = CARTESIAN_POINT('Ctrl Pts',(2.8652376417193,-9.19999999995039,136.809852443687)) ;
#113699 = CARTESIAN_POINT('Ctrl Pts',(5.14961401488543,-9.03499999995041,
135.062856530293)) ;
#113700 = CARTESIAN_POINT('Ctrl Pts',(5.27125844026773,-9.19999999995041,
135.181128649693)) ;
#113701 = CARTESIAN_POINT('Ctrl Pts',(6.67392971230693,-9.0349999999504,132.668686974082)) ;
#113702 = CARTESIAN_POINT('Ctrl Pts',(6.83158159539024,-9.19999999995041,
132.73040390682)) ;
#113703 = CARTESIAN_POINT('Ctrl Pts',(6.99695999145945,-9.0349999999504,130.835389354393)) ;
#113704 = CARTESIAN_POINT('Ctrl Pts',(7.16224251088857,-9.19999999995039,
130.853800044315)) ;
#113705 = CARTESIAN_POINT('Ctrl Pts',(6.98431061821543,-9.0349999999504,129.957869962039)) ;
#113706 = CARTESIAN_POINT('Ctrl Pts',(7.14929433383963,-9.1999999999504,129.955551847362)) ;
#113707 = CARTESIAN_POINT('',(6.99930913781763,-9.0499999999504,129.957659224341)) ;
#113708 = CARTESIAN_POINT('Ctrl Pts',(-29.0061794623337,-9.04979411927748,
110.502734993095)) ;
#113709 = CARTESIAN_POINT('Ctrl Pts',(-29.0082897317652,-9.1999999999504,
110.35254393692)) ;
#113710 = CARTESIAN_POINT('Ctrl Pts',(-30.1244489973375,-9.04979411927748,
110.518035751111)) ;
#113711 = CARTESIAN_POINT('Ctrl Pts',(-30.1439270242023,-9.19999999995041,
110.368082329788)) ;
#113712 = CARTESIAN_POINT('Ctrl Pts',(-31.2396537334849,-9.04979411927748,
110.729617347937)) ;
#113713 = CARTESIAN_POINT('Ctrl Pts',(-31.2764519194819,-9.1999999999504,
110.582949984148)) ;
#113714 = CARTESIAN_POINT('Ctrl Pts',(-32.2858198627326,-9.04979411927748,
111.12496300725)) ;
#113715 = CARTESIAN_POINT('Ctrl Pts',(-32.3388659738659,-9.1999999999504,
110.984435725954)) ;
#113716 = CARTESIAN_POINT('',(-32.2858925707319,-9.0499999999504,111.124770392613)) ;
#113717 = CARTESIAN_POINT('',(-29.0061823547883,-9.0499999999504,110.502529132742)) ;
#113718 = CARTESIAN_POINT('Ctrl Pts',(-32.2858925707319,-9.0499999999504,
111.124770392613)) ;
#113719 = CARTESIAN_POINT('Ctrl Pts',(-32.3388659738659,-9.1999999999504,
110.984435725954)) ;
#113720 = CARTESIAN_POINT('Ctrl Pts',(-32.6551091645665,-9.0499999999504,
111.261380203311)) ;
#113721 = CARTESIAN_POINT('Ctrl Pts',(-32.7450041950327,-9.1999999999504,
111.13470650637)) ;
#113722 = CARTESIAN_POINT('Ctrl Pts',(-33.1145538601681,-9.04999999995041,
111.698095731824)) ;
#113723 = CARTESIAN_POINT('Ctrl Pts',(-33.250393360795,-9.1999999999504,111.615093587184)) ;
#113724 = CARTESIAN_POINT('Ctrl Pts',(-33.2940355805978,-9.0499999999504,
112.479718963136)) ;
#113725 = CARTESIAN_POINT('Ctrl Pts',(-33.4478232528979,-9.1999999999504,
112.474879142272)) ;
#113726 = CARTESIAN_POINT('Ctrl Pts',(-33.1963363978295,-9.0499999999504,
113.071607322719)) ;
#113727 = CARTESIAN_POINT('Ctrl Pts',(-33.3403541520526,-9.1999999999504,
113.125956337085)) ;
#113728 = CARTESIAN_POINT('Ctrl Pts',(-32.878337377691,-9.04999999995041,
113.580951364404)) ;
#113729 = CARTESIAN_POINT('Ctrl Pts',(-32.9905552298659,-9.19999999995041,
113.686234783214)) ;
#113730 = CARTESIAN_POINT('Ctrl Pts',(-32.2273339833429,-9.04999999995041,
114.048398519428)) ;
#113731 = CARTESIAN_POINT('Ctrl Pts',(-32.2744514960019,-9.1999999999504,
114.200426654396)) ;
#113732 = CARTESIAN_POINT('Ctrl Pts',(-31.5937850640421,-9.0499999999504,
114.073143104941)) ;
#113733 = CARTESIAN_POINT('Ctrl Pts',(-31.5775476849482,-9.1999999999504,
114.227645696731)) ;
#113734 = CARTESIAN_POINT('Ctrl Pts',(-31.2264258318076,-9.0499999999504,
113.931464218094)) ;
#113735 = CARTESIAN_POINT('Ctrl Pts',(-31.1734524639126,-9.1999999999504,
114.071798898544)) ;
#113736 = CARTESIAN_POINT('',(-31.2264258318076,-9.0499999999504,113.931464218094)) ;
#113737 = CARTESIAN_POINT('Ctrl Pts',(-31.2264258318076,-9.0499999999504,
113.931464218094)) ;
#113738 = CARTESIAN_POINT('Ctrl Pts',(-31.1734524639126,-9.19999999995041,
114.071798898544)) ;
#113739 = CARTESIAN_POINT('Ctrl Pts',(-30.5047503325303,-9.0499999999504,
113.658743196313)) ;
#113740 = CARTESIAN_POINT('Ctrl Pts',(-30.4680025594377,-9.1999999999504,
113.805209524826)) ;
#113741 = CARTESIAN_POINT('Ctrl Pts',(-29.7354496684938,-9.04999999995041,
113.512787956471)) ;
#113742 = CARTESIAN_POINT('Ctrl Pts',(-29.7159983261929,-9.19999999995042,
113.662535842927)) ;
#113743 = CARTESIAN_POINT('Ctrl Pts',(-28.9640348151852,-9.0499999999504,
113.502233048948)) ;
#113744 = CARTESIAN_POINT('Ctrl Pts',(-28.9619274382105,-9.1999999999504,
113.652218244728)) ;
#113745 = CARTESIAN_POINT('',(-28.9640348151852,-9.0499999999504,113.502233048948)) ;
#113746 = CARTESIAN_POINT('Ctrl Pts',(-28.9640348151852,-9.0499999999504,
113.502233048948)) ;
#113747 = CARTESIAN_POINT('Ctrl Pts',(-28.9619274381555,-9.1999999999504,
113.652218246912)) ;
#113748 = CARTESIAN_POINT('Ctrl Pts',(-28.5703671785535,-9.04999999995041,
113.49928585092)) ;
#113749 = CARTESIAN_POINT('Ctrl Pts',(-28.5288930381478,-9.19999999995042,
113.648976325215)) ;
#113750 = CARTESIAN_POINT('Ctrl Pts',(-27.9898164318432,-9.0499999999504,
113.244784510051)) ;
#113751 = CARTESIAN_POINT('Ctrl Pts',(-27.8902872163334,-9.1999999999504,
113.369024853141)) ;
#113752 = CARTESIAN_POINT('Ctrl Pts',(-27.5552916853933,-9.0499999999504,
112.570739161072)) ;
#113753 = CARTESIAN_POINT('Ctrl Pts',(-27.4123099953964,-9.19999999995041,
112.627574967391)) ;
#113754 = CARTESIAN_POINT('Ctrl Pts',(-27.4459428508496,-9.0499999999504,
111.980891746487)) ;
#113755 = CARTESIAN_POINT('Ctrl Pts',(-27.2920262774471,-9.1999999999504,
111.978742812502)) ;
#113756 = CARTESIAN_POINT('Ctrl Pts',(-27.5718347027607,-9.04999999995039,
111.393774933819)) ;
#113757 = CARTESIAN_POINT('Ctrl Pts',(-27.4305073144874,-9.1999999999504,
111.332914318425)) ;
#113758 = CARTESIAN_POINT('Ctrl Pts',(-28.0251392380631,-9.04999999995041,
110.732845600627)) ;
#113759 = CARTESIAN_POINT('Ctrl Pts',(-27.9291423031889,-9.1999999999504,
110.605892050379)) ;
#113760 = CARTESIAN_POINT('Ctrl Pts',(-28.612537679088,-9.0499999999504,110.494183035205)) ;
#113761 = CARTESIAN_POINT('Ctrl Pts',(-28.5752805886998,-9.1999999999504,
110.343363232169)) ;
#113762 = CARTESIAN_POINT('Ctrl Pts',(-29.0061823547883,-9.0499999999504,
110.502529132742)) ;
#113763 = CARTESIAN_POINT('Ctrl Pts',(-29.0082897318249,-9.1999999999504,
110.352543933643)) ;
#113764 = CARTESIAN_POINT('Ctrl Pts',(-4.72036737313531,-9.0499999999504,
119.695237805925)) ;
#113765 = CARTESIAN_POINT('Ctrl Pts',(-4.57660177482253,-9.1999999999504,
119.652442318957)) ;
#113766 = CARTESIAN_POINT('Ctrl Pts',(-4.79367365129389,-9.04999999995039,
119.444137474753)) ;
#113767 = CARTESIAN_POINT('Ctrl Pts',(-4.66090400079055,-9.19999999995039,
119.363676940337)) ;
#113768 = CARTESIAN_POINT('Ctrl Pts',(-5.15142595671263,-9.04999999995038,
119.005623523177)) ;
#113769 = CARTESIAN_POINT('Ctrl Pts',(-5.07231914777193,-9.19999999995039,
118.859385893862)) ;
#113770 = CARTESIAN_POINT('Ctrl Pts',(-5.99494321694567,-9.04999999995039,
118.917647559852)) ;
#113771 = CARTESIAN_POINT('Ctrl Pts',(-6.04236399869572,-9.19999999995039,
118.758213536859)) ;
#113772 = CARTESIAN_POINT('Ctrl Pts',(-6.65417591390635,-9.04999999995041,
119.452805846097)) ;
#113773 = CARTESIAN_POINT('Ctrl Pts',(-6.80048159967586,-9.19999999995041,
119.373645566077)) ;
#113774 = CARTESIAN_POINT('Ctrl Pts',(-6.74142583978821,-9.0499999999504,
120.296857264431)) ;
#113775 = CARTESIAN_POINT('Ctrl Pts',(-6.90081901473353,-9.1999999999504,
120.344304696983)) ;
#113776 = CARTESIAN_POINT('Ctrl Pts',(-6.2067761094534,-9.04999999995039,
120.955784431796)) ;
#113777 = CARTESIAN_POINT('Ctrl Pts',(-6.28597182491173,-9.19999999995039,
121.102070939682)) ;
#113778 = CARTESIAN_POINT('Ctrl Pts',(-5.36219077623412,-9.04999999995039,
121.043293031702)) ;
#113779 = CARTESIAN_POINT('Ctrl Pts',(-5.31469869100537,-9.19999999995039,
121.202705829313)) ;
#113780 = CARTESIAN_POINT('Ctrl Pts',(-4.70410787109404,-9.04999999995041,
120.508327585707)) ;
#113781 = CARTESIAN_POINT('Ctrl Pts',(-4.55790335108104,-9.1999999999504,
120.587495567235)) ;
#113782 = CARTESIAN_POINT('Ctrl Pts',(-4.64441529656359,-9.0499999999504,
119.945550548028)) ;
#113783 = CARTESIAN_POINT('Ctrl Pts',(-4.48925688934139,-9.19999999995039,
119.940301972492)) ;
#113784 = CARTESIAN_POINT('Ctrl Pts',(-4.72036737313531,-9.0499999999504,
119.695237805925)) ;
#113785 = CARTESIAN_POINT('Ctrl Pts',(-4.57660177482253,-9.1999999999504,
119.652442318957)) ;
#113786 = CARTESIAN_POINT('',(-4.72036737313531,-9.0499999999504,119.695237805925)) ;
#113787 = CARTESIAN_POINT('Origin',(-28.8703041205685,-9.2000000000496,120.173187866852)) ;
#113788 = CARTESIAN_POINT('',(-30.0450876601579,-8.90000000004959,121.791793326842)) ;
#113789 = CARTESIAN_POINT('Origin',(-28.8703041205685,-8.90000000004959,120.173187866852)) ;
#113790 = CARTESIAN_POINT('',(-30.0450876601579,8.90000000004959,121.791793326842)) ;
#113791 = CARTESIAN_POINT('',(-30.0450876601579,-9.2000000000496,121.791793326842)) ;
#113792 = CARTESIAN_POINT('Origin',(-28.8703041205685,8.90000000004959,120.173187866852)) ;
#113793 = CARTESIAN_POINT('Origin',(-30.0450876601579,-9.2000000000496,121.791793326842)) ;
#113794 = CARTESIAN_POINT('',(-29.8688701292195,-9.2000000000496,121.549002507844)) ;
#113795 = CARTESIAN_POINT('Ctrl Pts',(-29.8688701292195,-9.2000000000496,
121.549002507844)) ;
#113796 = CARTESIAN_POINT('Ctrl Pts',(-29.6888722586779,-9.2000000000496,
121.679801257268)) ;
#113797 = CARTESIAN_POINT('Ctrl Pts',(-29.2766671363574,-9.2000000000496,
121.869462570365)) ;
#113798 = CARTESIAN_POINT('Ctrl Pts',(-28.5966094899589,-9.20000000004961,
121.895918474133)) ;
#113799 = CARTESIAN_POINT('Ctrl Pts',(-27.9581738536376,-9.20000000004958,
121.660008974116)) ;
#113800 = CARTESIAN_POINT('Ctrl Pts',(-27.4586313028868,-9.20000000004961,
121.197792875516)) ;
#113801 = CARTESIAN_POINT('Ctrl Pts',(-27.1739845654614,-9.20000000004959,
120.579569231899)) ;
#113802 = CARTESIAN_POINT('Ctrl Pts',(-27.1475967294287,-9.2000000000496,
119.899485204542)) ;
#113803 = CARTESIAN_POINT('Ctrl Pts',(-27.3834704179729,-9.20000000004961,
119.261061767752)) ;
#113804 = CARTESIAN_POINT('Ctrl Pts',(-27.8457060572027,-9.20000000004959,
118.761512772263)) ;
#113805 = CARTESIAN_POINT('Ctrl Pts',(-28.4639187630298,-9.20000000004959,
118.476869616603)) ;
#113806 = CARTESIAN_POINT('Ctrl Pts',(-29.1440090539224,-9.2000000000496,
118.450479738512)) ;
#113807 = CARTESIAN_POINT('Ctrl Pts',(-29.7824289744744,-9.20000000004958,
118.686354577768)) ;
#113808 = CARTESIAN_POINT('Ctrl Pts',(-30.2819799090915,-9.2000000000496,
119.148589579807)) ;
#113809 = CARTESIAN_POINT('Ctrl Pts',(-30.5666217872644,-9.2000000000496,
119.766803935434)) ;
#113810 = CARTESIAN_POINT('Ctrl Pts',(-30.593025972774,-9.20000000004959,
120.446909151552)) ;
#113811 = CARTESIAN_POINT('Ctrl Pts',(-30.3571041737437,-9.2000000000496,
121.085287178393)) ;
#113812 = CARTESIAN_POINT('Ctrl Pts',(-30.0490282665823,-9.20000000004959,
121.418401787627)) ;
#113813 = CARTESIAN_POINT('Ctrl Pts',(-29.8688701292195,-9.2000000000496,
121.549002507844)) ;
#113814 = CARTESIAN_POINT('Origin',(-30.0450876601579,9.2000000000496,121.791793326842)) ;
#113815 = CARTESIAN_POINT('',(-29.8688701292195,9.2000000000496,121.549002507844)) ;
#113816 = CARTESIAN_POINT('Ctrl Pts',(-29.8688701292195,9.2000000000496,121.549002507844)) ;
#113817 = CARTESIAN_POINT('Ctrl Pts',(-29.6888722586779,9.2000000000496,121.679801257268)) ;
#113818 = CARTESIAN_POINT('Ctrl Pts',(-29.2766671363573,9.20000000004959,
121.869462570365)) ;
#113819 = CARTESIAN_POINT('Ctrl Pts',(-28.5966094899589,9.20000000004961,
121.895918474133)) ;
#113820 = CARTESIAN_POINT('Ctrl Pts',(-27.9581738536375,9.20000000004957,
121.660008974116)) ;
#113821 = CARTESIAN_POINT('Ctrl Pts',(-27.4586313028868,9.20000000004962,
121.197792875516)) ;
#113822 = CARTESIAN_POINT('Ctrl Pts',(-27.1739845654613,9.20000000004957,
120.579569231898)) ;
#113823 = CARTESIAN_POINT('Ctrl Pts',(-27.1475967294288,9.20000000004963,
119.899485204542)) ;
#113824 = CARTESIAN_POINT('Ctrl Pts',(-27.3834704179728,9.20000000004958,
119.261061767752)) ;
#113825 = CARTESIAN_POINT('Ctrl Pts',(-27.8457060572028,9.2000000000496,118.761512772263)) ;
#113826 = CARTESIAN_POINT('Ctrl Pts',(-28.4639187630298,9.20000000004957,
118.476869616603)) ;
#113827 = CARTESIAN_POINT('Ctrl Pts',(-29.1440090539225,9.20000000004963,
118.450479738513)) ;
#113828 = CARTESIAN_POINT('Ctrl Pts',(-29.7824289744743,9.20000000004957,
118.686354577768)) ;
#113829 = CARTESIAN_POINT('Ctrl Pts',(-30.2819799090916,9.2000000000496,119.148589579807)) ;
#113830 = CARTESIAN_POINT('Ctrl Pts',(-30.5666217872643,9.2000000000496,119.766803935434)) ;
#113831 = CARTESIAN_POINT('Ctrl Pts',(-30.593025972774,9.20000000004959,120.446909151552)) ;
#113832 = CARTESIAN_POINT('Ctrl Pts',(-30.3571041737438,9.2000000000496,121.085287178393)) ;
#113833 = CARTESIAN_POINT('Ctrl Pts',(-30.0490282665823,9.2000000000496,121.418401787627)) ;
#113834 = CARTESIAN_POINT('Ctrl Pts',(-29.8688701292195,9.2000000000496,121.549002507844)) ;
#113835 = CARTESIAN_POINT('Ctrl Pts',(-30.0450876601579,-8.90000000004959,
121.791793326842)) ;
#113836 = CARTESIAN_POINT('Ctrl Pts',(-29.8333254600702,-8.90000000004959,
121.945674208536)) ;
#113837 = CARTESIAN_POINT('Ctrl Pts',(-29.3483782557085,-8.9000000000496,
122.168805164942)) ;
#113838 = CARTESIAN_POINT('Ctrl Pts',(-28.548310438228,-8.90000000004961,
122.199929757708)) ;
#113839 = CARTESIAN_POINT('Ctrl Pts',(-27.7972096887258,-8.90000000004958,
121.922389169964)) ;
#113840 = CARTESIAN_POINT('Ctrl Pts',(-27.2095125702208,-8.9000000000496,
121.378605523632)) ;
#113841 = CARTESIAN_POINT('Ctrl Pts',(-26.8746340558794,-8.90000000004959,
120.651283590262)) ;
#113842 = CARTESIAN_POINT('Ctrl Pts',(-26.8435895428338,-8.90000000004959,
119.851184734958)) ;
#113843 = CARTESIAN_POINT('Ctrl Pts',(-27.1210879996609,-8.90000000004961,
119.100098338637)) ;
#113844 = CARTESIAN_POINT('Ctrl Pts',(-27.6648946349492,-8.90000000004958,
118.512393637684)) ;
#113845 = CARTESIAN_POINT('Ctrl Pts',(-28.3922036993925,-8.90000000004959,
118.177519337191)) ;
#113846 = CARTESIAN_POINT('Ctrl Pts',(-29.1923099252244,-8.9000000000496,
118.146472421837)) ;
#113847 = CARTESIAN_POINT('Ctrl Pts',(-29.9433921833963,-8.90000000004959,
118.423972232679)) ;
#113848 = CARTESIAN_POINT('Ctrl Pts',(-30.5310991659206,-8.90000000004959,
118.967778117292)) ;
#113849 = CARTESIAN_POINT('Ctrl Pts',(-30.8659719637261,-8.90000000004961,
119.695089123834)) ;
#113850 = CARTESIAN_POINT('Ctrl Pts',(-30.8970357112146,-8.90000000004959,
120.495212908351)) ;
#113851 = CARTESIAN_POINT('Ctrl Pts',(-30.619480653913,-8.9000000000496,121.246245879451)) ;
#113852 = CARTESIAN_POINT('Ctrl Pts',(-30.2570384098916,-8.90000000004959,
121.63814542126)) ;
#113853 = CARTESIAN_POINT('Ctrl Pts',(-30.0450876601579,-8.90000000004959,
121.791793326842)) ;
#113854 = CARTESIAN_POINT('Ctrl Pts',(-29.8688701292195,-9.2000000000496,
121.549002507844)) ;
#113855 = CARTESIAN_POINT('Ctrl Pts',(-29.6888722586779,-9.2000000000496,
121.679801257268)) ;
#113856 = CARTESIAN_POINT('Ctrl Pts',(-29.2766671363574,-9.2000000000496,
121.869462570365)) ;
#113857 = CARTESIAN_POINT('Ctrl Pts',(-28.5966094899589,-9.20000000004961,
121.895918474133)) ;
#113858 = CARTESIAN_POINT('Ctrl Pts',(-27.9581738536376,-9.20000000004958,
121.660008974116)) ;
#113859 = CARTESIAN_POINT('Ctrl Pts',(-27.4586313028868,-9.20000000004961,
121.197792875516)) ;
#113860 = CARTESIAN_POINT('Ctrl Pts',(-27.1739845654614,-9.20000000004959,
120.579569231899)) ;
#113861 = CARTESIAN_POINT('Ctrl Pts',(-27.1475967294287,-9.2000000000496,
119.899485204542)) ;
#113862 = CARTESIAN_POINT('Ctrl Pts',(-27.3834704179729,-9.20000000004961,
119.261061767752)) ;
#113863 = CARTESIAN_POINT('Ctrl Pts',(-27.8457060572027,-9.20000000004959,
118.761512772263)) ;
#113864 = CARTESIAN_POINT('Ctrl Pts',(-28.4639187630298,-9.20000000004959,
118.476869616603)) ;
#113865 = CARTESIAN_POINT('Ctrl Pts',(-29.1440090539224,-9.2000000000496,
118.450479738512)) ;
#113866 = CARTESIAN_POINT('Ctrl Pts',(-29.7824289744744,-9.20000000004958,
118.686354577768)) ;
#113867 = CARTESIAN_POINT('Ctrl Pts',(-30.2819799090915,-9.2000000000496,
119.148589579807)) ;
#113868 = CARTESIAN_POINT('Ctrl Pts',(-30.5666217872644,-9.2000000000496,
119.766803935434)) ;
#113869 = CARTESIAN_POINT('Ctrl Pts',(-30.593025972774,-9.20000000004959,
120.446909151552)) ;
#113870 = CARTESIAN_POINT('Ctrl Pts',(-30.3571041737437,-9.2000000000496,
121.085287178393)) ;
#113871 = CARTESIAN_POINT('Ctrl Pts',(-30.0490282665823,-9.20000000004959,
121.418401787627)) ;
#113872 = CARTESIAN_POINT('Ctrl Pts',(-29.8688701292195,-9.2000000000496,
121.549002507844)) ;
#113873 = CARTESIAN_POINT('',(-30.0450876601579,-8.90000000004959,121.791793326842)) ;
#113874 = CARTESIAN_POINT('Ctrl Pts',(-30.0450876601579,8.90000000004959,
121.791793326842)) ;
#113875 = CARTESIAN_POINT('Ctrl Pts',(-29.8688701292195,9.2000000000496,121.549002507844)) ;
#113876 = CARTESIAN_POINT('Ctrl Pts',(-29.8333254600701,8.9000000000496,121.945674208536)) ;
#113877 = CARTESIAN_POINT('Ctrl Pts',(-29.6888722586779,9.2000000000496,121.679801257268)) ;
#113878 = CARTESIAN_POINT('Ctrl Pts',(-29.3483782557084,8.90000000004959,
122.168805164942)) ;
#113879 = CARTESIAN_POINT('Ctrl Pts',(-29.2766671363573,9.20000000004959,
121.869462570365)) ;
#113880 = CARTESIAN_POINT('Ctrl Pts',(-28.548310438228,8.90000000004961,122.199929757709)) ;
#113881 = CARTESIAN_POINT('Ctrl Pts',(-28.5966094899589,9.20000000004961,
121.895918474133)) ;
#113882 = CARTESIAN_POINT('Ctrl Pts',(-27.7972096887257,8.90000000004957,
121.922389169964)) ;
#113883 = CARTESIAN_POINT('Ctrl Pts',(-27.9581738536375,9.20000000004957,
121.660008974116)) ;
#113884 = CARTESIAN_POINT('Ctrl Pts',(-27.2095125702209,8.90000000004962,
121.378605523633)) ;
#113885 = CARTESIAN_POINT('Ctrl Pts',(-27.4586313028868,9.20000000004962,
121.197792875516)) ;
#113886 = CARTESIAN_POINT('Ctrl Pts',(-26.8746340558793,8.90000000004957,
120.651283590261)) ;
#113887 = CARTESIAN_POINT('Ctrl Pts',(-27.1739845654613,9.20000000004957,
120.579569231898)) ;
#113888 = CARTESIAN_POINT('Ctrl Pts',(-26.8435895428339,8.90000000004962,
119.851184734958)) ;
#113889 = CARTESIAN_POINT('Ctrl Pts',(-27.1475967294288,9.20000000004963,
119.899485204542)) ;
#113890 = CARTESIAN_POINT('Ctrl Pts',(-27.1210879996608,8.90000000004958,
119.100098338637)) ;
#113891 = CARTESIAN_POINT('Ctrl Pts',(-27.3834704179728,9.20000000004958,
119.261061767752)) ;
#113892 = CARTESIAN_POINT('Ctrl Pts',(-27.6648946349493,8.9000000000496,118.512393637685)) ;
#113893 = CARTESIAN_POINT('Ctrl Pts',(-27.8457060572028,9.2000000000496,118.761512772263)) ;
#113894 = CARTESIAN_POINT('Ctrl Pts',(-28.3922036993924,8.90000000004957,
118.177519337191)) ;
#113895 = CARTESIAN_POINT('Ctrl Pts',(-28.4639187630298,9.20000000004957,
118.476869616603)) ;
#113896 = CARTESIAN_POINT('Ctrl Pts',(-29.1923099252245,8.90000000004963,
118.146472421837)) ;
#113897 = CARTESIAN_POINT('Ctrl Pts',(-29.1440090539225,9.20000000004963,
118.450479738513)) ;
#113898 = CARTESIAN_POINT('Ctrl Pts',(-29.9433921833963,8.90000000004956,
118.423972232679)) ;
#113899 = CARTESIAN_POINT('Ctrl Pts',(-29.7824289744743,9.20000000004957,
118.686354577768)) ;
#113900 = CARTESIAN_POINT('Ctrl Pts',(-30.5310991659207,8.90000000004961,
118.967778117292)) ;
#113901 = CARTESIAN_POINT('Ctrl Pts',(-30.2819799090916,9.2000000000496,119.148589579807)) ;
#113902 = CARTESIAN_POINT('Ctrl Pts',(-30.8659719637261,8.90000000004959,
119.695089123834)) ;
#113903 = CARTESIAN_POINT('Ctrl Pts',(-30.5666217872643,9.2000000000496,119.766803935434)) ;
#113904 = CARTESIAN_POINT('Ctrl Pts',(-30.8970357112146,8.90000000004959,
120.495212908351)) ;
#113905 = CARTESIAN_POINT('Ctrl Pts',(-30.593025972774,9.20000000004959,120.446909151552)) ;
#113906 = CARTESIAN_POINT('Ctrl Pts',(-30.619480653913,8.9000000000496,121.246245879451)) ;
#113907 = CARTESIAN_POINT('Ctrl Pts',(-30.3571041737438,9.2000000000496,121.085287178393)) ;
#113908 = CARTESIAN_POINT('Ctrl Pts',(-30.2570384098916,8.90000000004959,
121.63814542126)) ;
#113909 = CARTESIAN_POINT('Ctrl Pts',(-30.0490282665823,9.2000000000496,121.418401787627)) ;
#113910 = CARTESIAN_POINT('Ctrl Pts',(-30.0450876601579,8.90000000004959,
121.791793326842)) ;
#113911 = CARTESIAN_POINT('Ctrl Pts',(-29.8688701292195,9.2000000000496,121.549002507844)) ;
#113912 = CARTESIAN_POINT('',(-30.0450876601579,8.90000000004959,121.791793326842)) ;
#113913 = CARTESIAN_POINT('Origin',(-28.8703041205687,-0.0122621421566816,
120.173187866852)) ;
#113914 = CARTESIAN_POINT('',(-23.1155414022614,-0.0122621421566816,121.871041233896)) ;
#113915 = CARTESIAN_POINT('',(-34.4604331353428,-0.0122621421566816,117.993633417388)) ;
#113916 = CARTESIAN_POINT('Origin',(-28.8703041205686,-0.0122621421566816,
120.173187866852)) ;
#113917 = CARTESIAN_POINT('',(-34.4604331353428,-3.01226214215668,117.993633417388)) ;
#113918 = CARTESIAN_POINT('',(-34.4604331353428,-0.0122621421566816,117.993633417388)) ;
#113919 = CARTESIAN_POINT('',(-23.1155414022614,-3.01226214215668,121.871041233896)) ;
#113920 = CARTESIAN_POINT('Origin',(-28.8703041205686,-3.01226214215668,120.173187866852)) ;
#113921 = CARTESIAN_POINT('',(-23.1155414022614,-0.0122621421566816,121.871041233896)) ;
#113922 = CARTESIAN_POINT('Origin',(-33.1491896568585,-0.0122621421566816,
114.630551473595)) ;
#113923 = CARTESIAN_POINT('',(-31.8379461783745,-0.0122621421566816,111.267469529802)) ;
#113924 = CARTESIAN_POINT('',(-34.4604331353428,-0.0122621421566816,117.993633417388)) ;
#113925 = CARTESIAN_POINT('',(-31.8379461783745,-3.01226214215668,111.267469529802)) ;
#113926 = CARTESIAN_POINT('',(-31.8379461783745,-0.0122621421566816,111.267469529802)) ;
#113927 = CARTESIAN_POINT('',(-34.4604331353428,-3.01226214215668,117.993633417388)) ;
#113928 = CARTESIAN_POINT('Origin',(-29.8146797867087,-0.0122621421566816,
112.056327757358)) ;
#113929 = CARTESIAN_POINT('',(-27.6453587579679,-0.0122621421566816,111.956575719337)) ;
#113930 = CARTESIAN_POINT('Origin',(-29.8146797867088,-0.0122621421566816,
112.056327757358)) ;
#113931 = CARTESIAN_POINT('',(-27.6453587579679,-3.01226214215668,111.956575719337)) ;
#113932 = CARTESIAN_POINT('',(-27.6453587579679,-0.0122621421566816,111.956575719337)) ;
#113933 = CARTESIAN_POINT('Origin',(-29.8146797867088,-3.01226214215668,112.056327757358)) ;
#113934 = CARTESIAN_POINT('Origin',(-25.1479976271673,-0.0122621421566816,
111.841739390749)) ;
#113935 = CARTESIAN_POINT('',(-23.9413057657522,-0.0122621421566816,114.031235851489)) ;
#113936 = CARTESIAN_POINT('Origin',(-25.1479976271667,-0.0122621421566816,
111.841739390748)) ;
#113937 = CARTESIAN_POINT('',(-23.9413057657522,-3.01226214215668,114.031235851489)) ;
#113938 = CARTESIAN_POINT('',(-23.9413057657522,-0.0122621421566816,114.031235851489)) ;
#113939 = CARTESIAN_POINT('Origin',(-25.1479976271667,-3.01226214215668,111.841739390748)) ;
#113940 = CARTESIAN_POINT('Origin',(1.81795236235752,-0.0122621421566816,
99.834598543949)) ;
#113941 = CARTESIAN_POINT('',(27.5772104904673,-0.0122621421566816,85.6379612364092)) ;
#113942 = CARTESIAN_POINT('',(-23.9413057657522,-0.0122621421566816,114.031235851489)) ;
#113943 = CARTESIAN_POINT('',(27.5772104904673,-3.01226214215668,85.6379612364092)) ;
#113944 = CARTESIAN_POINT('',(27.5772104904673,-0.0122621421566816,85.6379612364092)) ;
#113945 = CARTESIAN_POINT('',(-23.9413057657522,-3.01226214215668,114.031235851489)) ;
#113946 = CARTESIAN_POINT('Origin',(27.2606416518821,-0.0122621421566816,
83.9168324874666)) ;
#113947 = CARTESIAN_POINT('',(26.9440728132968,-0.0122621421566816,82.1957037385239)) ;
#113948 = CARTESIAN_POINT('',(27.5772104904673,-0.0122621421566816,85.6379612364092)) ;
#113949 = CARTESIAN_POINT('',(26.9440728132968,-3.01226214215668,82.1957037385239)) ;
#113950 = CARTESIAN_POINT('',(26.9440728132968,-0.0122621421566816,82.1957037385239)) ;
#113951 = CARTESIAN_POINT('',(27.5772104904673,-3.01226214215668,85.6379612364092)) ;
#113952 = CARTESIAN_POINT('Origin',(27.5772104904672,-0.0122621421566816,
85.6379612364093)) ;
#113953 = CARTESIAN_POINT('',(29.4881888524592,-0.0122621421566816,88.5702234518323)) ;
#113954 = CARTESIAN_POINT('Origin',(27.5772104904673,-0.0122621421566816,
85.6379612364091)) ;
#113955 = CARTESIAN_POINT('',(29.4881888524592,-3.01226214215668,88.5702234518323)) ;
#113956 = CARTESIAN_POINT('',(29.4881888524592,-0.0122621421566816,88.5702234518323)) ;
#113957 = CARTESIAN_POINT('Origin',(27.5772104904673,-3.01226214215668,85.6379612364091)) ;
#113958 = CARTESIAN_POINT('Origin',(7.74723983920157,-0.0122621421566816,
101.647870919597)) ;
#113959 = CARTESIAN_POINT('',(-13.9937091740561,-0.0122621421566816,114.725518387361)) ;
#113960 = CARTESIAN_POINT('',(29.4881888524592,-0.0122621421566816,88.5702234518323)) ;
#113961 = CARTESIAN_POINT('',(-13.9937091740561,-3.01226214215668,114.725518387361)) ;
#113962 = CARTESIAN_POINT('',(-13.9937091740561,-0.0122621421566816,114.725518387361)) ;
#113963 = CARTESIAN_POINT('',(29.4881888524592,-3.01226214215668,88.5702234518323)) ;
#113964 = CARTESIAN_POINT('Origin',(-12.7050739565465,-0.0122621421566816,
116.867811382307)) ;
#113965 = CARTESIAN_POINT('',(-14.5945183767409,-0.0122621421566816,118.504881870403)) ;
#113966 = CARTESIAN_POINT('Origin',(-12.7050739565464,-0.0122621421566816,
116.867811382307)) ;
#113967 = CARTESIAN_POINT('',(-14.5945183767409,-3.01226214215668,118.504881870403)) ;
#113968 = CARTESIAN_POINT('',(-14.5945183767409,-0.0122621421566816,118.504881870403)) ;
#113969 = CARTESIAN_POINT('Origin',(-12.7050739565464,-3.01226214215668,116.867811382307)) ;
#113970 = CARTESIAN_POINT('Origin',(-19.1291849852063,-0.0122621421566816,
122.433851041835)) ;
#113971 = CARTESIAN_POINT('',(-13.1666432326431,-0.0122621421566816,121.76445142357)) ;
#113972 = CARTESIAN_POINT('Origin',(-19.1291849852063,-0.0122621421566816,
122.433851041835)) ;
#113973 = CARTESIAN_POINT('',(-13.1666432326431,-3.01226214215668,121.76445142357)) ;
#113974 = CARTESIAN_POINT('',(-13.1666432326431,-0.0122621421566816,121.76445142357)) ;
#113975 = CARTESIAN_POINT('Origin',(-19.1291849852063,-3.01226214215671,122.433851041835)) ;
#113976 = CARTESIAN_POINT('Origin',(-16.6596005209322,-0.0122621421566816,
120.953825888281)) ;
#113977 = CARTESIAN_POINT('',(-20.1525578092214,-0.0122621421566816,120.143200352991)) ;
#113978 = CARTESIAN_POINT('',(-13.1666432326431,-0.0122621421566816,121.76445142357)) ;
#113979 = CARTESIAN_POINT('',(-20.1525578092214,-3.01226214215668,120.143200352991)) ;
#113980 = CARTESIAN_POINT('',(-20.1525578092214,-0.0122621421566816,120.143200352991)) ;
#113981 = CARTESIAN_POINT('',(-13.1666432326431,-3.01226214215668,121.76445142357)) ;
#113982 = CARTESIAN_POINT('Origin',(-20.7177236029669,-0.0122621421566816,
122.578480136831)) ;
#113983 = CARTESIAN_POINT('Origin',(-20.7177236029668,-0.0122621421566816,
122.578480136831)) ;
#113984 = CARTESIAN_POINT('Origin',(-20.7177236029668,-3.01226214215668,122.578480136831)) ;
#113985 = CARTESIAN_POINT('Origin',(-23.1155414022614,-0.0122621421566816,
121.871041233896)) ;
#113986 = CARTESIAN_POINT('',(-30.807979376547,-0.0122621421566815,112.171895593834)) ;
#113987 = CARTESIAN_POINT('Origin',(-29.8146797867089,-0.0122621421566816,
112.056327757358)) ;
#113988 = CARTESIAN_POINT('',(-27.6955205809792,-0.0122621421566782,118.554582406862)) ;
#113989 = CARTESIAN_POINT('Origin',(-28.8703041205685,-0.0122621421566797,
120.173187866852)) ;
#113990 = CARTESIAN_POINT('Origin',(-23.1155414022614,-3.01226214215668,121.871041233896)) ;
#113991 = CARTESIAN_POINT('',(-30.807979376547,-3.01226214215668,112.171895593834)) ;
#113992 = CARTESIAN_POINT('Origin',(-29.8146797867089,-3.01226214215668,112.056327757358)) ;
#113993 = CARTESIAN_POINT('',(-27.6955205809792,-3.01226214215668,118.554582406862)) ;
#113994 = CARTESIAN_POINT('Origin',(-28.8703041205685,-3.01226214215668,120.173187866852)) ;
#113995 = CARTESIAN_POINT('Origin',(-29.814679786709,-6.99999999995041,112.056327757358)) ;
#113996 = CARTESIAN_POINT('',(-30.807979376547,-6.99999999995041,112.171895593834)) ;
#113997 = CARTESIAN_POINT('Origin',(-28.8703041205685,0.,120.173187866852)) ;
#113998 = CARTESIAN_POINT('',(-27.6955205809792,0.,118.554582406862)) ;
#113999 = CARTESIAN_POINT('Origin',(-34.1140302566115,0.00967047744422178,
126.985310472154)) ;
#114000 = CARTESIAN_POINT('',(-34.2597706710927,0.00967047744422267,127.411056560318)) ;
#114001 = CARTESIAN_POINT('',(-33.9682898421302,0.00967047744422267,126.55956438399)) ;
#114002 = CARTESIAN_POINT('',(-34.2597706710927,0.00967047744422267,127.411056560318)) ;
#114003 = CARTESIAN_POINT('Origin',(-33.9682898421302,0.00967047744422267,
126.55956438399)) ;
#114004 = CARTESIAN_POINT('Ctrl Pts',(-33.9682898421302,14.28596080689,126.55956438399)) ;
#114005 = CARTESIAN_POINT('Ctrl Pts',(-33.9682898421302,14.28596080689,126.55956438399)) ;
#114006 = CARTESIAN_POINT('Ctrl Pts',(-33.9682898421302,14.28596080689,126.55956438399)) ;
#114007 = CARTESIAN_POINT('Ctrl Pts',(-33.9682898421302,14.28596080689,126.55956438399)) ;
#114008 = CARTESIAN_POINT('Ctrl Pts',(-33.9682898421302,14.28596080689,126.55956438399)) ;
#114009 = CARTESIAN_POINT('Ctrl Pts',(-33.9682898421302,14.28596080689,126.55956438399)) ;
#114010 = CARTESIAN_POINT('Ctrl Pts',(-33.9682898421302,14.28596080689,126.55956438399)) ;
#114011 = CARTESIAN_POINT('Ctrl Pts',(-33.9682898421302,14.28596080689,126.55956438399)) ;
#114012 = CARTESIAN_POINT('Ctrl Pts',(-33.9682898421302,14.28596080689,126.55956438399)) ;
#114013 = CARTESIAN_POINT('Ctrl Pts',(-34.1425850701396,14.28596080689,127.068726593901)) ;
#114014 = CARTESIAN_POINT('Ctrl Pts',(-33.631202312305,14.28596080689,127.243781954731)) ;
#114015 = CARTESIAN_POINT('Ctrl Pts',(-33.4569070842956,14.28596080689,126.73461974482)) ;
#114016 = CARTESIAN_POINT('Ctrl Pts',(-33.2826118562863,14.28596080689,126.225457534909)) ;
#114017 = CARTESIAN_POINT('Ctrl Pts',(-33.7939946141209,14.28596080689,126.050402174079)) ;
#114018 = CARTESIAN_POINT('Ctrl Pts',(-34.3053773719555,14.28596080689,125.875346813249)) ;
#114019 = CARTESIAN_POINT('Ctrl Pts',(-34.4796725999648,14.28596080689,126.38450902316)) ;
#114020 = CARTESIAN_POINT('Ctrl Pts',(-34.6539678279742,14.28596080689,126.893671233071)) ;
#114021 = CARTESIAN_POINT('Ctrl Pts',(-34.1425850701396,14.28596080689,127.068726593901)) ;
#114022 = CARTESIAN_POINT('Ctrl Pts',(-34.2921574298663,14.0096704774442,
127.505666802132)) ;
#114023 = CARTESIAN_POINT('Ctrl Pts',(-33.341928889009,14.0096704774442,127.830946834636)) ;
#114024 = CARTESIAN_POINT('Ctrl Pts',(-33.018061301273,14.0096704774442,126.884844416494)) ;
#114025 = CARTESIAN_POINT('Ctrl Pts',(-32.6941937135369,14.0096704774442,
125.938741998352)) ;
#114026 = CARTESIAN_POINT('Ctrl Pts',(-33.6444222543942,14.0096704774442,
125.613461965848)) ;
#114027 = CARTESIAN_POINT('Ctrl Pts',(-34.5946507952514,14.0096704774442,
125.288181933344)) ;
#114028 = CARTESIAN_POINT('Ctrl Pts',(-34.9185183829875,14.0096704774442,
126.234284351486)) ;
#114029 = CARTESIAN_POINT('Ctrl Pts',(-35.2423859707236,14.0096704774442,
127.180386769628)) ;
#114030 = CARTESIAN_POINT('Ctrl Pts',(-34.2921574298663,14.0096704774442,
127.505666802132)) ;
#114031 = CARTESIAN_POINT('',(-34.2921574298663,14.0096704774442,127.505666802132)) ;
#114032 = CARTESIAN_POINT('Origin',(-33.9682898421302,14.0096704774442,126.55956438399)) ;
#114033 = CARTESIAN_POINT('',(-33.9682898421302,14.28596080689,126.55956438399)) ;
#114034 = CARTESIAN_POINT('Origin',(-33.9682898421303,12.3381250858491,126.55956438399)) ;
#114035 = CARTESIAN_POINT('Ctrl Pts',(-34.2921574298663,14.0096704774442,
127.505666802132)) ;
#114036 = CARTESIAN_POINT('Ctrl Pts',(-34.2921574298663,13.5548108916342,
127.505666802132)) ;
#114037 = CARTESIAN_POINT('Ctrl Pts',(-33.341928889009,14.0096704774442,127.830946834636)) ;
#114038 = CARTESIAN_POINT('Ctrl Pts',(-33.341928889009,13.5548108916342,127.830946834636)) ;
#114039 = CARTESIAN_POINT('Ctrl Pts',(-33.018061301273,14.0096704774442,126.884844416494)) ;
#114040 = CARTESIAN_POINT('Ctrl Pts',(-33.018061301273,13.5548108916342,126.884844416494)) ;
#114041 = CARTESIAN_POINT('Ctrl Pts',(-32.6941937135369,14.0096704774442,
125.938741998352)) ;
#114042 = CARTESIAN_POINT('Ctrl Pts',(-32.6941937135369,13.5548108916342,
125.938741998352)) ;
#114043 = CARTESIAN_POINT('Ctrl Pts',(-33.6444222543942,14.0096704774442,
125.613461965848)) ;
#114044 = CARTESIAN_POINT('Ctrl Pts',(-33.6444222543942,13.5548108916342,
125.613461965848)) ;
#114045 = CARTESIAN_POINT('Ctrl Pts',(-34.5946507952514,14.0096704774442,
125.288181933344)) ;
#114046 = CARTESIAN_POINT('Ctrl Pts',(-34.5946507952514,13.5548108916342,
125.288181933344)) ;
#114047 = CARTESIAN_POINT('Ctrl Pts',(-34.9185183829875,14.0096704774442,
126.234284351486)) ;
#114048 = CARTESIAN_POINT('Ctrl Pts',(-34.9185183829875,13.5548108916342,
126.234284351486)) ;
#114049 = CARTESIAN_POINT('Ctrl Pts',(-35.2423859707236,14.0096704774442,
127.180386769628)) ;
#114050 = CARTESIAN_POINT('Ctrl Pts',(-35.2423859707236,13.5548108916342,
127.180386769628)) ;
#114051 = CARTESIAN_POINT('Ctrl Pts',(-34.2921574298663,14.0096704774442,
127.505666802132)) ;
#114052 = CARTESIAN_POINT('Ctrl Pts',(-34.2921574298663,13.5548108916342,
127.505666802132)) ;
#114053 = CARTESIAN_POINT('',(-34.2921574298663,13.6306208226026,127.505666802132)) ;
#114054 = CARTESIAN_POINT('Origin',(-33.9682898421302,13.6306208226026,126.55956438399)) ;
#114055 = CARTESIAN_POINT('',(-34.2921574298663,14.0096704774442,127.505666802132)) ;
#114056 = CARTESIAN_POINT('Ctrl Pts',(-34.2921574298663,13.6306208226026,
127.505666802132)) ;
#114057 = CARTESIAN_POINT('Ctrl Pts',(-33.341928889009,13.6306208226025,127.830946834636)) ;
#114058 = CARTESIAN_POINT('Ctrl Pts',(-33.018061301273,13.6306208226026,126.884844416494)) ;
#114059 = CARTESIAN_POINT('Ctrl Pts',(-32.6941937135369,13.6306208226025,
125.938741998352)) ;
#114060 = CARTESIAN_POINT('Ctrl Pts',(-33.6444222543942,13.6306208226026,
125.613461965848)) ;
#114061 = CARTESIAN_POINT('Ctrl Pts',(-34.5946507952514,13.6306208226025,
125.288181933344)) ;
#114062 = CARTESIAN_POINT('Ctrl Pts',(-34.9185183829875,13.6306208226026,
126.234284351486)) ;
#114063 = CARTESIAN_POINT('Ctrl Pts',(-35.2423859707236,13.6306208226025,
127.180386769628)) ;
#114064 = CARTESIAN_POINT('Ctrl Pts',(-34.2921574298663,13.6306208226026,
127.505666802132)) ;
#114065 = CARTESIAN_POINT('Ctrl Pts',(-34.2602567651234,13.6306208226026,
127.41247656885)) ;
#114066 = CARTESIAN_POINT('Ctrl Pts',(-33.4036248769071,13.6306208226025,
127.705716812078)) ;
#114067 = CARTESIAN_POINT('Ctrl Pts',(-33.111657953914,13.6306208226026,126.852804627218)) ;
#114068 = CARTESIAN_POINT('Ctrl Pts',(-32.8196910309208,13.6306208226025,
125.999892442358)) ;
#114069 = CARTESIAN_POINT('Ctrl Pts',(-33.676322919137,13.6306208226026,125.70665219913)) ;
#114070 = CARTESIAN_POINT('Ctrl Pts',(-34.5329548073533,13.6306208226025,
125.413411955902)) ;
#114071 = CARTESIAN_POINT('Ctrl Pts',(-34.8249217303465,13.6306208226026,
126.266324140762)) ;
#114072 = CARTESIAN_POINT('Ctrl Pts',(-35.1168886533397,13.6306208226025,
127.119236325622)) ;
#114073 = CARTESIAN_POINT('Ctrl Pts',(-34.2602567651234,13.6306208226026,
127.41247656885)) ;
#114074 = CARTESIAN_POINT('Ctrl Pts',(-34.2283561003805,13.6306208226026,
127.319286335568)) ;
#114075 = CARTESIAN_POINT('Ctrl Pts',(-33.4653208648053,13.6306208226025,
127.580486789519)) ;
#114076 = CARTESIAN_POINT('Ctrl Pts',(-33.205254606555,13.6306208226026,126.820764837941)) ;
#114077 = CARTESIAN_POINT('Ctrl Pts',(-32.9451883483047,13.6306208226025,
126.061042886363)) ;
#114078 = CARTESIAN_POINT('Ctrl Pts',(-33.70822358388,13.6306208226026,125.799842432412)) ;
#114079 = CARTESIAN_POINT('Ctrl Pts',(-34.4712588194552,13.6306208226025,
125.53864197846)) ;
#114080 = CARTESIAN_POINT('Ctrl Pts',(-34.7313250777055,13.6306208226026,
126.298363930038)) ;
#114081 = CARTESIAN_POINT('Ctrl Pts',(-34.9913913359558,13.6306208226025,
127.058085881616)) ;
#114082 = CARTESIAN_POINT('Ctrl Pts',(-34.2283561003805,13.6306208226026,
127.319286335568)) ;
#114083 = CARTESIAN_POINT('Ctrl Pts',(-34.1797759622201,13.6306208226025,
127.177370972847)) ;
#114084 = CARTESIAN_POINT('Ctrl Pts',(-33.5592750077734,13.6306208226025,
127.389779421923)) ;
#114085 = CARTESIAN_POINT('Ctrl Pts',(-33.3477888876835,13.6306208226025,
126.771972833066)) ;
#114086 = CARTESIAN_POINT('Ctrl Pts',(-33.1363027675937,13.6306208226025,
126.154166244209)) ;
#114087 = CARTESIAN_POINT('Ctrl Pts',(-33.7568037220404,13.6306208226025,
125.941757795133)) ;
#114088 = CARTESIAN_POINT('Ctrl Pts',(-34.377304676487,13.6306208226025,125.729349346057)) ;
#114089 = CARTESIAN_POINT('Ctrl Pts',(-34.5887907965769,13.6306208226025,
126.347155934914)) ;
#114090 = CARTESIAN_POINT('Ctrl Pts',(-34.8002769166668,13.6306208226025,
126.964962523771)) ;
#114091 = CARTESIAN_POINT('Ctrl Pts',(-34.1797759622201,13.6306208226025,
127.177370972847)) ;
#114092 = CARTESIAN_POINT('Ctrl Pts',(-34.1797759622201,13.4806208226026,
127.177370972847)) ;
#114093 = CARTESIAN_POINT('Ctrl Pts',(-33.5592750077734,13.4806208226026,
127.389779421923)) ;
#114094 = CARTESIAN_POINT('Ctrl Pts',(-33.3477888876836,13.4806208226026,
126.771972833066)) ;
#114095 = CARTESIAN_POINT('Ctrl Pts',(-33.1363027675937,13.4806208226026,
126.154166244209)) ;
#114096 = CARTESIAN_POINT('Ctrl Pts',(-33.7568037220404,13.4806208226026,
125.941757795133)) ;
#114097 = CARTESIAN_POINT('Ctrl Pts',(-34.377304676487,13.4806208226026,125.729349346057)) ;
#114098 = CARTESIAN_POINT('Ctrl Pts',(-34.5887907965769,13.4806208226026,
126.347155934914)) ;
#114099 = CARTESIAN_POINT('Ctrl Pts',(-34.8002769166668,13.4806208226026,
126.964962523771)) ;
#114100 = CARTESIAN_POINT('Ctrl Pts',(-34.1797759622201,13.4806208226026,
127.177370972847)) ;
#114101 = CARTESIAN_POINT('Ctrl Pts',(-34.1797759622201,13.3306208226026,
127.177370972847)) ;
#114102 = CARTESIAN_POINT('Ctrl Pts',(-33.5592750077734,13.3306208226026,
127.389779421923)) ;
#114103 = CARTESIAN_POINT('Ctrl Pts',(-33.3477888876835,13.3306208226026,
126.771972833066)) ;
#114104 = CARTESIAN_POINT('Ctrl Pts',(-33.1363027675937,13.3306208226026,
126.154166244209)) ;
#114105 = CARTESIAN_POINT('Ctrl Pts',(-33.7568037220404,13.3306208226026,
125.941757795133)) ;
#114106 = CARTESIAN_POINT('Ctrl Pts',(-34.377304676487,13.3306208226026,125.729349346057)) ;
#114107 = CARTESIAN_POINT('Ctrl Pts',(-34.5887907965769,13.3306208226026,
126.347155934914)) ;
#114108 = CARTESIAN_POINT('Ctrl Pts',(-34.8002769166668,13.3306208226026,
126.964962523771)) ;
#114109 = CARTESIAN_POINT('Ctrl Pts',(-34.1797759622201,13.3306208226026,
127.177370972847)) ;
#114110 = CARTESIAN_POINT('Ctrl Pts',(-34.2283561003805,13.3306208226026,
127.319286335568)) ;
#114111 = CARTESIAN_POINT('Ctrl Pts',(-33.4653208648053,13.3306208226026,
127.580486789519)) ;
#114112 = CARTESIAN_POINT('Ctrl Pts',(-33.205254606555,13.3306208226026,126.820764837941)) ;
#114113 = CARTESIAN_POINT('Ctrl Pts',(-32.9451883483047,13.3306208226026,
126.061042886363)) ;
#114114 = CARTESIAN_POINT('Ctrl Pts',(-33.70822358388,13.3306208226026,125.799842432412)) ;
#114115 = CARTESIAN_POINT('Ctrl Pts',(-34.4712588194552,13.3306208226026,
125.53864197846)) ;
#114116 = CARTESIAN_POINT('Ctrl Pts',(-34.7313250777055,13.3306208226026,
126.298363930038)) ;
#114117 = CARTESIAN_POINT('Ctrl Pts',(-34.9913913359558,13.3306208226026,
127.058085881616)) ;
#114118 = CARTESIAN_POINT('Ctrl Pts',(-34.2283561003805,13.3306208226026,
127.319286335568)) ;
#114119 = CARTESIAN_POINT('Ctrl Pts',(-34.2602567651234,13.3306208226026,
127.41247656885)) ;
#114120 = CARTESIAN_POINT('Ctrl Pts',(-33.4036248769071,13.3306208226026,
127.705716812078)) ;
#114121 = CARTESIAN_POINT('Ctrl Pts',(-33.111657953914,13.3306208226026,126.852804627218)) ;
#114122 = CARTESIAN_POINT('Ctrl Pts',(-32.8196910309208,13.3306208226026,
125.999892442358)) ;
#114123 = CARTESIAN_POINT('Ctrl Pts',(-33.676322919137,13.3306208226026,125.70665219913)) ;
#114124 = CARTESIAN_POINT('Ctrl Pts',(-34.5329548073533,13.3306208226026,
125.413411955902)) ;
#114125 = CARTESIAN_POINT('Ctrl Pts',(-34.8249217303465,13.3306208226026,
126.266324140762)) ;
#114126 = CARTESIAN_POINT('Ctrl Pts',(-35.1168886533397,13.3306208226026,
127.119236325622)) ;
#114127 = CARTESIAN_POINT('Ctrl Pts',(-34.2602567651234,13.3306208226026,
127.41247656885)) ;
#114128 = CARTESIAN_POINT('Ctrl Pts',(-34.2921574298663,13.3306208226026,
127.505666802132)) ;
#114129 = CARTESIAN_POINT('Ctrl Pts',(-33.341928889009,13.3306208226026,127.830946834636)) ;
#114130 = CARTESIAN_POINT('Ctrl Pts',(-33.018061301273,13.3306208226026,126.884844416494)) ;
#114131 = CARTESIAN_POINT('Ctrl Pts',(-32.6941937135369,13.3306208226026,
125.938741998352)) ;
#114132 = CARTESIAN_POINT('Ctrl Pts',(-33.6444222543942,13.3306208226026,
125.613461965848)) ;
#114133 = CARTESIAN_POINT('Ctrl Pts',(-34.5946507952514,13.3306208226026,
125.288181933344)) ;
#114134 = CARTESIAN_POINT('Ctrl Pts',(-34.9185183829875,13.3306208226026,
126.234284351486)) ;
#114135 = CARTESIAN_POINT('Ctrl Pts',(-35.2423859707236,13.3306208226026,
127.180386769628)) ;
#114136 = CARTESIAN_POINT('Ctrl Pts',(-34.2921574298663,13.3306208226026,
127.505666802132)) ;
#114137 = CARTESIAN_POINT('',(-34.2921574298663,13.3306208226026,127.505666802132)) ;
#114138 = CARTESIAN_POINT('Origin',(-33.9682898421302,13.3306208226026,126.55956438399)) ;
#114139 = CARTESIAN_POINT('Ctrl Pts',(-34.2921574298663,13.6306208226026,
127.505666802132)) ;
#114140 = CARTESIAN_POINT('Ctrl Pts',(-34.2602567651234,13.6306208226026,
127.41247656885)) ;
#114141 = CARTESIAN_POINT('Ctrl Pts',(-34.2283561003805,13.6306208226026,
127.319286335568)) ;
#114142 = CARTESIAN_POINT('Ctrl Pts',(-34.1797759622201,13.6306208226025,
127.177370972847)) ;
#114143 = CARTESIAN_POINT('Ctrl Pts',(-34.1797759622201,13.4806208226026,
127.177370972847)) ;
#114144 = CARTESIAN_POINT('Ctrl Pts',(-34.1797759622201,13.3306208226026,
127.177370972847)) ;
#114145 = CARTESIAN_POINT('Ctrl Pts',(-34.2283561003805,13.3306208226026,
127.319286335568)) ;
#114146 = CARTESIAN_POINT('Ctrl Pts',(-34.2602567651234,13.3306208226026,
127.41247656885)) ;
#114147 = CARTESIAN_POINT('Ctrl Pts',(-34.2921574298663,13.3306208226026,
127.505666802132)) ;
#114148 = CARTESIAN_POINT('Ctrl Pts',(-34.2921574298663,13.3306208226026,
127.505666802132)) ;
#114149 = CARTESIAN_POINT('Ctrl Pts',(-34.2921574298663,-2.53451959158744,
127.505666802132)) ;
#114150 = CARTESIAN_POINT('Ctrl Pts',(-33.341928889009,13.3306208226026,127.830946834636)) ;
#114151 = CARTESIAN_POINT('Ctrl Pts',(-33.341928889009,-2.53451959158744,
127.830946834636)) ;
#114152 = CARTESIAN_POINT('Ctrl Pts',(-33.018061301273,13.3306208226026,126.884844416494)) ;
#114153 = CARTESIAN_POINT('Ctrl Pts',(-33.018061301273,-2.53451959158744,
126.884844416494)) ;
#114154 = CARTESIAN_POINT('Ctrl Pts',(-32.6941937135369,13.3306208226026,
125.938741998352)) ;
#114155 = CARTESIAN_POINT('Ctrl Pts',(-32.6941937135369,-2.53451959158744,
125.938741998352)) ;
#114156 = CARTESIAN_POINT('Ctrl Pts',(-33.6444222543942,13.3306208226026,
125.613461965848)) ;
#114157 = CARTESIAN_POINT('Ctrl Pts',(-33.6444222543942,-2.53451959158744,
125.613461965848)) ;
#114158 = CARTESIAN_POINT('Ctrl Pts',(-34.5946507952514,13.3306208226026,
125.288181933344)) ;
#114159 = CARTESIAN_POINT('Ctrl Pts',(-34.5946507952514,-2.53451959158744,
125.288181933344)) ;
#114160 = CARTESIAN_POINT('Ctrl Pts',(-34.9185183829875,13.3306208226026,
126.234284351486)) ;
#114161 = CARTESIAN_POINT('Ctrl Pts',(-34.9185183829875,-2.53451959158744,
126.234284351486)) ;
#114162 = CARTESIAN_POINT('Ctrl Pts',(-35.2423859707236,13.3306208226026,
127.180386769628)) ;
#114163 = CARTESIAN_POINT('Ctrl Pts',(-35.2423859707236,-2.53451959158744,
127.180386769628)) ;
#114164 = CARTESIAN_POINT('Ctrl Pts',(-34.2921574298663,13.3306208226026,
127.505666802132)) ;
#114165 = CARTESIAN_POINT('Ctrl Pts',(-34.2921574298663,-2.53451959158744,
127.505666802132)) ;
#114166 = CARTESIAN_POINT('',(-34.2921574298663,0.109670477444222,127.505666802132)) ;
#114167 = CARTESIAN_POINT('Origin',(-33.9682898421302,0.109670477444222,126.55956438399)) ;
#114168 = CARTESIAN_POINT('',(-34.2921574298663,13.3306208226026,127.505666802132)) ;
#114169 = CARTESIAN_POINT('Ctrl Pts',(-34.2921574298663,0.109670477444222,
127.505666802132)) ;
#114170 = CARTESIAN_POINT('Ctrl Pts',(-33.341928889009,0.109670477444222,
127.830946834636)) ;
#114171 = CARTESIAN_POINT('Ctrl Pts',(-33.018061301273,0.109670477444222,
126.884844416494)) ;
#114172 = CARTESIAN_POINT('Ctrl Pts',(-32.6941937135369,0.109670477444222,
125.938741998352)) ;
#114173 = CARTESIAN_POINT('Ctrl Pts',(-33.6444222543942,0.109670477444222,
125.613461965848)) ;
#114174 = CARTESIAN_POINT('Ctrl Pts',(-34.5946507952514,0.109670477444222,
125.288181933344)) ;
#114175 = CARTESIAN_POINT('Ctrl Pts',(-34.9185183829875,0.109670477444222,
126.234284351486)) ;
#114176 = CARTESIAN_POINT('Ctrl Pts',(-35.2423859707236,0.109670477444222,
127.180386769628)) ;
#114177 = CARTESIAN_POINT('Ctrl Pts',(-34.2921574298663,0.109670477444222,
127.505666802132)) ;
#114178 = CARTESIAN_POINT('Ctrl Pts',(-34.2597706710927,0.00967047744422267,
127.411056560318)) ;
#114179 = CARTESIAN_POINT('Ctrl Pts',(-33.4045649843211,0.00967047744422267,
127.703808589571)) ;
#114180 = CARTESIAN_POINT('Ctrl Pts',(-33.1130841553587,0.00967047744422267,
126.852316413244)) ;
#114181 = CARTESIAN_POINT('Ctrl Pts',(-32.8216033263962,0.00967047744422267,
126.000824236916)) ;
#114182 = CARTESIAN_POINT('Ctrl Pts',(-33.6768090131678,0.00967047744422267,
125.708072207662)) ;
#114183 = CARTESIAN_POINT('Ctrl Pts',(-34.5320146999393,0.00967047744422267,
125.415320178408)) ;
#114184 = CARTESIAN_POINT('Ctrl Pts',(-34.8234955289018,0.00967047744422267,
126.266812354736)) ;
#114185 = CARTESIAN_POINT('Ctrl Pts',(-35.1149763578642,0.00967047744422267,
127.118304531064)) ;
#114186 = CARTESIAN_POINT('Ctrl Pts',(-34.2597706710927,0.00967047744422267,
127.411056560318)) ;
#114187 = CARTESIAN_POINT('',(-34.2921574298663,0.109670477444222,127.505666802132)) ;
#114188 = CARTESIAN_POINT('Origin',(-10.3705051027321,0.00967047744422356,
133.686232163474)) ;
#114189 = CARTESIAN_POINT('',(-10.9534667606571,0.00967047744422267,135.389216516129)) ;
#114190 = CARTESIAN_POINT('Origin',(-10.6619859316946,0.00967047744422267,
134.537724339801)) ;
#114191 = CARTESIAN_POINT('',(-10.6619859316946,0.00967047744422267,134.537724339801)) ;
#114192 = CARTESIAN_POINT('',(-10.9534667606571,0.00967047744422267,135.389216516129)) ;
#114193 = CARTESIAN_POINT('Ctrl Pts',(-10.6619859316946,14.28596080689,134.537724339801)) ;
#114194 = CARTESIAN_POINT('Ctrl Pts',(-10.836281159704,14.28596080689,135.046886549712)) ;
#114195 = CARTESIAN_POINT('Ctrl Pts',(-10.9858535194307,14.0096704774442,
135.483826757943)) ;
#114196 = CARTESIAN_POINT('Ctrl Pts',(-10.6619859316946,14.28596080689,134.537724339801)) ;
#114197 = CARTESIAN_POINT('Ctrl Pts',(-11.3476639175386,14.28596080689,134.871831188882)) ;
#114198 = CARTESIAN_POINT('Ctrl Pts',(-11.9360820602879,14.0096704774442,
135.158546725439)) ;
#114199 = CARTESIAN_POINT('Ctrl Pts',(-10.6619859316946,14.28596080689,134.537724339801)) ;
#114200 = CARTESIAN_POINT('Ctrl Pts',(-11.1733686895292,14.28596080689,134.362668978971)) ;
#114201 = CARTESIAN_POINT('Ctrl Pts',(-11.6122144725519,14.0096704774442,
134.212444307297)) ;
#114202 = CARTESIAN_POINT('Ctrl Pts',(-10.6619859316946,14.28596080689,134.537724339801)) ;
#114203 = CARTESIAN_POINT('Ctrl Pts',(-10.9990734615198,14.28596080689,133.85350676906)) ;
#114204 = CARTESIAN_POINT('Ctrl Pts',(-11.2883468848158,14.0096704774442,
133.266341889155)) ;
#114205 = CARTESIAN_POINT('Ctrl Pts',(-10.6619859316946,14.28596080689,134.537724339801)) ;
#114206 = CARTESIAN_POINT('Ctrl Pts',(-10.4876907036852,14.28596080689,134.02856212989)) ;
#114207 = CARTESIAN_POINT('Ctrl Pts',(-10.3381183439585,14.0096704774442,
133.591621921659)) ;
#114208 = CARTESIAN_POINT('Ctrl Pts',(-10.6619859316946,14.28596080689,134.537724339801)) ;
#114209 = CARTESIAN_POINT('Ctrl Pts',(-9.97630794585064,14.28596080689,134.20361749072)) ;
#114210 = CARTESIAN_POINT('Ctrl Pts',(-9.38788980310125,14.0096704774442,
133.916901954163)) ;
#114211 = CARTESIAN_POINT('Ctrl Pts',(-10.6619859316946,14.28596080689,134.537724339801)) ;
#114212 = CARTESIAN_POINT('Ctrl Pts',(-10.15060317386,14.28596080689,134.712779700631)) ;
#114213 = CARTESIAN_POINT('Ctrl Pts',(-9.7117573908373,14.0096704774442,134.863004372305)) ;
#114214 = CARTESIAN_POINT('Ctrl Pts',(-10.6619859316946,14.28596080689,134.537724339801)) ;
#114215 = CARTESIAN_POINT('Ctrl Pts',(-10.3248984018694,14.28596080689,135.221941910542)) ;
#114216 = CARTESIAN_POINT('Ctrl Pts',(-10.0356249785734,14.0096704774442,
135.809106790447)) ;
#114217 = CARTESIAN_POINT('Ctrl Pts',(-10.6619859316946,14.28596080689,134.537724339801)) ;
#114218 = CARTESIAN_POINT('Ctrl Pts',(-10.836281159704,14.28596080689,135.046886549712)) ;
#114219 = CARTESIAN_POINT('Ctrl Pts',(-10.9858535194307,14.0096704774442,
135.483826757943)) ;
#114220 = CARTESIAN_POINT('',(-10.6619859316946,14.28596080689,134.537724339801)) ;
#114221 = CARTESIAN_POINT('',(-10.9858535194307,14.0096704774442,135.483826757943)) ;
#114222 = CARTESIAN_POINT('Origin',(-10.6619859316945,12.3381250858492,134.537724339801)) ;
#114223 = CARTESIAN_POINT('Origin',(-10.6619859316946,14.0096704774442,134.537724339801)) ;
#114224 = CARTESIAN_POINT('Ctrl Pts',(-10.9858535194307,14.0096704774442,
135.483826757943)) ;
#114225 = CARTESIAN_POINT('Ctrl Pts',(-10.9858535194307,13.5548108916342,
135.483826757943)) ;
#114226 = CARTESIAN_POINT('Ctrl Pts',(-11.9360820602879,14.0096704774442,
135.158546725439)) ;
#114227 = CARTESIAN_POINT('Ctrl Pts',(-11.9360820602879,13.5548108916342,
135.158546725439)) ;
#114228 = CARTESIAN_POINT('Ctrl Pts',(-11.6122144725518,14.0096704774442,
134.212444307297)) ;
#114229 = CARTESIAN_POINT('Ctrl Pts',(-11.6122144725518,13.5548108916342,
134.212444307297)) ;
#114230 = CARTESIAN_POINT('Ctrl Pts',(-11.2883468848158,14.0096704774442,
133.266341889155)) ;
#114231 = CARTESIAN_POINT('Ctrl Pts',(-11.2883468848158,13.5548108916342,
133.266341889155)) ;
#114232 = CARTESIAN_POINT('Ctrl Pts',(-10.3381183439585,14.0096704774442,
133.591621921659)) ;
#114233 = CARTESIAN_POINT('Ctrl Pts',(-10.3381183439585,13.5548108916342,
133.591621921659)) ;
#114234 = CARTESIAN_POINT('Ctrl Pts',(-9.3878898031013,14.0096704774442,133.916901954163)) ;
#114235 = CARTESIAN_POINT('Ctrl Pts',(-9.3878898031013,13.5548108916342,133.916901954163)) ;
#114236 = CARTESIAN_POINT('Ctrl Pts',(-9.71175739083736,14.0096704774442,
134.863004372305)) ;
#114237 = CARTESIAN_POINT('Ctrl Pts',(-9.71175739083736,13.5548108916342,
134.863004372305)) ;
#114238 = CARTESIAN_POINT('Ctrl Pts',(-10.0356249785734,14.0096704774442,
135.809106790447)) ;
#114239 = CARTESIAN_POINT('Ctrl Pts',(-10.0356249785734,13.5548108916342,
135.809106790447)) ;
#114240 = CARTESIAN_POINT('Ctrl Pts',(-10.9858535194307,14.0096704774442,
135.483826757943)) ;
#114241 = CARTESIAN_POINT('Ctrl Pts',(-10.9858535194307,13.5548108916342,
135.483826757943)) ;
#114242 = CARTESIAN_POINT('',(-10.9858535194307,13.6306208226026,135.483826757943)) ;
#114243 = CARTESIAN_POINT('',(-10.9858535194307,14.0096704774442,135.483826757943)) ;
#114244 = CARTESIAN_POINT('Origin',(-10.6619859316946,13.6306208226026,134.537724339801)) ;
#114245 = CARTESIAN_POINT('Ctrl Pts',(-10.9858535194307,13.6306208226026,
135.483826757943)) ;
#114246 = CARTESIAN_POINT('Ctrl Pts',(-10.9539528546878,13.6306208226026,
135.390636524661)) ;
#114247 = CARTESIAN_POINT('Ctrl Pts',(-10.9220521899449,13.6306208226026,
135.297446291379)) ;
#114248 = CARTESIAN_POINT('Ctrl Pts',(-10.8734720517845,13.6306208226025,
135.155530928658)) ;
#114249 = CARTESIAN_POINT('Ctrl Pts',(-10.8734720517845,13.4806208226026,
135.155530928658)) ;
#114250 = CARTESIAN_POINT('Ctrl Pts',(-10.8734720517845,13.3306208226026,
135.155530928658)) ;
#114251 = CARTESIAN_POINT('Ctrl Pts',(-10.9220521899449,13.3306208226026,
135.297446291379)) ;
#114252 = CARTESIAN_POINT('Ctrl Pts',(-10.9539528546878,13.3306208226026,
135.390636524661)) ;
#114253 = CARTESIAN_POINT('Ctrl Pts',(-10.9858535194307,13.3306208226026,
135.483826757943)) ;
#114254 = CARTESIAN_POINT('Ctrl Pts',(-11.9360820602879,13.6306208226025,
135.158546725439)) ;
#114255 = CARTESIAN_POINT('Ctrl Pts',(-11.810584742904,13.6306208226025,135.097396281433)) ;
#114256 = CARTESIAN_POINT('Ctrl Pts',(-11.6850874255201,13.6306208226025,
135.036245837428)) ;
#114257 = CARTESIAN_POINT('Ctrl Pts',(-11.4939730062311,13.6306208226025,
134.943122479582)) ;
#114258 = CARTESIAN_POINT('Ctrl Pts',(-11.4939730062311,13.4806208226026,
134.943122479582)) ;
#114259 = CARTESIAN_POINT('Ctrl Pts',(-11.4939730062311,13.3306208226026,
134.943122479582)) ;
#114260 = CARTESIAN_POINT('Ctrl Pts',(-11.6850874255201,13.3306208226026,
135.036245837428)) ;
#114261 = CARTESIAN_POINT('Ctrl Pts',(-11.810584742904,13.3306208226026,135.097396281433)) ;
#114262 = CARTESIAN_POINT('Ctrl Pts',(-11.9360820602879,13.3306208226026,
135.158546725439)) ;
#114263 = CARTESIAN_POINT('Ctrl Pts',(-11.6122144725518,13.6306208226026,
134.212444307297)) ;
#114264 = CARTESIAN_POINT('Ctrl Pts',(-11.5186178199108,13.6306208226026,
134.244484096573)) ;
#114265 = CARTESIAN_POINT('Ctrl Pts',(-11.4250211672698,13.6306208226026,
134.27652388585)) ;
#114266 = CARTESIAN_POINT('Ctrl Pts',(-11.2824868861412,13.6306208226025,
134.325315890725)) ;
#114267 = CARTESIAN_POINT('Ctrl Pts',(-11.2824868861412,13.4806208226026,
134.325315890725)) ;
#114268 = CARTESIAN_POINT('Ctrl Pts',(-11.2824868861412,13.3306208226026,
134.325315890725)) ;
#114269 = CARTESIAN_POINT('Ctrl Pts',(-11.4250211672698,13.3306208226026,
134.27652388585)) ;
#114270 = CARTESIAN_POINT('Ctrl Pts',(-11.5186178199108,13.3306208226026,
134.244484096573)) ;
#114271 = CARTESIAN_POINT('Ctrl Pts',(-11.6122144725518,13.3306208226026,
134.212444307297)) ;
#114272 = CARTESIAN_POINT('Ctrl Pts',(-11.2883468848158,13.6306208226025,
133.266341889155)) ;
#114273 = CARTESIAN_POINT('Ctrl Pts',(-11.2266508969177,13.6306208226025,
133.391571911713)) ;
#114274 = CARTESIAN_POINT('Ctrl Pts',(-11.1649549090195,13.6306208226025,
133.516801934272)) ;
#114275 = CARTESIAN_POINT('Ctrl Pts',(-11.0710007660514,13.6306208226025,
133.707509301869)) ;
#114276 = CARTESIAN_POINT('Ctrl Pts',(-11.0710007660514,13.4806208226026,
133.707509301869)) ;
#114277 = CARTESIAN_POINT('Ctrl Pts',(-11.0710007660514,13.3306208226026,
133.707509301869)) ;
#114278 = CARTESIAN_POINT('Ctrl Pts',(-11.1649549090195,13.3306208226026,
133.516801934272)) ;
#114279 = CARTESIAN_POINT('Ctrl Pts',(-11.2266508969177,13.3306208226026,
133.391571911713)) ;
#114280 = CARTESIAN_POINT('Ctrl Pts',(-11.2883468848158,13.3306208226026,
133.266341889155)) ;
#114281 = CARTESIAN_POINT('Ctrl Pts',(-10.3381183439585,13.6306208226026,
133.591621921659)) ;
#114282 = CARTESIAN_POINT('Ctrl Pts',(-10.3700190087014,13.6306208226026,
133.684812154941)) ;
#114283 = CARTESIAN_POINT('Ctrl Pts',(-10.4019196734443,13.6306208226026,
133.778002388223)) ;
#114284 = CARTESIAN_POINT('Ctrl Pts',(-10.4504998116047,13.6306208226025,
133.919917750944)) ;
#114285 = CARTESIAN_POINT('Ctrl Pts',(-10.4504998116047,13.4806208226026,
133.919917750944)) ;
#114286 = CARTESIAN_POINT('Ctrl Pts',(-10.4504998116047,13.3306208226026,
133.919917750944)) ;
#114287 = CARTESIAN_POINT('Ctrl Pts',(-10.4019196734443,13.3306208226026,
133.778002388223)) ;
#114288 = CARTESIAN_POINT('Ctrl Pts',(-10.3700190087014,13.3306208226026,
133.684812154941)) ;
#114289 = CARTESIAN_POINT('Ctrl Pts',(-10.3381183439585,13.3306208226026,
133.591621921659)) ;
#114290 = CARTESIAN_POINT('Ctrl Pts',(-9.3878898031013,13.6306208226025,133.916901954163)) ;
#114291 = CARTESIAN_POINT('Ctrl Pts',(-9.5133871204852,13.6306208226025,133.978052398169)) ;
#114292 = CARTESIAN_POINT('Ctrl Pts',(-9.63888443786911,13.6306208226025,
134.039202842175)) ;
#114293 = CARTESIAN_POINT('Ctrl Pts',(-9.8299988571581,13.6306208226025,134.13232620002)) ;
#114294 = CARTESIAN_POINT('Ctrl Pts',(-9.8299988571581,13.4806208226026,134.13232620002)) ;
#114295 = CARTESIAN_POINT('Ctrl Pts',(-9.8299988571581,13.3306208226026,134.13232620002)) ;
#114296 = CARTESIAN_POINT('Ctrl Pts',(-9.63888443786911,13.3306208226026,
134.039202842175)) ;
#114297 = CARTESIAN_POINT('Ctrl Pts',(-9.5133871204852,13.3306208226026,133.978052398169)) ;
#114298 = CARTESIAN_POINT('Ctrl Pts',(-9.3878898031013,13.3306208226026,133.916901954163)) ;
#114299 = CARTESIAN_POINT('Ctrl Pts',(-9.71175739083736,13.6306208226026,
134.863004372305)) ;
#114300 = CARTESIAN_POINT('Ctrl Pts',(-9.80535404347837,13.6306208226026,
134.830964583029)) ;
#114301 = CARTESIAN_POINT('Ctrl Pts',(-9.89895069611939,13.6306208226026,
134.798924793753)) ;
#114302 = CARTESIAN_POINT('Ctrl Pts',(-10.041484977248,13.6306208226025,134.750132788877)) ;
#114303 = CARTESIAN_POINT('Ctrl Pts',(-10.041484977248,13.4806208226026,134.750132788877)) ;
#114304 = CARTESIAN_POINT('Ctrl Pts',(-10.041484977248,13.3306208226026,134.750132788877)) ;
#114305 = CARTESIAN_POINT('Ctrl Pts',(-9.89895069611939,13.3306208226026,
134.798924793753)) ;
#114306 = CARTESIAN_POINT('Ctrl Pts',(-9.80535404347837,13.3306208226026,
134.830964583029)) ;
#114307 = CARTESIAN_POINT('Ctrl Pts',(-9.71175739083736,13.3306208226026,
134.863004372305)) ;
#114308 = CARTESIAN_POINT('Ctrl Pts',(-10.0356249785734,13.6306208226025,
135.809106790447)) ;
#114309 = CARTESIAN_POINT('Ctrl Pts',(-10.0973209664715,13.6306208226025,
135.683876767889)) ;
#114310 = CARTESIAN_POINT('Ctrl Pts',(-10.1590169543697,13.6306208226025,
135.558646745331)) ;
#114311 = CARTESIAN_POINT('Ctrl Pts',(-10.2529710973378,13.6306208226025,
135.367939377734)) ;
#114312 = CARTESIAN_POINT('Ctrl Pts',(-10.2529710973378,13.4806208226026,
135.367939377734)) ;
#114313 = CARTESIAN_POINT('Ctrl Pts',(-10.2529710973378,13.3306208226026,
135.367939377734)) ;
#114314 = CARTESIAN_POINT('Ctrl Pts',(-10.1590169543697,13.3306208226026,
135.558646745331)) ;
#114315 = CARTESIAN_POINT('Ctrl Pts',(-10.0973209664715,13.3306208226026,
135.683876767889)) ;
#114316 = CARTESIAN_POINT('Ctrl Pts',(-10.0356249785734,13.3306208226026,
135.809106790447)) ;
#114317 = CARTESIAN_POINT('Ctrl Pts',(-10.9858535194307,13.6306208226026,
135.483826757943)) ;
#114318 = CARTESIAN_POINT('Ctrl Pts',(-10.9539528546878,13.6306208226026,
135.390636524661)) ;
#114319 = CARTESIAN_POINT('Ctrl Pts',(-10.9220521899449,13.6306208226026,
135.297446291379)) ;
#114320 = CARTESIAN_POINT('Ctrl Pts',(-10.8734720517845,13.6306208226025,
135.155530928658)) ;
#114321 = CARTESIAN_POINT('Ctrl Pts',(-10.8734720517845,13.4806208226026,
135.155530928658)) ;
#114322 = CARTESIAN_POINT('Ctrl Pts',(-10.8734720517845,13.3306208226026,
135.155530928658)) ;
#114323 = CARTESIAN_POINT('Ctrl Pts',(-10.9220521899449,13.3306208226026,
135.297446291379)) ;
#114324 = CARTESIAN_POINT('Ctrl Pts',(-10.9539528546878,13.3306208226026,
135.390636524661)) ;
#114325 = CARTESIAN_POINT('Ctrl Pts',(-10.9858535194307,13.3306208226026,
135.483826757943)) ;
#114326 = CARTESIAN_POINT('',(-10.9858535194307,13.3306208226026,135.483826757943)) ;
#114327 = CARTESIAN_POINT('Ctrl Pts',(-10.9858535194307,13.6306208226026,
135.483826757943)) ;
#114328 = CARTESIAN_POINT('Ctrl Pts',(-10.9539528546878,13.6306208226026,
135.390636524661)) ;
#114329 = CARTESIAN_POINT('Ctrl Pts',(-10.9220521899449,13.6306208226026,
135.297446291379)) ;
#114330 = CARTESIAN_POINT('Ctrl Pts',(-10.8734720517845,13.6306208226025,
135.155530928658)) ;
#114331 = CARTESIAN_POINT('Ctrl Pts',(-10.8734720517845,13.4806208226026,
135.155530928658)) ;
#114332 = CARTESIAN_POINT('Ctrl Pts',(-10.8734720517845,13.3306208226026,
135.155530928658)) ;
#114333 = CARTESIAN_POINT('Ctrl Pts',(-10.9220521899449,13.3306208226026,
135.297446291379)) ;
#114334 = CARTESIAN_POINT('Ctrl Pts',(-10.9539528546878,13.3306208226026,
135.390636524661)) ;
#114335 = CARTESIAN_POINT('Ctrl Pts',(-10.9858535194307,13.3306208226026,
135.483826757943)) ;
#114336 = CARTESIAN_POINT('Origin',(-10.6619859316946,13.3306208226026,134.537724339801)) ;
#114337 = CARTESIAN_POINT('Ctrl Pts',(-10.9858535194307,13.3306208226026,
135.483826757943)) ;
#114338 = CARTESIAN_POINT('Ctrl Pts',(-10.9858535194307,-2.53451959158744,
135.483826757943)) ;
#114339 = CARTESIAN_POINT('Ctrl Pts',(-11.9360820602879,13.3306208226026,
135.158546725439)) ;
#114340 = CARTESIAN_POINT('Ctrl Pts',(-11.9360820602879,-2.53451959158744,
135.158546725439)) ;
#114341 = CARTESIAN_POINT('Ctrl Pts',(-11.6122144725518,13.3306208226026,
134.212444307297)) ;
#114342 = CARTESIAN_POINT('Ctrl Pts',(-11.6122144725518,-2.53451959158744,
134.212444307297)) ;
#114343 = CARTESIAN_POINT('Ctrl Pts',(-11.2883468848158,13.3306208226026,
133.266341889155)) ;
#114344 = CARTESIAN_POINT('Ctrl Pts',(-11.2883468848158,-2.53451959158744,
133.266341889155)) ;
#114345 = CARTESIAN_POINT('Ctrl Pts',(-10.3381183439585,13.3306208226026,
133.591621921659)) ;
#114346 = CARTESIAN_POINT('Ctrl Pts',(-10.3381183439585,-2.53451959158744,
133.591621921659)) ;
#114347 = CARTESIAN_POINT('Ctrl Pts',(-9.3878898031013,13.3306208226026,133.916901954163)) ;
#114348 = CARTESIAN_POINT('Ctrl Pts',(-9.3878898031013,-2.53451959158744,
133.916901954163)) ;
#114349 = CARTESIAN_POINT('Ctrl Pts',(-9.71175739083736,13.3306208226026,
134.863004372305)) ;
#114350 = CARTESIAN_POINT('Ctrl Pts',(-9.71175739083736,-2.53451959158744,
134.863004372305)) ;
#114351 = CARTESIAN_POINT('Ctrl Pts',(-10.0356249785734,13.3306208226026,
135.809106790447)) ;
#114352 = CARTESIAN_POINT('Ctrl Pts',(-10.0356249785734,-2.53451959158744,
135.809106790447)) ;
#114353 = CARTESIAN_POINT('Ctrl Pts',(-10.9858535194307,13.3306208226026,
135.483826757943)) ;
#114354 = CARTESIAN_POINT('Ctrl Pts',(-10.9858535194307,-2.53451959158744,
135.483826757943)) ;
#114355 = CARTESIAN_POINT('',(-10.9858535194307,0.109670477444222,135.483826757943)) ;
#114356 = CARTESIAN_POINT('',(-10.9858535194307,13.3306208226026,135.483826757943)) ;
#114357 = CARTESIAN_POINT('Origin',(-10.6619859316946,0.109670477444222,134.537724339801)) ;
#114358 = CARTESIAN_POINT('Ctrl Pts',(-10.9858535194307,0.109670477444222,
135.483826757943)) ;
#114359 = CARTESIAN_POINT('Ctrl Pts',(-10.9534667606571,0.00967047744422267,
135.389216516129)) ;
#114360 = CARTESIAN_POINT('Ctrl Pts',(-11.9360820602879,0.109670477444222,
135.158546725439)) ;
#114361 = CARTESIAN_POINT('Ctrl Pts',(-11.8086724474286,0.00967047744422267,
135.096464486875)) ;
#114362 = CARTESIAN_POINT('Ctrl Pts',(-11.6122144725518,0.109670477444222,
134.212444307297)) ;
#114363 = CARTESIAN_POINT('Ctrl Pts',(-11.5171916184661,0.00967047744422267,
134.244972310548)) ;
#114364 = CARTESIAN_POINT('Ctrl Pts',(-11.2883468848158,0.109670477444222,
133.266341889155)) ;
#114365 = CARTESIAN_POINT('Ctrl Pts',(-11.2257107895036,0.00967047744422267,
133.39348013422)) ;
#114366 = CARTESIAN_POINT('Ctrl Pts',(-10.3381183439585,0.109670477444222,
133.591621921659)) ;
#114367 = CARTESIAN_POINT('Ctrl Pts',(-10.3705051027321,0.00967047744422267,
133.686232163474)) ;
#114368 = CARTESIAN_POINT('Ctrl Pts',(-9.3878898031013,0.109670477444222,
133.916901954163)) ;
#114369 = CARTESIAN_POINT('Ctrl Pts',(-9.51529941596064,0.00967047744422267,
133.978984192727)) ;
#114370 = CARTESIAN_POINT('Ctrl Pts',(-9.71175739083736,0.109670477444222,
134.863004372305)) ;
#114371 = CARTESIAN_POINT('Ctrl Pts',(-9.80678024492309,0.00967047744422267,
134.830476369055)) ;
#114372 = CARTESIAN_POINT('Ctrl Pts',(-10.0356249785734,0.109670477444222,
135.809106790447)) ;
#114373 = CARTESIAN_POINT('Ctrl Pts',(-10.0982610738855,0.00967047744422267,
135.681968545383)) ;
#114374 = CARTESIAN_POINT('Ctrl Pts',(-10.9858535194307,0.109670477444222,
135.483826757943)) ;
#114375 = CARTESIAN_POINT('Ctrl Pts',(-10.9534667606571,0.00967047744422267,
135.389216516129)) ;
#114376 = CARTESIAN_POINT('',(-10.9858535194307,0.109670477444222,135.483826757943)) ;
#114377 = CARTESIAN_POINT('Origin',(-10.8407396157986,13.385947639229,133.868521514384)) ;
#114378 = CARTESIAN_POINT('',(-10.8223318974888,13.4658311995141,133.936074466937)) ;
#114379 = CARTESIAN_POINT('Origin',(-10.8428777772314,13.4930077522664,133.86914951366)) ;
#114380 = CARTESIAN_POINT('Ctrl Pts',(-11.2812798643659,13.1551399285885,
133.225361312885)) ;
#114381 = CARTESIAN_POINT('Ctrl Pts',(-11.2820187647633,13.1489709609094,
133.226788867079)) ;
#114382 = CARTESIAN_POINT('Ctrl Pts',(-11.2940725891313,13.0505878441039,
133.250318667877)) ;
#114383 = CARTESIAN_POINT('Ctrl Pts',(-11.3268196692865,12.8648900473044,
133.323006215356)) ;
#114384 = CARTESIAN_POINT('Ctrl Pts',(-11.3955581347561,12.6378996894465,
133.490786092827)) ;
#114385 = CARTESIAN_POINT('Ctrl Pts',(-11.4818126038911,12.4661938442505,
133.709651137204)) ;
#114386 = CARTESIAN_POINT('Ctrl Pts',(-11.5806418499012,12.3629468779938,
133.965082777503)) ;
#114387 = CARTESIAN_POINT('Ctrl Pts',(-11.6840920756584,12.3360866578135,
134.234357728742)) ;
#114388 = CARTESIAN_POINT('Ctrl Pts',(-11.7874232958009,12.3868467815327,
134.502988211751)) ;
#114389 = CARTESIAN_POINT('Ctrl Pts',(-11.8826517586958,12.5118616193735,
134.748082512994)) ;
#114390 = CARTESIAN_POINT('Ctrl Pts',(-11.9642364503466,12.7022376314793,
134.953268302114)) ;
#114391 = CARTESIAN_POINT('Ctrl Pts',(-12.0268555159077,12.9442211340136,
135.103070944459)) ;
#114392 = CARTESIAN_POINT('Ctrl Pts',(-12.0667868417897,13.2203922331636,
135.186606249474)) ;
#114393 = CARTESIAN_POINT('Ctrl Pts',(-12.0819921567622,13.5109001041669,
135.197934267535)) ;
#114394 = CARTESIAN_POINT('Ctrl Pts',(-12.0718871830781,13.7967277450532,
135.135125417403)) ;
#114395 = CARTESIAN_POINT('Ctrl Pts',(-12.0382787552941,14.0531634695327,
135.003985075531)) ;
#114396 = CARTESIAN_POINT('Ctrl Pts',(-11.984040511163,14.2659161102292,134.812412340654)) ;
#114397 = CARTESIAN_POINT('Ctrl Pts',(-11.9138317313736,14.4182155312585,
134.574200139104)) ;
#114398 = CARTESIAN_POINT('Ctrl Pts',(-11.8331828494072,14.4993926065239,
134.305392211434)) ;
#114399 = CARTESIAN_POINT('Ctrl Pts',(-11.7490444838035,14.5030674016304,
134.026483130585)) ;
#114400 = CARTESIAN_POINT('Ctrl Pts',(-11.6680809986179,14.4296658181567,
133.756898311423)) ;
#114401 = CARTESIAN_POINT('Ctrl Pts',(-11.5965958202758,14.2842405620309,
133.514968656249)) ;
#114402 = CARTESIAN_POINT('Ctrl Pts',(-11.5404239481228,14.0768885755418,
133.31772524141)) ;
#114403 = CARTESIAN_POINT('Ctrl Pts',(-11.5044626643021,13.821937566696,133.179448820527)) ;
#114404 = CARTESIAN_POINT('Ctrl Pts',(-11.492115437901,13.5404397832619,133.110400577556)) ;
#114405 = CARTESIAN_POINT('Ctrl Pts',(-11.5046895368218,13.2491903771815,
133.113990718504)) ;
#114406 = CARTESIAN_POINT('Ctrl Pts',(-11.5423996819585,12.9699188880577,
133.190943520196)) ;
#114407 = CARTESIAN_POINT('Ctrl Pts',(-11.6027127193453,12.7245502986717,
133.33412175314)) ;
#114408 = CARTESIAN_POINT('Ctrl Pts',(-11.6827307770101,12.5279694687298,
133.534676781188)) ;
#114409 = CARTESIAN_POINT('Ctrl Pts',(-11.7767909409935,12.3961377043517,
133.7763823545)) ;
#114410 = CARTESIAN_POINT('Ctrl Pts',(-11.8796482494039,12.3376103677892,
134.043626665423)) ;
#114411 = CARTESIAN_POINT('Ctrl Pts',(-11.9835249356267,12.3569098529355,
134.314074542349)) ;
#114412 = CARTESIAN_POINT('Ctrl Pts',(-12.0830151650733,12.452769019898,134.571498333322)) ;
#114413 = CARTESIAN_POINT('Ctrl Pts',(-12.1707022339469,12.6179593573441,
134.794565234874)) ;
#114414 = CARTESIAN_POINT('Ctrl Pts',(-12.2415306520725,12.8405880377693,
134.968374154773)) ;
#114415 = CARTESIAN_POINT('Ctrl Pts',(-12.2912076318387,13.1065246421439,
135.080214865833)) ;
#114416 = CARTESIAN_POINT('Ctrl Pts',(-12.3163775691246,13.3925179674891,
135.12078307657)) ;
#114417 = CARTESIAN_POINT('Ctrl Pts',(-12.3166058496797,13.6819916651313,
135.088335546118)) ;
#114418 = CARTESIAN_POINT('Ctrl Pts',(-12.2921472081091,13.9537242418059,
134.983669295533)) ;
#114419 = CARTESIAN_POINT('Ctrl Pts',(-12.2457390773696,14.1863734291659,
134.815010882744)) ;
#114420 = CARTESIAN_POINT('Ctrl Pts',(-12.1814800516644,14.3643807985693,
134.59423567404)) ;
#114421 = CARTESIAN_POINT('Ctrl Pts',(-12.1044683457898,14.4754559850244,
134.336147922274)) ;
#114422 = CARTESIAN_POINT('Ctrl Pts',(-12.0208090250937,14.5110246739577,
134.058551574174)) ;
#114423 = CARTESIAN_POINT('Ctrl Pts',(-11.9378612224862,14.4687063588107,
133.783197368949)) ;
#114424 = CARTESIAN_POINT('Ctrl Pts',(-11.8615647632541,14.3514018815055,
133.527145574601)) ;
#114425 = CARTESIAN_POINT('Ctrl Pts',(-11.798502564401,14.1671964752596,133.309749293991)) ;
#114426 = CARTESIAN_POINT('Ctrl Pts',(-11.754049052173,13.9308608041133,133.146872132253)) ;
#114427 = CARTESIAN_POINT('Ctrl Pts',(-11.7316977644638,13.6570089999716,
133.048397750488)) ;
#114428 = CARTESIAN_POINT('Ctrl Pts',(-11.7341180951435,13.3664659574419,
133.022308686926)) ;
#114429 = CARTESIAN_POINT('Ctrl Pts',(-11.761720921654,13.0805681472547,133.069846022257)) ;
#114430 = CARTESIAN_POINT('Ctrl Pts',(-11.8131936002259,12.8190539470386,
133.187112979174)) ;
#114431 = CARTESIAN_POINT('Ctrl Pts',(-11.886092857491,12.5999338423892,133.366806137464)) ;
#114432 = CARTESIAN_POINT('Ctrl Pts',(-11.9747587487869,12.4413957528131,
133.592859241921)) ;
#114433 = CARTESIAN_POINT('Ctrl Pts',(-12.0748052338517,12.3520378265489,
133.85195165464)) ;
#114434 = CARTESIAN_POINT('Ctrl Pts',(-12.1791704719716,12.339734386482,134.123710421306)) ;
#114435 = CARTESIAN_POINT('Ctrl Pts',(-12.2811942198852,12.4049383167358,
134.388634754176)) ;
#114436 = CARTESIAN_POINT('Ctrl Pts',(-12.3743104910804,12.5429634979505,
134.627548525017)) ;
#114437 = CARTESIAN_POINT('Ctrl Pts',(-12.4527350962615,12.7443553986761,
134.823486021638)) ;
#114438 = CARTESIAN_POINT('Ctrl Pts',(-12.5113245953194,12.9943521537239,
134.961502568807)) ;
#114439 = CARTESIAN_POINT('Ctrl Pts',(-12.5466491191103,13.2741647768729,
135.031655728832)) ;
#114440 = CARTESIAN_POINT('Ctrl Pts',(-12.557133530808,13.565720269456,135.029118946566)) ;
#114441 = CARTESIAN_POINT('Ctrl Pts',(-12.5424084976818,13.8474315556546,
134.952884078473)) ;
#114442 = CARTESIAN_POINT('Ctrl Pts',(-12.504658245782,14.0971649669908,134.809596596871)) ;
#114443 = CARTESIAN_POINT('Ctrl Pts',(-12.4468015681524,14.3002122843455,
134.607345660129)) ;
#114444 = CARTESIAN_POINT('Ctrl Pts',(-12.3740820116557,14.4394509674979,
134.361774496034)) ;
#114445 = CARTESIAN_POINT('Ctrl Pts',(-12.2928286579386,14.5058688200503,
134.091445642351)) ;
#114446 = CARTESIAN_POINT('Ctrl Pts',(-12.2085754911848,14.4952594831202,
133.812133112469)) ;
#114447 = CARTESIAN_POINT('Ctrl Pts',(-12.1285286312613,14.4071576912799,
133.54505905862)) ;
#114448 = CARTESIAN_POINT('Ctrl Pts',(-12.0595995840032,14.2488070341169,
133.310594609379)) ;
#114449 = CARTESIAN_POINT('Ctrl Pts',(-12.007204001394,14.032332595662,133.124541926762)) ;
#114450 = CARTESIAN_POINT('Ctrl Pts',(-11.9754518623539,13.7715185673777,
132.998664946929)) ;
#114451 = CARTESIAN_POINT('Ctrl Pts',(-11.9676077024159,13.4849968555095,
132.942553623633)) ;
#114452 = CARTESIAN_POINT('Ctrl Pts',(-11.9852141495617,13.1936954317484,
132.960744777079)) ;
#114453 = CARTESIAN_POINT('Ctrl Pts',(-12.0270155274854,12.9217410981826,
133.049976934939)) ;
#114454 = CARTESIAN_POINT('Ctrl Pts',(-12.0916442917843,12.6826993167214,
133.205531163459)) ;
#114455 = CARTESIAN_POINT('Ctrl Pts',(-12.1748344849184,12.4976839220085,
133.415374259801)) ;
#114456 = CARTESIAN_POINT('Ctrl Pts',(-12.2706003786281,12.3794711428103,
133.662174391645)) ;
#114457 = CARTESIAN_POINT('Ctrl Pts',(-12.3744503899862,12.3351744196322,
133.932269165389)) ;
#114458 = CARTESIAN_POINT('Ctrl Pts',(-12.4782650208009,12.3695012763354,
134.202412750315)) ;
#114459 = CARTESIAN_POINT('Ctrl Pts',(-12.5754721648271,12.4786183736045,
134.453365352351)) ;
#114460 = CARTESIAN_POINT('Ctrl Pts',(-12.6605578265862,12.6556201701116,
134.668788412585)) ;
#114461 = CARTESIAN_POINT('Ctrl Pts',(-12.7278290779799,12.8885376957079,
134.832076052564)) ;
#114462 = CARTESIAN_POINT('Ctrl Pts',(-12.7727942038789,13.1578672277872,
134.93044163856)) ;
#114463 = CARTESIAN_POINT('Ctrl Pts',(-12.7935589960753,13.4488181058444,
134.957796140316)) ;
#114464 = CARTESIAN_POINT('Ctrl Pts',(-12.7888443918457,13.7357351250712,
134.91097260511)) ;
#114465 = CARTESIAN_POINT('Ctrl Pts',(-12.7602605916963,14.0000244154435,
134.794478626913)) ;
#114466 = CARTESIAN_POINT('Ctrl Pts',(-12.7099141607957,14.2248063693443,
134.614145960045)) ;
#114467 = CARTESIAN_POINT('Ctrl Pts',(-12.6428897963242,14.3907221531774,
134.385334239461)) ;
#114468 = CARTESIAN_POINT('Ctrl Pts',(-12.5640447774941,14.4880878052934,
134.121834427977)) ;
#114469 = CARTESIAN_POINT('Ctrl Pts',(-12.4802617689659,14.5090844515927,
133.844015139513)) ;
#114470 = CARTESIAN_POINT('Ctrl Pts',(-12.3974642832698,14.4517331277302,
133.568827359843)) ;
#114471 = CARTESIAN_POINT('Ctrl Pts',(-12.3236763447296,14.3213873494252,
133.320287858352)) ;
#114472 = CARTESIAN_POINT('Ctrl Pts',(-12.2637347152158,14.1266126254878,
133.112060420808)) ;
#114473 = CARTESIAN_POINT('Ctrl Pts',(-12.2229774667805,13.8801113803002,
132.959735466426)) ;
#114474 = CARTESIAN_POINT('Ctrl Pts',(-12.2053838579744,13.6025840232108,
132.875302084043)) ;
#114475 = CARTESIAN_POINT('Ctrl Pts',(-12.2124772397581,13.3122088978665,
132.862974191922)) ;
#114476 = CARTESIAN_POINT('Ctrl Pts',(-12.2448145015933,13.0284665595888,
132.924236901387)) ;
#114477 = CARTESIAN_POINT('Ctrl Pts',(-12.3005599019218,12.7739765033465,
133.053999198988)) ;
#114478 = CARTESIAN_POINT('Ctrl Pts',(-12.3766445028271,12.5655228915478,
133.243117582921)) ;
#114479 = CARTESIAN_POINT('Ctrl Pts',(-12.4681423855166,12.4188418488155,
133.47731500825)) ;
#114480 = CARTESIAN_POINT('Ctrl Pts',(-12.5692422546882,12.3438198182334,
133.739584235759)) ;
#114481 = CARTESIAN_POINT('Ctrl Pts',(-12.6740334889537,12.3461749880073,
134.012474638995)) ;
#114482 = CARTESIAN_POINT('Ctrl Pts',(-12.7747162224539,12.4256199459212,
134.273532924423)) ;
#114483 = CARTESIAN_POINT('Ctrl Pts',(-12.8655945356852,12.5766359900473,
134.505860328425)) ;
#114484 = CARTESIAN_POINT('Ctrl Pts',(-12.9405208029623,12.7882864475543,
134.691614915467)) ;
#114485 = CARTESIAN_POINT('Ctrl Pts',(-12.9949316879518,13.0452019382586,
134.817458837911)) ;
#114486 = CARTESIAN_POINT('Ctrl Pts',(-13.025720643168,13.3293877258915,134.874271333741)) ;
#114487 = CARTESIAN_POINT('Ctrl Pts',(-13.0313457796955,13.6204035856812,
134.857561997613)) ;
#114488 = CARTESIAN_POINT('Ctrl Pts',(-13.0121238177563,13.8971496153171,
134.768280402699)) ;
#114489 = CARTESIAN_POINT('Ctrl Pts',(-12.9702433337836,14.1397539052331,
134.612839445253)) ;
#114490 = CARTESIAN_POINT('Ctrl Pts',(-12.9092683557999,14.3313464702874,
134.401559637406)) ;
#114491 = CARTESIAN_POINT('Ctrl Pts',(-12.8346344667875,14.4574458616527,
134.150487900523)) ;
#114492 = CARTESIAN_POINT('Ctrl Pts',(-12.7520232585293,14.5099723944026,
133.876034599555)) ;
#114493 = CARTESIAN_POINT('Ctrl Pts',(-12.6680149991839,14.4843439695083,
133.597416296755)) ;
#114494 = CARTESIAN_POINT('Ctrl Pts',(-12.5898605639027,14.3827749410654,
133.336012913517)) ;
#114495 = CARTESIAN_POINT('Ctrl Pts',(-12.5235110131134,14.2124739950545,
133.109063094795)) ;
#114496 = CARTESIAN_POINT('Ctrl Pts',(-12.47454385575,13.9855789386979,132.932891873958)) ;
#114497 = CARTESIAN_POINT('Ctrl Pts',(-12.44718714331,13.7185805864342,132.819871229684)) ;
#114498 = CARTESIAN_POINT('Ctrl Pts',(-12.4441083202369,13.4303185636673,
132.777757800251)) ;
#114499 = CARTESIAN_POINT('Ctrl Pts',(-12.4662081675216,13.1417758325219,
132.809228396078)) ;
#114500 = CARTESIAN_POINT('Ctrl Pts',(-12.5128438608682,12.8725286043858,
132.912265477798)) ;
#114501 = CARTESIAN_POINT('Ctrl Pts',(-12.5811355936144,12.6435096258014,
133.078662360882)) ;
#114502 = CARTESIAN_POINT('Ctrl Pts',(-12.6670557983815,12.4701546223289,
133.296533072804)) ;
#114503 = CARTESIAN_POINT('Ctrl Pts',(-12.7650980875458,12.3650501876111,
133.549835459936)) ;
#114504 = CARTESIAN_POINT('Ctrl Pts',(-12.8692895553206,12.3357586674927,
133.821013809302)) ;
#114505 = CARTESIAN_POINT('Ctrl Pts',(-12.9722194636702,12.3843195509594,
134.088641190149)) ;
#114506 = CARTESIAN_POINT('Ctrl Pts',(-13.0679235169665,12.5073666683789,
134.335069106556)) ;
#114507 = CARTESIAN_POINT('Ctrl Pts',(-13.1498474421669,12.6958200369819,
134.541296314724)) ;
#114508 = CARTESIAN_POINT('Ctrl Pts',(-13.2130846476701,12.9363649293222,
134.692916583502)) ;
#114509 = CARTESIAN_POINT('Ctrl Pts',(-13.2537553284003,13.212046231595,134.778583028313)) ;
#114510 = CARTESIAN_POINT('Ctrl Pts',(-13.2696867588976,13.5022481067603,
134.792052779991)) ;
#114511 = CARTESIAN_POINT('Ctrl Pts',(-13.2603291226857,13.7884016128943,
134.731444216182)) ;
#114512 = CARTESIAN_POINT('Ctrl Pts',(-13.2274358441086,14.045945075732,134.602400846472)) ;
#114513 = CARTESIAN_POINT('Ctrl Pts',(-13.1734739345736,14.2610680704969,
134.41149155897)) ;
#114514 = CARTESIAN_POINT('Ctrl Pts',(-13.1038966633744,14.4145624165552,
134.175255364668)) ;
#114515 = CARTESIAN_POINT('Ctrl Pts',(-13.0234728088093,14.4980852125695,
133.907100960487)) ;
#114516 = CARTESIAN_POINT('Ctrl Pts',(-12.939325995419,14.5041312739862,133.628163299805)) ;
#114517 = CARTESIAN_POINT('Ctrl Pts',(-12.8580140805557,14.4326962339747,
133.357486536545)) ;
#114518 = CARTESIAN_POINT('Ctrl Pts',(-12.7862358410937,14.289424830309,133.114743545619)) ;
#114519 = CARTESIAN_POINT('Ctrl Pts',(-12.7294171395877,14.0826507854277,
132.915479459106)) ;
#114520 = CARTESIAN_POINT('Ctrl Pts',(-12.6931113261045,13.8312291814697,
132.77650858526)) ;
#114521 = CARTESIAN_POINT('Ctrl Pts',(-12.6798565616288,13.5479805821752,
132.704527307887)) ;
#114522 = CARTESIAN_POINT('Ctrl Pts',(-12.6918329131031,13.2572981016289,
132.706442366543)) ;
#114523 = CARTESIAN_POINT('Ctrl Pts',(-12.7286154648152,12.9781391944844,
132.780789668285)) ;
#114524 = CARTESIAN_POINT('Ctrl Pts',(-12.788841308569,12.7298471383749,132.923457407859)) ;
#114525 = CARTESIAN_POINT('Ctrl Pts',(-12.8678064119023,12.5331718510569,
133.121190067536)) ;
#114526 = CARTESIAN_POINT('Ctrl Pts',(-12.9619860922532,12.3987050488903,
133.3630746114)) ;
#114527 = CARTESIAN_POINT('Ctrl Pts',(-13.0641173669679,12.3381977133859,
133.628393862531)) ;
#114528 = CARTESIAN_POINT('Ctrl Pts',(-13.1689636586994,12.3556285786372,
133.901368958815)) ;
#114529 = CARTESIAN_POINT('Ctrl Pts',(-13.2676215267395,12.448498640132,134.156721062578)) ;
#114530 = CARTESIAN_POINT('Ctrl Pts',(-13.3562794099848,12.6124651727369,
134.382428532808)) ;
#114531 = CARTESIAN_POINT('Ctrl Pts',(-13.4274024159188,12.8330193864531,
134.55721035227)) ;
#114532 = CARTESIAN_POINT('Ctrl Pts',(-13.4778657839761,13.0981216515098,
134.671314825157)) ;
#114533 = CARTESIAN_POINT('Ctrl Pts',(-13.5037873702561,13.3840423616995,
134.714047923931)) ;
#114534 = CARTESIAN_POINT('Ctrl Pts',(-13.5047230832927,13.6738043197191,
134.683656575562)) ;
#114535 = CARTESIAN_POINT('Ctrl Pts',(-13.4810350619758,13.9458856450603,
134.581307831703)) ;
#114536 = CARTESIAN_POINT('Ctrl Pts',(-13.4350850950003,14.1805609741337,
134.413888828413)) ;
#114537 = CARTESIAN_POINT('Ctrl Pts',(-13.3713435625267,14.3602096703021,
134.19466352274)) ;
#114538 = CARTESIAN_POINT('Ctrl Pts',(-13.2941228668166,14.4737146563849,
133.935766751957)) ;
#114539 = CARTESIAN_POINT('Ctrl Pts',(-13.2111150371913,14.510981736058,133.660304806086)) ;
#114540 = CARTESIAN_POINT('Ctrl Pts',(-13.1279555516473,14.4710234538019,
133.384286573336)) ;
#114541 = CARTESIAN_POINT('Ctrl Pts',(-13.0514607207591,14.3558611755068,
133.127695259553)) ;
#114542 = CARTESIAN_POINT('Ctrl Pts',(-12.987929872837,14.1736059642118,132.908940703681)) ;
#114543 = CARTESIAN_POINT('Ctrl Pts',(-12.9427874558613,13.9381264816024,
132.743987191645)) ;
#114544 = CARTESIAN_POINT('Ctrl Pts',(-12.9198159126567,13.665192099168,132.643720985883)) ;
#114545 = CARTESIAN_POINT('Ctrl Pts',(-12.9214159568252,13.3755914984187,
132.615321479283)) ;
#114546 = CARTESIAN_POINT('Ctrl Pts',(-12.9485033871058,13.0874857506397,
132.661141600498)) ;
#114547 = CARTESIAN_POINT('Ctrl Pts',(-12.9991534842726,12.8264337657975,
132.776172659393)) ;
#114548 = CARTESIAN_POINT('Ctrl Pts',(-13.0712502877118,12.6060974389448,
132.953593799865)) ;
#114549 = CARTESIAN_POINT('Ctrl Pts',(-13.1597261697062,12.4450313389733,
133.179001034814)) ;
#114550 = CARTESIAN_POINT('Ctrl Pts',(-13.2598221399245,12.3534666197661,
133.438152169847)) ;
#114551 = CARTESIAN_POINT('Ctrl Pts',(-13.3638496997786,12.3390029903486,
133.709021457282)) ;
#114552 = CARTESIAN_POINT('Ctrl Pts',(-13.466268319613,12.4020392430349,133.975026492123)) ;
#114553 = CARTESIAN_POINT('Ctrl Pts',(-13.5598211640111,12.5385711173323,
134.215165246668)) ;
#114554 = CARTESIAN_POINT('Ctrl Pts',(-13.6383382505058,12.737337324062,134.411540597844)) ;
#114555 = CARTESIAN_POINT('Ctrl Pts',(-13.6976697861643,12.9861206892308,
134.551707741949)) ;
#114556 = CARTESIAN_POINT('Ctrl Pts',(-13.7337928936498,13.2660910782566,
134.62410596592)) ;
#114557 = CARTESIAN_POINT('Ctrl Pts',(-13.7449404119012,13.5573227840952,
134.623538746113)) ;
#114558 = CARTESIAN_POINT('Ctrl Pts',(-13.731057609949,13.8386952169897,134.549882879065)) ;
#114559 = CARTESIAN_POINT('Ctrl Pts',(-13.6938267710482,14.0906007554108,
134.407982826979)) ;
#114560 = CARTESIAN_POINT('Ctrl Pts',(-13.6366983945426,14.2945039762926,
134.207985282423)) ;
#114561 = CARTESIAN_POINT('Ctrl Pts',(-13.5643971905334,14.4361574187858,
133.963631330981)) ;
#114562 = CARTESIAN_POINT('Ctrl Pts',(-13.4829079562931,14.5051117570611,
133.692450855681)) ;
#114563 = CARTESIAN_POINT('Ctrl Pts',(-13.398865589322,14.496582620466,133.413844416583)) ;
#114564 = CARTESIAN_POINT('Ctrl Pts',(-13.3188758691256,14.4113394819302,
133.147064384826)) ;
#114565 = CARTESIAN_POINT('Ctrl Pts',(-13.2492482094451,14.2546479447355,
132.910444808226)) ;
#114566 = CARTESIAN_POINT('Ctrl Pts',(-13.1961963849046,14.039143877786,132.722400695126)) ;
#114567 = CARTESIAN_POINT('Ctrl Pts',(-13.1638347550569,13.7793416572316,
132.594749383636)) ;
#114568 = CARTESIAN_POINT('Ctrl Pts',(-13.1552775077889,13.4941095874199,
132.536650789137)) ;
#114569 = CARTESIAN_POINT('Ctrl Pts',(-13.1720447629105,13.2026874966814,
132.552397812081)) ;
#114570 = CARTESIAN_POINT('Ctrl Pts',(-13.2133004298939,12.928833346161,132.639904988231)) ;
#114571 = CARTESIAN_POINT('Ctrl Pts',(-13.2774801251183,12.6885083712283,
132.794116581438)) ;
#114572 = CARTESIAN_POINT('Ctrl Pts',(-13.3597053837363,12.5026390795781,
133.001327621254)) ;
#114573 = CARTESIAN_POINT('Ctrl Pts',(-13.455701350823,12.3816810236162,133.248611444686)) ;
#114574 = CARTESIAN_POINT('Ctrl Pts',(-13.5588450701788,12.3354826595071,
133.516837122875)) ;
#114575 = CARTESIAN_POINT('Ctrl Pts',(-13.662986257812,12.3671988660942,133.787859387829)) ;
#114576 = CARTESIAN_POINT('Ctrl Pts',(-13.7608857501055,12.4748749581507,
134.040689706046)) ;
#114577 = CARTESIAN_POINT('Ctrl Pts',(-13.8461189502053,12.6498955190515,
134.256626571108)) ;
#114578 = CARTESIAN_POINT('Ctrl Pts',(-13.9137641762851,12.8801431332148,
134.421162047123)) ;
#114579 = CARTESIAN_POINT('Ctrl Pts',(-13.959688118663,13.1504415297617,134.52210348875)) ;
#114580 = CARTESIAN_POINT('Ctrl Pts',(-13.9810355826832,13.438739202615,134.551438413197)) ;
#114581 = CARTESIAN_POINT('Ctrl Pts',(-13.9771509252308,13.7280473502378,
134.50680820225)) ;
#114582 = CARTESIAN_POINT('Ctrl Pts',(-13.9490883356948,13.9932362064335,
134.391820118097)) ;
#114583 = CARTESIAN_POINT('Ctrl Pts',(-13.899552383743,14.2186783745982,134.213988401194)) ;
#114584 = CARTESIAN_POINT('Ctrl Pts',(-13.8326088799132,14.3872014330787,
133.985246691092)) ;
#114585 = CARTESIAN_POINT('Ctrl Pts',(-13.754354251272,14.486216521528,133.723625961275)) ;
#114586 = CARTESIAN_POINT('Ctrl Pts',(-13.6703274653614,14.5095010567365,
133.444968044136)) ;
#114587 = CARTESIAN_POINT('Ctrl Pts',(-13.587915515568,14.4548476689191,133.171125957688)) ;
#114588 = CARTESIAN_POINT('Ctrl Pts',(-13.5132496102258,14.3259646517619,
132.919798090487)) ;
#114589 = CARTESIAN_POINT('Ctrl Pts',(-13.4528381497739,14.1320240566172,
132.710133322283)) ;
#114590 = CARTESIAN_POINT('Ctrl Pts',(-13.4117984923924,13.8890687487633,
132.557286539592)) ;
#114591 = CARTESIAN_POINT('Ctrl Pts',(-13.3933038950219,13.6109288487181,
132.470050146704)) ;
#114592 = CARTESIAN_POINT('Ctrl Pts',(-13.3996927101153,13.3205780973656,
132.455665139994)) ;
#114593 = CARTESIAN_POINT('Ctrl Pts',(-13.4314451231204,13.0356410236252,
132.515132416829)) ;
#114594 = CARTESIAN_POINT('Ctrl Pts',(-13.4863521726588,12.7811568557338,
132.642583088239)) ;
#114595 = CARTESIAN_POINT('Ctrl Pts',(-13.5618719439237,12.5709851276515,
132.830045482527)) ;
#114596 = CARTESIAN_POINT('Ctrl Pts',(-13.6530001533805,12.4221766619671,
133.063156221214)) ;
#114597 = CARTESIAN_POINT('Ctrl Pts',(-13.7543438242653,12.3447406812541,
133.325997758698)) ;
#114598 = CARTESIAN_POINT('Ctrl Pts',(-13.858979447707,12.3451621602759,133.598484050117)) ;
#114599 = CARTESIAN_POINT('Ctrl Pts',(-13.9595871058779,12.4221617733591,
133.859413033911)) ;
#114600 = CARTESIAN_POINT('Ctrl Pts',(-14.0509368702114,12.5713293574021,
134.093085140404)) ;
#114601 = CARTESIAN_POINT('Ctrl Pts',(-14.1263288360547,12.7811357471148,
134.280239363245)) ;
#114602 = CARTESIAN_POINT('Ctrl Pts',(-14.181464730297,13.037385413305,134.408146154191)) ;
#114603 = CARTESIAN_POINT('Ctrl Pts',(-14.2129289597319,13.3202247802994,
134.46702998844)) ;
#114604 = CARTESIAN_POINT('Ctrl Pts',(-14.2193168783918,13.6126649497902,
134.452393596522)) ;
#114605 = CARTESIAN_POINT('Ctrl Pts',(-14.2008364796894,13.889109539137,134.365400616144)) ;
#114606 = CARTESIAN_POINT('Ctrl Pts',(-14.1595000662705,14.1334576219234,
134.211477497111)) ;
#114607 = CARTESIAN_POINT('Ctrl Pts',(-14.0992466494206,14.3262010857029,
134.002423062281)) ;
#114608 = CARTESIAN_POINT('Ctrl Pts',(-14.0244678789738,14.4552702241494,
133.750713932904)) ;
#114609 = CARTESIAN_POINT('Ctrl Pts',(-13.9418997721999,14.5094659873619,
133.476364746001)) ;
#114610 = CARTESIAN_POINT('Ctrl Pts',(-13.8583861168424,14.48627928254,133.199410244325)) ;
#114611 = CARTESIAN_POINT('Ctrl Pts',(-13.7797353567973,14.3867194330965,
132.936459435104)) ;
#114612 = CARTESIAN_POINT('Ctrl Pts',(-13.7130105219871,14.2183273389604,
132.708437979387)) ;
#114613 = CARTESIAN_POINT('Ctrl Pts',(-13.6633479068396,13.9922441011096,
132.530147180322)) ;
#114614 = CARTESIAN_POINT('Ctrl Pts',(-13.6354328184579,13.7260908863955,
132.415503205816)) ;
#114615 = CARTESIAN_POINT('Ctrl Pts',(-13.6315996421401,13.4392990683917,
132.371317925094)) ;
#114616 = CARTESIAN_POINT('Ctrl Pts',(-13.6531002743803,13.1491383926391,
132.400878674979)) ;
#114617 = CARTESIAN_POINT('Ctrl Pts',(-13.6988895423874,12.880138144259,132.501583429181)) ;
#114618 = CARTESIAN_POINT('Ctrl Pts',(-13.7669016038619,12.6488312040692,
132.66702117208)) ;
#114619 = CARTESIAN_POINT('Ctrl Pts',(-13.8519661020191,12.4746173052797,
132.882564533349)) ;
#114620 = CARTESIAN_POINT('Ctrl Pts',(-13.9499918537797,12.3669410581914,
133.13572242046)) ;
#114621 = CARTESIAN_POINT('Ctrl Pts',(-14.0540803057466,12.3355244467329,
133.406613758036)) ;
#114622 = CARTESIAN_POINT('Ctrl Pts',(-14.1570770496498,12.3818824637266,
133.674448586604)) ;
#114623 = CARTESIAN_POINT('Ctrl Pts',(-14.2529156063067,12.502442440452,133.921340780179)) ;
#114624 = CARTESIAN_POINT('Ctrl Pts',(-14.3357164299663,12.6900860359651,
134.129966525958)) ;
#114625 = CARTESIAN_POINT('Ctrl Pts',(-14.3993556473891,12.9290693621117,
134.282824648329)) ;
#114626 = CARTESIAN_POINT('Ctrl Pts',(-14.4406746427025,13.2033802627449,
134.370454904131)) ;
#114627 = CARTESIAN_POINT('Ctrl Pts',(-14.4573570221151,13.493885424346,134.386064394722)) ;
#114628 = CARTESIAN_POINT('Ctrl Pts',(-14.4487939272164,13.7798208359641,
134.327863613174)) ;
#114629 = CARTESIAN_POINT('Ctrl Pts',(-14.4163591296665,14.0398147256928,
134.199973199807)) ;
#114630 = CARTESIAN_POINT('Ctrl Pts',(-14.3630430477874,14.2555980954836,
134.011057985321)) ;
#114631 = CARTESIAN_POINT('Ctrl Pts',(-14.2938516112464,14.4112165057251,
133.775932908363)) ;
#114632 = CARTESIAN_POINT('Ctrl Pts',(-14.213327419341,14.4969135755094,133.50736843725)) ;
#114633 = CARTESIAN_POINT('Ctrl Pts',(-14.1296189321524,14.5049696810031,
133.229876903082)) ;
#114634 = CARTESIAN_POINT('Ctrl Pts',(-14.0481698596881,14.4360249735447,
132.958821806314)) ;
#114635 = CARTESIAN_POINT('Ctrl Pts',(-13.9759487851369,14.2945754362065,
132.714746600477)) ;
#114636 = CARTESIAN_POINT('Ctrl Pts',(-13.9186392005941,14.0897548858671,
132.514089317548)) ;
#114637 = CARTESIAN_POINT('Ctrl Pts',(-13.8816283734556,13.8387001375239,
132.372961040856)) ;
#114638 = CARTESIAN_POINT('Ctrl Pts',(-13.86765973633,13.5574044598577,132.299056743724)) ;
#114639 = CARTESIAN_POINT('Ctrl Pts',(-13.8789956043886,13.2644130009093,
132.2988381339)) ;
#114640 = CARTESIAN_POINT('Ctrl Pts',(-13.9149994984909,12.9862195730077,
132.371090109727)) ;
#114641 = CARTESIAN_POINT('Ctrl Pts',(-13.9743502243685,12.7371111819008,
132.511275565875)) ;
#114642 = CARTESIAN_POINT('Ctrl Pts',(-14.0530557762854,12.5380203242925,
132.708138925323)) ;
#114643 = CARTESIAN_POINT('Ctrl Pts',(-14.1469276806553,12.4015272632005,
132.949117652525)) ;
#114644 = CARTESIAN_POINT('Ctrl Pts',(-14.2489833656644,12.3389470103484,
133.214189844898)) ;
#114645 = CARTESIAN_POINT('Ctrl Pts',(-14.3533226131928,12.3537864997403,
133.485861761893)) ;
#114646 = CARTESIAN_POINT('Ctrl Pts',(-14.4528614890508,12.4449099176858,
133.743576395913)) ;
#114647 = CARTESIAN_POINT('Ctrl Pts',(-14.5418561425685,12.6072327563546,
133.97027761533)) ;
#114648 = CARTESIAN_POINT('Ctrl Pts',(-14.6133813155202,12.8259751420657,
134.146289595912)) ;
#114649 = CARTESIAN_POINT('Ctrl Pts',(-14.6644626717837,13.0894865209779,
134.262268329824)) ;
#114650 = CARTESIAN_POINT('Ctrl Pts',(-14.6912354788188,13.3763086244584,
134.307339213758)) ;
#114651 = CARTESIAN_POINT('Ctrl Pts',(-14.6927780845657,13.666102426872,134.278737035569)) ;
#114652 = CARTESIAN_POINT('Ctrl Pts',(-14.6699098049705,13.9378774393092,
134.178922193569)) ;
#114653 = CARTESIAN_POINT('Ctrl Pts',(-14.6244200591529,14.174793298913,134.012730262355)) ;
#114654 = CARTESIAN_POINT('Ctrl Pts',(-14.5612019536203,14.355667987911,133.795095051057)) ;
#114655 = CARTESIAN_POINT('Ctrl Pts',(-14.4846906294762,14.4711053294092,
133.538428577137)) ;
#114656 = CARTESIAN_POINT('Ctrl Pts',(-14.4011850462511,14.511170979715,133.261273870169)) ;
#114657 = CARTESIAN_POINT('Ctrl Pts',(-14.3178410780268,14.4729025341711,
132.984673903261)) ;
#114658 = CARTESIAN_POINT('Ctrl Pts',(-14.2414431710577,14.3605014183323,
132.728538157581)) ;
#114659 = CARTESIAN_POINT('Ctrl Pts',(-14.1770966200207,14.1789799497678,
132.507210107387)) ;
#114660 = CARTESIAN_POINT('Ctrl Pts',(-14.1315848885081,13.9453130755044,
132.341277366815)) ;
#114661 = CARTESIAN_POINT('Ctrl Pts',(-14.1079390036142,13.673613297581,132.239086339493)) ;
#114662 = CARTESIAN_POINT('Ctrl Pts',(-14.1087830481224,13.3843416477693,
132.208491884339)) ;
#114663 = CARTESIAN_POINT('Ctrl Pts',(-14.1351400941846,13.0956424787648,
132.252157038047)) ;
#114664 = CARTESIAN_POINT('Ctrl Pts',(-14.1851403795369,12.8335787485534,
132.365283706234)) ;
#114665 = CARTESIAN_POINT('Ctrl Pts',(-14.2566883427613,12.6116522531053,
132.541092961402)) ;
#114666 = CARTESIAN_POINT('Ctrl Pts',(-14.3449178102994,12.4486058050818,
132.765728820733)) ;
#114667 = CARTESIAN_POINT('Ctrl Pts',(-14.4444094609299,12.3551665981467,
133.023238128206)) ;
#114668 = CARTESIAN_POINT('Ctrl Pts',(-14.5487260750023,12.3383111368361,
133.294844327139)) ;
#114669 = CARTESIAN_POINT('Ctrl Pts',(-14.651135777708,12.3991318667188,133.560878201396)) ;
#114670 = CARTESIAN_POINT('Ctrl Pts',(-14.7450247980916,12.5336133546432,
133.801997324254)) ;
#114671 = CARTESIAN_POINT('Ctrl Pts',(-14.8240658891889,12.7304747525644,
133.999922781035)) ;
#114672 = CARTESIAN_POINT('Ctrl Pts',(-14.8843591623108,12.9801493565206,
134.142645016146)) ;
#114673 = CARTESIAN_POINT('Ctrl Pts',(-14.9207776314118,13.2569930870622,
134.216214669517)) ;
#114674 = CARTESIAN_POINT('Ctrl Pts',(-14.9327904526555,13.5493201067258,
134.218039568247)) ;
#114675 = CARTESIAN_POINT('Ctrl Pts',(-14.9195608823309,13.8310609228274,
134.146315593606)) ;
#114676 = CARTESIAN_POINT('Ctrl Pts',(-14.8829071658904,14.0843638099265,
134.006060198745)) ;
#114677 = CARTESIAN_POINT('Ctrl Pts',(-14.8262774665716,14.2896244491401,
133.807537482938)) ;
#114678 = CARTESIAN_POINT('Ctrl Pts',(-14.7544509561564,14.4330063116879,
133.564623744753)) ;
#114679 = CARTESIAN_POINT('Ctrl Pts',(-14.6730981695364,14.5042107415309,
133.293824015626)) ;
#114680 = CARTESIAN_POINT('Ctrl Pts',(-14.5890044461905,14.4979449999679,
133.015056574469)) ;
#114681 = CARTESIAN_POINT('Ctrl Pts',(-14.5085811345525,14.4144601779744,
132.746912885546)) ;
#114682 = CARTESIAN_POINT('Ctrl Pts',(-14.4386966820867,14.2595209902124,
132.509575163383)) ;
#114683 = CARTESIAN_POINT('Ctrl Pts',(-14.3852681727933,14.046214919979,132.32053362023)) ;
#114684 = CARTESIAN_POINT('Ctrl Pts',(-14.3521879692475,13.7868053449528,
132.190703349274)) ;
#114685 = CARTESIAN_POINT('Ctrl Pts',(-14.3429850788203,13.5027357390144,
132.130803960272)) ;
#114686 = CARTESIAN_POINT('Ctrl Pts',(-14.3589256787532,13.2114164567146,
132.144166678592)) ;
#114687 = CARTESIAN_POINT('Ctrl Pts',(-14.3996479591576,12.9359342983456,
132.230005501464)) ;
#114688 = CARTESIAN_POINT('Ctrl Pts',(-14.4630310316759,12.6951562018299,
132.381999972268)) ;
#114689 = CARTESIAN_POINT('Ctrl Pts',(-14.5447779273386,12.5073061272103,
132.587797294127)) ;
#114690 = CARTESIAN_POINT('Ctrl Pts',(-14.6405874915994,12.3841592686752,
132.834495044115)) ;
#114691 = CARTESIAN_POINT('Ctrl Pts',(-14.7436396651289,12.3356200239572,
133.102447533053)) ;
#114692 = CARTESIAN_POINT('Ctrl Pts',(-14.8482334000072,12.3655842279676,
133.374661826652)) ;
#114693 = CARTESIAN_POINT('Ctrl Pts',(-14.9456378863924,12.4702048591763,
133.62631542447)) ;
#114694 = CARTESIAN_POINT('Ctrl Pts',(-15.032031341998,12.6448837976238,133.845354670619)) ;
#114695 = CARTESIAN_POINT('Ctrl Pts',(-15.0997909854076,12.872508423284,134.010430965611)) ;
#114696 = CARTESIAN_POINT('Ctrl Pts',(-15.1466624677231,13.1434988331289,
134.11394299587)) ;
#114697 = CARTESIAN_POINT('Ctrl Pts',(-15.1684830221252,13.4301737780494,
134.144821454034)) ;
#114698 = CARTESIAN_POINT('Ctrl Pts',(-15.1655029363779,13.7187795914099,
134.102960274335)) ;
#114699 = CARTESIAN_POINT('Ctrl Pts',(-15.137871807278,13.9870154433738,133.988964277523)) ;
#114700 = CARTESIAN_POINT('Ctrl Pts',(-15.089103500937,14.2124398345738,133.813561355081)) ;
#114701 = CARTESIAN_POINT('Ctrl Pts',(-15.0226861816082,14.3830654461858,
133.586365342099)) ;
#114702 = CARTESIAN_POINT('Ctrl Pts',(-14.9442977084689,14.4846609541733,
133.324197217531)) ;
#114703 = CARTESIAN_POINT('Ctrl Pts',(-14.8603045751173,14.5097913616969,
133.045629352813)) ;
#114704 = CARTESIAN_POINT('Ctrl Pts',(-14.7781158124174,14.4576093080194,
132.772584210679)) ;
#114705 = CARTESIAN_POINT('Ctrl Pts',(-14.7029379087114,14.3304831317374,
132.519675058584)) ;
#114706 = CARTESIAN_POINT('Ctrl Pts',(-14.6421746060609,14.1386183822934,
132.309056084948)) ;
#114707 = CARTESIAN_POINT('Ctrl Pts',(-14.6004669656827,13.8965846856625,
132.154209706835)) ;
#114708 = CARTESIAN_POINT('Ctrl Pts',(-14.5812880337956,13.6198365630073,
132.065057969682)) ;
#114709 = CARTESIAN_POINT('Ctrl Pts',(-14.5869544254102,13.3288844737818,
132.048478781958)) ;
#114710 = CARTESIAN_POINT('Ctrl Pts',(-14.6178077703533,13.0447399832046,
132.105475686592)) ;
#114711 = CARTESIAN_POINT('Ctrl Pts',(-14.6721136258845,12.7881836368688,
132.231068090543)) ;
#114712 = CARTESIAN_POINT('Ctrl Pts',(-14.7475386699193,12.5755910115287,
132.418091523374)) ;
#114713 = CARTESIAN_POINT('Ctrl Pts',(-14.8378940236856,12.4257574465567,
132.649102005788)) ;
#114714 = CARTESIAN_POINT('Ctrl Pts',(-14.9388209084364,12.3460112405744,
132.910787274949)) ;
#114715 = CARTESIAN_POINT('Ctrl Pts',(-15.0435737078647,12.3439532504127,
133.183578235088)) ;
#114716 = CARTESIAN_POINT('Ctrl Pts',(-15.1446091167616,12.4188218900739,
133.445686307793)) ;
#114717 = CARTESIAN_POINT('Ctrl Pts',(-15.2365998734713,12.5668341062151,
133.681113263233)) ;
#114718 = CARTESIAN_POINT('Ctrl Pts',(-15.3120455807105,12.7739565310488,
133.868616342754)) ;
#114719 = CARTESIAN_POINT('Ctrl Pts',(-15.3679671650309,13.0292275295923,
133.998784482597)) ;
#114720 = CARTESIAN_POINT('Ctrl Pts',(-15.4001513908772,13.3121167714202,
134.059708256056)) ;
#114721 = CARTESIAN_POINT('Ctrl Pts',(-15.407302294284,13.6036711588795,134.047415072482)) ;
#114722 = CARTESIAN_POINT('Ctrl Pts',(-15.3894117903854,13.8822010088686,
133.961971555951)) ;
#114723 = CARTESIAN_POINT('Ctrl Pts',(-15.3488581880954,14.126534024312,133.810499271449)) ;
#114724 = CARTESIAN_POINT('Ctrl Pts',(-15.2890058404676,14.3215277156221,
133.602541497692)) ;
#114725 = CARTESIAN_POINT('Ctrl Pts',(-15.2146261037101,14.4523872469144,
133.352036701433)) ;
#114726 = CARTESIAN_POINT('Ctrl Pts',(-15.132276398967,14.509081269933,133.078352393805)) ;
#114727 = CARTESIAN_POINT('Ctrl Pts',(-15.048156334803,14.4877530584647,132.799404216537)) ;
#114728 = CARTESIAN_POINT('Ctrl Pts',(-14.9697741972722,14.3906972492053,
132.537447195776)) ;
#114729 = CARTESIAN_POINT('Ctrl Pts',(-14.9025432118204,14.2242127265294,
132.307919886886)) ;
#114730 = CARTESIAN_POINT('Ctrl Pts',(-14.8524134830202,14.0000453961231,
132.128331876439)) ;
#114731 = CARTESIAN_POINT('Ctrl Pts',(-14.8236827135926,13.7349941187306,
132.011308130338)) ;
#114732 = CARTESIAN_POINT('Ctrl Pts',(-14.8192110157222,13.4462938086935,
131.964998461715)) ;
#114733 = CARTESIAN_POINT('Ctrl Pts',(-14.8397608257614,13.1586524064852,
131.992109164985)) ;
#114734 = CARTESIAN_POINT('Ctrl Pts',(-14.8852506544382,12.8863235925418,
132.091631205511)) ;
#114735 = CARTESIAN_POINT('Ctrl Pts',(-14.952306886852,12.6553854575325,132.254505839022)) ;
#114736 = CARTESIAN_POINT('Ctrl Pts',(-15.036993538522,12.4787538591612,132.468885463633)) ;
#114737 = CARTESIAN_POINT('Ctrl Pts',(-15.1351325127102,12.3688114822916,
132.722256615459)) ;
#114738 = CARTESIAN_POINT('Ctrl Pts',(-15.2387002100067,12.3354319136936,
132.991765834986)) ;
#114739 = CARTESIAN_POINT('Ctrl Pts',(-15.3419020299315,12.3792576310417,
133.260178529464)) ;
#114740 = CARTESIAN_POINT('Ctrl Pts',(-15.4385746866519,12.4988398999205,
133.509304414363)) ;
#114741 = CARTESIAN_POINT('Ctrl Pts',(-15.5211785051019,12.6835118512005,
133.71760539492)) ;
#114742 = CARTESIAN_POINT('Ctrl Pts',(-15.585614912484,12.9214923912795,133.872725040323)) ;
#114743 = CARTESIAN_POINT('Ctrl Pts',(-15.6276593796861,13.1954916424955,
133.96242929729)) ;
#114744 = CARTESIAN_POINT('Ctrl Pts',(-15.6450448286836,13.4865485670219,
133.980012149667)) ;
#114745 = CARTESIAN_POINT('Ctrl Pts',(-15.6370948847114,13.772471589557,133.923647448758)) ;
#114746 = CARTESIAN_POINT('Ctrl Pts',(-15.6054576941134,14.0322259092952,
133.798239163953)) ;
#114747 = CARTESIAN_POINT('Ctrl Pts',(-15.5528532090993,14.2496185339524,
133.611440842472)) ;
#114748 = CARTESIAN_POINT('Ctrl Pts',(-15.483617346609,14.4079186586772,133.375986031408)) ;
#114749 = CARTESIAN_POINT('Ctrl Pts',(-15.4040148005417,14.495128940057,133.110405781656)) ;
#114750 = CARTESIAN_POINT('Ctrl Pts',(-15.3198980850125,14.5060206783235,
132.831544484233)) ;
#114751 = CARTESIAN_POINT('Ctrl Pts',(-15.2380342056834,14.4388851972431,
132.55918054693)) ;
#114752 = CARTESIAN_POINT('Ctrl Pts',(-15.1654389797841,14.2990479598781,
132.313981427395)) ;
#114753 = CARTESIAN_POINT('Ctrl Pts',(-15.107816605712,14.096277092635,132.112499036057)) ;
#114754 = CARTESIAN_POINT('Ctrl Pts',(-15.0701124492741,13.8463552274942,
131.969338122834)) ;
#114755 = CARTESIAN_POINT('Ctrl Pts',(-15.05554407707,13.5643762793268,131.893541407323)) ;
#114756 = CARTESIAN_POINT('Ctrl Pts',(-15.0659585050918,13.2747380866486,
131.891020251149)) ;
#114757 = CARTESIAN_POINT('Ctrl Pts',(-15.101446630055,12.9934296976024,131.961474427387)) ;
#114758 = CARTESIAN_POINT('Ctrl Pts',(-15.1601039100246,12.7438068041656,
132.099715492444)) ;
#114759 = CARTESIAN_POINT('Ctrl Pts',(-15.2384724882155,12.5426943442427,
132.295520501906)) ;
#114760 = CARTESIAN_POINT('Ctrl Pts',(-15.3316626347415,12.4046936236787,
132.534630966333)) ;
#114761 = CARTESIAN_POINT('Ctrl Pts',(-15.4337983976848,12.3396331759052,
132.799852893319)) ;
#114762 = CARTESIAN_POINT('Ctrl Pts',(-15.5380451833256,12.3522550875064,
133.071297592341)) ;
#114763 = CARTESIAN_POINT('Ctrl Pts',(-15.6378149553019,12.441158614988,133.329684714748)) ;
#114764 = CARTESIAN_POINT('Ctrl Pts',(-15.7271824288003,12.6013769713038,
133.55749869446)) ;
#114765 = CARTESIAN_POINT('Ctrl Pts',(-15.799387164279,12.819071640269,133.735430014399)) ;
#114766 = CARTESIAN_POINT('Ctrl Pts',(-15.8509954325536,13.0807346140254,
133.853055281245)) ;
#114767 = CARTESIAN_POINT('Ctrl Pts',(-15.8785701981475,13.3675408612144,
133.900413861765)) ;
#114768 = CARTESIAN_POINT('Ctrl Pts',(-15.880950069095,13.6570979280699,133.874320504545)) ;
#114769 = CARTESIAN_POINT('Ctrl Pts',(-15.8584614917164,13.9319893911641,
133.775308859387)) ;
#114770 = CARTESIAN_POINT('Ctrl Pts',(-15.8140300794619,14.1676085258846,
133.612576918087)) ;
#114771 = CARTESIAN_POINT('Ctrl Pts',(-15.7508365618172,14.3519029604138,
133.394745430706)) ;
#114772 = CARTESIAN_POINT('Ctrl Pts',(-15.6747542377325,14.4687263868581,
133.139424327783)) ;
#114773 = CARTESIAN_POINT('Ctrl Pts',(-15.5916310901521,14.5110206744739,
132.86348513324)) ;
#114774 = CARTESIAN_POINT('Ctrl Pts',(-15.5082277554707,14.4754839101951,
132.586740900539)) ;
#114775 = CARTESIAN_POINT('Ctrl Pts',(-15.4310148106346,14.3641243881349,
132.327975519891)) ;
#114776 = CARTESIAN_POINT('Ctrl Pts',(-15.366796148105,14.1859981150162,132.10732571318)) ;
#114777 = CARTESIAN_POINT('Ctrl Pts',(-15.3203690301936,13.9527739629267,
131.938549874937)) ;
#114778 = CARTESIAN_POINT('Ctrl Pts',(-15.2960642034895,13.6818171869407,
131.83443758756)) ;
#114779 = CARTESIAN_POINT('Ctrl Pts',(-15.2962284106988,13.3923456599437,
131.801803057666)) ;
#114780 = CARTESIAN_POINT('Ctrl Pts',(-15.3217088635482,13.1044625348289,
131.843052348479)) ;
#114781 = CARTESIAN_POINT('Ctrl Pts',(-15.3712895624886,12.8400820200563,
131.954780479996)) ;
#114782 = CARTESIAN_POINT('Ctrl Pts',(-15.4421215709794,12.6174283224968,
132.128595071256)) ;
#114783 = CARTESIAN_POINT('Ctrl Pts',(-15.5300656767636,12.4521814963559,
132.352341736955)) ;
#114784 = CARTESIAN_POINT('Ctrl Pts',(-15.6293654089259,12.3567835155047,
132.609283754024)) ;
#114785 = CARTESIAN_POINT('Ctrl Pts',(-15.7333497867975,12.3377092271658,
132.880009523703)) ;
#114786 = CARTESIAN_POINT('Ctrl Pts',(-15.8360089773108,12.3962076032604,
133.146742886939)) ;
#114787 = CARTESIAN_POINT('Ctrl Pts',(-15.930453723468,12.5290432373042,133.389409066584)) ;
#114788 = CARTESIAN_POINT('Ctrl Pts',(-16.009869584066,12.7244085230837,133.588441629327)) ;
#114789 = CARTESIAN_POINT('Ctrl Pts',(-16.0704566796156,12.9709500550387,
133.732258312717)) ;
#114790 = CARTESIAN_POINT('Ctrl Pts',(-16.1079755146477,13.2494402817627,
133.808760193825)) ;
#114791 = CARTESIAN_POINT('Ctrl Pts',(-16.1205567949924,13.5418967084717,
133.812230503726)) ;
#114792 = CARTESIAN_POINT('Ctrl Pts',(-16.1080660019669,13.8230883914708,
133.742789063125)) ;
#114793 = CARTESIAN_POINT('Ctrl Pts',(-16.0720612901439,14.0775910910953,
133.604421793909)) ;
#114794 = CARTESIAN_POINT('Ctrl Pts',(-16.016031312662,14.2842118886259,133.407692540579)) ;
#114795 = CARTESIAN_POINT('Ctrl Pts',(-15.9444811188164,14.4299775435325,
133.165534218954)) ;
#114796 = CARTESIAN_POINT('Ctrl Pts',(-15.8629277653847,14.503331032243,132.894001914259)) ;
#114797 = CARTESIAN_POINT('Ctrl Pts',(-15.7793496289803,14.4992417837061,
132.616952244808)) ;
#114798 = CARTESIAN_POINT('Ctrl Pts',(-15.6984734089822,14.4177939822546,
132.347381532007)) ;
#114799 = CARTESIAN_POINT('Ctrl Pts',(-15.6283650852396,14.2650806147523,
132.109470216545)) ;
#114800 = CARTESIAN_POINT('Ctrl Pts',(-15.5743268050137,14.0529681509037,
131.918590385591)) ;
#114801 = CARTESIAN_POINT('Ctrl Pts',(-15.5406403700371,13.7955270319932,
131.787101135372)) ;
#114802 = CARTESIAN_POINT('Ctrl Pts',(-15.5306638256876,13.5095709535078,
131.724666349948)) ;
#114803 = CARTESIAN_POINT('Ctrl Pts',(-15.5460171831695,13.2189036520177,
131.736403340103)) ;
#114804 = CARTESIAN_POINT('Ctrl Pts',(-15.5859137154081,12.9437120966298,
131.819943466577)) ;
#114805 = CARTESIAN_POINT('Ctrl Pts',(-15.6485475179313,12.7018113312773,
131.969792071976)) ;
#114806 = CARTESIAN_POINT('Ctrl Pts',(-15.7301725881226,12.5115374792667,
132.175093619939)) ;
#114807 = CARTESIAN_POINT('Ctrl Pts',(-15.8255194984171,12.3865362509785,
132.420501324227)) ;
#114808 = CARTESIAN_POINT('Ctrl Pts',(-15.9289904176059,12.3360647683775,
132.689500393083)) ;
#114809 = CARTESIAN_POINT('Ctrl Pts',(-16.0322109432962,12.3630945002041,
132.958176956719)) ;
#114810 = CARTESIAN_POINT('Ctrl Pts',(-16.1310535797055,12.4665769548229,
133.213630713827)) ;
#114811 = CARTESIAN_POINT('Ctrl Pts',(-16.2171162898203,12.637873730405,133.432016347732)) ;
#114812 = CARTESIAN_POINT('Ctrl Pts',(-16.2861070614099,12.8661806742055,
133.600365416687)) ;
#114813 = CARTESIAN_POINT('Ctrl Pts',(-16.3331577984964,13.1333277515124,
133.704775971435)) ;
#114814 = CARTESIAN_POINT('Ctrl Pts',(-16.3560616077762,13.4221934836715,
133.738517459493)) ;
#114815 = CARTESIAN_POINT('Ctrl Pts',(-16.3536937500244,13.7107571318464,
133.698487549138)) ;
#114816 = CARTESIAN_POINT('Ctrl Pts',(-16.3267795290435,13.9798563780996,
133.58659147111)) ;
#114817 = CARTESIAN_POINT('Ctrl Pts',(-16.2784408821239,14.2070905580459,
133.412375341533)) ;
#114818 = CARTESIAN_POINT('Ctrl Pts',(-16.2125397227886,14.3790287482914,
133.186748864503)) ;
#114819 = CARTESIAN_POINT('Ctrl Pts',(-16.1346594708171,14.4826462514907,
132.926162382995)) ;
#114820 = CARTESIAN_POINT('Ctrl Pts',(-16.0504302213959,14.5101765749395,
132.646782279628)) ;
#114821 = CARTESIAN_POINT('Ctrl Pts',(-15.9682674268405,14.4602521093363,
132.373878730922)) ;
#114822 = CARTESIAN_POINT('Ctrl Pts',(-15.892694390541,14.3349863303821,132.119771873462)) ;
#114823 = CARTESIAN_POINT('Ctrl Pts',(-15.8317129503708,14.1459036519263,
131.908681279387)) ;
#114824 = CARTESIAN_POINT('Ctrl Pts',(-15.7891216920241,13.9042674567381,
131.751109063095)) ;
#114825 = CARTESIAN_POINT('Ctrl Pts',(-15.7692741641614,13.6274934121279,
131.659929127433)) ;
#114826 = CARTESIAN_POINT('Ctrl Pts',(-15.774240842792,13.3375401227482,131.641402457855)) ;
#114827 = CARTESIAN_POINT('Ctrl Pts',(-15.8042482653973,13.0529656397982,
131.695949415826)) ;
#114828 = CARTESIAN_POINT('Ctrl Pts',(-15.8584516986935,12.793542004979,131.820979830249)) ;
#114829 = CARTESIAN_POINT('Ctrl Pts',(-15.9326864597706,12.5815361452067,
132.004842248444)) ;
#114830 = CARTESIAN_POINT('Ctrl Pts',(-16.0230837910625,12.4287258471182,
132.235797836759)) ;
#114831 = CARTESIAN_POINT('Ctrl Pts',(-16.1240643432101,12.3470719994747,
132.497574210549)) ;
#114832 = CARTESIAN_POINT('Ctrl Pts',(-16.2285925774014,12.3430683223392,
132.769776197563)) ;
#114833 = CARTESIAN_POINT('Ctrl Pts',(-16.3294552263757,12.4155936091128,
133.031491197843)) ;
#114834 = CARTESIAN_POINT('Ctrl Pts',(-16.42158697565,12.5608875783812,133.267432939441)) ;
#114835 = CARTESIAN_POINT('Ctrl Pts',(-16.4979791687381,12.7672957855937,
133.457539227448)) ;
#114836 = CARTESIAN_POINT('Ctrl Pts',(-16.5545469684218,13.0219896288371,
133.589546147221)) ;
#114837 = CARTESIAN_POINT('Ctrl Pts',(-16.5873216769804,13.3035436342973,
133.652289558074)) ;
#114838 = CARTESIAN_POINT('Ctrl Pts',(-16.5952372158022,13.5948422510341,
133.642264450776)) ;
#114839 = CARTESIAN_POINT('Ctrl Pts',(-16.5781262828345,13.8739529691167,
133.559117325056)) ;
#114840 = CARTESIAN_POINT('Ctrl Pts',(-16.5380768677347,14.1203174233417,
133.409012301568)) ;
#114841 = CARTESIAN_POINT('Ctrl Pts',(-16.4787184094645,14.3167168643634,
133.20251930448)) ;
#114842 = CARTESIAN_POINT('Ctrl Pts',(-16.4048795075091,14.4494066861711,
132.953678390524)) ;
#114843 = CARTESIAN_POINT('Ctrl Pts',(-16.3225697948458,14.5084702688582,
132.680063070833)) ;
#114844 = CARTESIAN_POINT('Ctrl Pts',(-16.2386731326133,14.489700746972,132.401879914645)) ;
#114845 = CARTESIAN_POINT('Ctrl Pts',(-16.159666302226,14.3946106074975,132.13794942029)) ;
#114846 = CARTESIAN_POINT('Ctrl Pts',(-16.0919372674924,14.2294635345246,
131.906906848158)) ;
#114847 = CARTESIAN_POINT('Ctrl Pts',(-16.0414142644033,14.0073333887475,
131.726263966149)) ;
#114848 = CARTESIAN_POINT('Ctrl Pts',(-16.0120005571222,13.7435828448799,
131.607279354952)) ;
#114849 = CARTESIAN_POINT('Ctrl Pts',(-16.0067413555039,13.454824745877,131.558621231445)) ;
#114850 = CARTESIAN_POINT('Ctrl Pts',(-16.0266816029947,13.1663898496403,
131.58388276017)) ;
#114851 = CARTESIAN_POINT('Ctrl Pts',(-16.071174096646,12.8948251888563,131.680693404511)) ;
#114852 = CARTESIAN_POINT('Ctrl Pts',(-16.1378143759152,12.6613614393991,
131.842219614895)) ;
#114853 = CARTESIAN_POINT('Ctrl Pts',(-16.2222899580583,12.4827884864443,
132.055914031115)) ;
#114854 = CARTESIAN_POINT('Ctrl Pts',(-16.3195947643377,12.3713198999723,
132.307032186213)) ;
#114855 = CARTESIAN_POINT('Ctrl Pts',(-16.42316155049,12.3351536539427,132.576506572357)) ;
#114856 = CARTESIAN_POINT('Ctrl Pts',(-16.5269587087536,12.3771106003778,
132.846499102918)) ;
#114857 = CARTESIAN_POINT('Ctrl Pts',(-16.6232634802675,12.493746042562,133.094781650953)) ;
#114858 = CARTESIAN_POINT('Ctrl Pts',(-16.7066715515362,12.6767291405437,
133.30534152523)) ;
#114859 = CARTESIAN_POINT('Ctrl Pts',(-16.7719969184263,12.9147362953278,
133.462888792416)) ;
#114860 = CARTESIAN_POINT('Ctrl Pts',(-16.8145117924752,13.1870897175325,
133.554081812245)) ;
#114861 = CARTESIAN_POINT('Ctrl Pts',(-16.832664410647,13.4771402294594,133.573993886311)) ;
#114862 = CARTESIAN_POINT('Ctrl Pts',(-16.8255195547471,13.7642376991577,
133.519905575425)) ;
#114863 = CARTESIAN_POINT('Ctrl Pts',(-16.7943070458963,14.0261140050281,
133.395578546783)) ;
#114864 = CARTESIAN_POINT('Ctrl Pts',(-16.7424882598997,14.2437566095146,
133.211251228587)) ;
#114865 = CARTESIAN_POINT('Ctrl Pts',(-16.6736113908412,14.4043004510961,
132.976804095223)) ;
#114866 = CARTESIAN_POINT('Ctrl Pts',(-16.5942186823598,14.4936451763547,
132.711836822872)) ;
#114867 = CARTESIAN_POINT('Ctrl Pts',(-16.5101466580755,14.5067755223083,
132.433108081231)) ;
#114868 = CARTESIAN_POINT('Ctrl Pts',(-16.4282410882398,14.4421251633059,
132.160681842967)) ;
#114869 = CARTESIAN_POINT('Ctrl Pts',(-16.3551632521983,14.3039891726026,
131.914003956164)) ;
#114870 = CARTESIAN_POINT('Ctrl Pts',(-16.2972497108617,14.1040922169467,
131.711842779145)) ;
#114871 = CARTESIAN_POINT('Ctrl Pts',(-16.2585983326173,13.8535852347893,
131.565668552377)) ;
#114872 = CARTESIAN_POINT('Ctrl Pts',(-16.243420453165,13.5730952435811,131.488208101679)) ;
#114873 = CARTESIAN_POINT('Ctrl Pts',(-16.2531006198612,13.2829861782011,
131.483481649537)) ;
#114874 = CARTESIAN_POINT('Ctrl Pts',(-16.2877661805878,13.0017737284941,
131.551621835108)) ;
#114875 = CARTESIAN_POINT('Ctrl Pts',(-16.3459738367156,12.7500890797144,
131.688431825914)) ;
#114876 = CARTESIAN_POINT('Ctrl Pts',(-16.4238184818004,12.5475577998432,
131.882729415997)) ;
#114877 = CARTESIAN_POINT('Ctrl Pts',(-16.5167586194788,12.4075652478031,
132.121078295711)) ;
#114878 = CARTESIAN_POINT('Ctrl Pts',(-16.6183907518262,12.3405227377109,
132.384938789592)) ;
#114879 = CARTESIAN_POINT('Ctrl Pts',(-16.7229364475564,12.3506975715296,
132.657173213167)) ;
#114880 = CARTESIAN_POINT('Ctrl Pts',(-16.8232859030364,12.438177489278,132.917122022405)) ;
#114881 = CARTESIAN_POINT('Ctrl Pts',(-16.9125712124386,12.5958827964123,
133.1448620791)) ;
#114882 = CARTESIAN_POINT('Ctrl Pts',(-16.9854582743437,12.8123887822574,
133.324729525533)) ;
#114883 = CARTESIAN_POINT('Ctrl Pts',(-17.037709893631,13.0732934241726,133.444215844693)) ;
#114884 = CARTESIAN_POINT('Ctrl Pts',(-17.0659638164382,13.3601444544887,
133.493509177191)) ;
#114885 = CARTESIAN_POINT('Ctrl Pts',(-17.0689675284249,13.6487324697402,
133.469363185352)) ;
#114886 = CARTESIAN_POINT('Ctrl Pts',(-17.0474035047278,13.9231969052117,
133.37321432911)) ;
#114887 = CARTESIAN_POINT('Ctrl Pts',(-17.0033733673897,14.1616648845749,
133.211459633651)) ;
#114888 = CARTESIAN_POINT('Ctrl Pts',(-16.9406158991401,14.3474885130478,
132.994912465869)) ;
#114889 = CARTESIAN_POINT('Ctrl Pts',(-16.864876505793,14.4664584587802,132.740606759249)) ;
#114890 = CARTESIAN_POINT('Ctrl Pts',(-16.7814776117931,14.5109046603937,
132.463712586271)) ;
#114891 = CARTESIAN_POINT('Ctrl Pts',(-16.6983907346783,14.477538406395,132.188050973166)) ;
#114892 = CARTESIAN_POINT('Ctrl Pts',(-16.6207705482251,14.3681997132881,
131.928042842248)) ;
#114893 = CARTESIAN_POINT('Ctrl Pts',(-16.5561356079281,14.19161807787,131.706168442298)) ;
#114894 = CARTESIAN_POINT('Ctrl Pts',(-16.5092308734292,13.9603524956053,
131.536079167786)) ;
#114895 = CARTESIAN_POINT('Ctrl Pts',(-16.4841796106604,13.6895220911817,
131.429699941359)) ;
#114896 = CARTESIAN_POINT('Ctrl Pts',(-16.4836919093705,13.4007319641459,
131.395211960917)) ;
#114897 = CARTESIAN_POINT('Ctrl Pts',(-16.5082964988508,13.1132078283894,
131.433992211526)) ;
#114898 = CARTESIAN_POINT('Ctrl Pts',(-16.5574784700436,12.8466068578935,
131.544388229293)) ;
#114899 = CARTESIAN_POINT('Ctrl Pts',(-16.6273997075169,12.6236984730367,
131.715716955648)) ;
#114900 = CARTESIAN_POINT('Ctrl Pts',(-16.7150468521775,12.4561011970055,
131.938529922164)) ;
#114901 = CARTESIAN_POINT('Ctrl Pts',(-16.8139682824648,12.3585968124196,
132.194412407875)) ;
#114902 = CARTESIAN_POINT('Ctrl Pts',(-16.9182265147246,12.3371246735504,
132.465833558649)) ;
#114903 = CARTESIAN_POINT('Ctrl Pts',(-17.0209026074425,12.3935413485491,
132.732653318412)) ;
#114904 = CARTESIAN_POINT('Ctrl Pts',(-17.1153756443262,12.5236723848828,
132.975519307564)) ;
#114905 = CARTESIAN_POINT('Ctrl Pts',(-17.1956555914022,12.7179304240541,
133.176947444366)) ;
#114906 = CARTESIAN_POINT('Ctrl Pts',(-17.2569924030211,12.9643000603806,
133.322838842009)) ;
#114907 = CARTESIAN_POINT('Ctrl Pts',(-17.2949538933717,13.2410161239663,
133.400773057716)) ;
#114908 = CARTESIAN_POINT('Ctrl Pts',(-17.3083412632257,13.5320326358814,
133.40675253041)) ;
#114909 = CARTESIAN_POINT('Ctrl Pts',(-17.2965889183178,13.8151976332958,
133.339306952295)) ;
#114910 = CARTESIAN_POINT('Ctrl Pts',(-17.2611712342104,14.070965110173,133.202631251777)) ;
#114911 = CARTESIAN_POINT('Ctrl Pts',(-17.2055219190199,14.2795161854134,
133.006946181317)) ;
#114912 = CARTESIAN_POINT('Ctrl Pts',(-17.1344526197165,14.4266233568165,
132.766264881813)) ;
#114913 = CARTESIAN_POINT('Ctrl Pts',(-17.0535835623515,14.5021444966585,
132.496922447555)) ;
#114914 = CARTESIAN_POINT('Ctrl Pts',(-16.9693534559784,14.5004799279669,
132.217713549754)) ;
#114915 = CARTESIAN_POINT('Ctrl Pts',(-16.8885085804287,14.4210758361391,
131.948320350664)) ;
#114916 = CARTESIAN_POINT('Ctrl Pts',(-16.818249196986,14.2711637356508,131.710095463003)) ;
#114917 = CARTESIAN_POINT('Ctrl Pts',(-16.7633840110066,14.0600320259714,
131.516677712646)) ;
#114918 = CARTESIAN_POINT('Ctrl Pts',(-16.729034656478,13.8025046463563,131.383125760343)) ;
#114919 = CARTESIAN_POINT('Ctrl Pts',(-16.7184105236858,13.5194350300881,
131.319077858953)) ;
#114920 = CARTESIAN_POINT('Ctrl Pts',(-16.7329082611137,13.227929848522,131.328230796269)) ;
#114921 = CARTESIAN_POINT('Ctrl Pts',(-16.7721540100418,12.9514279979351,
131.409809044102)) ;
#114922 = CARTESIAN_POINT('Ctrl Pts',(-16.834426980546,12.7076270254922,131.558495828173)) ;
#114923 = CARTESIAN_POINT('Ctrl Pts',(-16.9152315370478,12.5164543914562,
131.761543944961)) ;
#114924 = CARTESIAN_POINT('Ctrl Pts',(-17.0104958015721,12.3891143889345,
132.006622580848)) ;
#114925 = CARTESIAN_POINT('Ctrl Pts',(-17.1132917121907,12.3364756158918,
132.273826383176)) ;
#114926 = CARTESIAN_POINT('Ctrl Pts',(-17.2173332534644,12.3612642231578,
132.54465957405)) ;
#114927 = CARTESIAN_POINT('Ctrl Pts',(-17.3163641429157,12.4629838840005,
132.800676032605)) ;
#114928 = CARTESIAN_POINT('Ctrl Pts',(-17.4026407183266,12.6321971699934,
133.01975282772)) ;
#114929 = CARTESIAN_POINT('Ctrl Pts',(-17.472100457449,12.8584558798932,133.189548524182)) ;
#114930 = CARTESIAN_POINT('Ctrl Pts',(-17.5200564206003,13.1261648647243,
133.296424663186)) ;
#114931 = CARTESIAN_POINT('Ctrl Pts',(-17.5435329958318,13.4141234552309,
133.331916813786)) ;
#114932 = CARTESIAN_POINT('Ctrl Pts',(-17.5418705107985,13.7023852342343,
133.294006470842)) ;
#114933 = CARTESIAN_POINT('Ctrl Pts',(-17.515866367185,13.9714212012371,133.184910655295)) ;
#114934 = CARTESIAN_POINT('Ctrl Pts',(-17.4677121548387,14.202020081249,133.01095053406)) ;
#114935 = CARTESIAN_POINT('Ctrl Pts',(-17.4023716167183,14.3750071736422,
132.787065724901)) ;
#114936 = CARTESIAN_POINT('Ctrl Pts',(-17.3247668097447,14.4806351346196,
132.527282453733)) ;
#114937 = CARTESIAN_POINT('Ctrl Pts',(-17.2410054869792,14.5105855297535,
132.24943004058)) ;
#114938 = CARTESIAN_POINT('Ctrl Pts',(-17.1581501091636,14.4625550657111,
131.974268906069)) ;
#114939 = CARTESIAN_POINT('Ctrl Pts',(-17.0827332780509,14.3400369417443,
131.720826863696)) ;
#114940 = CARTESIAN_POINT('Ctrl Pts',(-17.0209888868574,14.1521957535254,
131.507380128005)) ;
#114941 = CARTESIAN_POINT('Ctrl Pts',(-16.9778207788142,13.9116489154345,
131.348115653949)) ;
#114942 = CARTESIAN_POINT('Ctrl Pts',(-16.9572990580186,13.6358544266559,
131.25499330384)) ;
#114943 = CARTESIAN_POINT('Ctrl Pts',(-16.9615071381463,13.3459427675745,
131.23424300822)) ;
#114944 = CARTESIAN_POINT('Ctrl Pts',(-16.9909211180614,13.0604649745041,
131.286996740778)) ;
#114945 = CARTESIAN_POINT('Ctrl Pts',(-17.0441007990242,12.8015143832803,
131.409241549806)) ;
#114946 = CARTESIAN_POINT('Ctrl Pts',(-17.1180304186239,12.586871423154,131.592073079015)) ;
#114947 = CARTESIAN_POINT('Ctrl Pts',(-17.2080500636742,12.4323032180318,
131.821934768459)) ;
#114948 = CARTESIAN_POINT('Ctrl Pts',(-17.3084611337155,12.348604012381,132.082157360211)) ;
#114949 = CARTESIAN_POINT('Ctrl Pts',(-17.4130111461555,12.3418345254331,
132.3544143668)) ;
#114950 = CARTESIAN_POINT('Ctrl Pts',(-17.5146765749007,12.4127257697425,
132.618266949295)) ;
#114951 = CARTESIAN_POINT('Ctrl Pts',(-17.606721170884,12.5554430365515,132.854114383774)) ;
#114952 = CARTESIAN_POINT('Ctrl Pts',(-17.6839111619126,12.7608029240068,
133.046442139626)) ;
#114953 = CARTESIAN_POINT('Ctrl Pts',(-17.7410331806284,13.0143079229722,
133.180091411217)) ;
#114954 = CARTESIAN_POINT('Ctrl Pts',(-17.7745360164768,13.2953661026702,
133.244952941826)) ;
#114955 = CARTESIAN_POINT('Ctrl Pts',(-17.7831520054483,13.587499191953,133.236886150184)) ;
#114956 = CARTESIAN_POINT('Ctrl Pts',(-17.7666348632763,13.8669338626205,
133.155497022517)) ;
#114957 = CARTESIAN_POINT('Ctrl Pts',(-17.7273863718362,14.1134263503453,
133.007875421063)) ;
#114958 = CARTESIAN_POINT('Ctrl Pts',(-17.6683893078491,14.3121780897716,
132.802342611055)) ;
#114959 = CARTESIAN_POINT('Ctrl Pts',(-17.5946147982464,14.4470050265316,
132.553591742459)) ;
#114960 = CARTESIAN_POINT('Ctrl Pts',(-17.5125911040324,14.5078086325279,
132.280874384855)) ;
#114961 = CARTESIAN_POINT('Ctrl Pts',(-17.4289255794743,14.4913412737729,
132.003473976216)) ;
#114962 = CARTESIAN_POINT('Ctrl Pts',(-17.3497030184291,14.3985299043882,
131.738923406222)) ;
#114963 = CARTESIAN_POINT('Ctrl Pts',(-17.2814947859058,14.2353764928408,
131.506472748856)) ;
#114964 = CARTESIAN_POINT('Ctrl Pts',(-17.2301833982271,14.0132824388172,
131.32333677435)) ;
#114965 = CARTESIAN_POINT('Ctrl Pts',(-17.2003726149901,13.751770584179,131.203370984278)) ;
#114966 = CARTESIAN_POINT('Ctrl Pts',(-17.1942692410409,13.4639004603942,
131.15229798358)) ;
#114967 = CARTESIAN_POINT('Ctrl Pts',(-17.2136563233809,13.1736259559936,
131.175755585428)) ;
#114968 = CARTESIAN_POINT('Ctrl Pts',(-17.2572199771084,12.9029494351804,
131.270058586451)) ;
#114969 = CARTESIAN_POINT('Ctrl Pts',(-17.3234518657098,12.6670694829694,
131.430263375814)) ;
#114970 = CARTESIAN_POINT('Ctrl Pts',(-17.4076950363158,12.4867414535482,
131.643224441991)) ;
#114971 = CARTESIAN_POINT('Ctrl Pts',(-17.5042594533731,12.3736046950475,
131.892333562312)) ;
#114972 = CARTESIAN_POINT('Ctrl Pts',(-17.6083225797878,12.3351061359291,
132.163067552705)) ;
#114973 = CARTESIAN_POINT('Ctrl Pts',(-17.7115102747659,12.3747297412366,
132.431506046747)) ;
#114974 = CARTESIAN_POINT('Ctrl Pts',(-17.80835655534,12.4890530273647,132.681306942846)) ;
#114975 = CARTESIAN_POINT('Ctrl Pts',(-17.8927139370083,12.6718473822343,
132.894413198474)) ;
#114976 = CARTESIAN_POINT('Ctrl Pts',(-17.9581348743092,12.9071471042355,
133.05245843071)) ;
#114977 = CARTESIAN_POINT('Ctrl Pts',(-18.0014489044881,13.1791583633753,
133.145922177929)) ;
#114978 = CARTESIAN_POINT('Ctrl Pts',(-18.020261151911,13.4685703303894,133.16781609884)) ;
#114979 = CARTESIAN_POINT('Ctrl Pts',(-18.0138792132709,13.7556865610863,
133.115998787948)) ;
#114980 = CARTESIAN_POINT('Ctrl Pts',(-17.9834392562243,14.0184520779736,
132.993960277943)) ;
#114981 = CARTESIAN_POINT('Ctrl Pts',(-17.9319093006337,14.2386835545227,
132.810307624848)) ;
#114982 = CARTESIAN_POINT('Ctrl Pts',(-17.8634196060343,14.4009245247973,
132.577005577925)) ;
#114983 = CARTESIAN_POINT('Ctrl Pts',(-17.7839956342627,14.4923209079493,
132.311848278652)) ;
#114984 = CARTESIAN_POINT('Ctrl Pts',(-17.7003715420016,14.5074993821674,
132.034597515729)) ;
#114985 = CARTESIAN_POINT('Ctrl Pts',(-17.6179715693461,14.4446391320812,
131.760580504429)) ;
#114986 = CARTESIAN_POINT('Ctrl Pts',(-17.5449472629492,14.309013886893,131.514230915999)) ;
#114987 = CARTESIAN_POINT('Ctrl Pts',(-17.4863929079662,14.1104149351794,
131.310125649846)) ;
#114988 = CARTESIAN_POINT('Ctrl Pts',(-17.4472233098488,13.8614588559076,
131.162498832848)) ;
#114989 = CARTESIAN_POINT('Ctrl Pts',(-17.4312869960412,13.5819687002437,
131.082859767227)) ;
#114990 = CARTESIAN_POINT('Ctrl Pts',(-17.4402797073093,13.2906279013141,
131.075985151787)) ;
#114991 = CARTESIAN_POINT('Ctrl Pts',(-17.4743143198391,13.009243305788,131.142317233284)) ;
#114992 = CARTESIAN_POINT('Ctrl Pts',(-17.5315517099284,12.7575168112921,
131.276452625469)) ;
#114993 = CARTESIAN_POINT('Ctrl Pts',(-17.6091410096472,12.5525240138587,
131.469879021206)) ;
#114994 = CARTESIAN_POINT('Ctrl Pts',(-17.7014737885802,12.4108770336832,
131.706544893167)) ;
#114995 = CARTESIAN_POINT('Ctrl Pts',(-17.8032831969416,12.3412909140522,
131.97080490142)) ;
#114996 = CARTESIAN_POINT('Ctrl Pts',(-17.9077079735701,12.3493861735078,
132.242732393973)) ;
#114997 = CARTESIAN_POINT('Ctrl Pts',(-18.0080021312736,12.4342727909203,
132.502613425746)) ;
#114998 = CARTESIAN_POINT('Ctrl Pts',(-18.097851259794,12.5900489009072,132.731956223757)) ;
#114999 = CARTESIAN_POINT('Ctrl Pts',(-18.1714811565311,12.8056265995217,
132.913906681068)) ;
#115000 = CARTESIAN_POINT('Ctrl Pts',(-18.2242791522083,13.0653848746049,
133.035014327401)) ;
#115001 = CARTESIAN_POINT('Ctrl Pts',(-18.2532373491338,13.3504851063388,
133.086511791274)) ;
#115002 = CARTESIAN_POINT('Ctrl Pts',(-18.2570176970517,13.6412798147236,
133.064399324168)) ;
#115003 = CARTESIAN_POINT('Ctrl Pts',(-18.2361288879767,13.915548156852,132.970331104728)) ;
#115004 = CARTESIAN_POINT('Ctrl Pts',(-18.1927521468012,14.1552942040558,
132.810491998612)) ;
#115005 = CARTESIAN_POINT('Ctrl Pts',(-18.1304889717146,14.3429101935435,
132.595396822877)) ;
#115006 = CARTESIAN_POINT('Ctrl Pts',(-18.0549535994053,14.4639893047867,
132.341644352442)) ;
#115007 = CARTESIAN_POINT('Ctrl Pts',(-17.9720169774795,14.5107279953385,
132.066239556179)) ;
#115008 = CARTESIAN_POINT('Ctrl Pts',(-17.88839874123,14.4794893752074,131.788842595817)) ;
#115009 = CARTESIAN_POINT('Ctrl Pts',(-17.8108656194136,14.3727211578977,
131.529246532274)) ;
#115010 = CARTESIAN_POINT('Ctrl Pts',(-17.7456151211965,14.1977799584113,
131.305501822006)) ;
#115011 = CARTESIAN_POINT('Ctrl Pts',(-17.6981151394564,13.9680803032242,
131.13369579038)) ;
#115012 = CARTESIAN_POINT('Ctrl Pts',(-17.6723054333923,13.6967826933105,
131.024941140418)) ;
#115013 = CARTESIAN_POINT('Ctrl Pts',(-17.6711447708163,13.4094043760888,
130.98862536116)) ;
#115014 = CARTESIAN_POINT('Ctrl Pts',(-17.6950445630246,13.1212039321583,
131.025303143358)) ;
#115015 = CARTESIAN_POINT('Ctrl Pts',(-17.74333311896,12.8546896237207,131.133221894845)) ;
#115016 = CARTESIAN_POINT('Ctrl Pts',(-17.81282756458,12.6293810356165,131.303196900116)) ;
#115017 = CARTESIAN_POINT('Ctrl Pts',(-17.9005194706817,12.4594635396626,
131.525988684649)) ;
#115018 = CARTESIAN_POINT('Ctrl Pts',(-17.9986989569018,12.3604529302704,
131.779876218196)) ;
#115019 = CARTESIAN_POINT('Ctrl Pts',(-18.1032340963646,12.3366695079855,
132.05199660503)) ;
#115020 = CARTESIAN_POINT('Ctrl Pts',(-18.2056125319901,12.3907630606801,
132.318086056791)) ;
#115021 = CARTESIAN_POINT('Ctrl Pts',(-18.300613364825,12.5187717527639,132.562441868016)) ;
#115022 = CARTESIAN_POINT('Ctrl Pts',(-18.3816465085652,12.7125553045139,
132.765918032423)) ;
#115023 = CARTESIAN_POINT('Ctrl Pts',(-18.4429853099616,12.9551208485313,
132.912159665352)) ;
#115024 = CARTESIAN_POINT('Ctrl Pts',(-18.4820336765163,13.2325620060974,
132.993078593711)) ;
#115025 = CARTESIAN_POINT('Ctrl Pts',(-18.496084383933,13.5243419796884,133.00090515124)) ;
#115026 = CARTESIAN_POINT('Ctrl Pts',(-18.4850639350324,13.8069926528057,
132.935714610325)) ;
#115027 = CARTESIAN_POINT('Ctrl Pts',(-18.4503367662865,14.0639000199269,
132.801056058483)) ;
#115028 = CARTESIAN_POINT('Ctrl Pts',(-18.3952268191814,14.2741558930926,
132.606941700926)) ;
#115029 = CARTESIAN_POINT('Ctrl Pts',(-18.3243680288223,14.4234615625839,
132.366801537788)) ;
#115030 = CARTESIAN_POINT('Ctrl Pts',(-18.2437816042926,14.5011170686614,
132.098327447916)) ;
#115031 = CARTESIAN_POINT('Ctrl Pts',(-18.1592384984199,14.5013614779113,
131.81807310291)) ;
#115032 = CARTESIAN_POINT('Ctrl Pts',(-18.0789307375107,14.4249956630962,
131.550560960519)) ;
#115033 = CARTESIAN_POINT('Ctrl Pts',(-18.0076541118125,14.2760171565871,
131.309082565097)) ;
#115034 = CARTESIAN_POINT('Ctrl Pts',(-17.9524899575172,14.0665442400002,
131.114862544505)) ;
#115035 = CARTESIAN_POINT('Ctrl Pts',(-17.9175014310239,13.8110528410318,
130.979547647309)) ;
#115036 = CARTESIAN_POINT('Ctrl Pts',(-17.9061688391216,13.5262786463887,
130.913174372637)) ;
#115037 = CARTESIAN_POINT('Ctrl Pts',(-17.919877948496,13.2368369901033,130.920277108179)) ;
#115038 = CARTESIAN_POINT('Ctrl Pts',(-17.9586197277239,12.9583255903659,
131.000212959745)) ;
#115039 = CARTESIAN_POINT('Ctrl Pts',(-18.0199083066583,12.7145800096232,
131.146219952724)) ;
#115040 = CARTESIAN_POINT('Ctrl Pts',(-18.1009974511921,12.5201730384604,
131.349794172582)) ;
#115041 = CARTESIAN_POINT('Ctrl Pts',(-18.1949562384929,12.392297716127,131.59141902566)) ;
#115042 = CARTESIAN_POINT('Ctrl Pts',(-18.2981754606917,12.3368042043637,
131.859663996403)) ;
#115043 = CARTESIAN_POINT('Ctrl Pts',(-18.4019398290045,12.3594079574846,
132.129799825424)) ;
#115044 = CARTESIAN_POINT('Ctrl Pts',(-18.5013383418749,12.4588426243277,
132.386856715267)) ;
#115045 = CARTESIAN_POINT('Ctrl Pts',(-18.5881323912535,12.6263832935465,
132.607414342136)) ;
#115046 = CARTESIAN_POINT('Ctrl Pts',(-18.6581587702516,12.8513078071139,
132.778854814353)) ;
#115047 = CARTESIAN_POINT('Ctrl Pts',(-18.7067345904951,13.1175341941134,
132.887608467018)) ;
#115048 = CARTESIAN_POINT('Ctrl Pts',(-18.731003412201,13.4059954970849,132.925314381533)) ;
#115049 = CARTESIAN_POINT('Ctrl Pts',(-18.7300968071152,13.6942419645787,
132.889656262388)) ;
#115050 = CARTESIAN_POINT('Ctrl Pts',(-18.7044541735128,13.9656571359195,
132.781395875164)) ;
#115051 = CARTESIAN_POINT('Ctrl Pts',(-18.6575265026644,14.1945698215837,
132.611470543872)) ;
#115052 = CARTESIAN_POINT('Ctrl Pts',(-18.5922406519204,14.3711224528334,
132.387486886082)) ;
#115053 = CARTESIAN_POINT('Ctrl Pts',(-18.5149037393986,14.4785950091488,
132.128508392993)) ;
#115054 = CARTESIAN_POINT('Ctrl Pts',(-18.4311371510558,14.5108133112394,
131.850601957705)) ;
#115055 = CARTESIAN_POINT('Ctrl Pts',(-18.3483146549276,14.4650394200622,
131.575598992863)) ;
#115056 = CARTESIAN_POINT('Ctrl Pts',(-18.2726066198908,14.3446919400874,
131.321313280288)) ;
#115057 = CARTESIAN_POINT('Ctrl Pts',(-18.2103307361537,14.1586507898245,
131.106307024848)) ;
#115058 = CARTESIAN_POINT('Ctrl Pts',(-18.1664432390162,13.9182142591253,
130.944795156692)) ;
#115059 = CARTESIAN_POINT('Ctrl Pts',(-18.1453636366719,13.6446894301756,
130.850233747273)) ;
#115060 = CARTESIAN_POINT('Ctrl Pts',(-18.1488348343508,13.3538163555555,
130.82719813754)) ;
#115061 = CARTESIAN_POINT('Ctrl Pts',(-18.1774811245967,13.0687529323482,
130.877811758373)) ;
#115062 = CARTESIAN_POINT('Ctrl Pts',(-18.2300437642224,12.8084025711039,
130.998208929724)) ;
#115063 = CARTESIAN_POINT('Ctrl Pts',(-18.3034001053734,12.5923662507696,
131.179384620874)) ;
#115064 = CARTESIAN_POINT('Ctrl Pts',(-18.3931634370597,12.4355966936421,
131.408445657945)) ;
#115065 = CARTESIAN_POINT('Ctrl Pts',(-18.4935575860177,12.3498834173245,
131.668562849344)) ;
#115066 = CARTESIAN_POINT('Ctrl Pts',(-18.5975530541275,12.3409542808635,
131.939369081028)) ;
#115067 = CARTESIAN_POINT('Ctrl Pts',(-18.6994673351223,12.4093757248112,
132.203931136602)) ;
#115068 = CARTESIAN_POINT('Ctrl Pts',(-18.7921201529756,12.5505196315372,
132.441467645947)) ;
#115069 = CARTESIAN_POINT('Ctrl Pts',(-18.8697017731338,12.7541803006072,
132.634971878383)) ;
#115070 = CARTESIAN_POINT('Ctrl Pts',(-18.9273307484839,13.0055267425044,
132.770220733639)) ;
#115071 = CARTESIAN_POINT('Ctrl Pts',(-18.9617100390982,13.2870724884799,
132.83751270461)) ;
#115072 = CARTESIAN_POINT('Ctrl Pts',(-18.9710255677151,13.5781354317469,
132.831615285865)) ;
#115073 = CARTESIAN_POINT('Ctrl Pts',(-18.9553578084607,13.8583662507443,
132.752702523973)) ;
#115074 = CARTESIAN_POINT('Ctrl Pts',(-18.9165383575917,14.1072755060793,
132.606171710367)) ;
#115075 = CARTESIAN_POINT('Ctrl Pts',(-18.8581587772242,14.3069765889331,
132.4025330216)) ;
#115076 = CARTESIAN_POINT('Ctrl Pts',(-18.7850681968336,14.443614067786,132.155907192059)) ;
#115077 = CARTESIAN_POINT('Ctrl Pts',(-18.702941141321,14.5071928082345,131.882773592227)) ;
#115078 = CARTESIAN_POINT('Ctrl Pts',(-18.6190408117616,14.4928945220509,
131.604612881179)) ;
#115079 = CARTESIAN_POINT('Ctrl Pts',(-18.5396187459799,14.4021254936154,
131.339485656911)) ;
#115080 = CARTESIAN_POINT('Ctrl Pts',(-18.4711933901986,14.2413770477371,
131.106496569037)) ;
#115081 = CARTESIAN_POINT('Ctrl Pts',(-18.4192605637911,14.0210258594474,
130.921552581758)) ;
#115082 = CARTESIAN_POINT('Ctrl Pts',(-18.3886405960536,13.7594508415378,
130.799092122936)) ;
#115083 = CARTESIAN_POINT('Ctrl Pts',(-18.381928462571,13.4716753030503,130.746210031867)) ;
#115084 = CARTESIAN_POINT('Ctrl Pts',(-18.4004216312574,13.18278007244,130.767242888151)) ;
#115085 = CARTESIAN_POINT('Ctrl Pts',(-18.4435339670258,12.9097866347109,
130.860039653288)) ;
#115086 = CARTESIAN_POINT('Ctrl Pts',(-18.5088204983959,12.6739761120234,
131.017674750893)) ;
#115087 = CARTESIAN_POINT('Ctrl Pts',(-18.5926770612546,12.4911376353209,
131.229439455072)) ;
#115088 = CARTESIAN_POINT('Ctrl Pts',(-18.6895108158381,12.3755758788311,
131.479159592622)) ;
#115089 = CARTESIAN_POINT('Ctrl Pts',(-18.7928542788589,12.3352662329562,
131.747989657394)) ;
#115090 = CARTESIAN_POINT('Ctrl Pts',(-18.8962659376777,12.3722006143293,
132.017051741353)) ;
#115091 = CARTESIAN_POINT('Ctrl Pts',(-18.9940984306609,12.4858118722087,
132.26946955847)) ;
#115092 = CARTESIAN_POINT('Ctrl Pts',(-19.0779483654093,12.6649628027199,
132.481462828409)) ;
#115093 = CARTESIAN_POINT('Ctrl Pts',(-19.144324386781,12.8995424291904,132.64216747859)) ;
#115094 = CARTESIAN_POINT('Ctrl Pts',(-19.1882893988472,13.1707489990253,
132.73754255469)) ;
#115095 = CARTESIAN_POINT('Ctrl Pts',(-19.2078747746244,13.4602465419289,
132.76165779285)) ;
#115096 = CARTESIAN_POINT('Ctrl Pts',(-19.2021695943243,13.7479094104328,
132.711797460233)) ;
#115097 = CARTESIAN_POINT('Ctrl Pts',(-19.1724541288044,14.0110933638022,
132.591943088721)) ;
#115098 = CARTESIAN_POINT('Ctrl Pts',(-19.1214789970609,14.2330195298938,
132.409891780119)) ;
#115099 = CARTESIAN_POINT('Ctrl Pts',(-19.0533824116154,14.397056415232,132.177734508543)) ;
#115100 = CARTESIAN_POINT('Ctrl Pts',(-18.9744610193818,14.4906410938832,
131.914150162339)) ;
#115101 = CARTESIAN_POINT('Ctrl Pts',(-18.890345578861,14.5080280130628,131.635247249356)) ;
#115102 = CARTESIAN_POINT('Ctrl Pts',(-18.8085392860132,14.4480725424633,
131.363277720596)) ;
#115103 = CARTESIAN_POINT('Ctrl Pts',(-18.7346273925197,14.3139470607326,
131.114108989611)) ;
#115104 = CARTESIAN_POINT('Ctrl Pts',(-18.6756142626322,14.1169437524237,
130.908679443903)) ;
#115105 = CARTESIAN_POINT('Ctrl Pts',(-18.6357563526766,13.8684682048696,
130.758950982595)) ;
#115106 = CARTESIAN_POINT('Ctrl Pts',(-18.6192189361488,13.5907243651,130.677694418299)) ;
#115107 = CARTESIAN_POINT('Ctrl Pts',(-18.6274186795787,13.2994062522709,
130.668497076563)) ;
#115108 = CARTESIAN_POINT('Ctrl Pts',(-18.6607053713449,13.0173302811176,
130.732637587237)) ;
#115109 = CARTESIAN_POINT('Ctrl Pts',(-18.7175745221499,12.7634586998748,
130.865557336184)) ;
#115110 = CARTESIAN_POINT('Ctrl Pts',(-18.7946062779487,12.5574053612187,
131.057405473283)) ;
#115111 = CARTESIAN_POINT('Ctrl Pts',(-18.8863176363417,12.4141338116398,
131.292346024062)) ;
#115112 = CARTESIAN_POINT('Ctrl Pts',(-18.9880396659882,12.342233208706,131.556318246303)) ;
#115113 = CARTESIAN_POINT('Ctrl Pts',(-19.092367557879,12.3479816385131,131.828001920729)) ;
#115114 = CARTESIAN_POINT('Ctrl Pts',(-19.1930265312653,12.4308508598937,
132.088893600864)) ;
#115115 = CARTESIAN_POINT('Ctrl Pts',(-19.2830355733598,12.5841342714032,
132.318802233278)) ;
#115116 = CARTESIAN_POINT('Ctrl Pts',(-19.3575448753726,12.7991564308112,
132.503166321675)) ;
#115117 = CARTESIAN_POINT('Ctrl Pts',(-19.410786935153,13.0569999610756,132.625693509338)) ;
#115118 = CARTESIAN_POINT('Ctrl Pts',(-19.4405356262244,13.3421921034464,
132.679428679679)) ;
#115119 = CARTESIAN_POINT('Ctrl Pts',(-19.4450790880921,13.6321454574867,
132.659662972591)) ;
#115120 = CARTESIAN_POINT('Ctrl Pts',(-19.4247875387373,13.9089725412032,
132.567125349093)) ;
#115121 = CARTESIAN_POINT('Ctrl Pts',(-19.381825668748,14.1498188340954,132.408476398238)) ;
#115122 = CARTESIAN_POINT('Ctrl Pts',(-19.3204518279194,14.3379335225619,
132.196198119276)) ;
#115123 = CARTESIAN_POINT('Ctrl Pts',(-19.2450347897687,14.4615825769609,
131.942693860373)) ;
#115124 = CARTESIAN_POINT('Ctrl Pts',(-19.162267963524,14.5104718339952,131.667809535155)) ;
#115125 = CARTESIAN_POINT('Ctrl Pts',(-19.0783524563333,14.4813917081873,
131.389457000585)) ;
#115126 = CARTESIAN_POINT('Ctrl Pts',(-19.0006162859046,14.3764101476522,
131.129272642533)) ;
#115127 = CARTESIAN_POINT('Ctrl Pts',(-18.9351626104612,14.2041613001764,
130.905077291113)) ;
#115128 = CARTESIAN_POINT('Ctrl Pts',(-18.8868641696125,13.9743839791119,
130.730738018104)) ;
#115129 = CARTESIAN_POINT('Ctrl Pts',(-18.8605695212481,13.7063210401926,
130.620861352139)) ;
#115130 = CARTESIAN_POINT('Ctrl Pts',(-18.8586114405782,13.416701167449,130.581917827711)) ;
#115131 = CARTESIAN_POINT('Ctrl Pts',(-18.8818454285258,13.1291677758352,
130.616763647551)) ;
#115132 = CARTESIAN_POINT('Ctrl Pts',(-18.9294289009308,12.86171027905,130.722620411742)) ;
#115133 = CARTESIAN_POINT('Ctrl Pts',(-18.9984336324713,12.6350478480017,
130.891152728659)) ;
#115134 = CARTESIAN_POINT('Ctrl Pts',(-19.0852684560724,12.4638699665219,
131.111590594525)) ;
#115135 = CARTESIAN_POINT('Ctrl Pts',(-19.1836902605787,12.3621126869917,
131.366013493841)) ;
#115136 = CARTESIAN_POINT('Ctrl Pts',(-19.2880034593845,12.336288293437,131.637540200635)) ;
#115137 = CARTESIAN_POINT('Ctrl Pts',(-19.3907293591919,12.3882079133966,
131.9045787098)) ;
#115138 = CARTESIAN_POINT('Ctrl Pts',(-19.4861202999562,12.5148240028862,
132.150020522081)) ;
#115139 = CARTESIAN_POINT('Ctrl Pts',(-19.566984502277,12.7050812653244,132.353293437429)) ;
#115140 = CARTESIAN_POINT('Ctrl Pts',(-19.6294717703468,12.9482677220772,
132.502618790391)) ;
#115141 = CARTESIAN_POINT('Ctrl Pts',(-19.6689768655333,13.2238578222556,
132.585025535771)) ;
#115142 = CARTESIAN_POINT('Ctrl Pts',(-19.6838357324499,13.5162932448957,
132.595118812429)) ;
#115143 = CARTESIAN_POINT('Ctrl Pts',(-19.6735197937544,13.799165239793,132.532024333921)) ;
#115144 = CARTESIAN_POINT('Ctrl Pts',(-19.6392454600331,14.0580267764743,
132.398557205212)) ;
#115145 = CARTESIAN_POINT('Ctrl Pts',(-19.5848869196862,14.2686028129511,
132.206807442572)) ;
#115146 = CARTESIAN_POINT('Ctrl Pts',(-19.5145008411043,14.4199618502008,
131.968069495771)) ;
#115147 = CARTESIAN_POINT('Ctrl Pts',(-19.4340220268986,14.4998958219189,
131.699871465245)) ;
#115148 = CARTESIAN_POINT('Ctrl Pts',(-19.3495759662661,14.5025664794371,
131.419941342377)) ;
#115149 = CARTESIAN_POINT('Ctrl Pts',(-19.2688627445457,14.4280652825415,
131.151146889785)) ;
#115150 = CARTESIAN_POINT('Ctrl Pts',(-19.197514432747,14.2819177513075,130.909621465088)) ;
#115151 = CARTESIAN_POINT('Ctrl Pts',(-19.1413921728409,14.0723877227319,
130.712339919469)) ;
#115152 = CARTESIAN_POINT('Ctrl Pts',(-19.1060584048045,13.8191595273478,
130.576195818314)) ;
#115153 = CARTESIAN_POINT('Ctrl Pts',(-19.0939136018658,13.5356702848312,
130.507524027747)) ;
#115154 = CARTESIAN_POINT('Ctrl Pts',(-19.1068958007053,13.2451626614465,
130.512392184105)) ;
#115155 = CARTESIAN_POINT('Ctrl Pts',(-19.1449564065195,12.9658959397094,
130.5903314269)) ;
#115156 = CARTESIAN_POINT('Ctrl Pts',(-19.2057189790489,12.720867949973,130.73477557543)) ;
#115157 = CARTESIAN_POINT('Ctrl Pts',(-19.2858400354675,12.5256178596935,
130.935699785553)) ;
#115158 = CARTESIAN_POINT('Ctrl Pts',(-19.3800402811628,12.3947249390078,
131.177818876414)) ;
#115159 = CARTESIAN_POINT('Ctrl Pts',(-19.4831200353959,12.3373274128747,
131.445666380565)) ;
#115160 = CARTESIAN_POINT('Ctrl Pts',(-19.5867485454506,12.3577351376061,
131.715460652154)) ;
#115161 = CARTESIAN_POINT('Ctrl Pts',(-19.6862131801358,12.4546492514378,
131.972779675498)) ;
#115162 = CARTESIAN_POINT('Ctrl Pts',(-19.7738286134021,12.6210676591383,
132.195587853881)) ;
#115163 = CARTESIAN_POINT('Ctrl Pts',(-19.8442902702029,12.8446766854148,
132.368316433847)) ;
#115164 = CARTESIAN_POINT('Ctrl Pts',(-19.8933608798738,13.108808163257,132.478653710118)) ;
#115165 = CARTESIAN_POINT('Ctrl Pts',(-19.9184859283659,13.3979062620311,
132.518747291947)) ;
#115166 = CARTESIAN_POINT('Ctrl Pts',(-19.9181983031023,13.6859097607706,
132.484944374893)) ;
#115167 = CARTESIAN_POINT('Ctrl Pts',(-19.8935840118438,13.9567565280856,
132.379898432991)) ;
#115168 = CARTESIAN_POINT('Ctrl Pts',(-19.8465997978561,14.1899349125241,
132.209373856163)) ;
#115169 = CARTESIAN_POINT('Ctrl Pts',(-19.7823820361551,14.3662692626876,
131.988864508273)) ;
#115170 = CARTESIAN_POINT('Ctrl Pts',(-19.7048377925854,14.4768289979695,
131.729048105592)) ;
#115171 = CARTESIAN_POINT('Ctrl Pts',(-19.621356858463,14.5109207090365,131.452070562692)) ;
#115172 = CARTESIAN_POINT('Ctrl Pts',(-19.5383256537918,14.4673589954117,
131.176412965102)) ;
#115173 = CARTESIAN_POINT('Ctrl Pts',(-19.462343360731,14.3490298117359,130.921339630599)) ;
#115174 = CARTESIAN_POINT('Ctrl Pts',(-19.399598094763,14.1643442573792,130.70492417211)) ;
#115175 = CARTESIAN_POINT('Ctrl Pts',(-19.3553585530389,13.9269540764464,
130.542614298548)) ;
#115176 = CARTESIAN_POINT('Ctrl Pts',(-19.3333939719036,13.6529087066834,
130.44529695513)) ;
#115177 = CARTESIAN_POINT('Ctrl Pts',(-19.3361541913265,13.3625040426011,
130.420224634067)) ;
#115178 = CARTESIAN_POINT('Ctrl Pts',(-19.3641172961552,13.0764917625792,
130.468781137817)) ;
#115179 = CARTESIAN_POINT('Ctrl Pts',(-19.4160399610195,12.8152457852602,
130.587319851219)) ;
#115180 = CARTESIAN_POINT('Ctrl Pts',(-19.4888652574942,12.5977360848388,
130.766942106929)) ;
#115181 = CARTESIAN_POINT('Ctrl Pts',(-19.5781388686584,12.4392301767845,
130.994608862376)) ;
#115182 = CARTESIAN_POINT('Ctrl Pts',(-19.6782931891438,12.3513755992719,
131.254028736787)) ;
#115183 = CARTESIAN_POINT('Ctrl Pts',(-19.7822229405507,12.3399316332142,
131.524661009902)) ;
#115184 = CARTESIAN_POINT('Ctrl Pts',(-19.88504344773,12.4070554351268,131.791616350641)) ;
#115185 = CARTESIAN_POINT('Ctrl Pts',(-19.9771610745846,12.5451369869361,
132.027897931008)) ;
#115186 = CARTESIAN_POINT('Ctrl Pts',(-20.0556173721215,12.7477726868892,
132.223821692675)) ;
#115187 = CARTESIAN_POINT('Ctrl Pts',(-20.1137903255926,12.9979367372735,
132.360683275234)) ;
#115188 = CARTESIAN_POINT('Ctrl Pts',(-20.1489013724765,13.2792370978739,
132.430071631305)) ;
#115189 = CARTESIAN_POINT('Ctrl Pts',(-20.1588787384282,13.5701580555343,
132.426125674529)) ;
#115190 = CARTESIAN_POINT('Ctrl Pts',(-20.143937682242,13.8505377724051,132.349389311992)) ;
#115191 = CARTESIAN_POINT('Ctrl Pts',(-20.1057318059421,14.1007512372239,
132.20463305785)) ;
#115192 = CARTESIAN_POINT('Ctrl Pts',(-20.0478354950526,14.3021715583994,
132.002395149785)) ;
#115193 = CARTESIAN_POINT('Ctrl Pts',(-19.9748500391882,14.4410638226486,
131.755979394128)) ;
#115194 = CARTESIAN_POINT('Ctrl Pts',(-19.892940104349,14.506420576945,131.483512074612)) ;
#115195 = CARTESIAN_POINT('Ctrl Pts',(-19.8092678890523,14.4944296739133,
131.206120710523)) ;
#115196 = CARTESIAN_POINT('Ctrl Pts',(-19.7294350859359,14.4055611915821,
130.939713797808)) ;
#115197 = CARTESIAN_POINT('Ctrl Pts',(-19.66081208133,14.2469875620131,130.706232624641)) ;
#115198 = CARTESIAN_POINT('Ctrl Pts',(-19.6083158027718,14.0284942715184,
130.519673218377)) ;
#115199 = CARTESIAN_POINT('Ctrl Pts',(-19.5769557514165,13.7670074742828,
130.394940588624)) ;
#115200 = CARTESIAN_POINT('Ctrl Pts',(-19.5695668686991,13.4805781215048,
130.340191561689)) ;
#115201 = CARTESIAN_POINT('Ctrl Pts',(-19.5872696261961,13.1913388058783,
130.358899107894)) ;
#115202 = CARTESIAN_POINT('Ctrl Pts',(-19.6297522740938,12.9172330933754,
130.449814911348)) ;
#115203 = CARTESIAN_POINT('Ctrl Pts',(-19.6944389773908,12.6799728703758,
130.60569175476)) ;
#115204 = CARTESIAN_POINT('Ctrl Pts',(-19.7782230780513,12.4949910418975,
130.817115688087)) ;
#115205 = CARTESIAN_POINT('Ctrl Pts',(-19.8739923402946,12.3781840447206,
131.063992159593)) ;
#115206 = CARTESIAN_POINT('Ctrl Pts',(-19.9780674608701,12.3352411023339,
131.33468497079)) ;
#115207 = CARTESIAN_POINT('Ctrl Pts',(-20.0810744379286,12.3701183957634,
131.602725123913)) ;
#115208 = CARTESIAN_POINT('Ctrl Pts',(-20.179252895713,12.4815908370187,131.85612905703)) ;
#115209 = CARTESIAN_POINT('Ctrl Pts',(-20.2634570739637,12.6586744463426,
132.069206441814)) ;
#115210 = CARTESIAN_POINT('Ctrl Pts',(-20.3305901520664,12.8927064505131,
132.232014267973)) ;
#115211 = CARTESIAN_POINT('Ctrl Pts',(-20.3750331233153,13.1615895986342,
132.328969789793)) ;
#115212 = CARTESIAN_POINT('Ctrl Pts',(-20.3954965997089,13.4527337961883,
132.355428882089)) ;
#115213 = CARTESIAN_POINT('Ctrl Pts',(-20.3904573045894,13.7397606263225,
132.307631593907)) ;
#115214 = CARTESIAN_POINT('Ctrl Pts',(-20.3613437715797,14.0044956878458,
132.189457679076)) ;
#115215 = CARTESIAN_POINT('Ctrl Pts',(-20.3110168045734,14.2270717047825,
132.009394785638)) ;
#115216 = CARTESIAN_POINT('Ctrl Pts',(-20.2436381751946,14.3928428531141,
131.779444891534)) ;
#115217 = CARTESIAN_POINT('Ctrl Pts',(-20.164336633125,14.4891679896536,131.51449038135)) ;
#115218 = CARTESIAN_POINT('Ctrl Pts',(-20.0809111882638,14.5086708936273,
131.237865647246)) ;
#115219 = CARTESIAN_POINT('Ctrl Pts',(-19.9983950566067,14.4507091204102,
130.963592375788)) ;
#115220 = CARTESIAN_POINT('Ctrl Pts',(-19.9244190141413,14.318823465338,130.714351089596)) ;
#115221 = CARTESIAN_POINT('Ctrl Pts',(-19.8648700988791,14.1234067424229,
130.507330724768)) ;
#115222 = CARTESIAN_POINT('Ctrl Pts',(-19.8245161746179,13.8772496577341,
130.356293737963)) ;
#115223 = CARTESIAN_POINT('Ctrl Pts',(-19.8070957881005,13.5994498547175,
130.272359938913)) ;
#115224 = CARTESIAN_POINT('Ctrl Pts',(-19.8146864693653,13.3067289539218,
130.261220009531)) ;
#115225 = CARTESIAN_POINT('Ctrl Pts',(-19.8471784531872,13.025513208076,130.323196727465)) ;
#115226 = CARTESIAN_POINT('Ctrl Pts',(-19.9032180692331,12.7708776887036,
130.453754380472)) ;
#115227 = CARTESIAN_POINT('Ctrl Pts',(-19.9797679754465,12.5628412979246,
130.644157296538)) ;
#115228 = CARTESIAN_POINT('Ctrl Pts',(-20.0712997390683,12.4171764122364,
130.878502714501)) ;
#115229 = CARTESIAN_POINT('Ctrl Pts',(-20.173220666744,12.3431378359771,131.142938313351)) ;
#115230 = CARTESIAN_POINT('Ctrl Pts',(-20.2769543623743,12.3467434972734,
131.413078047708)) ;
#115231 = CARTESIAN_POINT('Ctrl Pts',(-20.3779474556413,12.4272274658185,
131.674911921515)) ;
#115232 = CARTESIAN_POINT('Ctrl Pts',(-20.4684824931614,12.5790158149027,
131.906293765199)) ;
#115233 = CARTESIAN_POINT('Ctrl Pts',(-20.5433178346082,12.7916687829571,
132.091724629749)) ;
#115234 = CARTESIAN_POINT('Ctrl Pts',(-20.59747019779,13.0498138992039,132.216737279054)) ;
#115235 = CARTESIAN_POINT('Ctrl Pts',(-20.6277539698486,13.3331756720239,
132.272199599018)) ;
#115236 = CARTESIAN_POINT('Ctrl Pts',(-20.63310319697,13.6238935345468,132.254712776567)) ;
#115237 = CARTESIAN_POINT('Ctrl Pts',(-20.6135004102223,13.9010885274901,
132.164225860573)) ;
#115238 = CARTESIAN_POINT('Ctrl Pts',(-20.5712628793398,14.1432054793993,
132.007719764268)) ;
#115239 = CARTESIAN_POINT('Ctrl Pts',(-20.5099062183509,14.3341070280144,
131.795269476235)) ;
#115240 = CARTESIAN_POINT('Ctrl Pts',(-20.4352339689786,14.4587991787124,
131.544150012527)) ;
#115241 = CARTESIAN_POINT('Ctrl Pts',(-20.3525489079931,14.5101605081857,
131.269477291802)) ;
#115242 = CARTESIAN_POINT('Ctrl Pts',(-20.2687361872864,14.4834097576633,
130.991492371573)) ;
#115243 = CARTESIAN_POINT('Ctrl Pts',(-20.1906756501309,14.380986704451,130.730363509583)) ;
#115244 = CARTESIAN_POINT('Ctrl Pts',(-20.1243569260148,14.2089571607828,
130.503381990289)) ;
#115245 = CARTESIAN_POINT('Ctrl Pts',(-20.0759333865454,13.9828180453883,
130.329004955831)) ;
#115246 = CARTESIAN_POINT('Ctrl Pts',(-20.0486953445985,13.7132629209954,
130.216063933579)) ;
#115247 = CARTESIAN_POINT('Ctrl Pts',(-20.0461136758052,13.42583764063,130.175529664949)) ;
#115248 = CARTESIAN_POINT('Ctrl Pts',(-20.0685766436055,13.1374631065902,
130.208056459246)) ;
#115249 = CARTESIAN_POINT('Ctrl Pts',(-20.1154485813734,12.8691197006536,
130.31184888817)) ;
#115250 = CARTESIAN_POINT('Ctrl Pts',(-20.1842161886027,12.6403113443668,
130.479551228157)) ;
#115251 = CARTESIAN_POINT('Ctrl Pts',(-20.2699974667944,12.468420702256,130.697148821309)) ;
#115252 = CARTESIAN_POINT('Ctrl Pts',(-20.368777345651,12.3638000217504,130.952399609198)) ;
#115253 = CARTESIAN_POINT('Ctrl Pts',(-20.4724837589939,12.3359859144704,
131.22233281641)) ;
#115254 = CARTESIAN_POINT('Ctrl Pts',(-20.5755189014966,12.3855342690204,
131.490214378318)) ;
#115255 = CARTESIAN_POINT('Ctrl Pts',(-20.6710370148352,12.5097023136888,
131.736103980719)) ;
#115256 = CARTESIAN_POINT('Ctrl Pts',(-20.7526999022241,12.6987169895182,
131.941597617443)) ;
#115257 = CARTESIAN_POINT('Ctrl Pts',(-20.8159200282362,12.9413958856346,
132.092978431002)) ;
#115258 = CARTESIAN_POINT('Ctrl Pts',(-20.8560148207953,13.2164083911014,
132.177101494275)) ;
#115259 = CARTESIAN_POINT('Ctrl Pts',(-20.8715568106971,13.5077476116907,
132.18930496735)) ;
#115260 = CARTESIAN_POINT('Ctrl Pts',(-20.8618791478333,13.7917084995172,
132.127994218716)) ;
#115261 = CARTESIAN_POINT('Ctrl Pts',(-20.8285666993428,14.0497089633418,
131.997596945122)) ;
#115262 = CARTESIAN_POINT('Ctrl Pts',(-20.7745879228126,14.2632250030891,
131.806787903495)) ;
#115263 = CARTESIAN_POINT('Ctrl Pts',(-20.7043311974277,14.4168537708596,
131.568328459368)) ;
#115264 = CARTESIAN_POINT('Ctrl Pts',(-20.6239603167272,14.4987598986465,
131.300415425815)) ;
#115265 = CARTESIAN_POINT('Ctrl Pts',(-20.539754785129,14.5035045718472,131.021276419093)) ;
#115266 = CARTESIAN_POINT('Ctrl Pts',(-20.4588117616689,14.4313229997249,
130.751803459987)) ;
#115267 = CARTESIAN_POINT('Ctrl Pts',(-20.3868956375626,14.286096674379,130.508478859911)) ;
#115268 = CARTESIAN_POINT('Ctrl Pts',(-20.3308554449234,14.0806888556304,
130.311826279916)) ;
#115269 = CARTESIAN_POINT('Ctrl Pts',(-20.2944696102375,13.8265805447723,
130.172317712221)) ;
#115270 = CARTESIAN_POINT('Ctrl Pts',(-20.2817095072984,13.5441879409374,
130.101929815543)) ;
#115271 = CARTESIAN_POINT('Ctrl Pts',(-20.2939970046262,13.2530370689606,
130.104694604891)) ;
#115272 = CARTESIAN_POINT('Ctrl Pts',(-20.3312192505214,12.9741114175935,
130.18030810907)) ;
#115273 = CARTESIAN_POINT('Ctrl Pts',(-20.391477731723,12.7272119216586,130.323195480133)) ;
#115274 = CARTESIAN_POINT('Ctrl Pts',(-20.4710215017653,12.5305677659782,
130.522476172394)) ;
#115275 = CARTESIAN_POINT('Ctrl Pts',(-20.5648765077218,12.3976028767503,
130.763584707341)) ;
#115276 = CARTESIAN_POINT('Ctrl Pts',(-20.6677354645716,12.3378877564715,
131.030810858964)) ;
#115277 = CARTESIAN_POINT('Ctrl Pts',(-20.771610142133,12.3561146457162,131.301258410359)) ;
#115278 = CARTESIAN_POINT('Ctrl Pts',(-20.8710140356471,12.4504996091204,
131.558507272223)) ;
#115279 = CARTESIAN_POINT('Ctrl Pts',(-20.9591976245712,12.6151918179393,
131.782920165643)) ;
#115280 = CARTESIAN_POINT('Ctrl Pts',(-21.0301909969835,12.8367627956422,
131.957264907826)) ;
#115281 = CARTESIAN_POINT('Ctrl Pts',(-21.0802720431719,13.102471284239,132.070248175628)) ;
#115282 = CARTESIAN_POINT('Ctrl Pts',(-21.1058128562322,13.388098474674,132.11192368682)) ;
#115283 = CARTESIAN_POINT('Ctrl Pts',(-21.1063578527298,13.6786302634614,
132.08028850925)) ;
#115284 = CARTESIAN_POINT('Ctrl Pts',(-21.0823275663731,13.9495118019851,
131.977027551482)) ;
#115285 = CARTESIAN_POINT('Ctrl Pts',(-21.0362217842379,14.1831630717315,
131.809216673534)) ;
#115286 = CARTESIAN_POINT('Ctrl Pts',(-20.9721884045855,14.3622887251467,
131.589091305906)) ;
#115287 = CARTESIAN_POINT('Ctrl Pts',(-20.8947792880245,14.4748192529362,
131.32962547702)) ;
#115288 = CARTESIAN_POINT('Ctrl Pts',(-20.8116749026299,14.5109473630978,
131.053861074448)) ;
#115289 = CARTESIAN_POINT('Ctrl Pts',(-20.7286272549608,14.46989386631,130.778195045776)) ;
#115290 = CARTESIAN_POINT('Ctrl Pts',(-20.6522431108941,14.3536144736526,
130.521907930923)) ;
#115291 = CARTESIAN_POINT('Ctrl Pts',(-20.5889583813436,14.17062113719,130.303892930056)) ;
#115292 = CARTESIAN_POINT('Ctrl Pts',(-20.5440524129988,13.933736573907,130.13953810035)) ;
#115293 = CARTESIAN_POINT('Ctrl Pts',(-20.5214975045223,13.6617104442443,
130.040649083481)) ;
#115294 = CARTESIAN_POINT('Ctrl Pts',(-20.5235105668905,13.3701432171844,
130.013237741548)) ;
#115295 = CARTESIAN_POINT('Ctrl Pts',(-20.5508607538459,13.0839501475181,
130.0600249237)) ;
#115296 = CARTESIAN_POINT('Ctrl Pts',(-20.6019342296123,12.8226369063403,
130.176200002378)) ;
#115297 = CARTESIAN_POINT('Ctrl Pts',(-20.674162245095,12.6036153158418,130.354083975274)) ;
#115298 = CARTESIAN_POINT('Ctrl Pts',(-20.7628382753172,12.4432239429731,
130.580060592785)) ;
#115299 = CARTESIAN_POINT('Ctrl Pts',(-20.8633579914741,12.3525997513282,
130.840351394468)) ;
#115300 = CARTESIAN_POINT('Ctrl Pts',(-20.9671168641114,12.3393903655815,
131.110528978872)) ;
#115301 = CARTESIAN_POINT('Ctrl Pts',(-21.0694306011919,12.403468098602,131.376231401918)) ;
#115302 = CARTESIAN_POINT('Ctrl Pts',(-21.1627219404933,12.5405072085783,
131.615661785443)) ;
#115303 = CARTESIAN_POINT('Ctrl Pts',(-21.2416127937835,12.7420005519616,
131.812839172161)) ;
#115304 = CARTESIAN_POINT('Ctrl Pts',(-21.3001704333997,12.9900801149227,
131.950949061272)) ;
#115305 = CARTESIAN_POINT('Ctrl Pts',(-21.3360159038547,13.2708158721555,
132.022475029764)) ;
#115306 = CARTESIAN_POINT('Ctrl Pts',(-21.3467250085586,13.5613604134334,
132.020708203514)) ;
#115307 = CARTESIAN_POINT('Ctrl Pts',(-21.332530072888,13.8428560081929,131.946099675255)) ;
#115308 = CARTESIAN_POINT('Ctrl Pts',(-21.2946880005883,14.0951246502648,
131.802259522002)) ;
#115309 = CARTESIAN_POINT('Ctrl Pts',(-21.2376357521135,14.2968154125605,
131.602698948677)) ;
#115310 = CARTESIAN_POINT('Ctrl Pts',(-21.164806246768,14.4382062812648,131.356634806151)) ;
#115311 = CARTESIAN_POINT('Ctrl Pts',(-21.0832408338308,14.5055713938207,
131.085254319312)) ;
#115312 = CARTESIAN_POINT('Ctrl Pts',(-20.9994162423038,14.4957941932041,
130.807360837672)) ;
#115313 = CARTESIAN_POINT('Ctrl Pts',(-20.9195959138854,14.4095662340998,
130.541102349046)) ;
#115314 = CARTESIAN_POINT('Ctrl Pts',(-20.8500186277359,14.2515335127425,
130.304558118666)) ;
#115315 = CARTESIAN_POINT('Ctrl Pts',(-20.7972486154139,14.0347236874785,
130.11728882556)) ;
#115316 = CARTESIAN_POINT('Ctrl Pts',(-20.7653613268004,13.7751700114088,
129.991129528377)) ;
#115317 = CARTESIAN_POINT('Ctrl Pts',(-20.7571817990629,13.489555102194,129.934113768398)) ;
#115318 = CARTESIAN_POINT('Ctrl Pts',(-20.7742556911792,13.1989624545804,
129.950844344899)) ;
#115319 = CARTESIAN_POINT('Ctrl Pts',(-20.8159809707414,12.9245155762064,
130.03960916018)) ;
#115320 = CARTESIAN_POINT('Ctrl Pts',(-20.8805367450398,12.6850932088169,
130.194926855194)) ;
#115321 = CARTESIAN_POINT('Ctrl Pts',(-20.9626356003938,12.5007200500438,
130.401901459438)) ;
#115322 = CARTESIAN_POINT('Ctrl Pts',(-21.0591957946408,12.3802348015134,
130.650687618331)) ;
#115323 = CARTESIAN_POINT('Ctrl Pts',(-21.1622370545661,12.3354177830535,
130.918672003733)) ;
#115324 = CARTESIAN_POINT('Ctrl Pts',(-21.2662887681593,12.3682931650198,
131.189443526458)) ;
#115325 = CARTESIAN_POINT('Ctrl Pts',(-21.3637199956931,12.4764500222757,
131.44102792815)) ;
#115326 = CARTESIAN_POINT('Ctrl Pts',(-21.4490683123423,12.6527561756398,
131.657189302748)) ;
#115327 = CARTESIAN_POINT('Ctrl Pts',(-21.5164968590452,12.8841372675975,
131.821041651181)) ;
#115328 = CARTESIAN_POINT('Ctrl Pts',(-21.5620729321248,13.1550291136418,
131.920951331736)) ;
#115329 = CARTESIAN_POINT('Ctrl Pts',(-21.5829990360394,13.4437302360126,
131.949026741888)) ;
#115330 = CARTESIAN_POINT('Ctrl Pts',(-21.5787261653874,13.7319393007276,
131.903366364301)) ;
#115331 = CARTESIAN_POINT('Ctrl Pts',(-21.5503975227815,13.9965481623833,
131.787623344815)) ;
#115332 = CARTESIAN_POINT('Ctrl Pts',(-21.5005342471165,14.2215298170475,
131.608800269925)) ;
#115333 = CARTESIAN_POINT('Ctrl Pts',(-21.4333938850247,14.3891483272759,
131.379489123203)) ;
#115334 = CARTESIAN_POINT('Ctrl Pts',(-21.3548735774567,14.4871687024338,
131.117033634355)) ;
#115335 = CARTESIAN_POINT('Ctrl Pts',(-21.2709428978837,14.5093408079897,
130.838711318976)) ;
#115336 = CARTESIAN_POINT('Ctrl Pts',(-21.1882422406468,14.4530254583256,
130.563868416307)) ;
#115337 = CARTESIAN_POINT('Ctrl Pts',(-21.1143270880585,14.3240305585518,
130.31499305445)) ;
#115338 = CARTESIAN_POINT('Ctrl Pts',(-21.0539688868397,14.1290979717854,
130.105410602035)) ;
#115339 = CARTESIAN_POINT('Ctrl Pts',(-21.0132069302916,13.8855604155571,
129.953378103653)) ;
#115340 = CARTESIAN_POINT('Ctrl Pts',(-20.9950030451873,13.6058416707122,
129.866845755651)) ;
#115341 = CARTESIAN_POINT('Ctrl Pts',(-21.0018793397198,13.3160021377259,
129.853947611582)) ;
#115342 = CARTESIAN_POINT('Ctrl Pts',(-21.0337293398582,13.0326886676077,
129.913868033499)) ;
#115343 = CARTESIAN_POINT('Ctrl Pts',(-21.0893772116349,12.7766372190837,
130.043216529831)) ;
#115344 = CARTESIAN_POINT('Ctrl Pts',(-21.1653161877122,12.5676698161814,
130.231901557219)) ;
#115345 = CARTESIAN_POINT('Ctrl Pts',(-21.2561790285771,12.4206517790888,
130.464404545457)) ;
#115346 = CARTESIAN_POINT('Ctrl Pts',(-21.3575675366688,12.3443150505119,
130.727387699059)) ;
#115347 = CARTESIAN_POINT('Ctrl Pts',(-21.4618210845223,12.3454567433165,
130.998884337509)) ;
#115348 = CARTESIAN_POINT('Ctrl Pts',(-21.5631430702427,12.4241540146565,
131.261630006307)) ;
#115349 = CARTESIAN_POINT('Ctrl Pts',(-21.6537810155053,12.5736454649868,
131.493407152973)) ;
#115350 = CARTESIAN_POINT('Ctrl Pts',(-21.7290950924145,12.7844244258342,
131.680270904741)) ;
#115351 = CARTESIAN_POINT('Ctrl Pts',(-21.7839298109933,13.041264478038,131.807295952736)) ;
#115352 = CARTESIAN_POINT('Ctrl Pts',(-21.8150448539116,13.3250313838274,
131.865081031141)) ;
#115353 = CARTESIAN_POINT('Ctrl Pts',(-21.8210632536644,13.6156492492809,
131.849571033927)) ;
#115354 = CARTESIAN_POINT('Ctrl Pts',(-21.8022545212773,13.8929002803611,
131.761487721122)) ;
#115355 = CARTESIAN_POINT('Ctrl Pts',(-21.7605924585031,14.1366366428793,
131.606614879296)) ;
#115356 = CARTESIAN_POINT('Ctrl Pts',(-21.6999698317163,14.3287833833703,
131.396421302764)) ;
#115357 = CARTESIAN_POINT('Ctrl Pts',(-21.6253197774301,14.4563288342089,
131.145218098165)) ;
#115358 = CARTESIAN_POINT('Ctrl Pts',(-21.5425945750513,14.5097636463918,
130.870367772935)) ;
#115359 = CARTESIAN_POINT('Ctrl Pts',(-21.4589621479375,14.4852491819093,
130.593003563587)) ;
#115360 = CARTESIAN_POINT('Ctrl Pts',(-21.380714091029,14.385213180382,130.331360934625)) ;
#115361 = CARTESIAN_POINT('Ctrl Pts',(-21.3138290434139,14.2148994362801,
130.102677640231)) ;
#115362 = CARTESIAN_POINT('Ctrl Pts',(-21.264802027938,13.9895605141043,129.92646714371)) ;
#115363 = CARTESIAN_POINT('Ctrl Pts',(-21.2370048320792,13.7226496289756,
129.812102485109)) ;
#115364 = CARTESIAN_POINT('Ctrl Pts',(-21.2336042417307,13.4342098859693,
129.769013814372)) ;
#115365 = CARTESIAN_POINT('Ctrl Pts',(-21.2553236046358,13.1458182759752,
129.799407215841)) ;
#115366 = CARTESIAN_POINT('Ctrl Pts',(-21.3016988392798,12.8759127132536,
129.901648132077)) ;
#115367 = CARTESIAN_POINT('Ctrl Pts',(-21.3694669987003,12.6468868556867,
130.066623481143)) ;
#115368 = CARTESIAN_POINT('Ctrl Pts',(-21.4553373193102,12.4721832296684,
130.284273605613)) ;
#115369 = CARTESIAN_POINT('Ctrl Pts',(-21.5530256217249,12.3661739274481,
130.536616813639)) ;
#115370 = CARTESIAN_POINT('Ctrl Pts',(-21.6575177270796,12.3355863385396,
130.808562220896)) ;
#115371 = CARTESIAN_POINT('Ctrl Pts',(-21.7604456918656,12.3831198658751,
131.076206190241)) ;
#115372 = CARTESIAN_POINT('Ctrl Pts',(-21.8563696469902,12.5053833023315,
131.323242388746)) ;
#115373 = CARTESIAN_POINT('Ctrl Pts',(-21.9382966693068,12.6923270702948,
131.529584453516)) ;
#115374 = CARTESIAN_POINT('Ctrl Pts',(-22.0021645015312,12.9335865705139,
131.682862448256)) ;
#115375 = CARTESIAN_POINT('Ctrl Pts',(-22.0430213128192,13.2085814539572,
131.769129801508)) ;
#115376 = CARTESIAN_POINT('Ctrl Pts',(-22.0592352836556,13.4990557588074,
131.783380739882)) ;
#115377 = CARTESIAN_POINT('Ctrl Pts',(-22.0503004073671,13.7836907462661,
131.724216167399)) ;
#115378 = CARTESIAN_POINT('Ctrl Pts',(-22.0176371901026,14.0427281414566,
131.595717480909)) ;
#115379 = CARTESIAN_POINT('Ctrl Pts',(-21.9641995370827,14.2577309750281,
131.406490661624)) ;
#115380 = CARTESIAN_POINT('Ctrl Pts',(-21.8944782363852,14.4131664617501,
131.169654967239)) ;
#115381 = CARTESIAN_POINT('Ctrl Pts',(-21.8141620072022,14.4973755702956,
130.901832610092)) ;
#115382 = CARTESIAN_POINT('Ctrl Pts',(-21.7303937720881,14.5046724130054,
130.624142862364)) ;
#115383 = CARTESIAN_POINT('Ctrl Pts',(-21.6486693225774,14.4343111747756,
130.352140919931)) ;
#115384 = CARTESIAN_POINT('Ctrl Pts',(-21.5766530687314,14.2913904033354,
130.108640611113)) ;
#115385 = CARTESIAN_POINT('Ctrl Pts',(-21.5199914526865,14.0872940403586,
129.910112364196)) ;
#115386 = CARTESIAN_POINT('Ctrl Pts',(-21.4830382408884,13.8349907742835,
129.769035274606)) ;
#115387 = CARTESIAN_POINT('Ctrl Pts',(-21.4694985396213,13.5522018199285,
129.696252361388)) ;
#115388 = CARTESIAN_POINT('Ctrl Pts',(-21.4810885813508,13.2611771320633,
129.697002826515)) ;
#115389 = CARTESIAN_POINT('Ctrl Pts',(-21.5176805732444,12.9814107201437,
129.770743949859)) ;
#115390 = CARTESIAN_POINT('Ctrl Pts',(-21.5771191123903,12.7341369610279,
129.911345858839)) ;
#115391 = CARTESIAN_POINT('Ctrl Pts',(-21.6563209788842,12.535166216503,130.109544290444)) ;
#115392 = CARTESIAN_POINT('Ctrl Pts',(-21.7502713534583,12.4000170891871,
130.350799701057)) ;
#115393 = CARTESIAN_POINT('Ctrl Pts',(-21.8524815344102,12.3385941106561,
130.616296707476)) ;
#115394 = CARTESIAN_POINT('Ctrl Pts',(-21.9565712501459,12.3545286685026,
130.887315313701)) ;
#115395 = CARTESIAN_POINT('Ctrl Pts',(-22.0562577481496,12.4469846430608,
131.14537139149)) ;
#115396 = CARTESIAN_POINT('Ctrl Pts',(-22.1449360417052,12.6102579412087,
131.371180205731)) ;
#115397 = CARTESIAN_POINT('Ctrl Pts',(-22.2161370464207,12.8296977311719,
131.546256445573)) ;
#115398 = CARTESIAN_POINT('Ctrl Pts',(-22.2667592690025,13.0929763552362,
131.660982603106)) ;
#115399 = CARTESIAN_POINT('Ctrl Pts',(-22.2932535098378,13.3798715107165,
131.705248169509)) ;
#115400 = CARTESIAN_POINT('Ctrl Pts',(-22.2944576782056,13.6705227535771,
131.675549761758)) ;
#115401 = CARTESIAN_POINT('Ctrl Pts',(-22.2711545117995,13.9421700423004,
131.57442408932)) ;
#115402 = CARTESIAN_POINT('Ctrl Pts',(-22.2253820822901,14.1780191011813,
131.407446635602)) ;
#115403 = CARTESIAN_POINT('Ctrl Pts',(-22.1619741826909,14.3579768124892,
131.189272795754)) ;
#115404 = CARTESIAN_POINT('Ctrl Pts',(-22.0850483275451,14.4725057553617,
130.931291857228)) ;
#115405 = CARTESIAN_POINT('Ctrl Pts',(-22.0018889458697,14.5110248787396,
130.655306915796)) ;
#115406 = CARTESIAN_POINT('Ctrl Pts',(-21.9186831269904,14.4721191969269,
130.37915685792)) ;
#115407 = CARTESIAN_POINT('Ctrl Pts',(-21.8419983594231,14.3577454336847,
130.121978165508)) ;
#115408 = CARTESIAN_POINT('Ctrl Pts',(-21.7784559689967,14.1770688666527,
129.90331119887)) ;
#115409 = CARTESIAN_POINT('Ctrl Pts',(-21.7328730623761,13.9416997327419,
129.73698112711)) ;
#115410 = CARTESIAN_POINT('Ctrl Pts',(-21.7095937547817,13.6694104353782,
129.635852457523)) ;
#115411 = CARTESIAN_POINT('Ctrl Pts',(-21.7108544164153,13.3798585935035,
129.60644988842)) ;
#115412 = CARTESIAN_POINT('Ctrl Pts',(-21.7373587408651,13.0927640382574,
129.650717582232)) ;
#115413 = CARTESIAN_POINT('Ctrl Pts',(-21.7879727694938,12.8294542733058,
129.765423278)) ;
#115414 = CARTESIAN_POINT('Ctrl Pts',(-21.8596572059499,12.6090080043084,
129.941724810289)) ;
#115415 = CARTESIAN_POINT('Ctrl Pts',(-21.9481186483126,12.4466659582347,
130.167016290758)) ;
#115416 = CARTESIAN_POINT('Ctrl Pts',(-22.0478029406896,12.3544265354386,
130.425067159699)) ;
#115417 = CARTESIAN_POINT('Ctrl Pts',(-22.1517530143636,12.338485550426,130.695728652991)) ;
#115418 = CARTESIAN_POINT('Ctrl Pts',(-22.2547791723717,12.4009576070215,
130.963329774343)) ;
#115419 = CARTESIAN_POINT('Ctrl Pts',(-22.3479076849026,12.5356622675021,
131.202441690569)) ;
#115420 = CARTESIAN_POINT('Ctrl Pts',(-22.427039674185,12.7342792931547,131.400473047047)) ;
#115421 = CARTESIAN_POINT('Ctrl Pts',(-22.4865817751364,12.9822470405306,
131.541298758196)) ;
#115422 = CARTESIAN_POINT('Ctrl Pts',(-22.5231351067208,13.2626104241267,
131.614868935857)) ;
#115423 = CARTESIAN_POINT('Ctrl Pts',(-22.5345613145019,13.5537330357078,
131.615129217148)) ;
#115424 = CARTESIAN_POINT('Ctrl Pts',(-22.5210072175352,13.8350780443648,
131.542464925158)) ;
#115425 = CARTESIAN_POINT('Ctrl Pts',(-22.4841282635127,14.0872562376869,
131.401629162015)) ;
#115426 = CARTESIAN_POINT('Ctrl Pts',(-22.4271936380161,14.2922552735091,
131.202157542)) ;
#115427 = CARTESIAN_POINT('Ctrl Pts',(-22.3548468095764,14.4349645919609,
130.957589374496)) ;
#115428 = CARTESIAN_POINT('Ctrl Pts',(-22.2738049730186,14.5045540577175,
130.687866104784)) ;
#115429 = CARTESIAN_POINT('Ctrl Pts',(-22.1896316409164,14.4973581396257,
130.408831550043)) ;
#115430 = CARTESIAN_POINT('Ctrl Pts',(-22.1093343470203,14.4126016842873,
130.14105358009)) ;
#115431 = CARTESIAN_POINT('Ctrl Pts',(-22.0399356599868,14.2578370889756,
129.905309744937)) ;
#115432 = CARTESIAN_POINT('Ctrl Pts',(-21.9863765422796,14.0423606370671,
129.715650705837)) ;
#115433 = CARTESIAN_POINT('Ctrl Pts',(-21.9537345461485,13.7833430848993,
129.58722594006)) ;
#115434 = CARTESIAN_POINT('Ctrl Pts',(-21.9448743026681,13.4972454461382,
129.528113894271)) ;
#115435 = CARTESIAN_POINT('Ctrl Pts',(-21.9611494569257,13.2077137971034,
129.542654652447)) ;
#115436 = CARTESIAN_POINT('Ctrl Pts',(-22.002288346979,12.9318531124,129.629618831657)) ;
#115437 = CARTESIAN_POINT('Ctrl Pts',(-22.0658546135328,12.6922552108513,
129.782222524194)) ;
#115438 = CARTESIAN_POINT('Ctrl Pts',(-22.1480419825475,12.504666487009,129.989213929092)) ;
#115439 = CARTESIAN_POINT('Ctrl Pts',(-22.2443302147763,12.3825157199122,
130.237218364436)) ;
#115440 = CARTESIAN_POINT('Ctrl Pts',(-22.3470392380216,12.3357140444497,
130.504298662281)) ;
#115441 = CARTESIAN_POINT('Ctrl Pts',(-22.4509464733217,12.3660679541908,
130.774724556597)) ;
#115442 = CARTESIAN_POINT('Ctrl Pts',(-22.549161413923,12.4727573812884,131.028420389511)) ;
#115443 = CARTESIAN_POINT('Ctrl Pts',(-22.6347030566716,12.6471452986828,
131.245220928735)) ;
#115444 = CARTESIAN_POINT('Ctrl Pts',(-22.7025433269035,12.8766362181276,
131.410346416835)) ;
#115445 = CARTESIAN_POINT('Ctrl Pts',(-22.7487814948906,13.1457609561308,
131.512289397035)) ;
#115446 = CARTESIAN_POINT('Ctrl Pts',(-22.7705721874272,13.436208516762,131.542656742186)) ;
#115447 = CARTESIAN_POINT('Ctrl Pts',(-22.7669909559281,13.7232902020091,
131.499187113643)) ;
#115448 = CARTESIAN_POINT('Ctrl Pts',(-22.739314974999,13.9896012284326,131.385259077282)) ;
#115449 = CARTESIAN_POINT('Ctrl Pts',(-22.6899563353196,14.2159296230216,
131.207905951156)) ;
#115450 = CARTESIAN_POINT('Ctrl Pts',(-22.6233672864789,14.3851342144556,
130.980263042488)) ;
#115451 = CARTESIAN_POINT('Ctrl Pts',(-22.5449702570784,14.4854516976048,
130.718115056966)) ;
#115452 = CARTESIAN_POINT('Ctrl Pts',(-22.461265093064,14.5096986607512,130.440515127017)) ;
#115453 = CARTESIAN_POINT('Ctrl Pts',(-22.378621004999,14.4561737731647,130.165930931039)) ;
#115454 = CARTESIAN_POINT('Ctrl Pts',(-22.3039082628437,14.3282785458503,
129.914502352423)) ;
#115455 = CARTESIAN_POINT('Ctrl Pts',(-22.2434277952934,14.1363003864466,
129.704779792514)) ;
#115456 = CARTESIAN_POINT('Ctrl Pts',(-22.2017896977858,13.8924839857025,
129.549971716453)) ;
#115457 = CARTESIAN_POINT('Ctrl Pts',(-22.1830205641406,13.6154602436594,
129.462035111654)) ;
#115458 = CARTESIAN_POINT('Ctrl Pts',(-22.1890712067793,13.3244466531158,
129.446574293387)) ;
#115459 = CARTESIAN_POINT('Ctrl Pts',(-22.2202555636145,13.0407282159145,
129.504562629151)) ;
#115460 = CARTESIAN_POINT('Ctrl Pts',(-22.2750211321796,12.7843965627726,
129.631442703902)) ;
#115461 = CARTESIAN_POINT('Ctrl Pts',(-22.3503429335631,12.5734338880589,
129.818316417424)) ;
#115462 = CARTESIAN_POINT('Ctrl Pts',(-22.4414173268538,12.4236459559127,
130.051229799352)) ;
#115463 = CARTESIAN_POINT('Ctrl Pts',(-22.5421394962141,12.3455712635568,
130.312426708327)) ;
#115464 = CARTESIAN_POINT('Ctrl Pts',(-22.6467265172187,12.3443023671055,
130.584788395612)) ;
#115465 = CARTESIAN_POINT('Ctrl Pts',(-22.7481657330948,12.420933178294,130.847899857883)) ;
#115466 = CARTESIAN_POINT('Ctrl Pts',(-22.8392055009209,12.5684896870098,
131.080841902066)) ;
#115467 = CARTESIAN_POINT('Ctrl Pts',(-22.9152137261507,12.7783872300958,
131.269645560269)) ;
#115468 = CARTESIAN_POINT('Ctrl Pts',(-22.9705402435953,13.0341435528073,
131.398130661038)) ;
#115469 = CARTESIAN_POINT('Ctrl Pts',(-23.0022377817911,13.3161552682329,
131.457761074721)) ;
#115470 = CARTESIAN_POINT('Ctrl Pts',(-23.009059140071,13.6077102167408,131.444501189894)) ;
#115471 = CARTESIAN_POINT('Ctrl Pts',(-22.9907943770449,13.8863966863271,
131.357908893058)) ;
#115472 = CARTESIAN_POINT('Ctrl Pts',(-22.9497275238959,14.1306963082603,
131.204837242028)) ;
#115473 = CARTESIAN_POINT('Ctrl Pts',(-22.8897860606364,14.3238933046915,
130.996741057129)) ;
#115474 = CARTESIAN_POINT('Ctrl Pts',(-22.8155047276147,14.4535137780173,
130.746625113997)) ;
#115475 = CARTESIAN_POINT('Ctrl Pts',(-22.7328983548189,14.5094099168095,
130.47211370142)) ;
#115476 = CARTESIAN_POINT('Ctrl Pts',(-22.6487340748289,14.4867701673882,
130.193005786419)) ;
#115477 = CARTESIAN_POINT('Ctrl Pts',(-22.5707021703194,14.3890643828725,
129.932173416396)) ;
#115478 = CARTESIAN_POINT('Ctrl Pts',(-22.5034195621283,14.2211869107964,
129.70237977909)) ;
#115479 = CARTESIAN_POINT('Ctrl Pts',(-22.4535961395973,13.9958858020985,
129.523655290175)) ;
#115480 = CARTESIAN_POINT('Ctrl Pts',(-22.4253306349521,13.7314793548645,
129.40812642471)) ;
#115481 = CARTESIAN_POINT('Ctrl Pts',(-22.4210875175899,13.4423639400344,
129.362455182987)) ;
#115482 = CARTESIAN_POINT('Ctrl Pts',(-22.4422895478426,13.1530743203904,
129.391256495026)) ;
#115483 = CARTESIAN_POINT('Ctrl Pts',(-22.487580667877,12.8842566111771,129.490582827144)) ;
#115484 = CARTESIAN_POINT('Ctrl Pts',(-22.5552977498778,12.6519995362001,
129.655140460866)) ;
#115485 = CARTESIAN_POINT('Ctrl Pts',(-22.6402716313289,12.4766942436469,
129.870371614395)) ;
#115486 = CARTESIAN_POINT('Ctrl Pts',(-22.7378885944903,12.3681120678918,
130.122423877062)) ;
#115487 = CARTESIAN_POINT('Ctrl Pts',(-22.8423855341256,12.3353450096833,
130.394363079284)) ;
#115488 = CARTESIAN_POINT('Ctrl Pts',(-22.9455053804218,12.3808789292608,
130.66253674151)) ;
#115489 = CARTESIAN_POINT('Ctrl Pts',(-23.0414119491019,12.5006496739186,
130.90963712832)) ;
#115490 = CARTESIAN_POINT('Ctrl Pts',(-23.1239874820464,12.6862348924807,
131.117800379368)) ;
#115491 = CARTESIAN_POINT('Ctrl Pts',(-23.1882404954987,12.9253055289241,
131.272326344278)) ;
#115492 = CARTESIAN_POINT('Ctrl Pts',(-23.2299054869804,13.1996774467986,
131.360925356354)) ;
#115493 = CARTESIAN_POINT('Ctrl Pts',(-23.2469197712831,13.4900583198245,
131.37750845876)) ;
#115494 = CARTESIAN_POINT('Ctrl Pts',(-23.2386702442009,13.7765694769724,
131.320183787516)) ;
#115495 = CARTESIAN_POINT('Ctrl Pts',(-23.2064532063664,14.036835662277,131.192930360202)) ;
#115496 = CARTESIAN_POINT('Ctrl Pts',(-23.1537890318512,14.2522894974628,
131.006121661116)) ;
#115497 = CARTESIAN_POINT('Ctrl Pts',(-23.0841408392017,14.410142650821,130.769355953609)) ;
#115498 = CARTESIAN_POINT('Ctrl Pts',(-23.0044224542759,14.4959011359271,
130.503451200898)) ;
#115499 = CARTESIAN_POINT('Ctrl Pts',(-22.9205051252153,14.5055615596735,
130.225254015656)) ;
#115500 = CARTESIAN_POINT('Ctrl Pts',(-22.8387642579551,14.4373879166647,
129.953265322989)) ;
#115501 = CARTESIAN_POINT('Ctrl Pts',(-22.7664377143828,14.2968056087925,
129.708895562602)) ;
#115502 = CARTESIAN_POINT('Ctrl Pts',(-22.7090205846332,14.0934340145334,
129.508020332236)) ;
#115503 = CARTESIAN_POINT('Ctrl Pts',(-22.6715788423865,13.8423638114029,
129.365551179356)) ;
#115504 = CARTESIAN_POINT('Ctrl Pts',(-22.6573294356865,13.5615577206812,
129.290854833297)) ;
#115505 = CARTESIAN_POINT('Ctrl Pts',(-22.6681862864359,13.2694348944804,
129.289338191419)) ;
#115506 = CARTESIAN_POINT('Ctrl Pts',(-22.7039617574597,12.9897647818979,
129.360785289403)) ;
#115507 = CARTESIAN_POINT('Ctrl Pts',(-22.7629534424542,12.7403852471457,
129.499963464368)) ;
#115508 = CARTESIAN_POINT('Ctrl Pts',(-22.8415892215112,12.5401778472151,
129.696554511139)) ;
#115509 = CARTESIAN_POINT('Ctrl Pts',(-22.9348979213409,12.4032538731495,
129.936029182917)) ;
#115510 = CARTESIAN_POINT('Ctrl Pts',(-23.0370685674519,12.3392654765734,
130.201366375023)) ;
#115511 = CARTESIAN_POINT('Ctrl Pts',(-23.141478431911,12.3529795705707,130.473233214815)) ;
#115512 = CARTESIAN_POINT('Ctrl Pts',(-23.2412861780916,12.44341496887,130.731668708428)) ;
#115513 = CARTESIAN_POINT('Ctrl Pts',(-23.330047912579,12.6038142404483,130.957868037024)) ;
#115514 = CARTESIAN_POINT('Ctrl Pts',(-23.4023245485338,12.8232746698558,
131.135851245433)) ;
#115515 = CARTESIAN_POINT('Ctrl Pts',(-23.4533693512746,13.0848674095602,
131.251920028465)) ;
#115516 = CARTESIAN_POINT('Ctrl Pts',(-23.4806176034136,13.3712340427374,
131.298395105942)) ;
#115517 = CARTESIAN_POINT('Ctrl Pts',(-23.4825810779044,13.6620670155129,
131.270922868641)) ;
#115518 = CARTESIAN_POINT('Ctrl Pts',(-23.4599091408466,13.9347879219274,
131.171598398464)) ;
#115519 = CARTESIAN_POINT('Ctrl Pts',(-23.4149763968351,14.1711547034761,
131.007212926626)) ;
#115520 = CARTESIAN_POINT('Ctrl Pts',(-23.3516961209413,14.3538985958079,
130.789228498426)) ;
#115521 = CARTESIAN_POINT('Ctrl Pts',(-23.2754093744269,14.4699515410886,
130.533273425003)) ;
#115522 = CARTESIAN_POINT('Ctrl Pts',(-23.1921867842084,14.511011729743,130.257027506385)) ;
#115523 = CARTESIAN_POINT('Ctrl Pts',(-23.1089561500767,14.4745400421894,
129.980842840064)) ;
#115524 = CARTESIAN_POINT('Ctrl Pts',(-23.031552894356,14.3614974996119,129.721369859714)) ;
#115525 = CARTESIAN_POINT('Ctrl Pts',(-22.9678477580129,14.1829580277845,
129.502345220066)) ;
#115526 = CARTESIAN_POINT('Ctrl Pts',(-22.9216856506781,13.9492404929465,
129.334353763701)) ;
#115527 = CARTESIAN_POINT('Ctrl Pts',(-22.8977300159152,13.6775800982586,
129.231228230102)) ;
#115528 = CARTESIAN_POINT('Ctrl Pts',(-22.8981933527482,13.3886494635436,
129.19954520776)) ;
#115529 = CARTESIAN_POINT('Ctrl Pts',(-22.9242400045738,13.0993478015478,
129.242254988579)) ;
#115530 = CARTESIAN_POINT('Ctrl Pts',(-22.9739037222349,12.8369458310676,
129.354415199943)) ;
#115531 = CARTESIAN_POINT('Ctrl Pts',(-23.0453252131747,12.6140529768099,
129.529801908795)) ;
#115532 = CARTESIAN_POINT('Ctrl Pts',(-23.1330410816671,12.4507323341902,
129.753058144926)) ;
#115533 = CARTESIAN_POINT('Ctrl Pts',(-23.2324941335687,12.3558899306528,
130.010420059215)) ;
#115534 = CARTESIAN_POINT('Ctrl Pts',(-23.3371521212107,12.3380969081111,
130.282910607247)) ;
#115535 = CARTESIAN_POINT('Ctrl Pts',(-23.4390406262999,12.3976016694818,
130.547608591386)) ;
#115536 = CARTESIAN_POINT('Ctrl Pts',(-23.5331839274626,12.530583824708,130.789474316628)) ;
#115537 = CARTESIAN_POINT('Ctrl Pts',(-23.6129508354768,12.7283490506027,
130.989275182951)) ;
#115538 = CARTESIAN_POINT('Ctrl Pts',(-23.6728864226876,12.9742771227128,
131.13136588872)) ;
#115539 = CARTESIAN_POINT('Ctrl Pts',(-23.71018774412,13.2539376227601,131.207121504005)) ;
#115540 = CARTESIAN_POINT('Ctrl Pts',(-23.7223865299285,13.5450903335013,
131.209633661058)) ;
#115541 = CARTESIAN_POINT('Ctrl Pts',(-23.7094914718236,13.8275787514848,
131.138820807372)) ;
#115542 = CARTESIAN_POINT('Ctrl Pts',(-23.6732974807833,14.080619519853,131.000028693289)) ;
#115543 = CARTESIAN_POINT('Ctrl Pts',(-23.616590785082,14.2877392133105,130.801091824847)) ;
#115544 = CARTESIAN_POINT('Ctrl Pts',(-23.5452916636683,14.431213841156,130.559896288173)) ;
#115545 = CARTESIAN_POINT('Ctrl Pts',(-23.4637700924587,14.5038738166411,
130.288489711948)) ;
#115546 = CARTESIAN_POINT('Ctrl Pts',(-23.3797591259085,14.4984557576167,
130.010000564517)) ;
#115547 = CARTESIAN_POINT('Ctrl Pts',(-23.2994671912968,14.4164646825051,
129.742342495005)) ;
#115548 = CARTESIAN_POINT('Ctrl Pts',(-23.2292002172557,14.2622140461571,
129.503806387235)) ;
#115549 = CARTESIAN_POINT('Ctrl Pts',(-23.1755337197615,14.0497489487789,
129.314087251754)) ;
#115550 = CARTESIAN_POINT('Ctrl Pts',(-23.1420903990703,13.7905258352839,
129.183151437944)) ;
#115551 = CARTESIAN_POINT('Ctrl Pts',(-23.1325295042077,13.506486494377,129.12218848079)) ;
#115552 = CARTESIAN_POINT('Ctrl Pts',(-23.1482921851681,13.2142515667239,
129.134926916223)) ;
#115553 = CARTESIAN_POINT('Ctrl Pts',(-23.188353413262,12.9406232851689,129.219102820939)) ;
#115554 = CARTESIAN_POINT('Ctrl Pts',(-23.2515823582444,12.6982138740687,
129.370525672368)) ;
#115555 = CARTESIAN_POINT('Ctrl Pts',(-23.3330631497147,12.5096112048297,
129.575565311669)) ;
#115556 = CARTESIAN_POINT('Ctrl Pts',(-23.4290906890084,12.3850648620669,
129.822774700949)) ;
#115557 = CARTESIAN_POINT('Ctrl Pts',(-23.531784997696,12.3359713268051,130.089781167871)) ;
#115558 = CARTESIAN_POINT('Ctrl Pts',(-23.6357879798494,12.3641515700291,
130.360476235555)) ;
#115559 = CARTESIAN_POINT('Ctrl Pts',(-23.7340953356143,12.4683944776065,
130.614508785511)) ;
#115560 = CARTESIAN_POINT('Ctrl Pts',(-23.8203211365081,12.6414744910879,
130.833207334208)) ;
#115561 = CARTESIAN_POINT('Ctrl Pts',(-23.8886881736005,12.8692739707259,
130.99991574651)) ;
#115562 = CARTESIAN_POINT('Ctrl Pts',(-23.9357467861378,13.1394382839076,
131.104034823546)) ;
#115563 = CARTESIAN_POINT('Ctrl Pts',(-23.9579774455155,13.4257125423889,
131.136139167156)) ;
#115564 = CARTESIAN_POINT('Ctrl Pts',(-23.9552750237727,13.7153678926771,
131.094978168242)) ;
#115565 = CARTESIAN_POINT('Ctrl Pts',(-23.9282090173285,13.9823826092166,
130.982854215722)) ;
#115566 = CARTESIAN_POINT('Ctrl Pts',(-23.8793697422226,14.210351268189,130.806979650137)) ;
#115567 = CARTESIAN_POINT('Ctrl Pts',(-23.8133153702057,14.3810373513132,
130.58096078673)) ;
#115568 = CARTESIAN_POINT('Ctrl Pts',(-23.735209224892,14.4835203874639,130.319669563206)) ;
#115569 = CARTESIAN_POINT('Ctrl Pts',(-23.6515414522142,14.5102051470099,
130.042171972968)) ;
#115570 = CARTESIAN_POINT('Ctrl Pts',(-23.5684272969825,14.4584272467564,
129.766068717826)) ;
#115571 = CARTESIAN_POINT('Ctrl Pts',(-23.4938231437372,14.3332271538461,
129.515148015428)) ;
#115572 = CARTESIAN_POINT('Ctrl Pts',(-23.4326135115301,14.1422679027751,
129.303162687106)) ;
#115573 = CARTESIAN_POINT('Ctrl Pts',(-23.3905185584406,13.9003526545792,
129.147122527455)) ;
#115574 = CARTESIAN_POINT('Ctrl Pts',(-23.3709966570516,13.6237176044633,
129.056941792442)) ;
#115575 = CARTESIAN_POINT('Ctrl Pts',(-23.3763211847102,13.3329588361478,
129.039378660403)) ;
#115576 = CARTESIAN_POINT('Ctrl Pts',(-23.4068246825045,13.0482791472687,
129.095326134194)) ;
#115577 = CARTESIAN_POINT('Ctrl Pts',(-23.4611218639704,12.7905984211716,
129.220781957599)) ;
#115578 = CARTESIAN_POINT('Ctrl Pts',(-23.5355417145057,12.5792074314873,
129.405190030391)) ;
#115579 = CARTESIAN_POINT('Ctrl Pts',(-23.6262276903051,12.4271420328258,
129.636951252849)) ;
#115580 = CARTESIAN_POINT('Ctrl Pts',(-23.72702713312,12.3466854620337,129.898286196702)) ;
#115581 = CARTESIAN_POINT('Ctrl Pts',(-23.8314987159718,12.3433384451733,
130.170343083653)) ;
#115582 = CARTESIAN_POINT('Ctrl Pts',(-23.9327910170219,12.417256873973,130.433143999051)) ;
#115583 = CARTESIAN_POINT('Ctrl Pts',(-24.0245736232509,12.5633304568432,
130.668126155051)) ;
#115584 = CARTESIAN_POINT('Ctrl Pts',(-24.1008197720403,12.7708593905581,
130.857750684135)) ;
#115585 = CARTESIAN_POINT('Ctrl Pts',(-24.1569294635632,13.025326349885,130.988518737243)) ;
#115586 = CARTESIAN_POINT('Ctrl Pts',(-24.1894985627988,13.3082178025067,
131.05053265747)) ;
#115587 = CARTESIAN_POINT('Ctrl Pts',(-24.196965740994,13.5990344955289,131.039249671657)) ;
#115588 = CARTESIAN_POINT('Ctrl Pts',(-24.1795877670942,13.8774216043795,
130.955375021049)) ;
#115589 = CARTESIAN_POINT('Ctrl Pts',(-24.1390939585473,14.1239848990119,
130.803863087357)) ;
#115590 = CARTESIAN_POINT('Ctrl Pts',(-24.0794901932382,14.3192776170792,
130.596679031769)) ;
#115591 = CARTESIAN_POINT('Ctrl Pts',(-24.0055352361048,14.4507732360595,
130.347522670003)) ;
#115592 = CARTESIAN_POINT('Ctrl Pts',(-23.9233178114793,14.5087792678555,
130.074243320989)) ;
#115593 = CARTESIAN_POINT('Ctrl Pts',(-23.8391129704671,14.4887238336712,
129.795024289797)) ;
#115594 = CARTESIAN_POINT('Ctrl Pts',(-23.7605064372372,14.3928285084541,
129.532382450158)) ;
#115595 = CARTESIAN_POINT('Ctrl Pts',(-23.6928180061624,14.2263682040696,
129.30137255382)) ;
#115596 = CARTESIAN_POINT('Ctrl Pts',(-23.6426620351328,14.0038696460673,
129.121863214626)) ;
#115597 = CARTESIAN_POINT('Ctrl Pts',(-23.613563581647,13.7389372008462,129.003713269081)) ;
#115598 = CARTESIAN_POINT('Ctrl Pts',(-23.6086509708226,13.4518073715824,
128.956278206236)) ;
#115599 = CARTESIAN_POINT('Ctrl Pts',(-23.6290105898186,13.1616327439453,
128.982551634326)) ;
#115600 = CARTESIAN_POINT('Ctrl Pts',(-23.6739522585566,12.8906304372966,
129.080681338749)) ;
#115601 = CARTESIAN_POINT('Ctrl Pts',(-23.7407279250101,12.6585325321797,
129.242687250476)) ;
#115602 = CARTESIAN_POINT('Ctrl Pts',(-23.8252467089156,12.4808578746759,
129.456558276985)) ;
#115603 = CARTESIAN_POINT('Ctrl Pts',(-23.9234212908845,12.369794968941,129.709975426016)) ;
#115604 = CARTESIAN_POINT('Ctrl Pts',(-24.0266916219991,12.3353140243209,
129.978700782335)) ;
#115605 = CARTESIAN_POINT('Ctrl Pts',(-24.1303332495694,12.3783402005982,
130.248268071055)) ;
#115606 = CARTESIAN_POINT('Ctrl Pts',(-24.2265146825975,12.4961137906607,
130.496181048475)) ;
#115607 = CARTESIAN_POINT('Ctrl Pts',(-24.3096595921357,12.6800956082709,
130.705970404282)) ;
#115608 = CARTESIAN_POINT('Ctrl Pts',(-24.3745179631744,12.9180877152906,
130.862244767084)) ;
#115609 = CARTESIAN_POINT('Ctrl Pts',(-24.4167847945233,13.1911275173993,
130.952669619891)) ;
#115610 = CARTESIAN_POINT('Ctrl Pts',(-24.4345812423772,13.4815072415882,
130.971518185869)) ;
#115611 = CARTESIAN_POINT('Ctrl Pts',(-24.4270213519574,13.7684314308885,
130.916204524826)) ;
#115612 = CARTESIAN_POINT('Ctrl Pts',(-24.3956514842814,14.029076308477,130.791530690429)) ;
#115613 = CARTESIAN_POINT('Ctrl Pts',(-24.343165506001,14.2473093926041,130.605025756878)) ;
#115614 = CARTESIAN_POINT('Ctrl Pts',(-24.2745743047042,14.4057091519906,
130.371660986809)) ;
#115615 = CARTESIAN_POINT('Ctrl Pts',(-24.1945925450092,14.4946178708306,
130.104760579953)) ;
#115616 = CARTESIAN_POINT('Ctrl Pts',(-24.11071512251,14.5063975208026,129.826695894897)) ;
#115617 = CARTESIAN_POINT('Ctrl Pts',(-24.0286060386776,14.4401278585609,
129.553540640394)) ;
#115618 = CARTESIAN_POINT('Ctrl Pts',(-23.9562423178897,14.3020001323071,
129.309200756072)) ;
#115619 = CARTESIAN_POINT('Ctrl Pts',(-23.8982704981956,14.100380875427,129.106698871819)) ;
#115620 = CARTESIAN_POINT('Ctrl Pts',(-23.8601423404147,13.8504602239821,
128.962217821069)) ;
#115621 = CARTESIAN_POINT('Ctrl Pts',(-23.8451537683981,13.5690360496352,
128.88522225926)) ;
#115622 = CARTESIAN_POINT('Ctrl Pts',(-23.85536903869,13.277347744237,128.881881865911)) ;
#115623 = CARTESIAN_POINT('Ctrl Pts',(-23.8903250024146,12.9978265767653,
128.951024979183)) ;
#115624 = CARTESIAN_POINT('Ctrl Pts',(-23.9487275671782,12.747023860199,129.088449649182)) ;
#115625 = CARTESIAN_POINT('Ctrl Pts',(-24.0267536508702,12.5453431667421,
129.283298823089)) ;
#115626 = CARTESIAN_POINT('Ctrl Pts',(-24.1198629233628,12.4062333259034,
129.52213584094)) ;
#115627 = CARTESIAN_POINT('Ctrl Pts',(-24.2215666079949,12.3400677949455,
129.786207600519)) ;
#115628 = CARTESIAN_POINT('Ctrl Pts',(-24.3264846884265,12.3515722965719,
130.059403729799)) ;
#115629 = CARTESIAN_POINT('Ctrl Pts',(-24.4261565993231,12.4396025465946,
130.317564726088)) ;
#115630 = CARTESIAN_POINT('Ctrl Pts',(-24.515504520949,12.5983879462257,130.545404926639)) ;
#115631 = CARTESIAN_POINT('Ctrl Pts',(-24.5881171815504,12.8155081778463,
130.724487254865)) ;
#115632 = CARTESIAN_POINT('Ctrl Pts',(-24.6401896035301,13.0777480891852,
130.8433438272)) ;
#115633 = CARTESIAN_POINT('Ctrl Pts',(-24.6679851185762,13.3640007134148,
130.891395810982)) ;
#115634 = CARTESIAN_POINT('Ctrl Pts',(-24.6706717433523,13.6530970190172,
130.866255003353)) ;
#115635 = CARTESIAN_POINT('Ctrl Pts',(-24.6486810155768,13.9274410550996,
130.768823051012)) ;
#115636 = CARTESIAN_POINT('Ctrl Pts',(-24.6043588117149,14.1649405448642,
130.60624558075)) ;
#115637 = CARTESIAN_POINT('Ctrl Pts',(-24.5413708101056,14.3499176915205,
130.389027795027)) ;
#115638 = CARTESIAN_POINT('Ctrl Pts',(-24.4653494690363,14.4676736740884,
130.133852904625)) ;
#115639 = CARTESIAN_POINT('Ctrl Pts',(-24.3825873013246,14.5109849198275,
129.859094894237)) ;
#115640 = CARTESIAN_POINT('Ctrl Pts',(-24.2987925768636,14.4763368011369,
129.58106163939)) ;
#115641 = CARTESIAN_POINT('Ctrl Pts',(-24.2217612201684,14.3664425274482,
129.322969701944)) ;
#115642 = CARTESIAN_POINT('Ctrl Pts',(-24.1570057110458,14.1882602546085,
129.100578369949)) ;
#115643 = CARTESIAN_POINT('Ctrl Pts',(-24.1105157071068,13.9563928712726,
128.931742068379)) ;
#115644 = CARTESIAN_POINT('Ctrl Pts',(-24.0858458393616,13.6856075071528,
128.826527819527)) ;
#115645 = CARTESIAN_POINT('Ctrl Pts',(-24.0856539585114,13.3967978155194,
128.792918629269)) ;
#115646 = CARTESIAN_POINT('Ctrl Pts',(-24.1107926076059,13.1083772147109,
128.833125740032)) ;
#115647 = CARTESIAN_POINT('Ctrl Pts',(-24.1600137825134,12.8436201216384,
128.943820657913)) ;
#115648 = CARTESIAN_POINT('Ctrl Pts',(-24.2308058798189,12.6197329650473,
129.117423409396)) ;
#115649 = CARTESIAN_POINT('Ctrl Pts',(-24.3182751718309,12.4541610182818,
129.339893353894)) ;
#115650 = CARTESIAN_POINT('Ctrl Pts',(-24.4176896908462,12.3575181073951,
129.59708909666)) ;
#115651 = CARTESIAN_POINT('Ctrl Pts',(-24.5213942641841,12.337407534574,129.86708474398)) ;
#115652 = CARTESIAN_POINT('Ctrl Pts',(-24.6242611097352,12.3950240477661,
130.134369464736)) ;
#115653 = CARTESIAN_POINT('Ctrl Pts',(-24.7182893080511,12.5255974682326,
130.376052536827)) ;
#115654 = CARTESIAN_POINT('Ctrl Pts',(-24.7987860343519,12.7221236513144,
130.577891266987)) ;
#115655 = CARTESIAN_POINT('Ctrl Pts',(-24.8592668458931,12.966643820031,130.721612719223)) ;
#115656 = CARTESIAN_POINT('Ctrl Pts',(-24.8973477603996,13.2467842966359,
130.799514303858)) ;
#115657 = CARTESIAN_POINT('Ctrl Pts',(-24.9101357439362,13.5364084867458,
130.803917200582)) ;
#115658 = CARTESIAN_POINT('Ctrl Pts',(-24.8980433329888,13.819301352246,130.735470391269)) ;
#115659 = CARTESIAN_POINT('Ctrl Pts',(-24.8624508729161,14.0737430594077,
130.598397208659)) ;
#115660 = CARTESIAN_POINT('Ctrl Pts',(-24.8063650001413,14.2823383256047,
130.401314654759)) ;
#115661 = CARTESIAN_POINT('Ctrl Pts',(-24.7352153152331,14.4280819786068,
130.160457808913)) ;
#115662 = CARTESIAN_POINT('Ctrl Pts',(-24.654277110767,14.5027907188546,129.890917785084)) ;
#115663 = CARTESIAN_POINT('Ctrl Pts',(-24.569599491767,14.4996009182714,129.610218523976)) ;
#115664 = CARTESIAN_POINT('Ctrl Pts',(-24.4895659727805,14.4198435135005,
129.343494691889)) ;
#115665 = CARTESIAN_POINT('Ctrl Pts',(-24.4190126879205,14.2682255575811,
129.104196361098)) ;
#115666 = CARTESIAN_POINT('Ctrl Pts',(-24.364598178107,14.0566692320112,128.91218100257)) ;
#115667 = CARTESIAN_POINT('Ctrl Pts',(-24.3305009683015,13.7984046917339,
128.779328284604)) ;
#115668 = CARTESIAN_POINT('Ctrl Pts',(-24.3202768420663,13.5146255183712,
128.716401612773)) ;
#115669 = CARTESIAN_POINT('Ctrl Pts',(-24.3351461344103,13.22379017507,128.726708255358)) ;
#115670 = CARTESIAN_POINT('Ctrl Pts',(-24.3747056074861,12.9476430099182,
128.809207275973)) ;
#115671 = CARTESIAN_POINT('Ctrl Pts',(-24.4373988447194,12.7041858709694,
128.959075140171)) ;
#115672 = CARTESIAN_POINT('Ctrl Pts',(-24.5182754986541,12.5142908380612,
129.162405255088)) ;
#115673 = CARTESIAN_POINT('Ctrl Pts',(-24.6137660742652,12.3877724329813,
129.408115006488)) ;
#115674 = CARTESIAN_POINT('Ctrl Pts',(-24.7167971690515,12.3361912043238,
129.675956387308)) ;
#115675 = CARTESIAN_POINT('Ctrl Pts',(-24.8208049085079,12.3624798224069,
129.946681899111)) ;
#115676 = CARTESIAN_POINT('Ctrl Pts',(-24.9189695732058,12.4640688022784,
130.200435824458)) ;
#115677 = CARTESIAN_POINT('Ctrl Pts',(-25.005956640633,12.6358046245907,130.421244636591)) ;
#115678 = CARTESIAN_POINT('Ctrl Pts',(-25.0747012664645,12.862048858162,130.589103084132)) ;
#115679 = CARTESIAN_POINT('Ctrl Pts',(-25.1223375525266,13.1294243703739,
130.69512008432)) ;
#115680 = CARTESIAN_POINT('Ctrl Pts',(-25.1455445896858,13.419127554444,130.729642616116)) ;
#115681 = CARTESIAN_POINT('Ctrl Pts',(-25.1435152363736,13.7060585256719,
130.690801967982)) ;
#115682 = CARTESIAN_POINT('Ctrl Pts',(-25.1170308827865,13.9758635071568,
130.580144935401)) ;
#115683 = CARTESIAN_POINT('Ctrl Pts',(-25.0688142460135,14.2044690811379,
130.40618368144)) ;
#115684 = CARTESIAN_POINT('Ctrl Pts',(-25.003123247664,14.3772046466544,130.18118138791)) ;
#115685 = CARTESIAN_POINT('Ctrl Pts',(-24.9252844700022,14.4817041640368,
129.920684773534)) ;
#115686 = CARTESIAN_POINT('Ctrl Pts',(-24.8415989541778,14.5103977605507,
129.643097336818)) ;
#115687 = CARTESIAN_POINT('Ctrl Pts',(-24.7589132492041,14.461387716176,129.368476107022)) ;
#115688 = CARTESIAN_POINT('Ctrl Pts',(-24.6835796855055,14.3378670523305,
129.115253926662)) ;
#115689 = CARTESIAN_POINT('Ctrl Pts',(-24.6219712562161,14.1487649480966,
128.902143850339)) ;
#115690 = CARTESIAN_POINT('Ctrl Pts',(-24.5791815584349,13.9077124472436,
128.744012805924)) ;
#115691 = CARTESIAN_POINT('Ctrl Pts',(-24.5590011432879,13.6318349091011,
128.651919455676)) ;
#115692 = CARTESIAN_POINT('Ctrl Pts',(-24.5636129562954,13.3411961915081,
128.632272182411)) ;
#115693 = CARTESIAN_POINT('Ctrl Pts',(-24.5933692421231,13.0563347009616,
128.686073174335)) ;
#115694 = CARTESIAN_POINT('Ctrl Pts',(-24.6470060166101,12.7976622253545,
128.809603060301)) ;
#115695 = CARTESIAN_POINT('Ctrl Pts',(-24.7208016129616,12.584625305209,128.992205539617)) ;
#115696 = CARTESIAN_POINT('Ctrl Pts',(-24.8118536009071,12.429833286881,129.224781939929)) ;
#115697 = CARTESIAN_POINT('Ctrl Pts',(-24.911545430168,12.3481748757021,129.483189757942)) ;
#115698 = CARTESIAN_POINT('Ctrl Pts',(-25.0164125625319,12.3422836205948,
129.75626651559)) ;
#115699 = CARTESIAN_POINT('Ctrl Pts',(-25.117816306108,12.414162317258,130.019416608038)) ;
#115700 = CARTESIAN_POINT('Ctrl Pts',(-25.2100635855326,12.55849168118,130.255714929222)) ;
#115701 = CARTESIAN_POINT('Ctrl Pts',(-25.2867433505999,12.7644624942609,
130.446624226534)) ;
#115702 = CARTESIAN_POINT('Ctrl Pts',(-25.3433959651672,13.0174115077838,
130.579031809203)) ;
#115703 = CARTESIAN_POINT('Ctrl Pts',(-25.3766991434267,13.2998964348547,
130.643172314106)) ;
#115704 = CARTESIAN_POINT('Ctrl Pts',(-25.3849027762527,13.5908799629275,
130.634029729427)) ;
#115705 = CARTESIAN_POINT('Ctrl Pts',(-25.3681244270798,13.8706960081611,
130.551809717868)) ;
#115706 = CARTESIAN_POINT('Ctrl Pts',(-25.3281885696402,14.1180202656557,
130.401959719847)) ;
#115707 = CARTESIAN_POINT('Ctrl Pts',(-25.2692654377525,14.3143765894564,
130.196866938718)) ;
#115708 = CARTESIAN_POINT('Ctrl Pts',(-25.1954627990625,14.4481660809184,
129.948075722546)) ;
#115709 = CARTESIAN_POINT('Ctrl Pts',(-25.1135963031033,14.5080838606745,
129.675906827394)) ;
#115710 = CARTESIAN_POINT('Ctrl Pts',(-25.0294161558255,14.4905518531177,
129.396790506061)) ;
#115711 = CARTESIAN_POINT('Ctrl Pts',(-24.9503166631056,14.3964092296967,
129.132598410075)) ;
#115712 = CARTESIAN_POINT('Ctrl Pts',(-24.8824484698929,14.232304987228,128.901173407916)) ;
#115713 = CARTESIAN_POINT('Ctrl Pts',(-24.831656485841,14.0113006854444,128.719789796304)) ;
#115714 = CARTESIAN_POINT('Ctrl Pts',(-24.8018618709668,13.7469853282518,
128.599564702445)) ;
#115715 = CARTESIAN_POINT('Ctrl Pts',(-24.7961937055128,13.4601451324146,
128.54991646717)) ;
#115716 = CARTESIAN_POINT('Ctrl Pts',(-24.8160226315964,13.1687003200991,
128.574510511953)) ;
#115717 = CARTESIAN_POINT('Ctrl Pts',(-24.859902739483,12.8989650919222,128.669805113981)) ;
#115718 = CARTESIAN_POINT('Ctrl Pts',(-24.9266168659618,12.6635916504989,
128.831356633498)) ;
#115719 = CARTESIAN_POINT('Ctrl Pts',(-25.0103639202873,12.485239800862,129.043133485935)) ;
#115720 = CARTESIAN_POINT('Ctrl Pts',(-25.1082951885594,12.3719259500599,
129.295815313463)) ;
#115721 = CARTESIAN_POINT('Ctrl Pts',(-25.2113378058678,12.3351771032852,
129.563924734244)) ;
#115722 = CARTESIAN_POINT('Ctrl Pts',(-25.3153987713946,12.3762351050997,
129.834608633564)) ;
#115723 = CARTESIAN_POINT('Ctrl Pts',(-25.4113691303234,12.4911992435135,
130.082089209234)) ;
#115724 = CARTESIAN_POINT('Ctrl Pts',(-25.4955318190917,12.6745749260732,
130.29463045715)) ;
#115725 = CARTESIAN_POINT('Ctrl Pts',(-25.560704508805,12.9105841176317,130.451940846143)) ;
#115726 = CARTESIAN_POINT('Ctrl Pts',(-25.6037591586016,13.1834575472762,
130.544589177351)) ;
#115727 = CARTESIAN_POINT('Ctrl Pts',(-25.6221540731369,13.4728172007292,
130.565280977399)) ;
#115728 = CARTESIAN_POINT('Ctrl Pts',(-25.6154890774634,13.7593252111675,
130.512691578256)) ;
#115729 = CARTESIAN_POINT('Ctrl Pts',(-25.5845017414514,14.0229111380707,
130.388875573167)) ;
#115730 = CARTESIAN_POINT('Ctrl Pts',(-25.5329646548234,14.2409568530166,
130.205405121793)) ;
#115731 = CARTESIAN_POINT('Ctrl Pts',(-25.4643492210366,14.4024702596202,
129.971739445436)) ;
#115732 = CARTESIAN_POINT('Ctrl Pts',(-25.3848249850593,14.4930252918819,
129.706290426526)) ;
#115733 = CARTESIAN_POINT('Ctrl Pts',(-25.3009346998094,14.5071138077779,
129.428162516891)) ;
#115734 = CARTESIAN_POINT('Ctrl Pts',(-25.2189936227422,14.4434722304718,
129.155638517111)) ;
#115735 = CARTESIAN_POINT('Ctrl Pts',(-25.1460018098747,14.3072991508372,
128.909365963459)) ;
#115736 = CARTESIAN_POINT('Ctrl Pts',(-25.0872927957611,14.1061281755834,
128.704547183538)) ;
#115737 = CARTESIAN_POINT('Ctrl Pts',(-25.0487858755379,13.8584458365122,
128.559117426276)) ;
#115738 = CARTESIAN_POINT('Ctrl Pts',(-25.0330304801592,13.5782527615593,
128.479942965013)) ;
#115739 = CARTESIAN_POINT('Ctrl Pts',(-25.0424542208566,13.2862405830432,
128.474252693863)) ;
#115740 = CARTESIAN_POINT('Ctrl Pts',(-25.0767412324267,13.0054673407222,
128.541371132674)) ;
#115741 = CARTESIAN_POINT('Ctrl Pts',(-25.1348051000407,12.7527978446706,
128.67768872235)) ;
#115742 = CARTESIAN_POINT('Ctrl Pts',(-25.2119030388808,12.5507722085017,
128.870018404504)) ;
#115743 = CARTESIAN_POINT('Ctrl Pts',(-25.3047050008252,12.4092693590586,
129.107923829017)) ;
#115744 = CARTESIAN_POINT('Ctrl Pts',(-25.406443595545,12.3409406073707,129.37203421041)) ;
#115745 = CARTESIAN_POINT('Ctrl Pts',(-25.5110390200225,12.3499819194409,
129.644402105975)) ;
#115746 = CARTESIAN_POINT('Ctrl Pts',(-25.6114390222507,12.4363532158425,
129.904516274518)) ;
#115747 = CARTESIAN_POINT('Ctrl Pts',(-25.7007310200177,12.5925663631045,
130.132357144071)) ;
#115748 = CARTESIAN_POINT('Ctrl Pts',(-25.7740950725506,12.8085170384963,
130.313559518156)) ;
#115749 = CARTESIAN_POINT('Ctrl Pts',(-25.8267351162025,13.0694866152918,
130.434112913458)) ;
#115750 = CARTESIAN_POINT('Ctrl Pts',(-25.8553312907165,13.3550371201656,
130.48453070364)) ;
#115751 = CARTESIAN_POINT('Ctrl Pts',(-25.8586885366147,13.6462143005165,
130.461126760816)) ;
#115752 = CARTESIAN_POINT('Ctrl Pts',(-25.837444412916,13.9195287631536,130.366084906634)) ;
#115753 = CARTESIAN_POINT('Ctrl Pts',(-25.7937488394422,14.1586150899391,
130.205310735235)) ;
#115754 = CARTESIAN_POINT('Ctrl Pts',(-25.7313611315605,14.3449689837057,
129.989913913384)) ;
#115755 = CARTESIAN_POINT('Ctrl Pts',(-25.6556964572195,14.465239738532,129.735783996914)) ;
#115756 = CARTESIAN_POINT('Ctrl Pts',(-25.5723964230934,14.5107689866746,
129.459195604095)) ;
#115757 = CARTESIAN_POINT('Ctrl Pts',(-25.4893174125801,14.4787461978325,
129.183580822489)) ;
#115758 = CARTESIAN_POINT('Ctrl Pts',(-25.4113051186338,14.3700644324197,
128.922314853824)) ;
#115759 = CARTESIAN_POINT('Ctrl Pts',(-25.3465909420863,14.1946408166751,
128.700275185896)) ;
#115760 = CARTESIAN_POINT('Ctrl Pts',(-25.299369271165,13.963907732595,128.529234819729)) ;
#115761 = CARTESIAN_POINT('Ctrl Pts',(-25.2739922523,13.6940409321305,128.421969041019)) ;
#115762 = CARTESIAN_POINT('Ctrl Pts',(-25.2731534451911,13.4043243937501,
128.386332734542)) ;
#115763 = CARTESIAN_POINT('Ctrl Pts',(-25.2973628386527,13.1175424358185,
128.424062655725)) ;
#115764 = CARTESIAN_POINT('Ctrl Pts',(-25.3462006392316,12.8501254079525,
128.533419495547)) ;
#115765 = CARTESIAN_POINT('Ctrl Pts',(-25.4160919098287,12.6260375389968,
128.704569775621)) ;
#115766 = CARTESIAN_POINT('Ctrl Pts',(-25.5032418915579,12.4581545252769,
128.926046604269)) ;
#115767 = CARTESIAN_POINT('Ctrl Pts',(-25.6021785519615,12.3594525497003,
129.181922681907)) ;
#115768 = CARTESIAN_POINT('Ctrl Pts',(-25.7061730224389,12.3367944069397,
129.452652747223)) ;
#115769 = CARTESIAN_POINT('Ctrl Pts',(-25.8094492173163,12.3925085409291,
129.721047874811)) ;
#115770 = CARTESIAN_POINT('Ctrl Pts',(-25.9037624326914,12.5213898755188,
129.963557213451)) ;
#115771 = CARTESIAN_POINT('Ctrl Pts',(-25.9844805178092,12.7155724021421,
130.166157205425)) ;
#115772 = CARTESIAN_POINT('Ctrl Pts',(-26.0456691934443,12.9595220676015,
130.311865673155)) ;
#115773 = CARTESIAN_POINT('Ctrl Pts',(-26.0842093042236,13.2367788940881,
130.391368626224)) ;
#115774 = CARTESIAN_POINT('Ctrl Pts',(-26.0979544525776,13.5277643625836,
130.39839898417)) ;
#115775 = CARTESIAN_POINT('Ctrl Pts',(-26.0864824258526,13.8120453761231,
130.331665108325)) ;
#115776 = CARTESIAN_POINT('Ctrl Pts',(-26.05142082645,14.0676654739834,130.196112404188)) ;
#115777 = CARTESIAN_POINT('Ctrl Pts',(-25.9959721958356,14.2771419928287,
130.000979869832)) ;
#115778 = CARTESIAN_POINT('Ctrl Pts',(-25.9251922030581,14.425031880978,129.761195796767)) ;
#115779 = CARTESIAN_POINT('Ctrl Pts',(-25.8440763649555,14.5017260060049,
129.490996412094)) ;
#115780 = CARTESIAN_POINT('Ctrl Pts',(-25.7603662435499,14.5010099059246,
129.213512691512)) ;
#115781 = CARTESIAN_POINT('Ctrl Pts',(-25.6794136560246,14.4231233705973,
128.943812915352)) ;
#115782 = CARTESIAN_POINT('Ctrl Pts',(-25.6086694413268,14.2735700722065,
128.704038175328)) ;
#115783 = CARTESIAN_POINT('Ctrl Pts',(-25.5536232001884,14.0631260843178,
128.510103402269)) ;
#115784 = CARTESIAN_POINT('Ctrl Pts',(-25.5190005221295,13.8068513237717,
128.37583898455)) ;
#115785 = CARTESIAN_POINT('Ctrl Pts',(-25.5079988886962,13.5229068768556,
128.310556815572)) ;
#115786 = CARTESIAN_POINT('Ctrl Pts',(-25.522136912891,13.2323185296325,128.31877011903)) ;
#115787 = CARTESIAN_POINT('Ctrl Pts',(-25.5609778387885,12.955462422634,128.399168054502)) ;
#115788 = CARTESIAN_POINT('Ctrl Pts',(-25.622981897995,12.7108337306576,128.547046303102)) ;
#115789 = CARTESIAN_POINT('Ctrl Pts',(-25.7035387876594,12.5189036902296,
128.749376462235)) ;
#115790 = CARTESIAN_POINT('Ctrl Pts',(-25.7983973245378,12.3906586207823,
128.993347141695)) ;
#115791 = CARTESIAN_POINT('Ctrl Pts',(-25.9014394205249,12.3366531336248,
129.261165642822)) ;
#115792 = CARTESIAN_POINT('Ctrl Pts',(-26.0053503635526,12.360297772879,129.531671267842)) ;
#115793 = CARTESIAN_POINT('Ctrl Pts',(-26.1046179703446,12.4609988515391,
129.788341417843)) ;
#115794 = CARTESIAN_POINT('Ctrl Pts',(-26.1910706407531,12.6291274638668,
130.0079564874)) ;
#115795 = CARTESIAN_POINT('Ctrl Pts',(-26.2610067862353,12.8555169755094,
130.179031109569)) ;
#115796 = CARTESIAN_POINT('Ctrl Pts',(-26.3090567054831,13.1215885522129,
130.286335393292)) ;
#115797 = CARTESIAN_POINT('Ctrl Pts',(-26.3329796835872,13.4096083938423,
130.323096945283)) ;
#115798 = CARTESIAN_POINT('Ctrl Pts',(-26.3317340747676,13.698212942693,130.286391172774)) ;
#115799 = CARTESIAN_POINT('Ctrl Pts',(-26.3058007346478,13.9691452295141,
130.177299627734)) ;
#115800 = CARTESIAN_POINT('Ctrl Pts',(-26.2583066398341,14.1982918407705,
130.005562251346)) ;
#115801 = CARTESIAN_POINT('Ctrl Pts',(-26.1931751350795,14.3728095621698,
129.782233989023)) ;
#115802 = CARTESIAN_POINT('Ctrl Pts',(-26.1155255616385,14.479662285758,129.522250222093)) ;
#115803 = CARTESIAN_POINT('Ctrl Pts',(-26.0318486038747,14.5107460879228,
129.244664158376)) ;
#115804 = CARTESIAN_POINT('Ctrl Pts',(-25.9488165487381,14.4636147982726,
128.968932999966)) ;
#115805 = CARTESIAN_POINT('Ctrl Pts',(-25.8735146658894,14.3427084720644,
128.715956195703)) ;
#115806 = CARTESIAN_POINT('Ctrl Pts',(-25.811125852612,14.1545214106307,128.500410033898)) ;
#115807 = CARTESIAN_POINT('Ctrl Pts',(-25.767859635489,13.914665784431,128.340908123874)) ;
#115808 = CARTESIAN_POINT('Ctrl Pts',(-25.7470531048229,13.6405172708492,
128.247102795506)) ;
#115809 = CARTESIAN_POINT('Ctrl Pts',(-25.7508957888745,13.3501102818962,
128.225215226321)) ;
#115810 = CARTESIAN_POINT('Ctrl Pts',(-25.7797927372613,13.0651843315454,
128.276561420719)) ;
#115811 = CARTESIAN_POINT('Ctrl Pts',(-25.8330708547357,12.80388772374,128.398847085602)) ;
#115812 = CARTESIAN_POINT('Ctrl Pts',(-25.9063371941856,12.5899465270377,
128.579947959411)) ;
#115813 = CARTESIAN_POINT('Ctrl Pts',(-25.9963126660368,12.4339563210189,
128.809607064104)) ;
#115814 = CARTESIAN_POINT('Ctrl Pts',(-26.0966203558645,12.3491846989202,
129.069534053189)) ;
#115815 = CARTESIAN_POINT('Ctrl Pts',(-26.2015343109458,12.3415474281895,
129.342731765695)) ;
#115816 = CARTESIAN_POINT('Ctrl Pts',(-26.3027211617629,12.4110292201394,
129.60537279447)) ;
#115817 = CARTESIAN_POINT('Ctrl Pts',(-26.3953588574291,12.5533605448057,
129.842803792173)) ;
#115818 = CARTESIAN_POINT('Ctrl Pts',(-26.4724658228993,12.7574391512257,
130.035002583383)) ;
#115819 = CARTESIAN_POINT('Ctrl Pts',(-26.5299060950814,13.0095817126533,
130.169659341123)) ;
#115820 = CARTESIAN_POINT('Ctrl Pts',(-26.5639504532064,13.2928226801242,
130.235818361087)) ;
#115821 = CARTESIAN_POINT('Ctrl Pts',(-26.5727935985865,13.5820119966617,
130.228755567199)) ;
#115822 = CARTESIAN_POINT('Ctrl Pts',(-26.5567072828717,13.8633229249982,
130.148453208055)) ;
#115823 = CARTESIAN_POINT('Ctrl Pts',(-26.5174678494182,14.1112602779132,
130.000718041267)) ;
#115824 = CARTESIAN_POINT('Ctrl Pts',(-26.4589493371831,14.3095521754014,
129.79675027408)) ;
#115825 = CARTESIAN_POINT('Ctrl Pts',(-26.3857504408749,14.4451057235358,
129.549834730436)) ;
#115826 = CARTESIAN_POINT('Ctrl Pts',(-26.3033581527554,14.5076745769451,
129.275854508276)) ;
#115827 = CARTESIAN_POINT('Ctrl Pts',(-26.2193621817028,14.4918702514085,
128.997365975633)) ;
#115828 = CARTESIAN_POINT('Ctrl Pts',(-26.1403227598029,14.4001695900989,
128.733462893607)) ;
#115829 = CARTESIAN_POINT('Ctrl Pts',(-26.0720785017029,14.238339270588,128.500982256028)) ;
#115830 = CARTESIAN_POINT('Ctrl Pts',(-26.0205445494064,14.0178457541506,
128.317291271494)) ;
#115831 = CARTESIAN_POINT('Ctrl Pts',(-25.9901309545097,13.7549024704848,
128.195319458128)) ;
#115832 = CARTESIAN_POINT('Ctrl Pts',(-25.9838907425677,13.4669383655623,
128.143823454231)) ;
#115833 = CARTESIAN_POINT('Ctrl Pts',(-26.002625472959,13.1792878389568,128.165694781332)) ;
#115834 = CARTESIAN_POINT('Ctrl Pts',(-26.0462578585361,12.9054935275296,
128.259864888277)) ;
#115835 = CARTESIAN_POINT('Ctrl Pts',(-26.1117838862911,12.6708451835732,
128.418257412013)) ;
#115836 = CARTESIAN_POINT('Ctrl Pts',(-26.1958394673662,12.4890109361581,
128.630614971608)) ;
#115837 = CARTESIAN_POINT('Ctrl Pts',(-26.292450313642,12.3747427440592,128.879802823841)) ;
#115838 = CARTESIAN_POINT('Ctrl Pts',(-26.3961466629634,12.335118127865,129.149563628382)) ;
#115839 = CARTESIAN_POINT('Ctrl Pts',(-26.4997927945682,12.3735357257966,
129.41921706946)) ;
#115840 = CARTESIAN_POINT('Ctrl Pts',(-26.5970562066531,12.4876827050984,
129.670119063763)) ;
#115841 = CARTESIAN_POINT('Ctrl Pts',(-26.6809623236233,12.668143871092,129.882175659137)) ;
#115842 = CARTESIAN_POINT('Ctrl Pts',(-26.7469567383412,12.9033827829949,
130.041784506141)) ;
#115843 = CARTESIAN_POINT('Ctrl Pts',(-26.7905248136644,13.1743601664502,
130.136070712378)) ;
#115844 = CARTESIAN_POINT('Ctrl Pts',(-26.8098089341939,13.4644840041335,
130.159245371207)) ;
#115845 = CARTESIAN_POINT('Ctrl Pts',(-26.8037407483827,13.7518155739233,
130.108342116625)) ;
#115846 = CARTESIAN_POINT('Ctrl Pts',(-26.7736744947239,14.0147480425275,
129.987433665233)) ;
#115847 = CARTESIAN_POINT('Ctrl Pts',(-26.7224117937105,14.2359322469135,
129.804543108639)) ;
#115848 = CARTESIAN_POINT('Ctrl Pts',(-26.6540459121311,14.3990328419962,
129.571575856472)) ;
#115849 = CARTESIAN_POINT('Ctrl Pts',(-26.5752101350165,14.4913721211862,
129.308326055989)) ;
#115850 = CARTESIAN_POINT('Ctrl Pts',(-26.4908765753451,14.5077030613306,
129.028705274742)) ;
#115851 = CARTESIAN_POINT('Ctrl Pts',(-26.4092296365473,14.4466726935246,
128.757236988289)) ;
#115852 = CARTESIAN_POINT('Ctrl Pts',(-26.3352722351391,14.3110620977678,
128.507833953029)) ;
#115853 = CARTESIAN_POINT('Ctrl Pts',(-26.2766889458892,14.1132680684101,
128.303711145387)) ;
#115854 = CARTESIAN_POINT('Ctrl Pts',(-26.2372639174626,13.8656264960883,
128.15541845975)) ;
#115855 = CARTESIAN_POINT('Ctrl Pts',(-26.2209130537975,13.5853317318957,
128.074439710367)) ;
#115856 = CARTESIAN_POINT('Ctrl Pts',(-26.2296856924358,13.2939513094312,
128.066914197785)) ;
#115857 = CARTESIAN_POINT('Ctrl Pts',(-26.2631798636915,13.0136081090702,
128.131828211089)) ;
#115858 = CARTESIAN_POINT('Ctrl Pts',(-26.3203316415523,12.7604084565328,
128.265584239078)) ;
#115859 = CARTESIAN_POINT('Ctrl Pts',(-26.397246993967,12.5556140537718,128.457218817256)) ;
#115860 = CARTESIAN_POINT('Ctrl Pts',(-26.4898764488098,12.412162783817,128.694571316763)) ;
#115861 = CARTESIAN_POINT('Ctrl Pts',(-26.5911530122536,12.3419224833159,
128.957426665658)) ;
#115862 = CARTESIAN_POINT('Ctrl Pts',(-26.6956543409951,12.3485705631489,
129.229554057824)) ;
#115863 = CARTESIAN_POINT('Ctrl Pts',(-26.7962358912617,12.4325162173742,
129.490217635024)) ;
#115864 = CARTESIAN_POINT('Ctrl Pts',(-26.8862177213639,12.5872706018155,
129.719968083883)) ;
#115865 = CARTESIAN_POINT('Ctrl Pts',(-26.9600298412944,12.8016741765326,
129.902501376654)) ;
#115866 = CARTESIAN_POINT('Ctrl Pts',(-27.0132363984096,13.0608926757193,
130.024793668328)) ;
#115867 = CARTESIAN_POINT('Ctrl Pts',(-27.0426146311277,13.3463627388947,
130.077448217005)) ;
#115868 = CARTESIAN_POINT('Ctrl Pts',(-27.0467658686963,13.6367413735624,
130.056476137218)) ;
#115869 = CARTESIAN_POINT('Ctrl Pts',(-27.0262045189193,13.912123441329,129.96328026669)) ;
#115870 = CARTESIAN_POINT('Ctrl Pts',(-26.9829610646689,14.1528033236638,
129.803766513539)) ;
#115871 = CARTESIAN_POINT('Ctrl Pts',(-26.9212047054132,14.3402810134416,
129.590308052972)) ;
#115872 = CARTESIAN_POINT('Ctrl Pts',(-26.8459513519056,14.4626257099404,
129.33741374041)) ;
#115873 = CARTESIAN_POINT('Ctrl Pts',(-26.7626484303445,14.5106364099982,
129.060769517447)) ;
#115874 = CARTESIAN_POINT('Ctrl Pts',(-26.6793325739832,14.4805445966973,
128.784392296914)) ;
#115875 = CARTESIAN_POINT('Ctrl Pts',(-26.6015120722546,14.3748126779467,
128.523896403084)) ;
#115876 = CARTESIAN_POINT('Ctrl Pts',(-26.5360012381168,14.2005693776624,
128.299367371948)) ;
#115877 = CARTESIAN_POINT('Ctrl Pts',(-26.4882466006821,13.9714224956824,
128.126808943075)) ;
#115878 = CARTESIAN_POINT('Ctrl Pts',(-26.4621696395529,13.7016038456452,
128.017397936684)) ;
#115879 = CARTESIAN_POINT('Ctrl Pts',(-26.4605573044593,13.4137877720204,
127.979694610522)) ;
#115880 = CARTESIAN_POINT('Ctrl Pts',(-26.4842037814474,13.1249621059971,
128.015572519599)) ;
#115881 = CARTESIAN_POINT('Ctrl Pts',(-26.5319266616535,12.858759801946,128.121953585796)) ;
#115882 = CARTESIAN_POINT('Ctrl Pts',(-26.601763218089,12.6311849064932,128.292661018411)) ;
#115883 = CARTESIAN_POINT('Ctrl Pts',(-26.6883690358658,12.4620614418067,
128.512623702752)) ;
#115884 = CARTESIAN_POINT('Ctrl Pts',(-26.7871596601743,12.3611529243014,
128.768034196029)) ;
#115885 = CARTESIAN_POINT('Ctrl Pts',(-26.8908594338048,12.336402737043,129.037980194775)) ;
#115886 = CARTESIAN_POINT('Ctrl Pts',(-26.9942677499415,12.3896954767389,
129.30676634427)) ;
#115887 = CARTESIAN_POINT('Ctrl Pts',(-27.0891228503658,12.5169545730866,
129.550776904504)) ;
#115888 = CARTESIAN_POINT('Ctrl Pts',(-27.170110122641,12.7090014500136,129.754247695197)) ;
#115889 = CARTESIAN_POINT('Ctrl Pts',(-27.2319803579197,12.9518209129291,
129.901923479105)) ;
#115890 = CARTESIAN_POINT('Ctrl Pts',(-27.2712167263555,13.2283911259786,
129.983462395853)) ;
#115891 = CARTESIAN_POINT('Ctrl Pts',(-27.2856848450787,13.5192444476926,
129.992606198651)) ;
#115892 = CARTESIAN_POINT('Ctrl Pts',(-27.2749998341,13.8035929406365,129.928231036212)) ;
#115893 = CARTESIAN_POINT('Ctrl Pts',(-27.2405107086992,14.0607675161601,
129.794281704174)) ;
#115894 = CARTESIAN_POINT('Ctrl Pts',(-27.1859404561386,14.2709776513911,
129.601886944103)) ;
#115895 = CARTESIAN_POINT('Ctrl Pts',(-27.1150473623168,14.4220258151157,
129.36152624086)) ;
#115896 = CARTESIAN_POINT('Ctrl Pts',(-27.0343785010806,14.5004899933202,
129.09274938976)) ;
#115897 = CARTESIAN_POINT('Ctrl Pts',(-26.950535069012,14.5020985766214,128.814815907977)) ;
#115898 = CARTESIAN_POINT('Ctrl Pts',(-26.8695870479016,14.426667623352,128.545218407416)) ;
#115899 = CARTESIAN_POINT('Ctrl Pts',(-26.798211588555,14.2786158189735,128.303482030973)) ;
#115900 = CARTESIAN_POINT('Ctrl Pts',(-26.7426992360049,14.0697690186074,
128.108208750919)) ;
#115901 = CARTESIAN_POINT('Ctrl Pts',(-26.7074412852036,13.8142976320865,
127.972057291302)) ;
#115902 = CARTESIAN_POINT('Ctrl Pts',(-26.6957645215905,13.5318062075926,
127.904912693824)) ;
#115903 = CARTESIAN_POINT('Ctrl Pts',(-26.7091353370237,13.2403761874523,
127.91080130822)) ;
#115904 = CARTESIAN_POINT('Ctrl Pts',(-26.74755505738,12.9618561593774,127.989837070354)) ;
#115905 = CARTESIAN_POINT('Ctrl Pts',(-26.8086943560285,12.7173263730279,
128.135355225743)) ;
#115906 = CARTESIAN_POINT('Ctrl Pts',(-26.8888831517,12.5233446886838,128.33655295725)) ;
#115907 = CARTESIAN_POINT('Ctrl Pts',(-26.9835011120047,12.3931312315505,
128.579802503126)) ;
#115908 = CARTESIAN_POINT('Ctrl Pts',(-27.0865721816442,12.337075246258,128.847656402371)) ;
#115909 = CARTESIAN_POINT('Ctrl Pts',(-27.1901303578273,12.3586764449227,
129.117256451724)) ;
#115910 = CARTESIAN_POINT('Ctrl Pts',(-27.2892091804132,12.4563696314589,
129.373537084527)) ;
#115911 = CARTESIAN_POINT('Ctrl Pts',(-27.3766437558911,12.6234424170359,
129.595825398964)) ;
#115912 = CARTESIAN_POINT('Ctrl Pts',(-27.447072154312,12.8484690314232,129.768349176844)) ;
#115913 = CARTESIAN_POINT('Ctrl Pts',(-27.4958104255805,13.1134860607375,
129.877675494575)) ;
#115914 = CARTESIAN_POINT('Ctrl Pts',(-27.5204851717528,13.402425050447,129.916492772369)) ;
#115915 = CARTESIAN_POINT('Ctrl Pts',(-27.5198611034755,13.6901681944769,
129.881727019293)) ;
#115916 = CARTESIAN_POINT('Ctrl Pts',(-27.4947206170695,13.9614083380647,
129.775024765156)) ;
#115917 = CARTESIAN_POINT('Ctrl Pts',(-27.4477408524357,14.1924050674132,
129.604730002262)) ;
#115918 = CARTESIAN_POINT('Ctrl Pts',(-27.3829916295066,14.3688010159201,
129.382496516221)) ;
#115919 = CARTESIAN_POINT('Ctrl Pts',(-27.305567395489,14.4776662097744,129.123157647789)) ;
#115920 = CARTESIAN_POINT('Ctrl Pts',(-27.2222300887403,14.5108828480259,
128.84666452346)) ;
#115921 = CARTESIAN_POINT('Ctrl Pts',(-27.1390665957671,14.4662997711349,
128.570551673275)) ;
#115922 = CARTESIAN_POINT('Ctrl Pts',(-27.063203525044,14.3468724358185,128.315811999268)) ;
#115923 = CARTESIAN_POINT('Ctrl Pts',(-27.000726116674,14.161614932188,128.10021376119)) ;
#115924 = CARTESIAN_POINT('Ctrl Pts',(-26.9566598775861,13.9230022753498,
127.938326275104)) ;
#115925 = CARTESIAN_POINT('Ctrl Pts',(-26.9350826150652,13.6485314062169,
127.842142219284)) ;
#115926 = CARTESIAN_POINT('Ctrl Pts',(-26.9382141999983,13.3583011743042,
127.818182839235)) ;
#115927 = CARTESIAN_POINT('Ctrl Pts',(-26.9665177873497,13.072504270402,127.867737400507)) ;
#115928 = CARTESIAN_POINT('Ctrl Pts',(-27.0188173523961,12.8117566735177,
127.987365016217)) ;
#115929 = CARTESIAN_POINT('Ctrl Pts',(-27.0915996802834,12.5955171582893,
128.166977325295)) ;
#115930 = CARTESIAN_POINT('Ctrl Pts',(-27.1817271815024,12.4369580568928,
128.396898077135)) ;
#115931 = CARTESIAN_POINT('Ctrl Pts',(-27.2813708056134,12.3507869630092,
128.655042348106)) ;
#115932 = CARTESIAN_POINT('Ctrl Pts',(-27.3857827418417,12.3404899643528,
128.926923079581)) ;
#115933 = CARTESIAN_POINT('Ctrl Pts',(-27.4876541467364,12.4078494476239,
129.191403822402)) ;
#115934 = CARTESIAN_POINT('Ctrl Pts',(-27.5807089481865,12.5483871977687,
129.430029656426)) ;
#115935 = CARTESIAN_POINT('Ctrl Pts',(-27.6584612758746,12.7513533086917,
129.624045981255)) ;
#115936 = CARTESIAN_POINT('Ctrl Pts',(-27.7163134902441,13.001941318222,129.759978308328)) ;
#115937 = CARTESIAN_POINT('Ctrl Pts',(-27.7510006841768,13.2828868274063,
129.828206089058)) ;
#115938 = CARTESIAN_POINT('Ctrl Pts',(-27.7607078220157,13.5743278631276,
129.823412590067)) ;
#115939 = CARTESIAN_POINT('Ctrl Pts',(-27.7452570064132,13.8554587804339,
129.745052642731)) ;
#115940 = CARTESIAN_POINT('Ctrl Pts',(-27.7068857846591,14.103739100914,129.599981463497)) ;
#115941 = CARTESIAN_POINT('Ctrl Pts',(-27.6487231943859,14.3046990175591,
129.396931127844)) ;
#115942 = CARTESIAN_POINT('Ctrl Pts',(-27.5755356695319,14.4424188711516,
129.149922663509)) ;
#115943 = CARTESIAN_POINT('Ctrl Pts',(-27.4939933548379,14.5067209234145,
128.878704097542)) ;
#115944 = CARTESIAN_POINT('Ctrl Pts',(-27.4097527588653,14.4936392684735,
128.599416389571)) ;
#115945 = CARTESIAN_POINT('Ctrl Pts',(-27.3303082230943,14.404006740505,128.334269093954)) ;
#115946 = CARTESIAN_POINT('Ctrl Pts',(-27.2614819305869,14.2433942656814,
128.099980444704)) ;
#115947 = CARTESIAN_POINT('Ctrl Pts',(-27.2096136486434,14.0252993056693,
127.915456300396)) ;
#115948 = CARTESIAN_POINT('Ctrl Pts',(-27.178469556164,13.7626963119846,127.791262873367)) ;
#115949 = CARTESIAN_POINT('Ctrl Pts',(-27.1714738989522,13.4766513624265,
127.737736625053)) ;
#115950 = CARTESIAN_POINT('Ctrl Pts',(-27.1895561727833,13.1866966293381,
127.757460183878)) ;
#115951 = CARTESIAN_POINT('Ctrl Pts',(-27.2326135994264,12.9123106961637,
127.849963433579)) ;
#115952 = CARTESIAN_POINT('Ctrl Pts',(-27.2974441217088,12.6769408805555,
128.006390666055)) ;
#115953 = CARTESIAN_POINT('Ctrl Pts',(-27.3808130116155,12.4935889535621,
128.216818650803)) ;
#115954 = CARTESIAN_POINT('Ctrl Pts',(-27.4776575476475,12.3766908568814,
128.466511171481)) ;
#115955 = CARTESIAN_POINT('Ctrl Pts',(-27.5810443505466,12.3352383862452,
128.735442117728)) ;
#115956 = CARTESIAN_POINT('Ctrl Pts',(-27.6845420847214,12.3713736006973,
129.004732437811)) ;
#115957 = CARTESIAN_POINT('Ctrl Pts',(-27.7818596677854,12.4827590293817,
129.255891826048)) ;
#115958 = CARTESIAN_POINT('Ctrl Pts',(-27.8667979944307,12.6627224306716,
129.47073002161)) ;
#115959 = CARTESIAN_POINT('Ctrl Pts',(-27.9330076414952,12.8955397849013,
129.631137908056)) ;
#115960 = CARTESIAN_POINT('Ctrl Pts',(-27.9774352268445,13.1663558963296,
129.72784335586)) ;
#115961 = CARTESIAN_POINT('Ctrl Pts',(-27.9973849513202,13.4563321062043,
129.752958193208)) ;
#115962 = CARTESIAN_POINT('Ctrl Pts',(-27.9920646322741,13.74354179735,129.704297361198)) ;
#115963 = CARTESIAN_POINT('Ctrl Pts',(-27.9626165416411,14.007863745204,129.585142101985)) ;
#115964 = CARTESIAN_POINT('Ctrl Pts',(-27.9119828992553,14.2299792391956,
129.404152786278)) ;
#115965 = CARTESIAN_POINT('Ctrl Pts',(-27.844287943155,14.3948659481182,129.173238937185)) ;
#115966 = CARTESIAN_POINT('Ctrl Pts',(-27.7651604606475,14.4898740802148,
128.908913740689)) ;
#115967 = CARTESIAN_POINT('Ctrl Pts',(-27.681397890891,14.5084149248409,128.631178035807)) ;
#115968 = CARTESIAN_POINT('Ctrl Pts',(-27.5990872491488,14.4492459338564,
128.357554758999)) ;
#115969 = CARTESIAN_POINT('Ctrl Pts',(-27.5253256223266,14.316609488643,128.108970615685)) ;
#115970 = CARTESIAN_POINT('Ctrl Pts',(-27.4659033295799,14.1198900556279,
127.9022461303)) ;
#115971 = CARTESIAN_POINT('Ctrl Pts',(-27.42591393932,13.8734079349303,127.752317228327)) ;
#115972 = CARTESIAN_POINT('Ctrl Pts',(-27.408865491139,13.5947694158123,127.669409669264)) ;
#115973 = CARTESIAN_POINT('Ctrl Pts',(-27.4167455300075,13.3033325180628,
127.659268253717)) ;
#115974 = CARTESIAN_POINT('Ctrl Pts',(-27.4497732461264,13.0207084742087,
127.722612022269)) ;
#115975 = CARTESIAN_POINT('Ctrl Pts',(-27.5060414733426,12.767628690545,127.853947272495)) ;
#115976 = CARTESIAN_POINT('Ctrl Pts',(-27.5826500146593,12.5604751539345,
128.044576460787)) ;
#115977 = CARTESIAN_POINT('Ctrl Pts',(-27.6748867687302,12.4152916729436,
128.280805111389)) ;
#115978 = CARTESIAN_POINT('Ctrl Pts',(-27.7760048062591,12.3428120631862,
128.543188432493)) ;
#115979 = CARTESIAN_POINT('Ctrl Pts',(-27.880802690774,12.3473797413046,128.816094258677)) ;
#115980 = CARTESIAN_POINT('Ctrl Pts',(-27.9814814316689,12.4294695368143,
129.077065134186)) ;
#115981 = CARTESIAN_POINT('Ctrl Pts',(-28.0714598999934,12.5816148375682,
129.306949475753)) ;
#115982 = CARTESIAN_POINT('Ctrl Pts',(-28.1460628162166,12.7949907280796,
129.491697351825)) ;
#115983 = CARTESIAN_POINT('Ctrl Pts',(-28.1999915303535,13.054101177031,129.616001192498)) ;
#115984 = CARTESIAN_POINT('Ctrl Pts',(-28.2299138854955,13.3386274126212,
129.670307692816)) ;
#115985 = CARTESIAN_POINT('Ctrl Pts',(-28.2347775216737,13.6281884734652,
129.651524250556)) ;
#115986 = CARTESIAN_POINT('Ctrl Pts',(-28.2149512862949,13.9042249218154,
129.560485972219)) ;
#115987 = CARTESIAN_POINT('Ctrl Pts',(-28.1723564864184,14.1463903457502,
129.402858889307)) ;
#115988 = CARTESIAN_POINT('Ctrl Pts',(-28.1106708276455,14.3364819716926,
129.189416939951)) ;
#115989 = CARTESIAN_POINT('Ctrl Pts',(-28.0360880693673,14.4598817702337,
128.938660433378)) ;
#115990 = CARTESIAN_POINT('Ctrl Pts',(-27.953057765994,14.5104486170863,128.662863635966)) ;
#115991 = CARTESIAN_POINT('Ctrl Pts',(-27.8692045369708,14.4822486369166,
128.384729130641)) ;
#115992 = CARTESIAN_POINT('Ctrl Pts',(-27.791608538637,14.3791733041028,128.125092916574)) ;
#115993 = CARTESIAN_POINT('Ctrl Pts',(-27.7253583208721,14.2063740303146,
127.898282623416)) ;
#115994 = CARTESIAN_POINT('Ctrl Pts',(-27.6770395587882,13.9777765864427,
127.723995413382)) ;
#115995 = CARTESIAN_POINT('Ctrl Pts',(-27.6504229397667,13.7109259499415,
127.613260324166)) ;
#115996 = CARTESIAN_POINT('Ctrl Pts',(-27.6480583043497,13.4211174151953,
127.573090826099)) ;
#115997 = CARTESIAN_POINT('Ctrl Pts',(-27.6709154004622,13.1336909339448,
127.606862509643)) ;
#115998 = CARTESIAN_POINT('Ctrl Pts',(-27.7180057890291,12.8658812639418,
127.711313356748)) ;
#115999 = CARTESIAN_POINT('Ctrl Pts',(-27.7873482366324,12.6367690190525,
127.880557040248)) ;
#116000 = CARTESIAN_POINT('Ctrl Pts',(-27.8736342999947,12.4658337897599,
128.099554794345)) ;
#116001 = CARTESIAN_POINT('Ctrl Pts',(-27.9718311891268,12.3631245211514,
128.353345809671)) ;
#116002 = CARTESIAN_POINT('Ctrl Pts',(-28.0756846325717,12.3360466241608,
128.623667434511)) ;
#116003 = CARTESIAN_POINT('Ctrl Pts',(-28.1788526517052,12.3868688002356,
128.891874367728)) ;
#116004 = CARTESIAN_POINT('Ctrl Pts',(-28.2741388501772,12.5119418325269,
129.137115030646)) ;
#116005 = CARTESIAN_POINT('Ctrl Pts',(-28.3556708751438,12.7021783709845,
129.342171425122)) ;
#116006 = CARTESIAN_POINT('Ctrl Pts',(-28.4184699311589,12.9449353770794,
129.492398354652)) ;
#116007 = CARTESIAN_POINT('Ctrl Pts',(-28.4583084084869,13.2214383784226,
129.575638041553)) ;
#116008 = CARTESIAN_POINT('Ctrl Pts',(-28.4734122859081,13.5108147708277,
129.586797648768)) ;
#116009 = CARTESIAN_POINT('Ctrl Pts',(-28.4633457731125,13.7968084175674,
129.524085701258)) ;
#116010 = CARTESIAN_POINT('Ctrl Pts',(-28.4296187997626,14.0536576083437,
129.392533959943)) ;
#116011 = CARTESIAN_POINT('Ctrl Pts',(-28.3754911658076,14.2659120564335,
129.201360310375)) ;
#116012 = CARTESIAN_POINT('Ctrl Pts',(-28.3050821824441,14.4185012516542,
128.962475031458)) ;
#116013 = CARTESIAN_POINT('Ctrl Pts',(-28.2247264730961,14.4992712221482,
128.694649965742)) ;
#116014 = CARTESIAN_POINT('Ctrl Pts',(-28.1405276912772,14.5031360116066,
128.415538484686)) ;
#116015 = CARTESIAN_POINT('Ctrl Pts',(-28.059513753469,14.4296202074177,128.145783486771)) ;
#116016 = CARTESIAN_POINT('Ctrl Pts',(-27.9880766403289,14.2844131247839,
127.904026806799)) ;
#116017 = CARTESIAN_POINT('Ctrl Pts',(-27.9318057397691,14.0764755685082,
127.706412345186)) ;
#116018 = CARTESIAN_POINT('Ctrl Pts',(-27.8959845576815,13.8227947339683,
127.568706785711)) ;
#116019 = CARTESIAN_POINT('Ctrl Pts',(-27.8835201350609,13.5398702989391,
127.499142873583)) ;
#116020 = CARTESIAN_POINT('Ctrl Pts',(-27.8962033555758,13.2487717783427,
127.50306914783)) ;
#116021 = CARTESIAN_POINT('Ctrl Pts',(-27.9337544855272,12.9703362151756,
127.579661290793)) ;
#116022 = CARTESIAN_POINT('Ctrl Pts',(-27.9942820451289,12.7241092781338,
127.723348072863)) ;
#116023 = CARTESIAN_POINT('Ctrl Pts',(-28.0741961867263,12.5279171433205,
127.923656462501)) ;
#116024 = CARTESIAN_POINT('Ctrl Pts',(-28.1684346295129,12.3959938665945,
128.165822555878)) ;
#116025 = CARTESIAN_POINT('Ctrl Pts',(-28.2708930006534,12.3376260980812,
128.432033363079)) ;
#116026 = CARTESIAN_POINT('Ctrl Pts',(-28.3752372703154,12.3570497794023,
128.703694565037)) ;
#116027 = CARTESIAN_POINT('Ctrl Pts',(-28.474218780803,12.4525559733436,128.959799081295)) ;
#116028 = CARTESIAN_POINT('Ctrl Pts',(-28.5620645646479,12.6176036105847,
129.183295489253)) ;
#116029 = CARTESIAN_POINT('Ctrl Pts',(-28.6330705369593,12.8410947019102,
129.357514549927)) ;
#116030 = CARTESIAN_POINT('Ctrl Pts',(-28.6825047729054,13.1055203518464,
129.468831178845)) ;
#116031 = CARTESIAN_POINT('Ctrl Pts',(-28.7078791143123,13.3928980327512,
129.509831198009)) ;
#116032 = CARTESIAN_POINT('Ctrl Pts',(-28.7080000857972,13.6824543649216,
129.477058491295)) ;
#116033 = CARTESIAN_POINT('Ctrl Pts',(-28.6836462060832,13.9532692757644,
129.372812982897)) ;
#116034 = CARTESIAN_POINT('Ctrl Pts',(-28.637210824604,14.1862511235797,129.204032177995)) ;
#116035 = CARTESIAN_POINT('Ctrl Pts',(-28.5729983268859,14.3643962082537,
128.983404490918)) ;
#116036 = CARTESIAN_POINT('Ctrl Pts',(-28.4953888433576,14.4759024807437,
128.723329064892)) ;
#116037 = CARTESIAN_POINT('Ctrl Pts',(-28.4124155755593,14.5109062464403,
128.448017144722)) ;
#116038 = CARTESIAN_POINT('Ctrl Pts',(-28.3292183756258,14.4687351628052,
128.171836440681)) ;
#116039 = CARTESIAN_POINT('Ctrl Pts',(-28.2530232843449,14.351243796897,127.916105712843)) ;
#116040 = CARTESIAN_POINT('Ctrl Pts',(-28.19012029587,14.1681343550178,127.699312985571)) ;
#116041 = CARTESIAN_POINT('Ctrl Pts',(-28.1452447510838,13.9291093552066,
127.534840373785)) ;
#116042 = CARTESIAN_POINT('Ctrl Pts',(-28.123183101824,13.6572015399983,127.437471920795)) ;
#116043 = CARTESIAN_POINT('Ctrl Pts',(-28.1255814706017,13.3659146668707,
127.411223933066)) ;
#116044 = CARTESIAN_POINT('Ctrl Pts',(-28.1531210645832,13.0809591455927,
127.458689441797)) ;
#116045 = CARTESIAN_POINT('Ctrl Pts',(-28.2046620168687,12.8188859308948,
127.576087509683)) ;
#116046 = CARTESIAN_POINT('Ctrl Pts',(-28.277541817743,12.5999510440463,127.755745614815)) ;
#116047 = CARTESIAN_POINT('Ctrl Pts',(-28.3661476402695,12.4414984825018,
127.981641389139)) ;
#116048 = CARTESIAN_POINT('Ctrl Pts',(-28.4661327647063,12.3520343108791,
128.240572616874)) ;
#116049 = CARTESIAN_POINT('Ctrl Pts',(-28.5708059444941,12.3398054622105,
128.513131254719)) ;
#116050 = CARTESIAN_POINT('Ctrl Pts',(-28.6724777538977,12.4047865271677,
128.777144444355)) ;
#116051 = CARTESIAN_POINT('Ctrl Pts',(-28.7659001413954,12.5431933869583,
129.016844456436)) ;
#116052 = CARTESIAN_POINT('Ctrl Pts',(-28.8442058560459,12.7444965603529,
129.212472342267)) ;
#116053 = CARTESIAN_POINT('Ctrl Pts',(-28.9027924661007,12.9945025224571,
129.350476244749)) ;
#116054 = CARTESIAN_POINT('Ctrl Pts',(-28.9381575691283,13.2745329094811,
129.420727068277)) ;
#116055 = CARTESIAN_POINT('Ctrl Pts',(-28.9485234575593,13.5670626370277,
129.417726861736)) ;
#116056 = CARTESIAN_POINT('Ctrl Pts',(-28.933960447473,13.8462370772247,129.342272430857)) ;
#116057 = CARTESIAN_POINT('Ctrl Pts',(-28.8959789907869,14.0979241250953,
129.198057982517)) ;
#116058 = CARTESIAN_POINT('Ctrl Pts',(-28.838332105253,14.2997383418867,128.996585250886)) ;
#116059 = CARTESIAN_POINT('Ctrl Pts',(-28.7657725957652,14.4393312193764,
128.7515156292)) ;
#116060 = CARTESIAN_POINT('Ctrl Pts',(-28.6837573347161,14.5060643569228,
128.478659684657)) ;
#116061 = CARTESIAN_POINT('Ctrl Pts',(-28.6001080114847,14.4951758782706,
128.201352828122)) ;
#116062 = CARTESIAN_POINT('Ctrl Pts',(-28.5200653111137,14.4072623281432,
127.934287968157)) ;
#116063 = CARTESIAN_POINT('Ctrl Pts',(-28.4511978062007,14.2495039694875,
127.70007480226)) ;
#116064 = CARTESIAN_POINT('Ctrl Pts',(-28.3983753819167,14.0308221258824,
127.512458103752)) ;
#116065 = CARTESIAN_POINT('Ctrl Pts',(-28.3669487720982,13.7719100664948,
127.38779922883)) ;
#116066 = CARTESIAN_POINT('Ctrl Pts',(-28.3590881011533,13.4847456450531,
127.331550611793)) ;
#116067 = CARTESIAN_POINT('Ctrl Pts',(-28.3764285791946,13.1955425031336,
127.349219523261)) ;
#116068 = CARTESIAN_POINT('Ctrl Pts',(-28.4187558984065,12.9200552968874,
127.439556443674)) ;
#116069 = CARTESIAN_POINT('Ctrl Pts',(-28.4830536897966,12.6831184385928,
127.594396583248)) ;
#116070 = CARTESIAN_POINT('Ctrl Pts',(-28.5659931747335,12.4980281206389,
127.803559634745)) ;
#116071 = CARTESIAN_POINT('Ctrl Pts',(-28.6623364928729,12.3791543430107,
128.051854714151)) ;
#116072 = CARTESIAN_POINT('Ctrl Pts',(-28.7659162180442,12.3353503717386,
128.321248640665)) ;
#116073 = CARTESIAN_POINT('Ctrl Pts',(-28.869394759317,12.3691099621928,128.590526992868)) ;
#116074 = CARTESIAN_POINT('Ctrl Pts',(-28.9675502196224,12.4795856785055,
128.843913403417)) ;
#116075 = CARTESIAN_POINT('Ctrl Pts',(-29.0518027446978,12.6553361009926,
129.057199931773)) ;
#116076 = CARTESIAN_POINT('Ctrl Pts',(-29.1192464163454,12.8882259217544,
129.220954123798)) ;
#116077 = CARTESIAN_POINT('Ctrl Pts',(-29.1642643498932,13.1581921393272,
129.319406321897)) ;
#116078 = CARTESIAN_POINT('Ctrl Pts',(-29.1849604313943,13.4482190387101,
129.34666282445)) ;
#116079 = CARTESIAN_POINT('Ctrl Pts',(-29.1803518618151,13.7352663202425,
129.300143313471)) ;
#116080 = CARTESIAN_POINT('Ctrl Pts',(-29.1516048942262,14.0004787425337,
129.183043232165)) ;
#116081 = CARTESIAN_POINT('Ctrl Pts',(-29.1015568370635,14.2242401467777,
129.003757674716)) ;
#116082 = CARTESIAN_POINT('Ctrl Pts',(-29.0339430184054,14.391486003047,128.772934980117)) ;
#116083 = CARTESIAN_POINT('Ctrl Pts',(-28.955492652777,14.4880341837757,128.510778479589)) ;
#116084 = CARTESIAN_POINT('Ctrl Pts',(-28.8714600975796,14.5089767222778,
128.232121389573)) ;
#116085 = CARTESIAN_POINT('Ctrl Pts',(-28.7892529362311,14.4520807364783,
127.958902917957)) ;
#116086 = CARTESIAN_POINT('Ctrl Pts',(-28.7150523793816,14.3213934969356,
127.708991446956)) ;
#116087 = CARTESIAN_POINT('Ctrl Pts',(-28.6551735760367,14.126427628205,127.500952233118)) ;
#116088 = CARTESIAN_POINT('Ctrl Pts',(-28.6144873955634,13.8807880817665,
127.348935930026)) ;
#116089 = CARTESIAN_POINT('Ctrl Pts',(-28.5968038371001,13.6022566506269,
127.264117077343)) ;
#116090 = CARTESIAN_POINT('Ctrl Pts',(-28.6039330637587,13.3123739575692,
127.251951536785)) ;
#116091 = CARTESIAN_POINT('Ctrl Pts',(-28.6361660227389,13.0290004002489,
127.312956120869)) ;
#116092 = CARTESIAN_POINT('Ctrl Pts',(-28.6919510174919,12.7741270713226,
127.442792020744)) ;
#116093 = CARTESIAN_POINT('Ctrl Pts',(-28.7679989254335,12.5657352250487,
127.631815876347)) ;
#116094 = CARTESIAN_POINT('Ctrl Pts',(-28.8594997341221,12.4188762117679,
127.866013266875)) ;
#116095 = CARTESIAN_POINT('Ctrl Pts',(-28.9608147014607,12.3438128452305,
128.128841957193)) ;
#116096 = CARTESIAN_POINT('Ctrl Pts',(-29.0652267516056,12.3461025205116,
128.400746493264)) ;
#116097 = CARTESIAN_POINT('Ctrl Pts',(-29.1661640470906,12.4255735874937,
128.662467769584)) ;
#116098 = CARTESIAN_POINT('Ctrl Pts',(-29.2569746802431,12.5765456735502,
128.894620530997)) ;
#116099 = CARTESIAN_POINT('Ctrl Pts',(-29.3318567873601,12.7879286592572,
129.080274286269)) ;
#116100 = CARTESIAN_POINT('Ctrl Pts',(-29.3863322538626,13.0448054046113,
129.206302436344)) ;
#116101 = CARTESIAN_POINT('Ctrl Pts',(-29.4171885363179,13.329756321322,129.26322288733)) ;
#116102 = CARTESIAN_POINT('Ctrl Pts',(-29.4227776954555,13.6201107178654,
129.246484513251)) ;
#116103 = CARTESIAN_POINT('Ctrl Pts',(-29.4036112081965,13.8967554382586,
129.157379684264)) ;
#116104 = CARTESIAN_POINT('Ctrl Pts',(-29.3617661068054,14.1394983367384,
129.002038511481)) ;
#116105 = CARTESIAN_POINT('Ctrl Pts',(-29.3006432267773,14.3315001569242,
128.790247960104)) ;
#116106 = CARTESIAN_POINT('Ctrl Pts',(-29.2260808954585,14.4575222943013,
128.539420298087)) ;
#116107 = CARTESIAN_POINT('Ctrl Pts',(-29.1430912249785,14.5099977938908,
128.263711456409)) ;
#116108 = CARTESIAN_POINT('Ctrl Pts',(-29.0596283023754,14.4843800867397,
127.986903750172)) ;
#116109 = CARTESIAN_POINT('Ctrl Pts',(-28.9813399566608,14.3828781461486,
127.725057189875)) ;
#116110 = CARTESIAN_POINT('Ctrl Pts',(-28.9150542416882,14.212816168216,127.498335145429)) ;
#116111 = CARTESIAN_POINT('Ctrl Pts',(-28.8659433323491,13.9854781681749,
127.321666885816)) ;
#116112 = CARTESIAN_POINT('Ctrl Pts',(-28.8385949971052,13.7179644909653,
127.2086184725)) ;
#116113 = CARTESIAN_POINT('Ctrl Pts',(-28.835583635112,13.4301920376034,127.166758116441)) ;
#116114 = CARTESIAN_POINT('Ctrl Pts',(-28.8575789748189,13.1421055633853,
127.197981715462)) ;
#116115 = CARTESIAN_POINT('Ctrl Pts',(-28.9045188244626,12.87150128464,127.301728733917)) ;
#116116 = CARTESIAN_POINT('Ctrl Pts',(-28.9725684665303,12.6436097991943,
127.46756519262)) ;
#116117 = CARTESIAN_POINT('Ctrl Pts',(-29.0586604842472,12.4698498437503,
127.68586545448)) ;
#116118 = CARTESIAN_POINT('Ctrl Pts',(-29.1565931939368,12.3651221856613,
127.938894371706)) ;
#116119 = CARTESIAN_POINT('Ctrl Pts',(-29.2604850351592,12.335692224637,128.209290972507)) ;
#116120 = CARTESIAN_POINT('Ctrl Pts',(-29.3638355952977,12.3844432071478,
128.478011145159)) ;
#116121 = CARTESIAN_POINT('Ctrl Pts',(-29.4592358664342,12.5072147901112,
128.723652752499)) ;
#116122 = CARTESIAN_POINT('Ctrl Pts',(-29.5413221888135,12.6957550150873,
128.930308953615)) ;
#116123 = CARTESIAN_POINT('Ctrl Pts',(-29.6047036187767,12.9372999479051,
129.082233550744)) ;
#116124 = CARTESIAN_POINT('Ctrl Pts',(-29.6452182047899,13.2121499543988,
129.167553115)) ;
#116125 = CARTESIAN_POINT('Ctrl Pts',(-29.6611042764023,13.5032465104466,
129.180780924663)) ;
#116126 = CARTESIAN_POINT('Ctrl Pts',(-29.6518819161121,13.7871080328991,
129.120848156331)) ;
#116127 = CARTESIAN_POINT('Ctrl Pts',(-29.6187108954398,14.0469104745439,
128.990694231868)) ;
#116128 = CARTESIAN_POINT('Ctrl Pts',(-29.5650955851099,14.2605649124229,
128.801033137001)) ;
#116129 = CARTESIAN_POINT('Ctrl Pts',(-29.494870755953,14.4153649488043,128.562594916595)) ;
#116130 = CARTESIAN_POINT('Ctrl Pts',(-29.4150387131859,14.4978582783663,
128.296438099207)) ;
#116131 = CARTESIAN_POINT('Ctrl Pts',(-29.3308499416307,14.5041773990225,
128.017349602118)) ;
#116132 = CARTESIAN_POINT('Ctrl Pts',(-29.2496148451093,14.4329779197685,
127.746941843894)) ;
#116133 = CARTESIAN_POINT('Ctrl Pts',(-29.1775262666222,14.2890422314917,
127.503142142852)) ;
#116134 = CARTESIAN_POINT('Ctrl Pts',(-29.1208969337368,14.082779433517,127.304531079944)) ;
#116135 = CARTESIAN_POINT('Ctrl Pts',(-29.0845225826136,13.8309337098099,
127.165299579887)) ;
#116136 = CARTESIAN_POINT('Ctrl Pts',(-29.0713186329842,13.5483120187831,
127.093542785031)) ;
#116137 = CARTESIAN_POINT('Ctrl Pts',(-29.083229857648,13.2574777531019,127.095253063998)) ;
#116138 = CARTESIAN_POINT('Ctrl Pts',(-29.1201441678816,12.9779697529959,
127.169929814834)) ;
#116139 = CARTESIAN_POINT('Ctrl Pts',(-29.1798340071233,12.7311580251373,
127.311268080156)) ;
#116140 = CARTESIAN_POINT('Ctrl Pts',(-29.259615046753,12.5323980592304,127.511032300878)) ;
#116141 = CARTESIAN_POINT('Ctrl Pts',(-29.3531954363121,12.3989897288854,
127.751398360947)) ;
#116142 = CARTESIAN_POINT('Ctrl Pts',(-29.4557047728638,12.3382487603058,
128.017686516644)) ;
#116143 = CARTESIAN_POINT('Ctrl Pts',(-29.5597398015999,12.3552058083452,
128.288561847953)) ;
#116144 = CARTESIAN_POINT('Ctrl Pts',(-29.6596151268484,12.4490680703867,
128.547063275398)) ;
#116145 = CARTESIAN_POINT('Ctrl Pts',(-29.747823539621,12.612854304799,128.771597225379)) ;
#116146 = CARTESIAN_POINT('Ctrl Pts',(-29.8189230473542,12.8333918295054,
128.946308444558)) ;
#116147 = CARTESIAN_POINT('Ctrl Pts',(-29.8692193933531,13.0975419155814,
129.060046052025)) ;
#116148 = CARTESIAN_POINT('Ctrl Pts',(-29.8952825556904,13.3843701567211,
129.103082744144)) ;
#116149 = CARTESIAN_POINT('Ctrl Pts',(-29.8961296754756,13.6749248626015,
129.072344167559)) ;
#116150 = CARTESIAN_POINT('Ctrl Pts',(-29.872352875635,13.9463602578246,128.969789222471)) ;
#116151 = CARTESIAN_POINT('Ctrl Pts',(-29.8267467901644,14.1798324379302,
128.803574285622)) ;
#116152 = CARTESIAN_POINT('Ctrl Pts',(-29.762567848699,14.3606302769089,128.582842462436)) ;
#116153 = CARTESIAN_POINT('Ctrl Pts',(-29.6859295100925,14.4733618864566,
128.325903972762)) ;
#116154 = CARTESIAN_POINT('Ctrl Pts',(-29.6022723165312,14.5110756600993,
128.048275924638)) ;
#116155 = CARTESIAN_POINT('Ctrl Pts',(-29.5194444158079,14.4709889009811,
127.773361424165)) ;
#116156 = CARTESIAN_POINT('Ctrl Pts',(-29.4427850873383,14.3556941984043,
127.516218240476)) ;
#116157 = CARTESIAN_POINT('Ctrl Pts',(-29.379260435332,14.1731666486328,127.297467610204)) ;
#116158 = CARTESIAN_POINT('Ctrl Pts',(-29.3342254132114,13.9378584167298,
127.132862710005)) ;
#116159 = CARTESIAN_POINT('Ctrl Pts',(-29.3112446912435,13.6656355311939,
127.03265253494)) ;
#116160 = CARTESIAN_POINT('Ctrl Pts',(-29.3129312287784,13.3744563081115,
127.004322113587)) ;
#116161 = CARTESIAN_POINT('Ctrl Pts',(-29.3398177129572,13.0885611803192,
127.049815834232)) ;
#116162 = CARTESIAN_POINT('Ctrl Pts',(-29.3906009924672,12.8263306498725,
127.165093753781)) ;
#116163 = CARTESIAN_POINT('Ctrl Pts',(-29.4625594349018,12.6063807769631,
127.342179164998)) ;
#116164 = CARTESIAN_POINT('Ctrl Pts',(-29.5513814104012,12.4447492933123,
127.568465791526)) ;
#116165 = CARTESIAN_POINT('Ctrl Pts',(-29.6511504516607,12.3535025882306,
127.826777567947)) ;
#116166 = CARTESIAN_POINT('Ctrl Pts',(-29.7556083087904,12.3391045054194,
128.098761532225)) ;
#116167 = CARTESIAN_POINT('Ctrl Pts',(-29.8574615889439,12.4018104241151,
128.363303066571)) ;
#116168 = CARTESIAN_POINT('Ctrl Pts',(-29.9515240336887,12.5389586489687,
128.604752086664)) ;
#116169 = CARTESIAN_POINT('Ctrl Pts',(-30.0298895040687,12.7377764458565,
128.800721216607)) ;
#116170 = CARTESIAN_POINT('Ctrl Pts',(-30.0891318078393,12.9863019722805,
128.940662639121)) ;
#116171 = CARTESIAN_POINT('Ctrl Pts',(-30.1252471064463,13.2660338630659,
129.013066477495)) ;
#116172 = CARTESIAN_POINT('Ctrl Pts',(-30.1363860269831,13.5582232268191,
129.012365283493)) ;
#116173 = CARTESIAN_POINT('Ctrl Pts',(-30.1224573425596,13.8387404070693,
128.9386660175)) ;
#116174 = CARTESIAN_POINT('Ctrl Pts',(-30.0853429984546,14.0904925183414,
128.797147021732)) ;
#116175 = CARTESIAN_POINT('Ctrl Pts',(-30.0277590711992,14.2955136011611,
128.595595560232)) ;
#116176 = CARTESIAN_POINT('Ctrl Pts',(-29.9558778598522,14.4360006812449,
128.352686763533)) ;
#116177 = CARTESIAN_POINT('Ctrl Pts',(-29.8742567679805,14.5051702931602,
128.081056456965)) ;
#116178 = CARTESIAN_POINT('Ctrl Pts',(-29.7902969630137,14.4966323764384,
127.802731519334)) ;
#116179 = CARTESIAN_POINT('Ctrl Pts',(-29.7100123387406,14.4108291399258,
127.534953213959)) ;
#116180 = CARTESIAN_POINT('Ctrl Pts',(-29.6407380446541,14.2547209501546,
127.299525468516)) ;
#116181 = CARTESIAN_POINT('Ctrl Pts',(-29.5875888674703,14.0388606089928,
127.111132269111)) ;
#116182 = CARTESIAN_POINT('Ctrl Pts',(-29.5552494813085,13.779405578044,126.983595808789)) ;
#116183 = CARTESIAN_POINT('Ctrl Pts',(-29.5467692399988,13.4926641580088,
126.925547219345)) ;
#116184 = CARTESIAN_POINT('Ctrl Pts',(-29.5633816541989,13.2038302112353,
126.941144586643)) ;
#116185 = CARTESIAN_POINT('Ctrl Pts',(-29.6048714410533,12.9280759931688,
127.02910382322)) ;
#116186 = CARTESIAN_POINT('Ctrl Pts',(-29.6688506403303,12.6887447492448,
127.182864366148)) ;
#116187 = CARTESIAN_POINT('Ctrl Pts',(-29.7513587249347,12.5022966343227,
127.39078364992)) ;
#116188 = CARTESIAN_POINT('Ctrl Pts',(-29.8469802454942,12.381763978882,127.637108683278)) ;
#116189 = CARTESIAN_POINT('Ctrl Pts',(-29.9508020024135,12.3354318114705,
127.907094928409)) ;
#116190 = CARTESIAN_POINT('Ctrl Pts',(-30.0541803012317,12.3672035513488,
128.176131637916)) ;
#116191 = CARTESIAN_POINT('Ctrl Pts',(-30.1521106585629,12.474426481286,128.429055203006)) ;
#116192 = CARTESIAN_POINT('Ctrl Pts',(-30.2377865470727,12.6503068829769,
128.646124078682)) ;
#116193 = CARTESIAN_POINT('Ctrl Pts',(-30.3053907898611,12.8812481424524,
128.810483543534)) ;
#116194 = CARTESIAN_POINT('Ctrl Pts',(-30.3510328505262,13.1494231082653,
128.910858646302)) ;
#116195 = CARTESIAN_POINT('Ctrl Pts',(-30.3725424728725,13.4405328283774,
128.94033906329)) ;
#116196 = CARTESIAN_POINT('Ctrl Pts',(-30.3685945252647,13.7272524095848,
128.895825068985)) ;
#116197 = CARTESIAN_POINT('Ctrl Pts',(-30.3405359677795,13.9933197786215,
128.780743464257)) ;
#116198 = CARTESIAN_POINT('Ctrl Pts',(-30.2910888155488,14.2183989061991,
128.603235194175)) ;
#116199 = CARTESIAN_POINT('Ctrl Pts',(-30.2238484293931,14.3876287517767,
128.373477627282)) ;
#116200 = CARTESIAN_POINT('Ctrl Pts',(-30.1457515284424,14.4861870970875,
128.112398717919)) ;
#116201 = CARTESIAN_POINT('Ctrl Pts',(-30.0617136501863,14.5095212297327,
127.833700802789)) ;
#116202 = CARTESIAN_POINT('Ctrl Pts',(-29.9792786676799,14.4547287275128,
127.559780909732)) ;
#116203 = CARTESIAN_POINT('Ctrl Pts',(-29.9048009680584,14.3261105544631,
127.309079981945)) ;
#116204 = CARTESIAN_POINT('Ctrl Pts',(-29.844419395189,14.1327425032557,127.099559452458)) ;
#116205 = CARTESIAN_POINT('Ctrl Pts',(-29.803152525388,13.8885306001009,126.945876263857)) ;
#116206 = CARTESIAN_POINT('Ctrl Pts',(-29.7847767393562,13.6107524410049,
126.859040355574)) ;
#116207 = CARTESIAN_POINT('Ctrl Pts',(-29.7910854802672,13.3210542583331,
126.844495484992)) ;
#116208 = CARTESIAN_POINT('Ctrl Pts',(-29.8229753868191,13.0351251235983,
126.904244014759)) ;
#116209 = CARTESIAN_POINT('Ctrl Pts',(-29.8776744286432,12.7816150209491,
127.031216029816)) ;
#116210 = CARTESIAN_POINT('Ctrl Pts',(-29.9534311716552,12.5706518061014,
127.219253692065)) ;
#116211 = CARTESIAN_POINT('Ctrl Pts',(-30.0445412838822,12.422091900903,127.452333377032)) ;
#116212 = CARTESIAN_POINT('Ctrl Pts',(-30.1457887502779,12.3448083833829,
127.714923612566)) ;
#116213 = CARTESIAN_POINT('Ctrl Pts',(-30.250148655895,12.3450375607664,127.986693881587)) ;
#116214 = CARTESIAN_POINT('Ctrl Pts',(-30.3511170822601,12.4222140372622,
128.248559607977)) ;
#116215 = CARTESIAN_POINT('Ctrl Pts',(-30.4423550067095,12.5713072693593,
128.481942746401)) ;
#116216 = CARTESIAN_POINT('Ctrl Pts',(-30.5177968325665,12.7812068465324,
128.669220610782)) ;
#116217 = CARTESIAN_POINT('Ctrl Pts',(-30.5730322088188,13.0378486801572,
128.797371634622)) ;
#116218 = CARTESIAN_POINT('Ctrl Pts',(-30.6044543099339,13.3220972424203,
128.855977004469)) ;
#116219 = CARTESIAN_POINT('Ctrl Pts',(-30.6107589621473,13.6116477161832,
128.841431739069)) ;
#116220 = CARTESIAN_POINT('Ctrl Pts',(-30.5922328646922,13.8896343949454,
128.754117840507)) ;
#116221 = CARTESIAN_POINT('Ctrl Pts',(-30.5510661396947,14.1329048293709,
128.60084368254)) ;
#116222 = CARTESIAN_POINT('Ctrl Pts',(-30.4905361238725,14.3266157424045,
128.390815616408)) ;
#116223 = CARTESIAN_POINT('Ctrl Pts',(-30.4160368539188,14.4550271923226,
128.140061981301)) ;
#116224 = CARTESIAN_POINT('Ctrl Pts',(-30.333450058965,14.5094869156272,127.865640071397)) ;
#116225 = CARTESIAN_POINT('Ctrl Pts',(-30.2498814405861,14.4863255111229,
127.588507289986)) ;
#116226 = CARTESIAN_POINT('Ctrl Pts',(-30.1712461824057,14.3868080890416,
127.325605825376)) ;
#116227 = CARTESIAN_POINT('Ctrl Pts',(-30.1044933380963,14.2186053771164,
127.097513189475)) ;
#116228 = CARTESIAN_POINT('Ctrl Pts',(-30.0547280039428,13.9916146831158,
126.918804037804)) ;
#116229 = CARTESIAN_POINT('Ctrl Pts',(-30.0268955041398,13.727139474133,126.804607454992)) ;
#116230 = CARTESIAN_POINT('Ctrl Pts',(-30.0231159202939,13.437362164295,126.760227532608)) ;
#116231 = CARTESIAN_POINT('Ctrl Pts',(-30.0443922432487,13.1504054531947,
126.789513820971)) ;
#116232 = CARTESIAN_POINT('Ctrl Pts',(-30.0906616171445,12.8786465021209,
126.89126693415)) ;
#116233 = CARTESIAN_POINT('Ctrl Pts',(-30.157970236125,12.6500332814425,127.055027994723)) ;
#116234 = CARTESIAN_POINT('Ctrl Pts',(-30.2434337782595,12.4743183897028,
127.271533917434)) ;
#116235 = CARTESIAN_POINT('Ctrl Pts',(-30.3417585829433,12.3668547922141,
127.525488336301)) ;
#116236 = CARTESIAN_POINT('Ctrl Pts',(-30.4450821005495,12.335562941567,127.79438563983)) ;
#116237 = CARTESIAN_POINT('Ctrl Pts',(-30.5484944936694,12.3817108072099,
128.063306891139)) ;
#116238 = CARTESIAN_POINT('Ctrl Pts',(-30.6445980415539,12.502839824897,128.310875860644)) ;
#116239 = CARTESIAN_POINT('Ctrl Pts',(-30.7271978616452,12.690351441453,128.518969835721)) ;
#116240 = CARTESIAN_POINT('Ctrl Pts',(-30.7907079505213,12.9285059391321,
128.671549365572)) ;
#116241 = CARTESIAN_POINT('Ctrl Pts',(-30.832295267727,13.2046731907038,128.75974213921)) ;
#116242 = CARTESIAN_POINT('Ctrl Pts',(-30.8487758407748,13.4951333113011,
128.774772845728)) ;
#116243 = CARTESIAN_POINT('Ctrl Pts',(-30.8402346447153,13.779501210584,128.716814376005)) ;
#116244 = CARTESIAN_POINT('Ctrl Pts',(-30.8078637040687,14.0394108332529,
128.589125311067)) ;
#116245 = CARTESIAN_POINT('Ctrl Pts',(-30.7546552751125,14.2552141196343,
128.400557285253)) ;
#116246 = CARTESIAN_POINT('Ctrl Pts',(-30.6851696086428,14.4112842226695,
128.164437543065)) ;
#116247 = CARTESIAN_POINT('Ctrl Pts',(-30.6053419982904,14.49663037618,127.89819080895)) ;
#116248 = CARTESIAN_POINT('Ctrl Pts',(-30.520751800545,14.5049768783044,127.617767628039)) ;
#116249 = CARTESIAN_POINT('Ctrl Pts',(-30.4397470692586,14.4360835729073,
127.348190225217)) ;
#116250 = CARTESIAN_POINT('Ctrl Pts',(-30.3673932451776,14.2946513922982,
127.103676961857)) ;
#116251 = CARTESIAN_POINT('Ctrl Pts',(-30.3101336108046,14.0899140100411,
126.903186984993)) ;
#116252 = CARTESIAN_POINT('Ctrl Pts',(-30.2730059348416,13.8386917046902,
126.761684342598)) ;
#116253 = CARTESIAN_POINT('Ctrl Pts',(-30.2591454609719,13.5555692125345,
126.687892009024)) ;
#116254 = CARTESIAN_POINT('Ctrl Pts',(-30.2703044262027,13.2663901180779,
126.687596604313)) ;
#116255 = CARTESIAN_POINT('Ctrl Pts',(-30.3064563015578,12.9858847333076,
126.760012223785)) ;
#116256 = CARTESIAN_POINT('Ctrl Pts',(-30.3656808780386,12.7375102459871,
126.899927974495)) ;
#116257 = CARTESIAN_POINT('Ctrl Pts',(-30.4446592433479,12.5376376287816,
127.097461701573)) ;
#116258 = CARTESIAN_POINT('Ctrl Pts',(-30.5383897496922,12.4015826977934,
127.338092518212)) ;
#116259 = CARTESIAN_POINT('Ctrl Pts',(-30.6402554773558,12.3390360902595,
127.602664560348)) ;
#116260 = CARTESIAN_POINT('Ctrl Pts',(-30.7445603425615,12.353575403094,127.874253187337)) ;
#116261 = CARTESIAN_POINT('Ctrl Pts',(-30.8445423217259,12.445274073871,128.133104829671)) ;
#116262 = CARTESIAN_POINT('Ctrl Pts',(-30.9331533396269,12.6067971683827,
128.358841764631)) ;
#116263 = CARTESIAN_POINT('Ctrl Pts',(-31.0052235518519,12.8274892534517,
128.536166471027)) ;
#116264 = CARTESIAN_POINT('Ctrl Pts',(-31.0557929024469,13.0891408927057,
128.650910668167)) ;
#116265 = CARTESIAN_POINT('Ctrl Pts',(-31.0826649707566,13.375740122579,128.696283133412)) ;
#116266 = CARTESIAN_POINT('Ctrl Pts',(-31.0842457464183,13.6659116032671,
128.667755109105)) ;
#116267 = CARTESIAN_POINT('Ctrl Pts',(-31.0612969342213,13.9383430672958,
128.567621981036)) ;
#116268 = CARTESIAN_POINT('Ctrl Pts',(-31.0158421470532,14.1747318786697,
128.401589927848)) ;
#116269 = CARTESIAN_POINT('Ctrl Pts',(-30.952741170991,14.3556000224366,128.184334680318)) ;
#116270 = CARTESIAN_POINT('Ctrl Pts',(-30.8757148543573,14.4715471852787,
127.925954832144)) ;
#116271 = CARTESIAN_POINT('Ctrl Pts',(-30.7926989079768,14.5109306884899,
127.650429154449)) ;
#116272 = CARTESIAN_POINT('Ctrl Pts',(-30.7096170404131,14.4734197510009,
127.374712802353)) ;
#116273 = CARTESIAN_POINT('Ctrl Pts',(-30.6324207964218,14.3595613312843,
127.115883659408)) ;
#116274 = CARTESIAN_POINT('Ctrl Pts',(-30.5687431637558,14.179466171533,126.896825275717)) ;
#116275 = CARTESIAN_POINT('Ctrl Pts',(-30.5229949276125,13.9455181185487,
126.730115674649)) ;
#116276 = CARTESIAN_POINT('Ctrl Pts',(-30.4993062024708,13.6723045745694,
126.627634301698)) ;
#116277 = CARTESIAN_POINT('Ctrl Pts',(-30.5003214317798,13.3834915874396,
126.597593551244)) ;
#116278 = CARTESIAN_POINT('Ctrl Pts',(-30.5264493139276,13.0966134068724,
126.640803917263)) ;
#116279 = CARTESIAN_POINT('Ctrl Pts',(-30.5766713219404,12.8330521051259,
126.754396922064)) ;
#116280 = CARTESIAN_POINT('Ctrl Pts',(-30.6483002280116,12.6112324338377,
126.930439181463)) ;
#116281 = CARTESIAN_POINT('Ctrl Pts',(-30.736661695068,12.4482429025448,127.155425447181)) ;
#116282 = CARTESIAN_POINT('Ctrl Pts',(-30.8357315528907,12.3553252392396,
127.411846833704)) ;
#116283 = CARTESIAN_POINT('Ctrl Pts',(-30.9400335857783,12.3382107107946,
127.683413725756)) ;
#116284 = CARTESIAN_POINT('Ctrl Pts',(-31.042636248853,12.3992481458877,127.94994445052)) ;
#116285 = CARTESIAN_POINT('Ctrl Pts',(-31.1362393771601,12.5331204758664,
128.190343537901)) ;
#116286 = CARTESIAN_POINT('Ctrl Pts',(-31.215635139957,12.7309387918669,128.389145202128)) ;
#116287 = CARTESIAN_POINT('Ctrl Pts',(-31.2756357249041,12.9791524410526,
128.53120468286)) ;
#116288 = CARTESIAN_POINT('Ctrl Pts',(-31.312400854353,13.2585790598106,128.605475928875)) ;
#116289 = CARTESIAN_POINT('Ctrl Pts',(-31.3241836080649,13.5499397896395,
128.606744173026)) ;
#116290 = CARTESIAN_POINT('Ctrl Pts',(-31.3110087346716,13.8311712407388,
128.535239748079)) ;
#116291 = CARTESIAN_POINT('Ctrl Pts',(-31.2742363093329,14.0848085651835,
128.394579152518)) ;
#116292 = CARTESIAN_POINT('Ctrl Pts',(-31.2178679894401,14.2892041446737,
128.196968022278)) ;
#116293 = CARTESIAN_POINT('Ctrl Pts',(-31.1457920021485,14.4332159069687,
127.953199131549)) ;
#116294 = CARTESIAN_POINT('Ctrl Pts',(-31.064501704361,14.5042073782218,127.682616508337)) ;
#116295 = CARTESIAN_POINT('Ctrl Pts',(-30.9803569070733,14.4978850554144,
127.403677198383)) ;
#116296 = CARTESIAN_POINT('Ctrl Pts',(-30.9001457048563,14.4145534025925,
127.136236709374)) ;
#116297 = CARTESIAN_POINT('Ctrl Pts',(-30.8302915857101,14.2600830965558,
126.899030948309)) ;
#116298 = CARTESIAN_POINT('Ctrl Pts',(-30.7766783037662,14.0459659620245,
126.70932486434)) ;
#116299 = CARTESIAN_POINT('Ctrl Pts',(-30.7436688177568,13.7875807752627,
126.579828846178)) ;
#116300 = CARTESIAN_POINT('Ctrl Pts',(-30.7344309347098,13.5015008973902,
126.519590640979)) ;
#116301 = CARTESIAN_POINT('Ctrl Pts',(-30.7503570117774,13.2119712102584,
126.533117195425)) ;
#116302 = CARTESIAN_POINT('Ctrl Pts',(-30.7909948356034,12.9363053782512,
126.618694908227)) ;
#116303 = CARTESIAN_POINT('Ctrl Pts',(-30.8544313460082,12.6952736602129,
126.770815078882)) ;
#116304 = CARTESIAN_POINT('Ctrl Pts',(-30.936259477995,12.507125678723,126.976810991267)) ;
#116305 = CARTESIAN_POINT('Ctrl Pts',(-31.0324849838793,12.3837628513247,
127.224594411425)) ;
#116306 = CARTESIAN_POINT('Ctrl Pts',(-31.1350680188049,12.3357954087756,
127.491330342941)) ;
#116307 = CARTESIAN_POINT('Ctrl Pts',(-31.23935127795,12.3652711251859,127.762742575844)) ;
#116308 = CARTESIAN_POINT('Ctrl Pts',(-31.3372466101365,12.4705156806676,
128.015655972246)) ;
#116309 = CARTESIAN_POINT('Ctrl Pts',(-31.4231098978925,12.6439184973371,
128.233370607722)) ;
#116310 = CARTESIAN_POINT('Ctrl Pts',(-31.4913656157794,12.8730354055636,
128.399662361953)) ;
#116311 = CARTESIAN_POINT('Ctrl Pts',(-31.5379531663441,13.1424159445997,
128.502550794473)) ;
#116312 = CARTESIAN_POINT('Ctrl Pts',(-31.5599892196137,13.4306391754528,
128.533873702179)) ;
#116313 = CARTESIAN_POINT('Ctrl Pts',(-31.5568791607716,13.7191539441457,
128.491638388163)) ;
#116314 = CARTESIAN_POINT('Ctrl Pts',(-31.5294551877072,13.9861293896989,
128.378414253767)) ;
#116315 = CARTESIAN_POINT('Ctrl Pts',(-31.4804720297221,14.2128684001206,
128.202207341774)) ;
#116316 = CARTESIAN_POINT('Ctrl Pts',(-31.4139631417804,14.3833347965248,
127.974731570058)) ;
#116317 = CARTESIAN_POINT('Ctrl Pts',(-31.3357239804157,14.4845639099252,
127.713064266216)) ;
#116318 = CARTESIAN_POINT('Ctrl Pts',(-31.2519760904658,14.5099092471542,
127.435310311413)) ;
#116319 = CARTESIAN_POINT('Ctrl Pts',(-31.169269063561,14.4573341215463,127.160540128222)) ;
#116320 = CARTESIAN_POINT('Ctrl Pts',(-31.0944827944426,14.3305258270945,
126.908931141692)) ;
#116321 = CARTESIAN_POINT('Ctrl Pts',(-31.0337818947545,14.1393930806654,
126.698567894651)) ;
#116322 = CARTESIAN_POINT('Ctrl Pts',(-30.991822622221,13.8963012865058,126.542832684996)) ;
#116323 = CARTESIAN_POINT('Ctrl Pts',(-30.9727169093987,13.618527952916,126.453788104164)) ;
#116324 = CARTESIAN_POINT('Ctrl Pts',(-30.9784116943508,13.3290638567204,
126.43746201239)) ;
#116325 = CARTESIAN_POINT('Ctrl Pts',(-31.0092534744897,13.0445549081066,
126.494384804869)) ;
#116326 = CARTESIAN_POINT('Ctrl Pts',(-31.0636975928906,12.7876683953407,
126.620329890945)) ;
#116327 = CARTESIAN_POINT('Ctrl Pts',(-31.1390893626737,12.5753843248543,
126.807286162987)) ;
#116328 = CARTESIAN_POINT('Ctrl Pts',(-31.2294856731981,12.4255194566962,
127.038405016624)) ;
#116329 = CARTESIAN_POINT('Ctrl Pts',(-31.3305520361071,12.3459765628223,
127.300458413669)) ;
#116330 = CARTESIAN_POINT('Ctrl Pts',(-31.434776599086,12.3439073333341,127.571874828474)) ;
#116331 = CARTESIAN_POINT('Ctrl Pts',(-31.5361216061782,12.4188279963137,
127.834788869403)) ;
#116332 = CARTESIAN_POINT('Ctrl Pts',(-31.6280697762185,12.5669347456838,
128.070100154879)) ;
#116333 = CARTESIAN_POINT('Ctrl Pts',(-31.7035334984892,12.7740276750078,
128.257653591068)) ;
#116334 = CARTESIAN_POINT('Ctrl Pts',(-31.759609829367,13.0302839963835,128.388157305165)) ;
#116335 = CARTESIAN_POINT('Ctrl Pts',(-31.7916573927032,13.3133908418281,
128.44867020828)) ;
#116336 = CARTESIAN_POINT('Ctrl Pts',(-31.7986966116337,13.603463644202,128.436213818987)) ;
#116337 = CARTESIAN_POINT('Ctrl Pts',(-31.7809913371395,13.8813033828735,
128.35140974243)) ;
#116338 = CARTESIAN_POINT('Ctrl Pts',(-31.7400851389627,14.1277803353935,
128.198621302036)) ;
#116339 = CARTESIAN_POINT('Ctrl Pts',(-31.6800730695565,14.3222499491186,
127.990196055143)) ;
#116340 = CARTESIAN_POINT('Ctrl Pts',(-31.6061655491007,14.4521801137134,
127.741284607191)) ;
#116341 = CARTESIAN_POINT('Ctrl Pts',(-31.5238300942761,14.5090397013049,
127.467639877269)) ;
#116342 = CARTESIAN_POINT('Ctrl Pts',(-31.4398666707468,14.4879536383768,
127.189213876511)) ;
#116343 = CARTESIAN_POINT('Ctrl Pts',(-31.3611027665607,14.3907169193799,
126.925998091316)) ;
#116344 = CARTESIAN_POINT('Ctrl Pts',(-31.2937040056646,14.2230874926912,
126.695841876849)) ;
#116345 = CARTESIAN_POINT('Ctrl Pts',(-31.2439920013192,14.0008521290395,
126.517762290878)) ;
#116346 = CARTESIAN_POINT('Ctrl Pts',(-31.2150907661555,13.7343152663338,
126.400042595703)) ;
#116347 = CARTESIAN_POINT('Ctrl Pts',(-31.2106083276963,13.4474451530714,
126.353922032443)) ;
#116348 = CARTESIAN_POINT('Ctrl Pts',(-31.2313383311631,13.1575373599845,
126.381288702569)) ;
#116349 = CARTESIAN_POINT('Ctrl Pts',(-31.2764056532061,12.8878586186382,
126.479905180231)) ;
#116350 = CARTESIAN_POINT('Ctrl Pts',(-31.3436059924202,12.6555337160297,
126.643048484565)) ;
#116351 = CARTESIAN_POINT('Ctrl Pts',(-31.4286039772841,12.4784852863875,
126.858237182344)) ;
#116352 = CARTESIAN_POINT('Ctrl Pts',(-31.5266156330296,12.3688435126028,
127.11128245237)) ;
#116353 = CARTESIAN_POINT('Ctrl Pts',(-31.630084559127,12.335379050582,127.380536177025)) ;
#116354 = CARTESIAN_POINT('Ctrl Pts',(-31.7333993373061,12.3794309050292,
127.649233966248)) ;
#116355 = CARTESIAN_POINT('Ctrl Pts',(-31.8295546512421,12.4979553005814,
127.897051153347)) ;
#116356 = CARTESIAN_POINT('Ctrl Pts',(-31.9129345986958,12.6843641512771,
128.107301604166)) ;
#116357 = CARTESIAN_POINT('Ctrl Pts',(-31.9769081760024,12.9208195190715,
128.261300839291)) ;
#116358 = CARTESIAN_POINT('Ctrl Pts',(-32.0192234596835,13.1965599156971,
128.351576775379)) ;
#116359 = CARTESIAN_POINT('Ctrl Pts',(-32.0364080377691,13.4854150034454,
128.36882968244)) ;
#116360 = CARTESIAN_POINT('Ctrl Pts',(-32.0286590942519,13.7715245103546,
128.313041033143)) ;
#116361 = CARTESIAN_POINT('Ctrl Pts',(-31.9967949405779,14.0329603333754,
128.186757372476)) ;
#116362 = CARTESIAN_POINT('Ctrl Pts',(-31.9442598511563,14.2495174070446,
128.000252912401)) ;
#116363 = CARTESIAN_POINT('Ctrl Pts',(-31.8752637456382,14.4077221355952,
127.765584521541)) ;
#116364 = CARTESIAN_POINT('Ctrl Pts',(-31.7949904880439,14.4954974794661,
127.497773147365)) ;
#116365 = CARTESIAN_POINT('Ctrl Pts',(-31.7112118667338,14.5058124227374,
127.220036909701)) ;
#116366 = CARTESIAN_POINT('Ctrl Pts',(-31.6295895835472,14.4390540160987,
126.948477953836)) ;
#116367 = CARTESIAN_POINT('Ctrl Pts',(-31.5567958768622,14.2988995016989,
126.702614005723)) ;
#116368 = CARTESIAN_POINT('Ctrl Pts',(-31.4992152164798,14.0959846822767,
126.501253268444)) ;
#116369 = CARTESIAN_POINT('Ctrl Pts',(-31.4616155663629,13.8467238077785,
126.358483470145)) ;
#116370 = CARTESIAN_POINT('Ctrl Pts',(-31.4469797675735,13.5651499595772,
126.282529118317)) ;
#116371 = CARTESIAN_POINT('Ctrl Pts',(-31.4573898379876,13.2745210705863,
126.279884269193)) ;
#116372 = CARTESIAN_POINT('Ctrl Pts',(-31.4929777781403,12.9930481847516,
126.350603500459)) ;
#116373 = CARTESIAN_POINT('Ctrl Pts',(-31.5514293278227,12.7442685275202,
126.488355718607)) ;
#116374 = CARTESIAN_POINT('Ctrl Pts',(-31.629789771733,12.5428869624623,126.684118709821)) ;
#116375 = CARTESIAN_POINT('Ctrl Pts',(-31.7230911251259,12.4047083280592,
126.923514916853)) ;
#116376 = CARTESIAN_POINT('Ctrl Pts',(-31.8251196709966,12.3396945526809,
127.188456991403)) ;
#116377 = CARTESIAN_POINT('Ctrl Pts',(-31.9293847768492,12.3521469576885,
127.459951466802)) ;
#116378 = CARTESIAN_POINT('Ctrl Pts',(-32.0293584096416,12.441314353945,127.718862688757)) ;
#116379 = CARTESIAN_POINT('Ctrl Pts',(-32.118508034267,12.6011043288198,127.946125196227)) ;
#116380 = CARTESIAN_POINT('Ctrl Pts',(-32.1909463624357,12.8194224397463,
128.124637671274)) ;
#116381 = CARTESIAN_POINT('Ctrl Pts',(-32.2424853469496,13.0811434342732,
128.242065843194)) ;
#116382 = CARTESIAN_POINT('Ctrl Pts',(-32.2700475124695,13.3679217852881,
128.289393931887)) ;
#116383 = CARTESIAN_POINT('Ctrl Pts',(-32.2723234688677,13.6574454003315,
128.262990706036)) ;
#116384 = CARTESIAN_POINT('Ctrl Pts',(-32.2501377563472,13.9304218890574,
128.16512094437)) ;
#116385 = CARTESIAN_POINT('Ctrl Pts',(-32.2052527136117,14.1686008595605,
128.000705406738)) ;
#116386 = CARTESIAN_POINT('Ctrl Pts',(-32.1424368825761,14.3514046814191,
127.78421431945)) ;
#116387 = CARTESIAN_POINT('Ctrl Pts',(-32.0661890017219,14.4688537010489,
127.528311842842)) ;
#116388 = CARTESIAN_POINT('Ctrl Pts',(-31.9829477124764,14.5110084065472,
127.25198980975)) ;
#116389 = CARTESIAN_POINT('Ctrl Pts',(-31.8996523370137,14.4754271659884,
126.975598872173)) ;
#116390 = CARTESIAN_POINT('Ctrl Pts',(-31.8224332847297,14.3641624802179,
126.716820698264)) ;
#116391 = CARTESIAN_POINT('Ctrl Pts',(-31.7580395500746,14.1852632695012,
126.495546204119)) ;
#116392 = CARTESIAN_POINT('Ctrl Pts',(-31.7118161309124,13.9526451401233,
126.327472065972)) ;
#116393 = CARTESIAN_POINT('Ctrl Pts',(-31.6875151171821,13.6818447118076,
126.223384381321)) ;
#116394 = CARTESIAN_POINT('Ctrl Pts',(-31.6876428707132,13.3926206452482,
126.190673672069)) ;
#116395 = CARTESIAN_POINT('Ctrl Pts',(-31.7132303697958,13.1038754923078,
126.232132655585)) ;
#116396 = CARTESIAN_POINT('Ctrl Pts',(-31.7626844305404,12.8403836297391,
126.343597807942)) ;
#116397 = CARTESIAN_POINT('Ctrl Pts',(-31.833493429736,12.6175434576375,126.517332769775)) ;
#116398 = CARTESIAN_POINT('Ctrl Pts',(-31.9215930084005,12.4520178789147,
126.741478574285)) ;
#116399 = CARTESIAN_POINT('Ctrl Pts',(-32.0209307914902,12.3567780608222,
126.998523271918)) ;
#116400 = CARTESIAN_POINT('Ctrl Pts',(-32.1246416504795,12.3376561109864,
127.268538964137)) ;
#116401 = CARTESIAN_POINT('Ctrl Pts',(-32.2275246940126,12.3963494804203,
127.535847716125)) ;
#116402 = CARTESIAN_POINT('Ctrl Pts',(-32.3214673626583,12.5282529228556,
127.777238677115)) ;
#116403 = CARTESIAN_POINT('Ctrl Pts',(-32.4013423719323,12.7243873042916,
127.977442347176)) ;
#116404 = CARTESIAN_POINT('Ctrl Pts',(-32.4619096573449,12.9708923918956,
128.121216797039)) ;
#116405 = CARTESIAN_POINT('Ctrl Pts',(-32.4994416556502,13.2502126197918,
128.197659332614)) ;
#116406 = CARTESIAN_POINT('Ctrl Pts',(-32.5119978982385,13.5400583828972,
128.201358931735)) ;
#116407 = CARTESIAN_POINT('Ctrl Pts',(-32.4994888167825,13.8239338286533,
128.131553230696)) ;
#116408 = CARTESIAN_POINT('Ctrl Pts',(-32.4634273595897,14.0777676729547,
127.99308635593)) ;
#116409 = CARTESIAN_POINT('Ctrl Pts',(-32.4075028614965,14.2841378500946,
127.796711420429)) ;
#116410 = CARTESIAN_POINT('Ctrl Pts',(-32.3359847249591,14.429815657766,127.554661094343)) ;
#116411 = CARTESIAN_POINT('Ctrl Pts',(-32.2546028623038,14.5033259168077,
127.283693381333)) ;
#116412 = CARTESIAN_POINT('Ctrl Pts',(-32.1704924928081,14.499135115111,127.004877771061)) ;
#116413 = CARTESIAN_POINT('Ctrl Pts',(-32.0900191687497,14.4177798325381,
126.736640312097)) ;
#116414 = CARTESIAN_POINT('Ctrl Pts',(-32.0200109297833,14.2657377102023,
126.499094130843)) ;
#116415 = CARTESIAN_POINT('Ctrl Pts',(-31.9656700623202,14.0527574173429,
126.30717910773)) ;
#116416 = CARTESIAN_POINT('Ctrl Pts',(-31.9319934820835,13.7942044324148,
126.175602610685)) ;
#116417 = CARTESIAN_POINT('Ctrl Pts',(-31.922152144827,13.509972220369,126.1137676569)) ;
#116418 = CARTESIAN_POINT('Ctrl Pts',(-31.9373531303038,13.219834764377,126.12511889965)) ;
#116419 = CARTESIAN_POINT('Ctrl Pts',(-31.9773715779164,12.9433154987134,
126.208868906181)) ;
#116420 = CARTESIAN_POINT('Ctrl Pts',(-32.0403631928475,12.7008042356819,
126.359640175799)) ;
#116421 = CARTESIAN_POINT('Ctrl Pts',(-32.1214625671299,12.5118988342583,
126.563632155226)) ;
#116422 = CARTESIAN_POINT('Ctrl Pts',(-32.2168510067031,12.3867144480253,
126.809132213192)) ;
#116423 = CARTESIAN_POINT('Ctrl Pts',(-32.3199033888381,12.3359851161897,
127.077044236849)) ;
#116424 = CARTESIAN_POINT('Ctrl Pts',(-32.4242222709057,12.3634203970633,
127.348571063411)) ;
#116425 = CARTESIAN_POINT('Ctrl Pts',(-32.5223579803355,12.4663876358086,
127.602200216398)) ;
#116426 = CARTESIAN_POINT('Ctrl Pts',(-32.6089883742709,12.6389701182042,
127.82200642748)) ;
#116427 = CARTESIAN_POINT('Ctrl Pts',(-32.6774297887948,12.8657474577828,
127.988998597794)) ;
#116428 = CARTESIAN_POINT('Ctrl Pts',(-32.724805208469,13.1346343436699,128.094136048027)) ;
#116429 = CARTESIAN_POINT('Ctrl Pts',(-32.7399114943369,13.3266512177486,
128.116225545094)) ;
#116430 = CARTESIAN_POINT('Ctrl Pts',(-32.7433109767759,13.4226801736581,
128.115135559137)) ;
#116431 = CARTESIAN_POINT('Ctrl Pts',(-11.3048362387632,13.1734341962953,
133.294175679076)) ;
#116432 = CARTESIAN_POINT('Ctrl Pts',(-11.3055397872598,13.1676985117492,
133.295499960923)) ;
#116433 = CARTESIAN_POINT('Ctrl Pts',(-11.3170134107587,13.0762045259503,
133.317334845661)) ;
#116434 = CARTESIAN_POINT('Ctrl Pts',(-11.3479906245566,12.9034782773047,
133.384852143393)) ;
#116435 = CARTESIAN_POINT('Ctrl Pts',(-11.4126663887472,12.6923998391673,
133.540763803588)) ;
#116436 = CARTESIAN_POINT('Ctrl Pts',(-11.493631562145,12.5327609209973,133.744177423375)) ;
#116437 = CARTESIAN_POINT('Ctrl Pts',(-11.5862892630392,12.4368205813749,
133.981580357227)) ;
#116438 = CARTESIAN_POINT('Ctrl Pts',(-11.6832291399257,12.4119420222618,
134.231836866922)) ;
#116439 = CARTESIAN_POINT('Ctrl Pts',(-11.78005525905,12.4592681303251,134.481464238848)) ;
#116440 = CARTESIAN_POINT('Ctrl Pts',(-11.8693322167585,12.5756589901857,
134.709172628028)) ;
#116441 = CARTESIAN_POINT('Ctrl Pts',(-11.9459105506398,12.7528353501054,
134.899733529327)) ;
#116442 = CARTESIAN_POINT('Ctrl Pts',(-12.0048397897214,12.9779970726337,
135.038757218061)) ;
#116443 = CARTESIAN_POINT('Ctrl Pts',(-12.0426597744358,13.2349353323575,
135.116124740278)) ;
#116444 = CARTESIAN_POINT('Ctrl Pts',(-12.0574764879123,13.5051817925228,
135.126317551283)) ;
#116445 = CARTESIAN_POINT('Ctrl Pts',(-12.0487533971068,13.7710455478253,
135.067545544702)) ;
#116446 = CARTESIAN_POINT('Ctrl Pts',(-12.0181630588652,14.0095405119009,
134.945221836394)) ;
#116447 = CARTESIAN_POINT('Ctrl Pts',(-11.9683909050091,14.207375982779,134.766695726132)) ;
#116448 = CARTESIAN_POINT('Ctrl Pts',(-11.903769353582,14.3489569036635,134.544805288448)) ;
#116449 = CARTESIAN_POINT('Ctrl Pts',(-11.8294467098174,14.4243647348289,
134.294477966775)) ;
#116450 = CARTESIAN_POINT('Ctrl Pts',(-11.751885562071,14.4276726167065,134.034782669487)) ;
#116451 = CARTESIAN_POINT('Ctrl Pts',(-11.6772862681535,14.3592846174027,
133.783789327162)) ;
#116452 = CARTESIAN_POINT('Ctrl Pts',(-11.611513681331,14.2239083327593,133.558547654538)) ;
#116453 = CARTESIAN_POINT('Ctrl Pts',(-11.5599948518806,14.0309432296264,
133.374897001415)) ;
#116454 = CARTESIAN_POINT('Ctrl Pts',(-11.5272842544717,13.793723337017,133.2461166906)) ;
#116455 = CARTESIAN_POINT('Ctrl Pts',(-11.516538548757,13.531837086658,133.181746910791)) ;
#116456 = CARTESIAN_POINT('Ctrl Pts',(-11.5289803651642,13.2609089527483,
133.184950619645)) ;
#116457 = CARTESIAN_POINT('Ctrl Pts',(-11.5648046980364,13.0011532245151,
133.256394467539)) ;
#116458 = CARTESIAN_POINT('Ctrl Pts',(-11.6216466377954,12.7729628061281,
133.389432711134)) ;
#116459 = CARTESIAN_POINT('Ctrl Pts',(-11.6968168147813,12.5901802135074,
133.575825804335)) ;
#116460 = CARTESIAN_POINT('Ctrl Pts',(-11.7850384827174,12.4676468179757,
133.800475594732)) ;
#116461 = CARTESIAN_POINT('Ctrl Pts',(-11.8814377069306,12.4133145081089,
134.04885414273)) ;
#116462 = CARTESIAN_POINT('Ctrl Pts',(-11.9787704166135,12.4313808819739,
134.300185342639)) ;
#116463 = CARTESIAN_POINT('Ctrl Pts',(-12.0720174352247,12.520660304575,134.539371072293)) ;
#116464 = CARTESIAN_POINT('Ctrl Pts',(-12.1542732554476,12.6744195620442,
134.746571867679)) ;
#116465 = CARTESIAN_POINT('Ctrl Pts',(-12.2208394898278,12.8815892822748,
134.907929827527)) ;
#116466 = CARTESIAN_POINT('Ctrl Pts',(-12.2677283074646,13.1290193057785,
135.011625583399)) ;
#116467 = CARTESIAN_POINT('Ctrl Pts',(-12.2918106276939,13.3950772223713,
135.049016578508)) ;
#116468 = CARTESIAN_POINT('Ctrl Pts',(-12.2926944047224,13.66434219871,135.018483925566)) ;
#116469 = CARTESIAN_POINT('Ctrl Pts',(-12.2706182916445,13.9170737503532,
134.920777667333)) ;
#116470 = CARTESIAN_POINT('Ctrl Pts',(-12.2281264946411,14.1334228182709,
134.763559895528)) ;
#116471 = CARTESIAN_POINT('Ctrl Pts',(-12.1690356539749,14.2989215662944,
134.557882314795)) ;
#116472 = CARTESIAN_POINT('Ctrl Pts',(-12.0980917977181,14.4021434485844,
134.317520347929)) ;
#116473 = CARTESIAN_POINT('Ctrl Pts',(-12.0209753725309,14.4351203020035,
134.059037518786)) ;
#116474 = CARTESIAN_POINT('Ctrl Pts',(-11.9445266332495,14.3956460292368,
133.802668787202)) ;
#116475 = CARTESIAN_POINT('Ctrl Pts',(-11.8742770006212,14.2864256382767,
133.564281364103)) ;
#116476 = CARTESIAN_POINT('Ctrl Pts',(-11.8163463282874,14.1149876156061,
133.361875622449)) ;
#116477 = CARTESIAN_POINT('Ctrl Pts',(-11.7757287928858,13.8950778859157,
133.210204358206)) ;
#116478 = CARTESIAN_POINT('Ctrl Pts',(-11.7556794040892,13.6402949383964,
133.118454428844)) ;
#116479 = CARTESIAN_POINT('Ctrl Pts',(-11.7586748594706,13.3700135586503,
133.094045455985)) ;
#116480 = CARTESIAN_POINT('Ctrl Pts',(-11.7850940030148,13.1040821018971,
133.138124942152)) ;
#116481 = CARTESIAN_POINT('Ctrl Pts',(-11.8337147621843,12.8608604058745,
133.247060692441)) ;
#116482 = CARTESIAN_POINT('Ctrl Pts',(-11.9022657738097,12.6570995861258,
133.414051481575)) ;
#116483 = CARTESIAN_POINT('Ctrl Pts',(-11.9854697021189,12.5097126273575,
133.624148755478)) ;
#116484 = CARTESIAN_POINT('Ctrl Pts',(-12.0792563949215,12.4266925864004,
133.864954668484)) ;
#116485 = CARTESIAN_POINT('Ctrl Pts',(-12.1770501733971,12.4153566077392,
134.117516473008)) ;
#116486 = CARTESIAN_POINT('Ctrl Pts',(-12.2726562901117,12.4761183331586,
134.363693217074)) ;
#116487 = CARTESIAN_POINT('Ctrl Pts',(-12.3599672381387,12.6046109786899,
134.585648111921)) ;
#116488 = CARTESIAN_POINT('Ctrl Pts',(-12.4336049342943,12.792032892229,134.767601788144)) ;
#116489 = CARTESIAN_POINT('Ctrl Pts',(-12.4887847478915,13.0246459231079,
134.895657747207)) ;
#116490 = CARTESIAN_POINT('Ctrl Pts',(-12.5223167102954,13.2849675496699,
134.960574363912)) ;
#116491 = CARTESIAN_POINT('Ctrl Pts',(-12.5327426141042,13.5561838423073,
134.957866664727)) ;
#116492 = CARTESIAN_POINT('Ctrl Pts',(-12.5197199828827,13.8182129454441,
134.886604960408)) ;
#116493 = CARTESIAN_POINT('Ctrl Pts',(-12.4852778576315,14.0504673994418,
134.752981386935)) ;
#116494 = CARTESIAN_POINT('Ctrl Pts',(-12.432142512104,14.2392687956967,134.564522703169)) ;
#116495 = CARTESIAN_POINT('Ctrl Pts',(-12.3651870124344,14.3686948710642,
134.335789865245)) ;
#116496 = CARTESIAN_POINT('Ctrl Pts',(-12.2902985792148,14.4303698610576,
134.084054618578)) ;
#116497 = CARTESIAN_POINT('Ctrl Pts',(-12.2126339213949,14.4203874495029,
133.82398885631)) ;
#116498 = CARTESIAN_POINT('Ctrl Pts',(-12.138892983068,14.3383234433453,133.5753360581)) ;
#116499 = CARTESIAN_POINT('Ctrl Pts',(-12.0755004122428,14.1909247439309,
133.357045112776)) ;
#116500 = CARTESIAN_POINT('Ctrl Pts',(-12.0274928686727,13.9894772519221,
133.18381104636)) ;
#116501 = CARTESIAN_POINT('Ctrl Pts',(-11.9986969915971,13.7468083909025,
133.066570085229)) ;
#116502 = CARTESIAN_POINT('Ctrl Pts',(-11.9921460683351,13.4802543553281,
133.014236646284)) ;
#116503 = CARTESIAN_POINT('Ctrl Pts',(-12.0092717413035,13.2092851257182,
133.031023331709)) ;
#116504 = CARTESIAN_POINT('Ctrl Pts',(-12.0488941477586,12.956342695595,133.113890140615)) ;
#116505 = CARTESIAN_POINT('Ctrl Pts',(-12.1097548196694,12.7340443035837,
133.258436779888)) ;
#116506 = CARTESIAN_POINT('Ctrl Pts',(-12.1878735220382,12.5620254475304,
133.453464717486)) ;
#116507 = CARTESIAN_POINT('Ctrl Pts',(-12.2776773534867,12.45216345603,133.682848097027)) ;
#116508 = CARTESIAN_POINT('Ctrl Pts',(-12.3749985350835,12.4110698281944,
133.933870441482)) ;
#116509 = CARTESIAN_POINT('Ctrl Pts',(-12.4722736125084,12.4431134785041,
134.184910270632)) ;
#116510 = CARTESIAN_POINT('Ctrl Pts',(-12.5633905416193,12.544720783163,134.418071752808)) ;
#116511 = CARTESIAN_POINT('Ctrl Pts',(-12.6432257122409,12.7094608170751,
134.618156747253)) ;
#116512 = CARTESIAN_POINT('Ctrl Pts',(-12.7064847924193,12.9261933498066,
134.769723779734)) ;
#116513 = CARTESIAN_POINT('Ctrl Pts',(-12.7489848469751,13.1767718308822,
134.860888243943)) ;
#116514 = CARTESIAN_POINT('Ctrl Pts',(-12.7689773196155,13.4474343048381,
134.885986597225)) ;
#116515 = CARTESIAN_POINT('Ctrl Pts',(-12.7652633609867,13.7143157453809,
134.842086211151)) ;
#116516 = CARTESIAN_POINT('Ctrl Pts',(-12.7393471136398,13.9601208806252,
134.733384856506)) ;
#116517 = CARTESIAN_POINT('Ctrl Pts',(-12.6931971015378,14.1691500146303,
134.565311032996)) ;
#116518 = CARTESIAN_POINT('Ctrl Pts',(-12.6315346459168,14.3234012813758,
134.352162858764)) ;
#116519 = CARTESIAN_POINT('Ctrl Pts',(-12.5588878324743,14.4138714388817,
134.10676963584)) ;
#116520 = CARTESIAN_POINT('Ctrl Pts',(-12.4816544367157,14.433295070235,133.848083489319)) ;
#116521 = CARTESIAN_POINT('Ctrl Pts',(-12.4053524670984,14.3798377067091,
133.59187082097)) ;
#116522 = CARTESIAN_POINT('Ctrl Pts',(-12.3374332785635,14.2584887860387,
133.360475482159)) ;
#116523 = CARTESIAN_POINT('Ctrl Pts',(-12.2824051002791,14.0772215251275,
133.166601528295)) ;
#116524 = CARTESIAN_POINT('Ctrl Pts',(-12.2452321826126,13.847858128252,133.024747347105)) ;
#116525 = CARTESIAN_POINT('Ctrl Pts',(-12.2296059826708,13.5896600373134,
132.946061283646)) ;
#116526 = CARTESIAN_POINT('Ctrl Pts',(-12.2369463909888,13.3195390353182,
132.934455021102)) ;
#116527 = CARTESIAN_POINT('Ctrl Pts',(-12.2677721689925,13.0556171631187,
132.991302288782)) ;
#116528 = CARTESIAN_POINT('Ctrl Pts',(-12.3203670457723,12.8189344364704,
133.111861078399)) ;
#116529 = CARTESIAN_POINT('Ctrl Pts',(-12.3918779427092,12.6251004110513,
133.287618469956)) ;
#116530 = CARTESIAN_POINT('Ctrl Pts',(-12.4777181682038,12.4887479855771,
133.505288390372)) ;
#116531 = CARTESIAN_POINT('Ctrl Pts',(-12.5724812251264,12.419067054962,133.749046122386)) ;
#116532 = CARTESIAN_POINT('Ctrl Pts',(-12.6706720979256,12.4213699638912,
134.00265513351)) ;
#116533 = CARTESIAN_POINT('Ctrl Pts',(-12.7650277550218,12.4953802031986,
134.245230364366)) ;
#116534 = CARTESIAN_POINT('Ctrl Pts',(-12.8502559447532,12.6359571478174,
134.46105227128)) ;
#116535 = CARTESIAN_POINT('Ctrl Pts',(-12.920636677838,12.8329196540899,134.633528157148)) ;
#116536 = CARTESIAN_POINT('Ctrl Pts',(-12.9719270374806,13.0719648930025,
134.750256204096)) ;
#116537 = CARTESIAN_POINT('Ctrl Pts',(-13.0012404417528,13.3363496355774,
134.802758227356)) ;
#116538 = CARTESIAN_POINT('Ctrl Pts',(-13.0071448579909,13.6070576006529,
134.786864740598)) ;
#116539 = CARTESIAN_POINT('Ctrl Pts',(-12.9899370940703,13.8644611285128,
134.703467147797)) ;
#116540 = CARTESIAN_POINT('Ctrl Pts',(-12.9516551926093,14.0900772537897,
134.558538596344)) ;
#116541 = CARTESIAN_POINT('Ctrl Pts',(-12.8956186659196,14.2682172289019,
134.361685303641)) ;
#116542 = CARTESIAN_POINT('Ctrl Pts',(-12.8268821751115,14.3854165946879,
134.127841418099)) ;
#116543 = CARTESIAN_POINT('Ctrl Pts',(-12.7507359710591,14.4341663213204,
133.872274094897)) ;
#116544 = CARTESIAN_POINT('Ctrl Pts',(-12.6733019917063,14.4102121337139,
133.612860993173)) ;
#116545 = CARTESIAN_POINT('Ctrl Pts',(-12.6013206553288,14.3156229192553,
133.369490855547)) ;
#116546 = CARTESIAN_POINT('Ctrl Pts',(-12.5403300034414,14.1571117362938,
133.15819579006)) ;
#116547 = CARTESIAN_POINT('Ctrl Pts',(-12.4955161110385,13.9459764077607,
132.99415734859)) ;
#116548 = CARTESIAN_POINT('Ctrl Pts',(-12.4708094097902,13.6975622322246,
132.888878084011)) ;
#116549 = CARTESIAN_POINT('Ctrl Pts',(-12.4686895251068,13.4293974985453,
132.849565965806)) ;
#116550 = CARTESIAN_POINT('Ctrl Pts',(-12.4899907029116,13.1610019357677,
132.87870343796)) ;
#116551 = CARTESIAN_POINT('Ctrl Pts',(-12.534115379757,12.9105848440385,132.974405179964)) ;
#116552 = CARTESIAN_POINT('Ctrl Pts',(-12.5983779539559,12.6976134711112,
133.129031831098)) ;
#116553 = CARTESIAN_POINT('Ctrl Pts',(-12.6790326424138,12.5364422844779,
133.331520584852)) ;
#116554 = CARTESIAN_POINT('Ctrl Pts',(-12.7709549115279,12.4387732297296,
133.566944783629)) ;
#116555 = CARTESIAN_POINT('Ctrl Pts',(-12.8685900163271,12.4116342438892,
133.818970272208)) ;
#116556 = CARTESIAN_POINT('Ctrl Pts',(-12.9650394138879,12.4569142353896,
134.067666376452)) ;
#116557 = CARTESIAN_POINT('Ctrl Pts',(-13.0547600940725,12.5714751747461,
134.296615286209)) ;
#116558 = CARTESIAN_POINT('Ctrl Pts',(-13.1316530817672,12.7468632873084,
134.48814580267)) ;
#116559 = CARTESIAN_POINT('Ctrl Pts',(-13.1911572181041,12.9706872458922,
134.628860794572)) ;
#116560 = CARTESIAN_POINT('Ctrl Pts',(-13.2296656594081,13.2271704836993,
134.708210769396)) ;
#116561 = CARTESIAN_POINT('Ctrl Pts',(-13.2451574771088,13.4971329274745,
134.720396296595)) ;
#116562 = CARTESIAN_POINT('Ctrl Pts',(-13.2371292685592,13.7633005024016,
134.663671340864)) ;
#116563 = CARTESIAN_POINT('Ctrl Pts',(-13.2072039915708,14.002826770648,134.543298284642)) ;
#116564 = CARTESIAN_POINT('Ctrl Pts',(-13.1576917384621,14.2028677119568,
134.365387614197)) ;
#116565 = CARTESIAN_POINT('Ctrl Pts',(-13.0936548161381,14.3455611134847,
134.145336236451)) ;
#116566 = CARTESIAN_POINT('Ctrl Pts',(-13.0195413649078,14.4231516282667,
133.895616180479)) ;
#116567 = CARTESIAN_POINT('Ctrl Pts',(-12.941972170223,14.4286657485207,133.635893474366)) ;
#116568 = CARTESIAN_POINT('Ctrl Pts',(-12.8670500417961,14.3621070241951,
133.383882958189)) ;
#116569 = CARTESIAN_POINT('Ctrl Pts',(-12.8010036125882,14.2287344049999,
133.157884092812)) ;
#116570 = CARTESIAN_POINT('Ctrl Pts',(-12.7488856829864,14.0363062184854,
132.972352197591)) ;
#116571 = CARTESIAN_POINT('Ctrl Pts',(-12.7158474360347,13.8023698285734,
132.842926745116)) ;
#116572 = CARTESIAN_POINT('Ctrl Pts',(-12.7042635666528,13.538853365046,132.775826591809)) ;
#116573 = CARTESIAN_POINT('Ctrl Pts',(-12.7161476495276,13.2684519615159,
132.777472109561)) ;
#116574 = CARTESIAN_POINT('Ctrl Pts',(-12.751106729114,13.0087998067706,132.846492569486)) ;
#116575 = CARTESIAN_POINT('Ctrl Pts',(-12.807873382857,12.7778891535909,132.979055104978)) ;
#116576 = CARTESIAN_POINT('Ctrl Pts',(-12.8820585633444,12.5950174463895,
133.162824352565)) ;
#116577 = CARTESIAN_POINT('Ctrl Pts',(-12.9703954300045,12.4700325386615,
133.387640500529)) ;
#116578 = CARTESIAN_POINT('Ctrl Pts',(-13.0661153420427,12.4138573770184,
133.634230474633)) ;
#116579 = CARTESIAN_POINT('Ctrl Pts',(-13.1643568917053,12.4301864135647,
133.887911381757)) ;
#116580 = CARTESIAN_POINT('Ctrl Pts',(-13.2568223360738,12.5166843884807,
134.125173786937)) ;
#116581 = CARTESIAN_POINT('Ctrl Pts',(-13.3399856657831,12.6693064636983,
134.334830220743)) ;
#116582 = CARTESIAN_POINT('Ctrl Pts',(-13.4068238350571,12.8745470940793,
134.49709490505)) ;
#116583 = CARTESIAN_POINT('Ctrl Pts',(-13.4544450063346,13.1212023426986,
134.602896573305)) ;
#116584 = CARTESIAN_POINT('Ctrl Pts',(-13.4792271367921,13.3871938876445,
134.642301021761)) ;
#116585 = CARTESIAN_POINT('Ctrl Pts',(-13.4807690699808,13.6567281593303,
134.613680601786)) ;
#116586 = CARTESIAN_POINT('Ctrl Pts',(-13.4594081480435,13.9097854189498,
134.518129927239)) ;
#116587 = CARTESIAN_POINT('Ctrl Pts',(-13.4173442290248,14.1280196349839,
134.362063092164)) ;
#116588 = CARTESIAN_POINT('Ctrl Pts',(-13.3587335058981,14.2950456009744,
134.157826230202)) ;
#116589 = CARTESIAN_POINT('Ctrl Pts',(-13.2875991149223,14.4005267641298,
133.916709156522)) ;
#116590 = CARTESIAN_POINT('Ctrl Pts',(-13.2110834913492,14.4350836720727,
133.660212652327)) ;
#116591 = CARTESIAN_POINT('Ctrl Pts',(-13.1344387177937,14.3978038966436,
133.403225607042)) ;
#116592 = CARTESIAN_POINT('Ctrl Pts',(-13.0640036054603,14.290575680997,133.164336325255)) ;
#116593 = CARTESIAN_POINT('Ctrl Pts',(-13.0056367075179,14.12095115065,132.960667025767)) ;
#116594 = CARTESIAN_POINT('Ctrl Pts',(-12.9643797564511,13.9018371946246,
132.807063981847)) ;
#116595 = CARTESIAN_POINT('Ctrl Pts',(-12.9437529478308,13.6479071600813,
132.713647362735)) ;
#116596 = CARTESIAN_POINT('Ctrl Pts',(-12.9459834540189,13.3785018299636,
132.687089601676)) ;
#116597 = CARTESIAN_POINT('Ctrl Pts',(-12.9719279522438,13.1105161592094,
132.729570917894)) ;
#116598 = CARTESIAN_POINT('Ctrl Pts',(-13.0197798563459,12.8677237069018,
132.836427718895)) ;
#116599 = CARTESIAN_POINT('Ctrl Pts',(-13.0875829119615,12.6628308000804,
133.00130569266)) ;
#116600 = CARTESIAN_POINT('Ctrl Pts',(-13.170612266529,12.5130918940735,133.21080218841)) ;
#116601 = CARTESIAN_POINT('Ctrl Pts',(-13.2644470385299,12.4280189169956,
133.451662716591)) ;
#116602 = CARTESIAN_POINT('Ctrl Pts',(-13.3619248043351,12.4146728594404,
133.703398332785)) ;
#116603 = CARTESIAN_POINT('Ctrl Pts',(-13.4579000655806,12.4734182584077,
133.950580622376)) ;
#116604 = CARTESIAN_POINT('Ctrl Pts',(-13.5456184208567,12.6005220023049,
134.173675299527)) ;
#116605 = CARTESIAN_POINT('Ctrl Pts',(-13.6193388851311,12.7855010880113,
134.35603845551)) ;
#116606 = CARTESIAN_POINT('Ctrl Pts',(-13.6752095918886,13.0169859630547,
134.486095608093)) ;
#116607 = CARTESIAN_POINT('Ctrl Pts',(-13.7094864157964,13.2774552371681,
134.55310035212)) ;
#116608 = CARTESIAN_POINT('Ctrl Pts',(-13.720528633581,13.5483710343065,134.552225521987)) ;
#116609 = CARTESIAN_POINT('Ctrl Pts',(-13.7082871445483,13.810085890561,134.483364361746)) ;
#116610 = CARTESIAN_POINT('Ctrl Pts',(-13.6743307894067,14.0443619160834,
134.351029938079)) ;
#116611 = CARTESIAN_POINT('Ctrl Pts',(-13.6218702674786,14.2339605947032,
134.164668424612)) ;
#116612 = CARTESIAN_POINT('Ctrl Pts',(-13.5553037879054,14.3656339160498,
133.937067111739)) ;
#116613 = CARTESIAN_POINT('Ctrl Pts',(-13.4801990168619,14.429668532247,133.684537332824)) ;
#116614 = CARTESIAN_POINT('Ctrl Pts',(-13.4027282664342,14.4216217933316,
133.425128314253)) ;
#116615 = CARTESIAN_POINT('Ctrl Pts',(-13.3290373690102,14.3422174614337,
133.176748800641)) ;
#116616 = CARTESIAN_POINT('Ctrl Pts',(-13.2649970207051,14.1963613484393,
132.956451230198)) ;
#116617 = CARTESIAN_POINT('Ctrl Pts',(-13.216380386921,13.9958156934089,132.781363475866)) ;
#116618 = CARTESIAN_POINT('Ctrl Pts',(-13.1870172083142,13.7540872313105,
132.662471429064)) ;
#116619 = CARTESIAN_POINT('Ctrl Pts',(-13.1798006866086,13.4887318703653,
132.608289446469)) ;
#116620 = CARTESIAN_POINT('Ctrl Pts',(-13.1961455681105,13.217649057413,132.622802604788)) ;
#116621 = CARTESIAN_POINT('Ctrl Pts',(-13.2352634058248,12.9629384688392,
132.704064619144)) ;
#116622 = CARTESIAN_POINT('Ctrl Pts',(-13.2957072323222,12.7394456661168,
132.847362756883)) ;
#116623 = CARTESIAN_POINT('Ctrl Pts',(-13.3729246066129,12.5666312709512,
133.039944449113)) ;
#116624 = CARTESIAN_POINT('Ctrl Pts',(-13.4629469008387,12.4542159420662,
133.26977760258)) ;
#116625 = CARTESIAN_POINT('Ctrl Pts',(-13.5596073928236,12.4113528372628,
133.519064068063)) ;
#116626 = CARTESIAN_POINT('Ctrl Pts',(-13.6571882769877,12.4409689748371,
133.770921960757)) ;
#116627 = CARTESIAN_POINT('Ctrl Pts',(-13.7489524527597,12.5412370844769,
134.005829405415)) ;
#116628 = CARTESIAN_POINT('Ctrl Pts',(-13.8289234256402,12.7041353062448,
134.206393920477)) ;
#116629 = CARTESIAN_POINT('Ctrl Pts',(-13.8925272076632,12.9183855377871,
134.359123275266)) ;
#116630 = CARTESIAN_POINT('Ctrl Pts',(-13.9359235262414,13.1698655592683,
134.4526808629)) ;
#116631 = CARTESIAN_POINT('Ctrl Pts',(-13.9564522187295,13.4380609708233,
134.479623940371)) ;
#116632 = CARTESIAN_POINT('Ctrl Pts',(-13.9535148154135,13.7071666218626,
134.437760908038)) ;
#116633 = CARTESIAN_POINT('Ctrl Pts',(-13.9280836146788,13.9538087956849,
134.330459802866)) ;
#116634 = CARTESIAN_POINT('Ctrl Pts',(-13.8826845846232,14.1634526907068,
134.164713123178)) ;
#116635 = CARTESIAN_POINT('Ctrl Pts',(-13.8211006600171,14.3201289730171,
133.951628153995)) ;
#116636 = CARTESIAN_POINT('Ctrl Pts',(-13.7489996042707,14.4121340863402,
133.707983629453)) ;
#116637 = CARTESIAN_POINT('Ctrl Pts',(-13.6715419537195,14.4336855953277,
133.448515884899)) ;
#116638 = CARTESIAN_POINT('Ctrl Pts',(-13.5955937037084,14.3827386084068,
133.193555965964)) ;
#116639 = CARTESIAN_POINT('Ctrl Pts',(-13.5268624238293,14.2627494800209,
132.959564701033)) ;
#116640 = CARTESIAN_POINT('Ctrl Pts',(-13.4713984747695,14.0822577525838,
132.764352915223)) ;
#116641 = CARTESIAN_POINT('Ctrl Pts',(-13.4339559473982,13.8561932154224,
132.622014295639)) ;
#116642 = CARTESIAN_POINT('Ctrl Pts',(-13.4174952487419,13.5974242945969,
132.540719456061)) ;
#116643 = CARTESIAN_POINT('Ctrl Pts',(-13.4241801184799,13.3273252607923,
132.527199302951)) ;
#116644 = CARTESIAN_POINT('Ctrl Pts',(-13.4544637530165,13.0622912163539,
132.582375891631)) ;
#116645 = CARTESIAN_POINT('Ctrl Pts',(-13.506275683364,12.8256130939751,132.700784905767)) ;
#116646 = CARTESIAN_POINT('Ctrl Pts',(-13.5772613807945,12.6301799024571,
132.87500207775)) ;
#116647 = CARTESIAN_POINT('Ctrl Pts',(-13.6627580520996,12.4918476681471,
133.091661612145)) ;
#116648 = CARTESIAN_POINT('Ctrl Pts',(-13.7577512235869,12.4199209913987,
133.335951670398)) ;
#116649 = CARTESIAN_POINT('Ctrl Pts',(-13.8557964795529,12.4204245912294,
133.589185764803)) ;
#116650 = CARTESIAN_POINT('Ctrl Pts',(-13.9500806778918,12.4921595921641,
133.831642259008)) ;
#116651 = CARTESIAN_POINT('Ctrl Pts',(-14.0357484512663,12.6310172827489,
134.048715775205)) ;
#116652 = CARTESIAN_POINT('Ctrl Pts',(-14.106561882642,12.8262646896106,134.222494894414)) ;
#116653 = CARTESIAN_POINT('Ctrl Pts',(-14.1585280596083,13.0646913803179,
134.341142107312)) ;
#116654 = CARTESIAN_POINT('Ctrl Pts',(-14.1884677945267,13.3278244086872,
134.395572491973)) ;
#116655 = CARTESIAN_POINT('Ctrl Pts',(-14.1950850105529,13.5998585157466,
134.381605937844)) ;
#116656 = CARTESIAN_POINT('Ctrl Pts',(-14.1785645598048,13.8569826798842,
134.300338480903)) ;
#116657 = CARTESIAN_POINT('Ctrl Pts',(-14.1407900933548,14.0842218842957,
134.156820745803)) ;
#116658 = CARTESIAN_POINT('Ctrl Pts',(-14.0854221164694,14.2634335835668,
133.962037966108)) ;
#116659 = CARTESIAN_POINT('Ctrl Pts',(-14.0165549752706,14.3833954654661,
133.727598260658)) ;
#116660 = CARTESIAN_POINT('Ctrl Pts',(-13.9404490568541,14.4336980433791,
133.472126825684)) ;
#116661 = CARTESIAN_POINT('Ctrl Pts',(-13.8634700735141,14.4120157811793,
133.214261819804)) ;
#116662 = CARTESIAN_POINT('Ctrl Pts',(-13.7910288031297,14.3192946840505,
132.969450563142)) ;
#116663 = CARTESIAN_POINT('Ctrl Pts',(-13.7296882371886,14.1625583197416,
132.757157972999)) ;
#116664 = CARTESIAN_POINT('Ctrl Pts',(-13.6842292209281,13.9521768872698,
132.591146991905)) ;
#116665 = CARTESIAN_POINT('Ctrl Pts',(-13.6590028959702,13.7045477483084,
132.484357602539)) ;
#116666 = CARTESIAN_POINT('Ctrl Pts',(-13.6561784444072,13.4377490370904,
132.443119072094)) ;
#116667 = CARTESIAN_POINT('Ctrl Pts',(-13.6769260302992,13.1678476255433,
132.470479975427)) ;
#116668 = CARTESIAN_POINT('Ctrl Pts',(-13.7202606402325,12.9176590110113,
132.564014027659)) ;
#116669 = CARTESIAN_POINT('Ctrl Pts',(-13.7842663792317,12.7025601678247,
132.717748248745)) ;
#116670 = CARTESIAN_POINT('Ctrl Pts',(-13.8641216089752,12.5405894739356,
132.9180739667)) ;
#116671 = CARTESIAN_POINT('Ctrl Pts',(-13.9560307417598,12.4405287609816,
133.153363600866)) ;
#116672 = CARTESIAN_POINT('Ctrl Pts',(-14.0535698736063,12.4114132286229,
133.405122651663)) ;
#116673 = CARTESIAN_POINT('Ctrl Pts',(-14.150081341787,12.454644377757,133.654012283986)) ;
#116674 = CARTESIAN_POINT('Ctrl Pts',(-14.239925801091,12.5668919625006,133.883394142555)) ;
#116675 = CARTESIAN_POINT('Ctrl Pts',(-14.3176379666624,12.7415275985948,
134.077154579645)) ;
#116676 = CARTESIAN_POINT('Ctrl Pts',(-14.3775148527287,12.9638992642169,
134.219021942572)) ;
#116677 = CARTESIAN_POINT('Ctrl Pts',(-14.416625030145,13.2191082193463,134.300199660408)) ;
#116678 = CARTESIAN_POINT('Ctrl Pts',(-14.4328165454319,13.4893534284064,
134.314375207921)) ;
#116679 = CARTESIAN_POINT('Ctrl Pts',(-14.4255256959129,13.7553188201862,
134.259890989959)) ;
#116680 = CARTESIAN_POINT('Ctrl Pts',(-14.3960306585438,13.9971251061997,
134.140588389539)) ;
#116681 = CARTESIAN_POINT('Ctrl Pts',(-14.3471169142548,14.1977811038748,
133.964533561341)) ;
#116682 = CARTESIAN_POINT('Ctrl Pts',(-14.2834390765795,14.342451043168,133.745515157142)) ;
#116683 = CARTESIAN_POINT('Ctrl Pts',(-14.2092345380845,14.4220642715211,
133.495412056176)) ;
#116684 = CARTESIAN_POINT('Ctrl Pts',(-14.132069405725,14.4294491071756,133.237035382782)) ;
#116685 = CARTESIAN_POINT('Ctrl Pts',(-14.0570189069592,14.3652072705711,
132.984672203024)) ;
#116686 = CARTESIAN_POINT('Ctrl Pts',(-13.9905610685186,14.2335292315096,
132.757432925954)) ;
#116687 = CARTESIAN_POINT('Ctrl Pts',(-13.9379853069469,14.0429180682628,
132.570604385206)) ;
#116688 = CARTESIAN_POINT('Ctrl Pts',(-13.9042931419094,13.809322141679,132.439170793502)) ;
#116689 = CARTESIAN_POINT('Ctrl Pts',(-13.8920413663919,13.5476219044277,
132.370281900748)) ;
#116690 = CARTESIAN_POINT('Ctrl Pts',(-13.9033354204781,13.2750712862456,
132.369941141271)) ;
#116691 = CARTESIAN_POINT('Ctrl Pts',(-13.9375660928449,13.0163165161328,
132.437013069917)) ;
#116692 = CARTESIAN_POINT('Ctrl Pts',(-13.9935170806933,12.7846452326426,
132.567266996895)) ;
#116693 = CARTESIAN_POINT('Ctrl Pts',(-14.0674634744735,12.5995256932136,
132.750227603435)) ;
#116694 = CARTESIAN_POINT('Ctrl Pts',(-14.1555144396674,12.4726551815389,
132.974201835968)) ;
#116695 = CARTESIAN_POINT('Ctrl Pts',(-14.2511648890409,12.4145513483266,
133.220562650021)) ;
#116696 = CARTESIAN_POINT('Ctrl Pts',(-14.3489313214769,12.428469046116,133.473033644997)) ;
#116697 = CARTESIAN_POINT('Ctrl Pts',(-14.4422211554228,12.5133431382162,
133.712493183629)) ;
#116698 = CARTESIAN_POINT('Ctrl Pts',(-14.525697832764,12.664436679697,133.923074942934)) ;
#116699 = CARTESIAN_POINT('Ctrl Pts',(-14.5929092045224,12.8679925136389,
134.086485175352)) ;
#116700 = CARTESIAN_POINT('Ctrl Pts',(-14.6411040107999,13.1131689974074,
134.19403153726)) ;
#116701 = CARTESIAN_POINT('Ctrl Pts',(-14.6666810110784,13.3800002481821,
134.235609154939)) ;
#116702 = CARTESIAN_POINT('Ctrl Pts',(-14.6687870768603,13.6495651471469,
134.208652991586)) ;
#116703 = CARTESIAN_POINT('Ctrl Pts',(-14.6481856090904,13.9023388794203,
134.115460103099)) ;
#116704 = CARTESIAN_POINT('Ctrl Pts',(-14.60655186501,14.122657772282,133.960532567143)) ;
#116705 = CARTESIAN_POINT('Ctrl Pts',(-14.5484263911728,14.2908247523975,
133.757774272579)) ;
#116706 = CARTESIAN_POINT('Ctrl Pts',(-14.4779478810864,14.3981040608109,
133.518731235387)) ;
#116707 = CARTESIAN_POINT('Ctrl Pts',(-14.4009739960646,14.435262692703,133.260657337003)) ;
#116708 = CARTESIAN_POINT('Ctrl Pts',(-14.3241585125819,14.3995540237045,
133.003128791361)) ;
#116709 = CARTESIAN_POINT('Ctrl Pts',(-14.2538096107005,14.2948938625941,
132.764663780773)) ;
#116710 = CARTESIAN_POINT('Ctrl Pts',(-14.1946882431415,14.1259509671256,
132.558599866101)) ;
#116711 = CARTESIAN_POINT('Ctrl Pts',(-14.1530855073718,13.908522649266,132.404086330448)) ;
#116712 = CARTESIAN_POINT('Ctrl Pts',(-14.1318304371245,13.6557404743469,
132.308879501732)) ;
#116713 = CARTESIAN_POINT('Ctrl Pts',(-14.133357452909,13.3866405652258,132.280280185455)) ;
#116714 = CARTESIAN_POINT('Ctrl Pts',(-14.1586230794445,13.1181024502092,
132.320757015806)) ;
#116715 = CARTESIAN_POINT('Ctrl Pts',(-14.205870750163,12.8743683126388,132.425842572683)) ;
#116716 = CARTESIAN_POINT('Ctrl Pts',(-14.273163571627,12.667995764075,132.589221439612)) ;
#116717 = CARTESIAN_POINT('Ctrl Pts',(-14.3559649810851,12.5164144284275,
132.798000513578)) ;
#116718 = CARTESIAN_POINT('Ctrl Pts',(-14.4492350728485,12.4295970392297,
133.037335011155)) ;
#116719 = CARTESIAN_POINT('Ctrl Pts',(-14.5469842766314,12.4140261285354,
133.289756077204)) ;
#116720 = CARTESIAN_POINT('Ctrl Pts',(-14.6429502867745,12.4707103016775,
133.536966230591)) ;
#116721 = CARTESIAN_POINT('Ctrl Pts',(-14.7309816493984,12.5959067650868,
133.760973594387)) ;
#116722 = CARTESIAN_POINT('Ctrl Pts',(-14.8051894304306,12.7791141929297,
133.944779681145)) ;
#116723 = CARTESIAN_POINT('Ctrl Pts',(-14.8619602274572,13.0114292224114,
134.07721183711)) ;
#116724 = CARTESIAN_POINT('Ctrl Pts',(-14.8965056574982,13.2689898399713,
134.145309850726)) ;
#116725 = CARTESIAN_POINT('Ctrl Pts',(-14.9083557189504,13.5409256282928,
134.146659285362)) ;
#116726 = CARTESIAN_POINT('Ctrl Pts',(-14.8967214619315,13.8029839862651,
134.079595640576)) ;
#116727 = CARTESIAN_POINT('Ctrl Pts',(-14.8633027813701,14.038560788847,133.948790636524)) ;
#116728 = CARTESIAN_POINT('Ctrl Pts',(-14.8113056824054,14.2294230403712,
133.763800964968)) ;
#116729 = CARTESIAN_POINT('Ctrl Pts',(-14.7451795001818,14.3627051094246,
133.5375393849)) ;
#116730 = CARTESIAN_POINT('Ctrl Pts',(-14.6702017629751,14.4288334049426,
133.285362852041)) ;
#116731 = CARTESIAN_POINT('Ctrl Pts',(-14.592683156035,14.4228924634038,133.025803055449)) ;
#116732 = CARTESIAN_POINT('Ctrl Pts',(-14.5185906675657,14.3451234718206,
132.776153366255)) ;
#116733 = CARTESIAN_POINT('Ctrl Pts',(-14.4543104706926,14.2008973362482,
132.555187148786)) ;
#116734 = CARTESIAN_POINT('Ctrl Pts',(-14.4053408850151,14.0023960855746,
132.379171294356)) ;
#116735 = CARTESIAN_POINT('Ctrl Pts',(-14.3753108185381,13.7610318696562,
132.258251275988)) ;
#116736 = CARTESIAN_POINT('Ctrl Pts',(-14.3674916680807,13.4967570532622,
132.202394155313)) ;
#116737 = CARTESIAN_POINT('Ctrl Pts',(-14.3830668644292,13.2257686273763,
132.214689433479)) ;
#116738 = CARTESIAN_POINT('Ctrl Pts',(-14.4216910972161,12.9695426801037,
132.294399307209)) ;
#116739 = CARTESIAN_POINT('Ctrl Pts',(-14.4813916484494,12.7456272140063,
132.435636164476)) ;
#116740 = CARTESIAN_POINT('Ctrl Pts',(-14.5581647215385,12.5709695556374,
132.626903642083)) ;
#116741 = CARTESIAN_POINT('Ctrl Pts',(-14.6480148950082,12.4565179199043,
132.856192443771)) ;
#116742 = CARTESIAN_POINT('Ctrl Pts',(-14.7445907682789,12.4114773768948,
133.105225955903)) ;
#116743 = CARTESIAN_POINT('Ctrl Pts',(-14.842595675186,12.4394645441859,133.358192549628)) ;
#116744 = CARTESIAN_POINT('Ctrl Pts',(-14.9338942089909,12.5368906975998,
133.592009053689)) ;
#116745 = CARTESIAN_POINT('Ctrl Pts',(-15.0149505022409,12.6994727132711,
133.795457044531)) ;
#116746 = CARTESIAN_POINT('Ctrl Pts',(-15.0786566558626,12.911284387256,133.948692029528)) ;
#116747 = CARTESIAN_POINT('Ctrl Pts',(-15.1229382273336,13.1634090150243,
134.044638248895)) ;
#116748 = CARTESIAN_POINT('Ctrl Pts',(-15.1439035555132,13.43009560959,134.073018366311)) ;
#116749 = CARTESIAN_POINT('Ctrl Pts',(-15.1418047731794,13.6985487058695,
134.033731705758)) ;
#116750 = CARTESIAN_POINT('Ctrl Pts',(-15.1167802714419,13.9480246666546,
133.927350353256)) ;
#116751 = CARTESIAN_POINT('Ctrl Pts',(-15.0720912700265,14.1576527817006,
133.763864153658)) ;
#116752 = CARTESIAN_POINT('Ctrl Pts',(-15.0109964235137,14.3162850148807,
133.552216483996)) ;
#116753 = CARTESIAN_POINT('Ctrl Pts',(-14.9387740010428,14.4106899860489,
133.308061015579)) ;
#116754 = CARTESIAN_POINT('Ctrl Pts',(-14.8613476917878,14.4339585124651,
133.048676571636)) ;
#116755 = CARTESIAN_POINT('Ctrl Pts',(-14.7856037318579,14.3853107733964,
132.794458393841)) ;
#116756 = CARTESIAN_POINT('Ctrl Pts',(-14.7163978676272,14.2669554463922,
132.558995140207)) ;
#116757 = CARTESIAN_POINT('Ctrl Pts',(-14.6606048304255,14.0883946272744,
132.362895619543)) ;
#116758 = CARTESIAN_POINT('Ctrl Pts',(-14.622541821991,13.8631868173472,132.218696170198)) ;
#116759 = CARTESIAN_POINT('Ctrl Pts',(-14.6054425239062,13.6057121370264,
132.135619590578)) ;
#116760 = CARTESIAN_POINT('Ctrl Pts',(-14.6114571502439,13.3350529276947,
132.120057688217)) ;
#116761 = CARTESIAN_POINT('Ctrl Pts',(-14.6409008769268,13.070755438595,132.172936727227)) ;
#116762 = CARTESIAN_POINT('Ctrl Pts',(-14.6921558771164,12.8321487482004,
132.289616780284)) ;
#116763 = CARTESIAN_POINT('Ctrl Pts',(-14.7630571786097,12.6344630496442,
132.46342517127)) ;
#116764 = CARTESIAN_POINT('Ctrl Pts',(-14.8478315319079,12.4951762287069,
132.678132083268)) ;
#116765 = CARTESIAN_POINT('Ctrl Pts',(-14.942435880663,12.4210996304978,132.921347561675)) ;
#116766 = CARTESIAN_POINT('Ctrl Pts',(-15.0405912621457,12.4192964067175,
133.174865728553)) ;
#116767 = CARTESIAN_POINT('Ctrl Pts',(-15.1352752169109,12.4890491878224,
133.418419532976)) ;
#116768 = CARTESIAN_POINT('Ctrl Pts',(-15.2215420412865,12.6268326334366,
133.63712537635)) ;
#116769 = CARTESIAN_POINT('Ctrl Pts',(-15.2924017249557,12.819583008208,133.811231474629)) ;
#116770 = CARTESIAN_POINT('Ctrl Pts',(-15.3450997694842,13.0571001381562,
133.93198280672)) ;
#116771 = CARTESIAN_POINT('Ctrl Pts',(-15.3757107378913,13.3202804831109,
133.988310681278)) ;
#116772 = CARTESIAN_POINT('Ctrl Pts',(-15.383035487643,13.5914915741981,133.976525348511)) ;
#116773 = CARTESIAN_POINT('Ctrl Pts',(-15.3670672892394,13.8505565623955,
133.896697391881)) ;
#116774 = CARTESIAN_POINT('Ctrl Pts',(-15.3300175768013,14.0777828680815,
133.755460891241)) ;
#116775 = CARTESIAN_POINT('Ctrl Pts',(-15.2750239975421,14.2590885920228,
133.561696857871)) ;
#116776 = CARTESIAN_POINT('Ctrl Pts',(-15.2065269555632,14.3807166711332,
133.328376960357)) ;
#116777 = CARTESIAN_POINT('Ctrl Pts',(-15.1306232310638,14.433343609964,133.073523056504)) ;
#116778 = CARTESIAN_POINT('Ctrl Pts',(-15.0530845875344,14.4133893696398,
132.813800939999)) ;
#116779 = CARTESIAN_POINT('Ctrl Pts',(-14.9808883290291,14.322997838196,132.569914498955)) ;
#116780 = CARTESIAN_POINT('Ctrl Pts',(-14.9190772112434,14.1680350352392,
132.356220049076)) ;
#116781 = CARTESIAN_POINT('Ctrl Pts',(-14.8731819599279,13.9594348156913,
132.189002061103)) ;
#116782 = CARTESIAN_POINT('Ctrl Pts',(-14.8471967295744,13.7128291975183,
132.079998756728)) ;
#116783 = CARTESIAN_POINT('Ctrl Pts',(-14.8437841989435,13.4442543437845,
132.036783194096)) ;
#116784 = CARTESIAN_POINT('Ctrl Pts',(-14.8636402089109,13.1766944137287,
132.061867124773)) ;
#116785 = CARTESIAN_POINT('Ctrl Pts',(-14.9067034374907,12.9234094680339,
132.154300428)) ;
#116786 = CARTESIAN_POINT('Ctrl Pts',(-14.9698154804404,12.7086523131788,
132.305653046529)) ;
#116787 = CARTESIAN_POINT('Ctrl Pts',(-15.0493208194513,12.5444332770708,
132.504896693896)) ;
#116788 = CARTESIAN_POINT('Ctrl Pts',(-15.1413379063356,12.442265427868,132.740384202576)) ;
#116789 = CARTESIAN_POINT('Ctrl Pts',(-15.2383898734991,12.4113238221151,
132.990859260472)) ;
#116790 = CARTESIAN_POINT('Ctrl Pts',(-15.3350927075092,12.4521999804418,
133.240286707603)) ;
#116791 = CARTESIAN_POINT('Ctrl Pts',(-15.4257173250681,12.5635389839908,
133.471744679301)) ;
#116792 = CARTESIAN_POINT('Ctrl Pts',(-15.5032411736603,12.7354102486573,
133.665205731719)) ;
#116793 = CARTESIAN_POINT('Ctrl Pts',(-15.5638610806042,12.9568497903179,
133.809176375546)) ;
#116794 = CARTESIAN_POINT('Ctrl Pts',(-15.6036470774416,13.2117694204113,
133.892283046633)) ;
#116795 = CARTESIAN_POINT('Ctrl Pts',(-15.6204942624616,13.4825284434545,
133.908293488513)) ;
#116796 = CARTESIAN_POINT('Ctrl Pts',(-15.6137728672592,13.7484828360667,
133.855517701894)) ;
#116797 = CARTESIAN_POINT('Ctrl Pts',(-15.5850166523139,13.990067054495,133.738525504946)) ;
#116798 = CARTESIAN_POINT('Ctrl Pts',(-15.536763965292,14.1922208547519,133.564439930301)) ;
#116799 = CARTESIAN_POINT('Ctrl Pts',(-15.4730487748542,14.3393855053723,
133.34511245468)) ;
#116800 = CARTESIAN_POINT('Ctrl Pts',(-15.399695343259,14.42040771759,133.09778751226)) ;
#116801 = CARTESIAN_POINT('Ctrl Pts',(-15.3221538787493,14.4304302239803,
132.838134252815)) ;
#116802 = CARTESIAN_POINT('Ctrl Pts',(-15.2467193227142,14.3678711876826,
132.58455206021)) ;
#116803 = CARTESIAN_POINT('Ctrl Pts',(-15.1799138507876,14.2376928211799,
132.356266335115)) ;
#116804 = CARTESIAN_POINT('Ctrl Pts',(-15.1270449347704,14.0489884118596,
132.168670045221)) ;
#116805 = CARTESIAN_POINT('Ctrl Pts',(-15.0927077016124,13.8164457415788,
132.035344800608)) ;
#116806 = CARTESIAN_POINT('Ctrl Pts',(-15.0799009992238,13.5541090228178,
131.964694386055)) ;
#116807 = CARTESIAN_POINT('Ctrl Pts',(-15.0903290157032,13.2846773793449,
131.962212925334)) ;
#116808 = CARTESIAN_POINT('Ctrl Pts',(-15.1240864041073,13.0230236388571,
132.02761116478)) ;
#116809 = CARTESIAN_POINT('Ctrl Pts',(-15.1793905460716,12.7908728134741,
132.156056831622)) ;
#116810 = CARTESIAN_POINT('Ctrl Pts',(-15.2530252671634,12.6038718896903,
132.338032999174)) ;
#116811 = CARTESIAN_POINT('Ctrl Pts',(-15.3404395281791,12.4755978547321,
132.560270582577)) ;
#116812 = CARTESIAN_POINT('Ctrl Pts',(-15.4361666301176,12.4151865518673,
132.806771124844)) ;
#116813 = CARTESIAN_POINT('Ctrl Pts',(-15.5338464527214,12.4270410419496,
133.059031997262)) ;
#116814 = CARTESIAN_POINT('Ctrl Pts',(-15.6273514722291,12.5098502218198,
133.299118129625)) ;
#116815 = CARTESIAN_POINT('Ctrl Pts',(-15.7111748136664,12.6589865553575,
133.510736241021)) ;
#116816 = CARTESIAN_POINT('Ctrl Pts',(-15.7790199467508,12.8615686437882,
133.675932015432)) ;
#116817 = CARTESIAN_POINT('Ctrl Pts',(-15.8277028915331,13.1050265779988,
133.785011642684)) ;
#116818 = CARTESIAN_POINT('Ctrl Pts',(-15.854027088166,13.3718443264194,133.828716982132)) ;
#116819 = CARTESIAN_POINT('Ctrl Pts',(-15.856910626616,13.6411903783996,133.804094970037)) ;
#116820 = CARTESIAN_POINT('Ctrl Pts',(-15.8366684723925,13.896863473321,133.711645717659)) ;
#116821 = CARTESIAN_POINT('Ctrl Pts',(-15.7960112831063,14.1159779541294,
133.559939274363)) ;
#116822 = CARTESIAN_POINT('Ctrl Pts',(-15.737913899012,14.287325692981,133.356994933494)) ;
#116823 = CARTESIAN_POINT('Ctrl Pts',(-15.6678321119962,14.3958947357892,
133.119202977711)) ;
#116824 = CARTESIAN_POINT('Ctrl Pts',(-15.5912113430045,14.435126510394,132.862258941414)) ;
#116825 = CARTESIAN_POINT('Ctrl Pts',(-15.5143394894088,14.4019578679091,
132.604594883037)) ;
#116826 = CARTESIAN_POINT('Ctrl Pts',(-15.4432379820011,14.298265208763,132.363682618734)) ;
#116827 = CARTESIAN_POINT('Ctrl Pts',(-15.3842287146298,14.1324802055206,
132.158250825652)) ;
#116828 = CARTESIAN_POINT('Ctrl Pts',(-15.3417783503285,13.915462828794,132.001092130861)) ;
#116829 = CARTESIAN_POINT('Ctrl Pts',(-15.319910313068,13.663371252365,131.904098346542)) ;
#116830 = CARTESIAN_POINT('Ctrl Pts',(-15.320806233112,13.3940849584222,131.873601342427)) ;
#116831 = CARTESIAN_POINT('Ctrl Pts',(-15.3452532949719,13.1263052968225,
131.911831826463)) ;
#116832 = CARTESIAN_POINT('Ctrl Pts',(-15.3921146290371,12.8804158989885,
132.015615977984)) ;
#116833 = CARTESIAN_POINT('Ctrl Pts',(-15.4587394301298,12.6733663230833,
132.177140209864)) ;
#116834 = CARTESIAN_POINT('Ctrl Pts',(-15.5412767697681,12.5197379443073,
132.385092289547)) ;
#116835 = CARTESIAN_POINT('Ctrl Pts',(-15.6343686383594,12.4310982287018,
132.623899504288)) ;
#116836 = CARTESIAN_POINT('Ctrl Pts',(-15.7318070432573,12.413462824637,132.875502765111)) ;
#116837 = CARTESIAN_POINT('Ctrl Pts',(-15.8280059948747,12.4679867146693,
133.123364071303)) ;
#116838 = CARTESIAN_POINT('Ctrl Pts',(-15.916556151159,12.5916525071464,133.348810603495)) ;
#116839 = CARTESIAN_POINT('Ctrl Pts',(-15.9911124965925,12.773468390421,133.533647244235)) ;
#116840 = CARTESIAN_POINT('Ctrl Pts',(-16.0481519771809,13.0028687582652,
133.667100411234)) ;
#116841 = CARTESIAN_POINT('Ctrl Pts',(-16.0837269854642,13.2619623581497,
133.737923863175)) ;
#116842 = CARTESIAN_POINT('Ctrl Pts',(-16.0961062506615,13.5340191309755,
133.740804033784)) ;
#116843 = CARTESIAN_POINT('Ctrl Pts',(-16.0851567800789,13.7955674320649,
133.675865201536)) ;
#116844 = CARTESIAN_POINT('Ctrl Pts',(-16.0523419685841,14.0322612851413,
133.546816470338)) ;
#116845 = CARTESIAN_POINT('Ctrl Pts',(-16.0009018123364,14.22438976877,133.363495292219)) ;
#116846 = CARTESIAN_POINT('Ctrl Pts',(-15.9350335261451,14.3598900784348,
133.137935317501)) ;
#116847 = CARTESIAN_POINT('Ctrl Pts',(-15.859872027803,14.4280176148554,132.885075302892)) ;
#116848 = CARTESIAN_POINT('Ctrl Pts',(-15.782828331798,14.4241023882727,132.627114452723)) ;
#116849 = CARTESIAN_POINT('Ctrl Pts',(-15.7083163890521,14.3482280503466,
132.376135467847)) ;
#116850 = CARTESIAN_POINT('Ctrl Pts',(-15.6438258833221,14.206072490763,132.154635276503)) ;
#116851 = CARTESIAN_POINT('Ctrl Pts',(-15.5942900234776,14.008680924911,131.976908199774)) ;
#116852 = CARTESIAN_POINT('Ctrl Pts',(-15.5636932851511,13.7691472453329,
131.85444476612)) ;
#116853 = CARTESIAN_POINT('Ctrl Pts',(-15.555160472364,13.5031161765621,131.796227500216)) ;
#116854 = CARTESIAN_POINT('Ctrl Pts',(-15.5701873565133,13.2327334709729,
131.807010775747)) ;
#116855 = CARTESIAN_POINT('Ctrl Pts',(-15.6080409619239,12.9767767271815,
131.884582975432)) ;
#116856 = CARTESIAN_POINT('Ctrl Pts',(-15.6670437728799,12.7518157779669,
132.023824499167)) ;
#116857 = CARTESIAN_POINT('Ctrl Pts',(-15.743706872708,12.5749030821108,132.214630826275)) ;
#116858 = CARTESIAN_POINT('Ctrl Pts',(-15.8331256984323,12.4587258790909,
132.442721035975)) ;
#116859 = CARTESIAN_POINT('Ctrl Pts',(-15.9300951754384,12.4118884075951,
132.692727681813)) ;
#116860 = CARTESIAN_POINT('Ctrl Pts',(-16.0268131871302,12.4371447896242,
132.942408691455)) ;
#116861 = CARTESIAN_POINT('Ctrl Pts',(-16.1194581635705,12.5335140110472,
133.17975745332)) ;
#116862 = CARTESIAN_POINT('Ctrl Pts',(-16.2002006821098,12.6929505579163,
133.382601408039)) ;
#116863 = CARTESIAN_POINT('Ctrl Pts',(-16.2650587042151,12.9053983605441,
133.538877628518)) ;
#116864 = CARTESIAN_POINT('Ctrl Pts',(-16.3094994650075,13.1539498809503,
133.635663755891)) ;
#116865 = CARTESIAN_POINT('Ctrl Pts',(-16.3314782918866,13.4226750852024,
133.666703127002)) ;
#116866 = CARTESIAN_POINT('Ctrl Pts',(-16.3299479186378,13.6910891488428,
133.629119729191)) ;
#116867 = CARTESIAN_POINT('Ctrl Pts',(-16.3055899550518,13.9413684449187,
133.524691151503)) ;
#116868 = CARTESIAN_POINT('Ctrl Pts',(-16.2613018501774,14.1526799175884,
133.362307720818)) ;
#116869 = CARTESIAN_POINT('Ctrl Pts',(-16.200685666699,14.3125333365339,133.152120048597)) ;
#116870 = CARTESIAN_POINT('Ctrl Pts',(-16.1289337339076,14.4088194545048,
132.909435999603)) ;
#116871 = CARTESIAN_POINT('Ctrl Pts',(-16.0512902573569,14.4343198922647,
132.649294671372)) ;
#116872 = CARTESIAN_POINT('Ctrl Pts',(-15.9755688396631,14.3877722216923,
132.395208079009)) ;
#116873 = CARTESIAN_POINT('Ctrl Pts',(-15.905996220698,14.2711471229662,132.158630019206)) ;
#116874 = CARTESIAN_POINT('Ctrl Pts',(-15.8499964373459,14.0951743050547,
131.962092155261)) ;
#116875 = CARTESIAN_POINT('Ctrl Pts',(-15.8111145068756,13.870335406886,131.815355861608)) ;
#116876 = CARTESIAN_POINT('Ctrl Pts',(-15.7933948348918,13.6128359937758,
131.730391952872)) ;
#116877 = CARTESIAN_POINT('Ctrl Pts',(-15.798756317796,13.3431053830175,131.71301861056)) ;
#116878 = CARTESIAN_POINT('Ctrl Pts',(-15.8274126253614,13.0784070527184,
131.763618606217)) ;
#116879 = CARTESIAN_POINT('Ctrl Pts',(-15.8785782774498,12.8371326222925,
131.879774862779)) ;
#116880 = CARTESIAN_POINT('Ctrl Pts',(-15.9483653149359,12.6399916348322,
132.050644310464)) ;
#116881 = CARTESIAN_POINT('Ctrl Pts',(-16.0331828514141,12.4979353055065,
132.265299850434)) ;
#116882 = CARTESIAN_POINT('Ctrl Pts',(-16.1278387494795,12.4220838760127,
132.508600246006)) ;
#116883 = CARTESIAN_POINT('Ctrl Pts',(-16.2257839895642,12.4184701174221,
132.761571575606)) ;
#116884 = CARTESIAN_POINT('Ctrl Pts',(-16.3203051085462,12.4860424298892,
133.004761298642)) ;
#116885 = CARTESIAN_POINT('Ctrl Pts',(-16.4067012578865,12.6212969688775,
133.223947844078)) ;
#116886 = CARTESIAN_POINT('Ctrl Pts',(-16.4784451122272,12.8133838986541,
133.400475111834)) ;
#116887 = CARTESIAN_POINT('Ctrl Pts',(-16.5317455281392,13.0503648242526,
133.522937144078)) ;
#116888 = CARTESIAN_POINT('Ctrl Pts',(-16.562904036609,13.3123036510868,133.58095920928)) ;
#116889 = CARTESIAN_POINT('Ctrl Pts',(-16.5709394990535,13.583277796962,133.571284430359)) ;
#116890 = CARTESIAN_POINT('Ctrl Pts',(-16.5556961065435,13.8428842825667,
133.493592881486)) ;
#116891 = CARTESIAN_POINT('Ctrl Pts',(-16.5191174489348,14.0720012464851,
133.353626853518)) ;
#116892 = CARTESIAN_POINT('Ctrl Pts',(-16.4645826787132,14.2546155052048,
133.16122511799)) ;
#116893 = CARTESIAN_POINT('Ctrl Pts',(-16.3965867046521,14.3779471220683,
132.929452933279)) ;
#116894 = CARTESIAN_POINT('Ctrl Pts',(-16.3207208376577,14.43277854508,132.674661781709)) ;
#116895 = CARTESIAN_POINT('Ctrl Pts',(-16.2433872066106,14.415204860474,132.415650965892)) ;
#116896 = CARTESIAN_POINT('Ctrl Pts',(-16.1706126792223,14.3266409888288,
132.169926667865)) ;
#116897 = CARTESIAN_POINT('Ctrl Pts',(-16.1083393228608,14.1729215219676,
131.954821567221)) ;
#116898 = CARTESIAN_POINT('Ctrl Pts',(-16.0620759324473,13.9662155734193,
131.786622134201)) ;
#116899 = CARTESIAN_POINT('Ctrl Pts',(-16.0354545331854,13.7208187019913,
131.675794589115)) ;
#116900 = CARTESIAN_POINT('Ctrl Pts',(-16.031310568843,13.4521886901424,131.630394366892)) ;
#116901 = CARTESIAN_POINT('Ctrl Pts',(-16.0506012298629,13.1838897555981,
131.653758282559)) ;
#116902 = CARTESIAN_POINT('Ctrl Pts',(-16.092732570887,12.9313138708941,131.743671378859)) ;
#116903 = CARTESIAN_POINT('Ctrl Pts',(-16.1554610604641,12.7142071151624,
131.893770222467)) ;
#116904 = CARTESIAN_POINT('Ctrl Pts',(-16.2347719855931,12.548182284736,132.092377316928)) ;
#116905 = CARTESIAN_POINT('Ctrl Pts',(-16.3260094928037,12.4445945488069,
132.325771295417)) ;
#116906 = CARTESIAN_POINT('Ctrl Pts',(-16.423061481813,12.4110615295413,132.576214245398)) ;
#116907 = CARTESIAN_POINT('Ctrl Pts',(-16.5203214945035,12.4502003407784,
132.827110054199)) ;
#116908 = CARTESIAN_POINT('Ctrl Pts',(-16.6105992456112,12.558798155004,133.057786090289)) ;
#116909 = CARTESIAN_POINT('Ctrl Pts',(-16.6888731564621,12.7290992906361,
133.253347731538)) ;
#116910 = CARTESIAN_POINT('Ctrl Pts',(-16.750323465089,12.9505642772134,133.399574934352)) ;
#116911 = CARTESIAN_POINT('Ctrl Pts',(-16.7905447407979,13.2039533601212,
133.484067750218)) ;
#116912 = CARTESIAN_POINT('Ctrl Pts',(-16.808103774948,13.4737768024146,133.502245809363)) ;
#116913 = CARTESIAN_POINT('Ctrl Pts',(-16.8021327956016,13.7408243075777,
133.451586700857)) ;
#116914 = CARTESIAN_POINT('Ctrl Pts',(-16.7737748215047,13.984382806197,133.335598519286)) ;
#116915 = CARTESIAN_POINT('Ctrl Pts',(-16.7262493219245,14.1867700036955,
133.163813020196)) ;
#116916 = CARTESIAN_POINT('Ctrl Pts',(-16.6628687750783,14.3360222992997,
132.945422090007)) ;
#116917 = CARTESIAN_POINT('Ctrl Pts',(-16.5897103505964,14.419030482185,132.698666801288)) ;
#116918 = CARTESIAN_POINT('Ctrl Pts',(-16.51221019719,14.4311357445316,132.43913622336)) ;
#116919 = CARTESIAN_POINT('Ctrl Pts',(-16.4367353245665,14.3708888244175,
132.185495743383)) ;
#116920 = CARTESIAN_POINT('Ctrl Pts',(-16.3694821265528,14.242292745065,131.955833156551)) ;
#116921 = CARTESIAN_POINT('Ctrl Pts',(-16.3163383080254,14.0562620175223,
131.767605594611)) ;
#116922 = CARTESIAN_POINT('Ctrl Pts',(-16.2811251005187,13.8231737937943,
131.631475169058)) ;
#116923 = CARTESIAN_POINT('Ctrl Pts',(-16.2677486292964,13.5622217788933,
131.559277105701)) ;
#116924 = CARTESIAN_POINT('Ctrl Pts',(-16.2774948188854,13.2923511462151,
131.554743523811)) ;
#116925 = CARTESIAN_POINT('Ctrl Pts',(-16.3104849708693,13.0307857162003,
131.617989399722)) ;
#116926 = CARTESIAN_POINT('Ctrl Pts',(-16.365373545646,12.7967159869363,131.745103480781)) ;
#116927 = CARTESIAN_POINT('Ctrl Pts',(-16.4385204924337,12.6083943270826,
131.925677858349)) ;
#116928 = CARTESIAN_POINT('Ctrl Pts',(-16.5257030828109,12.4782667432663,
132.147207427787)) ;
#116929 = CARTESIAN_POINT('Ctrl Pts',(-16.6209595515756,12.4160107733854,
132.392442931131)) ;
#116930 = CARTESIAN_POINT('Ctrl Pts',(-16.7189196059942,12.425588900326,132.645438963958)) ;
#116931 = CARTESIAN_POINT('Ctrl Pts',(-16.812966966938,12.5070742961233,132.886977697143)) ;
#116932 = CARTESIAN_POINT('Ctrl Pts',(-16.8967106834322,12.6538727227807,
133.098529303095)) ;
#116933 = CARTESIAN_POINT('Ctrl Pts',(-16.965192001625,12.8553498973186,133.265526413072)) ;
#116934 = CARTESIAN_POINT('Ctrl Pts',(-17.0144739641916,13.0981033261267,
133.376337583619)) ;
#116935 = CARTESIAN_POINT('Ctrl Pts',(-17.0414310098506,13.3649637765944,
133.421842396641)) ;
#116936 = CARTESIAN_POINT('Ctrl Pts',(-17.0448923056262,13.6334093866667,
133.3990331273)) ;
#116937 = CARTESIAN_POINT('Ctrl Pts',(-17.0255067032329,13.8886868084012,
133.309248012564)) ;
#116938 = CARTESIAN_POINT('Ctrl Pts',(-16.9852265152679,14.1104518117265,
133.158447905506)) ;
#116939 = CARTESIAN_POINT('Ctrl Pts',(-16.9275341963761,14.2832226170572,
132.956697371245)) ;
#116940 = CARTESIAN_POINT('Ctrl Pts',(-16.8577706859408,14.3937886197238,
132.719848790466)) ;
#116941 = CARTESIAN_POINT('Ctrl Pts',(-16.78089628133,14.4350213819736,132.462014367155)) ;
#116942 = CARTESIAN_POINT('Ctrl Pts',(-16.7043149562872,14.4038716569565,
132.205357182892)) ;
#116943 = CARTESIAN_POINT('Ctrl Pts',(-16.6328354464211,14.3020574397598,
131.963287583542)) ;
#116944 = CARTESIAN_POINT('Ctrl Pts',(-16.5734391248213,14.1377082667359,
131.756716566826)) ;
#116945 = CARTESIAN_POINT('Ctrl Pts',(-16.5305427209279,13.922512079821,131.598336680433)) ;
#116946 = CARTESIAN_POINT('Ctrl Pts',(-16.507982405518,13.6705375109782,131.499234166552)) ;
#116947 = CARTESIAN_POINT('Ctrl Pts',(-16.5082708749943,13.4018845306058,
131.467013585173)) ;
#116948 = CARTESIAN_POINT('Ctrl Pts',(-16.5319013398505,13.1344381767143,
131.502948161611)) ;
#116949 = CARTESIAN_POINT('Ctrl Pts',(-16.5783956200005,12.8864833216457,
131.605492726989)) ;
#116950 = CARTESIAN_POINT('Ctrl Pts',(-16.6441694983151,12.6791960458196,
131.764705926375)) ;
#116951 = CARTESIAN_POINT('Ctrl Pts',(-16.726432219592,12.5233811558849,131.971789575967)) ;
#116952 = CARTESIAN_POINT('Ctrl Pts',(-16.819171376903,12.4327816680599,132.209612016199)) ;
#116953 = CARTESIAN_POINT('Ctrl Pts',(-16.9168669847768,12.412915954978,132.461862014984)) ;
#116954 = CARTESIAN_POINT('Ctrl Pts',(-17.0130810554034,12.4655032606852,
132.709804508519)) ;
#116955 = CARTESIAN_POINT('Ctrl Pts',(-17.1016552917455,12.5866528980437,
132.935438549739)) ;
#116956 = CARTESIAN_POINT('Ctrl Pts',(-17.1770183654666,12.7674395130523,
133.122503206209)) ;
#116957 = CARTESIAN_POINT('Ctrl Pts',(-17.2347578061268,12.996680662144,133.257885737137)) ;
#116958 = CARTESIAN_POINT('Ctrl Pts',(-17.2707418868054,13.2541240952596,
133.33004341912)) ;
#116959 = CARTESIAN_POINT('Ctrl Pts',(-17.2838680119121,13.5248420441081,
133.335259727289)) ;
#116960 = CARTESIAN_POINT('Ctrl Pts',(-17.2736087985316,13.7882270430707,
133.272175979222)) ;
#116961 = CARTESIAN_POINT('Ctrl Pts',(-17.2413405150168,14.026098281457,133.144700506367)) ;
#116962 = CARTESIAN_POINT('Ctrl Pts',(-17.1902557486675,14.220023125983,132.962349683833)) ;
#116963 = CARTESIAN_POINT('Ctrl Pts',(-17.12483319593,14.3567721922805,132.738164016465)) ;
#116964 = CARTESIAN_POINT('Ctrl Pts',(-17.0503040398658,14.4269174319569,
132.487342101643)) ;
#116965 = CARTESIAN_POINT('Ctrl Pts',(-16.972658858244,14.4252573107259,132.22736950121)) ;
#116966 = CARTESIAN_POINT('Ctrl Pts',(-16.8981739750149,14.3512845156984,
131.976555512661)) ;
#116967 = CARTESIAN_POINT('Ctrl Pts',(-16.8335398285555,14.2117350890935,
131.754763421916)) ;
#116968 = CARTESIAN_POINT('Ctrl Pts',(-16.7832370832045,14.0152549017169,
131.574673760724)) ;
#116969 = CARTESIAN_POINT('Ctrl Pts',(-16.7520262621574,13.7756400409677,
131.450290290216)) ;
#116970 = CARTESIAN_POINT('Ctrl Pts',(-16.7428846424837,13.512293601297,131.390573199531)) ;
#116971 = CARTESIAN_POINT('Ctrl Pts',(-16.7571174189924,13.24113011058,131.398952116168)) ;
#116972 = CARTESIAN_POINT('Ctrl Pts',(-16.7943670713977,12.9839533998787,
131.474699240851)) ;
#116973 = CARTESIAN_POINT('Ctrl Pts',(-16.8530367769723,12.757224045122,131.612859940048)) ;
#116974 = CARTESIAN_POINT('Ctrl Pts',(-16.9289336870903,12.5794741736853,
131.801571530647)) ;
#116975 = CARTESIAN_POINT('Ctrl Pts',(-17.0182778782105,12.4611210903509,
132.029356074653)) ;
#116976 = CARTESIAN_POINT('Ctrl Pts',(-17.1146160701368,12.4122668276836,
132.277695181808)) ;
#116977 = CARTESIAN_POINT('Ctrl Pts',(-17.2121033058066,12.4354395008957,
132.529381521733)) ;
#116978 = CARTESIAN_POINT('Ctrl Pts',(-17.3049234321536,12.5301694700227,
132.767254707327)) ;
#116979 = CARTESIAN_POINT('Ctrl Pts',(-17.3858637794653,12.6876686468163,
132.970742976347)) ;
#116980 = CARTESIAN_POINT('Ctrl Pts',(-17.4511566609569,12.8982124507683,
133.128366185446)) ;
#116981 = CARTESIAN_POINT('Ctrl Pts',(-17.4964430877249,13.1472879171854,
133.227443906338)) ;
#116982 = CARTESIAN_POINT('Ctrl Pts',(-17.5189530226261,13.4151706330379,
133.260112246192)) ;
#116983 = CARTESIAN_POINT('Ctrl Pts',(-17.5180772977572,13.6833052761831,
133.224500236615)) ;
#116984 = CARTESIAN_POINT('Ctrl Pts',(-17.494562648909,13.9335262221531,133.122676890144)) ;
#116985 = CARTESIAN_POINT('Ctrl Pts',(-17.4504518079917,14.1479664879784,
132.960528520529)) ;
#116986 = CARTESIAN_POINT('Ctrl Pts',(-17.3903547316673,14.3087959148104,
132.751961242652)) ;
#116987 = CARTESIAN_POINT('Ctrl Pts',(-17.3188588627773,14.4069520206095,
132.510023786694)) ;
#116988 = CARTESIAN_POINT('Ctrl Pts',(-17.2416470088105,14.4347039368911,
132.251304094887)) ;
#116989 = CARTESIAN_POINT('Ctrl Pts',(-17.1652862735102,14.3899170830749,
131.995115519734)) ;
#116990 = CARTESIAN_POINT('Ctrl Pts',(-17.0958542528533,14.2758481997907,
131.759156683175)) ;
#116991 = CARTESIAN_POINT('Ctrl Pts',(-17.0391474079491,14.1010294693846,
131.560425945483)) ;
#116992 = CARTESIAN_POINT('Ctrl Pts',(-16.9997289321043,13.8772034754541,
131.412115133594)) ;
#116993 = CARTESIAN_POINT('Ctrl Pts',(-16.9813814044527,13.6206147826081,
131.325344173753)) ;
#116994 = CARTESIAN_POINT('Ctrl Pts',(-16.9860373202625,13.3509222115741,
131.305902124102)) ;
#116995 = CARTESIAN_POINT('Ctrl Pts',(-17.0141429076236,13.0853829719641,
131.354833697986)) ;
#116996 = CARTESIAN_POINT('Ctrl Pts',(-17.0643516475666,12.8445476848772,
131.468399606912)) ;
#116997 = CARTESIAN_POINT('Ctrl Pts',(-17.1338580586174,12.644952930344,131.638309780535)) ;
#116998 = CARTESIAN_POINT('Ctrl Pts',(-17.2183241864262,12.5012606918104,
131.851948185352)) ;
#116999 = CARTESIAN_POINT('Ctrl Pts',(-17.3124481152622,12.4235056732711,
132.09380438388)) ;
#117000 = CARTESIAN_POINT('Ctrl Pts',(-17.4104141135003,12.417318606479,132.346827753117)) ;
#117001 = CARTESIAN_POINT('Ctrl Pts',(-17.5056867648447,12.4833714427519,
132.592005351237)) ;
#117002 = CARTESIAN_POINT('Ctrl Pts',(-17.5919987183341,12.6162285125256,
132.811106229032)) ;
#117003 = CARTESIAN_POINT('Ctrl Pts',(-17.6644873151439,12.8073409623945,
132.989699975671)) ;
#117004 = CARTESIAN_POINT('Ctrl Pts',(-17.7183030404906,13.0432164497969,
133.113690694589)) ;
#117005 = CARTESIAN_POINT('Ctrl Pts',(-17.7501392643195,13.3046948495717,
133.173683613056)) ;
#117006 = CARTESIAN_POINT('Ctrl Pts',(-17.7588282011811,13.5764462618644,
133.165829921335)) ;
#117007 = CARTESIAN_POINT('Ctrl Pts',(-17.7441367232311,13.8363549423102,
133.089774039034)) ;
#117008 = CARTESIAN_POINT('Ctrl Pts',(-17.7083001328226,14.0655921172455,
132.952119497934)) ;
#117009 = CARTESIAN_POINT('Ctrl Pts',(-17.654103302564,14.2503953829721,132.760609433254)) ;
#117010 = CARTESIAN_POINT('Ctrl Pts',(-17.5861690172399,14.3757153759899,
132.528919395928)) ;
#117011 = CARTESIAN_POINT('Ctrl Pts',(-17.5105676394246,14.4321659861442,
132.274963313804)) ;
#117012 = CARTESIAN_POINT('Ctrl Pts',(-17.4334463905001,14.4167343147861,
132.016680455663)) ;
#117013 = CARTESIAN_POINT('Ctrl Pts',(-17.3604705956701,14.3302900075088,
131.770378332866)) ;
#117014 = CARTESIAN_POINT('Ctrl Pts',(-17.297751311033,14.1784243814557,131.55396233599)) ;
#117015 = CARTESIAN_POINT('Ctrl Pts',(-17.2507585604563,13.971750794682,131.38344223631)) ;
#117016 = CARTESIAN_POINT('Ctrl Pts',(-17.2237636735663,13.7284357059757,
131.271702420089)) ;
#117017 = CARTESIAN_POINT('Ctrl Pts',(-17.2188332794065,13.4606302027768,
131.224056001737)) ;
#117018 = CARTESIAN_POINT('Ctrl Pts',(-17.2376137110836,13.190619216966,131.245741417272)) ;
#117019 = CARTESIAN_POINT('Ctrl Pts',(-17.2788766995086,12.9388679934988,
131.333323569649)) ;
#117020 = CARTESIAN_POINT('Ctrl Pts',(-17.3412285355925,12.7195132188822,
131.482193704822)) ;
#117021 = CARTESIAN_POINT('Ctrl Pts',(-17.4203247959701,12.5518557366653,
131.680119292236)) ;
#117022 = CARTESIAN_POINT('Ctrl Pts',(-17.5108708872975,12.4467157565619,
131.911647299917)) ;
#117023 = CARTESIAN_POINT('Ctrl Pts',(-17.6083887104431,12.4110145774925,
132.163260737684)) ;
#117024 = CARTESIAN_POINT('Ctrl Pts',(-17.7050772468256,12.4479828352211,
132.412713479872)) ;
#117025 = CARTESIAN_POINT('Ctrl Pts',(-17.7958600990291,12.5544308126574,
132.644801506752)) ;
#117026 = CARTESIAN_POINT('Ctrl Pts',(-17.8750216891489,12.7245572127077,
132.842729488612)) ;
#117027 = CARTESIAN_POINT('Ctrl Pts',(-17.9365564723328,12.9435039801677,
132.989422242518)) ;
#117028 = CARTESIAN_POINT('Ctrl Pts',(-17.9775224282541,13.1965754196772,
133.076026647285)) ;
#117029 = CARTESIAN_POINT('Ctrl Pts',(-17.9956939192113,13.4658054148295,
133.09604875014)) ;
#117030 = CARTESIAN_POINT('Ctrl Pts',(-17.9904317119844,13.7328709435355,
133.047502469415)) ;
#117031 = CARTESIAN_POINT('Ctrl Pts',(-17.9627916507943,13.9772572574738,
132.933643191885)) ;
#117032 = CARTESIAN_POINT('Ctrl Pts',(-17.9155381808679,14.1820528886268,
132.762483278514)) ;
#117033 = CARTESIAN_POINT('Ctrl Pts',(-17.8525173753685,14.3328843450188,
132.545157295433)) ;
#117034 = CARTESIAN_POINT('Ctrl Pts',(-17.7793317704753,14.4178010956835,
132.298223906982)) ;
#117035 = CARTESIAN_POINT('Ctrl Pts',(-17.7022445272674,14.4318123970992,
132.040068999793)) ;
#117036 = CARTESIAN_POINT('Ctrl Pts',(-17.6263126401448,14.3732303174577,
131.78494696794)) ;
#117037 = CARTESIAN_POINT('Ctrl Pts',(-17.5591052998671,14.246970367672,131.555590267811)) ;
#117038 = CARTESIAN_POINT('Ctrl Pts',(-17.5053666762276,14.0621465768449,
131.365553019795)) ;
#117039 = CARTESIAN_POINT('Ctrl Pts',(-17.4696698326379,13.8305008090445,
131.228071032379)) ;
#117040 = CARTESIAN_POINT('Ctrl Pts',(-17.4555867985558,13.5704782336575,
131.153845884403)) ;
#117041 = CARTESIAN_POINT('Ctrl Pts',(-17.4646965033118,13.2994607453498,
131.147313037759)) ;
#117042 = CARTESIAN_POINT('Ctrl Pts',(-17.4970988814655,13.0377344275702,
131.208876933298)) ;
#117043 = CARTESIAN_POINT('Ctrl Pts',(-17.5510813018689,12.8036246677019,
131.333503702802)) ;
#117044 = CARTESIAN_POINT('Ctrl Pts',(-17.6239936560219,12.6130123925856,
131.513267510233)) ;
#117045 = CARTESIAN_POINT('Ctrl Pts',(-17.7106094314361,12.4813447985494,
131.733232511001)) ;
#117046 = CARTESIAN_POINT('Ctrl Pts',(-17.8060337046778,12.4167223946536,
131.978839859878)) ;
#117047 = CARTESIAN_POINT('Ctrl Pts',(-17.9038805613539,12.4243655838416,
132.231551517827)) ;
#117048 = CARTESIAN_POINT('Ctrl Pts',(-17.9978748431434,12.5034382504578,
132.473028954758)) ;
#117049 = CARTESIAN_POINT('Ctrl Pts',(-18.0821443467043,12.6484425830615,
132.686072200411)) ;
#117050 = CARTESIAN_POINT('Ctrl Pts',(-18.1513187618018,12.8490571219356,
132.855007023695)) ;
#117051 = CARTESIAN_POINT('Ctrl Pts',(-18.2011086603779,13.0907448949446,
132.967327226966)) ;
#117052 = CARTESIAN_POINT('Ctrl Pts',(-18.2287179809135,13.3559777711551,
133.014884267935)) ;
#117053 = CARTESIAN_POINT('Ctrl Pts',(-18.2329064963071,13.6264772467065,
132.993964165235)) ;
#117054 = CARTESIAN_POINT('Ctrl Pts',(-18.2141466812409,13.8815733250424,
132.90611529719)) ;
#117055 = CARTESIAN_POINT('Ctrl Pts',(-18.1744739172804,14.1045282295606,
132.757096482705)) ;
#117056 = CARTESIAN_POINT('Ctrl Pts',(-18.1172408746865,14.2789670310199,
132.556695647005)) ;
#117057 = CARTESIAN_POINT('Ctrl Pts',(-18.0476676879061,14.3914951662386,
132.320360288733)) ;
#117058 = CARTESIAN_POINT('Ctrl Pts',(-17.9712198186188,14.4348607606962,
132.063910845682)) ;
#117059 = CARTESIAN_POINT('Ctrl Pts',(-17.8941478594852,14.4056890546892,
131.805637282681)) ;
#117060 = CARTESIAN_POINT('Ctrl Pts',(-17.8227454815296,14.3062653173801,
131.563950734578)) ;
#117061 = CARTESIAN_POINT('Ctrl Pts',(-17.7627779364618,14.1434405254574,
131.355638920096)) ;
#117062 = CARTESIAN_POINT('Ctrl Pts',(-17.7193273445083,13.9296996080406,
131.195662221209)) ;
#117063 = CARTESIAN_POINT('Ctrl Pts',(-17.6960653225894,13.6772902050266,
131.094350026833)) ;
#117064 = CARTESIAN_POINT('Ctrl Pts',(-17.6957248215412,13.4099497148623,
131.060430155186)) ;
#117065 = CARTESIAN_POINT('Ctrl Pts',(-17.7187008254136,13.1418739584321,
131.094409308727)) ;
#117066 = CARTESIAN_POINT('Ctrl Pts',(-17.7643612609263,12.8939990940818,
131.194650629234)) ;
#117067 = CARTESIAN_POINT('Ctrl Pts',(-17.8297406925657,12.6844791174551,
131.352604596309)) ;
#117068 = CARTESIAN_POINT('Ctrl Pts',(-17.912048493683,12.5265062887792,131.559667994062)) ;
#117069 = CARTESIAN_POINT('Ctrl Pts',(-18.0040939259134,12.4345049990361,
131.795636342437)) ;
#117070 = CARTESIAN_POINT('Ctrl Pts',(-18.1020496484601,12.4124896095147,
132.048536521904)) ;
#117071 = CARTESIAN_POINT('Ctrl Pts',(-18.1979840618264,12.4629154785975,
132.295801289656)) ;
#117072 = CARTESIAN_POINT('Ctrl Pts',(-18.2870505883933,12.5820912201831,
132.5228214314)) ;
#117073 = CARTESIAN_POINT('Ctrl Pts',(-18.3631176317433,12.7624371254393,
132.71179031039)) ;
#117074 = CARTESIAN_POINT('Ctrl Pts',(-18.4208520067614,12.9881391647597,
132.847502465823)) ;
#117075 = CARTESIAN_POINT('Ctrl Pts',(-18.4578512180896,13.2462582186001,
132.922435272868)) ;
#117076 = CARTESIAN_POINT('Ctrl Pts',(-18.4715963342929,13.5176870879671,
132.929369118207)) ;
#117077 = CARTESIAN_POINT('Ctrl Pts',(-18.4620156422079,13.7805943652363,
132.86838448577)) ;
#117078 = CARTESIAN_POINT('Ctrl Pts',(-18.4303896901905,14.0195268693382,
132.742785403874)) ;
#117079 = CARTESIAN_POINT('Ctrl Pts',(-18.3798066675688,14.2150384579935,
132.561895383621)) ;
#117080 = CARTESIAN_POINT('Ctrl Pts',(-18.3145812893689,14.3538332405852,
132.338211899335)) ;
#117081 = CARTESIAN_POINT('Ctrl Pts',(-18.2403139322017,14.4259646788893,
132.088197467506)) ;
#117082 = CARTESIAN_POINT('Ctrl Pts',(-18.1623800872695,14.4260802935488,
131.827250512301)) ;
#117083 = CARTESIAN_POINT('Ctrl Pts',(-18.0883879084288,14.3549351031628,
131.578187846455)) ;
#117084 = CARTESIAN_POINT('Ctrl Pts',(-18.0228131840017,14.2162529727103,
131.353366204512)) ;
#117085 = CARTESIAN_POINT('Ctrl Pts',(-17.9722305417751,14.0213157651239,
131.1725299858)) ;
#117086 = CARTESIAN_POINT('Ctrl Pts',(-17.9404225452434,13.7835943457729,
131.046506253201)) ;
#117087 = CARTESIAN_POINT('Ctrl Pts',(-17.9306274462144,13.5186609566866,
130.984624399545)) ;
#117088 = CARTESIAN_POINT('Ctrl Pts',(-17.9441208496999,13.2494163240999,
130.991097001359)) ;
#117089 = CARTESIAN_POINT('Ctrl Pts',(-17.9809055295072,12.9903692068144,
131.065315650557)) ;
#117090 = CARTESIAN_POINT('Ctrl Pts',(-18.0386552877696,12.7636901200826,
131.200984817336)) ;
#117091 = CARTESIAN_POINT('Ctrl Pts',(-18.1148239173405,12.5829314316244,
131.390184918453)) ;
#117092 = CARTESIAN_POINT('Ctrl Pts',(-18.2029461040862,12.4640788592141,
131.614759525871)) ;
#117093 = CARTESIAN_POINT('Ctrl Pts',(-18.2996827120523,12.4125693600516,
131.864067074982)) ;
#117094 = CARTESIAN_POINT('Ctrl Pts',(-18.3969100719483,12.433709410136,132.115106582706)) ;
#117095 = CARTESIAN_POINT('Ctrl Pts',(-18.4900732804124,12.5263145122891,
132.353948507972)) ;
#117096 = CARTESIAN_POINT('Ctrl Pts',(-18.5714958868613,12.682258725893,132.558814736945)) ;
#117097 = CARTESIAN_POINT('Ctrl Pts',(-18.6373162617473,12.8915625393506,
132.717968364611)) ;
#117098 = CARTESIAN_POINT('Ctrl Pts',(-18.6831779936634,13.1392602988437,
132.818793451197)) ;
#117099 = CARTESIAN_POINT('Ctrl Pts',(-18.7064268279725,13.4076118605944,
132.85351971411)) ;
#117100 = CARTESIAN_POINT('Ctrl Pts',(-18.7062530712832,13.6757335665798,
132.820002437843)) ;
#117101 = CARTESIAN_POINT('Ctrl Pts',(-18.683078950832,13.9281677275871,132.718953226837)) ;
#117102 = CARTESIAN_POINT('Ctrl Pts',(-18.640099263916,14.1410411517753,132.560560995141)) ;
#117103 = CARTESIAN_POINT('Ctrl Pts',(-18.5800582899644,14.305185990512,132.35189900218)) ;
#117104 = CARTESIAN_POINT('Ctrl Pts',(-18.5088109665702,14.4050577723151,
132.110709800884)) ;
#117105 = CARTESIAN_POINT('Ctrl Pts',(-18.4315948961661,14.4349188595374,
131.851939151734)) ;
#117106 = CARTESIAN_POINT('Ctrl Pts',(-18.355263243623,14.3922309403959,131.59589764855)) ;
#117107 = CARTESIAN_POINT('Ctrl Pts',(-18.2855600543647,14.2801808361509,
131.359153670221)) ;
#117108 = CARTESIAN_POINT('Ctrl Pts',(-18.2283588377964,14.1070360328529,
131.158971852626)) ;
#117109 = CARTESIAN_POINT('Ctrl Pts',(-18.1882743461536,13.8833119932821,
131.0085695641)) ;
#117110 = CARTESIAN_POINT('Ctrl Pts',(-18.1694035223355,13.6288342780485,
130.920460577913)) ;
#117111 = CARTESIAN_POINT('Ctrl Pts',(-18.1733769016791,13.3582466690145,
130.898891973089)) ;
#117112 = CARTESIAN_POINT('Ctrl Pts',(-18.2007660526155,13.0930922580285,
130.945833159448)) ;
#117113 = CARTESIAN_POINT('Ctrl Pts',(-18.2504018512957,12.8509541830077,
131.057680258634)) ;
#117114 = CARTESIAN_POINT('Ctrl Pts',(-18.3193746459451,12.6500625833759,
131.226050457482)) ;
#117115 = CARTESIAN_POINT('Ctrl Pts',(-18.4036036450366,12.504322047528,131.438944253351)) ;
#117116 = CARTESIAN_POINT('Ctrl Pts',(-18.4977132388811,12.4246931678785,
131.680702606203)) ;
#117117 = CARTESIAN_POINT('Ctrl Pts',(-18.5951599185754,12.416496187653,131.932378104325)) ;
#117118 = CARTESIAN_POINT('Ctrl Pts',(-18.6906647519872,12.4802513742885,
132.178216477564)) ;
#117119 = CARTESIAN_POINT('Ctrl Pts',(-18.7775446534296,12.6116452281821,
132.398888779547)) ;
#117120 = CARTESIAN_POINT('Ctrl Pts',(-18.8503971402191,12.8011771463769,
132.578577969436)) ;
#117121 = CARTESIAN_POINT('Ctrl Pts',(-18.9046822847444,13.0350449035092,
132.704058615265)) ;
#117122 = CARTESIAN_POINT('Ctrl Pts',(-18.9373366903773,13.2969779492496,
132.766311743464)) ;
#117123 = CARTESIAN_POINT('Ctrl Pts',(-18.9466739392997,13.5677345965553,
132.760477775421)) ;
#117124 = CARTESIAN_POINT('Ctrl Pts',(-18.9327727327974,13.8283851031189,
132.686725578769)) ;
#117125 = CARTESIAN_POINT('Ctrl Pts',(-18.8973384738624,14.0598713577401,
132.550083801221)) ;
#117126 = CARTESIAN_POINT('Ctrl Pts',(-18.8437140744461,14.2455587170749,
132.360336246797)) ;
#117127 = CARTESIAN_POINT('Ctrl Pts',(-18.776413111715,14.3725641249717,132.130623413319)) ;
#117128 = CARTESIAN_POINT('Ctrl Pts',(-18.7007176017471,14.4315964655583,
131.876278049731)) ;
#117129 = CARTESIAN_POINT('Ctrl Pts',(-18.6233791710985,14.4181824327013,
131.617286371407)) ;
#117130 = CARTESIAN_POINT('Ctrl Pts',(-18.5502173289885,14.3336378405054,
131.370446907116)) ;
#117131 = CARTESIAN_POINT('Ctrl Pts',(-18.4872936427762,14.1840091545094,
131.15352964314)) ;
#117132 = CARTESIAN_POINT('Ctrl Pts',(-18.4397223531237,13.9789558731559,
130.981326851861)) ;
#117133 = CARTESIAN_POINT('Ctrl Pts',(-18.4119775228567,13.7355808052625,
130.867265425768)) ;
#117134 = CARTESIAN_POINT('Ctrl Pts',(-18.4064814941183,13.4678622499821,
130.817935896373)) ;
#117135 = CARTESIAN_POINT('Ctrl Pts',(-18.4244263066341,13.1991328428123,
130.83736685991)) ;
#117136 = CARTESIAN_POINT('Ctrl Pts',(-18.4652738657257,12.9452257319575,
130.923547616471)) ;
#117137 = CARTESIAN_POINT('Ctrl Pts',(-18.5267424147599,12.7259341486132,
131.070029383219)) ;
#117138 = CARTESIAN_POINT('Ctrl Pts',(-18.605481008747,12.5559411201038,131.266843153907)) ;
#117139 = CARTESIAN_POINT('Ctrl Pts',(-18.6962817397117,12.4485460987932,
131.498939242376)) ;
#117140 = CARTESIAN_POINT('Ctrl Pts',(-18.7931264919224,12.4111599413339,
131.748784863318)) ;
#117141 = CARTESIAN_POINT('Ctrl Pts',(-18.8900242356404,12.4456278255399,
131.998818087739)) ;
#117142 = CARTESIAN_POINT('Ctrl Pts',(-18.9817297898447,12.5514145660075,
132.233337505005)) ;
#117143 = CARTESIAN_POINT('Ctrl Pts',(-19.0604119039029,12.7181519497096,
132.430234211347)) ;
#117144 = CARTESIAN_POINT('Ctrl Pts',(-19.1228377309179,12.9364297066312,
132.579399304795)) ;
#117145 = CARTESIAN_POINT('Ctrl Pts',(-19.1644090080696,13.1887531775189,
132.667781651634)) ;
#117146 = CARTESIAN_POINT('Ctrl Pts',(-19.1833003674831,13.4580633206524,
132.689869485556)) ;
#117147 = CARTESIAN_POINT('Ctrl Pts',(-19.1786680296816,13.7256377650323,
132.643143208247)) ;
#117148 = CARTESIAN_POINT('Ctrl Pts',(-19.1517004243795,13.9704139197111,
132.531316059401)) ;
#117149 = CARTESIAN_POINT('Ctrl Pts',(-19.104963335141,14.1767864101741,132.361645187947)) ;
#117150 = CARTESIAN_POINT('Ctrl Pts',(-19.042308153427,14.3292888333563,132.145383688225)) ;
#117151 = CARTESIAN_POINT('Ctrl Pts',(-18.9695876630287,14.4162418922063,
131.899913807586)) ;
#117152 = CARTESIAN_POINT('Ctrl Pts',(-18.892047727718,14.4323070636622,131.640219675188)) ;
#117153 = CARTESIAN_POINT('Ctrl Pts',(-18.816661183209,14.3764282690484,131.387003920178)) ;
#117154 = CARTESIAN_POINT('Ctrl Pts',(-18.7486327689988,14.2515625943371,
131.155022379996)) ;
#117155 = CARTESIAN_POINT('Ctrl Pts',(-18.6944668016159,14.0682229013696,
130.963752671128)) ;
#117156 = CARTESIAN_POINT('Ctrl Pts',(-18.6581314611437,13.8370234728167,
130.824314562023)) ;
#117157 = CARTESIAN_POINT('Ctrl Pts',(-18.6434859969042,13.5786250860868,
130.748584888107)) ;
#117158 = CARTESIAN_POINT('Ctrl Pts',(-18.6518580481978,13.3076278419877,
130.739890903035)) ;
#117159 = CARTESIAN_POINT('Ctrl Pts',(-18.6835647729175,13.0452574114126,
130.799415914394)) ;
#117160 = CARTESIAN_POINT('Ctrl Pts',(-18.7372078222609,12.809151348438,130.922911372363)) ;
#117161 = CARTESIAN_POINT('Ctrl Pts',(-18.8096004840355,12.6175516783773,
131.101207495489)) ;
#117162 = CARTESIAN_POINT('Ctrl Pts',(-18.8956363694374,12.4843718423873,
131.319568496696)) ;
#117163 = CARTESIAN_POINT('Ctrl Pts',(-18.9909803439723,12.417595884224,131.564908742149)) ;
#117164 = CARTESIAN_POINT('Ctrl Pts',(-19.0887365409089,12.4230554793737,
131.817394766854)) ;
#117165 = CARTESIAN_POINT('Ctrl Pts',(-19.1830717025105,12.5002516157562,
132.059812929187)) ;
#117166 = CARTESIAN_POINT('Ctrl Pts',(-19.2674882263268,12.6429370956148,
132.273384344499)) ;
#117167 = CARTESIAN_POINT('Ctrl Pts',(-19.3374842285937,12.8430358914049,
132.444563896966)) ;
#117168 = CARTESIAN_POINT('Ctrl Pts',(-19.3876849067688,13.0829430235275,
132.558206408806)) ;
#117169 = CARTESIAN_POINT('Ctrl Pts',(-19.4160311708763,13.3482625175679,
132.607844720929)) ;
#117170 = CARTESIAN_POINT('Ctrl Pts',(-19.4209271929234,13.6179804749313,
132.589108934737)) ;
#117171 = CARTESIAN_POINT('Ctrl Pts',(-19.4027272157972,13.8754577443227,
132.502681343733)) ;
#117172 = CARTESIAN_POINT('Ctrl Pts',(-19.3634406682626,14.0994367889634,
132.354768976412)) ;
#117173 = CARTESIAN_POINT('Ctrl Pts',(-19.3070300640894,14.2743408092093,
132.156989617184)) ;
#117174 = CARTESIAN_POINT('Ctrl Pts',(-19.2375686089438,14.3892596649761,
131.920883182707)) ;
#117175 = CARTESIAN_POINT('Ctrl Pts',(-19.1612777685189,14.4346258039945,
131.664916915455)) ;
#117176 = CARTESIAN_POINT('Ctrl Pts',(-19.083930799282,14.4074612367265,131.405752807975)) ;
#117177 = CARTESIAN_POINT('Ctrl Pts',(-19.0123391520556,14.3096987873791,
131.163518218424)) ;
#117178 = CARTESIAN_POINT('Ctrl Pts',(-18.952179149292,14.1493774053066,130.954787077338)) ;
#117179 = CARTESIAN_POINT('Ctrl Pts',(-18.9079902596912,13.9355628673905,
130.792452884477)) ;
#117180 = CARTESIAN_POINT('Ctrl Pts',(-18.8842705546582,13.6861606086544,
130.6900983053)) ;
#117181 = CARTESIAN_POINT('Ctrl Pts',(-18.8831952536651,13.4167352141788,
130.653733612536)) ;
#117182 = CARTESIAN_POINT('Ctrl Pts',(-18.9055495545771,13.1492793403457,
130.686009635183)) ;
#117183 = CARTESIAN_POINT('Ctrl Pts',(-18.950554370829,12.9005268822979,130.784333466505)) ;
#117184 = CARTESIAN_POINT('Ctrl Pts',(-19.0154787069261,12.6897474327515,
130.940945875063)) ;
#117185 = CARTESIAN_POINT('Ctrl Pts',(-19.0969861591499,12.5306016381553,
131.145821087892)) ;
#117186 = CARTESIAN_POINT('Ctrl Pts',(-19.189260918282,12.4360458908817,131.382286850804)) ;
#117187 = CARTESIAN_POINT('Ctrl Pts',(-19.2870091730974,12.412131814103,131.634635629436)) ;
#117188 = CARTESIAN_POINT('Ctrl Pts',(-19.3832683990726,12.4605357915181,
131.882783283401)) ;
#117189 = CARTESIAN_POINT('Ctrl Pts',(-19.4726990706001,12.5784164167772,
132.110813581549)) ;
#117190 = CARTESIAN_POINT('Ctrl Pts',(-19.548603124899,12.75548162504,132.299596599868)) ;
#117191 = CARTESIAN_POINT('Ctrl Pts',(-19.6074115970358,12.9817623745855,
132.43817522236)) ;
#117192 = CARTESIAN_POINT('Ctrl Pts',(-19.6448326502932,13.2381597682889,
132.514493933174)) ;
#117193 = CARTESIAN_POINT('Ctrl Pts',(-19.6593315598521,13.5101991451629,
132.523535679866)) ;
#117194 = CARTESIAN_POINT('Ctrl Pts',(-19.6504054949689,13.7733130624052,
132.46450138847)) ;
#117195 = CARTESIAN_POINT('Ctrl Pts',(-19.6192034341109,14.0140640637462,
132.340009177099)) ;
#117196 = CARTESIAN_POINT('Ctrl Pts',(-19.5693158816681,14.2098744225724,
132.161320346302)) ;
#117197 = CARTESIAN_POINT('Ctrl Pts',(-19.504529632498,14.3505801926375,131.938940974337)) ;
#117198 = CARTESIAN_POINT('Ctrl Pts',(-19.4303629478852,14.4248316495575,
131.689182334829)) ;
#117199 = CARTESIAN_POINT('Ctrl Pts',(-19.3525182361724,14.4272048200234,
131.428536488696)) ;
#117200 = CARTESIAN_POINT('Ctrl Pts',(-19.2781506637438,14.3577939953671,
131.178279346935)) ;
#117201 = CARTESIAN_POINT('Ctrl Pts',(-19.212505421794,14.2217458175161,130.953414089471)) ;
#117202 = CARTESIAN_POINT('Ctrl Pts',(-19.16103693859,14.0267542055663,130.769727449748)) ;
#117203 = CARTESIAN_POINT('Ctrl Pts',(-19.1289036146384,13.7911380978429,
130.642932687612)) ;
#117204 = CARTESIAN_POINT('Ctrl Pts',(-19.1183510866146,13.5273991680406,
130.578912350849)) ;
#117205 = CARTESIAN_POINT('Ctrl Pts',(-19.1311706870696,13.2571617641776,
130.583305514474)) ;
#117206 = CARTESIAN_POINT('Ctrl Pts',(-19.1673218801738,12.9974109548792,
130.655666860345)) ;
#117207 = CARTESIAN_POINT('Ctrl Pts',(-19.2245830115337,12.7695380249157,
130.789882378042)) ;
#117208 = CARTESIAN_POINT('Ctrl Pts',(-19.2998473676005,12.5879937236174,
130.976618888734)) ;
#117209 = CARTESIAN_POINT('Ctrl Pts',(-19.3881991229152,12.4663339906868,
131.201653000597)) ;
#117210 = CARTESIAN_POINT('Ctrl Pts',(-19.4848060932389,12.41305303315,131.450591800084)) ;
#117211 = CARTESIAN_POINT('Ctrl Pts',(-19.5819062292555,12.4321501041493,
131.701314973679)) ;
#117212 = CARTESIAN_POINT('Ctrl Pts',(-19.675129897644,12.522410787778,131.940402492585)) ;
#117213 = CARTESIAN_POINT('Ctrl Pts',(-19.7573199379753,12.677312203341,132.14736167088)) ;
#117214 = CARTESIAN_POINT('Ctrl Pts',(-19.823545048816,12.8853931735732,132.307714185514)) ;
#117215 = CARTESIAN_POINT('Ctrl Pts',(-19.8698643346986,13.1311434381669,
132.410014121135)) ;
#117216 = CARTESIAN_POINT('Ctrl Pts',(-19.8939118774607,13.4000886870271,
132.446960025135)) ;
#117217 = CARTESIAN_POINT('Ctrl Pts',(-19.8943127889844,13.667985481151,132.415168505079)) ;
#117218 = CARTESIAN_POINT('Ctrl Pts',(-19.8720904633959,13.9198929118074,
132.317110124028)) ;
#117219 = CARTESIAN_POINT('Ctrl Pts',(-19.8290668706825,14.13673316727,132.158155563746)) ;
#117220 = CARTESIAN_POINT('Ctrl Pts',(-19.770011609999,14.300676131018,131.952727239332)) ;
#117221 = CARTESIAN_POINT('Ctrl Pts',(-19.6985762425733,14.4034182516523,
131.71075647086)) ;
#117222 = CARTESIAN_POINT('Ctrl Pts',(-19.6216236920745,14.4350219439221,
131.452850053903)) ;
#117223 = CARTESIAN_POINT('Ctrl Pts',(-19.5450987456045,14.3943912099649,
131.196198948101)) ;
#117224 = CARTESIAN_POINT('Ctrl Pts',(-19.475140036997,14.2842181242634,130.958722088422)) ;
#117225 = CARTESIAN_POINT('Ctrl Pts',(-19.4175029628842,14.11233380319,130.757229002199)) ;
#117226 = CARTESIAN_POINT('Ctrl Pts',(-19.3770857737604,13.8914433444145,
130.6060852262)) ;
#117227 = CARTESIAN_POINT('Ctrl Pts',(-19.3573954947611,13.6364806192018,
130.515411717742)) ;
#117228 = CARTESIAN_POINT('Ctrl Pts',(-19.3607065836319,13.3663281974235,
130.491948631403)) ;
#117229 = CARTESIAN_POINT('Ctrl Pts',(-19.3874616050322,13.1002905199636,
130.536976005828)) ;
#117230 = CARTESIAN_POINT('Ctrl Pts',(-19.4365018798327,12.8573187097229,
130.647094499789)) ;
#117231 = CARTESIAN_POINT('Ctrl Pts',(-19.5049808180712,12.6550559201632,
130.814019899914)) ;
#117232 = CARTESIAN_POINT('Ctrl Pts',(-19.5887535982055,12.5076995201524,
131.025617281051)) ;
#117233 = CARTESIAN_POINT('Ctrl Pts',(-19.6826402090088,12.4260782231414,
131.266727526869)) ;
#117234 = CARTESIAN_POINT('Ctrl Pts',(-19.780025633086,12.4155414284777,131.518242098443)) ;
#117235 = CARTESIAN_POINT('Ctrl Pts',(-19.8763791576049,12.4780902528913,
131.766305681798)) ;
#117236 = CARTESIAN_POINT('Ctrl Pts',(-19.9627548974109,12.6066343285888,
131.985813699722)) ;
#117237 = CARTESIAN_POINT('Ctrl Pts',(-20.0364241953336,12.7952135376049,
132.167753376354)) ;
#117238 = CARTESIAN_POINT('Ctrl Pts',(-20.0912151052384,13.0279818005268,
132.294735120035)) ;
#117239 = CARTESIAN_POINT('Ctrl Pts',(-20.1245512603828,13.2896873731217,
132.358938550464)) ;
#117240 = CARTESIAN_POINT('Ctrl Pts',(-20.1345039282667,13.5603127148141,
132.354920444132)) ;
#117241 = CARTESIAN_POINT('Ctrl Pts',(-20.1212776955433,13.8211026709328,
132.283193531999)) ;
#117242 = CARTESIAN_POINT('Ctrl Pts',(-20.0864145211484,14.0538031496825,
132.148202189386)) ;
#117243 = CARTESIAN_POINT('Ctrl Pts',(-20.0332397566341,14.2410907162982,
131.959757160238)) ;
#117244 = CARTESIAN_POINT('Ctrl Pts',(-19.9660383596576,14.3701940931664,
131.730238162019)) ;
#117245 = CARTESIAN_POINT('Ctrl Pts',(-19.8905439086927,14.4308809460844,
131.476512158403)) ;
#117246 = CARTESIAN_POINT('Ctrl Pts',(-19.8134151755877,14.4196139003572,
131.218236026987)) ;
#117247 = CARTESIAN_POINT('Ctrl Pts',(-19.7398726196564,14.336836882695,130.97020458083)) ;
#117248 = CARTESIAN_POINT('Ctrl Pts',(-19.6767629170673,14.1892311561633,
130.752829213023)) ;
#117249 = CARTESIAN_POINT('Ctrl Pts',(-19.6286665108586,13.9859053785223,
130.57912299113)) ;
#117250 = CARTESIAN_POINT('Ctrl Pts',(-19.6002355231938,13.7426112517957,
130.462946926761)) ;
#117251 = CARTESIAN_POINT('Ctrl Pts',(-19.594107429176,13.4761438814329,130.411880995108)) ;
#117252 = CARTESIAN_POINT('Ctrl Pts',(-19.6113174094104,13.2070931774866,
130.429149009167)) ;
#117253 = CARTESIAN_POINT('Ctrl Pts',(-19.6515803257306,12.9521503928351,
130.513580392613)) ;
#117254 = CARTESIAN_POINT('Ctrl Pts',(-19.712491346524,12.7315094289201,130.658427474088)) ;
#117255 = CARTESIAN_POINT('Ctrl Pts',(-19.7911656685738,12.55952255891,130.85492439979)) ;
#117256 = CARTESIAN_POINT('Ctrl Pts',(-19.8809709738294,12.4509681348577,
131.084378584018)) ;
#117257 = CARTESIAN_POINT('Ctrl Pts',(-19.9785025004899,12.4111337654698,
131.335955835968)) ;
#117258 = CARTESIAN_POINT('Ctrl Pts',(-20.0750208858797,12.4436883987287,
131.58504110594)) ;
#117259 = CARTESIAN_POINT('Ctrl Pts',(-20.1670489406682,12.5474867410868,
131.820478093993)) ;
#117260 = CARTESIAN_POINT('Ctrl Pts',(-20.2460595301685,12.7123018104689,
132.018383639864)) ;
#117261 = CARTESIAN_POINT('Ctrl Pts',(-20.3091917091409,12.930070804837,132.169503787281)) ;
#117262 = CARTESIAN_POINT('Ctrl Pts',(-20.3512037961698,13.1802337484168,
132.259358056901)) ;
#117263 = CARTESIAN_POINT('Ctrl Pts',(-20.3709163624956,13.4510759105696,
132.283623543489)) ;
#117264 = CARTESIAN_POINT('Ctrl Pts',(-20.3669009496228,13.7180592820174,
132.238817284807)) ;
#117265 = CARTESIAN_POINT('Ctrl Pts',(-20.3404947485754,13.9642785857624,
132.128552198951)) ;
#117266 = CARTESIAN_POINT('Ctrl Pts',(-20.2943585159327,14.1712561448263,
131.960731543111)) ;
#117267 = CARTESIAN_POINT('Ctrl Pts',(-20.2323687223324,14.3253724982605,
131.74652385602)) ;
#117268 = CARTESIAN_POINT('Ctrl Pts',(-20.1592998865513,14.4148742496936,
131.499776720627)) ;
#117269 = CARTESIAN_POINT('Ctrl Pts',(-20.0823960426978,14.4329087927554,
131.24220329871)) ;
#117270 = CARTESIAN_POINT('Ctrl Pts',(-20.0063538704039,14.3788838662948,
130.986842165717)) ;
#117271 = CARTESIAN_POINT('Ctrl Pts',(-19.9382630997815,14.2561020385484,
130.75479330686)) ;
#117272 = CARTESIAN_POINT('Ctrl Pts',(-19.8835990530441,14.0742378905462,
130.562042928093)) ;
#117273 = CARTESIAN_POINT('Ctrl Pts',(-19.8467989799249,13.8451951074059,
130.421387675447)) ;
#117274 = CARTESIAN_POINT('Ctrl Pts',(-19.8313341159971,13.5867436924812,
130.343166472382)) ;
#117275 = CARTESIAN_POINT('Ctrl Pts',(-19.8391431535007,13.3144406104729,
130.332664419117)) ;
#117276 = CARTESIAN_POINT('Ctrl Pts',(-19.8701070003036,13.0528697153062,
130.390177046887)) ;
#117277 = CARTESIAN_POINT('Ctrl Pts',(-19.922977018825,12.8160519673843,130.511475471805)) ;
#117278 = CARTESIAN_POINT('Ctrl Pts',(-19.9949224006439,12.6226066577663,
130.688427360909)) ;
#117279 = CARTESIAN_POINT('Ctrl Pts',(-20.0807929883206,12.4871997727771,
130.906234994754)) ;
#117280 = CARTESIAN_POINT('Ctrl Pts',(-20.1763248041148,12.4184347906441,
131.152006317102)) ;
#117281 = CARTESIAN_POINT('Ctrl Pts',(-20.2735243410858,12.421900095689,131.403058055158)) ;
#117282 = CARTESIAN_POINT('Ctrl Pts',(-20.3681714156429,12.4968773890891,
131.646353538918)) ;
#117283 = CARTESIAN_POINT('Ctrl Pts',(-20.453078884326,12.6381725134135,131.861295773607)) ;
#117284 = CARTESIAN_POINT('Ctrl Pts',(-20.5233761153413,12.8360676034159,
132.033469623726)) ;
#117285 = CARTESIAN_POINT('Ctrl Pts',(-20.5744273993862,13.0762564614049,
132.149423205006)) ;
#117286 = CARTESIAN_POINT('Ctrl Pts',(-20.6032682080112,13.3398739353009,
132.200670249098)) ;
#117287 = CARTESIAN_POINT('Ctrl Pts',(-20.6089153558675,13.6103042607725,
132.184053731351)) ;
#117288 = CARTESIAN_POINT('Ctrl Pts',(-20.5913552359384,13.8681248638129,
132.0995339823)) ;
#117289 = CARTESIAN_POINT('Ctrl Pts',(-20.5527417289415,14.0932870641316,
131.953614612924)) ;
#117290 = CARTESIAN_POINT('Ctrl Pts',(-20.4963514522557,14.2707836154913,
131.755672439689)) ;
#117291 = CARTESIAN_POINT('Ctrl Pts',(-20.4275781234429,14.3866738270234,
131.521785274535)) ;
#117292 = CARTESIAN_POINT('Ctrl Pts',(-20.3513635050219,14.4343395634598,
131.266014418455)) ;
#117293 = CARTESIAN_POINT('Ctrl Pts',(-20.2741102846849,14.4093417232231,
131.007191524153)) ;
#117294 = CARTESIAN_POINT('Ctrl Pts',(-20.2022164359657,14.3139583409208,
130.764077181119)) ;
#117295 = CARTESIAN_POINT('Ctrl Pts',(-20.1412573441085,14.1538396198972,
130.552752557387)) ;
#117296 = CARTESIAN_POINT('Ctrl Pts',(-20.0969445519394,13.9434082159672,
130.390384097063)) ;
#117297 = CARTESIAN_POINT('Ctrl Pts',(-20.0723542788181,13.6926166151685,
130.285177903961)) ;
#117298 = CARTESIAN_POINT('Ctrl Pts',(-20.0706938890781,13.4252309496683,
130.247334933765)) ;
#117299 = CARTESIAN_POINT('Ctrl Pts',(-20.092332751845,13.1569924841194,130.277454300474)) ;
#117300 = CARTESIAN_POINT('Ctrl Pts',(-20.1366756135325,12.907415746913,130.373858632925)) ;
#117301 = CARTESIAN_POINT('Ctrl Pts',(-20.2013825642992,12.6946405642384,
130.529698727295)) ;
#117302 = CARTESIAN_POINT('Ctrl Pts',(-20.2819050644324,12.5348309351463,
130.731934046482)) ;
#117303 = CARTESIAN_POINT('Ctrl Pts',(-20.3745177661893,12.4376124732534,
130.969168887914)) ;
#117304 = CARTESIAN_POINT('Ctrl Pts',(-20.4716979393396,12.411847051202,131.220037230897)) ;
#117305 = CARTESIAN_POINT('Ctrl Pts',(-20.5682462895583,12.4580456459642,
131.468969166317)) ;
#117306 = CARTESIAN_POINT('Ctrl Pts',(-20.6577938331677,12.5736491008617,
131.697417164121)) ;
#117307 = CARTESIAN_POINT('Ctrl Pts',(-20.7344433492042,12.7495591345061,
131.888265424488)) ;
#117308 = CARTESIAN_POINT('Ctrl Pts',(-20.7939354209719,12.9753683217391,
132.028755611113)) ;
#117309 = CARTESIAN_POINT('Ctrl Pts',(-20.8319052589719,13.2312289198464,
132.106671123273)) ;
#117310 = CARTESIAN_POINT('Ctrl Pts',(-20.8470373803621,13.5022490913223,
132.117677262767)) ;
#117311 = CARTESIAN_POINT('Ctrl Pts',(-20.8387067324782,13.7663766429706,
132.060301499346)) ;
#117312 = CARTESIAN_POINT('Ctrl Pts',(-20.8083941645055,14.0063275981214,
131.938667665989)) ;
#117313 = CARTESIAN_POINT('Ctrl Pts',(-20.7588632031017,14.2048735685629,
131.760851862467)) ;
#117314 = CARTESIAN_POINT('Ctrl Pts',(-20.6941991703353,14.3476911545505,
131.538730144757)) ;
#117315 = CARTESIAN_POINT('Ctrl Pts',(-20.6201333307794,14.4237776141336,
131.289235795019)) ;
#117316 = CARTESIAN_POINT('Ctrl Pts',(-20.5425102852112,14.4280807917519,
131.029325961589)) ;
#117317 = CARTESIAN_POINT('Ctrl Pts',(-20.467928775171,14.360827921304,130.778436656629)) ;
#117318 = CARTESIAN_POINT('Ctrl Pts',(-20.4017581108605,14.2256361349193,
130.551896055991)) ;
#117319 = CARTESIAN_POINT('Ctrl Pts',(-20.3503571718372,14.0344801252662,
130.368795956172)) ;
#117320 = CARTESIAN_POINT('Ctrl Pts',(-20.3172512957461,13.7980437562362,
130.238869010308)) ;
#117321 = CARTESIAN_POINT('Ctrl Pts',(-20.3061244134585,13.53532438393,130.173252180728)) ;
#117322 = CARTESIAN_POINT('Ctrl Pts',(-20.3182993207692,13.2644875678434,
130.175688064952)) ;
#117323 = CARTESIAN_POINT('Ctrl Pts',(-20.3536678560636,13.0050530170807,
130.245886392756)) ;
#117324 = CARTESIAN_POINT('Ctrl Pts',(-20.410462049302,12.775438141039,130.378653667283)) ;
#117325 = CARTESIAN_POINT('Ctrl Pts',(-20.4851886237847,12.5925960963687,
130.563862064022)) ;
#117326 = CARTESIAN_POINT('Ctrl Pts',(-20.5732195435502,12.4690082469491,
130.787956911041)) ;
#117327 = CARTESIAN_POINT('Ctrl Pts',(-20.6696209731858,12.4135709185057,
131.036318926835)) ;
#117328 = CARTESIAN_POINT('Ctrl Pts',(-20.7669518533453,12.4306394810107,
131.287650324526)) ;
#117329 = CARTESIAN_POINT('Ctrl Pts',(-20.8601171292825,12.5185474861746,
131.526674543202)) ;
#117330 = CARTESIAN_POINT('Ctrl Pts',(-20.942837156887,12.6718439913262,131.73512693663)) ;
#117331 = CARTESIAN_POINT('Ctrl Pts',(-21.009555833747,12.8780301439606,131.896984168492)) ;
#117332 = CARTESIAN_POINT('Ctrl Pts',(-21.056821363786,13.1252485962165,132.001742572807)) ;
#117333 = CARTESIAN_POINT('Ctrl Pts',(-21.0812481855893,13.3909665400584,
132.04016382239)) ;
#117334 = CARTESIAN_POINT('Ctrl Pts',(-21.0824288286502,13.6612160877443,
132.010385535498)) ;
#117335 = CARTESIAN_POINT('Ctrl Pts',(-21.0607478945341,13.9131568788034,
131.913987653532)) ;
#117336 = CARTESIAN_POINT('Ctrl Pts',(-21.0185378959284,14.1304384080089,
131.757557383989)) ;
#117337 = CARTESIAN_POINT('Ctrl Pts',(-20.9596569052815,14.2969775137474,
131.552483499945)) ;
#117338 = CARTESIAN_POINT('Ctrl Pts',(-20.8883479707721,14.4015522183562,
131.310837907487)) ;
#117339 = CARTESIAN_POINT('Ctrl Pts',(-20.811743048276,14.4350500547512,131.054060145774)) ;
#117340 = CARTESIAN_POINT('Ctrl Pts',(-20.7352017856346,14.396751965708,130.797400979344)) ;
#117341 = CARTESIAN_POINT('Ctrl Pts',(-20.6648700748169,14.2884849239284,
130.558794614213)) ;
#117342 = CARTESIAN_POINT('Ctrl Pts',(-20.606731654312,14.1181741044495,130.355813335934)) ;
#117343 = CARTESIAN_POINT('Ctrl Pts',(-20.5656967115575,13.8977533675812,
130.202766790401)) ;
#117344 = CARTESIAN_POINT('Ctrl Pts',(-20.5454538498325,13.6446685040666,
130.110631870406)) ;
#117345 = CARTESIAN_POINT('Ctrl Pts',(-20.5480734369409,13.3734340849695,
130.084992346971)) ;
#117346 = CARTESIAN_POINT('Ctrl Pts',(-20.5742578565967,13.1072277425428,
130.128374016336)) ;
#117347 = CARTESIAN_POINT('Ctrl Pts',(-20.6225056372082,12.8641926256241,
130.236294496297)) ;
#117348 = CARTESIAN_POINT('Ctrl Pts',(-20.6904289274689,12.6605228267135,
130.401603234601)) ;
#117349 = CARTESIAN_POINT('Ctrl Pts',(-20.7736447523668,12.5114117943071,
130.611629156176)) ;
#117350 = CARTESIAN_POINT('Ctrl Pts',(-20.8678757743497,12.4272142366947,
130.853549028094)) ;
#117351 = CARTESIAN_POINT('Ctrl Pts',(-20.9651014565131,12.4150347895705,
131.104641444644)) ;
#117352 = CARTESIAN_POINT('Ctrl Pts',(-21.060978957513,12.4747490693336,131.35154192915)) ;
#117353 = CARTESIAN_POINT('Ctrl Pts',(-21.1484527801317,12.6023244974168,
131.573977816226)) ;
#117354 = CARTESIAN_POINT('Ctrl Pts',(-21.2225268496985,12.7898413054048,
131.757084110712)) ;
#117355 = CARTESIAN_POINT('Ctrl Pts',(-21.2776732687232,13.0206705904154,
131.885228927191)) ;
#117356 = CARTESIAN_POINT('Ctrl Pts',(-21.3116929767443,13.2818516686094,
131.951421363387)) ;
#117357 = CARTESIAN_POINT('Ctrl Pts',(-21.3223256302397,13.5521276503918,
131.949431203066)) ;
#117358 = CARTESIAN_POINT('Ctrl Pts',(-21.3097945676816,13.8139567141273,
131.87968328586)) ;
#117359 = CARTESIAN_POINT('Ctrl Pts',(-21.2752727495354,14.048569772894,131.745542468365)) ;
#117360 = CARTESIAN_POINT('Ctrl Pts',(-21.2228787528856,14.236110064849,131.559589873959)) ;
#117361 = CARTESIAN_POINT('Ctrl Pts',(-21.1558243323814,14.3675383495349,
131.330396273337)) ;
#117362 = CARTESIAN_POINT('Ctrl Pts',(-21.0806484199029,14.4300942129039,
131.077681198035)) ;
#117363 = CARTESIAN_POINT('Ctrl Pts',(-21.0033788252062,14.4208865440108,
130.818936586364)) ;
#117364 = CARTESIAN_POINT('Ctrl Pts',(-20.9298451040332,14.3405661595428,
130.571042931108)) ;
#117365 = CARTESIAN_POINT('Ctrl Pts',(-20.8658533560393,14.1934623353678,
130.350815526822)) ;
#117366 = CARTESIAN_POINT('Ctrl Pts',(-20.8175001319599,13.9917022900947,
130.176448833883)) ;
#117367 = CARTESIAN_POINT('Ctrl Pts',(-20.7885759620872,13.7502057571416,
130.058945585873)) ;
#117368 = CARTESIAN_POINT('Ctrl Pts',(-20.7817113274138,13.4844948245858,
130.005770974268)) ;
#117369 = CARTESIAN_POINT('Ctrl Pts',(-20.7983394804369,13.2141841608485,
130.021199429463)) ;
#117370 = CARTESIAN_POINT('Ctrl Pts',(-20.8378966646696,12.9589228600533,
130.103630667804)) ;
#117371 = CARTESIAN_POINT('Ctrl Pts',(-20.8986899919378,12.7362703078518,
130.247957265141)) ;
#117372 = CARTESIAN_POINT('Ctrl Pts',(-20.9757867279196,12.5648475135275,
130.440319362778)) ;
#117373 = CARTESIAN_POINT('Ctrl Pts',(-21.0663368128741,12.452872637983,130.67154841129)) ;
#117374 = CARTESIAN_POINT('Ctrl Pts',(-21.1629005182569,12.411294196787,130.920610155833)) ;
#117375 = CARTESIAN_POINT('Ctrl Pts',(-21.260397731377,12.4419882066381,131.172234258394)) ;
#117376 = CARTESIAN_POINT('Ctrl Pts',(-21.3517237017797,12.5427027858175,
131.405983597941)) ;
#117377 = CARTESIAN_POINT('Ctrl Pts',(-21.4318039101064,12.706796402249,131.606755442303)) ;
#117378 = CARTESIAN_POINT('Ctrl Pts',(-21.4952071393745,12.9221001593752,
131.758848779645)) ;
#117379 = CARTESIAN_POINT('Ctrl Pts',(-21.538280315247,13.1741319900526,131.851446839118)) ;
#117380 = CARTESIAN_POINT('Ctrl Pts',(-21.5584177432059,13.4427023276839,
131.877218319414)) ;
#117381 = CARTESIAN_POINT('Ctrl Pts',(-21.5551172048958,13.7107857008536,
131.834398380484)) ;
#117382 = CARTESIAN_POINT('Ctrl Pts',(-21.5294381391568,13.9568883020333,
131.726395472109)) ;
#117383 = CARTESIAN_POINT('Ctrl Pts',(-21.483735439408,14.1661036589884,131.559726534066)) ;
#117384 = CARTESIAN_POINT('Ctrl Pts',(-21.4219683482731,14.3219384877272,
131.346112125423)) ;
#117385 = CARTESIAN_POINT('Ctrl Pts',(-21.3496214859993,14.4130180667709,
131.10169089437)) ;
#117386 = CARTESIAN_POINT('Ctrl Pts',(-21.2722521429854,14.4335349377785,
130.842535969221)) ;
#117387 = CARTESIAN_POINT('Ctrl Pts',(-21.1960388298333,14.3810414591398,
130.586644305319)) ;
#117388 = CARTESIAN_POINT('Ctrl Pts',(-21.1280003928797,14.2609491563611,
130.354936375839)) ;
#117389 = CARTESIAN_POINT('Ctrl Pts',(-21.0725876584999,14.0795345145358,
130.159800933147)) ;
#117390 = CARTESIAN_POINT('Ctrl Pts',(-21.035403480221,13.8529285433275,130.018220066341)) ;
#117391 = CARTESIAN_POINT('Ctrl Pts',(-21.01921653569,13.5926909018936,129.937579732469)) ;
#117392 = CARTESIAN_POINT('Ctrl Pts',(-21.0263535490702,13.3230679904021,
129.925443216821)) ;
#117393 = CARTESIAN_POINT('Ctrl Pts',(-21.056724206518,13.0595446516906,129.981042089682)) ;
#117394 = CARTESIAN_POINT('Ctrl Pts',(-21.1092312885458,12.821409078981,130.101215513039)) ;
#117395 = CARTESIAN_POINT('Ctrl Pts',(-21.1806069334904,12.6270968771254,
130.276569849838)) ;
#117396 = CARTESIAN_POINT('Ctrl Pts',(-21.2658529230612,12.4904302575877,
130.492664537939)) ;
#117397 = CARTESIAN_POINT('Ctrl Pts',(-21.3608874562241,12.4195264376518,
130.737086059353)) ;
#117398 = CARTESIAN_POINT('Ctrl Pts',(-21.4585744347889,12.4206997747971,
130.989400021545)) ;
#117399 = CARTESIAN_POINT('Ctrl Pts',(-21.5535287966605,12.4940150849619,
131.233544186021)) ;
#117400 = CARTESIAN_POINT('Ctrl Pts',(-21.6385302946146,12.6331733496192,
131.448855787369)) ;
#117401 = CARTESIAN_POINT('Ctrl Pts',(-21.7092724630891,12.8293255236082,
131.622363791874)) ;
#117402 = CARTESIAN_POINT('Ctrl Pts',(-21.7609583754883,13.0683011169746,
131.740190348621)) ;
#117403 = CARTESIAN_POINT('Ctrl Pts',(-21.7905747827233,13.3322965961088,
131.793597517871)) ;
#117404 = CARTESIAN_POINT('Ctrl Pts',(-21.7968440357838,13.6026348428664,
131.77882032904)) ;
#117405 = CARTESIAN_POINT('Ctrl Pts',(-21.7800208228364,13.8605087628932,
131.69653724068)) ;
#117406 = CARTESIAN_POINT('Ctrl Pts',(-21.741943453815,14.0871783650871,131.55213623212)) ;
#117407 = CARTESIAN_POINT('Ctrl Pts',(-21.68623340069,14.2658343770077,131.356293575374)) ;
#117408 = CARTESIAN_POINT('Ctrl Pts',(-21.6174834581691,14.3843789391541,
131.122326149126)) ;
#117409 = CARTESIAN_POINT('Ctrl Pts',(-21.5412324446713,14.4339734241572,
130.866388632503)) ;
#117410 = CARTESIAN_POINT('Ctrl Pts',(-21.4641445421631,14.4110559361857,
130.608142700945)) ;
#117411 = CARTESIAN_POINT('Ctrl Pts',(-21.3920751414043,14.3178925144465,
130.364549551773)) ;
#117412 = CARTESIAN_POINT('Ctrl Pts',(-21.3305900015809,14.1593686690055,
130.151640808334)) ;
#117413 = CARTESIAN_POINT('Ctrl Pts',(-21.28571730329,13.9496805388889,129.987566165016)) ;
#117414 = CARTESIAN_POINT('Ctrl Pts',(-21.2606021210969,13.7013470012748,
129.881036373736)) ;
#117415 = CARTESIAN_POINT('Ctrl Pts',(-21.2581837575686,13.4330164706509,
129.840817045843)) ;
#117416 = CARTESIAN_POINT('Ctrl Pts',(-21.2791303522906,13.1647607659068,
129.868952988127)) ;
#117417 = CARTESIAN_POINT('Ctrl Pts',(-21.3230136561864,12.9137311953691,
129.963914319132)) ;
#117418 = CARTESIAN_POINT('Ctrl Pts',(-21.3867869705194,12.7007529765594,
130.11721967487)) ;
#117419 = CARTESIAN_POINT('Ctrl Pts',(-21.4673969827414,12.5383275950027,
130.31950305487)) ;
#117420 = CARTESIAN_POINT('Ctrl Pts',(-21.5589884850291,12.4398166155699,
130.554035906025)) ;
#117421 = CARTESIAN_POINT('Ctrl Pts',(-21.6569056837699,12.4114725014285,
130.806774281656)) ;
#117422 = CARTESIAN_POINT('Ctrl Pts',(-21.7533528899772,12.4557968837197,
131.05548625053)) ;
#117423 = CARTESIAN_POINT('Ctrl Pts',(-21.8432789043905,12.5696290703402,
131.285000886597)) ;
#117424 = CARTESIAN_POINT('Ctrl Pts',(-21.9201726688622,12.7436129145437,
131.476639481316)) ;
#117425 = CARTESIAN_POINT('Ctrl Pts',(-21.9802672632297,12.9681021997866,
131.618894855905)) ;
#117426 = CARTESIAN_POINT('Ctrl Pts',(-22.0189477125869,13.2239470656193,
131.698804483607)) ;
#117427 = CARTESIAN_POINT('Ctrl Pts',(-22.0347032747222,13.4941632022952,
131.711716289731)) ;
#117428 = CARTESIAN_POINT('Ctrl Pts',(-22.0270640928502,13.7589185594046,
131.656336781611)) ;
#117429 = CARTESIAN_POINT('Ctrl Pts',(-21.9973553870793,13.999834830615,131.536469000517)) ;
#117430 = CARTESIAN_POINT('Ctrl Pts',(-21.9483276850161,14.1997645777198,
131.360124808153)) ;
#117431 = CARTESIAN_POINT('Ctrl Pts',(-21.8841603470841,14.3442636718176,
131.13951370011)) ;
#117432 = CARTESIAN_POINT('Ctrl Pts',(-21.8101465753952,14.4224928178984,
130.890102479285)) ;
#117433 = CARTESIAN_POINT('Ctrl Pts',(-21.7329264414407,14.429171124512,130.631541457606)) ;
#117434 = CARTESIAN_POINT('Ctrl Pts',(-21.6576229271443,14.3636109202534,
130.378296756051)) ;
#117435 = CARTESIAN_POINT('Ctrl Pts',(-21.5913563328133,14.2305642022342,
130.151592715176)) ;
#117436 = CARTESIAN_POINT('Ctrl Pts',(-21.5393783348571,14.0406276478755,
129.966746548751)) ;
#117437 = CARTESIAN_POINT('Ctrl Pts',(-21.5057424380608,13.8058700767644,
129.83536020891)) ;
#117438 = CARTESIAN_POINT('Ctrl Pts',(-21.4938927574469,13.5427809263485,
129.767514290558)) ;
#117439 = CARTESIAN_POINT('Ctrl Pts',(-21.5054182379161,13.2720606343581,
129.768076155216)) ;
#117440 = CARTESIAN_POINT('Ctrl Pts',(-21.5402011630011,13.0118430008048,
129.836532518463)) ;
#117441 = CARTESIAN_POINT('Ctrl Pts',(-21.5962302154441,12.7818788914411,
129.967174419834)) ;
#117442 = CARTESIAN_POINT('Ctrl Pts',(-21.670640798543,12.5968717145733,130.151376252176)) ;
#117443 = CARTESIAN_POINT('Ctrl Pts',(-21.7587635661607,12.471251749294,130.375607689773)) ;
#117444 = CARTESIAN_POINT('Ctrl Pts',(-21.8545581424731,12.4142248024153,
130.62236302727)) ;
#117445 = CARTESIAN_POINT('Ctrl Pts',(-21.9520906421161,12.4291610280905,
130.874226280264)) ;
#117446 = CARTESIAN_POINT('Ctrl Pts',(-22.0455195215998,12.5152749264354,
131.114002208116)) ;
#117447 = CARTESIAN_POINT('Ctrl Pts',(-22.1287010469112,12.6672522037425,
131.323753516195)) ;
#117448 = CARTESIAN_POINT('Ctrl Pts',(-22.1956105072192,12.8714563204239,
131.4862930258)) ;
#117449 = CARTESIAN_POINT('Ctrl Pts',(-22.243376326576,13.1164156174602,131.592674877965)) ;
#117450 = CARTESIAN_POINT('Ctrl Pts',(-22.2686940144247,13.3833143441499,
131.633503423445)) ;
#117451 = CARTESIAN_POINT('Ctrl Pts',(-22.2704874915353,13.6536761481919,
131.605526541394)) ;
#117452 = CARTESIAN_POINT('Ctrl Pts',(-22.24948244657,13.9063303510439,131.511114286094)) ;
#117453 = CARTESIAN_POINT('Ctrl Pts',(-22.20758512911,14.125656517117,131.355457053907)) ;
#117454 = CARTESIAN_POINT('Ctrl Pts',(-22.1492829761526,14.2929703980627,
131.152198443017)) ;
#117455 = CARTESIAN_POINT('Ctrl Pts',(-22.0784214005424,14.3994043116304,
130.911932860175)) ;
#117456 = CARTESIAN_POINT('Ctrl Pts',(-22.0017663750558,14.4351253202173,
130.654948854145)) ;
#117457 = CARTESIAN_POINT('Ctrl Pts',(-21.9250783887851,14.3988243960317,
130.397839099872)) ;
#117458 = CARTESIAN_POINT('Ctrl Pts',(-21.8544672752435,14.2923293352694,
130.158403148621)) ;
#117459 = CARTESIAN_POINT('Ctrl Pts',(-21.796086879611,14.1241731264117,129.95481572673)) ;
#117460 = CARTESIAN_POINT('Ctrl Pts',(-21.7544221874796,13.9051614113411,
129.799931790305)) ;
#117461 = CARTESIAN_POINT('Ctrl Pts',(-21.7335082685694,13.6518311651615,
129.705713043414)) ;
#117462 = CARTESIAN_POINT('Ctrl Pts',(-21.7354233483292,13.3824709073359,
129.678222201939)) ;
#117463 = CARTESIAN_POINT('Ctrl Pts',(-21.7608220827505,13.1154253755206,
129.719260176606)) ;
#117464 = CARTESIAN_POINT('Ctrl Pts',(-21.8086454011538,12.870532700791,129.825813473863)) ;
#117465 = CARTESIAN_POINT('Ctrl Pts',(-21.8760630288498,12.6655371324335,
129.98965053552)) ;
#117466 = CARTESIAN_POINT('Ctrl Pts',(-21.9590806571557,12.5146112693424,
130.199039203273)) ;
#117467 = CARTESIAN_POINT('Ctrl Pts',(-22.0525303154173,12.4289102076434,
130.438877066077)) ;
#117468 = CARTESIAN_POINT('Ctrl Pts',(-22.1499357478845,12.4141896647539,
130.690419940938)) ;
#117469 = CARTESIAN_POINT('Ctrl Pts',(-22.2464800920588,12.4724108271044,
130.939085979188)) ;
#117470 = CARTESIAN_POINT('Ctrl Pts',(-22.3337993299092,12.5978141623982,
131.161227476013)) ;
#117471 = CARTESIAN_POINT('Ctrl Pts',(-22.4080948789666,12.7826551138703,
131.345130318457)) ;
#117472 = CARTESIAN_POINT('Ctrl Pts',(-22.4641606542721,13.013381389437,131.47580076802)) ;
#117473 = CARTESIAN_POINT('Ctrl Pts',(-22.4988395076517,13.2742167666549,
131.543895101829)) ;
#117474 = CARTESIAN_POINT('Ctrl Pts',(-22.5101407381888,13.5450313802589,
131.543790291758)) ;
#117475 = CARTESIAN_POINT('Ctrl Pts',(-22.4982044056219,13.8067210995316,
131.475851915162)) ;
#117476 = CARTESIAN_POINT('Ctrl Pts',(-22.4645746319177,14.0412512155271,
131.34450786244)) ;
#117477 = CARTESIAN_POINT('Ctrl Pts',(-22.4122950867002,14.2318696546287,
131.158634956438)) ;
#117478 = CARTESIAN_POINT('Ctrl Pts',(-22.3456877419971,14.3645252689238,
130.930833330674)) ;
#117479 = CARTESIAN_POINT('Ctrl Pts',(-22.2709959410269,14.4291513639763,
130.679660185262)) ;
#117480 = CARTESIAN_POINT('Ctrl Pts',(-22.1934041314825,14.4223448397237,
130.419851989127)) ;
#117481 = CARTESIAN_POINT('Ctrl Pts',(-22.1194291252965,14.3433928726762,
130.170543084568)) ;
#117482 = CARTESIAN_POINT('Ctrl Pts',(-22.0555971430006,14.1993298116068,
129.951061058198)) ;
#117483 = CARTESIAN_POINT('Ctrl Pts',(-22.0065113703687,13.9988091287191,
129.774469836655)) ;
#117484 = CARTESIAN_POINT('Ctrl Pts',(-21.9768862871608,13.7578102679721,
129.654858267008)) ;
#117485 = CARTESIAN_POINT('Ctrl Pts',(-21.96939073113,13.491649195449,129.59973283208)) ;
#117486 = CARTESIAN_POINT('Ctrl Pts',(-21.9852726561706,13.2223244098795,
129.613124864141)) ;
#117487 = CARTESIAN_POINT('Ctrl Pts',(-22.0242864346578,12.96574693319,129.693881033276)) ;
#117488 = CARTESIAN_POINT('Ctrl Pts',(-22.0841556386316,12.7429297081588,
129.835684633343)) ;
#117489 = CARTESIAN_POINT('Ctrl Pts',(-22.1613403500013,12.5685157395234,
130.028061959146)) ;
#117490 = CARTESIAN_POINT('Ctrl Pts',(-22.2516375164601,12.4549912739037,
130.258564915234)) ;
#117491 = CARTESIAN_POINT('Ctrl Pts',(-22.3478911325682,12.4115665134561,
130.506787270611)) ;
#117492 = CARTESIAN_POINT('Ctrl Pts',(-22.4452527950756,12.439915366976,130.758091824848)) ;
#117493 = CARTESIAN_POINT('Ctrl Pts',(-22.5373117307679,12.5392662703676,
130.993804347961)) ;
#117494 = CARTESIAN_POINT('Ctrl Pts',(-22.617570466028,12.7015765318143,131.195172124663)) ;
#117495 = CARTESIAN_POINT('Ctrl Pts',(-22.6813553440246,12.9151235355211,
131.348450745226)) ;
#117496 = CARTESIAN_POINT('Ctrl Pts',(-22.7250421972977,13.1655123701317,
131.442940664013)) ;
#117497 = CARTESIAN_POINT('Ctrl Pts',(-22.7459884427464,13.435707308921,131.47084115714)) ;
#117498 = CARTESIAN_POINT('Ctrl Pts',(-22.7433276408327,13.7027427336547,
131.430060345605)) ;
#117499 = CARTESIAN_POINT('Ctrl Pts',(-22.7182573822089,13.9504288164231,
131.323744309634)) ;
#117500 = CARTESIAN_POINT('Ctrl Pts',(-22.6730240374832,14.1608970885181,
131.158442255366)) ;
#117501 = CARTESIAN_POINT('Ctrl Pts',(-22.6117684050325,14.3182076506529,
130.946379659081)) ;
#117502 = CARTESIAN_POINT('Ctrl Pts',(-22.5395371501238,14.4114239636762,
130.702243522924)) ;
#117503 = CARTESIAN_POINT('Ctrl Pts',(-22.4623760563283,14.43387114395,130.443760543668)) ;
#117504 = CARTESIAN_POINT('Ctrl Pts',(-22.3862131332903,14.3839736485786,
130.188109535788)) ;
#117505 = CARTESIAN_POINT('Ctrl Pts',(-22.3174374178138,14.2649034164715,
129.95402457402)) ;
#117506 = CARTESIAN_POINT('Ctrl Pts',(-22.2619059919946,14.0862373803975,
129.758759467005)) ;
#117507 = CARTESIAN_POINT('Ctrl Pts',(-22.2239114025602,13.8593710344565,
129.614595036615)) ;
#117508 = CARTESIAN_POINT('Ctrl Pts',(-22.2071929927876,13.6016402973256,
129.532649135829)) ;
#117509 = CARTESIAN_POINT('Ctrl Pts',(-22.2135652103266,13.3309242141033,
129.518127722561)) ;
#117510 = CARTESIAN_POINT('Ctrl Pts',(-22.2433163399307,13.0670234319289,
129.571929224673)) ;
#117511 = CARTESIAN_POINT('Ctrl Pts',(-22.2950002229724,12.828626261272,129.689806885452)) ;
#117512 = CARTESIAN_POINT('Ctrl Pts',(-22.365802048165,12.6324569777035,129.863476559603)) ;
#117513 = CARTESIAN_POINT('Ctrl Pts',(-22.4512496266196,12.4932134027072,
130.079952535297)) ;
#117514 = CARTESIAN_POINT('Ctrl Pts',(-22.5456609744461,12.4206918298189,
130.322713874521)) ;
#117515 = CARTESIAN_POINT('Ctrl Pts',(-22.643660846344,12.4196226590599,130.575832766512)) ;
#117516 = CARTESIAN_POINT('Ctrl Pts',(-22.7387240475708,12.4910154498675,
130.820318212751)) ;
#117517 = CARTESIAN_POINT('Ctrl Pts',(-22.8240998486431,12.6283739089441,
131.036714320096)) ;
#117518 = CARTESIAN_POINT('Ctrl Pts',(-22.8954898572855,12.8237068444054,
131.212026952757)) ;
#117519 = CARTESIAN_POINT('Ctrl Pts',(-22.9476329864119,13.0616748025397,
131.331212538775)) ;
#117520 = CARTESIAN_POINT('Ctrl Pts',(-22.9777884983749,13.3240381252934,
131.386338288127)) ;
#117521 = CARTESIAN_POINT('Ctrl Pts',(-22.984806720309,13.5952492770895,131.37365349371)) ;
#117522 = CARTESIAN_POINT('Ctrl Pts',(-22.9684914873927,13.8544594163448,
131.292756287018)) ;
#117523 = CARTESIAN_POINT('Ctrl Pts',(-22.9309664261002,14.081653901287,131.150031141549)) ;
#117524 = CARTESIAN_POINT('Ctrl Pts',(-22.8758875876101,14.2612879476329,
130.956139962611)) ;
#117525 = CARTESIAN_POINT('Ctrl Pts',(-22.807480111904,14.38176341734,130.723183101685)) ;
#117526 = CARTESIAN_POINT('Ctrl Pts',(-22.7313394071239,14.4336477337376,
130.467559606026)) ;
#117527 = CARTESIAN_POINT('Ctrl Pts',(-22.6537605132197,14.4124734002023,
130.207689335907)) ;
#117528 = CARTESIAN_POINT('Ctrl Pts',(-22.5818879901239,14.3214777532126,
129.964850139128)) ;
#117529 = CARTESIAN_POINT('Ctrl Pts',(-22.5200315465699,14.1652192668134,
129.750907755924)) ;
#117530 = CARTESIAN_POINT('Ctrl Pts',(-22.4744220607307,13.9555650448247,
129.584493284428)) ;
#117531 = CARTESIAN_POINT('Ctrl Pts',(-22.4488665968957,13.7095599731385,
129.476881160954)) ;
#117532 = CARTESIAN_POINT('Ctrl Pts',(-22.4456673420391,13.4405995134717,
129.434259316074)) ;
#117533 = CARTESIAN_POINT('Ctrl Pts',(-22.466134692506,13.1715077445613,129.460914435123)) ;
#117534 = CARTESIAN_POINT('Ctrl Pts',(-22.5090044012617,12.9214880531583,
129.553167187894)) ;
#117535 = CARTESIAN_POINT('Ctrl Pts',(-22.5727363504163,12.7055052901806,
129.706083200255)) ;
#117536 = CARTESIAN_POINT('Ctrl Pts',(-22.6525084041682,12.542519660956,129.906118446746)) ;
#117537 = CARTESIAN_POINT('Ctrl Pts',(-22.7440355247971,12.4416160246637,
130.140380677478)) ;
#117538 = CARTESIAN_POINT('Ctrl Pts',(-22.8419577727742,12.4112449651492,
130.393113475988)) ;
#117539 = CARTESIAN_POINT('Ctrl Pts',(-22.9385842532159,12.4537097184138,
130.642318308563)) ;
#117540 = CARTESIAN_POINT('Ctrl Pts',(-23.0284918398332,12.5652232692769,
130.871894090839)) ;
#117541 = CARTESIAN_POINT('Ctrl Pts',(-23.1059904833147,12.7379440024603,
131.065226412408)) ;
#117542 = CARTESIAN_POINT('Ctrl Pts',(-23.1664409525888,12.9603974208925,
131.208644145665)) ;
#117543 = CARTESIAN_POINT('Ctrl Pts',(-23.2058738661695,13.2156634379738,
131.290722671192)) ;
#117544 = CARTESIAN_POINT('Ctrl Pts',(-23.2223740608505,13.4857933225146,
131.305803982737)) ;
#117545 = CARTESIAN_POINT('Ctrl Pts',(-23.2153757035201,13.7522945834018,
131.252134307635)) ;
#117546 = CARTESIAN_POINT('Ctrl Pts',(-23.1860831994402,13.9943543864371,
131.133424212874)) ;
#117547 = CARTESIAN_POINT('Ctrl Pts',(-23.1377716895793,14.1947045665703,
130.959330792338)) ;
#117548 = CARTESIAN_POINT('Ctrl Pts',(-23.0736751781071,14.341452901732,130.738783006091)) ;
#117549 = CARTESIAN_POINT('Ctrl Pts',(-23.0002138225239,14.4211242912775,
130.491156682117)) ;
#117550 = CARTESIAN_POINT('Ctrl Pts',(-22.9228562469191,14.4300014441918,
130.232122262372)) ;
#117551 = CARTESIAN_POINT('Ctrl Pts',(-22.8475359109816,14.3664766103849,
129.978889630727)) ;
#117552 = CARTESIAN_POINT('Ctrl Pts',(-22.7809795595032,14.2356053057405,
129.751376119369)) ;
#117553 = CARTESIAN_POINT('Ctrl Pts',(-22.7283015195165,14.0463421699273,
129.564345016875)) ;
#117554 = CARTESIAN_POINT('Ctrl Pts',(-22.6942101862441,13.8127313116574,
129.431663289963)) ;
#117555 = CARTESIAN_POINT('Ctrl Pts',(-22.6816965286036,13.5514862656321,
129.362037523503)) ;
#117556 = CARTESIAN_POINT('Ctrl Pts',(-22.6925426421092,13.2797432937496,
129.360489515288)) ;
#117557 = CARTESIAN_POINT('Ctrl Pts',(-22.7265639166718,13.0196142656872,
129.426812143923)) ;
#117558 = CARTESIAN_POINT('Ctrl Pts',(-22.7821800145146,12.7876902930479,
129.556129340797)) ;
#117559 = CARTESIAN_POINT('Ctrl Pts',(-22.8560631060446,12.601531820227,129.738836537011)) ;
#117560 = CARTESIAN_POINT('Ctrl Pts',(-22.9435871387763,12.4742597851615,
129.961412674426)) ;
#117561 = CARTESIAN_POINT('Ctrl Pts',(-23.0393462544556,12.4148459828286,
130.208020099455)) ;
#117562 = CARTESIAN_POINT('Ctrl Pts',(-23.1371787911307,12.4277167902933,
130.460672834474)) ;
#117563 = CARTESIAN_POINT('Ctrl Pts',(-23.230720242296,12.5119511239392,130.700802831838)) ;
#117564 = CARTESIAN_POINT('Ctrl Pts',(-23.3139766894554,12.6612550507726,
130.910919767823)) ;
#117565 = CARTESIAN_POINT('Ctrl Pts',(-23.3818918394962,12.8654797343675,
131.076161928415)) ;
#117566 = CARTESIAN_POINT('Ctrl Pts',(-23.4300486843934,13.1088715380583,
131.183794226756)) ;
#117567 = CARTESIAN_POINT('Ctrl Pts',(-23.4560676914534,13.3752798477322,
131.226678355845)) ;
#117568 = CARTESIAN_POINT('Ctrl Pts',(-23.4585672304719,13.6458119714847,
131.200772103874)) ;
#117569 = CARTESIAN_POINT('Ctrl Pts',(-23.4381500504978,13.8994657965604,
131.108034372121)) ;
#117570 = CARTESIAN_POINT('Ctrl Pts',(-23.3970305648326,14.1192748903921,
130.954788430871)) ;
#117571 = CARTESIAN_POINT('Ctrl Pts',(-23.3388505991546,14.289180306213,130.75170335035)) ;
#117572 = CARTESIAN_POINT('Ctrl Pts',(-23.2685796505926,14.3970324953059,
130.513322005132)) ;
#117573 = CARTESIAN_POINT('Ctrl Pts',(-23.1918669872229,14.4351164743851,
130.256093295235)) ;
#117574 = CARTESIAN_POINT('Ctrl Pts',(-23.1151547683793,14.4010787676098,
129.99895063463)) ;
#117575 = CARTESIAN_POINT('Ctrl Pts',(-23.0438797487147,14.2958209234975,
129.757379843871)) ;
#117576 = CARTESIAN_POINT('Ctrl Pts',(-22.9853452749484,14.1296521766069,
129.553460069811)) ;
#117577 = CARTESIAN_POINT('Ctrl Pts',(-22.9431411507693,13.9121761436852,
129.397030923481)) ;
#117578 = CARTESIAN_POINT('Ctrl Pts',(-22.9215986259908,13.659430364987,129.300954719031)) ;
#117579 = CARTESIAN_POINT('Ctrl Pts',(-22.9227710010657,13.3906473352246,
129.271342984019)) ;
#117580 = CARTESIAN_POINT('Ctrl Pts',(-22.9477490187839,13.12154860475,129.310931003686)) ;
#117581 = CARTESIAN_POINT('Ctrl Pts',(-22.9946832883936,12.8774995309081,
129.415117779417)) ;
#117582 = CARTESIAN_POINT('Ctrl Pts',(-23.0618596955509,12.6702279872938,
129.578103482037)) ;
#117583 = CARTESIAN_POINT('Ctrl Pts',(-23.1441807626484,12.5183910771853,
129.785600084306)) ;
#117584 = CARTESIAN_POINT('Ctrl Pts',(-23.2374158209668,12.4302683284587,
130.024797603841)) ;
#117585 = CARTESIAN_POINT('Ctrl Pts',(-23.3354851080601,12.4138255810916,
130.278040824562)) ;
#117586 = CARTESIAN_POINT('Ctrl Pts',(-23.4309623901203,12.469284941687,130.524009939854)) ;
#117587 = CARTESIAN_POINT('Ctrl Pts',(-23.5192303902685,12.5930867722267,
130.748712365455)) ;
#117588 = CARTESIAN_POINT('Ctrl Pts',(-23.5941185443368,12.7771358580158,
130.934261108261)) ;
#117589 = CARTESIAN_POINT('Ctrl Pts',(-23.6505481822479,13.0059648630076,
131.066110013963)) ;
#117590 = CARTESIAN_POINT('Ctrl Pts',(-23.6859230327796,13.266147051347,131.13623790108)) ;
#117591 = CARTESIAN_POINT('Ctrl Pts',(-23.6979431807968,13.536990507266,131.13822821022)) ;
#117592 = CARTESIAN_POINT('Ctrl Pts',(-23.686621463364,13.7997447814263,131.072011498558)) ;
#117593 = CARTESIAN_POINT('Ctrl Pts',(-23.6536279786408,14.0350782594662,
130.942568905358)) ;
#117594 = CARTESIAN_POINT('Ctrl Pts',(-23.6015630359019,14.2276700254763,
130.757191818353)) ;
#117595 = CARTESIAN_POINT('Ctrl Pts',(-23.5359237415765,14.3610390583721,
130.532530125429)) ;
#117596 = CARTESIAN_POINT('Ctrl Pts',(-23.4607912004887,14.4285213443226,
130.279787586806)) ;
#117597 = CARTESIAN_POINT('Ctrl Pts',(-23.3833487009935,14.4233691665642,
130.020486659445)) ;
#117598 = CARTESIAN_POINT('Ctrl Pts',(-23.3093760780976,14.3469901017567,
129.771288961701)) ;
#117599 = CARTESIAN_POINT('Ctrl Pts',(-23.2447416178351,14.2034040422047,
129.549206908219)) ;
#117600 = CARTESIAN_POINT('Ctrl Pts',(-23.1955501320454,14.0056848767319,
129.372560459008)) ;
#117601 = CARTESIAN_POINT('Ctrl Pts',(-23.1651831662936,13.7644936141034,
129.250611487081)) ;
#117602 = CARTESIAN_POINT('Ctrl Pts',(-23.1570313325639,13.5002464496988,
129.193764768034)) ;
#117603 = CARTESIAN_POINT('Ctrl Pts',(-23.17244335945,13.2284058869682,129.205478850498)) ;
#117604 = CARTESIAN_POINT('Ctrl Pts',(-23.2104466819188,12.9739038042497,
129.283643071442)) ;
#117605 = CARTESIAN_POINT('Ctrl Pts',(-23.2700066779842,12.748470453343,129.424347957769)) ;
#117606 = CARTESIAN_POINT('Ctrl Pts',(-23.3465319156382,12.5731123494061,
129.614911120667)) ;
#117607 = CARTESIAN_POINT('Ctrl Pts',(-23.4365877316903,12.4573590885892,
129.844675535288)) ;
#117608 = CARTESIAN_POINT('Ctrl Pts',(-23.5328287006259,12.4118025442917,
130.092830099102)) ;
#117609 = CARTESIAN_POINT('Ctrl Pts',(-23.6302800263178,12.4381298230363,
130.34438605469)) ;
#117610 = CARTESIAN_POINT('Ctrl Pts',(-23.7224239211814,12.5352056579817,
130.580413513911)) ;
#117611 = CARTESIAN_POINT('Ctrl Pts',(-23.8033213508231,12.6963006078304,
130.783546488431)) ;
#117612 = CARTESIAN_POINT('Ctrl Pts',(-23.8675954361833,12.9082756117234,
130.938298311993)) ;
#117613 = CARTESIAN_POINT('Ctrl Pts',(-23.9120498738717,13.1596325354774,
131.034809909213)) ;
#117614 = CARTESIAN_POINT('Ctrl Pts',(-23.9333960142979,13.4259468867853,
131.06433034029)) ;
#117615 = CARTESIAN_POINT('Ctrl Pts',(-23.9315577140667,13.6953761022081,
131.025693667659)) ;
#117616 = CARTESIAN_POINT('Ctrl Pts',(-23.9070542170469,13.9437170228922,
130.92105547931)) ;
#117617 = CARTESIAN_POINT('Ctrl Pts',(-23.8623046093946,14.1557110770192,
130.757127908261)) ;
#117618 = CARTESIAN_POINT('Ctrl Pts',(-23.801544851302,14.3144000142637,130.546576005001)) ;
#117619 = CARTESIAN_POINT('Ctrl Pts',(-23.7295838462157,14.4096307818779,
130.303236352713)) ;
#117620 = CARTESIAN_POINT('Ctrl Pts',(-23.652457485825,14.4343455417677,130.044847948643)) ;
#117621 = CARTESIAN_POINT('Ctrl Pts',(-23.5758603047259,14.3860725443644,
129.78778248944)) ;
#117622 = CARTESIAN_POINT('Ctrl Pts',(-23.5071812655722,14.2695097476577,
129.554170604053)) ;
#117623 = CARTESIAN_POINT('Ctrl Pts',(-23.4509742936636,14.0917908235827,
129.356799362595)) ;
#117624 = CARTESIAN_POINT('Ctrl Pts',(-23.4125523047924,13.8666927964708,
129.211488897753)) ;
#117625 = CARTESIAN_POINT('Ctrl Pts',(-23.3951345162908,13.6093229660632,
129.127454830129)) ;
#117626 = CARTESIAN_POINT('Ctrl Pts',(-23.4008307641857,13.3388432839998,
129.110977590817)) ;
#117627 = CARTESIAN_POINT('Ctrl Pts',(-23.4299496613037,13.0740475195294,
129.162880281939)) ;
#117628 = CARTESIAN_POINT('Ctrl Pts',(-23.481199109324,12.8343947236294,129.279432874347)) ;
#117629 = CARTESIAN_POINT('Ctrl Pts',(-23.5511581873575,12.6378260096104,
129.450809857318)) ;
#117630 = CARTESIAN_POINT('Ctrl Pts',(-23.636245008783,12.496463053358,129.666214477056)) ;
#117631 = CARTESIAN_POINT('Ctrl Pts',(-23.7307304012867,12.4217254212934,
129.909104419076)) ;
#117632 = CARTESIAN_POINT('Ctrl Pts',(-23.8286224227458,12.4187226067802,
130.161940676462)) ;
#117633 = CARTESIAN_POINT('Ctrl Pts',(-23.9235467354779,12.4875916105364,
130.406139022881)) ;
#117634 = CARTESIAN_POINT('Ctrl Pts',(-24.0096166464853,12.6235711646796,
130.624432893392)) ;
#117635 = CARTESIAN_POINT('Ctrl Pts',(-24.0812256433191,12.8167006668533,
130.800511081773)) ;
#117636 = CARTESIAN_POINT('Ctrl Pts',(-24.1340977218945,13.0534699877681,
130.921821215751)) ;
#117637 = CARTESIAN_POINT('Ctrl Pts',(-24.1650674975322,13.316652871898,130.979163090976)) ;
#117638 = CARTESIAN_POINT('Ctrl Pts',(-24.1726847473952,13.5871780619914,
130.968318503901)) ;
#117639 = CARTESIAN_POINT('Ctrl Pts',(-24.1571918674132,13.8461109459276,
130.889950708408)) ;
#117640 = CARTESIAN_POINT('Ctrl Pts',(-24.1202020616415,14.0754122507699,
130.748674888431)) ;
#117641 = CARTESIAN_POINT('Ctrl Pts',(-24.0654386807843,14.2569964936062,
130.555630868985)) ;
#117642 = CARTESIAN_POINT('Ctrl Pts',(-23.9973344144518,14.3792169088182,
130.323565913951)) ;
#117643 = CARTESIAN_POINT('Ctrl Pts',(-23.9215531518041,14.4330645733332,
130.069088286981)) ;
#117644 = CARTESIAN_POINT('Ctrl Pts',(-23.843935936724,14.4142942248449,129.809113443856)) ;
#117645 = CARTESIAN_POINT('Ctrl Pts',(-23.7715313845943,14.3249818846189,
129.564589222325)) ;
#117646 = CARTESIAN_POINT('Ctrl Pts',(-23.7092978479596,14.170040968278,129.349514507389)) ;
#117647 = CARTESIAN_POINT('Ctrl Pts',(-23.6633746311722,13.9629929132432,
129.182370156649)) ;
#117648 = CARTESIAN_POINT('Ctrl Pts',(-23.6370484781814,13.716497262182,129.072318829966)) ;
#117649 = CARTESIAN_POINT('Ctrl Pts',(-23.6332221702439,13.4493823964161,
129.028057143487)) ;
#117650 = CARTESIAN_POINT('Ctrl Pts',(-23.652907637159,13.1794660173532,129.052361195891)) ;
#117651 = CARTESIAN_POINT('Ctrl Pts',(-23.6954564463867,12.9274139550297,
129.14350072815)) ;
#117652 = CARTESIAN_POINT('Ctrl Pts',(-23.7583088038747,12.7115777182511,
129.294045622303)) ;
#117653 = CARTESIAN_POINT('Ctrl Pts',(-23.8376585992602,12.5463884321844,
129.492816673603)) ;
#117654 = CARTESIAN_POINT('Ctrl Pts',(-23.9297100882255,12.4431786925169,
129.728346657304)) ;
#117655 = CARTESIAN_POINT('Ctrl Pts',(-24.0264837858184,12.4112124579401,
129.978093638198)) ;
#117656 = CARTESIAN_POINT('Ctrl Pts',(-24.1235984898852,12.4513454594276,
130.22859406653)) ;
#117657 = CARTESIAN_POINT('Ctrl Pts',(-24.2137616646637,12.5610016830577,
130.458926128585)) ;
#117658 = CARTESIAN_POINT('Ctrl Pts',(-24.2917907983411,12.7322315169158,
130.653770957505)) ;
#117659 = CARTESIAN_POINT('Ctrl Pts',(-24.3528048425234,12.953682166373,130.798815030454)) ;
#117660 = CARTESIAN_POINT('Ctrl Pts',(-24.3927962667222,13.207709520667,130.882592820559)) ;
#117661 = CARTESIAN_POINT('Ctrl Pts',(-24.410024457455,13.477838949959,130.899781358164)) ;
#117662 = CARTESIAN_POINT('Ctrl Pts',(-24.4036676831234,13.7447249701473,
130.847982315876)) ;
#117663 = CARTESIAN_POINT('Ctrl Pts',(-24.375161047068,13.9871378811425,130.731672734363)) ;
#117664 = CARTESIAN_POINT('Ctrl Pts',(-24.3270196390184,14.1900736221216,
130.557859433467)) ;
#117665 = CARTESIAN_POINT('Ctrl Pts',(-24.2638997897065,14.3373317370972,
130.34047792192)) ;
#117666 = CARTESIAN_POINT('Ctrl Pts',(-24.1901979000983,14.4199335161434,
130.091922667675)) ;
#117667 = CARTESIAN_POINT('Ctrl Pts',(-24.1128768889176,14.4307824011819,
129.833010984868)) ;
#117668 = CARTESIAN_POINT('Ctrl Pts',(-24.0372157103295,14.3690285687369,
129.578691757844)) ;
#117669 = CARTESIAN_POINT('Ctrl Pts',(-23.9706215331039,14.240441055026,129.351206228027)) ;
#117670 = CARTESIAN_POINT('Ctrl Pts',(-23.9174273385238,14.0528077050883,
129.162661043568)) ;
#117671 = CARTESIAN_POINT('Ctrl Pts',(-23.8826973596537,13.8202656328653,
129.028106967362)) ;
#117672 = CARTESIAN_POINT('Ctrl Pts',(-23.8694990287969,13.5584446016604,
128.956341170936)) ;
#117673 = CARTESIAN_POINT('Ctrl Pts',(-23.8797470733792,13.2871051677591,
128.95309651991)) ;
#117674 = CARTESIAN_POINT('Ctrl Pts',(-23.913003929438,13.0271137580964,129.017276092719)) ;
#117675 = CARTESIAN_POINT('Ctrl Pts',(-23.9680727824866,12.7938648791111,
129.144962113817)) ;
#117676 = CARTESIAN_POINT('Ctrl Pts',(-24.0413879782623,12.6063348860961,
129.32604954485)) ;
#117677 = CARTESIAN_POINT('Ctrl Pts',(-24.1287279410253,12.4770288288764,
129.548032891267)) ;
#117678 = CARTESIAN_POINT('Ctrl Pts',(-24.224050813435,12.4155889254397,129.793464619769)) ;
#117679 = CARTESIAN_POINT('Ctrl Pts',(-24.322359819618,12.4264045620756,130.047353904498)) ;
#117680 = CARTESIAN_POINT('Ctrl Pts',(-24.4157726362298,12.5084012335638,
130.287230439798)) ;
#117681 = CARTESIAN_POINT('Ctrl Pts',(-24.4995762096403,12.6562045204938,
130.49887414061)) ;
#117682 = CARTESIAN_POINT('Ctrl Pts',(-24.5678017919042,12.8582527624523,
130.665140658846)) ;
#117683 = CARTESIAN_POINT('Ctrl Pts',(-24.6169191275358,13.1022479915201,
130.775364646435)) ;
#117684 = CARTESIAN_POINT('Ctrl Pts',(-24.6434477080034,13.3685510945704,
130.81971558088)) ;
#117685 = CARTESIAN_POINT('Ctrl Pts',(-24.6466154461254,13.6374690116671,
130.795980231762)) ;
#117686 = CARTESIAN_POINT('Ctrl Pts',(-24.6268337461158,13.8926337185126,
130.70500143045)) ;
#117687 = CARTESIAN_POINT('Ctrl Pts',(-24.5862814048627,14.1134973759114,
130.553436720401)) ;
#117688 = CARTESIAN_POINT('Ctrl Pts',(-24.5283747688501,14.2854804463777,
130.351062940108)) ;
#117689 = CARTESIAN_POINT('Ctrl Pts',(-24.4583502405941,14.3949169663802,
130.113406317305)) ;
#117690 = CARTESIAN_POINT('Ctrl Pts',(-24.3820622863036,14.4350950477778,
129.857561187302)) ;
#117691 = CARTESIAN_POINT('Ctrl Pts',(-24.3048294246273,14.4027523557503,
129.59869685969)) ;
#117692 = CARTESIAN_POINT('Ctrl Pts',(-24.2338934400316,14.3004224268776,
129.358411107523)) ;
#117693 = CARTESIAN_POINT('Ctrl Pts',(-24.1743887417905,14.1345848166218,
129.151358775365)) ;
#117694 = CARTESIAN_POINT('Ctrl Pts',(-24.1318770833654,13.9188292644318,
128.994144267598)) ;
#117695 = CARTESIAN_POINT('Ctrl Pts',(-24.109670314531,13.6668968300226,128.896125378668)) ;
#117696 = CARTESIAN_POINT('Ctrl Pts',(-24.1102335611594,13.3982258229591,
128.864722114506)) ;
#117697 = CARTESIAN_POINT('Ctrl Pts',(-24.1343637033151,13.1299460140076,
128.901983111348)) ;
#117698 = CARTESIAN_POINT('Ctrl Pts',(-24.1808902872214,12.883706046321,129.004806420228)) ;
#117699 = CARTESIAN_POINT('Ctrl Pts',(-24.2474801294373,12.6755091493533,
129.166133279341)) ;
#117700 = CARTESIAN_POINT('Ctrl Pts',(-24.3295734455692,12.5215778727762,
129.372898584267)) ;
#117701 = CARTESIAN_POINT('Ctrl Pts',(-24.4227739567097,12.4317802296238,
129.611941575593)) ;
#117702 = CARTESIAN_POINT('Ctrl Pts',(-24.5199503056922,12.4131805085562,
129.862866562425)) ;
#117703 = CARTESIAN_POINT('Ctrl Pts',(-24.6163436963673,12.4668842419267,
130.111240618795)) ;
#117704 = CARTESIAN_POINT('Ctrl Pts',(-24.7045015836318,12.5884449970434,
130.335774968224)) ;
#117705 = CARTESIAN_POINT('Ctrl Pts',(-24.7800708345001,12.7713420307832,
130.523219246622)) ;
#117706 = CARTESIAN_POINT('Ctrl Pts',(-24.8370070768286,12.9988617172705,
130.656586079874)) ;
#117707 = CARTESIAN_POINT('Ctrl Pts',(-24.8731099788845,13.2594912156624,
130.728709369952)) ;
#117708 = CARTESIAN_POINT('Ctrl Pts',(-24.8856748885241,13.528913215532,130.73246060921)) ;
#117709 = CARTESIAN_POINT('Ctrl Pts',(-24.8750994611493,13.7920446626032,
130.668445308032)) ;
#117710 = CARTESIAN_POINT('Ctrl Pts',(-24.8426663011521,14.0286822474636,
130.540601272058)) ;
#117711 = CARTESIAN_POINT('Ctrl Pts',(-24.7911779391248,14.2226476411148,
130.356949256475)) ;
#117712 = CARTESIAN_POINT('Ctrl Pts',(-24.7256794891725,14.3581279629795,
130.132601154518)) ;
#117713 = CARTESIAN_POINT('Ctrl Pts',(-24.6510859996418,14.4275172103506,
129.881595712007)) ;
#117714 = CARTESIAN_POINT('Ctrl Pts',(-24.5730285429095,14.4244373538993,
129.620235686296)) ;
#117715 = CARTESIAN_POINT('Ctrl Pts',(-24.4992922348247,14.3501368659966,
129.371907663713)) ;
#117716 = CARTESIAN_POINT('Ctrl Pts',(-24.4343894489451,14.2089998659338,
129.149115926751)) ;
#117717 = CARTESIAN_POINT('Ctrl Pts',(-24.3845042562601,14.0121252002097,
128.970331894925)) ;
#117718 = CARTESIAN_POINT('Ctrl Pts',(-24.3535289344495,13.771824837408,128.846599032895)) ;
#117719 = CARTESIAN_POINT('Ctrl Pts',(-24.3447605801122,13.5078187869416,
128.787925053611)) ;
#117720 = CARTESIAN_POINT('Ctrl Pts',(-24.3593374965893,13.2372790594901,
128.797377589244)) ;
#117721 = CARTESIAN_POINT('Ctrl Pts',(-24.3968788753453,12.9804327969093,
128.873981225353)) ;
#117722 = CARTESIAN_POINT('Ctrl Pts',(-24.4559404822289,12.7540239326364,
129.013240141807)) ;
#117723 = CARTESIAN_POINT('Ctrl Pts',(-24.531902751001,12.5774627760268,129.202214044801)) ;
#117724 = CARTESIAN_POINT('Ctrl Pts',(-24.6214579569672,12.4598743078943,
129.43058501997)) ;
#117725 = CARTESIAN_POINT('Ctrl Pts',(-24.7180157878552,12.4120040784052,
129.679516293973)) ;
#117726 = CARTESIAN_POINT('Ctrl Pts',(-24.8154715108942,12.4365719244432,
129.931101642148)) ;
#117727 = CARTESIAN_POINT('Ctrl Pts',(-24.9074801725979,12.5311793554758,
130.166872263273)) ;
#117728 = CARTESIAN_POINT('Ctrl Pts',(-24.98908833934,12.6910252858477,130.371967891418)) ;
#117729 = CARTESIAN_POINT('Ctrl Pts',(-25.0537128322214,12.9015545976397,
130.527790346717)) ;
#117730 = CARTESIAN_POINT('Ctrl Pts',(-25.0987003896927,13.1503193803916,
130.62606971385)) ;
#117731 = CARTESIAN_POINT('Ctrl Pts',(-25.1209633642502,13.4198238208766,
130.657834390399)) ;
#117732 = CARTESIAN_POINT('Ctrl Pts',(-25.1197436702009,13.6867201897118,
130.621358969948)) ;
#117733 = CARTESIAN_POINT('Ctrl Pts',(-25.0957857760177,13.9376559886512,
130.518082389912)) ;
#117734 = CARTESIAN_POINT('Ctrl Pts',(-25.0516131934043,14.15024285779,130.35593488202)) ;
#117735 = CARTESIAN_POINT('Ctrl Pts',(-24.9911921923722,14.3108380618515,
130.146327637034)) ;
#117736 = CARTESIAN_POINT('Ctrl Pts',(-24.9194794299346,14.4079445273837,
129.903726724708)) ;
#117737 = CARTESIAN_POINT('Ctrl Pts',(-24.8423372287212,14.4345276708083,
129.645254031341)) ;
#117738 = CARTESIAN_POINT('Ctrl Pts',(-24.7661334231012,14.3888298887491,
129.389568134777)) ;
#117739 = CARTESIAN_POINT('Ctrl Pts',(-24.6967794246489,14.2738285073071,
129.153813837603)) ;
#117740 = CARTESIAN_POINT('Ctrl Pts',(-24.6402004549822,14.0978368978208,
128.955396136012)) ;
#117741 = CARTESIAN_POINT('Ctrl Pts',(-24.6011334207155,13.873540820756,128.808139971139)) ;
#117742 = CARTESIAN_POINT('Ctrl Pts',(-24.5831027131497,13.6168751421622,
128.72232648238)) ;
#117743 = CARTESIAN_POINT('Ctrl Pts',(-24.588135943568,13.3465065043273,128.703910280374)) ;
#117744 = CARTESIAN_POINT('Ctrl Pts',(-24.616558912276,13.0815409163059,128.753816302396)) ;
#117745 = CARTESIAN_POINT('Ctrl Pts',(-24.6671939709622,12.8409648020749,
128.868577387027)) ;
#117746 = CARTESIAN_POINT('Ctrl Pts',(-24.7365720466203,12.6428641094173,
129.038275126448)) ;
#117747 = CARTESIAN_POINT('Ctrl Pts',(-24.822005129513,12.4989647241715,129.254437227158)) ;
#117748 = CARTESIAN_POINT('Ctrl Pts',(-24.9154535440393,12.423107716889,129.494606388429)) ;
#117749 = CARTESIAN_POINT('Ctrl Pts',(-25.0137167725077,12.4177381354183,
129.748391405694)) ;
#117750 = CARTESIAN_POINT('Ctrl Pts',(-25.1087445130681,12.4847094665518,
129.992915516142)) ;
#117751 = CARTESIAN_POINT('Ctrl Pts',(-25.1952478577146,12.6190666936061,
130.212434292899)) ;
#117752 = CARTESIAN_POINT('Ctrl Pts',(-25.2672601104286,12.8107470171755,
130.389708558821)) ;
#117753 = CARTESIAN_POINT('Ctrl Pts',(-25.3206363863023,13.046104708988,130.512545094294)) ;
#117754 = CARTESIAN_POINT('Ctrl Pts',(-25.3522895929508,13.3089102809665,
130.571865598048)) ;
#117755 = CARTESIAN_POINT('Ctrl Pts',(-25.3605922534063,13.5795916473862,
130.563012299063)) ;
#117756 = CARTESIAN_POINT('Ctrl Pts',(-25.3456591401498,13.8398547760041,
130.486182706922)) ;
#117757 = CARTESIAN_POINT('Ctrl Pts',(-25.3091876372828,14.0698648400938,
130.346452999807)) ;
#117758 = CARTESIAN_POINT('Ctrl Pts',(-25.2550551240209,14.2524395531566,
130.155354875779)) ;
#117759 = CARTESIAN_POINT('Ctrl Pts',(-25.1870939300536,14.3767942781604,
129.923628056113)) ;
#117760 = CARTESIAN_POINT('Ctrl Pts',(-25.1116370247179,14.4324209526977,
129.670183261114)) ;
#117761 = CARTESIAN_POINT('Ctrl Pts',(-25.0340417226102,14.4159981333991,
129.410303004524)) ;
#117762 = CARTESIAN_POINT('Ctrl Pts',(-24.9611806568547,14.3283155565982,
129.164334994584)) ;
#117763 = CARTESIAN_POINT('Ctrl Pts',(-24.8987771733635,14.1755659528296,
128.948873846864)) ;
#117764 = CARTESIAN_POINT('Ctrl Pts',(-24.852262446507,13.9699068567355,128.779985228531)) ;
#117765 = CARTESIAN_POINT('Ctrl Pts',(-24.8252895194219,13.7239840394015,
128.668003026794)) ;
#117766 = CARTESIAN_POINT('Ctrl Pts',(-24.8207605382176,13.4571373132025,
128.62168264824)) ;
#117767 = CARTESIAN_POINT('Ctrl Pts',(-24.8399553561379,13.1860385292999,
128.644424296114)) ;
#117768 = CARTESIAN_POINT('Ctrl Pts',(-24.8815110859698,12.9351633483058,
128.73292877833)) ;
#117769 = CARTESIAN_POINT('Ctrl Pts',(-24.9443125871162,12.7162804285951,
128.883050489914)) ;
#117770 = CARTESIAN_POINT('Ctrl Pts',(-25.0229415062978,12.5504602957499,
129.079875923212)) ;
#117771 = CARTESIAN_POINT('Ctrl Pts',(-25.1147675609777,12.445157177056,129.314722815811)) ;
#117772 = CARTESIAN_POINT('Ctrl Pts',(-25.2113285559774,12.4110818139133,
129.563897712835)) ;
#117773 = CARTESIAN_POINT('Ctrl Pts',(-25.3088356645265,12.4493848627241,
129.815436071975)) ;
#117774 = CARTESIAN_POINT('Ctrl Pts',(-25.3987988307639,12.5564279113244,
130.045368057642)) ;
#117775 = CARTESIAN_POINT('Ctrl Pts',(-25.4777792677189,12.7270948639173,
130.242770584934)) ;
#117776 = CARTESIAN_POINT('Ctrl Pts',(-25.5390833290002,12.9467013244188,
130.388779692745)) ;
#117777 = CARTESIAN_POINT('Ctrl Pts',(-25.579809192093,13.2005745310841,130.474625025538)) ;
#117778 = CARTESIAN_POINT('Ctrl Pts',(-25.597592152945,13.4697555759231,130.493529148036)) ;
#117779 = CARTESIAN_POINT('Ctrl Pts',(-25.5920655494427,13.7362551955502,
130.444265292038)) ;
#117780 = CARTESIAN_POINT('Ctrl Pts',(-25.5639199870897,13.9814041489959,
130.328750855533)) ;
#117781 = CARTESIAN_POINT('Ctrl Pts',(-25.5166557810706,14.1841666435664,
130.157762612529)) ;
#117782 = CARTESIAN_POINT('Ctrl Pts',(-25.4535179771181,14.3343211623714,
129.940098533994)) ;
#117783 = CARTESIAN_POINT('Ctrl Pts',(-25.3802391406752,14.418455096693,129.692893970139)) ;
#117784 = CARTESIAN_POINT('Ctrl Pts',(-25.3029064752514,14.4314520041057,
129.433922593139)) ;
#117785 = CARTESIAN_POINT('Ctrl Pts',(-25.227398337514,14.3721435581282,129.180190901468)) ;
#117786 = CARTESIAN_POINT('Ctrl Pts',(-25.1602216705886,14.2453739060394,
128.950905918899)) ;
#117787 = CARTESIAN_POINT('Ctrl Pts',(-25.1063450402745,14.0581567741166,
128.760203803333)) ;
#117788 = CARTESIAN_POINT('Ctrl Pts',(-25.0712590260961,13.8276969055429,
128.624767412558)) ;
#117789 = CARTESIAN_POINT('Ctrl Pts',(-25.0573457795135,13.5670204809412,
128.550974352564)) ;
#117790 = CARTESIAN_POINT('Ctrl Pts',(-25.0668582109147,13.2953787817414,
128.545543170318)) ;
#117791 = CARTESIAN_POINT('Ctrl Pts',(-25.0994943187018,13.0342215951602,
128.607838884911)) ;
#117792 = CARTESIAN_POINT('Ctrl Pts',(-25.1542507866729,12.7992353621788,
128.734494690188)) ;
#117793 = CARTESIAN_POINT('Ctrl Pts',(-25.22669838614,12.6113833751158,128.913239507721)) ;
#117794 = CARTESIAN_POINT('Ctrl Pts',(-25.3137534702574,12.4798504311987,
129.13435679031)) ;
#117795 = CARTESIAN_POINT('Ctrl Pts',(-25.4091104699422,12.4163978737343,
129.379824853837)) ;
#117796 = CARTESIAN_POINT('Ctrl Pts',(-25.50711720003,12.4249214769568,129.632945439815)) ;
#117797 = CARTESIAN_POINT('Ctrl Pts',(-25.6012113649615,12.5053755581291,
129.874638598727)) ;
#117798 = CARTESIAN_POINT('Ctrl Pts',(-25.6849597712776,12.6507858524343,
130.086285179288)) ;
#117799 = CARTESIAN_POINT('Ctrl Pts',(-25.7538861814578,12.8517470379754,
130.254524032593)) ;
#117800 = CARTESIAN_POINT('Ctrl Pts',(-25.8035309429625,13.0945613893121,
130.366327420662)) ;
#117801 = CARTESIAN_POINT('Ctrl Pts',(-25.8308038778984,13.3602125815229,
130.412879679802)) ;
#117802 = CARTESIAN_POINT('Ctrl Pts',(-25.8345999378769,13.6310671509035,
130.390757628165)) ;
#117803 = CARTESIAN_POINT('Ctrl Pts',(-25.8155083574025,13.8852753501133,
130.302003918844)) ;
#117804 = CARTESIAN_POINT('Ctrl Pts',(-25.7755392118652,14.1076160518456,
130.152115623541)) ;
#117805 = CARTESIAN_POINT('Ctrl Pts',(-25.7181892166743,14.2808806548592,
129.951435285494)) ;
#117806 = CARTESIAN_POINT('Ctrl Pts',(-25.6484959082951,14.3926567066995,
129.714749299653)) ;
#117807 = CARTESIAN_POINT('Ctrl Pts',(-25.5717128930641,14.4348969494453,
129.457198833214)) ;
#117808 = CARTESIAN_POINT('Ctrl Pts',(-25.4951381495962,14.4049966963277,
129.20058472654)) ;
#117809 = CARTESIAN_POINT('Ctrl Pts',(-25.4232962621115,14.303792887026,128.957344138201)) ;
#117810 = CARTESIAN_POINT('Ctrl Pts',(-25.363824625125,14.1405203843961,128.750619307371)) ;
#117811 = CARTESIAN_POINT('Ctrl Pts',(-25.3206339986258,13.925819103477,128.591354682337)) ;
#117812 = CARTESIAN_POINT('Ctrl Pts',(-25.2977692410781,13.6747404913737,
128.491427879832)) ;
#117813 = CARTESIAN_POINT('Ctrl Pts',(-25.2977339239315,13.4052256729127,
128.458138778975)) ;
#117814 = CARTESIAN_POINT('Ctrl Pts',(-25.3209945002928,13.1384692552609,
128.493096955899)) ;
#117815 = CARTESIAN_POINT('Ctrl Pts',(-25.3671694617792,12.8897551675282,
128.59467494241)) ;
#117816 = CARTESIAN_POINT('Ctrl Pts',(-25.4329175346433,12.6813708112152,
128.753721852147)) ;
#117817 = CARTESIAN_POINT('Ctrl Pts',(-25.5147153277118,12.5252896551219,
128.959563529951)) ;
#117818 = CARTESIAN_POINT('Ctrl Pts',(-25.6074698502328,12.4335762169434,
129.197379956762)) ;
#117819 = CARTESIAN_POINT('Ctrl Pts',(-25.7049185069326,12.4126069646067,
129.448987978284)) ;
#117820 = CARTESIAN_POINT('Ctrl Pts',(-25.8016946801806,12.4645413585742,
129.698394833031)) ;
#117821 = CARTESIAN_POINT('Ctrl Pts',(-25.8901180162125,12.5845282308657,
129.923698284889)) ;
#117822 = CARTESIAN_POINT('Ctrl Pts',(-25.965890991119,12.7652450506007,130.111852309267)) ;
#117823 = CARTESIAN_POINT('Ctrl Pts',(-26.0234875630242,12.9922346613826,
130.247067297209)) ;
#117824 = CARTESIAN_POINT('Ctrl Pts',(-26.0600124784417,13.250181771579,130.32068333464)) ;
#117825 = CARTESIAN_POINT('Ctrl Pts',(-26.0734713454908,13.5208712081626,
130.326877389697)) ;
#117826 = CARTESIAN_POINT('Ctrl Pts',(-26.0634750774189,13.7852947823376,
130.264454593183)) ;
#117827 = CARTESIAN_POINT('Ctrl Pts',(-26.0315363440698,14.0230293048616,
130.13802460234)) ;
#117828 = CARTESIAN_POINT('Ctrl Pts',(-25.9806388976771,14.2178153725244,
129.956187274352)) ;
#117829 = CARTESIAN_POINT('Ctrl Pts',(-25.915484310865,14.3552930120595,129.732836491923)) ;
#117830 = CARTESIAN_POINT('Ctrl Pts',(-25.84072829782,14.4265292407486,129.481215829229)) ;
#117831 = CARTESIAN_POINT('Ctrl Pts',(-25.7635624076654,14.4257522410885,
129.222849529606)) ;
#117832 = CARTESIAN_POINT('Ctrl Pts',(-25.6889769434919,14.3531912390316,
128.97174979562)) ;
#117833 = CARTESIAN_POINT('Ctrl Pts',(-25.6238945066486,14.2139749778386,
128.748514598009)) ;
#117834 = CARTESIAN_POINT('Ctrl Pts',(-25.5734229709391,14.0181343967752,
128.567943742831)) ;
#117835 = CARTESIAN_POINT('Ctrl Pts',(-25.5419558649472,13.7796846047307,
128.442897581117)) ;
#117836 = CARTESIAN_POINT('Ctrl Pts',(-25.532465946712,13.5155236952114,128.38203152979)) ;
#117837 = CARTESIAN_POINT('Ctrl Pts',(-25.5463615849931,13.2452127497976,
128.38953676012)) ;
#117838 = CARTESIAN_POINT('Ctrl Pts',(-25.5832346236961,12.9877059092876,
128.464185979317)) ;
#117839 = CARTESIAN_POINT('Ctrl Pts',(-25.6416547744771,12.7602061146998,
128.601594688484)) ;
#117840 = CARTESIAN_POINT('Ctrl Pts',(-25.7173212787246,12.5817513014504,
128.789638745255)) ;
#117841 = CARTESIAN_POINT('Ctrl Pts',(-25.8062865385756,12.4625557645347,
129.016393612117)) ;
#117842 = CARTESIAN_POINT('Ctrl Pts',(-25.9028561833619,12.4124303731174,
129.265304380517)) ;
#117843 = CARTESIAN_POINT('Ctrl Pts',(-26.0002209633361,12.4345388042572,
129.516686941127)) ;
#117844 = CARTESIAN_POINT('Ctrl Pts',(-26.0932622644251,12.5283216388457,
129.755168414136)) ;
#117845 = CARTESIAN_POINT('Ctrl Pts',(-26.1743660605688,12.6848122289345,
129.95915801482)) ;
#117846 = CARTESIAN_POINT('Ctrl Pts',(-26.2401044733367,12.8954782844364,
130.117969955362)) ;
#117847 = CARTESIAN_POINT('Ctrl Pts',(-26.2854752226399,13.1430312169486,
130.217447678816)) ;
#117848 = CARTESIAN_POINT('Ctrl Pts',(-26.3084010697088,13.4109716006735,
130.251296348672)) ;
#117849 = CARTESIAN_POINT('Ctrl Pts',(-26.3079132586112,13.6794257001286,
130.216804302598)) ;
#117850 = CARTESIAN_POINT('Ctrl Pts',(-26.2844685673034,13.9314101129575,
130.114982755367)) ;
#117851 = CARTESIAN_POINT('Ctrl Pts',(-26.2409654932688,14.1445006499188,
129.954904200554)) ;
#117852 = CARTESIAN_POINT('Ctrl Pts',(-26.1810638490843,14.30675364297,129.746853736739)) ;
#117853 = CARTESIAN_POINT('Ctrl Pts',(-26.1095277456812,14.4060487021468,
129.504729024047)) ;
#117854 = CARTESIAN_POINT('Ctrl Pts',(-26.032393842977,14.4348548844435,129.246256945444)) ;
#117855 = CARTESIAN_POINT('Ctrl Pts',(-25.9558698637576,14.3909041683382,
128.989537588897)) ;
#117856 = CARTESIAN_POINT('Ctrl Pts',(-25.8865418310219,14.2783347545864,
128.754011972375)) ;
#117857 = CARTESIAN_POINT('Ctrl Pts',(-25.8292402720525,14.1031935593991,
128.553327018804)) ;
#117858 = CARTESIAN_POINT('Ctrl Pts',(-25.7897294043971,13.8800104934357,
128.404795472586)) ;
#117859 = CARTESIAN_POINT('Ctrl Pts',(-25.7711135585255,13.6249527950758,
128.317389710907)) ;
#117860 = CARTESIAN_POINT('Ctrl Pts',(-25.775431115054,13.3547990721566,128.296889369296)) ;
#117861 = CARTESIAN_POINT('Ctrl Pts',(-25.8030534354026,13.0897727529312,
128.34451204004)) ;
#117862 = CARTESIAN_POINT('Ctrl Pts',(-25.8533593061976,12.8467550013015,
128.458114990692)) ;
#117863 = CARTESIAN_POINT('Ctrl Pts',(-25.9222441241804,12.6478124741987,
128.626416287819)) ;
#117864 = CARTESIAN_POINT('Ctrl Pts',(-26.0066708855511,12.5027972402551,
128.839866149716)) ;
#117865 = CARTESIAN_POINT('Ctrl Pts',(-26.100698614946,12.4240443790735,129.08144772251)) ;
#117866 = CARTESIAN_POINT('Ctrl Pts',(-26.199005934577,12.4170503512975,129.335345715064)) ;
#117867 = CARTESIAN_POINT('Ctrl Pts',(-26.2938294993792,12.4817913528845,
129.579397911555)) ;
#117868 = CARTESIAN_POINT('Ctrl Pts',(-26.3806964957364,12.6142900077789,
129.799971178623)) ;
#117869 = CARTESIAN_POINT('Ctrl Pts',(-26.4531055700923,12.8042102941726,
129.978446194113)) ;
#117870 = CARTESIAN_POINT('Ctrl Pts',(-26.5072159038126,13.0388185676317,
130.10337532566)) ;
#117871 = CARTESIAN_POINT('Ctrl Pts',(-26.5395617534597,13.302328429414,130.164572555535)) ;
#117872 = CARTESIAN_POINT('Ctrl Pts',(-26.5484551324724,13.5713413202646,
130.157656507272)) ;
#117873 = CARTESIAN_POINT('Ctrl Pts',(-26.5341679133082,13.8329961698972,
130.082609782339)) ;
#117874 = CARTESIAN_POINT('Ctrl Pts',(-26.4983425431364,14.0635775985236,
129.944847992396)) ;
#117875 = CARTESIAN_POINT('Ctrl Pts',(-26.4445874292823,14.2479536598407,
129.754795364822)) ;
#117876 = CARTESIAN_POINT('Ctrl Pts',(-26.3771852728711,14.3739504234545,
129.524813623163)) ;
#117877 = CARTESIAN_POINT('Ctrl Pts',(-26.3012446932142,14.4320428147267,
129.269680538412)) ;
#117878 = CARTESIAN_POINT('Ctrl Pts',(-26.2238185485464,14.4172275166343,
129.010384196713)) ;
#117879 = CARTESIAN_POINT('Ctrl Pts',(-26.15101057134,14.3318167265824,128.764684803711)) ;
#117880 = CARTESIAN_POINT('Ctrl Pts',(-26.0882559725209,14.1811818661954,
128.548240904809)) ;
#117881 = CARTESIAN_POINT('Ctrl Pts',(-26.0410539159268,13.9759968010836,
128.377204526979)) ;
#117882 = CARTESIAN_POINT('Ctrl Pts',(-26.0135036934613,13.7313492742168,
128.263597377545)) ;
#117883 = CARTESIAN_POINT('Ctrl Pts',(-26.008446515134,13.4634561374574,128.21555732586)) ;
#117884 = CARTESIAN_POINT('Ctrl Pts',(-26.0266130110227,13.1958849564785,
128.235768690404)) ;
#117885 = CARTESIAN_POINT('Ctrl Pts',(-26.0679474653962,12.9412337113468,
128.323225935666)) ;
#117886 = CARTESIAN_POINT('Ctrl Pts',(-26.1296373289063,12.7230235201935,
128.470412014427)) ;
#117887 = CARTESIAN_POINT('Ctrl Pts',(-26.2085605635285,12.5539648159992,
128.667776639854)) ;
#117888 = CARTESIAN_POINT('Ctrl Pts',(-26.2991512181213,12.4477725871464,
128.899377928494)) ;
#117889 = CARTESIAN_POINT('Ctrl Pts',(-26.3963261077533,12.4110238125286,
129.150087833756)) ;
#117890 = CARTESIAN_POINT('Ctrl Pts',(-26.4934436652944,12.4468710259381,
129.400669592641)) ;
#117891 = CARTESIAN_POINT('Ctrl Pts',(-26.5846169547544,12.5531554017273,
129.633780736787)) ;
#117892 = CARTESIAN_POINT('Ctrl Pts',(-26.6633533642397,12.7211113672027,
129.830735256764)) ;
#117893 = CARTESIAN_POINT('Ctrl Pts',(-26.7254238754428,12.9400020306265,
129.978881349517)) ;
#117894 = CARTESIAN_POINT('Ctrl Pts',(-26.7666245201816,13.1921120605742,
130.066251668361)) ;
#117895 = CARTESIAN_POINT('Ctrl Pts',(-26.7852369169418,13.4620045410206,
130.087464045505)) ;
#117896 = CARTESIAN_POINT('Ctrl Pts',(-26.7802665924524,13.7292706250682,
130.039767932798)) ;
#117897 = CARTESIAN_POINT('Ctrl Pts',(-26.7529733274785,13.9738125834417,
129.926960110945)) ;
#117898 = CARTESIAN_POINT('Ctrl Pts',(-26.705968775378,14.1794946936577,129.756508727605)) ;
#117899 = CARTESIAN_POINT('Ctrl Pts',(-26.6430636408078,14.3311259021016,
129.539493754098)) ;
#117900 = CARTESIAN_POINT('Ctrl Pts',(-26.5704211107655,14.4169205484559,
129.294336057586)) ;
#117901 = CARTESIAN_POINT('Ctrl Pts',(-26.4926800660124,14.4320030369242,
129.033973746762)) ;
#117902 = CARTESIAN_POINT('Ctrl Pts',(-26.4174411143122,14.3751243958677,
128.781224876368)) ;
#117903 = CARTESIAN_POINT('Ctrl Pts',(-26.3493726747927,14.2488768695212,
128.549025048048)) ;
#117904 = CARTESIAN_POINT('Ctrl Pts',(-26.295605612608,14.0648019477406,128.35897170667)) ;
#117905 = CARTESIAN_POINT('Ctrl Pts',(-26.2596692630275,13.8343789431172,
128.22087036974)) ;
#117906 = CARTESIAN_POINT('Ctrl Pts',(-26.2452033860871,13.5736072409061,
128.145398162508)) ;
#117907 = CARTESIAN_POINT('Ctrl Pts',(-26.2541085207153,13.3025526358433,
128.138259705612)) ;
#117908 = CARTESIAN_POINT('Ctrl Pts',(-26.2860045190759,13.0417946956511,
128.198505035509)) ;
#117909 = CARTESIAN_POINT('Ctrl Pts',(-26.3399102327703,12.8063141545274,
128.322778456193)) ;
#117910 = CARTESIAN_POINT('Ctrl Pts',(-26.4121917469191,12.6158857625783,
128.50087637384)) ;
#117911 = CARTESIAN_POINT('Ctrl Pts',(-26.4990876279591,12.4825397359329,
128.721479595999)) ;
#117912 = CARTESIAN_POINT('Ctrl Pts',(-26.5940129888447,12.4173081349344,
128.965781411473)) ;
#117913 = CARTESIAN_POINT('Ctrl Pts',(-26.6919317707314,12.4236049843711,
129.218679452647)) ;
#117914 = CARTESIAN_POINT('Ctrl Pts',(-26.7861947841509,12.5018025571804,
129.460884921511)) ;
#117915 = CARTESIAN_POINT('Ctrl Pts',(-26.8705874596301,12.6458565227928,
129.674307979368)) ;
#117916 = CARTESIAN_POINT('Ctrl Pts',(-26.9399304853391,12.8453790155913,
129.843785872194)) ;
#117917 = CARTESIAN_POINT('Ctrl Pts',(-26.990100746493,13.0865651955858,129.957208344523)) ;
#117918 = CARTESIAN_POINT('Ctrl Pts',(-27.018102279043,13.3521426916341,130.005841189711)) ;
#117919 = CARTESIAN_POINT('Ctrl Pts',(-27.02263465622,13.6222556634887,129.985982518834)) ;
#117920 = CARTESIAN_POINT('Ctrl Pts',(-27.0041811090057,13.8783882532463,
129.898944093898)) ;
#117921 = CARTESIAN_POINT('Ctrl Pts',(-26.9646335695461,14.1022120327878,
129.750227079902)) ;
#117922 = CARTESIAN_POINT('Ctrl Pts',(-26.9078686115122,14.2765229338953,
129.551349815167)) ;
#117923 = CARTESIAN_POINT('Ctrl Pts',(-26.8385567991512,14.3902286899454,
129.315812307096)) ;
#117924 = CARTESIAN_POINT('Ctrl Pts',(-26.7617716565815,14.4347769429382,
129.058208230924)) ;
#117925 = CARTESIAN_POINT('Ctrl Pts',(-26.6849778202196,14.4066722645431,
128.800883546346)) ;
#117926 = CARTESIAN_POINT('Ctrl Pts',(-26.613309272385,14.3082119147666,128.558359128021)) ;
#117927 = CARTESIAN_POINT('Ctrl Pts',(-26.5531000001099,14.1460357865502,
128.349317353602)) ;
#117928 = CARTESIAN_POINT('Ctrl Pts',(-26.5094126533137,13.9328084550501,
128.188640550554)) ;
#117929 = CARTESIAN_POINT('Ctrl Pts',(-26.4858992546912,13.6817741223337,
128.086718384594)) ;
#117930 = CARTESIAN_POINT('Ctrl Pts',(-26.4851402376145,13.4140262375942,
128.051507824856)) ;
#117931 = CARTESIAN_POINT('Ctrl Pts',(-26.507882004842,13.1453688529206,128.084742838808)) ;
#117932 = CARTESIAN_POINT('Ctrl Pts',(-26.553013805695,12.8977836855868,128.183554680704)) ;
#117933 = CARTESIAN_POINT('Ctrl Pts',(-26.6187173976324,12.6861562793818,
128.342188636974)) ;
#117934 = CARTESIAN_POINT('Ctrl Pts',(-26.7000075083532,12.5289208756677,
128.546622742812)) ;
#117935 = CARTESIAN_POINT('Ctrl Pts',(-26.7926271999993,12.4351549245617,
128.784006318656)) ;
#117936 = CARTESIAN_POINT('Ctrl Pts',(-26.8898002619232,12.4122393500749,
129.034886075764)) ;
#117937 = CARTESIAN_POINT('Ctrl Pts',(-26.9866994174481,12.4619213661245,
129.284657255046)) ;
#117938 = CARTESIAN_POINT('Ctrl Pts',(-27.0756287380429,12.5803996271663,
129.511357053754)) ;
#117939 = CARTESIAN_POINT('Ctrl Pts',(-27.1516505419193,12.7591298548141,
129.700322405224)) ;
#117940 = CARTESIAN_POINT('Ctrl Pts',(-27.2098817946148,12.9850686452271,
129.837367763896)) ;
#117941 = CARTESIAN_POINT('Ctrl Pts',(-27.2470544937516,13.2423776276029,
129.912878159897)) ;
#117942 = CARTESIAN_POINT('Ctrl Pts',(-27.2611859668007,13.5129448157843,
129.921038532251)) ;
#117943 = CARTESIAN_POINT('Ctrl Pts',(-27.2519206533289,13.77743197275,129.860810679802)) ;
#117944 = CARTESIAN_POINT('Ctrl Pts',(-27.2205158418916,14.0166133244865,
129.73587144029)) ;
#117945 = CARTESIAN_POINT('Ctrl Pts',(-27.1704319083102,14.2120829890599,
129.556582398162)) ;
#117946 = CARTESIAN_POINT('Ctrl Pts',(-27.1051769675512,14.3524988741423,
129.332692223217)) ;
#117947 = CARTESIAN_POINT('Ctrl Pts',(-27.0308341297757,14.4253825551606,
129.082395350761)) ;
#117948 = CARTESIAN_POINT('Ctrl Pts',(-26.9535452058579,14.4267683079455,
128.823609311485)) ;
#117949 = CARTESIAN_POINT('Ctrl Pts',(-26.8789617854659,14.3564920605334,
128.572604483849)) ;
#117950 = CARTESIAN_POINT('Ctrl Pts',(-26.8132943369783,14.2186720033249,
128.347542708609)) ;
#117951 = CARTESIAN_POINT('Ctrl Pts',(-26.7623884221237,14.024316870989,128.165726044755)) ;
#117952 = CARTESIAN_POINT('Ctrl Pts',(-26.7303308114293,13.7866137007774,
128.038923620383)) ;
#117953 = CARTESIAN_POINT('Ctrl Pts',(-26.7202102299333,13.5238037993467,
127.976325040153)) ;
#117954 = CARTESIAN_POINT('Ctrl Pts',(-26.7333939658771,13.2527086934904,
127.981667146045)) ;
#117955 = CARTESIAN_POINT('Ctrl Pts',(-26.7698781643314,12.9936531386933,
128.05504873943)) ;
#117956 = CARTESIAN_POINT('Ctrl Pts',(-26.8274902750571,12.7662442453604,
128.190263050934)) ;
#117957 = CARTESIAN_POINT('Ctrl Pts',(-26.9028158586766,12.5858801794281,
128.377254060625)) ;
#117958 = CARTESIAN_POINT('Ctrl Pts',(-26.9915580162282,12.4648530906934,
128.603338840857)) ;
#117959 = CARTESIAN_POINT('Ctrl Pts',(-27.0881560037959,12.4128201898405,
128.852283164429)) ;
#117960 = CARTESIAN_POINT('Ctrl Pts',(-27.1851902816751,12.4330274008567,
129.102825190585)) ;
#117961 = CARTESIAN_POINT('Ctrl Pts',(-27.2780530128695,12.5240123078526,
129.340946985109)) ;
#117962 = CARTESIAN_POINT('Ctrl Pts',(-27.3600745221437,12.6795221093343,
129.547422309088)) ;
#117963 = CARTESIAN_POINT('Ctrl Pts',(-27.4262707883137,12.8889213981569,
129.707582915231)) ;
#117964 = CARTESIAN_POINT('Ctrl Pts',(-27.4722816893973,13.1354946974878,
129.80894186709)) ;
#117965 = CARTESIAN_POINT('Ctrl Pts',(-27.495909604768,13.4042911387148,129.844701076616)) ;
#117966 = CARTESIAN_POINT('Ctrl Pts',(-27.4959972441499,13.6719452303359,
129.812014408763)) ;
#117967 = CARTESIAN_POINT('Ctrl Pts',(-27.4732881371598,13.9242175359662,
129.712414853415)) ;
#117968 = CARTESIAN_POINT('Ctrl Pts',(-27.4302643966516,14.1390288765416,
129.553676677621)) ;
#117969 = CARTESIAN_POINT('Ctrl Pts',(-27.3707186087652,14.3030286155002,
129.346643794136)) ;
#117970 = CARTESIAN_POINT('Ctrl Pts',(-27.2993922220818,14.4041953321141,
129.105118341883)) ;
#117971 = CARTESIAN_POINT('Ctrl Pts',(-27.2225719034685,14.4349854776255,
128.847663054287)) ;
#117972 = CARTESIAN_POINT('Ctrl Pts',(-27.1459254586502,14.3934046912769,
128.590588216205)) ;
#117973 = CARTESIAN_POINT('Ctrl Pts',(-27.0760780136377,14.2822103213118,
128.353421767456)) ;
#117974 = CARTESIAN_POINT('Ctrl Pts',(-27.0186893527385,14.1097942547729,
128.152689099485)) ;
#117975 = CARTESIAN_POINT('Ctrl Pts',(-26.9784352679952,13.8877667397205,
128.001937919195)) ;
#117976 = CARTESIAN_POINT('Ctrl Pts',(-26.9591052561151,13.6324084843775,
127.912318673804)) ;
#117977 = CARTESIAN_POINT('Ctrl Pts',(-26.9627611736166,13.362418602374,127.88989100727)) ;
#117978 = CARTESIAN_POINT('Ctrl Pts',(-26.9898328416053,13.0965815355502,
127.935846808179)) ;
#117979 = CARTESIAN_POINT('Ctrl Pts',(-27.039223966776,12.8540736750208,128.046978106092)) ;
#117980 = CARTESIAN_POINT('Ctrl Pts',(-27.1076603275563,12.6529924848678,
128.213894702152)) ;
#117981 = CARTESIAN_POINT('Ctrl Pts',(-27.1922326941678,12.5055874669249,
128.427587444676)) ;
#117982 = CARTESIAN_POINT('Ctrl Pts',(-27.285639381657,12.4255318802945,128.667511983218)) ;
#117983 = CARTESIAN_POINT('Ctrl Pts',(-27.3834767186371,12.4160627421656,
128.920186580923)) ;
#117984 = CARTESIAN_POINT('Ctrl Pts',(-27.4789408405044,12.4788298708389,
129.16594996465)) ;
#117985 = CARTESIAN_POINT('Ctrl Pts',(-27.5661966226844,12.6096602147663,
129.387635338008)) ;
#117986 = CARTESIAN_POINT('Ctrl Pts',(-27.6392077262574,12.7985461290531,
129.567801300047)) ;
#117987 = CARTESIAN_POINT('Ctrl Pts',(-27.6936999893105,13.0317085131987,
129.693918325502)) ;
#117988 = CARTESIAN_POINT('Ctrl Pts',(-27.7266401612783,13.2930834714085,
129.757042595518)) ;
#117989 = CARTESIAN_POINT('Ctrl Pts',(-27.7363425654746,13.5641923615561,
129.752235268296)) ;
#117990 = CARTESIAN_POINT('Ctrl Pts',(-27.7226448073327,13.825680563738,129.678996462907)) ;
#117991 = CARTESIAN_POINT('Ctrl Pts',(-27.6876244443127,14.0565822354865,
129.543714023441)) ;
#117992 = CARTESIAN_POINT('Ctrl Pts',(-27.6342027276218,14.2434410576494,
129.354513026548)) ;
#117993 = CARTESIAN_POINT('Ctrl Pts',(-27.5668135419715,14.3714533294417,
129.124443036194)) ;
#117994 = CARTESIAN_POINT('Ctrl Pts',(-27.4916575321869,14.4311593636965,
128.871880546709)) ;
#117995 = CARTESIAN_POINT('Ctrl Pts',(-27.4140051961217,14.4188767520017,
128.611838878856)) ;
#117996 = CARTESIAN_POINT('Ctrl Pts',(-27.3408213155295,14.3353894135925,
128.364980603773)) ;
#117997 = CARTESIAN_POINT('Ctrl Pts',(-27.2775273425459,14.1858866633471,
128.146853314981)) ;
#117998 = CARTESIAN_POINT('Ctrl Pts',(-27.2300108576713,13.9829323617686,
127.975041914533)) ;
#117999 = CARTESIAN_POINT('Ctrl Pts',(-27.2017828862075,13.7386002363464,
127.859367243912)) ;
#118000 = CARTESIAN_POINT('Ctrl Pts',(-27.1960189632252,13.4724911093289,
127.809439215144)) ;
#118001 = CARTESIAN_POINT('Ctrl Pts',(-27.2135840337,13.2027754915033,127.827651886763)) ;
#118002 = CARTESIAN_POINT('Ctrl Pts',(-27.2543835497371,12.9475729624172,
127.91355918546)) ;
#118003 = CARTESIAN_POINT('Ctrl Pts',(-27.3154252564457,12.7286906957619,
128.05891829088)) ;
#118004 = CARTESIAN_POINT('Ctrl Pts',(-27.3937085066093,12.5582194265839,
128.254489784026)) ;
#118005 = CARTESIAN_POINT('Ctrl Pts',(-27.4845207555076,12.449581474798,128.486560407069)) ;
#118006 = CARTESIAN_POINT('Ctrl Pts',(-27.5814065424675,12.4111325027633,
128.736500175583)) ;
#118007 = CARTESIAN_POINT('Ctrl Pts',(-27.6783850149472,12.4448573237376,
128.986746017308)) ;
#118008 = CARTESIAN_POINT('Ctrl Pts',(-27.7696066911728,12.5485736287012,
129.220097658122)) ;
#118009 = CARTESIAN_POINT('Ctrl Pts',(-27.8493079778148,12.7160675413709,
129.419637082268)) ;
#118010 = CARTESIAN_POINT('Ctrl Pts',(-27.9115752367297,12.9327061605047,
129.56852821594)) ;
#118011 = CARTESIAN_POINT('Ctrl Pts',(-27.9535772039273,13.1846668295447,
129.658147795149)) ;
#118012 = CARTESIAN_POINT('Ctrl Pts',(-27.9728087721377,13.454422434914,129.68116470926)) ;
#118013 = CARTESIAN_POINT('Ctrl Pts',(-27.9685328637136,13.7215757053134,
129.635554875548)) ;
#118014 = CARTESIAN_POINT('Ctrl Pts',(-27.9418155959324,13.9674105502267,
129.524377068385)) ;
#118015 = CARTESIAN_POINT('Ctrl Pts',(-27.8953947806625,14.1739595025082,
129.355694529026)) ;
#118016 = CARTESIAN_POINT('Ctrl Pts',(-27.833111646103,14.3272528691842,129.140590034414)) ;
#118017 = CARTESIAN_POINT('Ctrl Pts',(-27.7602022571812,14.4155297813334,
128.894429525137)) ;
#118018 = CARTESIAN_POINT('Ctrl Pts',(-27.6829875719055,14.4326688958934,
128.635821913402)) ;
#118019 = CARTESIAN_POINT('Ctrl Pts',(-27.6071356051822,14.3775211091171,
128.381066125451)) ;
#118020 = CARTESIAN_POINT('Ctrl Pts',(-27.539243721018,14.2540409956265,128.149629044627)) ;
#118021 = CARTESIAN_POINT('Ctrl Pts',(-27.4846991991444,14.0709649077151,
127.957153811199)) ;
#118022 = CARTESIAN_POINT('Ctrl Pts',(-27.4482373871036,13.8416200756966,
127.817529893249)) ;
#118023 = CARTESIAN_POINT('Ctrl Pts',(-27.4331199621399,13.5823886653328,
127.740263361054)) ;
#118024 = CARTESIAN_POINT('Ctrl Pts',(-27.4411948007982,13.3112805522026,
127.730691007012)) ;
#118025 = CARTESIAN_POINT('Ctrl Pts',(-27.4726615076401,13.0483998972253,
127.789474656891)) ;
#118026 = CARTESIAN_POINT('Ctrl Pts',(-27.5257417126982,12.8130299251434,
127.911496855804)) ;
#118027 = CARTESIAN_POINT('Ctrl Pts',(-27.5977403806181,12.6204061484624,
128.088659391279)) ;
#118028 = CARTESIAN_POINT('Ctrl Pts',(-27.6842706096557,12.4854479729451,
128.308217781128)) ;
#118029 = CARTESIAN_POINT('Ctrl Pts',(-27.7790489564301,12.4181326854097,
128.552081197838)) ;
#118030 = CARTESIAN_POINT('Ctrl Pts',(-27.8772458109095,12.4224942327925,
128.805703678812)) ;
#118031 = CARTESIAN_POINT('Ctrl Pts',(-27.9715990075916,12.4989652676932,
129.048195975648)) ;
#118032 = CARTESIAN_POINT('Ctrl Pts',(-28.0559858430151,12.6405918868476,
129.261745686545)) ;
#118033 = CARTESIAN_POINT('Ctrl Pts',(-28.1260668022373,12.8391592679731,
129.433283736594)) ;
#118034 = CARTESIAN_POINT('Ctrl Pts',(-28.1769110512927,13.0802458850777,
129.548577043249)) ;
#118035 = CARTESIAN_POINT('Ctrl Pts',(-28.2054175915475,13.3449461423443,
129.598747575716)) ;
#118036 = CARTESIAN_POINT('Ctrl Pts',(-28.2106105175659,13.6142996015355,
129.58092607558)) ;
#118037 = CARTESIAN_POINT('Ctrl Pts',(-28.1928405096762,13.871042063758,129.495894578487)) ;
#118038 = CARTESIAN_POINT('Ctrl Pts',(-28.1538963099053,14.0962487888297,
129.348931858615)) ;
#118039 = CARTESIAN_POINT('Ctrl Pts',(-28.0972007895565,14.2729913868137,
129.150067416087)) ;
#118040 = CARTESIAN_POINT('Ctrl Pts',(-28.0285087313468,14.3876795373717,
128.916519193871)) ;
#118041 = CARTESIAN_POINT('Ctrl Pts',(-27.9519756057037,14.4346057861214,
128.659702361539)) ;
#118042 = CARTESIAN_POINT('Ctrl Pts',(-27.874685639495,14.4082599511792,128.400740873235)) ;
#118043 = CARTESIAN_POINT('Ctrl Pts',(-27.8032210859004,14.3122705937861,
128.159016222046)) ;
#118044 = CARTESIAN_POINT('Ctrl Pts',(-27.742326472995,14.1514361884325,127.947851059364)) ;
#118045 = CARTESIAN_POINT('Ctrl Pts',(-27.6981161142079,13.938718878438,127.785565576013)) ;
#118046 = CARTESIAN_POINT('Ctrl Pts',(-27.6740950339109,13.6904434101565,
127.682412738132)) ;
#118047 = CARTESIAN_POINT('Ctrl Pts',(-27.6726425154201,13.4208420564826,
127.644907773527)) ;
#118048 = CARTESIAN_POINT('Ctrl Pts',(-27.6946457242154,13.1534853885067,
127.676185027627)) ;
#118049 = CARTESIAN_POINT('Ctrl Pts',(-27.7391912414643,12.9044050301422,
127.773201636231)) ;
#118050 = CARTESIAN_POINT('Ctrl Pts',(-27.8044358222147,12.6913476051149,
127.930474372812)) ;
#118051 = CARTESIAN_POINT('Ctrl Pts',(-27.8854293394204,12.5324269089272,
128.134011207475)) ;
#118052 = CARTESIAN_POINT('Ctrl Pts',(-27.9774944389672,12.4369854999087,
128.369889652559)) ;
#118053 = CARTESIAN_POINT('Ctrl Pts',(-28.0748121994469,12.4119049756276,
128.621118828358)) ;
#118054 = CARTESIAN_POINT('Ctrl Pts',(-28.1714853990872,12.4592885776231,
128.870352685515)) ;
#118055 = CARTESIAN_POINT('Ctrl Pts',(-28.2608165469436,12.5757336581161,
129.098197079246)) ;
#118056 = CARTESIAN_POINT('Ctrl Pts',(-28.3373453945994,12.7527802479952,
129.288637876852)) ;
#118057 = CARTESIAN_POINT('Ctrl Pts',(-28.3964441530546,12.9786617700214,
129.428055264009)) ;
#118058 = CARTESIAN_POINT('Ctrl Pts',(-28.434178239495,13.2359087639226,129.50514747171)) ;
#118059 = CARTESIAN_POINT('Ctrl Pts',(-28.448897978943,13.5051025506678,129.515184910968)) ;
#118060 = CARTESIAN_POINT('Ctrl Pts',(-28.4402109620374,13.7711208061555,
129.456502833988)) ;
#118061 = CARTESIAN_POINT('Ctrl Pts',(-28.409511649221,14.0100002848338,129.333795685623)) ;
#118062 = CARTESIAN_POINT('Ctrl Pts',(-28.3598408263846,14.2073723791963,
129.1556415538)) ;
#118063 = CARTESIAN_POINT('Ctrl Pts',(-28.2950348334462,14.3492225893051,
128.933124083885)) ;
#118064 = CARTESIAN_POINT('Ctrl Pts',(-28.2209823020186,14.4242519725476,
128.683712259003)) ;
#118065 = CARTESIAN_POINT('Ctrl Pts',(-28.1433654691918,14.4277364692307,
128.423828382397)) ;
#118066 = CARTESIAN_POINT('Ctrl Pts',(-28.0687197378844,14.3592420521561,
128.172676590865)) ;
#118067 = CARTESIAN_POINT('Ctrl Pts',(-28.0029911633017,14.2240687585133,
127.94759605367)) ;
#118068 = CARTESIAN_POINT('Ctrl Pts',(-27.951382030676,14.030558632252,127.763599842461)) ;
#118069 = CARTESIAN_POINT('Ctrl Pts',(-27.9187982069096,13.7945207204753,
127.6353514582)) ;
#118070 = CARTESIAN_POINT('Ctrl Pts',(-27.9079473566677,13.5313068874669,
127.570501215384)) ;
#118071 = CARTESIAN_POINT('Ctrl Pts',(-27.9204903335361,13.2605193044374,
127.574017800966)) ;
#118072 = CARTESIAN_POINT('Ctrl Pts',(-27.956164420614,13.0015411948259,127.645126607839)) ;
#118073 = CARTESIAN_POINT('Ctrl Pts',(-28.0132085834406,12.7725524549383,
127.778637471497)) ;
#118074 = CARTESIAN_POINT('Ctrl Pts',(-28.0882808220234,12.5901314518039,
127.964801388622)) ;
#118075 = CARTESIAN_POINT('Ctrl Pts',(-28.1766696377702,12.4675131593939,
128.189879182512)) ;
#118076 = CARTESIAN_POINT('Ctrl Pts',(-28.2726948839223,12.4133289167984,
128.437297139227)) ;
#118077 = CARTESIAN_POINT('Ctrl Pts',(-28.3704658057419,12.4315113355368,
128.689755862838)) ;
#118078 = CARTESIAN_POINT('Ctrl Pts',(-28.4632360481242,12.5204618518985,
128.927715630924)) ;
#118079 = CARTESIAN_POINT('Ctrl Pts',(-28.5456402548427,12.6740885345687,
129.135315760515)) ;
#118080 = CARTESIAN_POINT('Ctrl Pts',(-28.6123738489482,12.8820605395618,
129.297054080419)) ;
#118081 = CARTESIAN_POINT('Ctrl Pts',(-28.6590331122904,13.1280848840325,
129.400264284258)) ;
#118082 = CARTESIAN_POINT('Ctrl Pts',(-28.6833089341504,13.3954305340358,
129.438055238725)) ;
#118083 = CARTESIAN_POINT('Ctrl Pts',(-28.6840931743626,13.6647721177767,
129.407220114326)) ;
#118084 = CARTESIAN_POINT('Ctrl Pts',(-28.6621121847327,13.9166503659834,
129.309906441971)) ;
#118085 = CARTESIAN_POINT('Ctrl Pts',(-28.6195959601702,14.1333087838378,
129.152574525308)) ;
#118086 = CARTESIAN_POINT('Ctrl Pts',(-28.5605481815634,14.2989356853765,
128.947034341319)) ;
#118087 = CARTESIAN_POINT('Ctrl Pts',(-28.4890535847478,14.4025578150193,
128.704822107942)) ;
#118088 = CARTESIAN_POINT('Ctrl Pts',(-28.4125691478489,14.4350103975139,
128.448465769779)) ;
#118089 = CARTESIAN_POINT('Ctrl Pts',(-28.3358905451254,14.3956728087921,
128.191327603003)) ;
#118090 = CARTESIAN_POINT('Ctrl Pts',(-28.2657346269624,14.2862787628231,
127.953238888574)) ;
#118091 = CARTESIAN_POINT('Ctrl Pts',(-28.2079489137776,14.1158603656016,
127.751395068649)) ;
#118092 = CARTESIAN_POINT('Ctrl Pts',(-28.1669469057147,13.8934485615438,
127.598238076761)) ;
#118093 = CARTESIAN_POINT('Ctrl Pts',(-28.1471610978907,13.6404741720686,
127.507517955386)) ;
#118094 = CARTESIAN_POINT('Ctrl Pts',(-28.1501382434426,13.3695007769354,
127.482960727044)) ;
#118095 = CARTESIAN_POINT('Ctrl Pts',(-28.1764960356968,13.1044457745781,
127.526973882184)) ;
#118096 = CARTESIAN_POINT('Ctrl Pts',(-28.225181846566,12.8607040814897,127.636031331103)) ;
#118097 = CARTESIAN_POINT('Ctrl Pts',(-28.2937142871452,12.6571155232214,
127.802989653399)) ;
#118098 = CARTESIAN_POINT('Ctrl Pts',(-28.3768619488044,12.5098080882698,
128.012940704154)) ;
#118099 = CARTESIAN_POINT('Ctrl Pts',(-28.4705911940242,12.4266891682411,
128.253596863206)) ;
#118100 = CARTESIAN_POINT('Ctrl Pts',(-28.5686736001448,12.4154229677179,
128.506902117577)) ;
#118101 = CARTESIAN_POINT('Ctrl Pts',(-28.6639498164915,12.4759770344289,
128.752232097602)) ;
#118102 = CARTESIAN_POINT('Ctrl Pts',(-28.7515478234264,12.6048251808736,
128.974917562034)) ;
#118103 = CARTESIAN_POINT('Ctrl Pts',(-28.8250741000503,12.7921644823966,
129.156583452211)) ;
#118104 = CARTESIAN_POINT('Ctrl Pts',(-28.8802512943592,13.0247861234327,
129.284627554489)) ;
#118105 = CARTESIAN_POINT('Ctrl Pts',(-28.9138214071778,13.2853104299406,
129.349634739468)) ;
#118106 = CARTESIAN_POINT('Ctrl Pts',(-28.9241393866765,13.5574329936333,
129.346494578339)) ;
#118107 = CARTESIAN_POINT('Ctrl Pts',(-28.9112612456758,13.8171020410684,
129.275962093259)) ;
#118108 = CARTESIAN_POINT('Ctrl Pts',(-28.8766091041569,14.0511737874882,
129.141473450271)) ;
#118109 = CARTESIAN_POINT('Ctrl Pts',(-28.8236655661538,14.2388281318634,
128.953740433956)) ;
#118110 = CARTESIAN_POINT('Ctrl Pts',(-28.7568581926641,14.3685838894511,
128.725474314568)) ;
#118111 = CARTESIAN_POINT('Ctrl Pts',(-28.6812672811723,14.4305511388163,
128.471385584917)) ;
#118112 = CARTESIAN_POINT('Ctrl Pts',(-28.6041593186733,14.4203097552105,
128.213187763723)) ;
#118113 = CARTESIAN_POINT('Ctrl Pts',(-28.5304223006701,14.3384208536168,
127.964543460545)) ;
#118114 = CARTESIAN_POINT('Ctrl Pts',(-28.4670853954553,14.191573241038,127.746486631087)) ;
#118115 = CARTESIAN_POINT('Ctrl Pts',(-28.4186878189402,13.9880715785311,
127.571796076703)) ;
#118116 = CARTESIAN_POINT('Ctrl Pts',(-28.3901888562639,13.7471726162761,
127.455689629108)) ;
#118117 = CARTESIAN_POINT('Ctrl Pts',(-28.3836245551766,13.4800206998336,
127.403228049252)) ;
#118118 = CARTESIAN_POINT('Ctrl Pts',(-28.4004971163095,13.2110031222513,
127.419530052212)) ;
#118119 = CARTESIAN_POINT('Ctrl Pts',(-28.4406184078603,12.9547749456752,
127.503422585335)) ;
#118120 = CARTESIAN_POINT('Ctrl Pts',(-28.5011655208637,12.7344342581801,
127.647306006591)) ;
#118121 = CARTESIAN_POINT('Ctrl Pts',(-28.5790499129694,12.5623453815543,
127.841701802032)) ;
#118122 = CARTESIAN_POINT('Ctrl Pts',(-28.6693949565012,12.4518692126569,
128.072474343319)) ;
#118123 = CARTESIAN_POINT('Ctrl Pts',(-28.7664627474836,12.4112334904619,
128.322845196979)) ;
#118124 = CARTESIAN_POINT('Ctrl Pts',(-28.8634228465911,12.442749147545,128.573081464854)) ;
#118125 = CARTESIAN_POINT('Ctrl Pts',(-28.9554286612127,12.5456206803201,
128.808503142631)) ;
#118126 = CARTESIAN_POINT('Ctrl Pts',(-29.0344828901899,12.7091960284291,
129.006604080656)) ;
#118127 = CARTESIAN_POINT('Ctrl Pts',(-29.0979031643936,12.9259029795746,
129.158604870418)) ;
#118128 = CARTESIAN_POINT('Ctrl Pts',(-29.1404537451632,13.1770736190436,
129.249849282073)) ;
#118129 = CARTESIAN_POINT('Ctrl Pts',(-29.160380259994,13.446876823357,129.27485767805)) ;
#118130 = CARTESIAN_POINT('Ctrl Pts',(-29.1567650507286,13.7138795618443,
129.231240033964)) ;
#118131 = CARTESIAN_POINT('Ctrl Pts',(-29.1306997030977,13.9605431609207,
129.121973670097)) ;
#118132 = CARTESIAN_POINT('Ctrl Pts',(-29.0848235950521,14.1686235242906,
128.954875473601)) ;
#118133 = CARTESIAN_POINT('Ctrl Pts',(-29.0226188426118,14.324111246448,128.739854084484)) ;
#118134 = CARTESIAN_POINT('Ctrl Pts',(-28.9503351461501,14.4138215674339,
128.495712046884)) ;
#118135 = CARTESIAN_POINT('Ctrl Pts',(-28.8728719219959,14.433194510591,128.236245701094)) ;
#118136 = CARTESIAN_POINT('Ctrl Pts',(-28.7971138201711,14.3801615030747,
127.981866628935)) ;
#118137 = CARTESIAN_POINT('Ctrl Pts',(-28.7288143739679,14.2584943373808,
127.749193854589)) ;
#118138 = CARTESIAN_POINT('Ctrl Pts',(-28.6738445624091,14.0770492595335,
127.555495097218)) ;
#118139 = CARTESIAN_POINT('Ctrl Pts',(-28.6367355115923,13.8484876221982,
127.413928530958)) ;
#118140 = CARTESIAN_POINT('Ctrl Pts',(-28.6210283832256,13.5893551833119,
127.334883350605)) ;
#118141 = CARTESIAN_POINT('Ctrl Pts',(-28.6284008712887,13.3196923685202,
127.323428440679)) ;
#118142 = CARTESIAN_POINT('Ctrl Pts',(-28.6591285906283,13.0561135108425,
127.380035823894)) ;
#118143 = CARTESIAN_POINT('Ctrl Pts',(-28.7117612730956,12.8190742431854,
127.500662990414)) ;
#118144 = CARTESIAN_POINT('Ctrl Pts',(-28.7832377724029,12.6252976951711,
127.676332558911)) ;
#118145 = CARTESIAN_POINT('Ctrl Pts',(-28.8690809391331,12.4887797495905,
127.894002489034)) ;
#118146 = CARTESIAN_POINT('Ctrl Pts',(-28.9640456085277,12.4190606643947,
128.138280288588)) ;
#118147 = CARTESIAN_POINT('Ctrl Pts',(-29.0618810901176,12.4213023126393,
128.390972937899)) ;
#118148 = CARTESIAN_POINT('Ctrl Pts',(-29.1564753036058,12.4953371872364,
128.634164403093)) ;
#118149 = CARTESIAN_POINT('Ctrl Pts',(-29.2416400202375,12.6358732180601,
128.849823957107)) ;
#118150 = CARTESIAN_POINT('Ctrl Pts',(-29.3119790802921,12.8325868641011,
129.022206276767)) ;
#118151 = CARTESIAN_POINT('Ctrl Pts',(-29.3633296045166,13.0715961519443,
129.139105648325)) ;
#118152 = CARTESIAN_POINT('Ctrl Pts',(-29.3927074261657,13.3366927750057,
129.191707126252)) ;
#118153 = CARTESIAN_POINT('Ctrl Pts',(-29.3985768140557,13.606785296831,129.175787373953)) ;
#118154 = CARTESIAN_POINT('Ctrl Pts',(-29.3814203497901,13.8640946124835,
129.092554350732)) ;
#118155 = CARTESIAN_POINT('Ctrl Pts',(-29.343171418544,14.0898396891215,128.947718536782)) ;
#118156 = CARTESIAN_POINT('Ctrl Pts',(-29.2869989434222,14.2683601358406,
128.75038942018)) ;
#118157 = CARTESIAN_POINT('Ctrl Pts',(-29.2183282878595,14.3854877046267,
128.516772892733)) ;
#118158 = CARTESIAN_POINT('Ctrl Pts',(-29.1418332811828,14.4341894572121,
128.260036672281)) ;
#118159 = CARTESIAN_POINT('Ctrl Pts',(-29.0649019264552,14.4102459921106,
128.002309393832)) ;
#118160 = CARTESIAN_POINT('Ctrl Pts',(-28.992797144068,14.3157190634071,127.758526648473)) ;
#118161 = CARTESIAN_POINT('Ctrl Pts',(-28.9318649553926,14.1574303068782,
127.547443662481)) ;
#118162 = CARTESIAN_POINT('Ctrl Pts',(-28.8869190669663,13.9458829151207,
127.382942524456)) ;
#118163 = CARTESIAN_POINT('Ctrl Pts',(-28.8622213277086,13.6969896292084,
127.277637199178)) ;
#118164 = CARTESIAN_POINT('Ctrl Pts',(-28.8601628813631,13.4292803760991,
127.238560560346)) ;
#118165 = CARTESIAN_POINT('Ctrl Pts',(-28.881365510104,13.161309101516,127.267468442087)) ;
#118166 = CARTESIAN_POINT('Ctrl Pts',(-28.9257769976233,12.9096301866455,
127.363829449715)) ;
#118167 = CARTESIAN_POINT('Ctrl Pts',(-28.9898111411058,12.6977069175332,
127.517935580813)) ;
#118168 = CARTESIAN_POINT('Ctrl Pts',(-29.0706272174786,12.5361591830993,
127.720823430246)) ;
#118169 = CARTESIAN_POINT('Ctrl Pts',(-29.1624465503808,12.4388403169488,
127.955993565838)) ;
#118170 = CARTESIAN_POINT('Ctrl Pts',(-29.2598010006521,12.4115721832676,
128.207292728113)) ;
#118171 = CARTESIAN_POINT('Ctrl Pts',(-29.3566445682897,12.457029405049,128.45700426414)) ;
#118172 = CARTESIAN_POINT('Ctrl Pts',(-29.4460805763726,12.5713337324556,
128.685222690321)) ;
#118173 = CARTESIAN_POINT('Ctrl Pts',(-29.5231255961065,12.7468028195077,
128.877151920439)) ;
#118174 = CARTESIAN_POINT('Ctrl Pts',(-29.5827662875995,12.9715572514285,
129.018148836661)) ;
#118175 = CARTESIAN_POINT('Ctrl Pts',(-29.621127294111,13.2272670730613,129.097177228825)) ;
#118176 = CARTESIAN_POINT('Ctrl Pts',(-29.6365791297085,13.4980618104753,
129.10913652102)) ;
#118177 = CARTESIAN_POINT('Ctrl Pts',(-29.6286710531426,13.7620973804226,
129.053043121291)) ;
#118178 = CARTESIAN_POINT('Ctrl Pts',(-29.5984934663747,14.0037248374368,
128.931633804845)) ;
#118179 = CARTESIAN_POINT('Ctrl Pts',(-29.5492988117199,14.2023999767799,
128.754886608175)) ;
#118180 = CARTESIAN_POINT('Ctrl Pts',(-29.4846658524462,14.3463072474208,
128.532783710775)) ;
#118181 = CARTESIAN_POINT('Ctrl Pts',(-29.4110973983037,14.422940695718,128.284924483478)) ;
#118182 = CARTESIAN_POINT('Ctrl Pts',(-29.3334897330232,14.4287087327574,
128.025061129065)) ;
#118183 = CARTESIAN_POINT('Ctrl Pts',(-29.258638100884,14.3623692114808,127.773301149535)) ;
#118184 = CARTESIAN_POINT('Ctrl Pts',(-29.1923062200584,14.2283780368313,
127.546318276707)) ;
#118185 = CARTESIAN_POINT('Ctrl Pts',(-29.1403623093104,14.0364257268117,
127.361394564376)) ;
#118186 = CARTESIAN_POINT('Ctrl Pts',(-29.1072616567678,13.8020945875402,
127.231726399014)) ;
#118187 = CARTESIAN_POINT('Ctrl Pts',(-29.0957233925479,13.5391614868317,
127.164835509363)) ;
#118188 = CARTESIAN_POINT('Ctrl Pts',(-29.1075472344212,13.2686187848472,
127.166290520158)) ;
#118189 = CARTESIAN_POINT('Ctrl Pts',(-29.1426301460642,13.0086420125285,
127.235617273875)) ;
#118190 = CARTESIAN_POINT('Ctrl Pts',(-29.1988929035827,12.7791081292504,
127.366944131897)) ;
#118191 = CARTESIAN_POINT('Ctrl Pts',(-29.2738449830755,12.5942977815412,
127.552601689651)) ;
#118192 = CARTESIAN_POINT('Ctrl Pts',(-29.3616192086889,12.470297081659,127.776006417397)) ;
#118193 = CARTESIAN_POINT('Ctrl Pts',(-29.4576937562919,12.4139049910115,
128.023496861741)) ;
#118194 = CARTESIAN_POINT('Ctrl Pts',(-29.5551748682929,12.4297924178913,
128.275226478106)) ;
#118195 = CARTESIAN_POINT('Ctrl Pts',(-29.6487814577024,12.5172147153485,
128.515415278977)) ;
#118196 = CARTESIAN_POINT('Ctrl Pts',(-29.7315236720721,12.6696685432672,
128.723981025361)) ;
#118197 = CARTESIAN_POINT('Ctrl Pts',(-29.7983400212672,12.8748935660195,
128.886180011621)) ;
#118198 = CARTESIAN_POINT('Ctrl Pts',(-29.8458033561014,13.1206629009233,
128.991641648077)) ;
#118199 = CARTESIAN_POINT('Ctrl Pts',(-29.8707194251093,13.3874986726008,
129.031327378694)) ;
#118200 = CARTESIAN_POINT('Ctrl Pts',(-29.8721807681616,13.6577700342002,
129.002383109698)) ;
#118201 = CARTESIAN_POINT('Ctrl Pts',(-29.8507362629684,13.9102263509794,
128.906641410683)) ;
#118202 = CARTESIAN_POINT('Ctrl Pts',(-29.8089880561964,14.1273421319092,
128.751696352259)) ;
#118203 = CARTESIAN_POINT('Ctrl Pts',(-29.7499753711012,14.2954362033895,
128.546056522854)) ;
#118204 = CARTESIAN_POINT('Ctrl Pts',(-29.6793771471953,14.4001990487277,
128.30676279706)) ;
#118205 = CARTESIAN_POINT('Ctrl Pts',(-29.6022634084759,14.4351706370755,
128.048249901816)) ;
#118206 = CARTESIAN_POINT('Ctrl Pts',(-29.5259240512111,14.3977719552174,
127.792290143655)) ;
#118207 = CARTESIAN_POINT('Ctrl Pts',(-29.4553374749208,14.2904204351337,
127.552887066617)) ;
#118208 = CARTESIAN_POINT('Ctrl Pts',(-29.396976625912,14.1205426319521,127.349221263366)) ;
#118209 = CARTESIAN_POINT('Ctrl Pts',(-29.3558187577604,13.9015880459834,
127.19594254992)) ;
#118210 = CARTESIAN_POINT('Ctrl Pts',(-29.3351815258141,13.6483197880018,
127.102578325798)) ;
#118211 = CARTESIAN_POINT('Ctrl Pts',(-29.3374965976238,13.3774460440173,
127.076084018573)) ;
#118212 = CARTESIAN_POINT('Ctrl Pts',(-29.3632483250244,13.1115164567619,
127.11826281631)) ;
#118213 = CARTESIAN_POINT('Ctrl Pts',(-29.4112273090806,12.8676277943346,
127.225348651307)) ;
#118214 = CARTESIAN_POINT('Ctrl Pts',(-29.4789001513316,12.6630942095761,
127.389914697204)) ;
#118215 = CARTESIAN_POINT('Ctrl Pts',(-29.5622543716497,12.5128296966432,
127.6002285727)) ;
#118216 = CARTESIAN_POINT('Ctrl Pts',(-29.655782504476,12.42805223675,127.840309014045)) ;
#118217 = CARTESIAN_POINT('Ctrl Pts',(-29.7536636355645,12.4147676661353,
128.093080631668)) ;
#118218 = CARTESIAN_POINT('Ctrl Pts',(-29.8491089640436,12.4732051898518,
128.338902853644)) ;
#118219 = CARTESIAN_POINT('Ctrl Pts',(-29.9373051654279,12.6008829742714,
128.563215033879)) ;
#118220 = CARTESIAN_POINT('Ctrl Pts',(-30.0108837724074,12.7859099614939,
128.745200476699)) ;
#118221 = CARTESIAN_POINT('Ctrl Pts',(-30.0666707267494,13.0171549052487,
128.875047914663)) ;
#118222 = CARTESIAN_POINT('Ctrl Pts',(-30.1009396863754,13.277402309204,128.94205811124)) ;
#118223 = CARTESIAN_POINT('Ctrl Pts',(-30.1119760819593,13.5492090907174,
128.941057414916)) ;
#118224 = CARTESIAN_POINT('Ctrl Pts',(-30.0996900511507,13.8101281640257,
128.872156772245)) ;
#118225 = CARTESIAN_POINT('Ctrl Pts',(-30.0658412126364,14.0442615498891,
128.740177177303)) ;
#118226 = CARTESIAN_POINT('Ctrl Pts',(-30.0129614418644,14.2348996277818,
128.552367794294)) ;
#118227 = CARTESIAN_POINT('Ctrl Pts',(-29.9467812118258,14.365488247491,128.326113063617)) ;
#118228 = CARTESIAN_POINT('Ctrl Pts',(-29.8715551104391,14.429722906614,128.073164206403)) ;
#118229 = CARTESIAN_POINT('Ctrl Pts',(-29.7941603221603,14.4216680373145,
127.814017409384)) ;
#118230 = CARTESIAN_POINT('Ctrl Pts',(-29.7201980568112,14.3417421595957,
127.564708377422)) ;
#118231 = CARTESIAN_POINT('Ctrl Pts',(-29.656483010943,14.1964292169101,127.345520658291)) ;
#118232 = CARTESIAN_POINT('Ctrl Pts',(-29.6077772460928,13.9955519637573,
127.170107835032)) ;
#118233 = CARTESIAN_POINT('Ctrl Pts',(-29.5784336722028,13.7541465447125,
127.051322930281)) ;
#118234 = CARTESIAN_POINT('Ctrl Pts',(-29.5712927220666,13.4873871522708,
126.997186762479)) ;
#118235 = CARTESIAN_POINT('Ctrl Pts',(-29.5874867790851,13.2187119669683,
127.01156199828)) ;
#118236 = CARTESIAN_POINT('Ctrl Pts',(-29.6268275872939,12.9622340924051,
127.093243502757)) ;
#118237 = CARTESIAN_POINT('Ctrl Pts',(-29.6870818963363,12.7396655368573,
127.236122661308)) ;
#118238 = CARTESIAN_POINT('Ctrl Pts',(-29.7645649139523,12.5663130362906,
127.429362402402)) ;
#118239 = CARTESIAN_POINT('Ctrl Pts',(-29.8542359643291,12.4542929852172,
127.658304546946)) ;
#118240 = CARTESIAN_POINT('Ctrl Pts',(-29.9515317793415,12.4113060985389,
127.909226798948)) ;
#118241 = CARTESIAN_POINT('Ctrl Pts',(-30.0483978993712,12.440972973662,128.159239721085)) ;
#118242 = CARTESIAN_POINT('Ctrl Pts',(-30.1401907845487,12.5408195803972,
128.394234115448)) ;
#118243 = CARTESIAN_POINT('Ctrl Pts',(-30.2205767778693,12.7045177215447,
128.595849815702)) ;
#118244 = CARTESIAN_POINT('Ctrl Pts',(-30.2841435840745,12.9194126862855,
128.748414866231)) ;
#118245 = CARTESIAN_POINT('Ctrl Pts',(-30.3272725943575,13.1689179469772,
128.841448687789)) ;
#118246 = CARTESIAN_POINT('Ctrl Pts',(-30.3479588136649,13.4397285772897,
128.868523727985)) ;
#118247 = CARTESIAN_POINT('Ctrl Pts',(-30.3449564456502,13.7064270482981,
128.82677202049)) ;
#118248 = CARTESIAN_POINT('Ctrl Pts',(-30.3195311548179,13.9538862841149,
128.719382880456)) ;
#118249 = CARTESIAN_POINT('Ctrl Pts',(-30.2742133985792,14.1631927449857,
128.553937662438)) ;
#118250 = CARTESIAN_POINT('Ctrl Pts',(-30.2123564115104,14.3205261030357,
128.33990642058)) ;
#118251 = CARTESIAN_POINT('Ctrl Pts',(-30.140400371972,14.4121066368491,128.096766582893)) ;
#118252 = CARTESIAN_POINT('Ctrl Pts',(-30.0629325421194,14.4337042758691,
127.837261507592)) ;
#118253 = CARTESIAN_POINT('Ctrl Pts',(-29.9869630886905,14.3826278342729,
127.582229125902)) ;
#118254 = CARTESIAN_POINT('Ctrl Pts',(-29.9184051994975,14.2628852897391,
127.348821521757)) ;
#118255 = CARTESIAN_POINT('Ctrl Pts',(-29.8629677727426,14.0829262304897,
127.15374414379)) ;
#118256 = CARTESIAN_POINT('Ctrl Pts',(-29.8253177094435,13.8556922728628,
127.010626598534)) ;
#118257 = CARTESIAN_POINT('Ctrl Pts',(-29.8089663723846,13.5972599907668,
126.929704638367)) ;
#118258 = CARTESIAN_POINT('Ctrl Pts',(-29.8155751015149,13.3277680057125,
126.91603611238)) ;
#118259 = CARTESIAN_POINT('Ctrl Pts',(-29.8459893717069,13.0618110658261,
126.971473920296)) ;
#118260 = CARTESIAN_POINT('Ctrl Pts',(-29.8976049223748,12.8260390349159,
127.089438246611)) ;
#118261 = CARTESIAN_POINT('Ctrl Pts',(-29.9688137126878,12.6298697180506,
127.264190142746)) ;
#118262 = CARTESIAN_POINT('Ctrl Pts',(-30.0542930667686,12.4917687928696,
127.480820902016)) ;
#118263 = CARTESIAN_POINT('Ctrl Pts',(-30.1491960832168,12.4199839443985,
127.724877330346)) ;
#118264 = CARTESIAN_POINT('Ctrl Pts',(-30.2469829227126,12.4203084099031,
127.977445944159)) ;
#118265 = CARTESIAN_POINT('Ctrl Pts',(-30.3416052555647,12.4922084263286,
128.220773062018)) ;
#118266 = CARTESIAN_POINT('Ctrl Pts',(-30.4271681599976,12.6309968831691,
128.437577974098)) ;
#118267 = CARTESIAN_POINT('Ctrl Pts',(-30.4980284200408,12.8263310850707,
128.611471879481)) ;
#118268 = CARTESIAN_POINT('Ctrl Pts',(-30.5500880714894,13.0651227719104,
128.730345775696)) ;
#118269 = CARTESIAN_POINT('Ctrl Pts',(-30.5799917287299,13.3295667495973,
128.784515371445)) ;
#118270 = CARTESIAN_POINT('Ctrl Pts',(-30.5865246799036,13.5989123639349,
128.770637027271)) ;
#118271 = CARTESIAN_POINT('Ctrl Pts',(-30.5699655121301,13.8574710596154,
128.689069047576)) ;
#118272 = CARTESIAN_POINT('Ctrl Pts',(-30.5323457648762,14.0837078972677,
128.54615654452)) ;
#118273 = CARTESIAN_POINT('Ctrl Pts',(-30.4767238876144,14.2638191910291,
128.350466442062)) ;
#118274 = CARTESIAN_POINT('Ctrl Pts',(-30.4081138852739,14.3831695722174,
128.116916906689)) ;
#118275 = CARTESIAN_POINT('Ctrl Pts',(-30.3319909445384,14.4337176680091,
127.861377615128)) ;
#118276 = CARTESIAN_POINT('Ctrl Pts',(-30.2549612223786,14.4120588735212,
127.603346669515)) ;
#118277 = CARTESIAN_POINT('Ctrl Pts',(-30.1825342935614,14.3193773095664,
127.358581367932)) ;
#118278 = CARTESIAN_POINT('Ctrl Pts',(-30.1211674273149,14.1628171058123,
127.146222590611)) ;
#118279 = CARTESIAN_POINT('Ctrl Pts',(-30.0756155237359,13.9515916314902,
126.979821977845)) ;
#118280 = CARTESIAN_POINT('Ctrl Pts',(-30.050461370889,13.705523326728,126.873449550959)) ;
#118281 = CARTESIAN_POINT('Ctrl Pts',(-30.047694629407,13.4359481915904,126.832028407442)) ;
#118282 = CARTESIAN_POINT('Ctrl Pts',(-30.0682250191869,13.169026252587,126.85913562874)) ;
#118283 = CARTESIAN_POINT('Ctrl Pts',(-30.1120139572627,12.916272819337,126.95364273637)) ;
#118284 = CARTESIAN_POINT('Ctrl Pts',(-30.1753570929207,12.7036779649805,
127.105819577044)) ;
#118285 = CARTESIAN_POINT('Ctrl Pts',(-30.2555879257156,12.5403117624792,
127.30703937934)) ;
#118286 = CARTESIAN_POINT('Ctrl Pts',(-30.3477768389897,12.4404489594076,
127.543069245436)) ;
#118287 = CARTESIAN_POINT('Ctrl Pts',(-30.4445994007357,12.4114485635984,
127.792975546885)) ;
#118288 = CARTESIAN_POINT('Ctrl Pts',(-30.541500222199,12.4544846359496,128.042874784627)) ;
#118289 = CARTESIAN_POINT('Ctrl Pts',(-30.6315932064016,12.5672617568272,
128.27288531667)) ;
#118290 = CARTESIAN_POINT('Ctrl Pts',(-30.7091172675057,12.7417744672769,
128.466151664717)) ;
#118291 = CARTESIAN_POINT('Ctrl Pts',(-30.7688720388517,12.9633750466865,
128.607760924337)) ;
#118292 = CARTESIAN_POINT('Ctrl Pts',(-30.8082363281393,13.2203111282886,
128.689459648843)) ;
#118293 = CARTESIAN_POINT('Ctrl Pts',(-30.8242398852336,13.4905143177326,
128.703096866433)) ;
#118294 = CARTESIAN_POINT('Ctrl Pts',(-30.8169657794985,13.755021596538,128.648839900988)) ;
#118295 = CARTESIAN_POINT('Ctrl Pts',(-30.7875298285178,13.9967495673617,
128.529724713065)) ;
#118296 = CARTESIAN_POINT('Ctrl Pts',(-30.7387155255935,14.1974242169902,
128.353993085411)) ;
#118297 = CARTESIAN_POINT('Ctrl Pts',(-30.6747667553044,14.3425139654286,
128.134048073582)) ;
#118298 = CARTESIAN_POINT('Ctrl Pts',(-30.6012043043127,14.4218015795288,
127.886103518124)) ;
#118299 = CARTESIAN_POINT('Ctrl Pts',(-30.5232263864792,14.4294553596466,
127.62499654632)) ;
#118300 = CARTESIAN_POINT('Ctrl Pts',(-30.4485854643026,14.3652618643662,
127.374009503978)) ;
#118301 = CARTESIAN_POINT('Ctrl Pts',(-30.382005194927,14.2335997278837,127.146362312716)) ;
#118302 = CARTESIAN_POINT('Ctrl Pts',(-30.3294754572321,14.043065952539,126.959689608292)) ;
#118303 = CARTESIAN_POINT('Ctrl Pts',(-30.2956753204816,13.8093139342674,
126.827907583262)) ;
#118304 = CARTESIAN_POINT('Ctrl Pts',(-30.2835287824806,13.5459140316558,
126.759122107196)) ;
#118305 = CARTESIAN_POINT('Ctrl Pts',(-30.2946484169742,13.2769104618193,
126.75871180703)) ;
#118306 = CARTESIAN_POINT('Ctrl Pts',(-30.329022809304,13.0160047166174,126.825934930956)) ;
#118307 = CARTESIAN_POINT('Ctrl Pts',(-30.3848542480685,12.7850162006338,
126.95593843375)) ;
#118308 = CARTESIAN_POINT('Ctrl Pts',(-30.4590572718797,12.5991696538989,
127.139522132046)) ;
#118309 = CARTESIAN_POINT('Ctrl Pts',(-30.5469752382055,12.4727066988936,
127.363172990166)) ;
#118310 = CARTESIAN_POINT('Ctrl Pts',(-30.6424477831083,12.4146340125785,
127.609068863606)) ;
#118311 = CARTESIAN_POINT('Ctrl Pts',(-30.7401818962368,12.4282724622725,
127.861462595189)) ;
#118312 = CARTESIAN_POINT('Ctrl Pts',(-30.8338872261793,12.5136821957653,
128.101978493891)) ;
#118313 = CARTESIAN_POINT('Ctrl Pts',(-30.917003754287,12.6640313593757,128.31166457867)) ;
#118314 = CARTESIAN_POINT('Ctrl Pts',(-30.9847278681875,12.8694014058608,
128.476293188432)) ;
#118315 = CARTESIAN_POINT('Ctrl Pts',(-31.0324410263083,13.1128473164404,
128.582693695894)) ;
#118316 = CARTESIAN_POINT('Ctrl Pts',(-31.0581101474431,13.3794713552814,
128.624552035848)) ;
#118317 = CARTESIAN_POINT('Ctrl Pts',(-31.0602524783805,13.6493875459495,
128.597664462069)) ;
#118318 = CARTESIAN_POINT('Ctrl Pts',(-31.0395778251596,13.9027716733404,
128.504174750462)) ;
#118319 = CARTESIAN_POINT('Ctrl Pts',(-30.9979754649405,14.1226003916879,
128.34939664965)) ;
#118320 = CARTESIAN_POINT('Ctrl Pts',(-30.9399581342553,14.2907614910249,
128.14699206746)) ;
#118321 = CARTESIAN_POINT('Ctrl Pts',(-30.8690051734005,14.3985142710539,
127.906354089039)) ;
#118322 = CARTESIAN_POINT('Ctrl Pts',(-30.7924824842021,14.4350393250775,
127.649796923618)) ;
#118323 = CARTESIAN_POINT('Ctrl Pts',(-30.7159080944081,14.400035592365,127.393090625893)) ;
#118324 = CARTESIAN_POINT('Ctrl Pts',(-30.6448246928201,14.2940192580209,
127.152118703661)) ;
#118325 = CARTESIAN_POINT('Ctrl Pts',(-30.5863183815752,14.1264036829356,
126.948167110242)) ;
#118326 = CARTESIAN_POINT('Ctrl Pts',(-30.5444975557761,13.9087136150407,
126.792930507996)) ;
#118327 = CARTESIAN_POINT('Ctrl Pts',(-30.5232063252145,13.6545233565068,
126.697452847525)) ;
#118328 = CARTESIAN_POINT('Ctrl Pts',(-30.524891337216,13.3858501360358,126.669368708623)) ;
#118329 = CARTESIAN_POINT('Ctrl Pts',(-30.5499389792202,13.11900556216,126.709423409167)) ;
#118330 = CARTESIAN_POINT('Ctrl Pts',(-30.5973969560023,12.8738785752154,
126.81494195181)) ;
#118331 = CARTESIAN_POINT('Ctrl Pts',(-30.6647651473232,12.6676054071639,
126.978537542802)) ;
#118332 = CARTESIAN_POINT('Ctrl Pts',(-30.7476901186471,12.516077131837,127.187642374558)) ;
#118333 = CARTESIAN_POINT('Ctrl Pts',(-30.8405646959683,12.4297444851197,
127.425965717175)) ;
#118334 = CARTESIAN_POINT('Ctrl Pts',(-30.9383003022728,12.4139325771417,
127.678350350006)) ;
#118335 = CARTESIAN_POINT('Ctrl Pts',(-31.0344472399923,12.4708186129552,
127.926022202956)) ;
#118336 = CARTESIAN_POINT('Ctrl Pts',(-31.1222102381147,12.5954480986012,
128.149360733914)) ;
#118337 = CARTESIAN_POINT('Ctrl Pts',(-31.1967512804994,12.7795462403225,
128.333980482879)) ;
#118338 = CARTESIAN_POINT('Ctrl Pts',(-31.2532458302397,13.0105017874409,
128.4657979126)) ;
#118339 = CARTESIAN_POINT('Ctrl Pts',(-31.2881200869954,13.2704658553687,
128.534545422152)) ;
#118340 = CARTESIAN_POINT('Ctrl Pts',(-31.2997537261348,13.5415024018121,
128.535378063465)) ;
#118341 = CARTESIAN_POINT('Ctrl Pts',(-31.288169122968,13.8030869084645,128.468519236206)) ;
#118342 = CARTESIAN_POINT('Ctrl Pts',(-31.254641174514,14.0389746831751,128.337336611109)) ;
#118343 = CARTESIAN_POINT('Ctrl Pts',(-31.2028842012387,14.2290323686529,
128.153196437362)) ;
#118344 = CARTESIAN_POINT('Ctrl Pts',(-31.1365285056857,14.3629000991712,
127.926138023514)) ;
#118345 = CARTESIAN_POINT('Ctrl Pts',(-31.0616081958548,14.4288302625026,
127.67416381072)) ;
#118346 = CARTESIAN_POINT('Ctrl Pts',(-30.98404256555,14.422836536164,127.414443978125)) ;
#118347 = CARTESIAN_POINT('Ctrl Pts',(-30.9101456342738,14.3452102750607,
127.165449135438)) ;
#118348 = CARTESIAN_POINT('Ctrl Pts',(-30.8458926888161,14.2014203774082,
126.944605876018)) ;
#118349 = CARTESIAN_POINT('Ctrl Pts',(-30.7967539777331,14.002164262405,126.76797119047)) ;
#118350 = CARTESIAN_POINT('Ctrl Pts',(-30.7667868700996,13.7617532002817,
126.64736275973)) ;
#118351 = CARTESIAN_POINT('Ctrl Pts',(-30.7589404789089,13.4956080912223,
126.591189468115)) ;
#118352 = CARTESIAN_POINT('Ctrl Pts',(-30.7744975468887,13.2262846444733,
126.603638049819)) ;
#118353 = CARTESIAN_POINT('Ctrl Pts',(-30.8130435438419,12.9698877409975,
126.683104985907)) ;
#118354 = CARTESIAN_POINT('Ctrl Pts',(-30.8727944794778,12.7457364397051,
126.82445862299)) ;
#118355 = CARTESIAN_POINT('Ctrl Pts',(-30.9496439744757,12.5708017682082,
127.015910626943)) ;
#118356 = CARTESIAN_POINT('Ctrl Pts',(-31.0398838023028,12.456149717707,127.24620830676)) ;
#118357 = CARTESIAN_POINT('Ctrl Pts',(-31.1360199136021,12.4116404870963,
127.494111078372)) ;
#118358 = CARTESIAN_POINT('Ctrl Pts',(-31.2337338612294,12.4391729305521,
127.746332624112)) ;
#118359 = CARTESIAN_POINT('Ctrl Pts',(-31.3254925425336,12.5371797605548,
127.981319248925)) ;
#118360 = CARTESIAN_POINT('Ctrl Pts',(-31.4060511368076,12.6985743465351,
128.183537479242)) ;
#118361 = CARTESIAN_POINT('Ctrl Pts',(-31.4702234675365,12.9117741381151,
128.337900585384)) ;
#118362 = CARTESIAN_POINT('Ctrl Pts',(-31.5142368155557,13.1624013185224,
128.433269095099)) ;
#118363 = CARTESIAN_POINT('Ctrl Pts',(-31.5354063774495,13.430527916598,128.462060753588)) ;
#118364 = CARTESIAN_POINT('Ctrl Pts',(-31.5331866509304,13.6988963503242,
128.422426334552)) ;
#118365 = CARTESIAN_POINT('Ctrl Pts',(-31.5083514057842,13.9472005331235,
128.316764555466)) ;
#118366 = CARTESIAN_POINT('Ctrl Pts',(-31.4634662153984,14.1580510542122,
128.152528884923)) ;
#118367 = CARTESIAN_POINT('Ctrl Pts',(-31.4022864663549,14.3165352263592,
127.940620929915)) ;
#118368 = CARTESIAN_POINT('Ctrl Pts',(-31.3302015606746,14.4105996600904,
127.696931825965)) ;
#118369 = CARTESIAN_POINT('Ctrl Pts',(-31.2530012510953,14.4340684661328,
127.438305075934)) ;
#118370 = CARTESIAN_POINT('Ctrl Pts',(-31.1767797421025,14.3850544028617,
127.182480796763)) ;
#118371 = CARTESIAN_POINT('Ctrl Pts',(-31.1079347894914,14.2669952592305,
126.948227958792)) ;
#118372 = CARTESIAN_POINT('Ctrl Pts',(-31.0521981502,14.08911548236,126.752366622373)) ;
#118373 = CARTESIAN_POINT('Ctrl Pts',(-31.0139044640317,13.8629229464963,
126.60733955489)) ;
#118374 = CARTESIAN_POINT('Ctrl Pts',(-30.996875692622,13.604494449949,126.524362266426)) ;
#118375 = CARTESIAN_POINT('Ctrl Pts',(-31.0029129348444,13.3352196406284,
126.509036582526)) ;
#118376 = CARTESIAN_POINT('Ctrl Pts',(-31.0323468270102,13.0705830393377,
126.561846564007)) ;
#118377 = CARTESIAN_POINT('Ctrl Pts',(-31.0837316199208,12.8316693122143,
126.678854555658)) ;
#118378 = CARTESIAN_POINT('Ctrl Pts',(-31.1546013076082,12.6342706901117,
126.852600636445)) ;
#118379 = CARTESIAN_POINT('Ctrl Pts',(-31.2394140271486,12.4949548455415,
127.067408352085)) ;
#118380 = CARTESIAN_POINT('Ctrl Pts',(-31.334148974029,12.421067631229,127.310966017458)) ;
#118381 = CARTESIAN_POINT('Ctrl Pts',(-31.4318092831184,12.4192534681359,
127.563206519924)) ;
#118382 = CARTESIAN_POINT('Ctrl Pts',(-31.5267833807971,12.4890550596445,
127.807509458574)) ;
#118383 = CARTESIAN_POINT('Ctrl Pts',(-31.6130103693316,12.6269264793826,
128.026107667869)) ;
#118384 = CARTESIAN_POINT('Ctrl Pts',(-31.683886847537,12.8196494832229,128.200260557426)) ;
#118385 = CARTESIAN_POINT('Ctrl Pts',(-31.7367312073383,13.0580835296679,
128.321322833757)) ;
#118386 = CARTESIAN_POINT('Ctrl Pts',(-31.7672152209321,13.321466149626,128.377268196697)) ;
#118387 = CARTESIAN_POINT('Ctrl Pts',(-31.7744327469934,13.5912986837364,
128.365332689352)) ;
#118388 = CARTESIAN_POINT('Ctrl Pts',(-31.7586348495878,13.8497218506693,
128.286100562908)) ;
#118389 = CARTESIAN_POINT('Ctrl Pts',(-31.7212629287116,14.0789422009193,
128.14363667606)) ;
#118390 = CARTESIAN_POINT('Ctrl Pts',(-31.6661208521593,14.2597600748466,
127.94943795922)) ;
#118391 = CARTESIAN_POINT('Ctrl Pts',(-31.5980586744624,14.3805241466999,
127.717602294976)) ;
#118392 = CARTESIAN_POINT('Ctrl Pts',(-31.5221682369762,14.4333051039602,
127.462785155928)) ;
#118393 = CARTESIAN_POINT('Ctrl Pts',(-31.444773905692,14.4135763254968,127.203549201476)) ;
#118394 = CARTESIAN_POINT('Ctrl Pts',(-31.3722256183231,14.3230160042054,
126.958490867883)) ;
#118395 = CARTESIAN_POINT('Ctrl Pts',(-31.3102615819759,14.1669880886898,
126.744210913267)) ;
#118396 = CARTESIAN_POINT('Ctrl Pts',(-31.2647484696902,13.9601855279978,
126.578397395436)) ;
#118397 = CARTESIAN_POINT('Ctrl Pts',(-31.2386090991305,13.7121979850729,
126.468745833126)) ;
#118398 = CARTESIAN_POINT('Ctrl Pts',(-31.2351816147922,13.44532544281,126.425707068262)) ;
#118399 = CARTESIAN_POINT('Ctrl Pts',(-31.2552112460232,13.1756579344581,
126.451027766751)) ;
#118400 = CARTESIAN_POINT('Ctrl Pts',(-31.2978741375129,12.9248371120238,
126.542620270216)) ;
#118401 = CARTESIAN_POINT('Ctrl Pts',(-31.3611235868385,12.7087904185415,
126.694221985858)) ;
#118402 = CARTESIAN_POINT('Ctrl Pts',(-31.4409206069476,12.5441839960965,
126.894217297466)) ;
#118403 = CARTESIAN_POINT('Ctrl Pts',(-31.5328183036128,12.4422953635853,
127.129402084781)) ;
#118404 = CARTESIAN_POINT('Ctrl Pts',(-31.629777727754,12.4112745925655,127.379639841948)) ;
#118405 = CARTESIAN_POINT('Ctrl Pts',(-31.7265865855766,12.4523611217467,
127.629332126508)) ;
#118406 = CARTESIAN_POINT('Ctrl Pts',(-31.8167258433804,12.5627156193445,
127.859574831218)) ;
#118407 = CARTESIAN_POINT('Ctrl Pts',(-31.8949781937964,12.736203215032,128.054846222434)) ;
#118408 = CARTESIAN_POINT('Ctrl Pts',(-31.9551628568403,12.9562236735918,
128.197777042418)) ;
#118409 = CARTESIAN_POINT('Ctrl Pts',(-31.9952052502965,13.212763202245,128.281413268464)) ;
#118410 = CARTESIAN_POINT('Ctrl Pts',(-32.0118603650355,13.4814739437606,
128.297119473937)) ;
#118411 = CARTESIAN_POINT('Ctrl Pts',(-32.0053261625225,13.747602021364,128.244879402817)) ;
#118412 = CARTESIAN_POINT('Ctrl Pts',(-31.976363124372,13.9907502143909,128.127070663906)) ;
#118413 = CARTESIAN_POINT('Ctrl Pts',(-31.9281731309669,14.192126827699,127.953259372413)) ;
#118414 = CARTESIAN_POINT('Ctrl Pts',(-31.8646791619465,14.3392030081547,
127.73466416975)) ;
#118415 = CARTESIAN_POINT('Ctrl Pts',(-31.7907074399582,14.420750007367,127.485261238863)) ;
#118416 = CARTESIAN_POINT('Ctrl Pts',(-31.7134776522141,14.4302362672735,
127.226655866822)) ;
#118417 = CARTESIAN_POINT('Ctrl Pts',(-31.6382657139275,14.3680283061645,
126.973823214759)) ;
#118418 = CARTESIAN_POINT('Ctrl Pts',(-31.5712774337174,14.237554410734,126.74491844459)) ;
#118419 = CARTESIAN_POINT('Ctrl Pts',(-31.5184473639748,14.0487160493496,
126.557435432275)) ;
#118420 = CARTESIAN_POINT('Ctrl Pts',(-31.4842054752315,13.8167884864147,
126.424474538241)) ;
#118421 = CARTESIAN_POINT('Ctrl Pts',(-31.4713351737196,13.5548285940714,
126.353677668392)) ;
#118422 = CARTESIAN_POINT('Ctrl Pts',(-31.4817616498199,13.2844751401064,
126.351080744583)) ;
#118423 = CARTESIAN_POINT('Ctrl Pts',(-31.5156125178178,13.0226684871857,
126.416725531107)) ;
#118424 = CARTESIAN_POINT('Ctrl Pts',(-31.5707227695967,12.7913020649599,
126.544716939095)) ;
#118425 = CARTESIAN_POINT('Ctrl Pts',(-31.6443503598457,12.6040508049077,
126.726654019701)) ;
#118426 = CARTESIAN_POINT('Ctrl Pts',(-31.7318689488069,12.4756114262356,
126.949157250561)) ;
#118427 = CARTESIAN_POINT('Ctrl Pts',(-31.8274955783218,12.4152434956171,
127.195397643288)) ;
#118428 = CARTESIAN_POINT('Ctrl Pts',(-31.9251925407204,12.4269403592131,
127.447704843771)) ;
#118429 = CARTESIAN_POINT('Ctrl Pts',(-32.0188886965611,12.5099952735333,
127.688277904106)) ;
#118430 = CARTESIAN_POINT('Ctrl Pts',(-32.1025075923148,12.6587328614396,
127.899383697514)) ;
#118431 = CARTESIAN_POINT('Ctrl Pts',(-32.1705721069073,12.8618951640278,
128.065119112413)) ;
#118432 = CARTESIAN_POINT('Ctrl Pts',(-32.2191904649823,13.1054069389763,
128.174015366068)) ;
#118433 = CARTESIAN_POINT('Ctrl Pts',(-32.2455028035797,13.3721986649784,
128.21769238138)) ;
#118434 = CARTESIAN_POINT('Ctrl Pts',(-32.2482898332498,13.6415133850086,
128.192782134854)) ;
#118435 = CARTESIAN_POINT('Ctrl Pts',(-32.2283241313474,13.8954057097587,
128.101397608046)) ;
#118436 = CARTESIAN_POINT('Ctrl Pts',(-32.1872523956957,14.1169004603375,
127.948121743342)) ;
#118437 = CARTESIAN_POINT('Ctrl Pts',(-32.1295014317082,14.286862322143,127.74642646493)) ;
#118438 = CARTESIAN_POINT('Ctrl Pts',(-32.0592677095131,14.3960130352986,
127.508092927699)) ;
#118439 = CARTESIAN_POINT('Ctrl Pts',(-31.9825379384265,14.435114922765,127.250792751949)) ;
#118440 = CARTESIAN_POINT('Ctrl Pts',(-31.9057656974593,14.4019052021935,
126.993457606121)) ;
#118441 = CARTESIAN_POINT('Ctrl Pts',(-31.8346583979873,14.2983009170395,
126.752533469883)) ;
#118442 = CARTESIAN_POINT('Ctrl Pts',(-31.7754887850036,14.1317969214597,
126.546520009402)) ;
#118443 = CARTESIAN_POINT('Ctrl Pts',(-31.7332254358825,13.915343377283,126.390014277616)) ;
#118444 = CARTESIAN_POINT('Ctrl Pts',(-31.711360602162,13.6633971798664,126.293043315709)) ;
#118445 = CARTESIAN_POINT('Ctrl Pts',(-31.7122219084162,13.3943409624926,
126.262475507033)) ;
#118446 = CARTESIAN_POINT('Ctrl Pts',(-31.7367708343716,13.1257595222001,
126.300900545406)) ;
#118447 = CARTESIAN_POINT('Ctrl Pts',(-31.7835119755956,12.880696500419,126.404440546327)) ;
#118448 = CARTESIAN_POINT('Ctrl Pts',(-31.850115664228,12.6734734022958,126.565890689936)) ;
#118449 = CARTESIAN_POINT('Ctrl Pts',(-31.9327988513976,12.5195858406816,
126.774213790266)) ;
#118450 = CARTESIAN_POINT('Ctrl Pts',(-32.0259263008221,12.4310932858069,
127.013116469777)) ;
#118451 = CARTESIAN_POINT('Ctrl Pts',(-32.1231083724527,12.4134132661188,
127.264059856825)) ;
#118452 = CARTESIAN_POINT('Ctrl Pts',(-32.2195172413699,12.468118840117,127.512455841876)) ;
#118453 = CARTESIAN_POINT('Ctrl Pts',(-32.3075963273976,12.5909169061166,
127.736717735728)) ;
#118454 = CARTESIAN_POINT('Ctrl Pts',(-32.3825833685287,12.773448841542,127.922642365176)) ;
#118455 = CARTESIAN_POINT('Ctrl Pts',(-32.4396040817083,13.0028153371377,
128.056056344726)) ;
#118456 = CARTESIAN_POINT('Ctrl Pts',(-32.4751933014337,13.2626811935882,
128.126823513117)) ;
#118457 = CARTESIAN_POINT('Ctrl Pts',(-32.4875431224731,13.5323090949329,
128.129920100657)) ;
#118458 = CARTESIAN_POINT('Ctrl Pts',(-32.4765829085235,13.7963542441069,
128.064639049108)) ;
#118459 = CARTESIAN_POINT('Ctrl Pts',(-32.4437139481186,14.0324257207359,
127.93549829729)) ;
#118460 = CARTESIAN_POINT('Ctrl Pts',(-32.3923709591125,14.2243211070582,
127.752507155027)) ;
#118461 = CARTESIAN_POINT('Ctrl Pts',(-32.326532192024,14.3597396565784,127.527047761077)) ;
#118462 = CARTESIAN_POINT('Ctrl Pts',(-32.2515288700067,14.4280132025405,
127.274713443137)) ;
#118463 = CARTESIAN_POINT('Ctrl Pts',(-32.1739944938922,14.424002708898,127.015108039322)) ;
#118464 = CARTESIAN_POINT('Ctrl Pts',(-32.0998540788628,14.3482149181964,
126.765370673455)) ;
#118465 = CARTESIAN_POINT('Ctrl Pts',(-32.035455068552,14.2066839719766,126.544210524556)) ;
#118466 = CARTESIAN_POINT('Ctrl Pts',(-31.9856410382067,14.0084845387879,
126.365519583357)) ;
#118467 = CARTESIAN_POINT('Ctrl Pts',(-31.9550561070796,13.7679164068615,
126.242974606502)) ;
#118468 = CARTESIAN_POINT('Ctrl Pts',(-31.9466445164154,13.5034894092934,
126.185316318488)) ;
#118469 = CARTESIAN_POINT('Ctrl Pts',(-31.9615283223229,13.2335994760701,
126.195740996152)) ;
#118470 = CARTESIAN_POINT('Ctrl Pts',(-31.9994986451266,12.9764076821957,
126.273507891197)) ;
#118471 = CARTESIAN_POINT('Ctrl Pts',(-32.0588369991395,12.7508792714819,
126.41360702449)) ;
#118472 = CARTESIAN_POINT('Ctrl Pts',(-32.1350060623825,12.5752390770026,
126.603196268328)) ;
#118473 = CARTESIAN_POINT('Ctrl Pts',(-32.2244641327029,12.4588915032614,
126.831372157513)) ;
#118474 = CARTESIAN_POINT('Ctrl Pts',(-32.3210414704613,12.4118138319928,
127.080368873198)) ;
#118475 = CARTESIAN_POINT('Ctrl Pts',(-32.4187885763319,12.4374481797596,
127.332697812372)) ;
#118476 = CARTESIAN_POINT('Ctrl Pts',(-32.5107712538563,12.5333386342992,
127.568352341056)) ;
#118477 = CARTESIAN_POINT('Ctrl Pts',(-32.5920459321703,12.693967439573,127.772513096516)) ;
#118478 = CARTESIAN_POINT('Ctrl Pts',(-32.6563892906433,12.9050030598073,
127.927533769727)) ;
#118479 = CARTESIAN_POINT('Ctrl Pts',(-32.7011347368276,13.1551457617761,
128.02498837055)) ;
#118480 = CARTESIAN_POINT('Ctrl Pts',(-32.7156355324634,13.3338156180663,
128.045309077602)) ;
#118481 = CARTESIAN_POINT('Ctrl Pts',(-32.7190213287863,13.4231220139207,
128.04417910927)) ;
#118482 = CARTESIAN_POINT('Ctrl Pts',(-11.3761033793275,13.1734341962953,
133.269779676638)) ;
#118483 = CARTESIAN_POINT('Ctrl Pts',(-11.3768069270304,13.1676985193225,
133.271103956166)) ;
#118484 = CARTESIAN_POINT('Ctrl Pts',(-11.3882805706462,13.0762043638356,
133.292938899671)) ;
#118485 = CARTESIAN_POINT('Ctrl Pts',(-11.4192577565396,12.9034783486566,
133.360456115887)) ;
#118486 = CARTESIAN_POINT('Ctrl Pts',(-11.4839335327708,12.6923998158235,
133.516367811255)) ;
#118487 = CARTESIAN_POINT('Ctrl Pts',(-11.5648987051196,12.5327609203509,
133.719781427978)) ;
#118488 = CARTESIAN_POINT('Ctrl Pts',(-11.6575564098631,12.4368205750072,
133.957184373076)) ;
#118489 = CARTESIAN_POINT('Ctrl Pts',(-11.7544962887077,12.4119420230158,
134.20744088849)) ;
#118490 = CARTESIAN_POINT('Ctrl Pts',(-11.8513224104514,12.4592681400663,
134.457068268069)) ;
#118491 = CARTESIAN_POINT('Ctrl Pts',(-11.9405993691722,12.5756590132109,
134.684776660205)) ;
#118492 = CARTESIAN_POINT('Ctrl Pts',(-12.0171777025799,12.7528353886377,
134.875337560121)) ;
#118493 = CARTESIAN_POINT('Ctrl Pts',(-12.0761069391572,12.9779971268721,
135.014361241539)) ;
#118494 = CARTESIAN_POINT('Ctrl Pts',(-12.1139269193626,13.2349353999384,
135.091728750585)) ;
#118495 = CARTESIAN_POINT('Ctrl Pts',(-12.12874362671,13.505181868833,135.101921543684)) ;
#118496 = CARTESIAN_POINT('Ctrl Pts',(-12.1200205283876,13.7710456278858,
135.043149515145)) ;
#118497 = CARTESIAN_POINT('Ctrl Pts',(-12.0894301826285,14.0095405856191,
134.920825784876)) ;
#118498 = CARTESIAN_POINT('Ctrl Pts',(-12.0396580216246,14.2073760437107,
134.742299653733)) ;
#118499 = CARTESIAN_POINT('Ctrl Pts',(-11.9750364644313,14.348956944597,134.520409199205)) ;
#118500 = CARTESIAN_POINT('Ctrl Pts',(-11.9007138169304,14.4243647503837,
134.270081866618)) ;
#118501 = CARTESIAN_POINT('Ctrl Pts',(-11.8231526682833,14.4276726038888,
134.010386566698)) ;
#118502 = CARTESIAN_POINT('Ctrl Pts',(-11.7485533763177,14.359284576391,133.759393230076)) ;
#118503 = CARTESIAN_POINT('Ctrl Pts',(-11.6827807941158,14.2239082664501,
133.534151570949)) ;
#118504 = CARTESIAN_POINT('Ctrl Pts',(-11.6312619715626,14.0309431435162,
133.350500937974)) ;
#118505 = CARTESIAN_POINT('Ctrl Pts',(-11.5985513826321,13.7937232390813,
133.221720651928)) ;
#118506 = CARTESIAN_POINT('Ctrl Pts',(-11.5878056858426,13.531836984712,133.157350898192)) ;
#118507 = CARTESIAN_POINT('Ctrl Pts',(-11.6002475109844,13.2609088557136,
133.160554632561)) ;
#118508 = CARTESIAN_POINT('Ctrl Pts',(-11.6360718512436,13.0011531405438,
133.231998502034)) ;
#118509 = CARTESIAN_POINT('Ctrl Pts',(-11.6929137966697,12.7729627395585,
133.365036762185)) ;
#118510 = CARTESIAN_POINT('Ctrl Pts',(-11.7680839767594,12.590180168645,133.551429864453)) ;
#118511 = CARTESIAN_POINT('Ctrl Pts',(-11.856305645623,12.4676467946536,133.776079657559)) ;
#118512 = CARTESIAN_POINT('Ctrl Pts',(-11.9527048680969,12.4133145045735,
134.024458200477)) ;
#118513 = CARTESIAN_POINT('Ctrl Pts',(-12.0500375750377,12.4313808939379,
134.275789392375)) ;
#118514 = CARTESIAN_POINT('Ctrl Pts',(-12.1432845891867,12.5206603265203,
134.514975108993)) ;
#118515 = CARTESIAN_POINT('Ctrl Pts',(-12.2255404050775,12.6744195884329,
134.722175891724)) ;
#118516 = CARTESIAN_POINT('Ctrl Pts',(-12.2921066353845,12.8815893082003,
134.883533839674)) ;
#118517 = CARTESIAN_POINT('Ctrl Pts',(-12.338995449753,13.1290193256912,134.987229585998)) ;
#118518 = CARTESIAN_POINT('Ctrl Pts',(-12.3630777682256,13.3950772370959,
135.024620575974)) ;
#118519 = CARTESIAN_POINT('Ctrl Pts',(-12.3639615444683,13.664342206485,134.994087920737)) ;
#118520 = CARTESIAN_POINT('Ctrl Pts',(-12.3418854317323,13.9170737521182,
134.896381663503)) ;
#118521 = CARTESIAN_POINT('Ctrl Pts',(-12.2993936354334,14.1334228172292,
134.739163893756)) ;
#118522 = CARTESIAN_POINT('Ctrl Pts',(-12.2403027953976,14.2989215646412,
134.533486314865)) ;
#118523 = CARTESIAN_POINT('Ctrl Pts',(-12.1693589392841,14.402143447902,134.293124348418)) ;
#118524 = CARTESIAN_POINT('Ctrl Pts',(-12.0922425132794,14.4351203022994,
134.034641516887)) ;
#118525 = CARTESIAN_POINT('Ctrl Pts',(-12.0157937728051,14.3956460287634,
133.778272781817)) ;
#118526 = CARTESIAN_POINT('Ctrl Pts',(-11.9455441386352,14.2864256341772,
133.539885354215)) ;
#118527 = CARTESIAN_POINT('Ctrl Pts',(-11.8876134651553,14.1149876043022,
133.337479609213)) ;
#118528 = CARTESIAN_POINT('Ctrl Pts',(-11.8469959298402,13.8950778661998,
133.185808345223)) ;
#118529 = CARTESIAN_POINT('Ctrl Pts',(-11.8269465422163,13.6402949079638,
133.094058419286)) ;
#118530 = CARTESIAN_POINT('Ctrl Pts',(-11.8299420004692,13.3700135183461,
133.069649454816)) ;
#118531 = CARTESIAN_POINT('Ctrl Pts',(-11.8563611483356,13.1040820554216,
133.113728953609)) ;
#118532 = CARTESIAN_POINT('Ctrl Pts',(-11.9049819128071,12.8608603578453,
133.222664719387)) ;
#118533 = CARTESIAN_POINT('Ctrl Pts',(-11.9735329306437,12.6570995418072,
133.389655526666)) ;
#118534 = CARTESIAN_POINT('Ctrl Pts',(-12.0567368640633,12.5097125952048,
133.599752815498)) ;
#118535 = CARTESIAN_POINT('Ctrl Pts',(-12.150523561375,12.4266925714705,133.840558741675)) ;
#118536 = CARTESIAN_POINT('Ctrl Pts',(-12.2483173423649,12.4153566152999,
134.093120553544)) ;
#118537 = CARTESIAN_POINT('Ctrl Pts',(-12.3439234591775,12.4761183658278,
134.339297297897)) ;
#118538 = CARTESIAN_POINT('Ctrl Pts',(-12.4312344046572,12.604611036471,134.561252185302)) ;
#118539 = CARTESIAN_POINT('Ctrl Pts',(-12.5048720957458,12.7920329725734,
134.743205846723)) ;
#118540 = CARTESIAN_POINT('Ctrl Pts',(-12.5600519020243,13.0246460204259,
134.871261784406)) ;
#118541 = CARTESIAN_POINT('Ctrl Pts',(-12.5935838556551,13.2849676562724,
134.936178375483)) ;
#118542 = CARTESIAN_POINT('Ctrl Pts',(-12.6040097500515,13.5561839498762,
134.933470648802)) ;
#118543 = CARTESIAN_POINT('Ctrl Pts',(-12.5909871097811,13.8182130447303,
134.862208918049)) ;
#118544 = CARTESIAN_POINT('Ctrl Pts',(-12.5565449767689,14.0504674828932,
134.728585321904)) ;
#118545 = CARTESIAN_POINT('Ctrl Pts',(-12.503409625585,14.2392688566164,134.540126621614)) ;
#118546 = CARTESIAN_POINT('Ctrl Pts',(-12.4364541228854,14.3686949061628,
134.311393774839)) ;
#118547 = CARTESIAN_POINT('Ctrl Pts',(-12.3615656889771,14.4303698699092,
134.059658526159)) ;
#118548 = CARTESIAN_POINT('Ctrl Pts',(-12.2839010334425,14.4203874335836,
133.799592770568)) ;
#118549 = CARTESIAN_POINT('Ctrl Pts',(-12.210160099743,14.3383234077631,133.550939985876)) ;
#118550 = CARTESIAN_POINT('Ctrl Pts',(-12.1467675345913,14.1909246948651,
133.332649057125)) ;
#118551 = CARTESIAN_POINT('Ctrl Pts',(-12.0987599970841,13.9894771952072,
133.159415008421)) ;
#118552 = CARTESIAN_POINT('Ctrl Pts',(-12.0699641262129,13.746808334038,133.042174065414)) ;
#118553 = CARTESIAN_POINT('Ctrl Pts',(-12.0634132082792,13.4802543050363,
132.989840642035)) ;
#118554 = CARTESIAN_POINT('Ctrl Pts',(-12.0805388848431,13.2092850864011,
133.006627337963)) ;
#118555 = CARTESIAN_POINT('Ctrl Pts',(-12.1201612936325,12.9563426654799,
133.089494153688)) ;
#118556 = CARTESIAN_POINT('Ctrl Pts',(-12.1810219658941,12.7340442860679,
133.234040793985)) ;
#118557 = CARTESIAN_POINT('Ctrl Pts',(-12.2591406672729,12.5620254392794,
133.429068728692)) ;
#118558 = CARTESIAN_POINT('Ctrl Pts',(-12.3489444975325,12.4521634534599,
133.65845210476)) ;
#118559 = CARTESIAN_POINT('Ctrl Pts',(-12.4462656769572,12.411069828673,133.909474442869)) ;
#118560 = CARTESIAN_POINT('Ctrl Pts',(-12.5435407529999,12.4431134787165,
134.160514267981)) ;
#118561 = CARTESIAN_POINT('Ctrl Pts',(-12.6346576814472,12.544720782059,134.393675748219)) ;
#118562 = CARTESIAN_POINT('Ctrl Pts',(-12.7144928520191,12.7094608145556,
134.593760742519)) ;
#118563 = CARTESIAN_POINT('Ctrl Pts',(-12.7777519327944,12.9261933483464,
134.745327776743)) ;
#118564 = CARTESIAN_POINT('Ctrl Pts',(-12.8202519877699,13.176771832056,134.836492242179)) ;
#118565 = CARTESIAN_POINT('Ctrl Pts',(-12.8402444603128,13.4474343122789,
134.861590595176)) ;
#118566 = CARTESIAN_POINT('Ctrl Pts',(-12.8365305004501,13.7143157583518,
134.817690205497)) ;
#118567 = CARTESIAN_POINT('Ctrl Pts',(-12.8106142510612,13.9601208974721,
134.708988844887)) ;
#118568 = CARTESIAN_POINT('Ctrl Pts',(-12.7644642354226,14.1691500345588,
134.540915011046)) ;
#118569 = CARTESIAN_POINT('Ctrl Pts',(-12.7028017761949,14.3234012984993,
134.327766826278)) ;
#118570 = CARTESIAN_POINT('Ctrl Pts',(-12.6301549587558,14.4138714488527,
134.082373591679)) ;
#118571 = CARTESIAN_POINT('Ctrl Pts',(-12.5529215600028,14.4332950677581,
133.82368743641)) ;
#118572 = CARTESIAN_POINT('Ctrl Pts',(-12.4766195880281,14.3798376866145,
133.567474761174)) ;
#118573 = CARTESIAN_POINT('Ctrl Pts',(-12.4087004001394,14.2584887466458,
133.336079424252)) ;
#118574 = CARTESIAN_POINT('Ctrl Pts',(-12.3536722242535,14.0772214658074,
133.142205477393)) ;
#118575 = CARTESIAN_POINT('Ctrl Pts',(-12.3164993112394,13.8478580499734,
133.000351309794)) ;
#118576 = CARTESIAN_POINT('Ctrl Pts',(-12.3008731181985,13.5896599466639,
132.921665266495)) ;
#118577 = CARTESIAN_POINT('Ctrl Pts',(-12.3082135346213,13.3195389388511,
132.910059027627)) ;
#118578 = CARTESIAN_POINT('Ctrl Pts',(-12.3390393214159,13.0556170681804,
132.966906320988)) ;
#118579 = CARTESIAN_POINT('Ctrl Pts',(-12.3916342065595,12.818934352168,133.087465135038)) ;
#118580 = CARTESIAN_POINT('Ctrl Pts',(-12.4631451106269,12.6251003449816,
133.263222547425)) ;
#118581 = CARTESIAN_POINT('Ctrl Pts',(-12.548985341136,12.4887479439426,133.48089248249)) ;
#118582 = CARTESIAN_POINT('Ctrl Pts',(-12.6437484005123,12.4190670413713,
133.724650221671)) ;
#118583 = CARTESIAN_POINT('Ctrl Pts',(-12.7419392728048,12.4213699793115,
133.978259231315)) ;
#118584 = CARTESIAN_POINT('Ctrl Pts',(-12.836294926695,12.4953802453317,134.220834452806)) ;
#118585 = CARTESIAN_POINT('Ctrl Pts',(-12.9215231107959,12.6359572118525,
134.436656343271)) ;
#118586 = CARTESIAN_POINT('Ctrl Pts',(-12.9919038366036,12.8329197331058,
134.609132207882)) ;
#118587 = CARTESIAN_POINT('Ctrl Pts',(-13.0431941881955,13.0719649791817,
134.725860231311)) ;
#118588 = CARTESIAN_POINT('Ctrl Pts',(-13.0725075844949,13.3363497207088,
134.77836223128)) ;
#118589 = CARTESIAN_POINT('Ctrl Pts',(-13.0784119937401,13.6070576774105,
134.762468724094)) ;
#118590 = CARTESIAN_POINT('Ctrl Pts',(-13.0612042244902,13.8644611915849,
134.679071115725)) ;
#118591 = CARTESIAN_POINT('Ctrl Pts',(-13.0229223196548,14.0900773002825,
134.534142554414)) ;
#118592 = CARTESIAN_POINT('Ctrl Pts',(-12.9668857918559,14.2682172577694,
134.337289258471)) ;
#118593 = CARTESIAN_POINT('Ctrl Pts',(-12.898149301531,14.385416608164,134.10344537434)) ;
#118594 = CARTESIAN_POINT('Ctrl Pts',(-12.8220030996413,14.4341663222017,
133.847878057457)) ;
#118595 = CARTESIAN_POINT('Ctrl Pts',(-12.7445691235808,14.4102121268538,
133.58846496535)) ;
#118596 = CARTESIAN_POINT('Ctrl Pts',(-12.6725877902746,14.3156229092393,
133.345094836696)) ;
#118597 = CARTESIAN_POINT('Ctrl Pts',(-12.6115971411473,14.157111727064,133.133799779272)) ;
#118598 = CARTESIAN_POINT('Ctrl Pts',(-12.566783250654,13.9459764019392,132.96976134338)) ;
#118599 = CARTESIAN_POINT('Ctrl Pts',(-12.5420765503289,13.6975622305703,
132.864482081499)) ;
#118600 = CARTESIAN_POINT('Ctrl Pts',(-12.53995666575,13.4293975003276,132.825169963598)) ;
#118601 = CARTESIAN_POINT('Ctrl Pts',(-12.5612578432039,13.1610019390536,
132.854307434728)) ;
#118602 = CARTESIAN_POINT('Ctrl Pts',(-12.6053825198436,12.910584846224,132.95000917613)) ;
#118603 = CARTESIAN_POINT('Ctrl Pts',(-12.6696450944826,12.6976134707592,
133.10463582855)) ;
#118604 = CARTESIAN_POINT('Ctrl Pts',(-12.7502997842175,12.536442281865,133.307124586035)) ;
#118605 = CARTESIAN_POINT('Ctrl Pts',(-12.8422220552916,12.4387732267397,
133.542548790537)) ;
#118606 = CARTESIAN_POINT('Ctrl Pts',(-12.9398571626702,12.4116342438423,
133.794574286652)) ;
#118607 = CARTESIAN_POINT('Ctrl Pts',(-13.0363065622486,12.4569142421678,
134.04327039679)) ;
#118608 = CARTESIAN_POINT('Ctrl Pts',(-13.1260272439089,12.5714751922183,
134.272219310858)) ;
#118609 = CARTESIAN_POINT('Ctrl Pts',(-13.2029202315668,12.7468633179545,
134.463749827211)) ;
#118610 = CARTESIAN_POINT('Ctrl Pts',(-13.2624243662056,12.9706872906827,
134.604464814153)) ;
#118611 = CARTESIAN_POINT('Ctrl Pts',(-13.3009328039148,13.2271705417113,
134.683814778475)) ;
#118612 = CARTESIAN_POINT('Ctrl Pts',(-13.3164246163393,13.4971329945125,
134.69600029026)) ;
#118613 = CARTESIAN_POINT('Ctrl Pts',(-13.3083964010065,13.7633005745665,
134.639275314715)) ;
#118614 = CARTESIAN_POINT('Ctrl Pts',(-13.2784711170363,14.0028268383939,
134.518902238097)) ;
#118615 = CARTESIAN_POINT('Ctrl Pts',(-13.2289588566988,14.2028677697453,
134.340991546535)) ;
#118616 = CARTESIAN_POINT('Ctrl Pts',(-13.1649219288007,14.3455611528234,
134.120940152505)) ;
#118617 = CARTESIAN_POINT('Ctrl Pts',(-13.0908084734639,14.4231516441217,
133.871220084537)) ;
#118618 = CARTESIAN_POINT('Ctrl Pts',(-13.0132392773694,14.428665737009,133.611497374306)) ;
#118619 = CARTESIAN_POINT('Ctrl Pts',(-12.9383171503362,14.3621069846461,
133.3594868622)) ;
#118620 = CARTESIAN_POINT('Ctrl Pts',(-12.872270725288,14.2287343396627,133.133488008975)) ;
#118621 = CARTESIAN_POINT('Ctrl Pts',(-12.8201528022822,14.0363061322534,
132.947956133022)) ;
#118622 = CARTESIAN_POINT('Ctrl Pts',(-12.7871145635481,13.8023697285695,
132.818530704553)) ;
#118623 = CARTESIAN_POINT('Ctrl Pts',(-12.7755307033747,13.5388532599518,
132.751430578147)) ;
#118624 = CARTESIAN_POINT('Ctrl Pts',(-12.7874147952686,13.2684518599204,
132.753076122246)) ;
#118625 = CARTESIAN_POINT('Ctrl Pts',(-12.8223738829444,13.0087997166185,
132.822096605802)) ;
#118626 = CARTESIAN_POINT('Ctrl Pts',(-12.8791405427355,12.7778890822412,
132.954659158962)) ;
#118627 = CARTESIAN_POINT('Ctrl Pts',(-12.9533257274006,12.5950173960976,
133.138428418753)) ;
#118628 = CARTESIAN_POINT('Ctrl Pts',(-13.0416625952284,12.4700325121189,
133.363244570128)) ;
#118629 = CARTESIAN_POINT('Ctrl Pts',(-13.1373825064978,12.4138573722268,
133.609834541986)) ;
#118630 = CARTESIAN_POINT('Ctrl Pts',(-13.2356240525979,12.4301864266095,
133.863515438704)) ;
#118631 = CARTESIAN_POINT('Ctrl Pts',(-13.3280894934625,12.5166844150512,
134.100777833648)) ;
#118632 = CARTESIAN_POINT('Ctrl Pts',(-13.4112528177748,12.6693064963876,
134.310434251688)) ;
#118633 = CARTESIAN_POINT('Ctrl Pts',(-13.4780909825541,12.8745471287187,
134.472698922864)) ;
#118634 = CARTESIAN_POINT('Ctrl Pts',(-13.5257121495714,13.1212023718215,
134.578500578674)) ;
#118635 = CARTESIAN_POINT('Ctrl Pts',(-13.5504942774336,13.3871939110425,
134.617905019548)) ;
#118636 = CARTESIAN_POINT('Ctrl Pts',(-13.5520362091492,13.6567281745513,
134.58928459527)) ;
#118637 = CARTESIAN_POINT('Ctrl Pts',(-13.5306752870686,13.9097854264049,
134.493733920305)) ;
#118638 = CARTESIAN_POINT('Ctrl Pts',(-13.4886113688084,14.1280196368697,
134.337667087445)) ;
#118639 = CARTESIAN_POINT('Ctrl Pts',(-13.4300006465922,14.2950456004005,
134.133430228144)) ;
#118640 = CARTESIAN_POINT('Ctrl Pts',(-13.3588662565052,14.4005267631623,
133.89231315706)) ;
#118641 = CARTESIAN_POINT('Ctrl Pts',(-13.2823506329123,14.4350836721885,
133.635816652807)) ;
#118642 = CARTESIAN_POINT('Ctrl Pts',(-13.205705858747,14.397803897227,133.378829605741)) ;
#118643 = CARTESIAN_POINT('Ctrl Pts',(-13.1352707452639,14.2905756800978,
133.139940320595)) ;
#118644 = CARTESIAN_POINT('Ctrl Pts',(-13.0769038461577,14.1209511451637,
132.936271017707)) ;
#118645 = CARTESIAN_POINT('Ctrl Pts',(-13.0356468946471,13.9018371823522,
132.78266797249)) ;
#118646 = CARTESIAN_POINT('Ctrl Pts',(-13.0150200866047,13.6479071387663,
132.689251355067)) ;
#118647 = CARTESIAN_POINT('Ctrl Pts',(-13.0172505947305,13.378501800303,132.662693599669)) ;
#118648 = CARTESIAN_POINT('Ctrl Pts',(-13.0431950965829,13.1105161208594,
132.705174926483)) ;
#118649 = CARTESIAN_POINT('Ctrl Pts',(-13.0910470050457,12.8677236673919,
132.812031740223)) ;
#118650 = CARTESIAN_POINT('Ctrl Pts',(-13.1588500660242,12.662830762423,132.976909729655)) ;
#118651 = CARTESIAN_POINT('Ctrl Pts',(-13.241879425623,12.513091865374,133.186406240102)) ;
#118652 = CARTESIAN_POINT('Ctrl Pts',(-13.335714202403,12.4280189029097,133.427266782244)) ;
#118653 = CARTESIAN_POINT('Ctrl Pts',(-13.4331919707127,12.4146728655739,
133.679002405755)) ;
#118654 = CARTESIAN_POINT('Ctrl Pts',(-13.529167232764,12.473418288016,133.9261846977)) ;
#118655 = CARTESIAN_POINT('Ctrl Pts',(-13.616885586122,12.6005220564223,134.149279369247)) ;
#118656 = CARTESIAN_POINT('Ctrl Pts',(-13.6906060457598,12.7855011637684,
134.331642511686)) ;
#118657 = CARTESIAN_POINT('Ctrl Pts',(-13.7464767458507,13.0169860566136,
134.461699644794)) ;
#118658 = CARTESIAN_POINT('Ctrl Pts',(-13.7807535613475,13.2774553414867,
134.52870436425)) ;
#118659 = CARTESIAN_POINT('Ctrl Pts',(-13.7917957698787,13.5483711409958,
134.527829507085)) ;
#118660 = CARTESIAN_POINT('Ctrl Pts',(-13.7795542716983,13.8100859907312,
134.458968320121)) ;
#118661 = CARTESIAN_POINT('Ctrl Pts',(-13.7455979084497,14.0443620014337,
134.326633872772)) ;
#118662 = CARTESIAN_POINT('Ctrl Pts',(-13.6931373802941,14.2339606584883,
134.140272341113)) ;
#118663 = CARTESIAN_POINT('Ctrl Pts',(-13.6265708969899,14.3656339537851,
133.912671017341)) ;
#118664 = CARTESIAN_POINT('Ctrl Pts',(-13.5514661250035,14.4296685423803,
133.660141235671)) ;
#118665 = CARTESIAN_POINT('Ctrl Pts',(-13.4739953762964,14.4216217772437,
133.400732222126)) ;
#118666 = CARTESIAN_POINT('Ctrl Pts',(-13.4003044829647,14.3422174229119,
133.152352720469)) ;
#118667 = CARTESIAN_POINT('Ctrl Pts',(-13.3362641407276,14.1963612940614,
132.932055167752)) ;
#118668 = CARTESIAN_POINT('Ctrl Pts',(-13.2876475135786,13.9958156297376,
132.756967432803)) ;
#118669 = CARTESIAN_POINT('Ctrl Pts',(-13.2582843417661,13.7540871657713,
132.638075405849)) ;
#118670 = CARTESIAN_POINT('Ctrl Pts',(-13.2510678261576,13.4887318093835,
132.583893441065)) ;
#118671 = CARTESIAN_POINT('Ctrl Pts',(-13.2674127122864,13.2176490073036,
132.5984066129)) ;
#118672 = CARTESIAN_POINT('Ctrl Pts',(-13.3065305530606,12.9629384302475,
132.679668636195)) ;
#118673 = CARTESIAN_POINT('Ctrl Pts',(-13.366974380418,12.739445641898,132.822966776447)) ;
#118674 = CARTESIAN_POINT('Ctrl Pts',(-13.4441917545612,12.5666312573546,
133.015548468246)) ;
#118675 = CARTESIAN_POINT('Ctrl Pts',(-13.5342140472049,12.4542159373709,
133.245381617091)) ;
#118676 = CARTESIAN_POINT('Ctrl Pts',(-13.6308745371879,12.4113528375642,
133.494668076726)) ;
#118677 = CARTESIAN_POINT('Ctrl Pts',(-13.7284554191117,12.4409689765868,
133.746525962875)) ;
#118678 = CARTESIAN_POINT('Ctrl Pts',(-13.8202195933766,12.5412370849313,
133.981433403131)) ;
#118679 = CARTESIAN_POINT('Ctrl Pts',(-13.9001905656391,12.7041353047709,
134.181997916387)) ;
#118680 = CARTESIAN_POINT('Ctrl Pts',(-13.9637943476695,12.9183855347654,
134.334727271198)) ;
#118681 = CARTESIAN_POINT('Ctrl Pts',(-14.0071906666907,13.1698655571926,
134.428284860126)) ;
#118682 = CARTESIAN_POINT('Ctrl Pts',(-14.0277193594189,13.4380609714907,
134.455227938298)) ;
#118683 = CARTESIAN_POINT('Ctrl Pts',(-14.0247819555589,13.7071666281258,
134.413364904376)) ;
#118684 = CARTESIAN_POINT('Ctrl Pts',(-13.9993507533856,13.95380880599,134.306063795002)) ;
#118685 = CARTESIAN_POINT('Ctrl Pts',(-13.9539517208912,14.1634527040787,
134.14031710819)) ;
#118686 = CARTESIAN_POINT('Ctrl Pts',(-13.8923677928476,14.3201289862677,
133.927232128965)) ;
#118687 = CARTESIAN_POINT('Ctrl Pts',(-13.8202667339251,14.4121340944115,
133.683587595144)) ;
#118688 = CARTESIAN_POINT('Ctrl Pts',(-13.742809080042,14.4336855937072,133.424119840857)) ;
#118689 = CARTESIAN_POINT('Ctrl Pts',(-13.6668608280909,14.3827385924792,
133.169159916255)) ;
#118690 = CARTESIAN_POINT('Ctrl Pts',(-13.5981295475996,14.2627494461532,
132.935168649536)) ;
#118691 = CARTESIAN_POINT('Ctrl Pts',(-13.5426656002654,14.0822576993362,
132.739956868766)) ;
#118692 = CARTESIAN_POINT('Ctrl Pts',(-13.5052230771177,13.856193146146,132.597618261521)) ;
#118693 = CARTESIAN_POINT('Ctrl Pts',(-13.4887623843814,13.5974242111817,
132.516323439236)) ;
#118694 = CARTESIAN_POINT('Ctrl Pts',(-13.4954472616452,13.3273251704849,
132.502803308112)) ;
#118695 = CARTESIAN_POINT('Ctrl Pts',(-13.5257309046639,13.062291125414,132.55797992157)) ;
#118696 = CARTESIAN_POINT('Ctrl Pts',(-13.5775428431027,12.8256130125541,
132.676388959343)) ;
#118697 = CARTESIAN_POINT('Ctrl Pts',(-13.6485285477905,12.6301798373562,
132.850606152527)) ;
#118698 = CARTESIAN_POINT('Ctrl Pts',(-13.7340252244735,12.4918476261695,
133.067265702632)) ;
#118699 = CARTESIAN_POINT('Ctrl Pts',(-13.8290183989182,12.4199209769537,
133.311555769525)) ;
#118700 = CARTESIAN_POINT('Ctrl Pts',(-13.9270636548616,12.4204246059211,
133.564789863863)) ;
#118701 = CARTESIAN_POINT('Ctrl Pts',(-14.0213478504549,12.492159634428,133.807246350047)) ;
#118702 = CARTESIAN_POINT('Ctrl Pts',(-14.1070156184682,12.6310173484571,
134.024319850583)) ;
#118703 = CARTESIAN_POINT('Ctrl Pts',(-14.1778290426334,12.8262647723397,
134.198098948728)) ;
#118704 = CARTESIAN_POINT('Ctrl Pts',(-14.2297952112719,13.0646914718589,
134.316746137298)) ;
#118705 = CARTESIAN_POINT('Ctrl Pts',(-14.259734937754,13.3278245014775,134.371176497314)) ;
#118706 = CARTESIAN_POINT('Ctrl Pts',(-14.2663521460769,13.5998586000628,
134.357209920682)) ;
#118707 = CARTESIAN_POINT('Ctrl Pts',(-14.2498316891277,13.8569827516154,
134.275942445626)) ;
#118708 = CARTESIAN_POINT('Ctrl Pts',(-14.2120572185788,14.0842219381739,
134.132424698552)) ;
#118709 = CARTESIAN_POINT('Ctrl Pts',(-14.1566892395711,14.2634336188574,
133.937641912658)) ;
#118710 = CARTESIAN_POINT('Ctrl Pts',(-14.0878220989839,14.3833954818559,
133.703202208994)) ;
#118711 = CARTESIAN_POINT('Ctrl Pts',(-14.0117161826671,14.433698045123,133.447730780154)) ;
#118712 = CARTESIAN_POINT('Ctrl Pts',(-13.9347372020107,14.412015772317,133.189865782114)) ;
#118713 = CARTESIAN_POINT('Ctrl Pts',(-13.8622959354617,14.319294669833,132.945054536655)) ;
#118714 = CARTESIAN_POINT('Ctrl Pts',(-13.8009553728816,14.16255830471,132.732761956331)) ;
#118715 = CARTESIAN_POINT('Ctrl Pts',(-13.7554963594563,13.9521768757504,
132.566750983519)) ;
#118716 = CARTESIAN_POINT('Ctrl Pts',(-13.7302700360325,13.7045477413862,
132.459961598635)) ;
#118717 = CARTESIAN_POINT('Ctrl Pts',(-13.7274455850892,13.4377490344594,
132.41872307)) ;
#118718 = CARTESIAN_POINT('Ctrl Pts',(-13.7481931708221,13.1678476271901,
132.446083972868)) ;
#118719 = CARTESIAN_POINT('Ctrl Pts',(-13.7915277802669,12.917659013908,132.539618023673)) ;
#118720 = CARTESIAN_POINT('Ctrl Pts',(-13.855533519147,12.7025601696351,132.693352244411)) ;
#118721 = CARTESIAN_POINT('Ctrl Pts',(-13.9353887493187,12.5405894739967,
132.893677963618)) ;
#118722 = CARTESIAN_POINT('Ctrl Pts',(-14.027297883474,12.4405287595892,133.128967601787)) ;
#118723 = CARTESIAN_POINT('Ctrl Pts',(-14.124837017402,12.4114132283242,133.380726658666)) ;
#118724 = CARTESIAN_POINT('Ctrl Pts',(-14.2213484874047,12.4546443819082,
133.629616296311)) ;
#118725 = CARTESIAN_POINT('Ctrl Pts',(-14.3111929481664,12.5668919742526,
133.858998159138)) ;
#118726 = CARTESIAN_POINT('Ctrl Pts',(-14.3889051145816,12.7415276223377,
134.052758598693)) ;
#118727 = CARTESIAN_POINT('Ctrl Pts',(-14.4487819994688,12.963899300171,134.194625958176)) ;
#118728 = CARTESIAN_POINT('Ctrl Pts',(-14.4878921741366,13.2191082670462,
134.275803667982)) ;
#118729 = CARTESIAN_POINT('Ctrl Pts',(-14.5040836850349,13.4893534858843,
134.289979202675)) ;
#118730 = CARTESIAN_POINT('Ctrl Pts',(-14.4967928296328,13.7553188833262,
134.235494967527)) ;
#118731 = CARTESIAN_POINT('Ctrl Pts',(-14.4672977855729,13.9971251681561,
134.116192347562)) ;
#118732 = CARTESIAN_POINT('Ctrl Pts',(-14.4183840345143,14.1977811573069,
133.940137499588)) ;
#118733 = CARTESIAN_POINT('Ctrl Pts',(-14.3547061912952,14.3424510805747,
133.721119079194)) ;
#118734 = CARTESIAN_POINT('Ctrl Pts',(-14.2805016481878,14.4220642873528,
133.471015964754)) ;
#118735 = CARTESIAN_POINT('Ctrl Pts',(-14.2033365143345,14.429449097017,133.212639286996)) ;
#118736 = CARTESIAN_POINT('Ctrl Pts',(-14.1282860163884,14.3652072331767,
132.960276109633)) ;
#118737 = CARTESIAN_POINT('Ctrl Pts',(-14.0618281815478,14.2335291681656,
132.73303684308)) ;
#118738 = CARTESIAN_POINT('Ctrl Pts',(-14.0092524260735,14.0429179829767,
132.546208320143)) ;
#118739 = CARTESIAN_POINT('Ctrl Pts',(-13.9755602690746,13.8093220415122,
132.414774751923)) ;
#118740 = CARTESIAN_POINT('Ctrl Pts',(-13.9633085026902,13.5476217971459,
132.345885885849)) ;
#118741 = CARTESIAN_POINT('Ctrl Pts',(-13.9746025661185,13.2750711815888,
132.345545153662)) ;
#118742 = CARTESIAN_POINT('Ctrl Pts',(-14.0088332469759,13.0163164213971,
132.412617107112)) ;
#118743 = CARTESIAN_POINT('Ctrl Pts',(-14.064784241679,12.7846451556795,132.542871054114)) ;
#118744 = CARTESIAN_POINT('Ctrl Pts',(-14.1387306401708,12.5995256384001,
132.725831674418)) ;
#118745 = CARTESIAN_POINT('Ctrl Pts',(-14.2267816071698,12.4726551517152,
132.949805912223)) ;
#118746 = CARTESIAN_POINT('Ctrl Pts',(-14.3224320561303,12.4145513421249,
133.19616672507)) ;
#118747 = CARTESIAN_POINT('Ctrl Pts',(-14.4201984857976,12.4284690605263,
133.448637711958)) ;
#118748 = CARTESIAN_POINT('Ctrl Pts',(-14.5134883154838,12.5133431684666,
133.688097238147)) ;
#118749 = CARTESIAN_POINT('Ctrl Pts',(-14.5969649871232,12.6644367182662,
133.898678980795)) ;
#118750 = CARTESIAN_POINT('Ctrl Pts',(-14.6641763539161,12.8679925564765,
134.062089198708)) ;
#118751 = CARTESIAN_POINT('Ctrl Pts',(-14.7123711551398,13.1131690365504,
134.169635545851)) ;
#118752 = CARTESIAN_POINT('Ctrl Pts',(-14.7379481518439,13.3800002802051,
134.211213153089)) ;
#118753 = CARTESIAN_POINT('Ctrl Pts',(-14.7400542154875,13.6495651704166,
134.18425698349)) ;
#118754 = CARTESIAN_POINT('Ctrl Pts',(-14.7194527468048,13.9023388943094,
134.091064092335)) ;
#118755 = CARTESIAN_POINT('Ctrl Pts',(-14.6778190034174,14.1226577783971,
133.936136558405)) ;
#118756 = CARTESIAN_POINT('Ctrl Pts',(-14.6196935304185,14.2908247544057,
133.733378266289)) ;
#118757 = CARTESIAN_POINT('Ctrl Pts',(-14.5492150216665,14.3981040604,133.494335232995)) ;
#118758 = CARTESIAN_POINT('Ctrl Pts',(-14.4722411376038,14.4352626925802,
133.236261337413)) ;
#118759 = CARTESIAN_POINT('Ctrl Pts',(-14.3954256541312,14.3995540245642,
132.978732791801)) ;
#118760 = CARTESIAN_POINT('Ctrl Pts',(-14.3250767517661,14.2948938638273,
132.740267779799)) ;
#118761 = CARTESIAN_POINT('Ctrl Pts',(-14.2659553830164,14.125950965529,132.534203861649)) ;
#118762 = CARTESIAN_POINT('Ctrl Pts',(-14.2243526466944,13.9085226432365,
132.379690324383)) ;
#118763 = CARTESIAN_POINT('Ctrl Pts',(-14.2030975765256,13.655740461518,132.284483495896)) ;
#118764 = CARTESIAN_POINT('Ctrl Pts',(-14.2046245934485,13.3866405451627,
132.255884182945)) ;
#118765 = CARTESIAN_POINT('Ctrl Pts',(-14.2298902227146,13.1181024213027,
132.296361021273)) ;
#118766 = CARTESIAN_POINT('Ctrl Pts',(-14.2771378969919,12.8743682814219,
132.401446588546)) ;
#118767 = CARTESIAN_POINT('Ctrl Pts',(-14.3444307231662,12.6679957327003,
132.564825469235)) ;
#118768 = CARTESIAN_POINT('Ctrl Pts',(-14.4272321374204,12.5164144034558,
132.773604557212)) ;
#118769 = CARTESIAN_POINT('Ctrl Pts',(-14.5205022334955,12.4295970264179,
133.012939067384)) ;
#118770 = CARTESIAN_POINT('Ctrl Pts',(-14.6182514403091,12.4140261333183,
133.265360142286)) ;
#118771 = CARTESIAN_POINT('Ctrl Pts',(-14.7142174515708,12.4707103278581,
133.512570298941)) ;
#118772 = CARTESIAN_POINT('Ctrl Pts',(-14.8022488129207,12.5959068144279,
133.736577659016)) ;
#118773 = CARTESIAN_POINT('Ctrl Pts',(-14.876456590018,12.7791142632462,133.920383734278)) ;
#118774 = CARTESIAN_POINT('Ctrl Pts',(-14.9332273811375,13.0114293123004,
134.052815872987)) ;
#118775 = CARTESIAN_POINT('Ctrl Pts',(-14.9677728031387,13.2689899400059,
134.120913863117)) ;
#118776 = CARTESIAN_POINT('Ctrl Pts',(-14.9796228556439,13.5409257328685,
134.122263271617)) ;
#118777 = CARTESIAN_POINT('Ctrl Pts',(-14.9679885894929,13.8029840857302,
134.055199600153)) ;
#118778 = CARTESIAN_POINT('Ctrl Pts',(-14.9345699006002,14.0385608749257,
133.924394571764)) ;
#118779 = CARTESIAN_POINT('Ctrl Pts',(-14.8825727950335,14.2294231057281,
133.739404880922)) ;
#118780 = CARTESIAN_POINT('Ctrl Pts',(-14.816446608533,14.3627051490732,133.513143288359)) ;
#118781 = CARTESIAN_POINT('Ctrl Pts',(-14.741468869848,14.428833416405,133.260966751182)) ;
#118782 = CARTESIAN_POINT('Ctrl Pts',(-14.6639502642104,14.4228924472986,
133.001406958395)) ;
#118783 = CARTESIAN_POINT('Ctrl Pts',(-14.5898577797733,14.3451234315922,
132.75175728098)) ;
#118784 = CARTESIAN_POINT('Ctrl Pts',(-14.5255775888799,14.2008972781255,
132.530791080979)) ;
#118785 = CARTESIAN_POINT('Ctrl Pts',(-14.4766080099444,14.0023960154245,
132.354775246245)) ;
#118786 = CARTESIAN_POINT('Ctrl Pts',(-14.4465779509174,13.761031796391,132.233855249639)) ;
#118787 = CARTESIAN_POINT('Ctrl Pts',(-14.4387588071979,13.4967569826491,
132.177998148648)) ;
#118788 = CARTESIAN_POINT('Ctrl Pts',(-14.4543340091487,13.2257685669237,
132.19029344318)) ;
#118789 = CARTESIAN_POINT('Ctrl Pts',(-14.4929582457325,12.9695426329055,
132.270003328001)) ;
#118790 = CARTESIAN_POINT('Ctrl Pts',(-14.5526587987454,12.7456271817385,
132.411240190467)) ;
#118791 = CARTESIAN_POINT('Ctrl Pts',(-14.6294318722115,12.5709695365104,
132.602507669175)) ;
#118792 = CARTESIAN_POINT('Ctrl Pts',(-14.7192820441727,12.4565179124428,
132.831796466456)) ;
#118793 = CARTESIAN_POINT('Ctrl Pts',(-14.8158579152677,12.411477377022,133.080829972233)) ;
#118794 = CARTESIAN_POINT('Ctrl Pts',(-14.9138628191828,12.4394645473503,
133.333796557217)) ;
#118795 = CARTESIAN_POINT('Ctrl Pts',(-15.0051613513395,12.5368907011572,
133.567613056464)) ;
#118796 = CARTESIAN_POINT('Ctrl Pts',(-15.0862176428517,12.6994727139768,
133.771061042229)) ;
#118797 = CARTESIAN_POINT('Ctrl Pts',(-15.1499237960889,12.9112843857967,
133.924296026103)) ;
#118798 = CARTESIAN_POINT('Ctrl Pts',(-15.1942053675931,13.1634090116609,
134.020242245567)) ;
#118799 = CARTESIAN_POINT('Ctrl Pts',(-15.2151706961316,13.4300956070728,
134.048622364032)) ;
#118800 = CARTESIAN_POINT('Ctrl Pts',(-15.2130719138631,13.698548706025,134.009335703669)) ;
#118801 = CARTESIAN_POINT('Ctrl Pts',(-15.1880474111806,13.948024671753,133.902954348406)) ;
#118802 = CARTESIAN_POINT('Ctrl Pts',(-15.1433584082714,14.1576527891806,
133.739468144445)) ;
#118803 = CARTESIAN_POINT('Ctrl Pts',(-15.0822635591605,14.3162850237807,
133.527820467193)) ;
#118804 = CARTESIAN_POINT('Ctrl Pts',(-15.0100411334749,14.4106899925297,
133.283664989385)) ;
#118805 = CARTESIAN_POINT('Ctrl Pts',(-14.9326148210013,14.4339585114454,
133.024280536039)) ;
#118806 = CARTESIAN_POINT('Ctrl Pts',(-14.8568708594425,14.3853107611265,
132.770062353486)) ;
#118807 = CARTESIAN_POINT('Ctrl Pts',(-14.7876649938724,14.2669554182004,
132.53459909594)) ;
#118808 = CARTESIAN_POINT('Ctrl Pts',(-14.7318719578663,14.0883945818005,
132.338499578768)) ;
#118809 = CARTESIAN_POINT('Ctrl Pts',(-14.6938089527837,13.8631867563802,
132.194300139215)) ;
#118810 = CARTESIAN_POINT('Ctrl Pts',(-14.6767096598151,13.6057120624757,
132.111223574541)) ;
#118811 = CARTESIAN_POINT('Ctrl Pts',(-14.6827242929546,13.3350528446723,
132.09566169205)) ;
#118812 = CARTESIAN_POINT('Ctrl Pts',(-14.7121680274684,13.0707553542234,
132.148540753936)) ;
#118813 = CARTESIAN_POINT('Ctrl Pts',(-14.7634230355336,12.8321486706852,
132.265220829999)) ;
#118814 = CARTESIAN_POINT('Ctrl Pts',(-14.8343243445453,12.634462986152,132.439029242949)) ;
#118815 = CARTESIAN_POINT('Ctrl Pts',(-14.9190987032166,12.4951761871636,
132.653736170643)) ;
#118816 = CARTESIAN_POINT('Ctrl Pts',(-15.0137030553733,12.4210996152358,
132.896951658987)) ;
#118817 = CARTESIAN_POINT('Ctrl Pts',(-15.1118584374447,12.4192964203799,
133.150469827584)) ;
#118818 = CARTESIAN_POINT('Ctrl Pts',(-15.2065423898953,12.4890492296412,
133.394023625246)) ;
#118819 = CARTESIAN_POINT('Ctrl Pts',(-15.2928092091889,12.6268326997912,
133.612729453774)) ;
#118820 = CARTESIAN_POINT('Ctrl Pts',(-15.36366888592,12.8195830933143,133.786835531785)) ;
#118821 = CARTESIAN_POINT('Ctrl Pts',(-15.4163669219874,13.0571002340723,
133.90758683916)) ;
#118822 = CARTESIAN_POINT('Ctrl Pts',(-15.4469778815777,13.3202805814274,
133.963914687961)) ;
#118823 = CARTESIAN_POINT('Ctrl Pts',(-15.4543026229993,13.5914916661993,
133.95212933086)) ;
#118824 = CARTESIAN_POINT('Ctrl Pts',(-15.4383344177632,13.850556640903,133.87230135427)) ;
#118825 = CARTESIAN_POINT('Ctrl Pts',(-15.4012847002577,14.0777829295082,
133.731064838827)) ;
#118826 = CARTESIAN_POINT('Ctrl Pts',(-15.3462911182543,14.2590886329476,
133.53730079744)) ;
#118827 = CARTESIAN_POINT('Ctrl Pts',(-15.2777940762264,14.3807166913486,
133.303980899783)) ;
#118828 = CARTESIAN_POINT('Ctrl Pts',(-15.2018903534353,14.433343612586,133.049127000921)) ;
#118829 = CARTESIAN_POINT('Ctrl Pts',(-15.1243517133712,14.4133893592863,
132.789404894538)) ;
#118830 = CARTESIAN_POINT('Ctrl Pts',(-15.0521554583449,14.3229978195751,
132.545518463658)) ;
#118831 = CARTESIAN_POINT('Ctrl Pts',(-14.9903443446377,14.1680350137977,
132.331824025693)) ;
#118832 = CARTESIAN_POINT('Ctrl Pts',(-14.9444490968226,13.9594347962821,
132.164606047946)) ;
#118833 = CARTESIAN_POINT('Ctrl Pts',(-14.9184638689497,13.7128291828127,
132.055602750817)) ;
#118834 = CARTESIAN_POINT('Ctrl Pts',(-14.9150513396177,13.4442543360426,
132.012387191979)) ;
#118835 = CARTESIAN_POINT('Ctrl Pts',(-14.934907349885,13.1766944104108,132.037471123533)) ;
#118836 = CARTESIAN_POINT('Ctrl Pts',(-14.9779705778938,12.9234094695572,
132.129904425091)) ;
#118837 = CARTESIAN_POINT('Ctrl Pts',(-15.0410826203302,12.7086523153548,
132.281257042121)) ;
#118838 = CARTESIAN_POINT('Ctrl Pts',(-15.12058795907,12.5444332786266,132.480500688696)) ;
#118839 = CARTESIAN_POINT('Ctrl Pts',(-15.2126050466934,12.4422654276919,
132.715988199535)) ;
#118840 = CARTESIAN_POINT('Ctrl Pts',(-15.3096570151281,12.4113238218205,
132.966463261144)) ;
#118841 = CARTESIAN_POINT('Ctrl Pts',(-15.4063598506817,12.4521999821779,
133.215890712785)) ;
#118842 = CARTESIAN_POINT('Ctrl Pts',(-15.4969844701974,12.5635389919688,
133.447348690198)) ;
#118843 = CARTESIAN_POINT('Ctrl Pts',(-15.5745083193793,12.7354102649258,
133.64080974434)) ;
#118844 = CARTESIAN_POINT('Ctrl Pts',(-15.6351282259747,12.9568498172893,
133.784780387148)) ;
#118845 = CARTESIAN_POINT('Ctrl Pts',(-15.674914220919,13.2117694586679,133.867887052705)) ;
#118846 = CARTESIAN_POINT('Ctrl Pts',(-15.6917614023731,13.4825284922973,
133.883897484168)) ;
#118847 = CARTESIAN_POINT('Ctrl Pts',(-15.6850400020228,13.7484828909248,
133.83112168251)) ;
#118848 = CARTESIAN_POINT('Ctrl Pts',(-15.6562837813056,13.9900671084782,
133.714129468702)) ;
#118849 = CARTESIAN_POINT('Ctrl Pts',(-15.6080310880803,14.1922209027102,
133.540043875935)) ;
#118850 = CARTESIAN_POINT('Ctrl Pts',(-15.5443158917429,14.3393855403521,
133.320716383079)) ;
#118851 = CARTESIAN_POINT('Ctrl Pts',(-15.4709624560433,14.4204077329138,
133.07339142867)) ;
#118852 = CARTESIAN_POINT('Ctrl Pts',(-15.3934209892206,14.4304302154213,
132.813738162468)) ;
#118853 = CARTESIAN_POINT('Ctrl Pts',(-15.3179864333146,14.367871152587,132.56015597024)) ;
#118854 = CARTESIAN_POINT('Ctrl Pts',(-15.2511809644484,14.2376927603017,
132.331870254085)) ;
#118855 = CARTESIAN_POINT('Ctrl Pts',(-15.1983120540608,14.0489883287211,
132.144273980636)) ;
#118856 = CARTESIAN_POINT('Ctrl Pts',(-15.1639748285967,13.8164456424353,
132.0109487585)) ;
#118857 = CARTESIAN_POINT('Ctrl Pts',(-15.1511681352343,13.5541089152985,
131.940298370315)) ;
#118858 = CARTESIAN_POINT('Ctrl Pts',(-15.1615961610843,13.2846772722545,
131.937816936968)) ;
#118859 = CARTESIAN_POINT('Ctrl Pts',(-15.1953535583714,13.0230235410346,
132.003215202363)) ;
#118860 = CARTESIAN_POINT('Ctrl Pts',(-15.2506577077313,12.790872732509,132.13166089081)) ;
#118861 = CARTESIAN_POINT('Ctrl Pts',(-15.3242924340642,12.603871831162,132.313637073672)) ;
#118862 = CARTESIAN_POINT('Ctrl Pts',(-15.4117066977416,12.4755978216217,
132.535874664851)) ;
#118863 = CARTESIAN_POINT('Ctrl Pts',(-15.5074337996065,12.4151865443115,
132.782375206903)) ;
#118864 = CARTESIAN_POINT('Ctrl Pts',(-15.6051136198306,12.4270410572104,
133.034636072369)) ;
#118865 = CARTESIAN_POINT('Ctrl Pts',(-15.6986186350994,12.5098502555296,
133.274722192349)) ;
#118866 = CARTESIAN_POINT('Ctrl Pts',(-15.7824419706046,12.6589866002263,
133.486340286416)) ;
#118867 = CARTESIAN_POINT('Ctrl Pts',(-15.8502870980143,12.8615686944882,
133.65153604425)) ;
#118868 = CARTESIAN_POINT('Ctrl Pts',(-15.8989700371052,13.1050266274507,
133.760615654876)) ;
#118869 = CARTESIAN_POINT('Ctrl Pts',(-15.925294229189,13.3718443687466,133.804320981034)) ;
#118870 = CARTESIAN_POINT('Ctrl Pts',(-15.9281777645095,13.6411904118671,
133.779698959797)) ;
#118871 = CARTESIAN_POINT('Ctrl Pts',(-15.9079356090688,13.8968634944342,
133.687249703864)) ;
#118872 = CARTESIAN_POINT('Ctrl Pts',(-15.8672784194845,14.1159779670334,
133.535543259696)) ;
#118873 = CARTESIAN_POINT('Ctrl Pts',(-15.8091810365908,14.287325697854,133.332598922334)) ;
#118874 = CARTESIAN_POINT('Ctrl Pts',(-15.7390992509777,14.3958947367542,
133.094806970649)) ;
#118875 = CARTESIAN_POINT('Ctrl Pts',(-15.6624784834203,14.4351265100489,
132.837862938543)) ;
#118876 = CARTESIAN_POINT('Ctrl Pts',(-15.5856066307678,14.401957868372,132.580198882921)) ;
#118877 = CARTESIAN_POINT('Ctrl Pts',(-15.5145051235158,14.2982652104899,
132.339286619073)) ;
#118878 = CARTESIAN_POINT('Ctrl Pts',(-15.4554958556116,14.132480207139,132.133854824434)) ;
#118879 = CARTESIAN_POINT('Ctrl Pts',(-15.4130454905872,13.915462827869,131.976696127531)) ;
#118880 = CARTESIAN_POINT('Ctrl Pts',(-15.3911774530101,13.6633712465324,
131.879702342287)) ;
#118881 = CARTESIAN_POINT('Ctrl Pts',(-15.3920733735863,13.3940849462189,
131.849205339726)) ;
#118882 = CARTESIAN_POINT('Ctrl Pts',(-15.4165204372103,13.1263052775463,
131.887435828916)) ;
#118883 = CARTESIAN_POINT('Ctrl Pts',(-15.4633817742367,12.8804158751522,
131.991219989087)) ;
#118884 = CARTESIAN_POINT('Ctrl Pts',(-15.5300065791661,12.6733662983206,
132.152744232175)) ;
#118885 = CARTESIAN_POINT('Ctrl Pts',(-15.6125439232497,12.5197379232373,
132.360696324844)) ;
#118886 = CARTESIAN_POINT('Ctrl Pts',(-15.705635796009,12.4310982173194,132.599503551761)) ;
#118887 = CARTESIAN_POINT('Ctrl Pts',(-15.803074203752,12.4134628281618,132.851106820896)) ;
#118888 = CARTESIAN_POINT('Ctrl Pts',(-15.8992731570117,12.4679867371616,
133.098968131885)) ;
#118889 = CARTESIAN_POINT('Ctrl Pts',(-15.9878233128369,12.5916525516401,
133.324414662735)) ;
#118890 = CARTESIAN_POINT('Ctrl Pts',(-16.062379654878,12.7734684549556,133.509251293565)) ;
#118891 = CARTESIAN_POINT('Ctrl Pts',(-16.1194191301887,13.0028688411228,
133.642704445147)) ;
#118892 = CARTESIAN_POINT('Ctrl Pts',(-16.1549941311676,13.2619624535534,
133.71352787575)) ;
#118893 = CARTESIAN_POINT('Ctrl Pts',(-16.1673733877208,13.5340192322936,
133.716408021107)) ;
#118894 = CARTESIAN_POINT('Ctrl Pts',(-16.1564239082465,13.7955675293532,
133.651469162884)) ;
#118895 = CARTESIAN_POINT('Ctrl Pts',(-16.1236090883118,14.0322613707932,
133.522420407032)) ;
#118896 = CARTESIAN_POINT('Ctrl Pts',(-16.0721689251693,14.224389834904,133.339099208771)) ;
#118897 = CARTESIAN_POINT('Ctrl Pts',(-16.0063006341945,14.3598901194567,
133.113539220079)) ;
#118898 = CARTESIAN_POINT('Ctrl Pts',(-15.9311391339714,14.4280176273918,
132.860679199975)) ;
#118899 = CARTESIAN_POINT('Ctrl Pts',(-15.8540954386379,14.4241023725172,
132.602718351768)) ;
#118900 = CARTESIAN_POINT('Ctrl Pts',(-15.7795834996639,14.3482280088461,
132.35173937791)) ;
#118901 = CARTESIAN_POINT('Ctrl Pts',(-15.7150929997006,14.2060724290961,
132.130239203412)) ;
#118902 = CARTESIAN_POINT('Ctrl Pts',(-15.6655571468787,14.0086808494732,
131.952512147199)) ;
#118903 = CARTESIAN_POINT('Ctrl Pts',(-15.6349604163456,13.7691471639152,
131.830048736311)) ;
#118904 = CARTESIAN_POINT('Ctrl Pts',(-15.6264276111756,13.5031160987729,
131.771831492658)) ;
#118905 = CARTESIAN_POINT('Ctrl Pts',(-15.6414545015548,13.2327334020777,
131.782614786388)) ;
#118906 = CARTESIAN_POINT('Ctrl Pts',(-15.6793081117188,12.9767766707072,
131.86018699996)) ;
#118907 = CARTESIAN_POINT('Ctrl Pts',(-15.7383109254035,12.7518157375075,
131.999428531665)) ;
#118908 = CARTESIAN_POINT('Ctrl Pts',(-15.8149740258483,12.5749030577416,
132.190234860575)) ;
#118909 = CARTESIAN_POINT('Ctrl Pts',(-15.9043928505203,12.458725868686,132.418325067201)) ;
#118910 = CARTESIAN_POINT('Ctrl Pts',(-16.0013623248274,12.4118884071783,
132.668331705155)) ;
#118911 = CARTESIAN_POINT('Ctrl Pts',(-16.0980803345127,12.4371447951342,
132.918012708935)) ;
#118912 = CARTESIAN_POINT('Ctrl Pts',(-16.1907253077105,12.5335140178268,
133.155361461328)) ;
#118913 = CARTESIAN_POINT('Ctrl Pts',(-16.2714678242786,12.6929505633227,
133.358205410288)) ;
#118914 = CARTESIAN_POINT('Ctrl Pts',(-16.3363258449632,12.9053983623053,
133.514481626618)) ;
#118915 = CARTESIAN_POINT('Ctrl Pts',(-16.3807666053811,13.1539498796381,
133.611267752896)) ;
#118916 = CARTESIAN_POINT('Ctrl Pts',(-16.4027454324204,13.4226750818637,
133.642307124475)) ;
#118917 = CARTESIAN_POINT('Ctrl Pts',(-16.401215059512,13.6910891460654,133.604723727658)) ;
#118918 = CARTESIAN_POINT('Ctrl Pts',(-16.3768570956532,13.9413684453662,
133.500295149174)) ;
#118919 = CARTESIAN_POINT('Ctrl Pts',(-16.332568989847,14.1526799208371,133.337911715767)) ;
#118920 = CARTESIAN_POINT('Ctrl Pts',(-16.2719528045487,14.3125333416555,
133.127724038229)) ;
#118921 = CARTESIAN_POINT('Ctrl Pts',(-16.2002008694076,14.4088194589569,
132.885039982371)) ;
#118922 = CARTESIAN_POINT('Ctrl Pts',(-16.1225573895585,14.4343198918705,
132.624898644505)) ;
#118923 = CARTESIAN_POINT('Ctrl Pts',(-16.0468359703471,14.3877722127897,
132.370812047708)) ;
#118924 = CARTESIAN_POINT('Ctrl Pts',(-15.9772633495729,14.2711471004472,
132.134233982621)) ;
#118925 = CARTESIAN_POINT('Ctrl Pts',(-15.9212635671219,14.0951742684999,
131.937696121308)) ;
#118926 = CARTESIAN_POINT('Ctrl Pts',(-15.8823816388333,13.870335354891,131.790959834028)) ;
#118927 = CARTESIAN_POINT('Ctrl Pts',(-15.8646619711302,13.612835927565,131.705995937797)) ;
#118928 = CARTESIAN_POINT('Ctrl Pts',(-15.8700234600786,13.3431053086278,
131.688622613142)) ;
#118929 = CARTESIAN_POINT('Ctrl Pts',(-15.8986797747435,13.0784069754049,
131.739222629538)) ;
#118930 = CARTESIAN_POINT('Ctrl Pts',(-15.9498454347427,12.8371325485697,
131.85537890921)) ;
#118931 = CARTESIAN_POINT('Ctrl Pts',(-16.019632479177,12.6399915744991,132.026248377193)) ;
#118932 = CARTESIAN_POINT('Ctrl Pts',(-16.1044500214334,12.4979352646964,
132.240903934042)) ;
#118933 = CARTESIAN_POINT('Ctrl Pts',(-16.1991059233172,12.4220838603556,
132.484204340769)) ;
#118934 = CARTESIAN_POINT('Ctrl Pts',(-16.297051164384,12.4184701300548,132.737175673238)) ;
#118935 = CARTESIAN_POINT('Ctrl Pts',(-16.3915722814502,12.4860424705287,
132.980365390677)) ;
#118936 = CARTESIAN_POINT('Ctrl Pts',(-16.4779684262832,12.6212970350437,
133.199551922946)) ;
#118937 = CARTESIAN_POINT('Ctrl Pts',(-16.5497122738182,12.8133839848722,
133.376079170821)) ;
#118938 = CARTESIAN_POINT('Ctrl Pts',(-16.6030126812763,13.050364922785,133.498541178369)) ;
#118939 = CARTESIAN_POINT('Ctrl Pts',(-16.6341711807537,13.3123037538977,
133.556563217302)) ;
#118940 = CARTESIAN_POINT('Ctrl Pts',(-16.6422066343876,13.5832778951352,
133.546888412643)) ;
#118941 = CARTESIAN_POINT('Ctrl Pts',(-16.6269632342962,13.8428843681781,
133.469196841622)) ;
#118942 = CARTESIAN_POINT('Ctrl Pts',(-16.5903845709853,14.0720013140808,
133.329230796997)) ;
#118943 = CARTESIAN_POINT('Ctrl Pts',(-16.5358497973119,14.2546155515289,
133.136829051385)) ;
#118944 = CARTESIAN_POINT('Ctrl Pts',(-16.4678538223331,14.3779471461467,
132.905056863993)) ;
#118945 = CARTESIAN_POINT('Ctrl Pts',(-16.3919879568045,14.4327785489293,
132.650265716705)) ;
#118946 = CARTESIAN_POINT('Ctrl Pts',(-16.3146543287815,14.4152048482771,
132.391254909722)) ;
#118947 = CARTESIAN_POINT('Ctrl Pts',(-16.2418798056375,14.3266409658442,
132.145530624094)) ;
#118948 = CARTESIAN_POINT('Ctrl Pts',(-16.1796064540115,14.1729214945641,
131.930425537284)) ;
#118949 = CARTESIAN_POINT('Ctrl Pts',(-16.1333430675989,13.9662155459552,
131.762226115951)) ;
#118950 = CARTESIAN_POINT('Ctrl Pts',(-16.1067216716661,13.7208186783693,
131.65139858059)) ;
#118951 = CARTESIAN_POINT('Ctrl Pts',(-16.1025777094809,13.4521886748155,
131.60599836467)) ;
#118952 = CARTESIAN_POINT('Ctrl Pts',(-16.1218683713234,13.1838897462868,
131.629362282739)) ;
#118953 = CARTESIAN_POINT('Ctrl Pts',(-16.1639997121743,12.9313138678917,
131.719275378533)) ;
#118954 = CARTESIAN_POINT('Ctrl Pts',(-16.2267282009721,12.7142071157524,
131.869374219865)) ;
#118955 = CARTESIAN_POINT('Ctrl Pts',(-16.3060391253692,12.5481822862925,
132.067981312188)) ;
#118956 = CARTESIAN_POINT('Ctrl Pts',(-16.3972766323407,12.4445945495957,
132.301375289978)) ;
#118957 = CARTESIAN_POINT('Ctrl Pts',(-16.4943286218477,12.4110615292549,
132.551818241413)) ;
#118958 = CARTESIAN_POINT('Ctrl Pts',(-16.5915886358839,12.4502003410622,
132.802714054145)) ;
#118959 = CARTESIAN_POINT('Ctrl Pts',(-16.6818663882812,12.5587981584367,
133.033390094002)) ;
#118960 = CARTESIAN_POINT('Ctrl Pts',(-16.7601403001768,12.7290992999271,
133.228951738304)) ;
#118961 = CARTESIAN_POINT('Ctrl Pts',(-16.8215906092358,12.9505642966122,
133.375178942379)) ;
#118962 = CARTESIAN_POINT('Ctrl Pts',(-16.8618118836172,13.2039533885785,
133.459671754367)) ;
#118963 = CARTESIAN_POINT('Ctrl Pts',(-16.8793709151704,13.4737768400672,
133.477849805927)) ;
#118964 = CARTESIAN_POINT('Ctrl Pts',(-16.8733999316165,13.7408243528461,
133.42719068513)) ;
#118965 = CARTESIAN_POINT('Ctrl Pts',(-16.8450419521337,13.9843828533781,
133.311202487825)) ;
#118966 = CARTESIAN_POINT('Ctrl Pts',(-16.7975164472383,14.1867700455966,
133.139416973208)) ;
#118967 = CARTESIAN_POINT('Ctrl Pts',(-16.7341358946275,14.3360223311849,
132.921026026179)) ;
#118968 = CARTESIAN_POINT('Ctrl Pts',(-16.660977465977,14.4190304968155,132.674270725282)) ;
#118969 = CARTESIAN_POINT('Ctrl Pts',(-16.5834773099444,14.4311357374112,
132.414740139683)) ;
#118970 = CARTESIAN_POINT('Ctrl Pts',(-16.5080024369756,14.3708887924222,
132.161099658697)) ;
#118971 = CARTESIAN_POINT('Ctrl Pts',(-16.4407492412971,14.2422926877059,
131.931437078686)) ;
#118972 = CARTESIAN_POINT('Ctrl Pts',(-16.3876054278893,14.0562619383273,
131.743209531702)) ;
#118973 = CARTESIAN_POINT('Ctrl Pts',(-16.3523922274863,13.8231736969123,
131.607079126901)) ;
#118974 = CARTESIAN_POINT('Ctrl Pts',(-16.3390157650434,13.5622216724448,
131.534881089191)) ;
#118975 = CARTESIAN_POINT('Ctrl Pts',(-16.3487619639683,13.2923510388066,
131.530347534574)) ;
#118976 = CARTESIAN_POINT('Ctrl Pts',(-16.3817521250503,13.0307856163929,
131.593593437063)) ;
#118977 = CARTESIAN_POINT('Ctrl Pts',(-16.4366407076592,12.7967159031727,
131.720707541001)) ;
#118978 = CARTESIAN_POINT('Ctrl Pts',(-16.5097876602422,12.6083942654361,
131.901281935499)) ;
#118979 = CARTESIAN_POINT('Ctrl Pts',(-16.5969702538156,12.4782667075604,
132.122811514274)) ;
#118980 = CARTESIAN_POINT('Ctrl Pts',(-16.6922267232362,12.4160107642981,
132.368047019534)) ;
#118981 = CARTESIAN_POINT('Ctrl Pts',(-16.7901867754655,12.425588916255,132.621043045965)) ;
#118982 = CARTESIAN_POINT('Ctrl Pts',(-16.8842341319186,12.5070743322311,
132.862581766032)) ;
#118983 = CARTESIAN_POINT('Ctrl Pts',(-16.967977842745,12.6538727730597,133.074133355427)) ;
#118984 = CARTESIAN_POINT('Ctrl Pts',(-17.0364591546495,12.8553499552797,
133.241130447034)) ;
#118985 = CARTESIAN_POINT('Ctrl Pts',(-17.0857411108294,13.098103384175,133.351941598924)) ;
#118986 = CARTESIAN_POINT('Ctrl Pts',(-17.1126981511373,13.3649638276871,
133.397446396314)) ;
#118987 = CARTESIAN_POINT('Ctrl Pts',(-17.116159442986,13.6334094300958,133.374637115501)) ;
#118988 = CARTESIAN_POINT('Ctrl Pts',(-17.0967738382637,13.8886868396263,
133.284851993961)) ;
#118989 = CARTESIAN_POINT('Ctrl Pts',(-17.056493649699,14.1104518310445,133.134051885151)) ;
#118990 = CARTESIAN_POINT('Ctrl Pts',(-16.9988013317732,14.2832226261628,
132.932301353712)) ;
#118991 = CARTESIAN_POINT('Ctrl Pts',(-16.9290378227814,14.3937886224781,
132.69545277715)) ;
#118992 = CARTESIAN_POINT('Ctrl Pts',(-16.8521634203114,14.4350213815805,
132.437618360093)) ;
#118993 = CARTESIAN_POINT('Ctrl Pts',(-16.7755820965094,14.4038716563582,
132.180961179455)) ;
#118994 = CARTESIAN_POINT('Ctrl Pts',(-16.7041025877262,14.302057440806,131.938891583268)) ;
#118995 = CARTESIAN_POINT('Ctrl Pts',(-16.6447062661467,14.1377082691097,
131.732320566612)) ;
#118996 = CARTESIAN_POINT('Ctrl Pts',(-16.6018098618319,13.9225120820519,
131.573940678987)) ;
#118997 = CARTESIAN_POINT('Ctrl Pts',(-16.5792495458964,13.6705375102117,
131.474838163571)) ;
#118998 = CARTESIAN_POINT('Ctrl Pts',(-16.5795380154602,13.401884525291,131.442617582448)) ;
#118999 = CARTESIAN_POINT('Ctrl Pts',(-16.6031684812186,13.1344381659713,
131.478552161521)) ;
#119000 = CARTESIAN_POINT('Ctrl Pts',(-16.6496627637314,12.8864833048174,
131.581096733802)) ;
#119001 = CARTESIAN_POINT('Ctrl Pts',(-16.7154366448062,12.6791960280418,
131.740309941251)) ;
#119002 = CARTESIAN_POINT('Ctrl Pts',(-16.7976993700621,12.5233811391943,
131.947393602466)) ;
#119003 = CARTESIAN_POINT('Ctrl Pts',(-16.8904385311137,12.4327816584244,
132.185216053626)) ;
#119004 = CARTESIAN_POINT('Ctrl Pts',(-16.9881341422106,12.4129159573699,
132.437466061827)) ;
#119005 = CARTESIAN_POINT('Ctrl Pts',(-17.0843482146644,12.4655032796393,
132.685408560699)) ;
#119006 = CARTESIAN_POINT('Ctrl Pts',(-17.172922450877,12.5866529362795,132.911042601542)) ;
#119007 = CARTESIAN_POINT('Ctrl Pts',(-17.2482855222662,12.7674395708452,
133.098107251199)) ;
#119008 = CARTESIAN_POINT('Ctrl Pts',(-17.3060249584729,12.9966807390071,
133.233489769117)) ;
#119009 = CARTESIAN_POINT('Ctrl Pts',(-17.3420090323852,13.2541241840609,
133.305647431334)) ;
#119010 = CARTESIAN_POINT('Ctrl Pts',(-17.3551351495104,13.5248421394856,
133.310863716187)) ;
#119011 = CARTESIAN_POINT('Ctrl Pts',(-17.3448759274726,13.7882271369091,
133.247779942829)) ;
#119012 = CARTESIAN_POINT('Ctrl Pts',(-17.3126076355024,14.0260983655197,
133.120304445274)) ;
#119013 = CARTESIAN_POINT('Ctrl Pts',(-17.2615228620159,14.2200231919602,
132.93795360189)) ;
#119014 = CARTESIAN_POINT('Ctrl Pts',(-17.1961003041983,14.356772234067,132.713767919682)) ;
#119015 = CARTESIAN_POINT('Ctrl Pts',(-17.1215711456038,14.4269174457709,
132.462945997468)) ;
#119016 = CARTESIAN_POINT('Ctrl Pts',(-17.0439259643199,14.4252572954794,
132.202973398023)) ;
#119017 = CARTESIAN_POINT('Ctrl Pts',(-16.9694410843738,14.3512844735739,
131.952159419064)) ;
#119018 = CARTESIAN_POINT('Ctrl Pts',(-16.9048069433037,14.2117350246389,
131.730367344063)) ;
#119019 = CARTESIAN_POINT('Ctrl Pts',(-16.8545042052513,14.0152548216542,
131.550277704192)) ;
#119020 = CARTESIAN_POINT('Ctrl Pts',(-16.8232933924181,13.7756399540023,
131.425894257679)) ;
#119021 = CARTESIAN_POINT('Ctrl Pts',(-16.8141517807368,13.5122935142519,
131.366177190341)) ;
#119022 = CARTESIAN_POINT('Ctrl Pts',(-16.8283845644128,13.241130032097,131.374556127916)) ;
#119023 = CARTESIAN_POINT('Ctrl Pts',(-16.8656342224088,12.9839533345939,
131.450303268931)) ;
#119024 = CARTESIAN_POINT('Ctrl Pts',(-16.9243039312876,12.7572239976212,
131.58846397778)) ;
#119025 = CARTESIAN_POINT('Ctrl Pts',(-17.0002008430187,12.5794741431288,
131.777175573092)) ;
#119026 = CARTESIAN_POINT('Ctrl Pts',(-17.089545033272,12.4611210765961,132.004960114565)) ;
#119027 = CARTESIAN_POINT('Ctrl Pts',(-17.1858832231545,12.4122668265322,
132.253299215749)) ;
#119028 = CARTESIAN_POINT('Ctrl Pts',(-17.2833704558394,12.4354395083141,
132.504985546955)) ;
#119029 = CARTESIAN_POINT('Ctrl Pts',(-17.3761905784988,12.5301694803305,
132.742858721776)) ;
#119030 = CARTESIAN_POINT('Ctrl Pts',(-17.4571309233802,12.6876686572945,
132.946346983697)) ;
#119031 = CARTESIAN_POINT('Ctrl Pts',(-17.5224238027242,12.8982124580512,
133.103970186522)) ;
#119032 = CARTESIAN_POINT('Ctrl Pts',(-17.5677102283566,13.1472879194742,
133.203047904097)) ;
#119033 = CARTESIAN_POINT('Ctrl Pts',(-17.5902201631136,13.4151706318018,
133.23571624353)) ;
#119034 = CARTESIAN_POINT('Ctrl Pts',(-17.5893444385462,13.6833052731468,
133.200104234833)) ;
#119035 = CARTESIAN_POINT('Ctrl Pts',(-17.5658297900368,13.9335262194554,
133.098280889353)) ;
#119036 = CARTESIAN_POINT('Ctrl Pts',(-17.5217189486775,14.1479664880633,
132.936132518446)) ;
#119037 = CARTESIAN_POINT('Ctrl Pts',(-17.4616218712877,14.3087959168501,
132.727565237457)) ;
#119038 = CARTESIAN_POINT('Ctrl Pts',(-17.3901260006563,14.4069520231813,
132.485627776412)) ;
#119039 = CARTESIAN_POINT('Ctrl Pts',(-17.3129141442959,14.4347039370495,
132.226908077612)) ;
#119040 = CARTESIAN_POINT('Ctrl Pts',(-17.2365534068234,14.3899170768859,
131.970719496114)) ;
#119041 = CARTESIAN_POINT('Ctrl Pts',(-17.1671213847056,14.2758481834518,
131.734760655287)) ;
#119042 = CARTESIAN_POINT('Ctrl Pts',(-17.110414539759,14.1010294405417,131.536029917471)) ;
#119043 = CARTESIAN_POINT('Ctrl Pts',(-17.070996065358,13.8772034323747,131.3877191098)) ;
#119044 = CARTESIAN_POINT('Ctrl Pts',(-17.0526485411338,13.6206147260663,
131.300948159971)) ;
#119045 = CARTESIAN_POINT('Ctrl Pts',(-17.0573044621097,13.3509221462812,
131.281506125412)) ;
#119046 = CARTESIAN_POINT('Ctrl Pts',(-17.0854100559566,13.0853829020601,
131.330437718243)) ;
#119047 = CARTESIAN_POINT('Ctrl Pts',(-17.1356188030015,12.8445476179022,
131.444003647915)) ;
#119048 = CARTESIAN_POINT('Ctrl Pts',(-17.2051252209905,12.6449528736105,
131.613913841807)) ;
#119049 = CARTESIAN_POINT('Ctrl Pts',(-17.2895913546192,12.501260652652,131.827552263625)) ;
#119050 = CARTESIAN_POINT('Ctrl Pts',(-17.3837152874089,12.423505657414,132.069408473703)) ;
#119051 = CARTESIAN_POINT('Ctrl Pts',(-17.4816812872353,12.4173186176401,
132.32243184758)) ;
#119052 = CARTESIAN_POINT('Ctrl Pts',(-17.576953937296,12.4833714818954,132.56760944195)) ;
#119053 = CARTESIAN_POINT('Ctrl Pts',(-17.6632658867121,12.6162285773946,
132.786710307845)) ;
#119054 = CARTESIAN_POINT('Ctrl Pts',(-17.7357544770908,12.8073410485065,
132.965304035698)) ;
#119055 = CARTESIAN_POINT('Ctrl Pts',(-17.7895701941442,13.0432165498209,
133.089294730388)) ;
#119056 = CARTESIAN_POINT('Ctrl Pts',(-17.8214064088599,13.3046949553566,
133.149287622234)) ;
#119057 = CARTESIAN_POINT('Ctrl Pts',(-17.8300953365612,13.5764463640802,
133.141433903753)) ;
#119058 = CARTESIAN_POINT('Ctrl Pts',(-17.8154038505538,13.8363550328947,
133.065377997914)) ;
#119059 = CARTESIAN_POINT('Ctrl Pts',(-17.7795672536449,14.0655921907836,
132.927723437825)) ;
#119060 = CARTESIAN_POINT('Ctrl Pts',(-17.725370419326,14.2503954340108,132.736213361284)) ;
#119061 = CARTESIAN_POINT('Ctrl Pts',(-17.6574361327673,14.3757154030236,
132.504523320352)) ;
#119062 = CARTESIAN_POINT('Ctrl Pts',(-17.5818347558726,14.4321659912553,
132.250567240917)) ;
#119063 = CARTESIAN_POINT('Ctrl Pts',(-17.5047135094807,14.4167343012476,
131.992284390174)) ;
#119064 = CARTESIAN_POINT('Ctrl Pts',(-17.4317377190015,14.3302899803119,
131.745982280086)) ;
#119065 = CARTESIAN_POINT('Ctrl Pts',(-17.3690184396363,14.1784243472653,
131.529566298611)) ;
#119066 = CARTESIAN_POINT('Ctrl Pts',(-17.3220256941153,13.9717507603948,
131.3590462137)) ;
#119067 = CARTESIAN_POINT('Ctrl Pts',(-17.2950308109835,13.7284356730931,
131.247306408457)) ;
#119068 = CARTESIAN_POINT('Ctrl Pts',(-17.2901004199583,13.4606301780327,
131.199659999263)) ;
#119069 = CARTESIAN_POINT('Ctrl Pts',(-17.3088808530583,13.1906192009326,
131.221345418955)) ;
#119070 = CARTESIAN_POINT('Ctrl Pts',(-17.3501438419449,12.9388679840775,
131.30892757268)) ;
#119071 = CARTESIAN_POINT('Ctrl Pts',(-17.4124956771912,12.7195132163599,
131.457797705406)) ;
#119072 = CARTESIAN_POINT('Ctrl Pts',(-17.4915919365344,12.5518557369755,
131.655723289798)) ;
#119073 = CARTESIAN_POINT('Ctrl Pts',(-17.582138027078,12.4467157573859,131.88725129519)) ;
#119074 = CARTESIAN_POINT('Ctrl Pts',(-17.6796558499135,12.4110145774445,
132.138864732051)) ;
#119075 = CARTESIAN_POINT('Ctrl Pts',(-17.7763443868199,12.4479828345384,
132.388317475769)) ;
#119076 = CARTESIAN_POINT('Ctrl Pts',(-17.8671272399962,12.5544308128886,
132.620405505491)) ;
#119077 = CARTESIAN_POINT('Ctrl Pts',(-17.9462888315339,12.7245572177545,
132.818333491493)) ;
#119078 = CARTESIAN_POINT('Ctrl Pts',(-18.0078236151475,12.9435039918997,
132.965026246654)) ;
#119079 = CARTESIAN_POINT('Ctrl Pts',(-18.0487895704932,13.1965754394182,
133.051630649739)) ;
#119080 = CARTESIAN_POINT('Ctrl Pts',(-18.0669610596337,13.465805442607,133.071652747287)) ;
#119081 = CARTESIAN_POINT('Ctrl Pts',(-18.0616988491559,13.7328709787398,
133.023106457066)) ;
#119082 = CARTESIAN_POINT('Ctrl Pts',(-18.0340587835222,13.9772572958127,
132.909247166554)) ;
#119083 = CARTESIAN_POINT('Ctrl Pts',(-17.9868053084932,14.1820529249742,
132.738087238278)) ;
#119084 = CARTESIAN_POINT('Ctrl Pts',(-17.9237844975308,14.3328843736513,
132.520761239238)) ;
#119085 = CARTESIAN_POINT('Ctrl Pts',(-17.8505988882096,14.417801109475,132.273827837852)) ;
#119086 = CARTESIAN_POINT('Ctrl Pts',(-17.773511642618,14.4318123913692,132.0156729237)) ;
#119087 = CARTESIAN_POINT('Ctrl Pts',(-17.6975797543095,14.373230288219,131.760550888382)) ;
#119088 = CARTESIAN_POINT('Ctrl Pts',(-17.6303724161098,14.2469703146016,
131.531194194324)) ;
#119089 = CARTESIAN_POINT('Ctrl Pts',(-17.5766337968563,14.062146501963,131.34115695912)) ;
#119090 = CARTESIAN_POINT('Ctrl Pts',(-17.5409369598325,13.8305007160398,
131.203674990885)) ;
#119091 = CARTESIAN_POINT('Ctrl Pts',(-17.5268539340979,13.5704781299009,
131.129449867294)) ;
#119092 = CARTESIAN_POINT('Ctrl Pts',(-17.5359636480712,13.299460638904,131.122917047577)) ;
#119093 = CARTESIAN_POINT('Ctrl Pts',(-17.5683660353675,13.0377343274411,
131.184480969823)) ;
#119094 = CARTESIAN_POINT('Ctrl Pts',(-17.6223484639304,12.8036245820339,
131.309107763163)) ;
#119095 = CARTESIAN_POINT('Ctrl Pts',(-17.6952608243721,12.6130123285287,
131.488871588966)) ;
#119096 = CARTESIAN_POINT('Ctrl Pts',(-17.7818766036407,12.4813447603753,
131.708836600993)) ;
#119097 = CARTESIAN_POINT('Ctrl Pts',(-17.8773008779211,12.4167223842582,
131.954443952904)) ;
#119098 = CARTESIAN_POINT('Ctrl Pts',(-17.9751477328863,12.42436559993,132.207155605855)) ;
#119099 = CARTESIAN_POINT('Ctrl Pts',(-18.0691420106269,12.5034382891946,
132.448633030959)) ;
#119100 = CARTESIAN_POINT('Ctrl Pts',(-18.1534115083128,12.6484426384731,
132.661676259449)) ;
#119101 = CARTESIAN_POINT('Ctrl Pts',(-18.2225859165493,12.8490571867036,
132.83061106269)) ;
#119102 = CARTESIAN_POINT('Ctrl Pts',(-18.2723758082232,13.0907449616811,
132.942931245798)) ;
#119103 = CARTESIAN_POINT('Ctrl Pts',(-18.2999851225752,13.3559778335449,
132.990488268703)) ;
#119104 = CARTESIAN_POINT('Ctrl Pts',(-18.3041736331466,13.626477299062,132.969568151916)) ;
#119105 = CARTESIAN_POINT('Ctrl Pts',(-18.2854138148956,13.8815733654641,
132.881719274568)) ;
#119106 = CARTESIAN_POINT('Ctrl Pts',(-18.2457410495779,14.1045282563564,
132.732700456118)) ;
#119107 = CARTESIAN_POINT('Ctrl Pts',(-18.1885080075373,14.2789670451528,
132.532299622035)) ;
#119108 = CARTESIAN_POINT('Ctrl Pts',(-18.1189348222045,14.3914951714323,
132.295964267991)) ;
#119109 = CARTESIAN_POINT('Ctrl Pts',(-18.0424869550482,14.434860760417,132.039514831165)) ;
#119110 = CARTESIAN_POINT('Ctrl Pts',(-17.965414998045,14.4056890526457,131.781241274387)) ;
#119111 = CARTESIAN_POINT('Ctrl Pts',(-17.8940126216972,14.3062653162723,
131.539554730981)) ;
#119112 = CARTESIAN_POINT('Ctrl Pts',(-17.8340450774883,14.1434405265247,
131.331242919008)) ;
#119113 = CARTESIAN_POINT('Ctrl Pts',(-17.7905944856401,13.9296996110321,
131.171266220429)) ;
#119114 = CARTESIAN_POINT('Ctrl Pts',(-17.7673324632912,13.6772902073351,
131.069954024796)) ;
#119115 = CARTESIAN_POINT('Ctrl Pts',(-17.7669919620145,13.4099497148246,
131.036034152482)) ;
#119116 = CARTESIAN_POINT('Ctrl Pts',(-17.7899679662138,13.1418739541198,
131.070013306978)) ;
#119117 = CARTESIAN_POINT('Ctrl Pts',(-17.8356284031104,12.8939990849847,
131.170254631528)) ;
#119118 = CARTESIAN_POINT('Ctrl Pts',(-17.9010078368496,12.6844791056233,
131.328208604738)) ;
#119119 = CARTESIAN_POINT('Ctrl Pts',(-17.9833156417732,12.5265062757821,
131.535272013609)) ;
#119120 = CARTESIAN_POINT('Ctrl Pts',(-18.0753610768667,12.4345049912951,
131.771240370348)) ;
#119121 = CARTESIAN_POINT('Ctrl Pts',(-18.1733168029141,12.4124896110262,
132.024140560041)) ;
#119122 = CARTESIAN_POINT('Ctrl Pts',(-18.2692512178841,12.4629154938197,
132.271405332479)) ;
#119123 = CARTESIAN_POINT('Ctrl Pts',(-18.3583177450786,12.582091252431,132.498425476056)) ;
#119124 = CARTESIAN_POINT('Ctrl Pts',(-18.4343847870178,12.7624371771161,
132.687394350924)) ;
#119125 = CARTESIAN_POINT('Ctrl Pts',(-18.4921191579233,12.9881392321824,
132.823106494344)) ;
#119126 = CARTESIAN_POINT('Ctrl Pts',(-18.5291183635577,13.2462582998136,
132.898039284755)) ;
#119127 = CARTESIAN_POINT('Ctrl Pts',(-18.5428634723026,13.5176871774874,
132.904973108306)) ;
#119128 = CARTESIAN_POINT('Ctrl Pts',(-18.533282772069,13.7805944540118,132.843988452066)) ;
#119129 = CARTESIAN_POINT('Ctrl Pts',(-18.5016568117638,14.0195269504541,
132.718389345958)) ;
#119130 = CARTESIAN_POINT('Ctrl Pts',(-18.4510737818769,14.2150385228552,
132.537499304482)) ;
#119131 = CARTESIAN_POINT('Ctrl Pts',(-18.3858483982378,14.3538332825844,
132.313815804307)) ;
#119132 = CARTESIAN_POINT('Ctrl Pts',(-18.3115810381023,14.425964693576,132.063801363807)) ;
#119133 = CARTESIAN_POINT('Ctrl Pts',(-18.2336471930446,14.4260802790596,
131.802854408235)) ;
#119134 = CARTESIAN_POINT('Ctrl Pts',(-18.1596550168565,14.3549350609901,
131.553791750138)) ;
#119135 = CARTESIAN_POINT('Ctrl Pts',(-18.0940802977715,14.2162529068252,
131.3289701238)) ;
#119136 = CARTESIAN_POINT('Ctrl Pts',(-18.043497662721,14.0213156820109,131.148133926052)) ;
#119137 = CARTESIAN_POINT('Ctrl Pts',(-18.0116896745285,13.7835942530776,
131.022110217814)) ;
#119138 = CARTESIAN_POINT('Ctrl Pts',(-18.0018945840821,13.5186608640693,
130.96022838923)) ;
#119139 = CARTESIAN_POINT('Ctrl Pts',(-18.015387995345,13.2494162372405,130.966701013763)) ;
#119140 = CARTESIAN_POINT('Ctrl Pts',(-18.0521726814189,12.9903691341897,
131.040919681268)) ;
#119141 = CARTESIAN_POINT('Ctrl Pts',(-18.1099224441214,12.7636900645103,
131.176588861018)) ;
#119142 = CARTESIAN_POINT('Ctrl Pts',(-18.1860910752611,12.58293139644,131.365788966717)) ;
#119143 = CARTESIAN_POINT('Ctrl Pts',(-18.2742132626293,12.464078841243,131.590363575954)) ;
#119144 = CARTESIAN_POINT('Ctrl Pts',(-18.3709498681828,12.4125693581943,
131.839671118017)) ;
#119145 = CARTESIAN_POINT('Ctrl Pts',(-18.4681772253489,12.4337094194749,
132.090710617766)) ;
#119146 = CARTESIAN_POINT('Ctrl Pts',(-18.5613404295381,12.5263145270348,
132.329552530544)) ;
#119147 = CARTESIAN_POINT('Ctrl Pts',(-18.6427630328411,12.6822587422614,
132.534418750328)) ;
#119148 = CARTESIAN_POINT('Ctrl Pts',(-18.7085834048123,12.8915625531578,
132.693572369479)) ;
#119149 = CARTESIAN_POINT('Ctrl Pts',(-18.7544451348481,13.1392603074742,
132.794397450571)) ;
#119150 = CARTESIAN_POINT('Ctrl Pts',(-18.7776939684164,13.4076118636345,
132.829123711321)) ;
#119151 = CARTESIAN_POINT('Ctrl Pts',(-18.7775202118103,13.6757335658836,
132.795606435297)) ;
#119152 = CARTESIAN_POINT('Ctrl Pts',(-18.7543460918851,13.9281677247044,
132.694557225827)) ;
#119153 = CARTESIAN_POINT('Ctrl Pts',(-18.7113664052483,14.1410411495776,
132.536164994947)) ;
#119154 = CARTESIAN_POINT('Ctrl Pts',(-18.6513254308885,14.3051859901722,
132.327503000793)) ;
#119155 = CARTESIAN_POINT('Ctrl Pts',(-18.5800781063794,14.4050577733478,
132.08631379624)) ;
#119156 = CARTESIAN_POINT('Ctrl Pts',(-18.5028620340349,14.4349188598701,
131.827543141422)) ;
#119157 = CARTESIAN_POINT('Ctrl Pts',(-18.4265303796658,14.3922309368258,
131.571501632903)) ;
#119158 = CARTESIAN_POINT('Ctrl Pts',(-18.3568271888468,14.2801808251174,
131.334757650015)) ;
#119159 = CARTESIAN_POINT('Ctrl Pts',(-18.2996259717083,14.1070360117015,
131.134575830755)) ;
#119160 = CARTESIAN_POINT('Ctrl Pts',(-18.2595414806214,13.8833119581465,
130.984173543853)) ;
#119161 = CARTESIAN_POINT('Ctrl Pts',(-18.2406706595755,13.6288342320535,
130.896064565764)) ;
#119162 = CARTESIAN_POINT('Ctrl Pts',(-18.2446440431587,13.3582466127621,
130.874495973325)) ;
#119163 = CARTESIAN_POINT('Ctrl Pts',(-18.2720331997506,13.0930921970462,
130.921437176205)) ;
#119164 = CARTESIAN_POINT('Ctrl Pts',(-18.3216690049672,12.8509541226963,
131.033284294486)) ;
#119165 = CARTESIAN_POINT('Ctrl Pts',(-18.3906418061962,12.650062531176,131.201654512555)) ;
#119166 = CARTESIAN_POINT('Ctrl Pts',(-18.4748708111884,12.504322010349,131.414548325661)) ;
#119167 = CARTESIAN_POINT('Ctrl Pts',(-18.5689804093053,12.424693152161,131.656306690995)) ;
#119168 = CARTESIAN_POINT('Ctrl Pts',(-18.6664270906772,12.4164961973712,
131.907982194017)) ;
#119169 = CARTESIAN_POINT('Ctrl Pts',(-18.7619319234567,12.4802514111472,
132.153820565409)) ;
#119170 = CARTESIAN_POINT('Ctrl Pts',(-18.8488118214195,12.6116452910191,
132.374492857226)) ;
#119171 = CARTESIAN_POINT('Ctrl Pts',(-18.9216643022121,12.8011772311019,
132.554182029598)) ;
#119172 = CARTESIAN_POINT('Ctrl Pts',(-18.9759494387784,13.0350450036084,
132.679662652176)) ;
#119173 = CARTESIAN_POINT('Ctrl Pts',(-19.008603835286,13.2969780565828,132.741915753718)) ;
#119174 = CARTESIAN_POINT('Ctrl Pts',(-19.0179410748661,13.5677347022496,
132.736081758383)) ;
#119175 = CARTESIAN_POINT('Ctrl Pts',(-19.0040398597584,13.8283851985519,
132.662329536592)) ;
#119176 = CARTESIAN_POINT('Ctrl Pts',(-18.9686055938327,14.0598714357244,
132.525687738623)) ;
#119177 = CARTESIAN_POINT('Ctrl Pts',(-18.9149811896249,14.2455587727683,
132.335940170202)) ;
#119178 = CARTESIAN_POINT('Ctrl Pts',(-18.8476802246462,14.3725641558704,
132.106227330158)) ;
#119179 = CARTESIAN_POINT('Ctrl Pts',(-18.7719847153341,14.4315964719956,
131.851881968485)) ;
#119180 = CARTESIAN_POINT('Ctrl Pts',(-18.6946462872458,14.4181824180769,
131.592890297641)) ;
#119181 = CARTESIAN_POINT('Ctrl Pts',(-18.6214844495098,14.3336378097198,
131.346050846128)) ;
#119182 = CARTESIAN_POINT('Ctrl Pts',(-18.558560768651,14.1840091136267,131.12913359779)) ;
#119183 = CARTESIAN_POINT('Ctrl Pts',(-18.5109894847597,13.9789558298509,
130.956930823342)) ;
#119184 = CARTESIAN_POINT('Ctrl Pts',(-18.4832446592943,13.735580763414,130.842869411275)) ;
#119185 = CARTESIAN_POINT('Ctrl Pts',(-18.4777486344568,13.4678622164134,
130.793539893276)) ;
#119186 = CARTESIAN_POINT('Ctrl Pts',(-18.495693449302,13.1991328170732,130.812970863617)) ;
#119187 = CARTESIAN_POINT('Ctrl Pts',(-18.5365410093149,12.9452257159657,
130.89915162287)) ;
#119188 = CARTESIAN_POINT('Ctrl Pts',(-18.5980095580789,12.7259341405257,
131.045633388828)) ;
#119189 = CARTESIAN_POINT('Ctrl Pts',(-18.6767481508151,12.5559411179341,
131.242447155862)) ;
#119190 = CARTESIAN_POINT('Ctrl Pts',(-18.7675488804155,12.4485460989971,
131.474543240346)) ;
#119191 = CARTESIAN_POINT('Ctrl Pts',(-18.864393631756,12.411159941536,131.724388858746)) ;
#119192 = CARTESIAN_POINT('Ctrl Pts',(-18.9612913750933,12.4456278245902,
131.974422082055)) ;
#119193 = CARTESIAN_POINT('Ctrl Pts',(-19.0529969299443,12.5514145649144,
132.208941501209)) ;
#119194 = CARTESIAN_POINT('Ctrl Pts',(-19.1316790447807,12.7181519501975,
132.405838209825)) ;
#119195 = CARTESIAN_POINT('Ctrl Pts',(-19.1941048725885,12.9364297118054,
132.555003305589)) ;
#119196 = CARTESIAN_POINT('Ctrl Pts',(-19.2356761496976,13.1887531889945,
132.643385652304)) ;
#119197 = CARTESIAN_POINT('Ctrl Pts',(-19.2545675080689,13.4580633394379,
132.665473483181)) ;
#119198 = CARTESIAN_POINT('Ctrl Pts',(-19.2499351678231,13.7256377913563,
132.618747198731)) ;
#119199 = CARTESIAN_POINT('Ctrl Pts',(-19.222967559006,13.9704139495142,132.506920039618)) ;
#119200 = CARTESIAN_POINT('Ctrl Pts',(-19.1762304653284,14.1767864400758,
132.337249155195)) ;
#119201 = CARTESIAN_POINT('Ctrl Pts',(-19.1135752785484,14.3292888579234,
132.120987640675)) ;
#119202 = CARTESIAN_POINT('Ctrl Pts',(-19.0408547841555,14.4162419047305,
131.875517748366)) ;
#119203 = CARTESIAN_POINT('Ctrl Pts',(-18.9633148456444,14.4323070590761,
131.615823606619)) ;
#119204 = CARTESIAN_POINT('Ctrl Pts',(-18.8879283003201,14.3764282439281,
131.362607849227)) ;
#119205 = CARTESIAN_POINT('Ctrl Pts',(-18.8198998869481,14.2515625460975,
131.130626311494)) ;
#119206 = CARTESIAN_POINT('Ctrl Pts',(-18.7657339233337,14.0682228318719,
130.939356613635)) ;
#119207 = CARTESIAN_POINT('Ctrl Pts',(-18.7293985887039,13.8370233843303,
130.799918521597)) ;
#119208 = CARTESIAN_POINT('Ctrl Pts',(-18.714753132366,13.5786249866576,130.724188870764)) ;
#119209 = CARTESIAN_POINT('Ctrl Pts',(-18.7231251925275,13.3076277382397,
130.715494911597)) ;
#119210 = CARTESIAN_POINT('Ctrl Pts',(-18.7548319263464,13.0452573122607,
130.775019949537)) ;
#119211 = CARTESIAN_POINT('Ctrl Pts',(-18.8084749840881,12.8091512622852,
130.89851543204)) ;
#119212 = CARTESIAN_POINT('Ctrl Pts',(-18.8808676525224,12.617551612867,131.076811574621)) ;
#119213 = CARTESIAN_POINT('Ctrl Pts',(-18.966903542301,12.4843718023618,131.295172588613)) ;
#119214 = CARTESIAN_POINT('Ctrl Pts',(-19.0622475184182,12.4175958724791,
131.540512838689)) ;
#119215 = CARTESIAN_POINT('Ctrl Pts',(-19.1600037141583,12.4230554954089,
131.792998859898)) ;
#119216 = CARTESIAN_POINT('Ctrl Pts',(-19.2543388718931,12.5002516562104,
132.035417010935)) ;
#119217 = CARTESIAN_POINT('Ctrl Pts',(-19.338755390033,12.6429371553798,132.248988409665)) ;
#119218 = CARTESIAN_POINT('Ctrl Pts',(-19.4087513849138,12.8430359620073,
132.420167940555)) ;
#119219 = CARTESIAN_POINT('Ctrl Pts',(-19.4589520558227,13.0829430987805,
132.533810431169)) ;
#119220 = CARTESIAN_POINT('Ctrl Pts',(-19.4872983129428,13.348262589156,132.58344872288)) ;
#119221 = CARTESIAN_POINT('Ctrl Pts',(-19.4921943292312,13.617980538018,132.564712919865)) ;
#119222 = CARTESIAN_POINT('Ctrl Pts',(-19.4739943482068,13.8754577927148,
132.478285317474)) ;
#119223 = CARTESIAN_POINT('Ctrl Pts',(-19.4347077988006,14.0994368224178,
132.330372944685)) ;
#119224 = CARTESIAN_POINT('Ctrl Pts',(-19.3782971940941,14.2743408293056,
132.132593583898)) ;
#119225 = CARTESIAN_POINT('Ctrl Pts',(-19.3088357404323,14.3892596729095,
131.896487153757)) ;
#119226 = CARTESIAN_POINT('Ctrl Pts',(-19.2325449021963,14.4346258040112,
131.640520892899)) ;
#119227 = CARTESIAN_POINT('Ctrl Pts',(-19.1551979357679,14.4074612330324,
131.381356793623)) ;
#119228 = CARTESIAN_POINT('Ctrl Pts',(-19.083606290679,14.3096987835835,131.139122210316)) ;
#119229 = CARTESIAN_POINT('Ctrl Pts',(-19.0234462893368,14.1493774031888,
130.930391073382)) ;
#119230 = CARTESIAN_POINT('Ctrl Pts',(-18.9792574006034,13.935562868649,130.768056883055)) ;
#119231 = CARTESIAN_POINT('Ctrl Pts',(-18.9555376955123,13.6861606118435,
130.665702303709)) ;
#119232 = CARTESIAN_POINT('Ctrl Pts',(-18.954462394183,13.4167352169348,130.629337609962)) ;
#119233 = CARTESIAN_POINT('Ctrl Pts',(-18.9768166950085,13.1492793406519,
130.661613632357)) ;
#119234 = CARTESIAN_POINT('Ctrl Pts',(-19.0218215119309,12.9005268787558,
130.759937465637)) ;
#119235 = CARTESIAN_POINT('Ctrl Pts',(-19.0867458494723,12.6897474261303,
130.916549878415)) ;
#119236 = CARTESIAN_POINT('Ctrl Pts',(-19.1682533043497,12.5306016297354,
131.121425098996)) ;
#119237 = CARTESIAN_POINT('Ctrl Pts',(-19.260528066382,12.4360458848473,131.35789087038)) ;
#119238 = CARTESIAN_POINT('Ctrl Pts',(-19.3582763243507,12.412131814889,131.610239658224)) ;
#119239 = CARTESIAN_POINT('Ctrl Pts',(-19.4545355523176,12.4605358033904,
131.858387318007)) ;
#119240 = CARTESIAN_POINT('Ctrl Pts',(-19.5439662249688,12.5784164440372,
132.086417619438)) ;
#119241 = CARTESIAN_POINT('Ctrl Pts',(-19.6198702779238,12.7554816677878,
132.275200633831)) ;
#119242 = CARTESIAN_POINT('Ctrl Pts',(-19.6786787472394,12.981762434369,132.413779248081)) ;
#119243 = CARTESIAN_POINT('Ctrl Pts',(-19.7160997954442,13.2381598405705,
132.490097944135)) ;
#119244 = CARTESIAN_POINT('Ctrl Pts',(-19.7305986983189,13.5101992275675,
132.499139671301)) ;
#119245 = CARTESIAN_POINT('Ctrl Pts',(-19.7216726258315,13.7733131452284,
132.440105357691)) ;
#119246 = CARTESIAN_POINT('Ctrl Pts',(-19.6904705567742,14.0140641414936,
132.315613122368)) ;
#119247 = CARTESIAN_POINT('Ctrl Pts',(-19.6405829973198,14.2098744851872,
132.136924271088)) ;
#119248 = CARTESIAN_POINT('Ctrl Pts',(-19.5757967424892,14.350580234219,131.914544882587)) ;
#119249 = CARTESIAN_POINT('Ctrl Pts',(-19.5016300544753,14.424831664933,131.664786233143)) ;
#119250 = CARTESIAN_POINT('Ctrl Pts',(-19.4237853420446,14.4272048065726,
131.404140384913)) ;
#119251 = CARTESIAN_POINT('Ctrl Pts',(-19.3494177718881,14.3577939538396,
131.15388324979)) ;
#119252 = CARTESIAN_POINT('Ctrl Pts',(-19.2837725347632,14.2217457510102,
130.929018006421)) ;
#119253 = CARTESIAN_POINT('Ctrl Pts',(-19.2323040587634,14.0267541205093,
130.745331387743)) ;
#119254 = CARTESIAN_POINT('Ctrl Pts',(-19.2001707430858,13.7911380012518,
130.618536649777)) ;
#119255 = CARTESIAN_POINT('Ctrl Pts',(-19.1896182239787,13.5273990690374,
130.554516339063)) ;
#119256 = CARTESIAN_POINT('Ctrl Pts',(-19.2024378328386,13.2571616705375,
130.55890952724)) ;
#119257 = CARTESIAN_POINT('Ctrl Pts',(-19.2385890329441,12.9974108749585,
130.631270893564)) ;
#119258 = CARTESIAN_POINT('Ctrl Pts',(-19.2958501694243,12.7695379625925,
130.76548642622)) ;
#119259 = CARTESIAN_POINT('Ctrl Pts',(-19.3711145282568,12.5879936819102,
130.952222944991)) ;
#119260 = CARTESIAN_POINT('Ctrl Pts',(-19.4594662841901,12.4663339694794,
131.177257058661)) ;
#119261 = CARTESIAN_POINT('Ctrl Pts',(-19.5560732523899,12.4130530302768,
131.426195851942)) ;
#119262 = CARTESIAN_POINT('Ctrl Pts',(-19.6531733858751,12.4321501151392,
131.676919018143)) ;
#119263 = CARTESIAN_POINT('Ctrl Pts',(-19.7463970498452,12.5224108071959,
131.916006524141)) ;
#119264 = CARTESIAN_POINT('Ctrl Pts',(-19.8285870860188,12.6773122255345,
132.122965690291)) ;
#119265 = CARTESIAN_POINT('Ctrl Pts',(-19.8948121933427,12.8853931942508,
132.283318194652)) ;
#119266 = CARTESIAN_POINT('Ctrl Pts',(-19.9411314766599,13.1311434549155,
132.385618122778)) ;
#119267 = CARTESIAN_POINT('Ctrl Pts',(-19.965179017902,13.4000886960601,132.422564022338)) ;
#119268 = CARTESIAN_POINT('Ctrl Pts',(-19.9655799290756,13.6679854854521,
132.390772501259)) ;
#119269 = CARTESIAN_POINT('Ctrl Pts',(-19.9433576038818,13.9198929114768,
132.292714121361)) ;
#119270 = CARTESIAN_POINT('Ctrl Pts',(-19.9003340118905,14.1367331650745,
132.133759563188)) ;
#119271 = CARTESIAN_POINT('Ctrl Pts',(-19.8412787515206,14.3006761293965,
131.928331239691)) ;
#119272 = CARTESIAN_POINT('Ctrl Pts',(-19.7698433836344,14.4034182515294,
131.686360469873)) ;
#119273 = CARTESIAN_POINT('Ctrl Pts',(-19.6928908319003,14.4350219442823,
131.428454049308)) ;
#119274 = CARTESIAN_POINT('Ctrl Pts',(-19.6163658838612,14.3943912084008,
131.171802938922)) ;
#119275 = CARTESIAN_POINT('Ctrl Pts',(-19.5464071737182,14.2842181176635,
130.934326074757)) ;
#119276 = CARTESIAN_POINT('Ctrl Pts',(-19.4887700986895,14.1123337883522,
130.732832985859)) ;
#119277 = CARTESIAN_POINT('Ctrl Pts',(-19.4483529098591,13.8914433195642,
130.581689210717)) ;
#119278 = CARTESIAN_POINT('Ctrl Pts',(-19.4286626325355,13.6364805830374,
130.491015707154)) ;
#119279 = CARTESIAN_POINT('Ctrl Pts',(-19.4319737247805,13.3663281514523,
130.467552630673)) ;
#119280 = CARTESIAN_POINT('Ctrl Pts',(-19.4587287510164,13.1002904677936,
130.512580019223)) ;
#119281 = CARTESIAN_POINT('Ctrl Pts',(-19.5077690316902,12.857318656671,130.622698530342)) ;
#119282 = CARTESIAN_POINT('Ctrl Pts',(-19.5762479760817,12.6550558730351,
130.789623948442)) ;
#119283 = CARTESIAN_POINT('Ctrl Pts',(-19.660020761891,12.5076994857307,131.001221346156)) ;
#119284 = CARTESIAN_POINT('Ctrl Pts',(-19.7539073771051,12.4260782078646,
131.24233160486)) ;
#119285 = CARTESIAN_POINT('Ctrl Pts',(-19.8512928032056,12.415541436623,131.493846182344)) ;
#119286 = CARTESIAN_POINT('Ctrl Pts',(-19.9476463280343,12.4780902877727,
131.741909766604)) ;
#119287 = CARTESIAN_POINT('Ctrl Pts',(-20.0340220644824,12.6066343882026,
131.961417774719)) ;
#119288 = CARTESIAN_POINT('Ctrl Pts',(-20.1076913571221,12.7952136199714,
132.143357435918)) ;
#119289 = CARTESIAN_POINT('Ctrl Pts',(-20.1624822594016,13.027981899229,132.270339157323)) ;
#119290 = CARTESIAN_POINT('Ctrl Pts',(-20.1958184055906,13.289687480561,132.334542561591)) ;
#119291 = CARTESIAN_POINT('Ctrl Pts',(-20.2057710640606,13.5603128220289,
132.330524427759)) ;
#119292 = CARTESIAN_POINT('Ctrl Pts',(-20.1925448224243,13.8211027693198,
132.258797489589)) ;
#119293 = CARTESIAN_POINT('Ctrl Pts',(-20.1576816405266,14.0538032313773,
132.123806125058)) ;
#119294 = CARTESIAN_POINT('Ctrl Pts',(-20.1045068706167,14.241090775664,131.935361080149)) ;
#119295 = CARTESIAN_POINT('Ctrl Pts',(-20.0373054709632,14.3701941266746,
131.705842074109)) ;
#119296 = CARTESIAN_POINT('Ctrl Pts',(-19.9618110201247,14.4308809538835,
131.452116070863)) ;
#119297 = CARTESIAN_POINT('Ctrl Pts',(-19.884682289029,14.419613884929,131.193839945316)) ;
#119298 = CARTESIAN_POINT('Ctrl Pts',(-19.8111397376494,14.336836848792,130.945808512456)) ;
#119299 = CARTESIAN_POINT('Ctrl Pts',(-19.7480300404302,14.1892311094166,
130.728433160336)) ;
#119300 = CARTESIAN_POINT('Ctrl Pts',(-19.699933640509,13.9859053267194,130.55472695681)) ;
#119301 = CARTESIAN_POINT('Ctrl Pts',(-19.6715026585646,13.742611201067,130.438550909152)) ;
#119302 = CARTESIAN_POINT('Ctrl Pts',(-19.6653745692253,13.4761438373695,
130.387484991165)) ;
#119303 = CARTESIAN_POINT('Ctrl Pts',(-19.682584552737,13.2070931418873,130.404753014799)) ;
#119304 = CARTESIAN_POINT('Ctrl Pts',(-19.7228474706637,12.9521503687759,
130.489184402937)) ;
#119305 = CARTESIAN_POINT('Ctrl Pts',(-19.7837584916582,12.7315094149766,
130.634031485)) ;
#119306 = CARTESIAN_POINT('Ctrl Pts',(-19.8624328122891,12.5595225536488,
130.830528406558)) ;
#119307 = CARTESIAN_POINT('Ctrl Pts',(-19.9522381164699,12.4509681334738,
131.059982587645)) ;
#119308 = CARTESIAN_POINT('Ctrl Pts',(-20.0497696412485,12.4111337658692,
131.311559834098)) ;
#119309 = CARTESIAN_POINT('Ctrl Pts',(-20.1462880258714,12.4436883984276,
131.56064510183)) ;
#119310 = CARTESIAN_POINT('Ctrl Pts',(-20.2383160802438,12.547486739405,131.796082088667)) ;
#119311 = CARTESIAN_POINT('Ctrl Pts',(-20.3173266702043,12.7123018084608,
131.993987635883)) ;
#119312 = CARTESIAN_POINT('Ctrl Pts',(-20.3804588499448,12.9300708055824,
132.145107785543)) ;
#119313 = CARTESIAN_POINT('Ctrl Pts',(-20.4224709372142,13.1802337524753,
132.234962055865)) ;
#119314 = CARTESIAN_POINT('Ctrl Pts',(-20.442183503171,13.4510759220384,132.259227541376)) ;
#119315 = CARTESIAN_POINT('Ctrl Pts',(-20.4381680886622,13.7180592996578,
132.214421277915)) ;
#119316 = CARTESIAN_POINT('Ctrl Pts',(-20.4117618848203,13.964278608138,132.104156183895)) ;
#119317 = CARTESIAN_POINT('Ctrl Pts',(-20.3656256486064,14.1712561679291,
131.936335517623)) ;
#119318 = CARTESIAN_POINT('Ctrl Pts',(-20.3036358508574,14.325372518196,131.722127818412)) ;
#119319 = CARTESIAN_POINT('Ctrl Pts',(-20.2305670104494,14.4148742609065,
131.475380669503)) ;
#119320 = CARTESIAN_POINT('Ctrl Pts',(-20.1536631641384,14.4329087895001,
131.217807240407)) ;
#119321 = CARTESIAN_POINT('Ctrl Pts',(-20.0776209899408,14.3788838445396,
130.962446101852)) ;
#119322 = CARTESIAN_POINT('Ctrl Pts',(-20.0095302198618,14.2561019956526,
130.730397244583)) ;
#119323 = CARTESIAN_POINT('Ctrl Pts',(-19.9548661761338,14.0742378272797,
130.537646874608)) ;
#119324 = CARTESIAN_POINT('Ctrl Pts',(-19.9180661082019,13.8451950259534,
130.396991637115)) ;
#119325 = CARTESIAN_POINT('Ctrl Pts',(-19.9026012514215,13.5867435987056,
130.31877045493)) ;
#119326 = CARTESIAN_POINT('Ctrl Pts',(-19.9104102974492,13.3144405101765,
130.308268426565)) ;
#119327 = CARTESIAN_POINT('Ctrl Pts',(-19.9413741530792,13.0528696187883,
130.365781080122)) ;
#119328 = CARTESIAN_POINT('Ctrl Pts',(-19.994244180026,12.8160518820106,130.487079529653)) ;
#119329 = CARTESIAN_POINT('Ctrl Pts',(-20.0661895688882,12.6226065915497,
130.664031439332)) ;
#119330 = CARTESIAN_POINT('Ctrl Pts',(-20.15206016138,12.4871997315169,130.881839087243)) ;
#119331 = CARTESIAN_POINT('Ctrl Pts',(-20.2475919792039,12.4184347778258,
131.127610415521)) ;
#119332 = CARTESIAN_POINT('Ctrl Pts',(-20.3447915155676,12.4219001112793,
131.378662151802)) ;
#119333 = CARTESIAN_POINT('Ctrl Pts',(-20.4394385866213,12.4968774308013,
131.621957625327)) ;
#119334 = CARTESIAN_POINT('Ctrl Pts',(-20.5243460496228,12.6381725760813,
131.83689984342)) ;
#119335 = CARTESIAN_POINT('Ctrl Pts',(-20.5946432733037,12.836067679816,132.009073672112)) ;
#119336 = CARTESIAN_POINT('Ctrl Pts',(-20.645694549428,13.0762565431926,132.125027230254)) ;
#119337 = CARTESIAN_POINT('Ctrl Pts',(-20.6745353505578,13.3398740160854,
132.176274252452)) ;
#119338 = CARTESIAN_POINT('Ctrl Pts',(-20.6801824917773,13.6103043330608,
132.159657715316)) ;
#119339 = CARTESIAN_POINT('Ctrl Pts',(-20.6626223670688,13.8681249215715,
132.075137952304)) ;
#119340 = CARTESIAN_POINT('Ctrl Pts',(-20.6240088572483,14.093287105724,131.929218574679)) ;
#119341 = CARTESIAN_POINT('Ctrl Pts',(-20.5676185800388,14.2707836403436,
131.731276399914)) ;
#119342 = CARTESIAN_POINT('Ctrl Pts',(-20.4988452517907,14.3866738384329,
131.49738923641)) ;
#119343 = CARTESIAN_POINT('Ctrl Pts',(-20.422630635606,14.4343395639672,131.241618386863)) ;
#119344 = CARTESIAN_POINT('Ctrl Pts',(-20.3453774182086,14.4093417175208,
130.982795501148)) ;
#119345 = CARTESIAN_POINT('Ctrl Pts',(-20.2734835723203,14.3139583331245,
130.739681166384)) ;
#119346 = CARTESIAN_POINT('Ctrl Pts',(-20.2125244829768,14.1538396141847,
130.528356549995)) ;
#119347 = CARTESIAN_POINT('Ctrl Pts',(-20.1682116920328,13.9434082127298,
130.365988093249)) ;
#119348 = CARTESIAN_POINT('Ctrl Pts',(-20.1436214196191,13.6926166165872,
130.260781902215)) ;
#119349 = CARTESIAN_POINT('Ctrl Pts',(-20.1419610296582,13.425230952717,130.222938931373)) ;
#119350 = CARTESIAN_POINT('Ctrl Pts',(-20.1635998921199,13.1569924871447,
130.253058297191)) ;
#119351 = CARTESIAN_POINT('Ctrl Pts',(-20.2079427538387,12.9074157476161,
130.349462629733)) ;
#119352 = CARTESIAN_POINT('Ctrl Pts',(-20.2726497055643,12.6946405616374,
130.505302726905)) ;
#119353 = CARTESIAN_POINT('Ctrl Pts',(-20.3531722071491,12.5348309308551,
130.707538050332)) ;
#119354 = CARTESIAN_POINT('Ctrl Pts',(-20.4457849117443,12.4376124689349,
130.944772900056)) ;
#119355 = CARTESIAN_POINT('Ctrl Pts',(-20.5429650872583,12.4118470514465,
131.195641249944)) ;
#119356 = CARTESIAN_POINT('Ctrl Pts',(-20.6395134396743,12.4580456544619,
131.444573191783)) ;
#119357 = CARTESIAN_POINT('Ctrl Pts',(-20.729060984578,12.5736491216982,131.673021193367)) ;
#119358 = CARTESIAN_POINT('Ctrl Pts',(-20.805710500231,12.7495591694402,131.863869452614)) ;
#119359 = CARTESIAN_POINT('Ctrl Pts',(-20.8652025700878,12.9753683734727,
132.004359633657)) ;
#119360 = CARTESIAN_POINT('Ctrl Pts',(-20.9031724037638,13.2312289838448,
132.082275133185)) ;
#119361 = CARTESIAN_POINT('Ctrl Pts',(-20.9183045192812,13.5022491651901,
132.093281255523)) ;
#119362 = CARTESIAN_POINT('Ctrl Pts',(-20.9099738643423,13.7663767191028,
132.035905471493)) ;
#119363 = CARTESIAN_POINT('Ctrl Pts',(-20.8796612889415,14.0063276697149,
131.914271616436)) ;
#119364 = CARTESIAN_POINT('Ctrl Pts',(-20.8301303204373,14.2048736282249,
131.736455792172)) ;
#119365 = CARTESIAN_POINT('Ctrl Pts',(-20.7654662816806,14.347691195203,131.514334056963)) ;
#119366 = CARTESIAN_POINT('Ctrl Pts',(-20.6914004383808,14.4237776298714,
131.264839696289)) ;
#119367 = CARTESIAN_POINT('Ctrl Pts',(-20.6137773916912,14.4280807794616,
131.004929859582)) ;
#119368 = CARTESIAN_POINT('Ctrl Pts',(-20.539195883422,14.3608278808949,130.754040559795)) ;
#119369 = CARTESIAN_POINT('Ctrl Pts',(-20.4730252235718,14.2256360688744,
130.527499972187)) ;
#119370 = CARTESIAN_POINT('Ctrl Pts',(-20.4216242912697,14.0344800390557,
130.344399892003)) ;
#119371 = CARTESIAN_POINT('Ctrl Pts',(-20.3885184235804,13.7980436571723,
130.214472970683)) ;
#119372 = CARTESIAN_POINT('Ctrl Pts',(-20.377391550382,13.5353242806262,130.148856167655)) ;
#119373 = CARTESIAN_POINT('Ctrl Pts',(-20.3895664665377,13.2644874689488,
130.151292077717)) ;
#119374 = CARTESIAN_POINT('Ctrl Pts',(-20.424935009537,13.0050529303368,130.22149042803)) ;
#119375 = CARTESIAN_POINT('Ctrl Pts',(-20.4817292085783,12.7754380725172,
130.354257719508)) ;
#119376 = CARTESIAN_POINT('Ctrl Pts',(-20.5564557866067,12.5925960491714,
130.539466126606)) ;
#119377 = CARTESIAN_POINT('Ctrl Pts',(-20.6444867076033,12.4690082220502,
130.763560977221)) ;
#119378 = CARTESIAN_POINT('Ctrl Pts',(-20.7408881356029,12.4135709144517,
131.011922988235)) ;
#119379 = CARTESIAN_POINT('Ctrl Pts',(-20.8382190130878,12.4306394934732,
131.263254378113)) ;
#119380 = CARTESIAN_POINT('Ctrl Pts',(-20.9313842847165,12.518547510187,131.502278584203)) ;
#119381 = CARTESIAN_POINT('Ctrl Pts',(-21.0141043074733,12.6718440202401,
131.71073096347)) ;
#119382 = CARTESIAN_POINT('Ctrl Pts',(-21.0808229800916,12.8780301734486,
131.87258818294)) ;
#119383 = CARTESIAN_POINT('Ctrl Pts',(-21.1280885064397,13.1252486196316,
131.977346576472)) ;
#119384 = CARTESIAN_POINT('Ctrl Pts',(-21.1525153261514,13.3909665583226,
132.015767819946)) ;
#119385 = CARTESIAN_POINT('Ctrl Pts',(-21.1536959682209,13.6612160977101,
131.985989530158)) ;
#119386 = CARTESIAN_POINT('Ctrl Pts',(-21.1320150342008,13.9131568829426,
131.889591648472)) ;
#119387 = CARTESIAN_POINT('Ctrl Pts',(-21.0898050363088,14.1304384080909,
131.733161381014)) ;
#119388 = CARTESIAN_POINT('Ctrl Pts',(-21.0309240465131,14.2969775123332,
131.528087499457)) ;
#119389 = CARTESIAN_POINT('Ctrl Pts',(-20.9596151124055,14.4015522175217,
131.286441908172)) ;
#119390 = CARTESIAN_POINT('Ctrl Pts',(-20.8830101894348,14.4350500549688,
131.029664145072)) ;
#119391 = CARTESIAN_POINT('Ctrl Pts',(-20.8064689258357,14.3967519657553,
130.773004975845)) ;
#119392 = CARTESIAN_POINT('Ctrl Pts',(-20.736137213621,14.288484921225,130.534398606633)) ;
#119393 = CARTESIAN_POINT('Ctrl Pts',(-20.6779987919655,14.1181740958946,
130.331417324993)) ;
#119394 = CARTESIAN_POINT('Ctrl Pts',(-20.6369638489005,13.897753350153,130.178370778553)) ;
#119395 = CARTESIAN_POINT('Ctrl Pts',(-20.6167209882591,13.6446684780805,
130.086235861724)) ;
#119396 = CARTESIAN_POINT('Ctrl Pts',(-20.619340577804,13.3734340480479,130.060596345406)) ;
#119397 = CARTESIAN_POINT('Ctrl Pts',(-20.6455250015525,13.1072276991085,
130.103978026727)) ;
#119398 = CARTESIAN_POINT('Ctrl Pts',(-20.6937727870842,12.8641925809132,
130.211898521061)) ;
#119399 = CARTESIAN_POINT('Ctrl Pts',(-20.7616960829119,12.660522785721,130.377207275628)) ;
#119400 = CARTESIAN_POINT('Ctrl Pts',(-20.8449119130546,12.511411763425,130.587233212525)) ;
#119401 = CARTESIAN_POINT('Ctrl Pts',(-20.9391429401049,12.4272142219304,
130.829153099245)) ;
#119402 = CARTESIAN_POINT('Ctrl Pts',(-21.0363686243683,12.4150347964973,
131.08024552193)) ;
#119403 = CARTESIAN_POINT('Ctrl Pts',(-21.1322461258614,12.4747491007078,
131.327146007877)) ;
#119404 = CARTESIAN_POINT('Ctrl Pts',(-21.2197199461853,12.6023245536218,
131.549581888249)) ;
#119405 = CARTESIAN_POINT('Ctrl Pts',(-21.2937940109995,12.7898413846695,
131.732688168851)) ;
#119406 = CARTESIAN_POINT('Ctrl Pts',(-21.348940422816,13.0206706862551,131.860832964274)) ;
#119407 = CARTESIAN_POINT('Ctrl Pts',(-21.382960122206,13.2818517746603,131.927025375257)) ;
#119408 = CARTESIAN_POINT('Ctrl Pts',(-21.3935927663565,13.5521277577084,
131.925035187636)) ;
#119409 = CARTESIAN_POINT('Ctrl Pts',(-21.3810616946639,13.813956814144,131.855287243746)) ;
#119410 = CARTESIAN_POINT('Ctrl Pts',(-21.3465398686618,14.0485698568868,
131.721146403302)) ;
#119411 = CARTESIAN_POINT('Ctrl Pts',(-21.2941458660045,14.2361101273789,
131.535193791347)) ;
#119412 = CARTESIAN_POINT('Ctrl Pts',(-21.2270914422676,14.3675383856298,
131.306000181281)) ;
#119413 = CARTESIAN_POINT('Ctrl Pts',(-21.1519155292443,14.4300942221494,
131.053285104387)) ;
#119414 = CARTESIAN_POINT('Ctrl Pts',(-21.0746459363559,14.4208865281834,
130.794540497998)) ;
#119415 = CARTESIAN_POINT('Ctrl Pts',(-21.001112219321,14.3405661224656,130.546646854831)) ;
#119416 = CARTESIAN_POINT('Ctrl Pts',(-20.937120477542,14.1934622842168,130.3264194687)) ;
#119417 = CARTESIAN_POINT('Ctrl Pts',(-20.8887672599036,13.9917022316215,
130.152052794577)) ;
#119418 = CARTESIAN_POINT('Ctrl Pts',(-20.8598430962362,13.7502056970642,
130.034549564694)) ;
#119419 = CARTESIAN_POINT('Ctrl Pts',(-20.8529784671607,13.4844947698669,
129.981374969442)) ;
#119420 = CARTESIAN_POINT('Ctrl Pts',(-20.8696066243062,13.2141841161546,
129.99680343668)) ;
#119421 = CARTESIAN_POINT('Ctrl Pts',(-20.9091638109946,12.9589228275276,
130.079234682195)) ;
#119422 = CARTESIAN_POINT('Ctrl Pts',(-20.9699571386437,12.736270288281,130.223561280645)) ;
#119423 = CARTESIAN_POINT('Ctrl Pts',(-21.0470538745652,12.5648475025287,
130.415923378106)) ;
#119424 = CARTESIAN_POINT('Ctrl Pts',(-21.1376039575189,12.452872634964,130.647152420772)) ;
#119425 = CARTESIAN_POINT('Ctrl Pts',(-21.2341676611939,12.4112941971035,
130.896214160326)) ;
#119426 = CARTESIAN_POINT('Ctrl Pts',(-21.3316648724746,12.4419882074806,
131.147838257514)) ;
#119427 = CARTESIAN_POINT('Ctrl Pts',(-21.4229908419088,12.5427027853094,
131.381587594232)) ;
#119428 = CARTESIAN_POINT('Ctrl Pts',(-21.5030710498832,12.7067963999461,
131.582359437564)) ;
#119429 = CARTESIAN_POINT('Ctrl Pts',(-21.5664742795253,12.9221001567719,
131.734452775999)) ;
#119430 = CARTESIAN_POINT('Ctrl Pts',(-21.6095474559259,13.1741319901515,
131.827050837015)) ;
#119431 = CARTESIAN_POINT('Ctrl Pts',(-21.6296848838974,13.44270233198,131.852822317348)) ;
#119432 = CARTESIAN_POINT('Ctrl Pts',(-21.6263843446627,13.7107857110311,
131.810002375717)) ;
#119433 = CARTESIAN_POINT('Ctrl Pts',(-21.600705277113,13.9568883161136,131.701999462053)) ;
#119434 = CARTESIAN_POINT('Ctrl Pts',(-21.5550025744097,14.1661036759461,
131.535330515378)) ;
#119435 = CARTESIAN_POINT('Ctrl Pts',(-21.4932354794709,14.3219385035442,
131.321716095624)) ;
#119436 = CARTESIAN_POINT('Ctrl Pts',(-21.4208886136072,14.4130180760167,
131.077294854083)) ;
#119437 = CARTESIAN_POINT('Ctrl Pts',(-21.3435192673736,14.4335349357277,
130.818139919528)) ;
#119438 = CARTESIAN_POINT('Ctrl Pts',(-21.267305951962,14.3810414404785,130.562248249026)) ;
#119439 = CARTESIAN_POINT('Ctrl Pts',(-21.1992675154702,14.2609491196068,
130.330540320895)) ;
#119440 = CARTESIAN_POINT('Ctrl Pts',(-21.1438547829946,14.0795344573349,
130.135404883766)) ;
#119441 = CARTESIAN_POINT('Ctrl Pts',(-21.106670609368,13.8529284696564,129.993824030551)) ;
#119442 = CARTESIAN_POINT('Ctrl Pts',(-21.0904836711693,13.5926908131845,
129.913183715177)) ;
#119443 = CARTESIAN_POINT('Ctrl Pts',(-21.09762069255,13.3230678960584,129.9010472229)) ;
#119444 = CARTESIAN_POINT('Ctrl Pts',(-21.1279913585488,13.0595445585026,
129.956646120741)) ;
#119445 = CARTESIAN_POINT('Ctrl Pts',(-21.1804984490399,12.8214089952354,
130.076819568822)) ;
#119446 = CARTESIAN_POINT('Ctrl Pts',(-21.2518741011598,12.6270968112276,
130.252173926582)) ;
#119447 = CARTESIAN_POINT('Ctrl Pts',(-21.3371200957935,12.4904302156697,
130.468268629472)) ;
#119448 = CARTESIAN_POINT('Ctrl Pts',(-21.4321546316194,12.4195264236209,
130.712690158666)) ;
#119449 = CARTESIAN_POINT('Ctrl Pts',(-21.5298416099683,12.4206997898043,
130.965004120227)) ;
#119450 = CARTESIAN_POINT('Ctrl Pts',(-21.6247959686863,12.4940151271389,
131.20914827549)) ;
#119451 = CARTESIAN_POINT('Ctrl Pts',(-21.709797461265,12.6331734144625,131.424459861136)) ;
#119452 = CARTESIAN_POINT('Ctrl Pts',(-21.7805396224499,12.829325604419,131.597967844346)) ;
#119453 = CARTESIAN_POINT('Ctrl Pts',(-21.8322255266126,13.0683012054675,
131.715794377032)) ;
#119454 = CARTESIAN_POINT('Ctrl Pts',(-21.8618419256898,13.332296684324,131.769201522451)) ;
#119455 = CARTESIAN_POINT('Ctrl Pts',(-21.868111171437,13.6026349235875,131.754424312256)) ;
#119456 = CARTESIAN_POINT('Ctrl Pts',(-21.8512879527441,13.8605088298962,
131.672141207112)) ;
#119457 = CARTESIAN_POINT('Ctrl Pts',(-21.8132105801239,14.0871784145907,
131.527740188039)) ;
#119458 = CARTESIAN_POINT('Ctrl Pts',(-21.7575005254597,14.2658344085649,
131.331897526796)) ;
#119459 = CARTESIAN_POINT('Ctrl Pts',(-21.688750583467,14.3843789538156,131.097930102092)) ;
#119460 = CARTESIAN_POINT('Ctrl Pts',(-21.6124995723037,14.4339734253515,
130.841992592288)) ;
#119461 = CARTESIAN_POINT('Ctrl Pts',(-21.5354116726094,14.4110559285979,
130.58374666895)) ;
#119462 = CARTESIAN_POINT('Ctrl Pts',(-21.4633422750838,14.3178925023023,
130.340153529223)) ;
#119463 = CARTESIAN_POINT('Ctrl Pts',(-21.4018571386856,14.159368658012,130.12724479579)) ;
#119464 = CARTESIAN_POINT('Ctrl Pts',(-21.3569844423544,13.9496805303502,
129.963170158196)) ;
#119465 = CARTESIAN_POINT('Ctrl Pts',(-21.3318692614842,13.7013469975745,
129.856640370781)) ;
#119466 = CARTESIAN_POINT('Ctrl Pts',(-21.3294508982289,13.433016471187,129.816421043685)) ;
#119467 = CARTESIAN_POINT('Ctrl Pts',(-21.3503974926524,13.1647607687427,
129.844556985097)) ;
#119468 = CARTESIAN_POINT('Ctrl Pts',(-21.3942807962129,12.9137311981176,
129.939518315123)) ;
#119469 = CARTESIAN_POINT('Ctrl Pts',(-21.4580541106587,12.7007529774686,
130.092823671191)) ;
#119470 = CARTESIAN_POINT('Ctrl Pts',(-21.5386641239171,12.5383275935417,
130.295107054219)) ;
#119471 = CARTESIAN_POINT('Ctrl Pts',(-21.6302556277388,12.4398166133593,
130.529639909855)) ;
#119472 = CARTESIAN_POINT('Ctrl Pts',(-21.7281728291257,12.4114725012227,
130.782378293215)) ;
#119473 = CARTESIAN_POINT('Ctrl Pts',(-21.8246200372728,12.4557968893907,
131.031090267756)) ;
#119474 = CARTESIAN_POINT('Ctrl Pts',(-21.9145460533065,12.5696290859636,
131.260604908557)) ;
#119475 = CARTESIAN_POINT('Ctrl Pts',(-21.9914398177255,12.7436129416571,
131.452243503122)) ;
#119476 = CARTESIAN_POINT('Ctrl Pts',(-22.0515344110072,12.9681022420836,
131.594498874539)) ;
#119477 = CARTESIAN_POINT('Ctrl Pts',(-22.0902148569532,13.2239471204996,
131.674408492276)) ;
#119478 = CARTESIAN_POINT('Ctrl Pts',(-22.1059704140512,13.4941632666535,
131.687320283684)) ;
#119479 = CARTESIAN_POINT('Ctrl Pts',(-22.0983312258742,13.7589186275191,
131.631940757146)) ;
#119480 = CARTESIAN_POINT('Ctrl Pts',(-22.0686225131946,13.9998348960523,
131.51207295587)) ;
#119481 = CARTESIAN_POINT('Ctrl Pts',(-22.0195948042942,14.1997646334102,
131.335728743533)) ;
#119482 = CARTESIAN_POINT('Ctrl Pts',(-21.9554274604182,14.3442637107108,
131.115117618126)) ;
#119483 = CARTESIAN_POINT('Ctrl Pts',(-21.8814136845686,14.4224928337565,
130.865706385146)) ;
#119484 = CARTESIAN_POINT('Ctrl Pts',(-21.8041935492296,14.4291711137562,
130.607145359423)) ;
#119485 = CARTESIAN_POINT('Ctrl Pts',(-21.7288900359016,14.3636108814792,
130.353900660696)) ;
#119486 = CARTESIAN_POINT('Ctrl Pts',(-21.6626234455838,14.2305641375214,
130.127196631545)) ;
#119487 = CARTESIAN_POINT('Ctrl Pts',(-21.610645454006,14.0406275620916,129.942350483753)) ;
#119488 = CARTESIAN_POINT('Ctrl Pts',(-21.5770095653815,13.8058699764793,
129.810964167784)) ;
#119489 = CARTESIAN_POINT('Ctrl Pts',(-21.5651598939791,13.5427808202944,
129.743118276341)) ;
#119490 = CARTESIAN_POINT('Ctrl Pts',(-21.5766853836118,13.2720605312769,
129.743680167768)) ;
#119491 = CARTESIAN_POINT('Ctrl Pts',(-21.6114683168991,13.0118429090763,
129.812136554977)) ;
#119492 = CARTESIAN_POINT('Ctrl Pts',(-21.6674973759044,12.7818788170933,
129.942778475518)) ;
#119493 = CARTESIAN_POINT('Ctrl Pts',(-21.7419079631877,12.5968716626886,
130.126980320084)) ;
#119494 = CARTESIAN_POINT('Ctrl Pts',(-21.8300307322548,12.4712517214802,
130.351211761914)) ;
#119495 = CARTESIAN_POINT('Ctrl Pts',(-21.9258253078081,12.4142247969978,
130.597967097194)) ;
#119496 = CARTESIAN_POINT('Ctrl Pts',(-22.0233578047668,12.4291610418386,
130.849830342346)) ;
#119497 = CARTESIAN_POINT('Ctrl Pts',(-22.1167866797565,12.5152749541959,
131.08960625707)) ;
#119498 = CARTESIAN_POINT('Ctrl Pts',(-22.1999681996922,12.6672522382755,
131.299357549445)) ;
#119499 = CARTESIAN_POINT('Ctrl Pts',(-22.266877655469,12.8714563581182,131.461897045814)) ;
#119500 = CARTESIAN_POINT('Ctrl Pts',(-22.3146434703836,13.1164156516164,
131.568278885002)) ;
#119501 = CARTESIAN_POINT('Ctrl Pts',(-22.3399611550803,13.3833143712004,
131.609107421274)) ;
#119502 = CARTESIAN_POINT('Ctrl Pts',(-22.3417546305339,13.6536761659143,
131.581130534382)) ;
#119503 = CARTESIAN_POINT('Ctrl Pts',(-22.3207495851336,13.9063303611245,
131.486718277812)) ;
#119504 = CARTESIAN_POINT('Ctrl Pts',(-22.2788522684653,14.1256565202968,
131.331061047938)) ;
#119505 = CARTESIAN_POINT('Ctrl Pts',(-22.2205501163383,14.2929703983871,
131.127802439473)) ;
#119506 = CARTESIAN_POINT('Ctrl Pts',(-22.1496885418691,14.3994043107509,
130.887536859964)) ;
#119507 = CARTESIAN_POINT('Ctrl Pts',(-22.0730335167053,14.4351253202345,
130.630552854878)) ;
#119508 = CARTESIAN_POINT('Ctrl Pts',(-21.996345530088,14.3988243968592,130.373443099592)) ;
#119509 = CARTESIAN_POINT('Ctrl Pts',(-21.9257344155299,14.2923293351463,
130.134007145371)) ;
#119510 = CARTESIAN_POINT('Ctrl Pts',(-21.867354018945,14.1241731231248,129.930419720698)) ;
#119511 = CARTESIAN_POINT('Ctrl Pts',(-21.825689326131,13.9051614017352,129.775535782279)) ;
#119512 = CARTESIAN_POINT('Ctrl Pts',(-21.8047754075895,13.6518311474299,
129.681317036466)) ;
#119513 = CARTESIAN_POINT('Ctrl Pts',(-21.806690488997,13.3824708815404,129.653826199804)) ;
#119514 = CARTESIAN_POINT('Ctrl Pts',(-21.8320892264618,13.1154253424266,
129.694864183361)) ;
#119515 = CARTESIAN_POINT('Ctrl Pts',(-21.8799125491881,12.870532663978,129.801417493247)) ;
#119516 = CARTESIAN_POINT('Ctrl Pts',(-21.9473301818534,12.6655370974074,
129.965254569421)) ;
#119517 = CARTESIAN_POINT('Ctrl Pts',(-22.0303478152381,12.5146112418993,
130.174643252011)) ;
#119518 = CARTESIAN_POINT('Ctrl Pts',(-22.1237974779465,12.4289101941166,
130.414481127805)) ;
#119519 = CARTESIAN_POINT('Ctrl Pts',(-22.22120291299,12.414189670065,130.666024010192)) ;
#119520 = CARTESIAN_POINT('Ctrl Pts',(-22.3177472586075,12.4724108557129,
130.914690052658)) ;
#119521 = CARTESIAN_POINT('Ctrl Pts',(-22.4050664943516,12.5978142142,131.13683154333)) ;
#119522 = CARTESIAN_POINT('Ctrl Pts',(-22.4793620392904,12.7826551877608,
131.320734373742)) ;
#119523 = CARTESIAN_POINT('Ctrl Pts',(-22.5354278081203,13.0133814811485,
131.451404804388)) ;
#119524 = CARTESIAN_POINT('Ctrl Pts',(-22.5701066532852,13.2742168699271,
131.5194991142)) ;
#119525 = CARTESIAN_POINT('Ctrl Pts',(-22.5814078746339,13.5450314863386,
131.519394277287)) ;
#119526 = CARTESIAN_POINT('Ctrl Pts',(-22.5694715329342,13.8067211996107,
131.451455874011)) ;
#119527 = CARTESIAN_POINT('Ctrl Pts',(-22.5358417510326,14.041251301363,131.320111797343)) ;
#119528 = CARTESIAN_POINT('Ctrl Pts',(-22.4835621993957,14.2318697191873,
131.134238872589)) ;
#119529 = CARTESIAN_POINT('Ctrl Pts',(-22.4169548508548,14.3645253073145,
130.906437235613)) ;
#119530 = CARTESIAN_POINT('Ctrl Pts',(-22.3422630485774,14.4291513748126,
130.655264086382)) ;
#119531 = CARTESIAN_POINT('Ctrl Pts',(-22.2646712406155,14.4223448235858,
130.395455894871)) ;
#119532 = CARTESIAN_POINT('Ctrl Pts',(-22.1906962386533,14.3433928337176,
130.146147002651)) ;
#119533 = CARTESIAN_POINT('Ctrl Pts',(-22.126864261988,14.1993297551337,129.926664992728)) ;
#119534 = CARTESIAN_POINT('Ctrl Pts',(-22.0777784963834,13.9988090626419,
129.750073791715)) ;
#119535 = CARTESIAN_POINT('Ctrl Pts',(-22.0481534201508,13.7578101990109,
129.630462242444)) ;
#119536 = CARTESIAN_POINT('Ctrl Pts',(-22.04065787053,13.4916491318397,129.575336826241)) ;
#119537 = CARTESIAN_POINT('Ctrl Pts',(-22.0565398005928,13.2223243547225,
129.588728872974)) ;
#119538 = CARTESIAN_POINT('Ctrl Pts',(-22.0955535823169,12.9657468918016,
129.669485051564)) ;
#119539 = CARTESIAN_POINT('Ctrl Pts',(-22.1554227877338,12.7429296801426,
129.811288655846)) ;
#119540 = CARTESIAN_POINT('Ctrl Pts',(-22.2326074989573,12.5685157240841,
130.003665981222)) ;
#119541 = CARTESIAN_POINT('Ctrl Pts',(-22.3229046634719,12.4549912685616,
130.234168931631)) ;
#119542 = CARTESIAN_POINT('Ctrl Pts',(-22.4191582779013,12.4115665135432,
130.482391282104)) ;
#119543 = CARTESIAN_POINT('Ctrl Pts',(-22.5165199381588,12.4399153694957,
130.733695829769)) ;
#119544 = CARTESIAN_POINT('Ctrl Pts',(-22.6085788719043,12.539266271838,130.969408347194)) ;
#119545 = CARTESIAN_POINT('Ctrl Pts',(-22.6888376062549,12.7015765311082,
131.170776121239)) ;
#119546 = CARTESIAN_POINT('Ctrl Pts',(-22.7526224840521,12.9151235328842,
131.32405474122)) ;
#119547 = CARTESIAN_POINT('Ctrl Pts',(-22.7963093376422,13.1655123669942,
131.418544660933)) ;
#119548 = CARTESIAN_POINT('Ctrl Pts',(-22.8172555834161,13.4357073087156,
131.44644515501)) ;
#119549 = CARTESIAN_POINT('Ctrl Pts',(-22.8145947811972,13.7027427371582,
131.405664342584)) ;
#119550 = CARTESIAN_POINT('Ctrl Pts',(-22.7895245214645,13.9504288241065,
131.299348303374)) ;
#119551 = CARTESIAN_POINT('Ctrl Pts',(-22.7442911744941,14.1608970997243,
131.134046242548)) ;
#119552 = CARTESIAN_POINT('Ctrl Pts',(-22.683035539054,14.3182076621176,130.921983637529)) ;
#119553 = CARTESIAN_POINT('Ctrl Pts',(-22.6108042807872,14.4114239711584,
130.677847491563)) ;
#119554 = CARTESIAN_POINT('Ctrl Pts',(-22.5336431840969,14.4338711426872,
130.41936450385)) ;
#119555 = CARTESIAN_POINT('Ctrl Pts',(-22.4574802588175,14.3839736341,130.163713489423)) ;
#119556 = CARTESIAN_POINT('Ctrl Pts',(-22.3887045426789,14.2649033849915,
129.929628525721)) ;
#119557 = CARTESIAN_POINT('Ctrl Pts',(-22.3331731185059,14.0862373314476,
129.734363423515)) ;
#119558 = CARTESIAN_POINT('Ctrl Pts',(-22.2951785325991,13.8593709680806,
129.59019900343)) ;
#119559 = CARTESIAN_POINT('Ctrl Pts',(-22.278460128517,13.6016402175067,129.508253119268)) ;
#119560 = CARTESIAN_POINT('Ctrl Pts',(-22.2848323533062,13.3309241263673,
129.493731727179)) ;
#119561 = CARTESIAN_POINT('Ctrl Pts',(-22.3145834910505,13.0670233439019,
129.547533253071)) ;
#119562 = CARTESIAN_POINT('Ctrl Pts',(-22.3662673822252,12.8286261810775,
129.665410937609)) ;
#119563 = CARTESIAN_POINT('Ctrl Pts',(-22.4370692147307,12.6324569131355,
129.839080633123)) ;
#119564 = CARTESIAN_POINT('Ctrl Pts',(-22.5225167986892,12.4932133607205,
130.055556624894)) ;
#119565 = CARTESIAN_POINT('Ctrl Pts',(-22.6169281495309,12.4206918149119,
130.298317972927)) ;
#119566 = CARTESIAN_POINT('Ctrl Pts',(-22.7149280217507,12.4196226732146,
130.551436865858)) ;
#119567 = CARTESIAN_POINT('Ctrl Pts',(-22.8099912203035,12.4910154919702,
130.795922304285)) ;
#119568 = CARTESIAN_POINT('Ctrl Pts',(-22.8953670162546,12.6283739750249,
131.012318396671)) ;
#119569 = CARTESIAN_POINT('Ctrl Pts',(-22.9667570176051,12.8237069279728,
131.18763100803)) ;
#119570 = CARTESIAN_POINT('Ctrl Pts',(-23.0189001383716,13.0616748954868,
131.306816569627)) ;
#119571 = CARTESIAN_POINT('Ctrl Pts',(-23.0490556418348,13.3240382203917,
131.361942294149)) ;
#119572 = CARTESIAN_POINT('Ctrl Pts',(-23.0560738557443,13.5952493651547,
131.349257476289)) ;
#119573 = CARTESIAN_POINT('Ctrl Pts',(-23.0397586164554,13.8544594901405,
131.268360250981)) ;
#119574 = CARTESIAN_POINT('Ctrl Pts',(-23.0022335507907,14.0816539575776,
131.12563509274)) ;
#119575 = CARTESIAN_POINT('Ctrl Pts',(-22.9471547098177,14.2612879852104,
130.931743906549)) ;
#119576 = CARTESIAN_POINT('Ctrl Pts',(-22.8787472340573,14.3817634357603,
130.698787045464)) ;
#119577 = CARTESIAN_POINT('Ctrl Pts',(-22.8026065314009,14.4336477356996,
130.443163556008)) ;
#119578 = CARTESIAN_POINT('Ctrl Pts',(-22.7250276410476,14.4124733910525,
130.183293296263)) ;
#119579 = CARTESIAN_POINT('Ctrl Pts',(-22.6531551209299,14.3214777368465,
129.940454108184)) ;
#119580 = CARTESIAN_POINT('Ctrl Pts',(-22.5912986814561,14.1652192493521,
129.726511736899)) ;
#119581 = CARTESIAN_POINT('Ctrl Pts',(-22.5456891986183,13.9555650304119,
129.560097274171)) ;
#119582 = CARTESIAN_POINT('Ctrl Pts',(-22.5201337366245,13.7095599623908,
129.452485156075)) ;
#119583 = CARTESIAN_POINT('Ctrl Pts',(-22.5169344827566,13.4405995094296,
129.409863314084)) ;
#119584 = CARTESIAN_POINT('Ctrl Pts',(-22.5374018331414,13.1715077447804,
129.436518432893)) ;
#119585 = CARTESIAN_POINT('Ctrl Pts',(-22.5802715414608,12.9214880554527,
129.528771184389)) ;
#119586 = CARTESIAN_POINT('Ctrl Pts',(-22.6440034901965,12.7055052925361,
129.681687195527)) ;
#119587 = CARTESIAN_POINT('Ctrl Pts',(-22.7237755441732,12.5425196617187,
129.881722442674)) ;
#119588 = CARTESIAN_POINT('Ctrl Pts',(-22.8153026656991,12.4416160239473,
130.115984676027)) ;
#119589 = CARTESIAN_POINT('Ctrl Pts',(-22.9132249157816,12.4112449647392,
130.368717480688)) ;
#119590 = CARTESIAN_POINT('Ctrl Pts',(-23.0098513980588,12.4537097217899,
130.617922318624)) ;
#119591 = CARTESIAN_POINT('Ctrl Pts',(-23.0997589861042,12.5652232795711,
130.847498105072)) ;
#119592 = CARTESIAN_POINT('Ctrl Pts',(-23.177257630143,12.7379440224027,131.040830428269)) ;
#119593 = CARTESIAN_POINT('Ctrl Pts',(-23.237708098821,12.960397453185,131.184248159784)) ;
#119594 = CARTESIAN_POINT('Ctrl Pts',(-23.2771410099792,13.2156634821883,
131.266326678235)) ;
#119595 = CARTESIAN_POINT('Ctrl Pts',(-23.2936412005976,13.4857933764674,
131.281407977912)) ;
#119596 = CARTESIAN_POINT('Ctrl Pts',(-23.2866428376385,13.7522946438347,
131.227738286367)) ;
#119597 = CARTESIAN_POINT('Ctrl Pts',(-23.2573503270286,13.9943544460531,
131.109028172531)) ;
#119598 = CARTESIAN_POINT('Ctrl Pts',(-23.2090388110104,14.1947046175958,
130.934934734007)) ;
#119599 = CARTESIAN_POINT('Ctrl Pts',(-23.1449422933138,14.3414529387325,
130.714386929577)) ;
#119600 = CARTESIAN_POINT('Ctrl Pts',(-23.071480933739,14.4211243068953,130.466760593943)) ;
#119601 = CARTESIAN_POINT('Ctrl Pts',(-22.9941233562367,14.4300014348132,
130.207726168655)) ;
#119602 = CARTESIAN_POINT('Ctrl Pts',(-22.9188030207876,14.3664765738552,
129.954493538436)) ;
#119603 = CARTESIAN_POINT('Ctrl Pts',(-22.8522466727456,14.235605243378,129.726980037117)) ;
#119604 = CARTESIAN_POINT('Ctrl Pts',(-22.7995686386573,14.0463420855303,
129.539948951854)) ;
#119605 = CARTESIAN_POINT('Ctrl Pts',(-22.7654773132939,13.8127312117544,
129.407267248046)) ;
#119606 = CARTESIAN_POINT('Ctrl Pts',(-22.7529636647336,13.5514861581268,
129.337641508112)) ;
#119607 = CARTESIAN_POINT('Ctrl Pts',(-22.7638097876353,13.2797431877816,
129.336093527345)) ;
#119608 = CARTESIAN_POINT('Ctrl Pts',(-22.7978310708524,13.0196141695931,
129.402416181262)) ;
#119609 = CARTESIAN_POINT('Ctrl Pts',(-22.8534471757938,12.7876902143184,
129.531733398873)) ;
#119610 = CARTESIAN_POINT('Ctrl Pts',(-22.9273302721824,12.6015317639528,
129.714440609281)) ;
#119611 = CARTESIAN_POINT('Ctrl Pts',(-23.0148543072416,12.4742597537388,
129.937016753495)) ;
#119612 = CARTESIAN_POINT('Ctrl Pts',(-23.1106134225891,12.4148459760243,
130.183624177554)) ;
#119613 = CARTESIAN_POINT('Ctrl Pts',(-23.2084459565588,12.4277168050886,
130.43627690467)) ;
#119614 = CARTESIAN_POINT('Ctrl Pts',(-23.3019874032968,12.5119511552026,
130.676406889101)) ;
#119615 = CARTESIAN_POINT('Ctrl Pts',(-23.3852438450899,12.6612550924709,
130.886523809409)) ;
#119616 = CARTESIAN_POINT('Ctrl Pts',(-23.4531589894234,12.8654797795072,
131.051765953329)) ;
#119617 = CARTESIAN_POINT('Ctrl Pts',(-23.5013158293354,13.1088715817203,
131.159398237107)) ;
#119618 = CARTESIAN_POINT('Ctrl Pts',(-23.5273348323144,13.3752798847283,
131.202282354274)) ;
#119619 = CARTESIAN_POINT('Ctrl Pts',(-23.5298343688226,13.6458119983222,
131.17637609497)) ;
#119620 = CARTESIAN_POINT('Ctrl Pts',(-23.5094171878235,13.899465813918,131.083638360223)) ;
#119621 = CARTESIAN_POINT('Ctrl Pts',(-23.4682977024105,14.1192748992269,
130.930392419709)) ;
#119622 = CARTESIAN_POINT('Ctrl Pts',(-23.410117737834,14.2891803091472,130.727307342406)) ;
#119623 = CARTESIAN_POINT('Ctrl Pts',(-23.3398467906228,14.3970324953894,
130.488926001134)) ;
#119624 = CARTESIAN_POINT('Ctrl Pts',(-23.2631341283584,14.4351164741298,
130.231697294466)) ;
#119625 = CARTESIAN_POINT('Ctrl Pts',(-23.1864219100301,14.4010787684845,
129.974554635366)) ;
#119626 = CARTESIAN_POINT('Ctrl Pts',(-23.1151468899051,14.2958209248288,
129.732983843262)) ;
#119627 = CARTESIAN_POINT('Ctrl Pts',(-23.0566124154398,14.129652176779,129.52906406716)) ;
#119628 = CARTESIAN_POINT('Ctrl Pts',(-23.0144082905123,13.912176140122,129.372634918644)) ;
#119629 = CARTESIAN_POINT('Ctrl Pts',(-22.9928657656156,13.6594303550192,
129.276558713849)) ;
#119630 = CARTESIAN_POINT('Ctrl Pts',(-22.9940381415481,13.3906473187371,
129.246946981342)) ;
#119631 = CARTESIAN_POINT('Ctrl Pts',(-23.0190161616895,13.1215485791247,
129.286535008088)) ;
#119632 = CARTESIAN_POINT('Ctrl Pts',(-23.0659504345269,12.877499502744,129.390721793247)) ;
#119633 = CARTESIAN_POINT('Ctrl Pts',(-23.1331268462785,12.6702279580221,
129.553707509289)) ;
#119634 = CARTESIAN_POINT('Ctrl Pts',(-23.2154479176507,12.5183910541011,
129.761204124045)) ;
#119635 = CARTESIAN_POINT('Ctrl Pts',(-23.3086829803135,12.4302683160369,
130.000401656271)) ;
#119636 = CARTESIAN_POINT('Ctrl Pts',(-23.4067522708612,12.4138255854832,
130.253644887084)) ;
#119637 = CARTESIAN_POINT('Ctrl Pts',(-23.5022295536224,12.4692849661908,
130.499614004423)) ;
#119638 = CARTESIAN_POINT('Ctrl Pts',(-23.590497552906,12.5930868189149,130.724316427498)) ;
#119639 = CARTESIAN_POINT('Ctrl Pts',(-23.6653857036061,12.7771359268665,
130.909865160465)) ;
#119640 = CARTESIAN_POINT('Ctrl Pts',(-23.7218153355874,13.0059649491312,
131.041714048845)) ;
#119641 = CARTESIAN_POINT('Ctrl Pts',(-23.7571901785065,13.2661471501604,
131.111841913724)) ;
#119642 = CARTESIAN_POINT('Ctrl Pts',(-23.7692103176648,13.536990610461,131.113832196985)) ;
#119643 = CARTESIAN_POINT('Ctrl Pts',(-23.7578885911495,13.7997448803438,
131.04761545879)) ;
#119644 = CARTESIAN_POINT('Ctrl Pts',(-23.7248950980706,14.0350783455638,
130.918172841181)) ;
#119645 = CARTESIAN_POINT('Ctrl Pts',(-23.6728301485584,14.2276700912271,
130.73279573439)) ;
#119646 = CARTESIAN_POINT('Ctrl Pts',(-23.607190849765,14.3610390987627,130.508134028413)) ;
#119647 = CARTESIAN_POINT('Ctrl Pts',(-23.5320583070199,14.4285213562849,
130.255391484949)) ;
#119648 = CARTESIAN_POINT('Ctrl Pts',(-23.4546158086494,14.4233691506753,
129.996090560874)) ;
#119649 = CARTESIAN_POINT('Ctrl Pts',(-23.380643189452,14.3469900608794,129.746892873934)) ;
#119650 = CARTESIAN_POINT('Ctrl Pts',(-23.3160087352734,14.2034039826352,
129.524810838225)) ;
#119651 = CARTESIAN_POINT('Ctrl Pts',(-23.2668172562997,14.0056848042437,
129.348164408924)) ;
#119652 = CARTESIAN_POINT('Ctrl Pts',(-23.2364502982385,13.7644935379873,
129.226215459464)) ;
#119653 = CARTESIAN_POINT('Ctrl Pts',(-23.2282984715539,13.5002463759362,
129.169368760998)) ;
#119654 = CARTESIAN_POINT('Ctrl Pts',(-23.24371050422,13.2284058241885,129.181082860346)) ;
#119655 = CARTESIAN_POINT('Ctrl Pts',(-23.2817138310726,12.9739037522761,
129.259247094097)) ;
#119656 = CARTESIAN_POINT('Ctrl Pts',(-23.3412738291248,12.7484704180283,
129.399951986227)) ;
#119657 = CARTESIAN_POINT('Ctrl Pts',(-23.4177990674146,12.5731123279677,
129.590515150982)) ;
#119658 = CARTESIAN_POINT('Ctrl Pts',(-23.5078548816841,12.45735908031,129.820279560396)) ;
#119659 = CARTESIAN_POINT('Ctrl Pts',(-23.604095848768,12.4118025440313,130.068434118801)) ;
#119660 = CARTESIAN_POINT('Ctrl Pts',(-23.701547171813,12.4381298273325,130.319990066657)) ;
#119661 = CARTESIAN_POINT('Ctrl Pts',(-23.7936910641617,12.5352056627263,
130.556017518531)) ;
#119662 = CARTESIAN_POINT('Ctrl Pts',(-23.8745884919989,12.696300610242,130.759150487779)) ;
#119663 = CARTESIAN_POINT('Ctrl Pts',(-23.9388625765618,12.9082756113126,
130.913902309013)) ;
#119664 = CARTESIAN_POINT('Ctrl Pts',(-23.983317014121,13.1596325323724,131.010413905855)) ;
#119665 = CARTESIAN_POINT('Ctrl Pts',(-24.0046631549015,13.4259468835544,
131.039934337967)) ;
#119666 = CARTESIAN_POINT('Ctrl Pts',(-24.0028248548074,13.6953761011822,
131.001297665737)) ;
#119667 = CARTESIAN_POINT('Ctrl Pts',(-23.9783213573141,13.9437170252716,
130.896659476004)) ;
#119668 = CARTESIAN_POINT('Ctrl Pts',(-23.93357174813,14.155711083142,130.73273190048)) ;
#119669 = CARTESIAN_POINT('Ctrl Pts',(-23.8728119878527,14.3144000216169,
130.522179990839)) ;
#119670 = CARTESIAN_POINT('Ctrl Pts',(-23.8008509799533,14.4096307873655,
130.278840330333)) ;
#119671 = CARTESIAN_POINT('Ctrl Pts',(-23.7237246168415,14.4343455413494,
130.020451918313)) ;
#119672 = CARTESIAN_POINT('Ctrl Pts',(-23.6471274329311,14.3860725328483,
129.763386450898)) ;
#119673 = CARTESIAN_POINT('Ctrl Pts',(-23.5784483932488,14.2695097224109,
129.529774563967)) ;
#119674 = CARTESIAN_POINT('Ctrl Pts',(-23.5222414219864,14.0917907818256,
129.332403324397)) ;
#119675 = CARTESIAN_POINT('Ctrl Pts',(-23.4838194360288,13.8666927390169,
129.187092868066)) ;
#119676 = CARTESIAN_POINT('Ctrl Pts',(-23.4664016523007,13.6093228948058,
129.103058814387)) ;
#119677 = CARTESIAN_POINT('Ctrl Pts',(-23.4720979067043,13.3388432041032,
129.086581594088)) ;
#119678 = CARTESIAN_POINT('Ctrl Pts',(-23.5012168114343,13.0740474373603,
129.138484307447)) ;
#119679 = CARTESIAN_POINT('Ctrl Pts',(-23.5524662673914,12.8343946472962,
129.25503692304)) ;
#119680 = CARTESIAN_POINT('Ctrl Pts',(-23.6224253524384,12.6378259475901,
129.4264139265)) ;
#119681 = CARTESIAN_POINT('Ctrl Pts',(-23.7075121796353,12.4964630119009,
129.641818563098)) ;
#119682 = CARTESIAN_POINT('Ctrl Pts',(-23.8019975756317,12.421725405798,129.884708515321)) ;
#119683 = CARTESIAN_POINT('Ctrl Pts',(-23.8998895978672,12.4187226198539,
130.137544774975)) ;
#119684 = CARTESIAN_POINT('Ctrl Pts',(-23.9948139084966,12.4875916518615,
130.381743115251)) ;
#119685 = CARTESIAN_POINT('Ctrl Pts',(-24.0808838147119,12.6235712310503,
130.600036971764)) ;
#119686 = CARTESIAN_POINT('Ctrl Pts',(-24.1524928045672,12.8167007524725,
130.776115139759)) ;
#119687 = CARTESIAN_POINT('Ctrl Pts',(-24.2053648747095,13.053470084932,130.897425249101)) ;
#119688 = CARTESIAN_POINT('Ctrl Pts',(-24.2363346414086,13.3166529719994,
130.954767098214)) ;
#119689 = CARTESIAN_POINT('Ctrl Pts',(-24.2439518827779,13.5871781568045,
130.943922486326)) ;
#119690 = CARTESIAN_POINT('Ctrl Pts',(-24.2284589955264,13.8461110281262,
130.865554669598)) ;
#119691 = CARTESIAN_POINT('Ctrl Pts',(-24.1914691846138,14.0754123142472,
130.724278834602)) ;
#119692 = CARTESIAN_POINT('Ctrl Pts',(-24.1367058007406,14.2569965366052,
130.531234806345)) ;
#119693 = CARTESIAN_POINT('Ctrl Pts',(-24.0686015337967,14.3792169308405,
130.299169849526)) ;
#119694 = CARTESIAN_POINT('Ctrl Pts',(-23.9928202726193,14.4330645765252,
130.044692226851)) ;
#119695 = CARTESIAN_POINT('Ctrl Pts',(-23.9152030610562,14.4142942137405,
129.784717394)) ;
#119696 = CARTESIAN_POINT('Ctrl Pts',(-23.8427985126538,14.3249818640555,
129.540193183357)) ;
#119697 = CARTESIAN_POINT('Ctrl Pts',(-23.7805649806732,14.1700409450456,
129.325118482017)) ;
#119698 = CARTESIAN_POINT('Ctrl Pts',(-23.7346417673261,13.9629928904563,
129.157974141327)) ;
#119699 = CARTESIAN_POINT('Ctrl Pts',(-23.7083156172197,13.716497244272,129.04792282307)) ;
#119700 = CARTESIAN_POINT('Ctrl Pts',(-23.7044893109021,13.449382384683,129.003661141323)) ;
#119701 = CARTESIAN_POINT('Ctrl Pts',(-23.724174778289,13.179466012535,129.027965195106)) ;
#119702 = CARTESIAN_POINT('Ctrl Pts',(-23.7667235870963,12.9274139548691,
129.119104726136)) ;
#119703 = CARTESIAN_POINT('Ctrl Pts',(-23.8295759439689,12.7115777199899,
129.269649618492)) ;
#119704 = CARTESIAN_POINT('Ctrl Pts',(-23.9089257388214,12.5463884339408,
129.468420668235)) ;
#119705 = CARTESIAN_POINT('Ctrl Pts',(-24.0009772282109,12.4431786927595,
129.703950653175)) ;
#119706 = CARTESIAN_POINT('Ctrl Pts',(-24.0977509267161,12.4112124576001,
129.953697636734)) ;
#119707 = CARTESIAN_POINT('Ctrl Pts',(-24.1948656324168,12.4513454606681,
130.20419806984)) ;
#119708 = CARTESIAN_POINT('Ctrl Pts',(-24.285028808609,12.5610016888449,130.434530136024)) ;
#119709 = CARTESIAN_POINT('Ctrl Pts',(-24.3630579432247,12.7322315301459,
130.629374967685)) ;
#119710 = CARTESIAN_POINT('Ctrl Pts',(-24.4240719874066,12.9536821902703,
130.774419040633)) ;
#119711 = CARTESIAN_POINT('Ctrl Pts',(-24.4640634099182,13.2077095547012,
130.858196825809)) ;
#119712 = CARTESIAN_POINT('Ctrl Pts',(-24.4812915975361,13.4778389937593,
130.875385354315)) ;
#119713 = CARTESIAN_POINT('Ctrl Pts',(-24.4749348184018,13.7447250212435,
130.823586297997)) ;
#119714 = CARTESIAN_POINT('Ctrl Pts',(-24.4464281767638,13.9871379324524,
130.707276700175)) ;
#119715 = CARTESIAN_POINT('Ctrl Pts',(-24.3982867625321,14.1900736683291,
130.53346338122)) ;
#119716 = CARTESIAN_POINT('Ctrl Pts',(-24.3351669079392,14.3373317705726,
130.316081854246)) ;
#119717 = CARTESIAN_POINT('Ctrl Pts',(-24.2614650136263,14.4199335314477,
130.067526586258)) ;
#119718 = CARTESIAN_POINT('Ctrl Pts',(-24.1841440002385,14.4307823932299,
129.808614897003)) ;
#119719 = CARTESIAN_POINT('Ctrl Pts',(-24.1084828214291,14.3690285346023,
129.554295669333)) ;
#119720 = CARTESIAN_POINT('Ctrl Pts',(-24.041888647281,14.2404409958973,129.326810148506)) ;
#119721 = CARTESIAN_POINT('Ctrl Pts',(-23.9886944579791,14.0528076235366,
129.138264979465)) ;
#119722 = CARTESIAN_POINT('Ctrl Pts',(-23.953964486593,13.8202655346865,129.003710925122)) ;
#119723 = CARTESIAN_POINT('Ctrl Pts',(-23.9407661646502,13.5584444943241,
128.931945154736)) ;
#119724 = CARTESIAN_POINT('Ctrl Pts',(-23.951014218669,13.2871050604655,128.928700531277)) ;
#119725 = CARTESIAN_POINT('Ctrl Pts',(-23.9842710836601,13.0271136592546,
128.99288013018)) ;
#119726 = CARTESIAN_POINT('Ctrl Pts',(-24.0393399443066,12.7938647968009,
129.120566173473)) ;
#119727 = CARTESIAN_POINT('Ctrl Pts',(-24.1126551456015,12.6063348260336,
129.301653620629)) ;
#119728 = CARTESIAN_POINT('Ctrl Pts',(-24.1999951112264,12.4770287945195,
129.523636975406)) ;
#119729 = CARTESIAN_POINT('Ctrl Pts',(-24.2953179840485,12.4155889171301,
129.769068705113)) ;
#119730 = CARTESIAN_POINT('Ctrl Pts',(-24.3936269874943,12.4264045775595,
130.022957981845)) ;
#119731 = CARTESIAN_POINT('Ctrl Pts',(-24.487039800036,12.5084012682064,130.262834505256)) ;
#119732 = CARTESIAN_POINT('Ctrl Pts',(-24.5708433676683,12.6562045678091,
130.474478189188)) ;
#119733 = CARTESIAN_POINT('Ctrl Pts',(-24.6390689439144,12.8582528163381,
130.640744689845)) ;
#119734 = CARTESIAN_POINT('Ctrl Pts',(-24.688186273424,13.1022480435351,130.75096865955)) ;
#119735 = CARTESIAN_POINT('Ctrl Pts',(-24.7147148491463,13.3685511401161,
130.795319580132)) ;
#119736 = CARTESIAN_POINT('Ctrl Pts',(-24.7178825838308,13.6374690489365,
130.771584220973)) ;
#119737 = CARTESIAN_POINT('Ctrl Pts',(-24.6981008820832,13.8926337439443,
130.680605414583)) ;
#119738 = CARTESIAN_POINT('Ctrl Pts',(-24.6575485405634,14.1134973909665,
130.529040703755)) ;
#119739 = CARTESIAN_POINT('Ctrl Pts',(-24.5996419056856,14.2854804526752,
130.326666926777)) ;
#119740 = CARTESIAN_POINT('Ctrl Pts',(-24.529617378917,14.3949169679371,130.08901030832)) ;
#119741 = CARTESIAN_POINT('Ctrl Pts',(-24.4533294260154,14.4350950474159,
129.833165182374)) ;
#119742 = CARTESIAN_POINT('Ctrl Pts',(-24.3760965657258,14.4027523558799,
129.574300858813)) ;
#119743 = CARTESIAN_POINT('Ctrl Pts',(-24.3051605815314,14.3004224284984,
129.334015107818)) ;
#119744 = CARTESIAN_POINT('Ctrl Pts',(-24.2456558829535,14.1345848186711,
129.126962774676)) ;
#119745 = CARTESIAN_POINT('Ctrl Pts',(-24.203144223906,13.9188292649382,128.969748265091)) ;
#119746 = CARTESIAN_POINT('Ctrl Pts',(-24.1809374546638,13.6668968263447,
128.87172937497)) ;
#119747 = CARTESIAN_POINT('Ctrl Pts',(-24.1815007016074,13.3982258139503,
128.840326111729)) ;
#119748 = CARTESIAN_POINT('Ctrl Pts',(-24.2056308452266,13.1299459979309,
128.877587112846)) ;
#119749 = CARTESIAN_POINT('Ctrl Pts',(-24.2521574317291,12.8837060255956,
128.98041042931)) ;
#119750 = CARTESIAN_POINT('Ctrl Pts',(-24.3187472777364,12.6755091265604,
129.141737299498)) ;
#119751 = CARTESIAN_POINT('Ctrl Pts',(-24.400840597816,12.5215778534682,129.348502615957)) ;
#119752 = CARTESIAN_POINT('Ctrl Pts',(-24.4940411132764,12.4317802187368,
129.587545619902)) ;
#119753 = CARTESIAN_POINT('Ctrl Pts',(-24.5912174648574,12.4131805115513,
129.838470614325)) ;
#119754 = CARTESIAN_POINT('Ctrl Pts',(-24.6876108574417,12.4668842631246,
130.086844676273)) ;
#119755 = CARTESIAN_POINT('Ctrl Pts',(-24.7757687439987,12.5884450381112,
130.311379023635)) ;
#119756 = CARTESIAN_POINT('Ctrl Pts',(-24.8513379924622,12.7713420936062,
130.498823295008)) ;
#119757 = CARTESIAN_POINT('Ctrl Pts',(-24.9082742295121,12.9988617969997,
130.63219011284)) ;
#119758 = CARTESIAN_POINT('Ctrl Pts',(-24.94437712461,13.2594913097142,130.704313382591)) ;
#119759 = CARTESIAN_POINT('Ctrl Pts',(-24.9569420258268,13.5289133142041,
130.708064597244)) ;
#119760 = CARTESIAN_POINT('Ctrl Pts',(-24.9463665896322,13.7920447587741,
130.644049270301)) ;
#119761 = CARTESIAN_POINT('Ctrl Pts',(-24.913933421227,14.028682332542,130.516205209765)) ;
#119762 = CARTESIAN_POINT('Ctrl Pts',(-24.8624450520878,14.2226477073875,
130.332553173407)) ;
#119763 = CARTESIAN_POINT('Ctrl Pts',(-24.7969465973085,14.358128004445,130.108205057348)) ;
#119764 = CARTESIAN_POINT('Ctrl Pts',(-24.722353105465,14.427517223623,129.857199608081)) ;
#119765 = CARTESIAN_POINT('Ctrl Pts',(-24.644295649574,14.4244373383238,129.595839584828)) ;
#119766 = CARTESIAN_POINT('Ctrl Pts',(-24.5705593446945,14.3501368241958,
129.347511571609)) ;
#119767 = CARTESIAN_POINT('Ctrl Pts',(-24.5056565645644,14.2089998029508,
129.124719851443)) ;
#119768 = CARTESIAN_POINT('Ctrl Pts',(-24.4557713790485,14.0121251226583,
128.94593584056)) ;
#119769 = CARTESIAN_POINT('Ctrl Pts',(-24.4247960653296,13.7718247542597,
128.822203002167)) ;
#119770 = CARTESIAN_POINT('Ctrl Pts',(-24.416027718643,13.5078187050463,128.763529045233)) ;
#119771 = CARTESIAN_POINT('Ctrl Pts',(-24.4306046417983,13.2372789861246,
128.772981600375)) ;
#119772 = CARTESIAN_POINT('Ctrl Pts',(-24.4681460256884,12.9804327366812,
128.849585251481)) ;
#119773 = CARTESIAN_POINT('Ctrl Pts',(-24.5272076352715,12.7540238900059,
128.988844175822)) ;
#119774 = CARTESIAN_POINT('Ctrl Pts',(-24.6031699054307,12.577462748724,129.177818082868)) ;
#119775 = CARTESIAN_POINT('Ctrl Pts',(-24.6927251102051,12.4598742961996,
129.406189054556)) ;
#119776 = CARTESIAN_POINT('Ctrl Pts',(-24.7892829387905,12.4120040777539,
129.655120321832)) ;
#119777 = CARTESIAN_POINT('Ctrl Pts',(-24.8867386589966,12.4365719304023,
129.906705661731)) ;
#119778 = CARTESIAN_POINT('Ctrl Pts',(-24.978747317987,12.5311793642618,130.142476274929)) ;
#119779 = CARTESIAN_POINT('Ctrl Pts',(-25.060355481887,12.6910252925006,130.347571894772)) ;
#119780 = CARTESIAN_POINT('Ctrl Pts',(-25.1249799734368,12.901554601713,130.503394346182)) ;
#119781 = CARTESIAN_POINT('Ctrl Pts',(-25.1699675301259,13.1503193803292,
130.601673711029)) ;
#119782 = CARTESIAN_POINT('Ctrl Pts',(-25.1922305047665,13.4198238179189,
130.633438387821)) ;
#119783 = CARTESIAN_POINT('Ctrl Pts',(-25.1910108110703,13.6867201864748,
130.596962968401)) ;
#119784 = CARTESIAN_POINT('Ctrl Pts',(-25.167052916905,13.9376559874792,130.493686388418)) ;
#119785 = CARTESIAN_POINT('Ctrl Pts',(-25.1228803335291,14.1502428596578,
130.331538878298)) ;
#119786 = CARTESIAN_POINT('Ctrl Pts',(-25.0624593309472,14.3108380657866,
130.121931628785)) ;
#119787 = CARTESIAN_POINT('Ctrl Pts',(-24.9907465662706,14.4079445311136,
129.879330709918)) ;
#119788 = CARTESIAN_POINT('Ctrl Pts',(-24.9136043625224,14.4345276707165,
129.620858009147)) ;
#119789 = CARTESIAN_POINT('Ctrl Pts',(-24.8374005548157,14.3888298809399,
129.365172106487)) ;
#119790 = CARTESIAN_POINT('Ctrl Pts',(-24.7680465549556,14.2738284878411,
129.1294178052)) ;
#119791 = CARTESIAN_POINT('Ctrl Pts',(-24.7114675854268,14.0978368640531,
128.931000104012)) ;
#119792 = CARTESIAN_POINT('Ctrl Pts',(-24.6724005531575,13.8735407720446,
128.783743944974)) ;
#119793 = CARTESIAN_POINT('Ctrl Pts',(-24.6543698495407,13.616875079998,128.697930467751)) ;
#119794 = CARTESIAN_POINT('Ctrl Pts',(-24.659403085665,13.3465064329097,128.679514282414)) ;
#119795 = CARTESIAN_POINT('Ctrl Pts',(-24.6878260612952,13.0815408414728,
128.729420324657)) ;
#119796 = CARTESIAN_POINT('Ctrl Pts',(-24.7384611274853,12.8409647311381,
128.844181431209)) ;
#119797 = CARTESIAN_POINT('Ctrl Pts',(-24.8078392099398,12.642864050615,129.013879190485)) ;
#119798 = CARTESIAN_POINT('Ctrl Pts',(-24.8932722991771,12.498964683589,129.230041309728)) ;
#119799 = CARTESIAN_POINT('Ctrl Pts',(-24.9867207169967,12.4231077011215,
129.47021048062)) ;
#119800 = CARTESIAN_POINT('Ctrl Pts',(-25.0849839469443,12.4177381472718,
129.723995502206)) ;
#119801 = CARTESIAN_POINT('Ctrl Pts',(-25.180011685858,12.4847095066073,129.968519607844)) ;
#119802 = CARTESIAN_POINT('Ctrl Pts',(-25.2665150261769,12.6190667593984,
130.188038371959)) ;
#119803 = CARTESIAN_POINT('Ctrl Pts',(-25.338527272186,12.8107471033722,130.365312618294)) ;
#119804 = CARTESIAN_POINT('Ctrl Pts',(-25.3919035397376,13.0461048084143,
130.488149129457)) ;
#119805 = CARTESIAN_POINT('Ctrl Pts',(-25.4235567372588,13.3089103849839,
130.547469606547)) ;
#119806 = CARTESIAN_POINT('Ctrl Pts',(-25.431859388785,13.5795917474079,130.538616281477)) ;
#119807 = CARTESIAN_POINT('Ctrl Pts',(-25.416926267712,13.839854863598,130.461786666502)) ;
#119808 = CARTESIAN_POINT('Ctrl Pts',(-25.380454759044,14.069864909241,130.322056942441)) ;
#119809 = CARTESIAN_POINT('Ctrl Pts',(-25.3263222418805,14.2524396014981,
130.130958807015)) ;
#119810 = CARTESIAN_POINT('Ctrl Pts',(-25.2583610468973,14.3767943035019,
129.899231984381)) ;
#119811 = CARTESIAN_POINT('Ctrl Pts',(-25.1829041424142,14.4324209572319,
129.645787191873)) ;
#119812 = CARTESIAN_POINT('Ctrl Pts',(-25.105308843592,14.4159981206257,129.385906944881)) ;
#119813 = CARTESIAN_POINT('Ctrl Pts',(-25.0324477821256,14.3283155320889,
129.13993894747)) ;
#119814 = CARTESIAN_POINT('Ctrl Pts',(-24.9700443034682,14.1755659228116,
128.924477813871)) ;
#119815 = CARTESIAN_POINT('Ctrl Pts',(-24.9235295808672,13.969906825541,128.75558920797)) ;
#119816 = CARTESIAN_POINT('Ctrl Pts',(-24.8965566575616,13.7239840128541,
128.643607017274)) ;
#119817 = CARTESIAN_POINT('Ctrl Pts',(-24.8920276788171,13.4571372933653,
128.597286645905)) ;
#119818 = CARTESIAN_POINT('Ctrl Pts',(-24.9112224977238,13.1860385186985,
128.620028296661)) ;
#119819 = CARTESIAN_POINT('Ctrl Pts',(-24.9527782276845,12.9351633427926,
128.708532779253)) ;
#119820 = CARTESIAN_POINT('Ctrl Pts',(-25.0155797279094,12.716280428453,128.858654488145)) ;
#119821 = CARTESIAN_POINT('Ctrl Pts',(-25.0942086463885,12.5504602967878,
129.055479919391)) ;
#119822 = CARTESIAN_POINT('Ctrl Pts',(-25.1860347004579,12.4451571780271,
129.290326810206)) ;
#119823 = CARTESIAN_POINT('Ctrl Pts',(-25.2825956957081,12.4110818136484,
129.539501707962)) ;
#119824 = CARTESIAN_POINT('Ctrl Pts',(-25.3801028054309,12.4493848627275,
129.791040070531)) ;
#119825 = CARTESIAN_POINT('Ctrl Pts',(-25.4700659725975,12.556427913144,130.020972058912)) ;
#119826 = CARTESIAN_POINT('Ctrl Pts',(-25.5490464109895,12.7270948717805,
130.218374590402)) ;
#119827 = CARTESIAN_POINT('Ctrl Pts',(-25.6103504725284,12.9467013402175,
130.364383698966)) ;
#119828 = CARTESIAN_POINT('Ctrl Pts',(-25.651076334731,13.2005745563337,130.450229029158)) ;
#119829 = CARTESIAN_POINT('Ctrl Pts',(-25.6688592932256,13.4697556094875,
130.46913314477)) ;
#119830 = CARTESIAN_POINT('Ctrl Pts',(-25.6633326860655,13.7362552359381,
130.419869278086)) ;
#119831 = CARTESIAN_POINT('Ctrl Pts',(-25.6351871184438,13.9814041933257,
130.30435482619)) ;
#119832 = CARTESIAN_POINT('Ctrl Pts',(-25.5879229073729,14.1841666830384,
130.133366568428)) ;
#119833 = CARTESIAN_POINT('Ctrl Pts',(-25.5247850978363,14.3343211929266,
129.91570247358)) ;
#119834 = CARTESIAN_POINT('Ctrl Pts',(-25.4515062569338,14.4184551111194,
129.668497896698)) ;
#119835 = CARTESIAN_POINT('Ctrl Pts',(-25.3741735889697,14.4314519975607,
129.409526512277)) ;
#119836 = CARTESIAN_POINT('Ctrl Pts',(-25.2986654507318,14.3721435273992,
129.155794819144)) ;
#119837 = CARTESIAN_POINT('Ctrl Pts',(-25.2314887860347,14.2453738509882,
128.926509843084)) ;
#119838 = CARTESIAN_POINT('Ctrl Pts',(-25.177612160251,14.0581566958374,128.735807740753)) ;
#119839 = CARTESIAN_POINT('Ctrl Pts',(-25.1425261531772,13.8276968106527,
128.600371370732)) ;
#119840 = CARTESIAN_POINT('Ctrl Pts',(-25.1286129151028,13.5670203755234,
128.526578335593)) ;
#119841 = CARTESIAN_POINT('Ctrl Pts',(-25.1381253558712,13.2953786744785,
128.521147180712)) ;
#119842 = CARTESIAN_POINT('Ctrl Pts',(-25.1707614727794,13.0342214950179,
128.58344292195)) ;
#119843 = CARTESIAN_POINT('Ctrl Pts',(-25.2255179487015,12.7992352777049,
128.710098750454)) ;
#119844 = CARTESIAN_POINT('Ctrl Pts',(-25.2979655542483,12.6113833120471,
128.888843585747)) ;
#119845 = CARTESIAN_POINT('Ctrl Pts',(-25.3850206418746,12.4798503942449,
129.109960878586)) ;
#119846 = CARTESIAN_POINT('Ctrl Pts',(-25.4803776423451,12.416397864002,129.355428944409)) ;
#119847 = CARTESIAN_POINT('Ctrl Pts',(-25.5783843703953,12.4249214929509,
129.608549524434)) ;
#119848 = CARTESIAN_POINT('Ctrl Pts',(-25.672478530963,12.5053755952326,129.850242670599)) ;
#119849 = CARTESIAN_POINT('Ctrl Pts',(-25.756226931752,12.6507859052006,130.061889235013)) ;
#119850 = CARTESIAN_POINT('Ctrl Pts',(-25.8251533352949,12.8517470992337,
130.230128068929)) ;
#119851 = CARTESIAN_POINT('Ctrl Pts',(-25.8747980900926,13.0945614507412,
130.341931437405)) ;
#119852 = CARTESIAN_POINT('Ctrl Pts',(-25.9020710193289,13.3602126376938,
130.388483679895)) ;
#119853 = CARTESIAN_POINT('Ctrl Pts',(-25.9058670751018,13.6310671963869,
130.366361615972)) ;
#119854 = CARTESIAN_POINT('Ctrl Pts',(-25.8867754919466,13.8852753848623,
130.277607898819)) ;
#119855 = CARTESIAN_POINT('Ctrl Pts',(-25.846806345492,14.1076160740045,130.127719600837)) ;
#119856 = CARTESIAN_POINT('Ctrl Pts',(-25.7894563509561,14.2808806662079,
129.927039264704)) ;
#119857 = CARTESIAN_POINT('Ctrl Pts',(-25.7197630440978,14.3926567103846,
129.690353283305)) ;
#119858 = CARTESIAN_POINT('Ctrl Pts',(-25.6429800311209,14.4348969491125,
129.432802823452)) ;
#119859 = CARTESIAN_POINT('Ctrl Pts',(-25.5664052890858,14.4049966950683,
129.176188720963)) ;
#119860 = CARTESIAN_POINT('Ctrl Pts',(-25.4945634031681,14.3037928875116,
128.932948137202)) ;
#119861 = CARTESIAN_POINT('Ctrl Pts',(-25.435091766399,14.1405203865162,128.726223307007)) ;
#119862 = CARTESIAN_POINT('Ctrl Pts',(-25.3919011396787,13.9258191062473,
128.566958681327)) ;
#119863 = CARTESIAN_POINT('Ctrl Pts',(-25.3690363816211,13.6747404924344,
128.467031877332)) ;
#119864 = CARTESIAN_POINT('Ctrl Pts',(-25.3690010643952,13.4052256695436,
128.433742776243)) ;
#119865 = CARTESIAN_POINT('Ctrl Pts',(-25.3922616413952,13.1384692475265,
128.468700955033)) ;
#119866 = CARTESIAN_POINT('Ctrl Pts',(-25.4384366048813,12.8897551535746,
128.570278947386)) ;
#119867 = CARTESIAN_POINT('Ctrl Pts',(-25.5041846804616,12.6813707953234,
128.729325865057)) ;
#119868 = CARTESIAN_POINT('Ctrl Pts',(-25.585982476974,12.5252896402636,128.935167552922)) ;
#119869 = CARTESIAN_POINT('Ctrl Pts',(-25.6787370032368,12.4335762079788,
129.172983990663)) ;
#119870 = CARTESIAN_POINT('Ctrl Pts',(-25.7761856628954,12.4126069664436,
129.424592020829)) ;
#119871 = CARTESIAN_POINT('Ctrl Pts',(-25.8729618386419,12.4645413764585,
129.673998882875)) ;
#119872 = CARTESIAN_POINT('Ctrl Pts',(-25.9613851744278,12.5845282668637,
129.899302334015)) ;
#119873 = CARTESIAN_POINT('Ctrl Pts',(-26.0371581474449,12.7652451064021,
130.087456352873)) ;
#119874 = CARTESIAN_POINT('Ctrl Pts',(-26.0947547148825,12.9922347341953,
130.222671327764)) ;
#119875 = CARTESIAN_POINT('Ctrl Pts',(-26.1312796240102,13.2501818574091,
130.296287346821)) ;
#119876 = CARTESIAN_POINT('Ctrl Pts',(-26.1447384833071,13.5208713010695,
130.302481379232)) ;
#119877 = CARTESIAN_POINT('Ctrl Pts',(-26.1347422066459,13.7852948748941,
130.240058557626)) ;
#119878 = CARTESIAN_POINT('Ctrl Pts',(-26.1028034649425,14.0230293879869,
130.113628542378)) ;
#119879 = CARTESIAN_POINT('Ctrl Pts',(-26.0519060113355,14.2178154382897,
129.931791193316)) ;
#119880 = CARTESIAN_POINT('Ctrl Pts',(-25.9867514193326,14.3552930540828,
129.708440395722)) ;
#119881 = CARTESIAN_POINT('Ctrl Pts',(-25.9119954035665,14.4265292549101,
129.456819725079)) ;
#119882 = CARTESIAN_POINT('Ctrl Pts',(-25.834829513542,14.425752226316,129.198453425837)) ;
#119883 = CARTESIAN_POINT('Ctrl Pts',(-25.7602440523618,14.3531911968223,
128.947353700595)) ;
#119884 = CARTESIAN_POINT('Ctrl Pts',(-25.6951616209711,14.2139749127786,
128.724118518912)) ;
#119885 = CARTESIAN_POINT('Ctrl Pts',(-25.6446900925232,14.0181343155111,
128.543547684947)) ;
#119886 = CARTESIAN_POINT('Ctrl Pts',(-25.6132229947609,13.7796845152241,
128.418501547274)) ;
#119887 = CARTESIAN_POINT('Ctrl Pts',(-25.6037330848021,13.5155236059082,
128.357635520124)) ;
#119888 = CARTESIAN_POINT('Ctrl Pts',(-25.617628730475,13.245212667821,128.365140772047)) ;
#119889 = CARTESIAN_POINT('Ctrl Pts',(-25.6545017751569,12.987705840382,128.439790008711)) ;
#119890 = CARTESIAN_POINT('Ctrl Pts',(-25.7129219295576,12.7602060641004,
128.577198728452)) ;
#119891 = CARTESIAN_POINT('Ctrl Pts',(-25.7885884356989,12.5817512683668,
128.765242790756)) ;
#119892 = CARTESIAN_POINT('Ctrl Pts',(-25.877553695151,12.4625557490256,128.991997656452)) ;
#119893 = CARTESIAN_POINT('Ctrl Pts',(-25.9741233376341,12.4124303716615,
129.240908418124)) ;
#119894 = CARTESIAN_POINT('Ctrl Pts',(-26.0714881147419,12.4345388124725,
129.49229097036)) ;
#119895 = CARTESIAN_POINT('Ctrl Pts',(-26.164529411831,12.5283216508309,129.730772431684)) ;
#119896 = CARTESIAN_POINT('Ctrl Pts',(-26.2456332053162,12.6848122418478,
129.934762024602)) ;
#119897 = CARTESIAN_POINT('Ctrl Pts',(-26.3113716154821,12.8954782936503,
130.093573957543)) ;
#119898 = CARTESIAN_POINT('Ctrl Pts',(-26.3567423635182,13.1430312218348,
130.193051677295)) ;
#119899 = CARTESIAN_POINT('Ctrl Pts',(-26.3796682101619,13.4109716011332,
130.22690034591)) ;
#119900 = CARTESIAN_POINT('Ctrl Pts',(-26.379180399323,13.6794256976715,130.192408300591)) ;
#119901 = CARTESIAN_POINT('Ctrl Pts',(-26.355735708432,13.9314101100325,130.090586754578)) ;
#119902 = CARTESIAN_POINT('Ctrl Pts',(-26.3122326343032,14.1445006487741,
129.930508199489)) ;
#119903 = CARTESIAN_POINT('Ctrl Pts',(-26.2523309894027,14.3067536437968,
129.722457733583)) ;
#119904 = CARTESIAN_POINT('Ctrl Pts',(-26.180794884382,14.406048704081,129.480333016166)) ;
#119905 = CARTESIAN_POINT('Ctrl Pts',(-26.103660979524,14.4348548847552,129.221860931271)) ;
#119906 = CARTESIAN_POINT('Ctrl Pts',(-26.027136998052,14.3909041630567,128.965141568143)) ;
#119907 = CARTESIAN_POINT('Ctrl Pts',(-25.9578089641216,14.2783347408893,
128.729615948131)) ;
#119908 = CARTESIAN_POINT('Ctrl Pts',(-25.9005074043686,14.1031935326512,
128.528930992271)) ;
#119909 = CARTESIAN_POINT('Ctrl Pts',(-25.8609965381137,13.8800104531449,
128.380399450144)) ;
#119910 = CARTESIAN_POINT('Ctrl Pts',(-25.8423806954271,13.6249527431351,
128.29299369777)) ;
#119911 = CARTESIAN_POINT('Ctrl Pts',(-25.8466982567422,13.3547990106838,
128.272493370141)) ;
#119912 = CARTESIAN_POINT('Ctrl Pts',(-25.8743205831141,13.0897726871477,
128.320116058481)) ;
#119913 = CARTESIAN_POINT('Ctrl Pts',(-25.9246264611834,12.8467549358408,
128.433719030383)) ;
#119914 = CARTESIAN_POINT('Ctrl Pts',(-25.9935112856203,12.6478124194814,
128.602020346365)) ;
#119915 = CARTESIAN_POINT('Ctrl Pts',(-26.0779380529408,12.5027972017395,
128.815470225642)) ;
#119916 = CARTESIAN_POINT('Ctrl Pts',(-26.171965786403,12.4240443631204,129.057051810318)) ;
#119917 = CARTESIAN_POINT('Ctrl Pts',(-26.2702731079583,12.4170503620235,
129.310949808494)) ;
#119918 = CARTESIAN_POINT('Ctrl Pts',(-26.3650966714635,12.4817913910706,
129.555002001196)) ;
#119919 = CARTESIAN_POINT('Ctrl Pts',(-26.45196366406,12.6142900720352,129.775575257278)) ;
#119920 = CARTESIAN_POINT('Ctrl Pts',(-26.5243727321012,12.8042103797361,
129.95405025432)) ;
#119921 = CARTESIAN_POINT('Ctrl Pts',(-26.578483057693,13.0388186679886,130.078979362122)) ;
#119922 = CARTESIAN_POINT('Ctrl Pts',(-26.6108288981163,13.3023285356057,
130.140176565052)) ;
#119923 = CARTESIAN_POINT('Ctrl Pts',(-26.6197222679655,13.5713414244093,
130.13326049002)) ;
#119924 = CARTESIAN_POINT('Ctrl Pts',(-26.6054350404599,13.8329962624196,
130.05821374072)) ;
#119925 = CARTESIAN_POINT('Ctrl Pts',(-26.5696096637515,14.0635776732595,
129.920451931681)) ;
#119926 = CARTESIAN_POINT('Ctrl Pts',(-26.5158545454307,14.2479537129057,
129.730399291059)) ;
#119927 = CARTESIAN_POINT('Ctrl Pts',(-26.4484523870756,14.3739504524616,
129.500417543721)) ;
#119928 = CARTESIAN_POINT('Ctrl Pts',(-26.3725118085867,14.4320428202114,
129.245284462382)) ;
#119929 = CARTESIAN_POINT('Ctrl Pts',(-26.2950856667936,14.4172275028747,
128.985988129081)) ;
#119930 = CARTESIAN_POINT('Ctrl Pts',(-26.2222776936055,14.3318166981341,
128.740288747817)) ;
#119931 = CARTESIAN_POINT('Ctrl Pts',(-26.1595230999705,14.1811818293068,
128.52384486406)) ;
#119932 = CARTESIAN_POINT('Ctrl Pts',(-26.1123210485869,13.9759967622757,
128.352808501451)) ;
#119933 = CARTESIAN_POINT('Ctrl Pts',(-26.084770830645,13.7313492386451,128.239201365232)) ;
#119934 = CARTESIAN_POINT('Ctrl Pts',(-26.0797136555551,13.4634561102099,
128.191161323004)) ;
#119935 = CARTESIAN_POINT('Ctrl Pts',(-26.0978801533651,13.195884935421,128.211372693161)) ;
#119936 = CARTESIAN_POINT('Ctrl Pts',(-26.1392146081528,12.9412337002998,
128.298829939633)) ;
#119937 = CARTESIAN_POINT('Ctrl Pts',(-26.2009044712201,12.7230235152343,
128.4460160171)) ;
#119938 = CARTESIAN_POINT('Ctrl Pts',(-26.2798277046628,12.5539648154296,
128.643380639081)) ;
#119939 = CARTESIAN_POINT('Ctrl Pts',(-26.3704183582616,12.4477725877379,
128.874981924817)) ;
#119940 = CARTESIAN_POINT('Ctrl Pts',(-26.4675932472334,12.4110238126212,
129.125691828151)) ;
#119941 = CARTESIAN_POINT('Ctrl Pts',(-26.56471080497,12.4468710250015,129.376273587607)) ;
#119942 = CARTESIAN_POINT('Ctrl Pts',(-26.6558840954224,12.553155401547,129.609384734652)) ;
#119943 = CARTESIAN_POINT('Ctrl Pts',(-26.7346205058782,12.7211113699614,
129.806339257464)) ;
#119944 = CARTESIAN_POINT('Ctrl Pts',(-26.7966910177754,12.9400020395614,
129.954485352245)) ;
#119945 = CARTESIAN_POINT('Ctrl Pts',(-26.8378916621286,13.1921120762229,
130.041855669963)) ;
#119946 = CARTESIAN_POINT('Ctrl Pts',(-26.8565040574598,13.4620045651565,
130.063068042932)) ;
#119947 = CARTESIAN_POINT('Ctrl Pts',(-26.8515337300207,13.7292706567068,
130.015371921608)) ;
#119948 = CARTESIAN_POINT('Ctrl Pts',(-26.8242404610039,13.9738126182776,
129.902564087945)) ;
#119949 = CARTESIAN_POINT('Ctrl Pts',(-26.7772359040396,14.1794947275424,
129.732112690396)) ;
#119950 = CARTESIAN_POINT('Ctrl Pts',(-26.7143307640667,14.3311259291818,
129.515097701107)) ;
#119951 = CARTESIAN_POINT('Ctrl Pts',(-26.6416882302053,14.4169205617397,
129.269939993438)) ;
#119952 = CARTESIAN_POINT('Ctrl Pts',(-26.5639471821135,14.4320030315974,
129.009577672861)) ;
#119953 = CARTESIAN_POINT('Ctrl Pts',(-26.4887082299279,14.3751243687379,
128.756828801049)) ;
#119954 = CARTESIAN_POINT('Ctrl Pts',(-26.4206397914384,14.2488768179311,
128.524628975738)) ;
#119955 = CARTESIAN_POINT('Ctrl Pts',(-26.3668727336172,14.0648018746923,
128.334575647107)) ;
#119956 = CARTESIAN_POINT('Ctrl Pts',(-26.3309363903451,13.8343788522074,
128.196474328605)) ;
#119957 = CARTESIAN_POINT('Ctrl Pts',(-26.3164705215498,13.5736071381831,
128.121002145167)) ;
#119958 = CARTESIAN_POINT('Ctrl Pts',(-26.3253756653385,13.3025525300613,
128.113863715032)) ;
#119959 = CARTESIAN_POINT('Ctrl Pts',(-26.3572716727716,13.0417945957582,
128.174109071432)) ;
#119960 = CARTESIAN_POINT('Ctrl Pts',(-26.4111773947375,12.8063140685278,
128.298382516279)) ;
#119961 = CARTESIAN_POINT('Ctrl Pts',(-26.4834589153869,12.6158856975737,
128.476480452916)) ;
#119962 = CARTESIAN_POINT('Ctrl Pts',(-26.570354800423,12.4825396970198,128.697083686748)) ;
#119963 = CARTESIAN_POINT('Ctrl Pts',(-26.6652801627027,12.4173081237828,
128.941385506295)) ;
#119964 = CARTESIAN_POINT('Ctrl Pts',(-26.7631989430957,12.423605000428,129.194283543105)) ;
#119965 = CARTESIAN_POINT('Ctrl Pts',(-26.8574619524539,12.5018025966581,
129.436489000106)) ;
#119966 = CARTESIAN_POINT('Ctrl Pts',(-26.9418546221037,12.6458565798938,
129.649912040933)) ;
#119967 = CARTESIAN_POINT('Ctrl Pts',(-27.0111976409268,12.8453790833706,
129.819389913643)) ;
#119968 = CARTESIAN_POINT('Ctrl Pts',(-27.061367894877,13.0865652662194,129.932812364929)) ;
#119969 = CARTESIAN_POINT('Ctrl Pts',(-27.089369420874,13.3521427577607,129.981445190974)) ;
#119970 = CARTESIAN_POINT('Ctrl Pts',(-27.0939017928513,13.6222557202932,
129.961586504907)) ;
#119971 = CARTESIAN_POINT('Ctrl Pts',(-27.0754482421394,13.8783882969557,
129.874548069754)) ;
#119972 = CARTESIAN_POINT('Ctrl Pts',(-27.0359007012441,14.1022120618795,
129.725831051564)) ;
#119973 = CARTESIAN_POINT('Ctrl Pts',(-26.9791357431868,14.2765229506337,
129.52695378676)) ;
#119974 = CARTESIAN_POINT('Ctrl Pts',(-26.909823932067,14.3902286964009,129.291416282315)) ;
#119975 = CARTESIAN_POINT('Ctrl Pts',(-26.8330387921819,14.4347769427253,
129.033812213985)) ;
#119976 = CARTESIAN_POINT('Ctrl Pts',(-26.7562449577674,14.4066722617846,
128.776487535096)) ;
#119977 = CARTESIAN_POINT('Ctrl Pts',(-26.6845764119764,14.3082119125381,
128.533963122741)) ;
#119978 = CARTESIAN_POINT('Ctrl Pts',(-26.6243671408649,14.1460357867196,
128.324921351722)) ;
#119979 = CARTESIAN_POINT('Ctrl Pts',(-26.5806797943847,13.9328084574968,
128.164244549597)) ;
#119980 = CARTESIAN_POINT('Ctrl Pts',(-26.5571663955051,13.681774125451,128.062322382885)) ;
#119981 = CARTESIAN_POINT('Ctrl Pts',(-26.5564073780867,13.414026239165,128.027111822149)) ;
#119982 = CARTESIAN_POINT('Ctrl Pts',(-26.5791491455037,13.1453688505525,
128.060346836654)) ;
#119983 = CARTESIAN_POINT('Ctrl Pts',(-26.6242809472691,12.8977836793382,
128.159158681216)) ;
#119984 = CARTESIAN_POINT('Ctrl Pts',(-26.6899845415361,12.6861562687701,
128.317792644291)) ;
#119985 = CARTESIAN_POINT('Ctrl Pts',(-26.7712746549743,12.5289208649723,
128.522226758068)) ;
#119986 = CARTESIAN_POINT('Ctrl Pts',(-26.863894350046,12.4351549173609,128.759610343918)) ;
#119987 = CARTESIAN_POINT('Ctrl Pts',(-26.9610674145653,12.41223935111,129.010490108608)) ;
#119988 = CARTESIAN_POINT('Ctrl Pts',(-27.0579665728015,12.4619213802628,
129.260261295811)) ;
#119989 = CARTESIAN_POINT('Ctrl Pts',(-27.1468958938683,12.5803996576492,
129.486961095898)) ;
#119990 = CARTESIAN_POINT('Ctrl Pts',(-27.2229176963561,12.7591299029993,
129.675926443311)) ;
#119991 = CARTESIAN_POINT('Ctrl Pts',(-27.281148945456,12.9850687098392,129.81297179148)) ;
#119992 = CARTESIAN_POINT('Ctrl Pts',(-27.3183216390964,13.2423777054139,
129.888482171424)) ;
#119993 = CARTESIAN_POINT('Ctrl Pts',(-27.33245310508,13.5129449016412,129.896642523138)) ;
#119994 = CARTESIAN_POINT('Ctrl Pts',(-27.3231877835587,13.7774320597186,
129.836414647175)) ;
#119995 = CARTESIAN_POINT('Ctrl Pts',(-27.2917829639029,14.0166134042629,
129.711475383655)) ;
#119996 = CARTESIAN_POINT('Ctrl Pts',(-27.2416990232453,14.2120830530507,
129.532186320855)) ;
#119997 = CARTESIAN_POINT('Ctrl Pts',(-27.1764440767512,14.352498916215,129.308296129156)) ;
#119998 = CARTESIAN_POINT('Ctrl Pts',(-27.1021012358692,14.4253825701344,
129.057999247625)) ;
#119999 = CARTESIAN_POINT('Ctrl Pts',(-27.0248123116318,14.426768294094,128.799213207415)) ;
#120000 = CARTESIAN_POINT('Ctrl Pts',(-26.950228893693,14.3564920185828,128.548208386946)) ;
#120001 = CARTESIAN_POINT('Ctrl Pts',(-26.8845614503941,14.2186719371757,
128.323146626863)) ;
#120002 = CARTESIAN_POINT('Ctrl Pts',(-26.8336555426971,14.024316786925,128.141329983919)) ;
#120003 = CARTESIAN_POINT('Ctrl Pts',(-26.801597940401,13.7866136068205,128.01452758408)) ;
#120004 = CARTESIAN_POINT('Ctrl Pts',(-26.7914773675253,13.5238037033397,
127.951929029032)) ;
#120005 = CARTESIAN_POINT('Ctrl Pts',(-26.8046611115732,13.2527086042196,
127.957271158598)) ;
#120006 = CARTESIAN_POINT('Ctrl Pts',(-26.8411453165669,12.9936530632693,
128.030652771087)) ;
#120007 = CARTESIAN_POINT('Ctrl Pts',(-26.8987574318875,12.7662441874236,
128.165867096014)) ;
#120008 = CARTESIAN_POINT('Ctrl Pts',(-26.9740830180008,12.5858801409006,
128.352858112991)) ;
#120009 = CARTESIAN_POINT('Ctrl Pts',(-27.0628251755867,12.4648530718858,
128.578942893323)) ;
#120010 = CARTESIAN_POINT('Ctrl Pts',(-27.1594231609068,12.4128201875619,
128.827887210328)) ;
#120011 = CARTESIAN_POINT('Ctrl Pts',(-27.2564574363076,12.4330274107103,
129.078429229244)) ;
#120012 = CARTESIAN_POINT('Ctrl Pts',(-27.3493201635517,12.524012324909,129.316551012229)) ;
#120013 = CARTESIAN_POINT('Ctrl Pts',(-27.4313416689702,12.6795221282536,
129.523026324944)) ;
#120014 = CARTESIAN_POINT('Ctrl Pts',(-27.4975379318319,12.8889214141028,
129.683186921422)) ;
#120015 = CARTESIAN_POINT('Ctrl Pts',(-27.5435488308571,13.1354947089828,
129.784545867269)) ;
#120016 = CARTESIAN_POINT('Ctrl Pts',(-27.5671767452064,13.4042911436029,
129.82030507381)) ;
#120017 = CARTESIAN_POINT('Ctrl Pts',(-27.5672643845209,13.6719452313923,
129.787618405761)) ;
#120018 = CARTESIAN_POINT('Ctrl Pts',(-27.5445552780615,13.9242175336792,
129.688018851963)) ;
#120019 = CARTESIAN_POINT('Ctrl Pts',(-27.5015315379868,14.1390288741834,
129.529280677435)) ;
#120020 = CARTESIAN_POINT('Ctrl Pts',(-27.4419857500411,14.3030286144717,
129.322247793777)) ;
#120021 = CARTESIAN_POINT('Ctrl Pts',(-27.3706593624215,14.4041953326341,
129.080722338789)) ;
#120022 = CARTESIAN_POINT('Ctrl Pts',(-27.2938390424101,14.4349854779899,
128.823267047109)) ;
#120023 = CARTESIAN_POINT('Ctrl Pts',(-27.2171925956617,14.3934046886661,
128.566192203389)) ;
#120024 = CARTESIAN_POINT('Ctrl Pts',(-27.147345149048,14.2822103121525,128.329025749962)) ;
#120025 = CARTESIAN_POINT('Ctrl Pts',(-27.0899564874658,14.1097942363152,
128.128293079995)) ;
#120026 = CARTESIAN_POINT('Ctrl Pts',(-27.0497024032013,13.8877667094565,
127.977541901105)) ;
#120027 = CARTESIAN_POINT('Ctrl Pts',(-27.0303723935246,13.6324084420419,
127.88792266215)) ;
#120028 = CARTESIAN_POINT('Ctrl Pts',(-27.0340283149476,13.3624185504467,
127.865495007072)) ;
#120029 = CARTESIAN_POINT('Ctrl Pts',(-27.0610999882633,13.0965814778885,
127.911450823542)) ;
#120030 = CARTESIAN_POINT('Ctrl Pts',(-27.1104911197653,12.8540736174815,
128.022582139951)) ;
#120031 = CARTESIAN_POINT('Ctrl Pts',(-27.1789274866825,12.652992435015,128.189498753939)) ;
#120032 = CARTESIAN_POINT('Ctrl Pts',(-27.263499859652,12.5055874303856,128.403191515036)) ;
#120033 = CARTESIAN_POINT('Ctrl Pts',(-27.3569065509663,12.4255318647486,
128.643116064752)) ;
#120034 = CARTESIAN_POINT('Ctrl Pts',(-27.4547438900964,12.4160627512278,
128.895790668738)) ;
#120035 = CARTESIAN_POINT('Ctrl Pts',(-27.5502080114701,12.4788299066414,
129.141554051022)) ;
#120036 = CARTESIAN_POINT('Ctrl Pts',(-27.6374637904928,12.6096602766835,
129.363239415158)) ;
#120037 = CARTESIAN_POINT('Ctrl Pts',(-27.710474888215,12.7985462130252,129.543405360105)) ;
#120038 = CARTESIAN_POINT('Ctrl Pts',(-27.7649671434383,13.031708612879,129.669522362687)) ;
#120039 = CARTESIAN_POINT('Ctrl Pts',(-27.7979073063491,13.293083578928,129.732646606245)) ;
#120040 = CARTESIAN_POINT('Ctrl Pts',(-27.8076097011333,13.5641924680593,
129.727839251528)) ;
#120041 = CARTESIAN_POINT('Ctrl Pts',(-27.7939119342835,13.8256806601297,
129.6546004207)) ;
#120042 = CARTESIAN_POINT('Ctrl Pts',(-27.7588915640264,14.0565823152587,
129.519317960093)) ;
#120043 = CARTESIAN_POINT('Ctrl Pts',(-27.7054698422737,14.2434411149003,
129.330116948414)) ;
#120044 = CARTESIAN_POINT('Ctrl Pts',(-27.6380806543802,14.3714533613372,
129.100046951507)) ;
#120045 = CARTESIAN_POINT('Ctrl Pts',(-27.5629246445623,14.4311593709141,
128.847484461924)) ;
#120046 = CARTESIAN_POINT('Ctrl Pts',(-27.4852723112633,14.4188767370812,
128.587442802152)) ;
#120047 = CARTESIAN_POINT('Ctrl Pts',(-27.4120884349404,14.3353893813971,
128.340584539541)) ;
#120048 = CARTESIAN_POINT('Ctrl Pts',(-27.3487944677133,14.1858866209329,
128.122457267565)) ;
#120049 = CARTESIAN_POINT('Ctrl Pts',(-27.3012779883249,13.9829323143578,
127.950645883144)) ;
#120050 = CARTESIAN_POINT('Ctrl Pts',(-27.2730500223035,13.7386001915966,
127.834971228421)) ;
#120051 = CARTESIAN_POINT('Ctrl Pts',(-27.2672861034049,13.472491070878,127.785043211583)) ;
#120052 = CARTESIAN_POINT('Ctrl Pts',(-27.284851176658,13.2027754622607,127.803255891318)) ;
#120053 = CARTESIAN_POINT('Ctrl Pts',(-27.3256506936343,12.9475729445581,
127.889163192759)) ;
#120054 = CARTESIAN_POINT('Ctrl Pts',(-27.3866924004005,12.7286906854066,
128.034522298347)) ;
#120055 = CARTESIAN_POINT('Ctrl Pts',(-27.4649756495311,12.5582194228626,
128.230093788475)) ;
#120056 = CARTESIAN_POINT('Ctrl Pts',(-27.5557878968131,12.4495814745878,
128.462164406796)) ;
#120057 = CARTESIAN_POINT('Ctrl Pts',(-27.6526736826316,12.4111325030014,
128.712104171976)) ;
#120058 = CARTESIAN_POINT('Ctrl Pts',(-27.7496521545279,12.4448573230465,
128.962350011997)) ;
#120059 = CARTESIAN_POINT('Ctrl Pts',(-27.8408738308629,12.5485736269638,
129.19570165313)) ;
#120060 = CARTESIAN_POINT('Ctrl Pts',(-27.9205751184065,12.7160675409956,
129.39524107991)) ;
#120061 = CARTESIAN_POINT('Ctrl Pts',(-27.9828423779555,12.9327061634172,
129.544132215434)) ;
#120062 = CARTESIAN_POINT('Ctrl Pts',(-28.0248443453271,13.1846668378338,
129.633751795151)) ;
#120063 = CARTESIAN_POINT('Ctrl Pts',(-28.0440759127581,13.4544224505961,
129.656768706986)) ;
#120064 = CARTESIAN_POINT('Ctrl Pts',(-28.0398000022802,13.7215757277082,
129.611158867274)) ;
#120065 = CARTESIAN_POINT('Ctrl Pts',(-28.0130827312133,13.9674105771419,
129.499981050513)) ;
#120066 = CARTESIAN_POINT('Ctrl Pts',(-27.9666619118937,14.173959529566,129.331298499324)) ;
#120067 = CARTESIAN_POINT('Ctrl Pts',(-27.9043787727222,14.3272528917974,
129.116193991239)) ;
#120068 = CARTESIAN_POINT('Ctrl Pts',(-27.8314693794371,14.4155297933765,
128.870033469215)) ;
#120069 = CARTESIAN_POINT('Ctrl Pts',(-27.7542546913223,14.4326688919931,
128.611425849187)) ;
#120070 = CARTESIAN_POINT('Ctrl Pts',(-27.6784027230996,14.3775210851954,
128.356670056856)) ;
#120071 = CARTESIAN_POINT('Ctrl Pts',(-27.6105108398773,14.2540409497735,
128.125232978784)) ;
#120072 = CARTESIAN_POINT('Ctrl Pts',(-27.5559663213141,14.0709648404294,
127.932757755026)) ;
#120073 = CARTESIAN_POINT('Ctrl Pts',(-27.5195045149598,13.8416199904244,
127.793133853687)) ;
#120074 = CARTESIAN_POINT('Ctrl Pts',(-27.504387097539,13.582388567831,127.715867343528)) ;
#120075 = CARTESIAN_POINT('Ctrl Pts',(-27.512461944946,13.3112804497714,127.706295015043)) ;
#120076 = CARTESIAN_POINT('Ctrl Pts',(-27.5439286608517,13.0483997987315,
127.765078691399)) ;
#120077 = CARTESIAN_POINT('Ctrl Pts',(-27.5970088742453,12.8130298392026,
127.887100914663)) ;
#120078 = CARTESIAN_POINT('Ctrl Pts',(-27.6690075490512,12.6204060823588,
128.064263470253)) ;
#120079 = CARTESIAN_POINT('Ctrl Pts',(-27.7555377826022,12.4854479324355,
128.283821873288)) ;
#120080 = CARTESIAN_POINT('Ctrl Pts',(-27.8503161312509,12.4181326730335,
128.527685295473)) ;
#120081 = CARTESIAN_POINT('Ctrl Pts',(-27.9485129845829,12.4224942487035,
128.781307773095)) ;
#120082 = CARTESIAN_POINT('Ctrl Pts',(-28.0428661775056,12.4989653084942,
129.023800058949)) ;
#120083 = CARTESIAN_POINT('Ctrl Pts',(-28.1272530074145,12.6405919477357,
129.237349753736)) ;
#120084 = CARTESIAN_POINT('Ctrl Pts',(-28.1973339593537,12.8391593414189,
129.408887782509)) ;
#120085 = CARTESIAN_POINT('Ctrl Pts',(-28.2481782006358,13.080245962358,129.524181066457)) ;
#120086 = CARTESIAN_POINT('Ctrl Pts',(-28.2766847337897,13.3449462168028,
129.57435157818)) ;
#120087 = CARTESIAN_POINT('Ctrl Pts',(-28.2818776537657,13.6142996681917,
129.556530060392)) ;
#120088 = CARTESIAN_POINT('Ctrl Pts',(-28.2641076414484,13.8710421169928,
129.471498550365)) ;
#120089 = CARTESIAN_POINT('Ctrl Pts',(-28.2251634394076,14.0962488257935,
129.324535823862)) ;
#120090 = CARTESIAN_POINT('Ctrl Pts',(-28.1684679190227,14.2729914081674,
129.125671381229)) ;
#120091 = CARTESIAN_POINT('Ctrl Pts',(-28.0997758612644,14.38767954712,128.892123160332)) ;
#120092 = CARTESIAN_POINT('Ctrl Pts',(-28.0232427382542,14.4346057861831,
128.63530633569)) ;
#120093 = CARTESIAN_POINT('Ctrl Pts',(-27.9459527748653,14.4082599468392,
128.376344855625)) ;
#120094 = CARTESIAN_POINT('Ctrl Pts',(-27.8744882234117,14.3122705880149,
128.13462021069)) ;
#120095 = CARTESIAN_POINT('Ctrl Pts',(-27.8135936127414,14.151436185241,127.923455054537)) ;
#120096 = CARTESIAN_POINT('Ctrl Pts',(-27.7693832548727,13.9387188784377,
127.761169573869)) ;
#120097 = CARTESIAN_POINT('Ctrl Pts',(-27.7453621747428,13.6904434125759,
127.658016736476)) ;
#120098 = CARTESIAN_POINT('Ctrl Pts',(-27.7439096559699,13.4208420598601,
127.620511771047)) ;
#120099 = CARTESIAN_POINT('Ctrl Pts',(-27.7659128645592,13.1534853902676,
127.651789024545)) ;
#120100 = CARTESIAN_POINT('Ctrl Pts',(-27.8104583821031,12.9044050288982,
127.748805634011)) ;
#120101 = CARTESIAN_POINT('Ctrl Pts',(-27.8757029644118,12.6913475994885,
127.906078375144)) ;
#120102 = CARTESIAN_POINT('Ctrl Pts',(-27.9566964837822,12.5324269019675,
128.109615216131)) ;
#120103 = CARTESIAN_POINT('Ctrl Pts',(-28.0487615859234,12.4369854947191,
128.345493668793)) ;
#120104 = CARTESIAN_POINT('Ctrl Pts',(-28.1460793490075,12.4119049760396,
128.596722852201)) ;
#120105 = CARTESIAN_POINT('Ctrl Pts',(-28.2427525510562,12.459288588066,128.845956716394)) ;
#120106 = CARTESIAN_POINT('Ctrl Pts',(-28.3320836999319,12.5757336822765,
129.073801113102)) ;
#120107 = CARTESIAN_POINT('Ctrl Pts',(-28.4086125469476,12.7527802879128,
129.264241908838)) ;
#120108 = CARTESIAN_POINT('Ctrl Pts',(-28.4677113029093,12.9786618268138,
129.403659288711)) ;
#120109 = CARTESIAN_POINT('Ctrl Pts',(-28.5054453845473,13.2359088344013,
129.480751482382)) ;
#120110 = CARTESIAN_POINT('Ctrl Pts',(-28.5201651176751,13.5051026285248,
129.490788903178)) ;
#120111 = CARTESIAN_POINT('Ctrl Pts',(-28.511478093157,13.7711208876962,129.43210680396)) ;
#120112 = CARTESIAN_POINT('Ctrl Pts',(-28.4807787726203,14.0100003599807,
129.309399633042)) ;
#120113 = CARTESIAN_POINT('Ctrl Pts',(-28.4311079427157,14.2073724408212,
129.131245480571)) ;
#120114 = CARTESIAN_POINT('Ctrl Pts',(-28.3663019439018,14.3492226306733,
128.908727993492)) ;
#120115 = CARTESIAN_POINT('Ctrl Pts',(-28.2922494089841,14.4242519881516,
128.659316158414)) ;
#120116 = CARTESIAN_POINT('Ctrl Pts',(-28.2146325752778,14.4277364563771,
128.399432279239)) ;
#120117 = CARTESIAN_POINT('Ctrl Pts',(-28.1399868460076,14.3592420110673,
128.148280493659)) ;
#120118 = CARTESIAN_POINT('Ctrl Pts',(-28.0742582761007,14.2240686922171,
127.923199970122)) ;
#120119 = CARTESIAN_POINT('Ctrl Pts',(-28.0226491504683,14.0305585465179,
127.739203779342)) ;
#120120 = CARTESIAN_POINT('Ctrl Pts',(-27.9900653350808,13.7945206228156,
127.610955419559)) ;
#120121 = CARTESIAN_POINT('Ctrl Pts',(-27.9792144938345,13.5313067865741,
127.546105203021)) ;
#120122 = CARTESIAN_POINT('Ctrl Pts',(-27.9917574792818,13.2605192088026,
127.549621813665)) ;
#120123 = CARTESIAN_POINT('Ctrl Pts',(-28.0274315736986,13.0015411116714,
127.620730641976)) ;
#120124 = CARTESIAN_POINT('Ctrl Pts',(-28.0844757419312,12.7725523899085,
127.754241521427)) ;
#120125 = CARTESIAN_POINT('Ctrl Pts',(-28.1595479835507,12.5901314079498,
127.940405447423)) ;
#120126 = CARTESIAN_POINT('Ctrl Pts',(-28.2479367999414,12.4675131368497,
128.165483243194)) ;
#120127 = CARTESIAN_POINT('Ctrl Pts',(-28.3439620446915,12.4133289133512,
128.412901195813)) ;
#120128 = CARTESIAN_POINT('Ctrl Pts',(-28.441732963266,12.4315113469885,128.665359909944)) ;
#120129 = CARTESIAN_POINT('Ctrl Pts',(-28.5345032017863,12.5204618731953,
128.903319666748)) ;
#120130 = CARTESIAN_POINT('Ctrl Pts',(-28.6169074040931,12.6740885600686,
129.110919783452)) ;
#120131 = CARTESIAN_POINT('Ctrl Pts',(-28.6836409940969,12.8820605633652,
129.272658091374)) ;
#120132 = CARTESIAN_POINT('Ctrl Pts',(-28.7303002545427,13.1280849033747,
129.375868286751)) ;
#120133 = CARTESIAN_POINT('Ctrl Pts',(-28.7545760746282,13.3954305468035,
129.413659236035)) ;
#120134 = CARTESIAN_POINT('Ctrl Pts',(-28.755360314267,13.6647721239679,129.38282410996)) ;
#120135 = CARTESIAN_POINT('Ctrl Pts',(-28.7333793249386,13.9166503672092,
129.285510438486)) ;
#120136 = CARTESIAN_POINT('Ctrl Pts',(-28.6908631010797,14.1333087824096,
129.128178523878)) ;
#120137 = CARTESIAN_POINT('Ctrl Pts',(-28.631815323096,14.2989356836214,128.92263834171)) ;
#120138 = CARTESIAN_POINT('Ctrl Pts',(-28.5603207260596,14.4025578145927,
128.680426107688)) ;
#120139 = CARTESIAN_POINT('Ctrl Pts',(-28.4838362884011,14.435010397795,128.424069767306)) ;
#120140 = CARTESIAN_POINT('Ctrl Pts',(-28.4071576842928,14.3956728080676,
128.166931596484)) ;
#120141 = CARTESIAN_POINT('Ctrl Pts',(-28.3370017645789,14.2862787578303,
127.928842877525)) ;
#120142 = CARTESIAN_POINT('Ctrl Pts',(-28.2792160505065,14.1158603541274,
127.726999055007)) ;
#120143 = CARTESIAN_POINT('Ctrl Pts',(-28.2382140420626,13.8934485383183,
127.573842062006)) ;
#120144 = CARTESIAN_POINT('Ctrl Pts',(-28.2184282359382,13.6404741399982,
127.483121945596)) ;
#120145 = CARTESIAN_POINT('Ctrl Pts',(-28.2214053844835,13.3695007340468,
127.458564725998)) ;
#120146 = CARTESIAN_POINT('Ctrl Pts',(-28.2477631811765,13.1044457267252,
127.502577894106)) ;
#120147 = CARTESIAN_POINT('Ctrl Pts',(-28.2964489975592,12.860704031683,127.611635359131)) ;
#120148 = CARTESIAN_POINT('Ctrl Pts',(-28.3649814444321,12.6571154777524,
127.778593699813)) ;
#120149 = CARTESIAN_POINT('Ctrl Pts',(-28.4481291111947,12.5098080554844,
127.988544765476)) ;
#120150 = CARTESIAN_POINT('Ctrl Pts',(-28.5418583608862,12.4266891530237,
128.229200937591)) ;
#120151 = CARTESIAN_POINT('Ctrl Pts',(-28.6399407697042,12.4154229755217,
128.482506199842)) ;
#120152 = CARTESIAN_POINT('Ctrl Pts',(-28.7352169858173,12.4759770673935,
128.727836179184)) ;
#120153 = CARTESIAN_POINT('Ctrl Pts',(-28.8228149902792,12.6048252394354,
128.950521636392)) ;
#120154 = CARTESIAN_POINT('Ctrl Pts',(-28.8963412616457,12.7921645634063,
129.132187511211)) ;
#120155 = CARTESIAN_POINT('Ctrl Pts',(-28.9515184485553,13.0247862212583,
129.260231591874)) ;
#120156 = CARTESIAN_POINT('Ctrl Pts',(-28.9850885525312,13.2853105369572,
129.32523875102)) ;
#120157 = CARTESIAN_POINT('Ctrl Pts',(-28.9954065225807,13.5574331010645,
129.322098562288)) ;
#120158 = CARTESIAN_POINT('Ctrl Pts',(-28.9825283726118,13.8171021403353,
129.25156605101)) ;
#120159 = CARTESIAN_POINT('Ctrl Pts',(-28.9478762234082,14.0511738702826,
129.117077385573)) ;
#120160 = CARTESIAN_POINT('Ctrl Pts',(-28.8949326798189,14.2388281925165,
128.929344352938)) ;
#120161 = CARTESIAN_POINT('Ctrl Pts',(-28.828125303218,14.3685839243643,128.701078224462)) ;
#120162 = CARTESIAN_POINT('Ctrl Pts',(-28.7525343917434,14.430551147229,128.446989494862)) ;
#120163 = CARTESIAN_POINT('Ctrl Pts',(-28.6754264311018,14.4203097396042,
128.188791679093)) ;
#120164 = CARTESIAN_POINT('Ctrl Pts',(-28.601689417703,14.3384208186475,127.940147389365)) ;
#120165 = CARTESIAN_POINT('Ctrl Pts',(-28.5383525180067,14.191573192343,127.722090576029)) ;
#120166 = CARTESIAN_POINT('Ctrl Pts',(-28.4899549480932,13.9880715249732,
127.54740004093)) ;
#120167 = CARTESIAN_POINT('Ctrl Pts',(-28.461455990991,13.74717256078,127.431293609618)) ;
#120168 = CARTESIAN_POINT('Ctrl Pts',(-28.4548916951247,13.4800206517718,
127.378832045014)) ;
#120169 = CARTESIAN_POINT('Ctrl Pts',(-28.4717642598864,13.2110030826081,
127.395134058574)) ;
#120170 = CARTESIAN_POINT('Ctrl Pts',(-28.5118855531922,12.9547749192264,
127.479026596824)) ;
#120171 = CARTESIAN_POINT('Ctrl Pts',(-28.5724326667241,12.7344342414435,
127.622910019624)) ;
#120172 = CARTESIAN_POINT('Ctrl Pts',(-28.650317058003,12.56234537382,127.817305812651)) ;
#120173 = CARTESIAN_POINT('Ctrl Pts',(-28.74066209986,12.4518692107331,128.048078349045)) ;
#120174 = CARTESIAN_POINT('Ctrl Pts',(-28.8377298890326,12.4112334908308,
128.298449197418)) ;
#120175 = CARTESIAN_POINT('Ctrl Pts',(-28.9346899869299,12.4427491476605,
128.548685461757)) ;
#120176 = CARTESIAN_POINT('Ctrl Pts',(-29.026695800843,12.5456206788136,128.784107137465)) ;
#120177 = CARTESIAN_POINT('Ctrl Pts',(-29.1057500300418,12.7091960260598,
128.982208076137)) ;
#120178 = CARTESIAN_POINT('Ctrl Pts',(-29.1691703048475,12.9259029784642,
129.134208867658)) ;
#120179 = CARTESIAN_POINT('Ctrl Pts',(-29.2117208860627,13.1770736213742,
129.225453280615)) ;
#120180 = CARTESIAN_POINT('Ctrl Pts',(-29.2316474006686,13.4468768316793,
129.250461675935)) ;
#120181 = CARTESIAN_POINT('Ctrl Pts',(-29.2280321901409,13.7138795758086,
129.206844028161)) ;
#120182 = CARTESIAN_POINT('Ctrl Pts',(-29.2019668400944,13.9605431797111,
129.097577657237)) ;
#120183 = CARTESIAN_POINT('Ctrl Pts',(-29.1560907287724,14.1686235448508,
128.93047945117)) ;
#120184 = CARTESIAN_POINT('Ctrl Pts',(-29.0938859718026,14.324111265305,128.715458048821)) ;
#120185 = CARTESIAN_POINT('Ctrl Pts',(-29.0216022718212,14.4138215777412,
128.47131600094)) ;
#120186 = CARTESIAN_POINT('Ctrl Pts',(-28.944139044341,14.4331945078177,128.211849645434)) ;
#120187 = CARTESIAN_POINT('Ctrl Pts',(-28.868380940979,14.3801614828431,127.957470568784)) ;
#120188 = CARTESIAN_POINT('Ctrl Pts',(-28.800081494987,14.2584942969663,127.724797795054)) ;
#120189 = CARTESIAN_POINT('Ctrl Pts',(-28.745111686049,14.0770491987957,127.53109904534)) ;
#120190 = CARTESIAN_POINT('Ctrl Pts',(-28.7080026400916,13.848487543227,127.389532493275)) ;
#120191 = CARTESIAN_POINT('Ctrl Pts',(-28.6922955186714,13.5893550911286,
127.310487333215)) ;
#120192 = CARTESIAN_POINT('Ctrl Pts',(-28.6996680149708,13.3196922711331,
127.299032447349)) ;
#120193 = CARTESIAN_POINT('Ctrl Pts',(-28.7303957431008,13.0561134153821,
127.355639856244)) ;
#120194 = CARTESIAN_POINT('Ctrl Pts',(-28.783028433985,12.8190741584449,127.476267047352)) ;
#120195 = CARTESIAN_POINT('Ctrl Pts',(-28.8545049403867,12.6252976289265,
127.651936636573)) ;
#120196 = CARTESIAN_POINT('Ctrl Pts',(-28.9403481121036,12.4887797079064,
127.869606581264)) ;
#120197 = CARTESIAN_POINT('Ctrl Pts',(-29.0353127838495,12.4190606508798,
128.113884387687)) ;
#120198 = CARTESIAN_POINT('Ctrl Pts',(-29.1331482649175,12.4213023279721,
128.366577035473)) ;
#120199 = CARTESIAN_POINT('Ctrl Pts',(-29.2277424750904,12.4953372291496,
128.609768490982)) ;
#120200 = CARTESIAN_POINT('Ctrl Pts',(-29.3129071860777,12.6358732815743,
128.825428028507)) ;
#120201 = CARTESIAN_POINT('Ctrl Pts',(-29.3832462389174,12.8325869424309,
128.997810327091)) ;
#120202 = CARTESIAN_POINT('Ctrl Pts',(-29.4345967551139,13.0715962372375,
129.114709675196)) ;
#120203 = CARTESIAN_POINT('Ctrl Pts',(-29.4639745688401,13.3366928582969,
129.167311129979)) ;
#120204 = CARTESIAN_POINT('Ctrl Pts',(-29.4698439499065,13.6067853722367,
129.151391357745)) ;
#120205 = CARTESIAN_POINT('Ctrl Pts',(-29.4526874804027,13.8640946743987,
129.068158319223)) ;
#120206 = CARTESIAN_POINT('Ctrl Pts',(-29.4144385458815,14.0898397345162,
128.923322495705)) ;
#120207 = CARTESIAN_POINT('Ctrl Pts',(-29.3582660699698,14.268360163449,128.725993376795)) ;
#120208 = CARTESIAN_POINT('Ctrl Pts',(-29.2895954148743,14.3854877174078,
128.492376850714)) ;
#120209 = CARTESIAN_POINT('Ctrl Pts',(-29.2131004108755,14.4341894579408,
128.235640638085)) ;
#120210 = CARTESIAN_POINT('Ctrl Pts',(-29.1361690586815,14.4102459856392,
127.977913367037)) ;
#120211 = CARTESIAN_POINT('Ctrl Pts',(-29.0640642794503,14.3157190540823,
127.734130630897)) ;
#120212 = CARTESIAN_POINT('Ctrl Pts',(-29.0031320933351,14.1574302983803,
127.523047652384)) ;
#120213 = CARTESIAN_POINT('Ctrl Pts',(-28.9581862068265,13.9458829104796,
127.358546519961)) ;
#120214 = CARTESIAN_POINT('Ctrl Pts',(-28.9334884683389,13.6969896287775,
127.253241196933)) ;
#120215 = CARTESIAN_POINT('Ctrl Pts',(-28.9314300219935,13.429280378355,127.214164558102)) ;
#120216 = CARTESIAN_POINT('Ctrl Pts',(-28.9526326503617,13.1613091049485,
127.243072438753)) ;
#120217 = CARTESIAN_POINT('Ctrl Pts',(-28.997044137834,12.9096301880815,127.339433446245)) ;
#120218 = CARTESIAN_POINT('Ctrl Pts',(-29.0610782818279,12.6977069165648,
127.493539578836)) ;
#120219 = CARTESIAN_POINT('Ctrl Pts',(-29.1418943597176,12.5361591796786,
127.696427432701)) ;
#120220 = CARTESIAN_POINT('Ctrl Pts',(-29.2337136946606,12.4388403136538,
127.931597574254)) ;
#120221 = CARTESIAN_POINT('Ctrl Pts',(-29.3310681473004,12.4115721831835,
128.182896743448)) ;
#120222 = CARTESIAN_POINT('Ctrl Pts',(-29.4279117173817,12.457029412505,128.432608286614)) ;
#120223 = CARTESIAN_POINT('Ctrl Pts',(-29.5173477265947,12.5713337507617,
128.660826716096)) ;
#120224 = CARTESIAN_POINT('Ctrl Pts',(-29.5943927463647,12.7468028515201,
128.85275594632)) ;
#120225 = CARTESIAN_POINT('Ctrl Pts',(-29.6540334361348,12.9715572990884,
128.993752857509)) ;
#120226 = CARTESIAN_POINT('Ctrl Pts',(-29.6923944387496,13.2272671330663,
129.072781238289)) ;
#120227 = CARTESIAN_POINT('Ctrl Pts',(-29.7078462688087,13.498061880378,129.084740514306)) ;
#120228 = CARTESIAN_POINT('Ctrl Pts',(-29.6999381855932,13.762097452862,129.028647095151)) ;
#120229 = CARTESIAN_POINT('Ctrl Pts',(-29.6697605913369,14.0037249073099,
128.907237756829)) ;
#120230 = CARTESIAN_POINT('Ctrl Pts',(-29.6205659297938,14.2024000350369,
128.730490540037)) ;
#120231 = CARTESIAN_POINT('Ctrl Pts',(-29.5559329643647,14.3463072876563,
128.508387624656)) ;
#120232 = CARTESIAN_POINT('Ctrl Pts',(-29.4823645066708,14.4229407115658,
128.260528386984)) ;
#120233 = CARTESIAN_POINT('Ctrl Pts',(-29.4047568399833,14.428708721228,128.000665028461)) ;
#120234 = CARTESIAN_POINT('Ctrl Pts',(-29.3299052093241,14.3623691718519,
127.748905053254)) ;
#120235 = CARTESIAN_POINT('Ctrl Pts',(-29.2635733327006,14.2283779712588,
127.521922192701)) ;
#120236 = CARTESIAN_POINT('Ctrl Pts',(-29.2116294286318,14.036425640657,127.336998499882)) ;
#120237 = CARTESIAN_POINT('Ctrl Pts',(-29.1785287843388,13.8020944878478,
127.20733035862)) ;
#120238 = CARTESIAN_POINT('Ctrl Pts',(-29.1669905292766,13.539161382227,127.140439495721)) ;
#120239 = CARTESIAN_POINT('Ctrl Pts',(-29.178814380148,13.2686186839106,127.141894532802)) ;
#120240 = CARTESIAN_POINT('Ctrl Pts',(-29.2138972997033,13.008641923509,127.211221309632)) ;
#120241 = CARTESIAN_POINT('Ctrl Pts',(-29.2701600634812,12.7791080577395,
127.342548185939)) ;
#120242 = CARTESIAN_POINT('Ctrl Pts',(-29.3451121464908,12.594297732826,127.528205753968)) ;
#120243 = CARTESIAN_POINT('Ctrl Pts',(-29.4328863736172,12.4702970553751,
127.751610486133)) ;
#120244 = CARTESIAN_POINT('Ctrl Pts',(-29.5289609200398,12.4139049863059,
127.999100927029)) ;
#120245 = CARTESIAN_POINT('Ctrl Pts',(-29.6264420292929,12.4297924309748,
128.250830535367)) ;
#120246 = CARTESIAN_POINT('Ctrl Pts',(-29.7200486139469,12.5172147404821,
128.491019322346)) ;
#120247 = CARTESIAN_POINT('Ctrl Pts',(-29.8027908234805,12.6696685741938,
128.699585054602)) ;
#120248 = CARTESIAN_POINT('Ctrl Pts',(-29.86960716835,12.8748935986054,128.861784028226)) ;
#120249 = CARTESIAN_POINT('Ctrl Pts',(-29.9170704992435,13.1206629289391,
128.96724565317)) ;
#120250 = CARTESIAN_POINT('Ctrl Pts',(-29.9419865656854,13.3874986938653,
129.006931376291)) ;
#120251 = CARTESIAN_POINT('Ctrl Pts',(-29.9434479075333,13.6577700467963,
128.977987103776)) ;
#120252 = CARTESIAN_POINT('Ctrl Pts',(-29.9220034023051,13.9102263569756,
128.882245404659)) ;
#120253 = CARTESIAN_POINT('Ctrl Pts',(-29.8802551960757,14.1273421335156,
128.72730034782)) ;
#120254 = CARTESIAN_POINT('Ctrl Pts',(-29.8212425120714,14.2954362023137,
128.521660521602)) ;
#120255 = CARTESIAN_POINT('Ctrl Pts',(-29.7506442887973,14.4001990478318,
128.282366797653)) ;
#120256 = CARTESIAN_POINT('Ctrl Pts',(-29.6735305499138,14.4351706372086,
128.023853901931)) ;
#120257 = CARTESIAN_POINT('Ctrl Pts',(-29.5971911919457,14.3977719556556,
127.767894141714)) ;
#120258 = CARTESIAN_POINT('Ctrl Pts',(-29.5266046143525,14.2904204336126,
127.52849106087)) ;
#120259 = CARTESIAN_POINT('Ctrl Pts',(-29.4682437641198,14.1205426251184,
127.324825254044)) ;
#120260 = CARTESIAN_POINT('Ctrl Pts',(-29.4270858956956,13.9015880320261,
127.171546539802)) ;
#120261 = CARTESIAN_POINT('Ctrl Pts',(-29.4064486644553,13.6483197654843,
127.078182317743)) ;
#120262 = CARTESIAN_POINT('Ctrl Pts',(-29.4087637384098,13.3774460111694,
127.051688016783)) ;
#120263 = CARTESIAN_POINT('Ctrl Pts',(-29.4345154694378,13.1115164178379,
127.093866825116)) ;
#120264 = CARTESIAN_POINT('Ctrl Pts',(-29.4824944581263,12.8676277530858,
127.200952673646)) ;
#120265 = CARTESIAN_POINT('Ctrl Pts',(-29.550167305721,12.6630941709717,127.365518735153)) ;
#120266 = CARTESIAN_POINT('Ctrl Pts',(-29.6335215314997,12.5128296668561,
127.575832626601)) ;
#120267 = CARTESIAN_POINT('Ctrl Pts',(-29.7270496687932,12.4280522223888,
127.815913080995)) ;
#120268 = CARTESIAN_POINT('Ctrl Pts',(-29.8249308027257,12.4147676725694,
128.068684706927)) ;
#120269 = CARTESIAN_POINT('Ctrl Pts',(-29.9203761314657,12.4732052197203,
128.314506929665)) ;
#120270 = CARTESIAN_POINT('Ctrl Pts',(-30.0085723311821,12.6008830294735,
128.538819105028)) ;
#120271 = CARTESIAN_POINT('Ctrl Pts',(-30.0821509332757,12.7859100383565,
128.720804533574)) ;
#120272 = CARTESIAN_POINT('Ctrl Pts',(-30.1379378808088,13.0171549996097,
128.850651951648)) ;
#120273 = CARTESIAN_POINT('Ctrl Pts',(-30.1722068319512,13.277402414091,128.917662123442)) ;
#120274 = CARTESIAN_POINT('Ctrl Pts',(-30.1832432181997,13.549209197848,128.916661399848)) ;
#120275 = CARTESIAN_POINT('Ctrl Pts',(-30.170957178296,13.8101282641669,128.847760730607)) ;
#120276 = CARTESIAN_POINT('Ctrl Pts',(-30.1371083316874,14.0442616351561,
128.71578111202)) ;
#120277 = CARTESIAN_POINT('Ctrl Pts',(-30.0842285549006,14.234899690822,128.527971711439)) ;
#120278 = CARTESIAN_POINT('Ctrl Pts',(-30.0180483211186,14.3654882849947,
128.301716969827)) ;
#120279 = CARTESIAN_POINT('Ctrl Pts',(-29.9428222189424,14.4297229165876,
128.048768110306)) ;
#120280 = CARTESIAN_POINT('Ctrl Pts',(-29.8654274323927,14.4216680213317,
127.789621318339)) ;
#120281 = CARTESIAN_POINT('Ctrl Pts',(-29.7914651714803,14.3417421219821,
127.540312299338)) ;
#120282 = CARTESIAN_POINT('Ctrl Pts',(-29.7277501313066,14.1964291634702,
127.321124596841)) ;
#120283 = CARTESIAN_POINT('Ctrl Pts',(-29.6790443731307,13.9955519017587,
127.14571179308)) ;
#120284 = CARTESIAN_POINT('Ctrl Pts',(-29.6497008058792,13.7541464807844,
127.026926907722)) ;
#120285 = CARTESIAN_POINT('Ctrl Pts',(-29.6425598616829,13.4873870948836,
126.972790757272)) ;
#120286 = CARTESIAN_POINT('Ctrl Pts',(-29.6587539231936,13.2187119173844,
126.987166006195)) ;
#120287 = CARTESIAN_POINT('Ctrl Pts',(-29.6980947341361,12.9622340564561,
127.068847518659)) ;
#120288 = CARTESIAN_POINT('Ctrl Pts',(-29.7583490440813,12.7396655137431,
127.211726679847)) ;
#120289 = CARTESIAN_POINT('Ctrl Pts',(-29.8358320612097,12.5663130240366,
127.404966419517)) ;
#120290 = CARTESIAN_POINT('Ctrl Pts',(-29.9255031103164,12.4542929808878,
127.63390856035)) ;
#120291 = CARTESIAN_POINT('Ctrl Pts',(-30.0227989228316,12.4113060989113,
127.884830805057)) ;
#120292 = CARTESIAN_POINT('Ctrl Pts',(-30.1196650413285,12.4409729751149,
128.134843722716)) ;
#120293 = CARTESIAN_POINT('Ctrl Pts',(-30.2114579250078,12.5408195806537,
128.369838112703)) ;
#120294 = CARTESIAN_POINT('Ctrl Pts',(-30.2918439177153,12.7045177195062,
128.571453811166)) ;
#120295 = CARTESIAN_POINT('Ctrl Pts',(-30.3554107241379,12.9194126835292,
128.72401886233)) ;
#120296 = CARTESIAN_POINT('Ctrl Pts',(-30.3985397348488,13.1689179450109,
128.817052685138)) ;
#120297 = CARTESIAN_POINT('Ctrl Pts',(-30.4192259543522,13.4397285799231,
128.844127725907)) ;
#120298 = CARTESIAN_POINT('Ctrl Pts',(-30.4162235857149,13.706427055275,128.802376016593)) ;
#120299 = CARTESIAN_POINT('Ctrl Pts',(-30.390798293272,13.953886295735,128.694986871854)) ;
#120300 = CARTESIAN_POINT('Ctrl Pts',(-30.3454805345728,14.1631927592464,
128.529541646648)) ;
#120301 = CARTESIAN_POINT('Ctrl Pts',(-30.2836235435482,14.3205261176051,
128.315510393234)) ;
#120302 = CARTESIAN_POINT('Ctrl Pts',(-30.2116675009614,14.4121066452954,
128.072370546642)) ;
#120303 = CARTESIAN_POINT('Ctrl Pts',(-30.1341996677374,14.4337042741575,
127.812865461492)) ;
#120304 = CARTESIAN_POINT('Ctrl Pts',(-30.0582302123766,14.3826278175705,
127.557833074158)) ;
#120305 = CARTESIAN_POINT('Ctrl Pts',(-29.9896723229114,14.2628852550259,
127.324425469218)) ;
#120306 = CARTESIAN_POINT('Ctrl Pts',(-29.934234898034,14.08292617671,127.129348096737)) ;
#120307 = CARTESIAN_POINT('Ctrl Pts',(-29.8965848388362,13.8556922014923,
126.986230563461)) ;
#120308 = CARTESIAN_POINT('Ctrl Pts',(-29.8802335079759,13.597259905774,126.905308621401)) ;
#120309 = CARTESIAN_POINT('Ctrl Pts',(-29.8868422446893,13.3277679144463,
126.891640117567)) ;
#120310 = CARTESIAN_POINT('Ctrl Pts',(-29.9172565235401,13.0618109735796,
126.947077950778)) ;
#120311 = CARTESIAN_POINT('Ctrl Pts',(-29.9688720822212,12.826038953014,127.065042300501)) ;
#120312 = CARTESIAN_POINT('Ctrl Pts',(-30.040080879908,12.6298696524396,127.239794218177)) ;
#120313 = CARTESIAN_POINT('Ctrl Pts',(-30.1255602392865,12.4917687507878,
127.456424992923)) ;
#120314 = CARTESIAN_POINT('Ctrl Pts',(-30.2204632585728,12.4199839299598,
127.700481429544)) ;
#120315 = CARTESIAN_POINT('Ctrl Pts',(-30.3182500980047,12.4203084245316,
127.95305004317)) ;
#120316 = CARTESIAN_POINT('Ctrl Pts',(-30.4128724280061,12.4922084684858,
128.196377152701)) ;
#120317 = CARTESIAN_POINT('Ctrl Pts',(-30.49843532704,12.6309969485081,128.41318204901)) ;
#120318 = CARTESIAN_POINT('Ctrl Pts',(-30.5692955798566,12.8263311670906,
128.587075933282)) ;
#120319 = CARTESIAN_POINT('Ctrl Pts',(-30.6213552229333,13.0651228622206,
128.70594980504)) ;
#120320 = CARTESIAN_POINT('Ctrl Pts',(-30.6512588718474,13.3295668395412,
128.760119376466)) ;
#120321 = CARTESIAN_POINT('Ctrl Pts',(-30.6577918154966,13.5989124476963,
128.74624101031)) ;
#120322 = CARTESIAN_POINT('Ctrl Pts',(-30.6412326417354,13.8574711293399,
128.664673013124)) ;
#120323 = CARTESIAN_POINT('Ctrl Pts',(-30.6036128903169,14.0837079504238,
128.521760497902)) ;
#120324 = CARTESIAN_POINT('Ctrl Pts',(-30.5479910114117,14.2638192247761,
128.326070390643)) ;
#120325 = CARTESIAN_POINT('Ctrl Pts',(-30.4793810094137,14.3831695883009,
128.092520856271)) ;
#120326 = CARTESIAN_POINT('Ctrl Pts',(-30.4032580708324,14.4337176696405,
127.836981571003)) ;
#120327 = CARTESIAN_POINT('Ctrl Pts',(-30.3262283514109,14.4120588650256,
127.578950633389)) ;
#120328 = CARTESIAN_POINT('Ctrl Pts',(-30.2538014263296,14.3193772960994,
127.33418534272)) ;
#120329 = CARTESIAN_POINT('Ctrl Pts',(-30.1924345633591,14.162817091715,127.121826574969)) ;
#120330 = CARTESIAN_POINT('Ctrl Pts',(-30.1468826625933,13.9515916217657,
126.955425970421)) ;
#120331 = CARTESIAN_POINT('Ctrl Pts',(-30.1217285110034,13.7055233203187,
126.849053547207)) ;
#120332 = CARTESIAN_POINT('Ctrl Pts',(-30.1189617700997,13.4359481909895,
126.80763240538)) ;
#120333 = CARTESIAN_POINT('Ctrl Pts',(-30.1394921596568,13.1690262543573,
126.834739626026)) ;
#120334 = CARTESIAN_POINT('Ctrl Pts',(-30.1832810972736,12.9162728223831,
126.929246732316)) ;
#120335 = CARTESIAN_POINT('Ctrl Pts',(-30.2466242328709,12.7036779666449,
127.081423572812)) ;
#120336 = CARTESIAN_POINT('Ctrl Pts',(-30.3268550662309,12.5403117621087,
127.282643376759)) ;
#120337 = CARTESIAN_POINT('Ctrl Pts',(-30.4190439813045,12.4404489575973,
127.518673248112)) ;
#120338 = CARTESIAN_POINT('Ctrl Pts',(-30.515866544653,12.4114485633587,127.768579554242)) ;
#120339 = CARTESIAN_POINT('Ctrl Pts',(-30.6127673682806,12.4544846403687,
128.018478798306)) ;
#120340 = CARTESIAN_POINT('Ctrl Pts',(-30.7028603542064,12.5672617699685,
128.248489335384)) ;
#120341 = CARTESIAN_POINT('Ctrl Pts',(-30.7803844158743,12.7417744927464,
128.441755685078)) ;
#120342 = CARTESIAN_POINT('Ctrl Pts',(-30.8401391858009,12.9633750836739,
128.583364940552)) ;
#120343 = CARTESIAN_POINT('Ctrl Pts',(-30.8795034723959,13.2203111794704,
128.665063657192)) ;
#120344 = CARTESIAN_POINT('Ctrl Pts',(-30.8955070246914,13.4905143785451,
128.678700860762)) ;
#120345 = CARTESIAN_POINT('Ctrl Pts',(-30.8882329130397,13.7550216610133,
128.624443878034)) ;
#120346 = CARTESIAN_POINT('Ctrl Pts',(-30.8587969553298,13.996749630301,128.505328670453)) ;
#120347 = CARTESIAN_POINT('Ctrl Pts',(-30.8099826456517,14.1974242710986,
128.32959702307)) ;
#120348 = CARTESIAN_POINT('Ctrl Pts',(-30.746033869509,14.342514003419,128.109651994141)) ;
#120349 = CARTESIAN_POINT('Ctrl Pts',(-30.6724714145086,14.4218015954934,
127.861707426972)) ;
#120350 = CARTESIAN_POINT('Ctrl Pts',(-30.5944934945582,14.4294553492896,
127.600600448985)) ;
#120351 = CARTESIAN_POINT('Ctrl Pts',(-30.5198525735962,14.3652618267525,
127.349613410191)) ;
#120352 = CARTESIAN_POINT('Ctrl Pts',(-30.4532723078222,14.2335996642439,
127.121966229449)) ;
#120353 = CARTESIAN_POINT('Ctrl Pts',(-30.400742576325,14.0430658671341,126.93529354313)) ;
#120354 = CARTESIAN_POINT('Ctrl Pts',(-30.3669424476525,13.8093138339715,
126.803511541699)) ;
#120355 = CARTESIAN_POINT('Ctrl Pts',(-30.354795918861,13.5459139250659,126.734726092536)) ;
#120356 = CARTESIAN_POINT('Ctrl Pts',(-30.3659155625559,13.2769103570782,
126.734315819249)) ;
#120357 = CARTESIAN_POINT('Ctrl Pts',(-30.4002899633489,13.0160046226691,
126.801538967899)) ;
#120358 = CARTESIAN_POINT('Ctrl Pts',(-30.4561214089056,12.7850161242088,
126.931542490534)) ;
#120359 = CARTESIAN_POINT('Ctrl Pts',(-30.5303244371711,12.5991696001074,
127.115126201843)) ;
#120360 = CARTESIAN_POINT('Ctrl Pts',(-30.6182424052493,12.4727066695535,
127.338777065082)) ;
#120361 = CARTESIAN_POINT('Ctrl Pts',(-30.7137149498342,12.4146340063818,
127.584672937593)) ;
#120362 = CARTESIAN_POINT('Ctrl Pts',(-30.8114490602173,12.428272476576,127.837066661156)) ;
#120363 = CARTESIAN_POINT('Ctrl Pts',(-30.9051543854586,12.5136822248399,
128.077582546125)) ;
#120364 = CARTESIAN_POINT('Ctrl Pts',(-30.9882709083332,12.6640313971838,
128.287268615616)) ;
#120365 = CARTESIAN_POINT('Ctrl Pts',(-31.0559950168127,12.8694014453016,
128.451897209542)) ;
#120366 = CARTESIAN_POINT('Ctrl Pts',(-31.1037081705792,13.1128473541502,
128.558297704285)) ;
#120367 = CARTESIAN_POINT('Ctrl Pts',(-31.1293772881811,13.3794713860966,
128.600156033917)) ;
#120368 = CARTESIAN_POINT('Ctrl Pts',(-31.1315196171046,13.6493875676937,
128.573268454256)) ;
#120369 = CARTESIAN_POINT('Ctrl Pts',(-31.1108449632028,13.9027716863457,
128.479778740659)) ;
#120370 = CARTESIAN_POINT('Ctrl Pts',(-31.0692426036565,14.1226003969304,
128.325000641813)) ;
#120371 = CARTESIAN_POINT('Ctrl Pts',(-31.0112252737707,14.2907614924808,
128.122596061958)) ;
#120372 = CARTESIAN_POINT('Ctrl Pts',(-30.9402723144273,14.3985142703266,
127.881958087952)) ;
#120373 = CARTESIAN_POINT('Ctrl Pts',(-30.8637496257416,14.4350393250072,
127.625400924029)) ;
#120374 = CARTESIAN_POINT('Ctrl Pts',(-30.7871752359977,14.4000355933247,
127.368694626451)) ;
#120375 = CARTESIAN_POINT('Ctrl Pts',(-30.7160918334904,14.294019258596,127.127722701532)) ;
#120376 = CARTESIAN_POINT('Ctrl Pts',(-30.6575855213183,14.1264036808229,
126.923771105405)) ;
#120377 = CARTESIAN_POINT('Ctrl Pts',(-30.6157646948906,13.9087136081249,
126.768534501323)) ;
#120378 = CARTESIAN_POINT('Ctrl Pts',(-30.5944734643708,13.6545233409047,
126.673056840974)) ;
#120379 = CARTESIAN_POINT('Ctrl Pts',(-30.5961584778505,13.3858501132774,
126.644972706391)) ;
#120380 = CARTESIAN_POINT('Ctrl Pts',(-30.6212061225492,13.1190055325829,
126.685027414806)) ;
#120381 = CARTESIAN_POINT('Ctrl Pts',(-30.6686641032527,12.8738785417747,
126.790545968904)) ;
#120382 = CARTESIAN_POINT('Ctrl Pts',(-30.7360322995194,12.6676053740016,
126.954141574344)) ;
#120383 = CARTESIAN_POINT('Ctrl Pts',(-30.8189572758642,12.5160771056389,
127.163246420767)) ;
#120384 = CARTESIAN_POINT('Ctrl Pts',(-30.9118318570724,12.4297444721253,
127.40156977474)) ;
#120385 = CARTESIAN_POINT('Ctrl Pts',(-31.0095674663916,12.4139325819383,
127.653954416377)) ;
#120386 = CARTESIAN_POINT('Ctrl Pts',(-31.1057144053207,12.4708186398046,
127.901626272861)) ;
#120387 = CARTESIAN_POINT('Ctrl Pts',(-31.1934774018543,12.5954481483175,
128.124964799178)) ;
#120388 = CARTESIAN_POINT('Ctrl Pts',(-31.2680184404151,12.7795463119932,
128.309584536972)) ;
#120389 = CARTESIAN_POINT('Ctrl Pts',(-31.3245129839954,13.0105018776207,
128.441401948698)) ;
#120390 = CARTESIAN_POINT('Ctrl Pts',(-31.359387232688,13.270465957133,128.510149434695)) ;
#120391 = CARTESIAN_POINT('Ctrl Pts',(-31.3710208627504,13.5415025070648,
128.510982049493)) ;
#120392 = CARTESIAN_POINT('Ctrl Pts',(-31.3594362504754,13.8030870082756,
128.444123195626)) ;
#120393 = CARTESIAN_POINT('Ctrl Pts',(-31.3259082937146,14.0389747692379,
128.312940546262)) ;
#120394 = CARTESIAN_POINT('Ctrl Pts',(-31.274151313902,14.2290324339817,128.128800353418)) ;
#120395 = CARTESIAN_POINT('Ctrl Pts',(-31.2077956141783,14.36290013857,127.901741927386)) ;
#120396 = CARTESIAN_POINT('Ctrl Pts',(-31.1328753029658,14.4288302738408,
127.649767710556)) ;
#120397 = CARTESIAN_POINT('Ctrl Pts',(-31.0553096740806,14.4228365201876,
127.390047882109)) ;
#120398 = CARTESIAN_POINT('Ctrl Pts',(-30.9814127467324,14.3452102352826,
127.141053050896)) ;
#120399 = CARTESIAN_POINT('Ctrl Pts',(-30.9171598071708,14.2014203196955,
126.9202098087)) ;
#120400 = CARTESIAN_POINT('Ctrl Pts',(-30.8680211029908,14.0021641937243,
126.743575143318)) ;
#120401 = CARTESIAN_POINT('Ctrl Pts',(-30.8380540025779,13.761753127779,126.622966733671)) ;
#120402 = CARTESIAN_POINT('Ctrl Pts',(-30.8302076181397,13.4956080237515,
126.566793461782)) ;
#120403 = CARTESIAN_POINT('Ctrl Pts',(-30.8457646914712,13.2262845852455,
126.57924205912)) ;
#120404 = CARTESIAN_POINT('Ctrl Pts',(-30.8843106921691,12.9698876950621,
126.658709006147)) ;
#120405 = CARTESIAN_POINT('Ctrl Pts',(-30.944061629397,12.7457364087332,126.80006264788)) ;
#120406 = CARTESIAN_POINT('Ctrl Pts',(-31.0209111245848,12.5708017503329,
126.991514652388)) ;
#120407 = CARTESIAN_POINT('Ctrl Pts',(-31.1111509504485,12.4561497112336,
127.22181232647)) ;
#120408 = CARTESIAN_POINT('Ctrl Pts',(-31.2072870600816,12.4116404870858,
127.469715093214)) ;
#120409 = CARTESIAN_POINT('Ctrl Pts',(-31.3050010050222,12.4391729336107,
127.721936631105)) ;
#120410 = CARTESIAN_POINT('Ctrl Pts',(-31.3967596844395,12.5371797633224,
127.956923250406)) ;
#120411 = CARTESIAN_POINT('Ctrl Pts',(-31.4773182773982,12.6985743471033,
128.159141476881)) ;
#120412 = CARTESIAN_POINT('Ctrl Pts',(-31.5414906076439,12.9117741360547,
128.313504581612)) ;
#120413 = CARTESIAN_POINT('Ctrl Pts',(-31.585503955842,13.1624013152274,128.408873091849)) ;
#120414 = CARTESIAN_POINT('Ctrl Pts',(-31.6066735180883,13.4305279145417,
128.437664751368)) ;
#120415 = CARTESIAN_POINT('Ctrl Pts',(-31.6044537914995,13.6988963516455,
128.398030332128)) ;
#120416 = CARTESIAN_POINT('Ctrl Pts',(-31.5796185454552,13.9472005386101,
128.292368550419)) ;
#120417 = CARTESIAN_POINT('Ctrl Pts',(-31.5347333532356,14.1580510630495,
128.128132874519)) ;
#120418 = CARTESIAN_POINT('Ctrl Pts',(-31.4735536013256,14.3165352363587,
127.916224911136)) ;
#120419 = CARTESIAN_POINT('Ctrl Pts',(-31.4014686925056,14.4105996668628,
127.672535798014)) ;
#120420 = CARTESIAN_POINT('Ctrl Pts',(-31.3242683799976,14.4340684651961,
127.413909039428)) ;
#120421 = CARTESIAN_POINT('Ctrl Pts',(-31.2480468687016,14.3850543896185,
127.158084753529)) ;
#120422 = CARTESIAN_POINT('Ctrl Pts',(-31.1792019153545,14.2669952300402,
126.923831913409)) ;
#120423 = CARTESIAN_POINT('Ctrl Pts',(-31.1234652774576,14.0891154364107,
126.727970581063)) ;
#120424 = CARTESIAN_POINT('Ctrl Pts',(-31.085171594464,13.8629228835357,126.582943522854)) ;
#120425 = CARTESIAN_POINT('Ctrl Pts',(-31.0681428284109,13.6044943724102,
126.499966250038)) ;
#120426 = CARTESIAN_POINT('Ctrl Pts',(-31.0741800776185,13.3352195562946,
126.484640586543)) ;
#120427 = CARTESIAN_POINT('Ctrl Pts',(-31.1036139777116,13.0705829535361,
126.537450591183)) ;
#120428 = CARTESIAN_POINT('Ctrl Pts',(-31.1549987786636,12.8316692334543,
126.654458606324)) ;
#120429 = CARTESIAN_POINT('Ctrl Pts',(-31.2258684738244,12.6342706260099,
126.828204708944)) ;
#120430 = CARTESIAN_POINT('Ctrl Pts',(-31.3106811987395,12.4949548036794,
127.043012440284)) ;
#120431 = CARTESIAN_POINT('Ctrl Pts',(-31.4054161489351,12.4210676160077,
127.286570115342)) ;
#120432 = CARTESIAN_POINT('Ctrl Pts',(-31.5030764584432,12.4192534817676,
127.538810619031)) ;
#120433 = CARTESIAN_POINT('Ctrl Pts',(-31.5980505537662,12.4890551014873,
127.783113550799)) ;
#120434 = CARTESIAN_POINT('Ctrl Pts',(-31.6842775371184,12.626926545497,128.001711744956)) ;
#120435 = CARTESIAN_POINT('Ctrl Pts',(-31.7551540083784,12.8196495679067,
128.175864614223)) ;
#120436 = CARTESIAN_POINT('Ctrl Pts',(-31.8079983596213,13.0580836243581,
128.296926865552)) ;
#120437 = CARTESIAN_POINT('Ctrl Pts',(-31.8384823645199,13.3214662460235,
128.352872203092)) ;
#120438 = CARTESIAN_POINT('Ctrl Pts',(-31.8456998824593,13.5912987745739,
128.340936672021)) ;
#120439 = CARTESIAN_POINT('Ctrl Pts',(-31.8299019781677,13.8497219287496,
128.261704525461)) ;
#120440 = CARTESIAN_POINT('Ctrl Pts',(-31.7925300527276,14.0789422598233,
128.11924062528)) ;
#120441 = CARTESIAN_POINT('Ctrl Pts',(-31.7373879737978,14.2597601138698,
127.925041901496)) ;
#120442 = CARTESIAN_POINT('Ctrl Pts',(-31.6693257955755,14.3805241665643,
127.693206235717)) ;
#120443 = CARTESIAN_POINT('Ctrl Pts',(-31.5934353598195,14.4333051065353,
127.438389101722)) ;
#120444 = CARTESIAN_POINT('Ctrl Pts',(-31.5160410317782,14.4135763153339,
127.179153156744)) ;
#120445 = CARTESIAN_POINT('Ctrl Pts',(-31.4434927483479,14.3230159864486,
126.934094834657)) ;
#120446 = CARTESIAN_POINT('Ctrl Pts',(-31.3815287161961,14.1669880697449,
126.719814892297)) ;
#120447 = CARTESIAN_POINT('Ctrl Pts',(-31.3360156066866,13.9601855092309,
126.554001382575)) ;
#120448 = CARTESIAN_POINT('Ctrl Pts',(-31.3098762387133,13.7121979724763,
126.444349827821)) ;
#120449 = CARTESIAN_POINT('Ctrl Pts',(-31.3064487554567,13.4453254354835,
126.401311066117)) ;
#120450 = CARTESIAN_POINT('Ctrl Pts',(-31.3264783868601,13.1756579328103,
126.42663176511)) ;
#120451 = CARTESIAN_POINT('Ctrl Pts',(-31.3691412779122,12.9248371133689,
126.518224267297)) ;
#120452 = CARTESIAN_POINT('Ctrl Pts',(-31.4323907266609,12.7087904209721,
126.669825981253)) ;
#120453 = CARTESIAN_POINT('Ctrl Pts',(-31.5121877466573,12.5441839973877,
126.869821292532)) ;
#120454 = CARTESIAN_POINT('Ctrl Pts',(-31.6040854442531,12.4422953631874,
127.105006082566)) ;
#120455 = CARTESIAN_POINT('Ctrl Pts',(-31.7010448696948,12.4112745922159,
127.355243843531)) ;
#120456 = CARTESIAN_POINT('Ctrl Pts',(-31.7978537292344,12.4523611240387,
127.604936133107)) ;
#120457 = CARTESIAN_POINT('Ctrl Pts',(-31.8879929885489,12.5627156272335,
127.83517884223)) ;
#120458 = CARTESIAN_POINT('Ctrl Pts',(-31.9662453401921,12.7362032335438,
128.030450237031)) ;
#120459 = CARTESIAN_POINT('Ctrl Pts',(-32.0264300023649,12.9562237014372,
128.17338105447)) ;
#120460 = CARTESIAN_POINT('Ctrl Pts',(-32.0664723939883,13.2127632436766,
128.257017275162)) ;
#120461 = CARTESIAN_POINT('Ctrl Pts',(-32.0831275048794,13.4814739931662,
128.272723469395)) ;
#120462 = CARTESIAN_POINT('Ctrl Pts',(-32.0765932972906,13.7476020769462,
128.220483383446)) ;
#120463 = CARTESIAN_POINT('Ctrl Pts',(-32.0476302528579,13.9907502707064,
128.102674626184)) ;
#120464 = CARTESIAN_POINT('Ctrl Pts',(-31.9994402533025,14.1921268766281,
127.928863316725)) ;
#120465 = CARTESIAN_POINT('Ctrl Pts',(-31.9359462785863,14.3392030436754,
127.710268097422)) ;
#120466 = CARTESIAN_POINT('Ctrl Pts',(-31.8619745518175,14.4207500230976,
127.46086515257)) ;
#120467 = CARTESIAN_POINT('Ctrl Pts',(-31.7847447622153,14.4302362583739,
127.202259775102)) ;
#120468 = CARTESIAN_POINT('Ctrl Pts',(-31.7095328243019,14.368028270843,126.949427124129)) ;
#120469 = CARTESIAN_POINT('Ctrl Pts',(-31.6425445471401,14.2375543492764,
126.720522362865)) ;
#120470 = CARTESIAN_POINT('Ctrl Pts',(-31.5897144831715,14.0487159657188,
126.533039367418)) ;
#120471 = CARTESIAN_POINT('Ctrl Pts',(-31.5554726021897,13.8167883871292,
126.400078496056)) ;
#120472 = CARTESIAN_POINT('Ctrl Pts',(-31.542602309707,13.5548284865375,126.329281652584)) ;
#120473 = CARTESIAN_POINT('Ctrl Pts',(-31.5530287952121,13.2844750332118,
126.326684756249)) ;
#120474 = CARTESIAN_POINT('Ctrl Pts',(-31.5868796720123,13.0226683900031,
126.392329568486)) ;
#120475 = CARTESIAN_POINT('Ctrl Pts',(-31.6419899311371,12.7913019843532,
126.520320997934)) ;
#120476 = CARTESIAN_POINT('Ctrl Pts',(-31.7156175265643,12.6040507467942,
126.702258093667)) ;
#120477 = CARTESIAN_POINT('Ctrl Pts',(-31.8031361180212,12.4756113935465,
126.924761331817)) ;
#120478 = CARTESIAN_POINT('Ctrl Pts',(-31.8987627474538,12.415243488117,127.171001724304)) ;
#120479 = CARTESIAN_POINT('Ctrl Pts',(-31.9964597074322,12.4269403743014,
127.423308917717)) ;
#120480 = CARTESIAN_POINT('Ctrl Pts',(-32.0901558588354,12.5099953063745,
127.663881965089)) ;
#120481 = CARTESIAN_POINT('Ctrl Pts',(-32.173774748925,12.6587329054093,127.874987741951)) ;
#120482 = CARTESIAN_POINT('Ctrl Pts',(-32.2418392577068,12.8618952127667,
128.040723139875)) ;
#120483 = CARTESIAN_POINT('Ctrl Pts',(-32.2904576103093,13.1054069861002,
128.149619377544)) ;
#120484 = CARTESIAN_POINT('Ctrl Pts',(-32.316769944543,13.3721987049067,128.193296380107)) ;
#120485 = CARTESIAN_POINT('Ctrl Pts',(-32.3195569713661,13.6415134162569,
128.168386125265)) ;
#120486 = CARTESIAN_POINT('Ctrl Pts',(-32.299591267985,13.8954057310282,128.077001594138)) ;
#120487 = CARTESIAN_POINT('Ctrl Pts',(-32.2585195327027,14.1169004710299,
127.923725730513)) ;
#120488 = CARTESIAN_POINT('Ctrl Pts',(-32.2007685695086,14.2868623267828,
127.722030454418)) ;
#120489 = CARTESIAN_POINT('Ctrl Pts',(-32.1305348488786,14.396013035847,127.48369692176)) ;
#120490 = CARTESIAN_POINT('Ctrl Pts',(-32.0538050791662,14.4351149224746,
127.226396750023)) ;
#120491 = CARTESIAN_POINT('Ctrl Pts',(-31.9770328389355,14.4019052027925,
126.969061606347)) ;
#120492 = CARTESIAN_POINT('Ctrl Pts',(-31.9059255394677,14.2983009187854,
126.728137470122)) ;
#120493 = CARTESIAN_POINT('Ctrl Pts',(-31.846755925753,14.1317969224175,126.522124007505)) ;
#120494 = CARTESIAN_POINT('Ctrl Pts',(-31.8044925759672,13.91534337541,126.365618273777)) ;
#120495 = CARTESIAN_POINT('Ctrl Pts',(-31.7826277420114,13.6633971728162,
126.268647311183)) ;
#120496 = CARTESIAN_POINT('Ctrl Pts',(-31.7834890488768,13.3943409490525,
126.238079504293)) ;
#120497 = CARTESIAN_POINT('Ctrl Pts',(-31.8080379768348,13.125759500651,126.276504548515)) ;
#120498 = CARTESIAN_POINT('Ctrl Pts',(-31.8547791210711,12.8806964753524,
126.380044558236)) ;
#120499 = CARTESIAN_POINT('Ctrl Pts',(-31.921382813645,12.6734733763792,126.541494713359)) ;
#120500 = CARTESIAN_POINT('Ctrl Pts',(-32.0040660055355,12.5195858185458,
126.74981782748)) ;
#120501 = CARTESIAN_POINT('Ctrl Pts',(-32.0971934592114,12.4310932740595,
126.988720519411)) ;
#120502 = CARTESIAN_POINT('Ctrl Pts',(-32.1943755333981,12.4134132696985,
127.239663913926)) ;
#120503 = CARTESIAN_POINT('Ctrl Pts',(-32.2907844041067,12.4681188633571,
127.48805990421)) ;
#120504 = CARTESIAN_POINT('Ctrl Pts',(-32.3788634891402,12.5909169506631,
127.712321795157)) ;
#120505 = CARTESIAN_POINT('Ctrl Pts',(-32.4538505271568,12.7734489072163,
127.898246415507)) ;
#120506 = CARTESIAN_POINT('Ctrl Pts',(-32.5108712348923,13.0028154211787,
128.031660379154)) ;
#120507 = CARTESIAN_POINT('Ctrl Pts',(-32.5464604471638,13.2626812904981,
128.10242752577)) ;
#120508 = CARTESIAN_POINT('Ctrl Pts',(-32.5588102595845,13.5323091961428,
128.105524088133)) ;
#120509 = CARTESIAN_POINT('Ctrl Pts',(-32.5478500365599,13.7963543423531,
128.040243010073)) ;
#120510 = CARTESIAN_POINT('Ctrl Pts',(-32.5149810677505,14.0324258066149,
127.911102233703)) ;
#120511 = CARTESIAN_POINT('Ctrl Pts',(-32.4636380719142,14.2243211732623,
127.728111071488)) ;
#120512 = CARTESIAN_POINT('Ctrl Pts',(-32.3977993001216,14.3597396975641,
127.502651663795)) ;
#120513 = CARTESIAN_POINT('Ctrl Pts',(-32.3227959762273,14.4280132150894,
127.250317340372)) ;
#120514 = CARTESIAN_POINT('Ctrl Pts',(-32.2452616010669,14.4240026931505,
126.990711939345)) ;
#120515 = CARTESIAN_POINT('Ctrl Pts',(-32.1711211897067,14.348214877112,126.740974584197)) ;
#120516 = CARTESIAN_POINT('Ctrl Pts',(-32.1067221850188,14.2066839106137,
126.519814451723)) ;
#120517 = CARTESIAN_POINT('Ctrl Pts',(-32.0569081619447,14.0084844644838,
126.341123531766)) ;
#120518 = CARTESIAN_POINT('Ctrl Pts',(-32.0263232386117,13.76791632806,126.218578577679)) ;
#120519 = CARTESIAN_POINT('Ctrl Pts',(-32.0179116552026,13.5034893328133,
126.160920310859)) ;
#120520 = CARTESIAN_POINT('Ctrl Pts',(-32.0327954673164,13.2335994078643,
126.171345006653)) ;
#120521 = CARTESIAN_POINT('Ctrl Pts',(-32.0707657946749,12.976407627843,126.249111915004)) ;
#120522 = CARTESIAN_POINT('Ctrl Pts',(-32.1301041508424,12.7508792337382,
126.389211054592)) ;
#120523 = CARTESIAN_POINT('Ctrl Pts',(-32.2062732152592,12.5752390532541,
126.578800301858)) ;
#120524 = CARTESIAN_POINT('Ctrl Pts',(-32.2957312839852,12.4588914929926,
126.806976186385)) ;
#120525 = CARTESIAN_POINT('Ctrl Pts',(-32.392308620738,12.4118138328558,127.055972899133)) ;
#120526 = CARTESIAN_POINT('Ctrl Pts',(-32.4900557202676,12.4374481799832,
127.308301819784)) ;
#120527 = CARTESIAN_POINT('Ctrl Pts',(-32.5820384027822,12.5333386552095,
127.543956363044)) ;
#120528 = CARTESIAN_POINT('Ctrl Pts',(-32.6633130647022,12.6939674039094,
127.748117070613)) ;
#120529 = CARTESIAN_POINT('Ctrl Pts',(-32.7276564437716,12.9050031482846,
127.903137803992)) ;
#120530 = CARTESIAN_POINT('Ctrl Pts',(-32.7724018637935,13.1551455919413,
128.000592328387)) ;
#120531 = CARTESIAN_POINT('Ctrl Pts',(-32.7869026808253,13.3338157805737,
128.020913097943)) ;
#120532 = CARTESIAN_POINT('Ctrl Pts',(-32.7902884693506,13.4231220893089,
128.019783106832)) ;
#120533 = CARTESIAN_POINT('Ctrl Pts',(-11.4473705198918,13.1734341962953,
133.2453836742)) ;
#120534 = CARTESIAN_POINT('Ctrl Pts',(-11.4480740668009,13.1676985268958,
133.24670795141)) ;
#120535 = CARTESIAN_POINT('Ctrl Pts',(-11.4595477305337,13.076204201721,133.268542953682)) ;
#120536 = CARTESIAN_POINT('Ctrl Pts',(-11.4905248885226,12.9034784200084,
133.336060088381)) ;
#120537 = CARTESIAN_POINT('Ctrl Pts',(-11.5552006767944,12.6923997924798,
133.491971818923)) ;
#120538 = CARTESIAN_POINT('Ctrl Pts',(-11.6361658480941,12.5327609197045,
133.695385432581)) ;
#120539 = CARTESIAN_POINT('Ctrl Pts',(-11.7288235566871,12.4368205686394,
133.932788388924)) ;
#120540 = CARTESIAN_POINT('Ctrl Pts',(-11.8257634374896,12.4119420237697,
134.183044910058)) ;
#120541 = CARTESIAN_POINT('Ctrl Pts',(-11.9225895618528,12.4592681498074,
134.432672297289)) ;
#120542 = CARTESIAN_POINT('Ctrl Pts',(-12.0118665215859,12.575659036236,134.660380692383)) ;
#120543 = CARTESIAN_POINT('Ctrl Pts',(-12.0884448545199,12.75283542717,134.850941590915)) ;
#120544 = CARTESIAN_POINT('Ctrl Pts',(-12.1473740885929,12.9779971811105,
134.989965265017)) ;
#120545 = CARTESIAN_POINT('Ctrl Pts',(-12.1851940642893,13.2349354675193,
135.067332760891)) ;
#120546 = CARTESIAN_POINT('Ctrl Pts',(-12.2000107655077,13.5051819451432,
135.077525536086)) ;
#120547 = CARTESIAN_POINT('Ctrl Pts',(-12.1912876596684,13.7710457079463,
135.018753485588)) ;
#120548 = CARTESIAN_POINT('Ctrl Pts',(-12.1606973063918,14.0095406593372,
134.896429733358)) ;
#120549 = CARTESIAN_POINT('Ctrl Pts',(-12.11092513824,14.2073761046424,134.717903581334)) ;
#120550 = CARTESIAN_POINT('Ctrl Pts',(-12.0463035752806,14.3489569855306,
134.496013109962)) ;
#120551 = CARTESIAN_POINT('Ctrl Pts',(-11.9719809240434,14.4243647659385,
134.24568576646)) ;
#120552 = CARTESIAN_POINT('Ctrl Pts',(-11.8944197744956,14.427672591071,133.985990463909)) ;
#120553 = CARTESIAN_POINT('Ctrl Pts',(-11.819820484482,14.3592845353793,133.734997132989)) ;
#120554 = CARTESIAN_POINT('Ctrl Pts',(-11.7540479069007,14.2239082001409,
133.50975548736)) ;
#120555 = CARTESIAN_POINT('Ctrl Pts',(-11.7025290912445,14.0309430574059,
133.326104874534)) ;
#120556 = CARTESIAN_POINT('Ctrl Pts',(-11.6698185107926,13.7937231411456,
133.197324613256)) ;
#120557 = CARTESIAN_POINT('Ctrl Pts',(-11.6590728229283,13.5318368827659,
133.132954885592)) ;
#120558 = CARTESIAN_POINT('Ctrl Pts',(-11.6715146568046,13.260908758679,133.136158645477)) ;
#120559 = CARTESIAN_POINT('Ctrl Pts',(-11.7073390044507,13.0011530565724,
133.20760253653)) ;
#120560 = CARTESIAN_POINT('Ctrl Pts',(-11.7641809555439,12.7729626729889,
133.340640813236)) ;
#120561 = CARTESIAN_POINT('Ctrl Pts',(-11.8393511387376,12.5901801237826,
133.527033924571)) ;
#120562 = CARTESIAN_POINT('Ctrl Pts',(-11.9275728085287,12.4676467713314,
133.751683720386)) ;
#120563 = CARTESIAN_POINT('Ctrl Pts',(-12.0239720292633,12.413314501038,134.000062258223)) ;
#120564 = CARTESIAN_POINT('Ctrl Pts',(-12.121304733462,12.4313809059018,134.251393442111)) ;
#120565 = CARTESIAN_POINT('Ctrl Pts',(-12.2145517431487,12.5206603484656,
134.490579145694)) ;
#120566 = CARTESIAN_POINT('Ctrl Pts',(-12.2968075547073,12.6744196148216,
134.697779915769)) ;
#120567 = CARTESIAN_POINT('Ctrl Pts',(-12.3633737809412,12.8815893341258,
134.85913785182)) ;
#120568 = CARTESIAN_POINT('Ctrl Pts',(-12.4102625920414,13.1290193456038,
134.962833588597)) ;
#120569 = CARTESIAN_POINT('Ctrl Pts',(-12.4343449087572,13.3950772518204,
135.000224573441)) ;
#120570 = CARTESIAN_POINT('Ctrl Pts',(-12.4352286842141,13.6643422142601,
134.969691915908)) ;
#120571 = CARTESIAN_POINT('Ctrl Pts',(-12.4131525718201,13.9170737538833,
134.871985659673)) ;
#120572 = CARTESIAN_POINT('Ctrl Pts',(-12.3706607762256,14.1334228161875,
134.714767891984)) ;
#120573 = CARTESIAN_POINT('Ctrl Pts',(-12.3115699368204,14.2989215629879,
134.509090314935)) ;
#120574 = CARTESIAN_POINT('Ctrl Pts',(-12.2406260808501,14.4021434472197,
134.268728348906)) ;
#120575 = CARTESIAN_POINT('Ctrl Pts',(-12.1635096540278,14.4351203025954,
134.010245514987)) ;
#120576 = CARTESIAN_POINT('Ctrl Pts',(-12.0870609123607,14.3956460282901,
133.753876776433)) ;
#120577 = CARTESIAN_POINT('Ctrl Pts',(-12.0168112766492,14.2864256300776,
133.515489344327)) ;
#120578 = CARTESIAN_POINT('Ctrl Pts',(-11.9588806020232,14.1149875929984,
133.313083595978)) ;
#120579 = CARTESIAN_POINT('Ctrl Pts',(-11.9182630667946,13.8950778464839,
133.16141233224)) ;
#120580 = CARTESIAN_POINT('Ctrl Pts',(-11.8982136803435,13.6402948775312,
133.069662409729)) ;
#120581 = CARTESIAN_POINT('Ctrl Pts',(-11.9012091414679,13.3700134780419,
133.045253453647)) ;
#120582 = CARTESIAN_POINT('Ctrl Pts',(-11.9276282936563,13.1040820089462,
133.089332965067)) ;
#120583 = CARTESIAN_POINT('Ctrl Pts',(-11.9762490634299,12.8608603098162,
133.198268746333)) ;
#120584 = CARTESIAN_POINT('Ctrl Pts',(-12.0448000874776,12.6570994974887,
133.365259571756)) ;
#120585 = CARTESIAN_POINT('Ctrl Pts',(-12.1280040260076,12.509712563052,133.575356875517)) ;
#120586 = CARTESIAN_POINT('Ctrl Pts',(-12.2217907278284,12.4266925565407,
133.816162814867)) ;
#120587 = CARTESIAN_POINT('Ctrl Pts',(-12.3195845113326,12.4153566228605,
134.06872463408)) ;
#120588 = CARTESIAN_POINT('Ctrl Pts',(-12.4151906282434,12.476118398497,134.31490137872)) ;
#120589 = CARTESIAN_POINT('Ctrl Pts',(-12.5025015711756,12.6046110942521,
134.536856258684)) ;
#120590 = CARTESIAN_POINT('Ctrl Pts',(-12.5761392571973,12.7920330529179,
134.718809905303)) ;
#120591 = CARTESIAN_POINT('Ctrl Pts',(-12.6313190561571,13.024646117744,134.846865821606)) ;
#120592 = CARTESIAN_POINT('Ctrl Pts',(-12.6648510010149,13.2849677628749,
134.911782387054)) ;
#120593 = CARTESIAN_POINT('Ctrl Pts',(-12.6752768859988,13.5561840574451,
134.909074632877)) ;
#120594 = CARTESIAN_POINT('Ctrl Pts',(-12.6622542366794,13.8182131440166,
134.83781287569)) ;
#120595 = CARTESIAN_POINT('Ctrl Pts',(-12.6278120959063,14.0504675663447,
134.704189256873)) ;
#120596 = CARTESIAN_POINT('Ctrl Pts',(-12.5746767390659,14.2392689175362,
134.515730540059)) ;
#120597 = CARTESIAN_POINT('Ctrl Pts',(-12.5077212333364,14.3686949412613,
134.286997684432)) ;
#120598 = CARTESIAN_POINT('Ctrl Pts',(-12.4328327987394,14.4303698787607,
134.035262433741)) ;
#120599 = CARTESIAN_POINT('Ctrl Pts',(-12.3551681454901,14.4203874176643,
133.775196684826)) ;
#120600 = CARTESIAN_POINT('Ctrl Pts',(-12.281427216418,14.3383233721809,133.526543913651)) ;
#120601 = CARTESIAN_POINT('Ctrl Pts',(-12.2180346569397,14.1909246457993,
133.308253001474)) ;
#120602 = CARTESIAN_POINT('Ctrl Pts',(-12.1700271254954,13.9894771384923,
133.135018970481)) ;
#120603 = CARTESIAN_POINT('Ctrl Pts',(-12.1412312608287,13.7468082771736,
133.017778045599)) ;
#120604 = CARTESIAN_POINT('Ctrl Pts',(-12.1346803482234,13.4802542547444,
132.965444637786)) ;
#120605 = CARTESIAN_POINT('Ctrl Pts',(-12.1518060283826,13.2092850470841,
132.982231344216)) ;
#120606 = CARTESIAN_POINT('Ctrl Pts',(-12.1914284395064,12.9563426353649,
133.065098166761)) ;
#120607 = CARTESIAN_POINT('Ctrl Pts',(-12.2522891121189,12.7340442685521,
133.209644808083)) ;
#120608 = CARTESIAN_POINT('Ctrl Pts',(-12.3304078125076,12.5620254310283,
133.404672739898)) ;
#120609 = CARTESIAN_POINT('Ctrl Pts',(-12.4202116415783,12.4521634508898,
133.634056112492)) ;
#120610 = CARTESIAN_POINT('Ctrl Pts',(-12.517532818831,12.4110698291516,133.885078444257)) ;
#120611 = CARTESIAN_POINT('Ctrl Pts',(-12.6148078934914,12.4431134789288,
134.136118265331)) ;
#120612 = CARTESIAN_POINT('Ctrl Pts',(-12.7059248212752,12.544720780955,134.36927974363)) ;
#120613 = CARTESIAN_POINT('Ctrl Pts',(-12.7857599917973,12.709460812036,134.569364737784)) ;
#120614 = CARTESIAN_POINT('Ctrl Pts',(-12.8490190731694,12.9261933468861,
134.720931773752)) ;
#120615 = CARTESIAN_POINT('Ctrl Pts',(-12.8915191285647,13.1767718332297,
134.812096240414)) ;
#120616 = CARTESIAN_POINT('Ctrl Pts',(-12.9115116010101,13.4474343197197,
134.837194593127)) ;
#120617 = CARTESIAN_POINT('Ctrl Pts',(-12.9077976399136,13.7143157713228,
134.793294199843)) ;
#120618 = CARTESIAN_POINT('Ctrl Pts',(-12.8818813884825,13.960120914319,134.684592833268)) ;
#120619 = CARTESIAN_POINT('Ctrl Pts',(-12.8357313693075,14.1691500544874,
134.516518989096)) ;
#120620 = CARTESIAN_POINT('Ctrl Pts',(-12.7740689064731,14.3234013156229,
134.303370793792)) ;
#120621 = CARTESIAN_POINT('Ctrl Pts',(-12.7014220850373,14.4138714588237,
134.057977547517)) ;
#120622 = CARTESIAN_POINT('Ctrl Pts',(-12.6241886832898,14.4332950652812,
133.799291383501)) ;
#120623 = CARTESIAN_POINT('Ctrl Pts',(-12.5478867089577,14.37983766652,133.543078701379)) ;
#120624 = CARTESIAN_POINT('Ctrl Pts',(-12.4799675217152,14.2584887072528,
133.311683366343)) ;
#120625 = CARTESIAN_POINT('Ctrl Pts',(-12.4249393482279,14.0772214064872,
133.117809426492)) ;
#120626 = CARTESIAN_POINT('Ctrl Pts',(-12.3877664398662,13.8478579716949,
132.975955272484)) ;
#120627 = CARTESIAN_POINT('Ctrl Pts',(-12.3721402537263,13.5896598560144,
132.897269249345)) ;
#120628 = CARTESIAN_POINT('Ctrl Pts',(-12.3794806782538,13.3195388423839,
132.885663034153)) ;
#120629 = CARTESIAN_POINT('Ctrl Pts',(-12.4103064738394,13.0556169732422,
132.942510353194)) ;
#120630 = CARTESIAN_POINT('Ctrl Pts',(-12.4629013673467,12.8189342678657,
133.063069191677)) ;
#120631 = CARTESIAN_POINT('Ctrl Pts',(-12.5344122785446,12.625100278912,133.238826624894)) ;
#120632 = CARTESIAN_POINT('Ctrl Pts',(-12.6202525140682,12.4887479023081,
133.456496574608)) ;
#120633 = CARTESIAN_POINT('Ctrl Pts',(-12.7150155758981,12.4190670277806,
133.700254320957)) ;
#120634 = CARTESIAN_POINT('Ctrl Pts',(-12.8132064476839,12.4213699947317,
133.95386332912)) ;
#120635 = CARTESIAN_POINT('Ctrl Pts',(-12.9075620983682,12.4953802874648,
134.196438541246)) ;
#120636 = CARTESIAN_POINT('Ctrl Pts',(-12.9927902768386,12.6359572758876,
134.412260415263)) ;
#120637 = CARTESIAN_POINT('Ctrl Pts',(-13.0631709953693,12.8329198121217,
134.584736258615)) ;
#120638 = CARTESIAN_POINT('Ctrl Pts',(-13.1144613389104,13.0719650653609,
134.701464258526)) ;
#120639 = CARTESIAN_POINT('Ctrl Pts',(-13.143774727237,13.3363498058402,134.753966235205)) ;
#120640 = CARTESIAN_POINT('Ctrl Pts',(-13.1496791294893,13.6070577541681,
134.738072707591)) ;
#120641 = CARTESIAN_POINT('Ctrl Pts',(-13.1324713549101,13.8644612546569,
134.654675083653)) ;
#120642 = CARTESIAN_POINT('Ctrl Pts',(-13.0941894467002,14.0900773467752,
134.509746512484)) ;
#120643 = CARTESIAN_POINT('Ctrl Pts',(-13.0381529177921,14.2682172866369,
134.3128932133)) ;
#120644 = CARTESIAN_POINT('Ctrl Pts',(-12.9694164279505,14.38541662164,134.079049330582)) ;
#120645 = CARTESIAN_POINT('Ctrl Pts',(-12.8932702282235,14.4341663230829,
133.823482020016)) ;
#120646 = CARTESIAN_POINT('Ctrl Pts',(-12.8158362554554,14.4102121199937,
133.564068937527)) ;
#120647 = CARTESIAN_POINT('Ctrl Pts',(-12.7438549252204,14.3156228992233,
133.320698817844)) ;
#120648 = CARTESIAN_POINT('Ctrl Pts',(-12.6828642788531,14.1571117178342,
133.109403768484)) ;
#120649 = CARTESIAN_POINT('Ctrl Pts',(-12.6380503902695,13.9459763961177,
132.945365338171)) ;
#120650 = CARTESIAN_POINT('Ctrl Pts',(-12.6133436908675,13.697562228916,132.840086078986)) ;
#120651 = CARTESIAN_POINT('Ctrl Pts',(-12.6112238063931,13.4293975021098,
132.800773961391)) ;
#120652 = CARTESIAN_POINT('Ctrl Pts',(-12.6325249834962,13.1610019423395,
132.829911431496)) ;
#120653 = CARTESIAN_POINT('Ctrl Pts',(-12.6766496599303,12.9105848484096,
132.925613172297)) ;
#120654 = CARTESIAN_POINT('Ctrl Pts',(-12.7409122350092,12.6976134704073,
133.080239826003)) ;
#120655 = CARTESIAN_POINT('Ctrl Pts',(-12.8215669260211,12.536442279252,133.282728587217)) ;
#120656 = CARTESIAN_POINT('Ctrl Pts',(-12.9134891990553,12.4387732237497,
133.518152797446)) ;
#120657 = CARTESIAN_POINT('Ctrl Pts',(-13.0111243090133,12.4116342437955,
133.770178301096)) ;
#120658 = CARTESIAN_POINT('Ctrl Pts',(-13.1075737106094,12.4569142489461,
134.018874417128)) ;
#120659 = CARTESIAN_POINT('Ctrl Pts',(-13.1972943937453,12.5714752096904,
134.247823335506)) ;
#120660 = CARTESIAN_POINT('Ctrl Pts',(-13.2741873813664,12.7468633486005,
134.439353851752)) ;
#120661 = CARTESIAN_POINT('Ctrl Pts',(-13.3336915143071,12.9706873354731,
134.580068833733)) ;
#120662 = CARTESIAN_POINT('Ctrl Pts',(-13.3721999484215,13.2271705997234,
134.659418787554)) ;
#120663 = CARTESIAN_POINT('Ctrl Pts',(-13.3876917555698,13.4971330615505,
134.671604283926)) ;
#120664 = CARTESIAN_POINT('Ctrl Pts',(-13.3796635334537,13.7633006467314,
134.614879288565)) ;
#120665 = CARTESIAN_POINT('Ctrl Pts',(-13.3497382425018,14.0028269061398,
134.494506191552)) ;
#120666 = CARTESIAN_POINT('Ctrl Pts',(-13.3002259749356,14.2028678275338,
134.316595478873)) ;
#120667 = CARTESIAN_POINT('Ctrl Pts',(-13.2361890414634,14.3455611921622,
134.09654406856)) ;
#120668 = CARTESIAN_POINT('Ctrl Pts',(-13.16207558202,14.4231516599767,133.846823988595)) ;
#120669 = CARTESIAN_POINT('Ctrl Pts',(-13.0845063845158,14.4286657254974,
133.587101274246)) ;
#120670 = CARTESIAN_POINT('Ctrl Pts',(-13.0095842588762,14.3621069450972,
133.335090766211)) ;
#120671 = CARTESIAN_POINT('Ctrl Pts',(-12.9435378379878,14.2287342743254,
133.109091925138)) ;
#120672 = CARTESIAN_POINT('Ctrl Pts',(-12.8914199215781,14.0363060460215,
132.923560068454)) ;
#120673 = CARTESIAN_POINT('Ctrl Pts',(-12.8583816910615,13.8023696285656,
132.794134663991)) ;
#120674 = CARTESIAN_POINT('Ctrl Pts',(-12.8467978400967,13.5388531548576,
132.727034564485)) ;
#120675 = CARTESIAN_POINT('Ctrl Pts',(-12.8586819410096,13.268451758325,132.728680134931)) ;
#120676 = CARTESIAN_POINT('Ctrl Pts',(-12.8936410367749,13.0087996264663,
132.797700642119)) ;
#120677 = CARTESIAN_POINT('Ctrl Pts',(-12.9504077026141,12.7778890108915,
132.930263212947)) ;
#120678 = CARTESIAN_POINT('Ctrl Pts',(-13.0245928914567,12.5950173458057,
133.114032484941)) ;
#120679 = CARTESIAN_POINT('Ctrl Pts',(-13.1129297604522,12.4700324855763,
133.338848639727)) ;
#120680 = CARTESIAN_POINT('Ctrl Pts',(-13.2086496709529,12.4138573674352,
133.58543860934)) ;
#120681 = CARTESIAN_POINT('Ctrl Pts',(-13.3068912134905,12.4301864396543,
133.83911949565)) ;
#120682 = CARTESIAN_POINT('Ctrl Pts',(-13.3993566508513,12.5166844416216,
134.076381880359)) ;
#120683 = CARTESIAN_POINT('Ctrl Pts',(-13.4825199697664,12.6693065290769,
134.286038282632)) ;
#120684 = CARTESIAN_POINT('Ctrl Pts',(-13.5493581300511,12.8745471633582,
134.448302940679)) ;
#120685 = CARTESIAN_POINT('Ctrl Pts',(-13.5969792928083,13.1212024009445,
134.554104584044)) ;
#120686 = CARTESIAN_POINT('Ctrl Pts',(-13.6217614180752,13.3871939344405,
134.593509017336)) ;
#120687 = CARTESIAN_POINT('Ctrl Pts',(-13.6233033483175,13.6567281897723,
134.564888588754)) ;
#120688 = CARTESIAN_POINT('Ctrl Pts',(-13.6019424260938,13.90978543386,134.469337913371)) ;
#120689 = CARTESIAN_POINT('Ctrl Pts',(-13.559878508592,14.1280196387556,134.313271082727)) ;
#120690 = CARTESIAN_POINT('Ctrl Pts',(-13.5012677872863,14.2950455998267,
134.109034226085)) ;
#120691 = CARTESIAN_POINT('Ctrl Pts',(-13.4301333980882,14.4005267621949,
133.867917157598)) ;
#120692 = CARTESIAN_POINT('Ctrl Pts',(-13.3536177744754,14.4350836723043,
133.611420653287)) ;
#120693 = CARTESIAN_POINT('Ctrl Pts',(-13.2769729997003,14.3978038978104,
133.354433604439)) ;
#120694 = CARTESIAN_POINT('Ctrl Pts',(-13.2065378850675,14.2905756791986,
133.115544315935)) ;
#120695 = CARTESIAN_POINT('Ctrl Pts',(-13.1481709847974,14.1209511396773,
132.911875009647)) ;
#120696 = CARTESIAN_POINT('Ctrl Pts',(-13.106914032843,13.9018371700798,132.758271963134)) ;
#120697 = CARTESIAN_POINT('Ctrl Pts',(-13.0862872253786,13.6479071174512,
132.664855347399)) ;
#120698 = CARTESIAN_POINT('Ctrl Pts',(-13.0885177354421,13.3785017706424,
132.638297597662)) ;
#120699 = CARTESIAN_POINT('Ctrl Pts',(-13.1144622409219,13.1105160825095,
132.680778935072)) ;
#120700 = CARTESIAN_POINT('Ctrl Pts',(-13.1623141537455,12.867723627882,132.787635761551)) ;
#120701 = CARTESIAN_POINT('Ctrl Pts',(-13.230117220087,12.6628307247657,132.952513766649)) ;
#120702 = CARTESIAN_POINT('Ctrl Pts',(-13.313146584717,12.5130918366744,133.162010291795)) ;
#120703 = CARTESIAN_POINT('Ctrl Pts',(-13.4069813662761,12.4280188888238,
133.402870847898)) ;
#120704 = CARTESIAN_POINT('Ctrl Pts',(-13.5044591370903,12.4146728717073,
133.654606478724)) ;
#120705 = CARTESIAN_POINT('Ctrl Pts',(-13.6004343999475,12.4734183176243,
133.901788773024)) ;
#120706 = CARTESIAN_POINT('Ctrl Pts',(-13.6881527513873,12.6005221105397,
134.124883438968)) ;
#120707 = CARTESIAN_POINT('Ctrl Pts',(-13.7618732063886,12.7855012395254,
134.307246567862)) ;
#120708 = CARTESIAN_POINT('Ctrl Pts',(-13.8177438998128,13.0169861501724,
134.437303681495)) ;
#120709 = CARTESIAN_POINT('Ctrl Pts',(-13.8520207068986,13.2774554458054,
134.50430837638)) ;
#120710 = CARTESIAN_POINT('Ctrl Pts',(-13.8630629061763,13.548371247685,134.503433492184)) ;
#120711 = CARTESIAN_POINT('Ctrl Pts',(-13.8508213988482,13.8100860909014,
134.434572278497)) ;
#120712 = CARTESIAN_POINT('Ctrl Pts',(-13.8168650274927,14.0443620867839,
134.302237807465)) ;
#120713 = CARTESIAN_POINT('Ctrl Pts',(-13.7644044931097,14.2339607222734,
134.115876257614)) ;
#120714 = CARTESIAN_POINT('Ctrl Pts',(-13.6978380060744,14.3656339915205,
133.888274922942)) ;
#120715 = CARTESIAN_POINT('Ctrl Pts',(-13.622733233145,14.4296685525136,133.635745138518)) ;
#120716 = CARTESIAN_POINT('Ctrl Pts',(-13.5452624861586,14.4216217611559,
133.37633613)) ;
#120717 = CARTESIAN_POINT('Ctrl Pts',(-13.4715715969191,14.3422173843901,
133.127956640297)) ;
#120718 = CARTESIAN_POINT('Ctrl Pts',(-13.4075312607501,14.1963612396834,
132.907659105306)) ;
#120719 = CARTESIAN_POINT('Ctrl Pts',(-13.3589146402362,13.9958155660663,
132.73257138974)) ;
#120720 = CARTESIAN_POINT('Ctrl Pts',(-13.329551475218,13.754087100232,132.613679382634)) ;
#120721 = CARTESIAN_POINT('Ctrl Pts',(-13.3223349657066,13.4887317484018,
132.559497435662)) ;
#120722 = CARTESIAN_POINT('Ctrl Pts',(-13.3386798564622,13.2176489571942,
132.574010621013)) ;
#120723 = CARTESIAN_POINT('Ctrl Pts',(-13.3777977002964,12.9629383916558,
132.655272653247)) ;
#120724 = CARTESIAN_POINT('Ctrl Pts',(-13.4382415285139,12.7394456176792,
132.798570796011)) ;
#120725 = CARTESIAN_POINT('Ctrl Pts',(-13.5154589025096,12.5666312437579,
132.991152487379)) ;
#120726 = CARTESIAN_POINT('Ctrl Pts',(-13.605481193571,12.4542159326756,133.220985631602)) ;
#120727 = CARTESIAN_POINT('Ctrl Pts',(-13.7021416815521,12.4113528378657,
133.470272085389)) ;
#120728 = CARTESIAN_POINT('Ctrl Pts',(-13.7997225612357,12.4409689783365,
133.722129964994)) ;
#120729 = CARTESIAN_POINT('Ctrl Pts',(-13.8914867339935,12.5412370853856,
133.957037400847)) ;
#120730 = CARTESIAN_POINT('Ctrl Pts',(-13.971457705638,12.7041353032971,134.157601912298)) ;
#120731 = CARTESIAN_POINT('Ctrl Pts',(-14.0350614876758,12.9183855317437,
134.31033126713)) ;
#120732 = CARTESIAN_POINT('Ctrl Pts',(-14.0784578071401,13.1698655551169,
134.403888857352)) ;
#120733 = CARTESIAN_POINT('Ctrl Pts',(-14.0989865001082,13.4380609721582,
134.430831936226)) ;
#120734 = CARTESIAN_POINT('Ctrl Pts',(-14.0960490957043,13.707166634389,134.388968900715)) ;
#120735 = CARTESIAN_POINT('Ctrl Pts',(-14.0706178920924,13.9538088162951,
134.281667787138)) ;
#120736 = CARTESIAN_POINT('Ctrl Pts',(-14.0252188571593,14.1634527174507,
134.115921093202)) ;
#120737 = CARTESIAN_POINT('Ctrl Pts',(-13.963634925678,14.3201289995184,133.902836103935)) ;
#120738 = CARTESIAN_POINT('Ctrl Pts',(-13.8915338635795,14.4121341024828,
133.659191560836)) ;
#120739 = CARTESIAN_POINT('Ctrl Pts',(-13.8140762063645,14.4336855920868,
133.399723796815)) ;
#120740 = CARTESIAN_POINT('Ctrl Pts',(-13.7381279524733,14.3827385765516,
133.144763866546)) ;
#120741 = CARTESIAN_POINT('Ctrl Pts',(-13.66939667137,14.2627494122855,132.910772598038)) ;
#120742 = CARTESIAN_POINT('Ctrl Pts',(-13.6139327257614,14.0822576460886,
132.71556082231)) ;
#120743 = CARTESIAN_POINT('Ctrl Pts',(-13.5764902068372,13.8561930768697,
132.573222227403)) ;
#120744 = CARTESIAN_POINT('Ctrl Pts',(-13.5600295200209,13.5974241277666,
132.491927422412)) ;
#120745 = CARTESIAN_POINT('Ctrl Pts',(-13.5667144048106,13.3273250801774,
132.478407313272)) ;
#120746 = CARTESIAN_POINT('Ctrl Pts',(-13.5969980563113,13.0622910344741,
132.533583951509)) ;
#120747 = CARTESIAN_POINT('Ctrl Pts',(-13.6488100028414,12.8256129311331,
132.651993012919)) ;
#120748 = CARTESIAN_POINT('Ctrl Pts',(-13.7197957147865,12.6301797722552,
132.826210227303)) ;
#120749 = CARTESIAN_POINT('Ctrl Pts',(-13.8052923968474,12.491847584192,133.042869793119)) ;
#120750 = CARTESIAN_POINT('Ctrl Pts',(-13.9002855742496,12.4199209625087,
133.287159868651)) ;
#120751 = CARTESIAN_POINT('Ctrl Pts',(-13.9983308301703,12.4204246206127,
133.540393962923)) ;
#120752 = CARTESIAN_POINT('Ctrl Pts',(-14.0926150230179,12.4921596766918,
133.782850441087)) ;
#120753 = CARTESIAN_POINT('Ctrl Pts',(-14.1782827856701,12.6310174141653,
133.999923925961)) ;
#120754 = CARTESIAN_POINT('Ctrl Pts',(-14.2490962026249,12.8262648550687,
134.173703003042)) ;
#120755 = CARTESIAN_POINT('Ctrl Pts',(-14.3010623629354,13.0646915634,134.292350167285)) ;
#120756 = CARTESIAN_POINT('Ctrl Pts',(-14.3310020809812,13.3278245942677,
134.346780502656)) ;
#120757 = CARTESIAN_POINT('Ctrl Pts',(-14.3376192816008,13.599858684379,134.33281390352)) ;
#120758 = CARTESIAN_POINT('Ctrl Pts',(-14.3210988184506,13.8569828233467,
134.25154641035)) ;
#120759 = CARTESIAN_POINT('Ctrl Pts',(-14.2833243438028,14.0842219920521,
134.108028651301)) ;
#120760 = CARTESIAN_POINT('Ctrl Pts',(-14.2279563626728,14.263433654148,133.913245859207)) ;
#120761 = CARTESIAN_POINT('Ctrl Pts',(-14.1590892226973,14.3833954982456,
133.67880615733)) ;
#120762 = CARTESIAN_POINT('Ctrl Pts',(-14.08298330848,14.4336980468668,133.423334734623)) ;
#120763 = CARTESIAN_POINT('Ctrl Pts',(-14.0060043305073,14.4120157634547,
133.165469744423)) ;
#120764 = CARTESIAN_POINT('Ctrl Pts',(-13.9335630677938,14.3192946556154,
132.920658510169)) ;
#120765 = CARTESIAN_POINT('Ctrl Pts',(-13.8722225085746,14.1625582896785,
132.708365939663)) ;
#120766 = CARTESIAN_POINT('Ctrl Pts',(-13.8267634979844,13.9521768642311,
132.542354975134)) ;
#120767 = CARTESIAN_POINT('Ctrl Pts',(-13.8015371760947,13.7045477344639,
132.43556559473)) ;
#120768 = CARTESIAN_POINT('Ctrl Pts',(-13.7987127257712,13.4377490318283,
132.394327067906)) ;
#120769 = CARTESIAN_POINT('Ctrl Pts',(-13.819460311345,13.1678476288368,132.421687970309)) ;
#120770 = CARTESIAN_POINT('Ctrl Pts',(-13.8627949203012,12.9176590168047,
132.515222019688)) ;
#120771 = CARTESIAN_POINT('Ctrl Pts',(-13.9268006590622,12.7025601714455,
132.668956240077)) ;
#120772 = CARTESIAN_POINT('Ctrl Pts',(-14.0066558896622,12.5405894740577,
132.869281960535)) ;
#120773 = CARTESIAN_POINT('Ctrl Pts',(-14.0985650251881,12.4405287581968,
133.104571602708)) ;
#120774 = CARTESIAN_POINT('Ctrl Pts',(-14.1961041611978,12.4114132280254,
133.356330665668)) ;
#120775 = CARTESIAN_POINT('Ctrl Pts',(-14.2926156330225,12.4546443860593,
133.605220308635)) ;
#120776 = CARTESIAN_POINT('Ctrl Pts',(-14.3824600952418,12.5668919860046,
133.834602175721)) ;
#120777 = CARTESIAN_POINT('Ctrl Pts',(-14.4601722625008,12.7415276460806,
134.028362617741)) ;
#120778 = CARTESIAN_POINT('Ctrl Pts',(-14.520049146209,12.9638993361252,134.170229973779)) ;
#120779 = CARTESIAN_POINT('Ctrl Pts',(-14.5591593181283,13.2191083147461,
134.251407675557)) ;
#120780 = CARTESIAN_POINT('Ctrl Pts',(-14.575350824638,13.4893535433623,134.265583197429)) ;
#120781 = CARTESIAN_POINT('Ctrl Pts',(-14.5680599633527,13.7553189464662,
134.211098945095)) ;
#120782 = CARTESIAN_POINT('Ctrl Pts',(-14.5385649126019,13.9971252301126,
134.091796305584)) ;
#120783 = CARTESIAN_POINT('Ctrl Pts',(-14.4896511547738,14.197781210739,133.915741437835)) ;
#120784 = CARTESIAN_POINT('Ctrl Pts',(-14.4259733060109,14.3424511179814,
133.696723001246)) ;
#120785 = CARTESIAN_POINT('Ctrl Pts',(-14.351768758291,14.4220643031845,133.446619873331)) ;
#120786 = CARTESIAN_POINT('Ctrl Pts',(-14.274603622944,14.4294490868584,133.18824319121)) ;
#120787 = CARTESIAN_POINT('Ctrl Pts',(-14.1995531258177,14.3652071957823,
132.935880016242)) ;
#120788 = CARTESIAN_POINT('Ctrl Pts',(-14.1330952945771,14.2335291048216,
132.708640760205)) ;
#120789 = CARTESIAN_POINT('Ctrl Pts',(-14.0805195452,14.0429178976906,132.52181225508)) ;
#120790 = CARTESIAN_POINT('Ctrl Pts',(-14.0468273962399,13.8093219413454,
132.390378710343)) ;
#120791 = CARTESIAN_POINT('Ctrl Pts',(-14.0345756389885,13.547621689864,132.321489870949)) ;
#120792 = CARTESIAN_POINT('Ctrl Pts',(-14.045869711759,13.275071076932,132.321149166054)) ;
#120793 = CARTESIAN_POINT('Ctrl Pts',(-14.0801004011068,13.0163163266613,
132.388221144306)) ;
#120794 = CARTESIAN_POINT('Ctrl Pts',(-14.1360514026648,12.7846450787164,
132.518475111333)) ;
#120795 = CARTESIAN_POINT('Ctrl Pts',(-14.209997805868,12.5995255835865,132.7014357454)) ;
#120796 = CARTESIAN_POINT('Ctrl Pts',(-14.2980487746721,12.4726551218916,
132.925409988479)) ;
#120797 = CARTESIAN_POINT('Ctrl Pts',(-14.3936992232197,12.4145513359232,
133.171770800119)) ;
#120798 = CARTESIAN_POINT('Ctrl Pts',(-14.4914656501182,12.4284690749365,
133.424241778918)) ;
#120799 = CARTESIAN_POINT('Ctrl Pts',(-14.5847554755448,12.513343198717,133.663701292664)) ;
#120800 = CARTESIAN_POINT('Ctrl Pts',(-14.6682321414824,12.6644367568353,
133.874283018656)) ;
#120801 = CARTESIAN_POINT('Ctrl Pts',(-14.7354435033099,12.8679925993142,
134.037693222063)) ;
#120802 = CARTESIAN_POINT('Ctrl Pts',(-14.7836382994798,13.1131690756933,
134.145239554443)) ;
#120803 = CARTESIAN_POINT('Ctrl Pts',(-14.8092152926094,13.380000312228,134.186817151239)) ;
#120804 = CARTESIAN_POINT('Ctrl Pts',(-14.8113213541148,13.6495651936862,
134.159860975393)) ;
#120805 = CARTESIAN_POINT('Ctrl Pts',(-14.7907198845191,13.9023389091985,
134.066668081572)) ;
#120806 = CARTESIAN_POINT('Ctrl Pts',(-14.7490861418248,14.1226577845122,
133.911740549666)) ;
#120807 = CARTESIAN_POINT('Ctrl Pts',(-14.6909606696642,14.2908247564139,
133.708982259999)) ;
#120808 = CARTESIAN_POINT('Ctrl Pts',(-14.6204821622466,14.398104059989,133.469939230604)) ;
#120809 = CARTESIAN_POINT('Ctrl Pts',(-14.5435082791429,14.4352626924574,
133.211865337823)) ;
#120810 = CARTESIAN_POINT('Ctrl Pts',(-14.4666927956805,14.3995540254238,
132.95433679224)) ;
#120811 = CARTESIAN_POINT('Ctrl Pts',(-14.3963438928318,14.2948938650605,
132.715871778826)) ;
#120812 = CARTESIAN_POINT('Ctrl Pts',(-14.3372225228914,14.1259509639325,
132.509807857198)) ;
#120813 = CARTESIAN_POINT('Ctrl Pts',(-14.2956197860169,13.9085226372069,
132.355294318318)) ;
#120814 = CARTESIAN_POINT('Ctrl Pts',(-14.2743647159268,13.6557404486892,
132.26008749006)) ;
#120815 = CARTESIAN_POINT('Ctrl Pts',(-14.2758917339881,13.3866405250996,
132.231488180435)) ;
#120816 = CARTESIAN_POINT('Ctrl Pts',(-14.3011573659847,13.1181023923962,
132.271965026739)) ;
#120817 = CARTESIAN_POINT('Ctrl Pts',(-14.3484050438208,12.8743682502049,
132.377050604409)) ;
#120818 = CARTESIAN_POINT('Ctrl Pts',(-14.4156978747053,12.6679957013257,
132.540429498857)) ;
#120819 = CARTESIAN_POINT('Ctrl Pts',(-14.4984992937558,12.5164143784842,
132.749208600845)) ;
#120820 = CARTESIAN_POINT('Ctrl Pts',(-14.5917693941425,12.4295970136061,
132.988543123613)) ;
#120821 = CARTESIAN_POINT('Ctrl Pts',(-14.6895186039868,12.4140261381013,
133.240964207369)) ;
#120822 = CARTESIAN_POINT('Ctrl Pts',(-14.7854846163672,12.4707103540387,
133.488174367292)) ;
#120823 = CARTESIAN_POINT('Ctrl Pts',(-14.8735159764431,12.595906863769,133.712181723645)) ;
#120824 = CARTESIAN_POINT('Ctrl Pts',(-14.9477237496053,12.7791143335627,
133.895987787412)) ;
#120825 = CARTESIAN_POINT('Ctrl Pts',(-15.0044945348177,13.0114294021893,
134.028419908865)) ;
#120826 = CARTESIAN_POINT('Ctrl Pts',(-15.0390399487791,13.2689900400404,
134.096517875508)) ;
#120827 = CARTESIAN_POINT('Ctrl Pts',(-15.0508899923374,13.5409258374442,
134.097867257872)) ;
#120828 = CARTESIAN_POINT('Ctrl Pts',(-15.0392557170542,13.8029841851952,
134.030803559731)) ;
#120829 = CARTESIAN_POINT('Ctrl Pts',(-15.0058370198303,14.0385609610044,
133.899998507003)) ;
#120830 = CARTESIAN_POINT('Ctrl Pts',(-14.9538399076615,14.229423171085,133.715008796875)) ;
#120831 = CARTESIAN_POINT('Ctrl Pts',(-14.8877137168842,14.3627051887218,
133.488747191819)) ;
#120832 = CARTESIAN_POINT('Ctrl Pts',(-14.8127359767209,14.4288334278673,
133.236570650323)) ;
#120833 = CARTESIAN_POINT('Ctrl Pts',(-14.7352173723857,14.4228924311934,
132.97701086134)) ;
#120834 = CARTESIAN_POINT('Ctrl Pts',(-14.6611248919809,14.3451233913639,
132.727361195705)) ;
#120835 = CARTESIAN_POINT('Ctrl Pts',(-14.5968447070673,14.2008972200028,
132.506395013173)) ;
#120836 = CARTESIAN_POINT('Ctrl Pts',(-14.5478751348737,14.0023959452744,
132.330379198133)) ;
#120837 = CARTESIAN_POINT('Ctrl Pts',(-14.5178450832966,13.7610317231258,
132.209459223291)) ;
#120838 = CARTESIAN_POINT('Ctrl Pts',(-14.5100259463151,13.496756912036,132.153602141983)) ;
#120839 = CARTESIAN_POINT('Ctrl Pts',(-14.5256011538682,13.2257685064712,
132.165897452881)) ;
#120840 = CARTESIAN_POINT('Ctrl Pts',(-14.5642253942489,12.9695425857073,
132.245607348793)) ;
#120841 = CARTESIAN_POINT('Ctrl Pts',(-14.6239259490414,12.7456271494707,
132.386844216458)) ;
#120842 = CARTESIAN_POINT('Ctrl Pts',(-14.7006990228845,12.5709695173834,
132.578111696268)) ;
#120843 = CARTESIAN_POINT('Ctrl Pts',(-14.7905491933371,12.4565179049814,
132.807400489142)) ;
#120844 = CARTESIAN_POINT('Ctrl Pts',(-14.8871250622566,12.4114773771493,
133.056433988563)) ;
#120845 = CARTESIAN_POINT('Ctrl Pts',(-14.9851299631796,12.4394645505146,
133.309400564807)) ;
#120846 = CARTESIAN_POINT('Ctrl Pts',(-15.0764284936881,12.5368907047146,
133.543217059238)) ;
#120847 = CARTESIAN_POINT('Ctrl Pts',(-15.1574847834624,12.6994727146824,
133.746665039927)) ;
#120848 = CARTESIAN_POINT('Ctrl Pts',(-15.2211909363152,12.9112843843373,
133.899900022678)) ;
#120849 = CARTESIAN_POINT('Ctrl Pts',(-15.2654725078526,13.1634090082974,
133.995846242239)) ;
#120850 = CARTESIAN_POINT('Ctrl Pts',(-15.2864378367501,13.4300956045555,
134.024226361752)) ;
#120851 = CARTESIAN_POINT('Ctrl Pts',(-15.2843390545469,13.6985487061805,
133.984939701581)) ;
#120852 = CARTESIAN_POINT('Ctrl Pts',(-15.2593145509194,13.9480246768514,
133.878558343557)) ;
#120853 = CARTESIAN_POINT('Ctrl Pts',(-15.2146255465162,14.1576527966606,
133.715072135231)) ;
#120854 = CARTESIAN_POINT('Ctrl Pts',(-15.1535306948074,14.3162850326807,
133.50342445039)) ;
#120855 = CARTESIAN_POINT('Ctrl Pts',(-15.0813082659069,14.4106899990105,
133.25926896319)) ;
#120856 = CARTESIAN_POINT('Ctrl Pts',(-15.0038819502148,14.4339585104257,
132.999884500443)) ;
#120857 = CARTESIAN_POINT('Ctrl Pts',(-14.928137987027,14.3853107488566,132.745666313131)) ;
#120858 = CARTESIAN_POINT('Ctrl Pts',(-14.8589321201176,14.2669553900087,
132.510203051672)) ;
#120859 = CARTESIAN_POINT('Ctrl Pts',(-14.8031390853071,14.0883945363266,
132.314103537993)) ;
#120860 = CARTESIAN_POINT('Ctrl Pts',(-14.7650760835763,13.8631866954131,
132.169904108232)) ;
#120861 = CARTESIAN_POINT('Ctrl Pts',(-14.747976795724,13.6057119879249,132.086827558504)) ;
#120862 = CARTESIAN_POINT('Ctrl Pts',(-14.7539914356653,13.3350527616499,
132.071265695883)) ;
#120863 = CARTESIAN_POINT('Ctrl Pts',(-14.7834351780099,13.0707552698518,
132.124144780644)) ;
#120864 = CARTESIAN_POINT('Ctrl Pts',(-14.8346901939508,12.8321485931701,
132.240824879715)) ;
#120865 = CARTESIAN_POINT('Ctrl Pts',(-14.9055915104809,12.6344629226598,
132.414633314627)) ;
#120866 = CARTESIAN_POINT('Ctrl Pts',(-14.9903658745253,12.4951761456202,
132.629340258018)) ;
#120867 = CARTESIAN_POINT('Ctrl Pts',(-15.0849702300836,12.4210995999737,
132.872555756299)) ;
#120868 = CARTESIAN_POINT('Ctrl Pts',(-15.1831256127438,12.4192964340424,
133.126073926616)) ;
#120869 = CARTESIAN_POINT('Ctrl Pts',(-15.2778095628797,12.4890492714601,
133.369627717516)) ;
#120870 = CARTESIAN_POINT('Ctrl Pts',(-15.3640763770914,12.6268327661457,
133.588333531199)) ;
#120871 = CARTESIAN_POINT('Ctrl Pts',(-15.4349360468843,12.8195831784206,
133.762439588941)) ;
#120872 = CARTESIAN_POINT('Ctrl Pts',(-15.4876340744907,13.0571003299884,
133.883190871599)) ;
#120873 = CARTESIAN_POINT('Ctrl Pts',(-15.518245025264,13.320280679744,133.939518694644)) ;
#120874 = CARTESIAN_POINT('Ctrl Pts',(-15.5255697583556,13.5914917582005,
133.927733313208)) ;
#120875 = CARTESIAN_POINT('Ctrl Pts',(-15.509601546287,13.8505567194106,133.847905316659)) ;
#120876 = CARTESIAN_POINT('Ctrl Pts',(-15.472551823714,14.0777829909349,133.706668786412)) ;
#120877 = CARTESIAN_POINT('Ctrl Pts',(-15.4175582389666,14.2590886738723,
133.512904737009)) ;
#120878 = CARTESIAN_POINT('Ctrl Pts',(-15.3490611968896,14.3807167115641,
133.279584839209)) ;
#120879 = CARTESIAN_POINT('Ctrl Pts',(-15.2731574758069,14.433343615208,133.024730945337)) ;
#120880 = CARTESIAN_POINT('Ctrl Pts',(-15.1956188392081,14.4133893489329,
132.765008849078)) ;
#120881 = CARTESIAN_POINT('Ctrl Pts',(-15.1234225876608,14.3229978009541,
132.521122428361)) ;
#120882 = CARTESIAN_POINT('Ctrl Pts',(-15.0616114780319,14.1680349923561,
132.307428002309)) ;
#120883 = CARTESIAN_POINT('Ctrl Pts',(-15.0157162337173,13.959434776873,132.140210034788)) ;
#120884 = CARTESIAN_POINT('Ctrl Pts',(-14.9897310083251,13.712829168107,132.031206744906)) ;
#120885 = CARTESIAN_POINT('Ctrl Pts',(-14.9863184802919,13.4442543283008,
131.987991189862)) ;
#120886 = CARTESIAN_POINT('Ctrl Pts',(-15.0061744908591,13.176694407093,132.013075122292)) ;
#120887 = CARTESIAN_POINT('Ctrl Pts',(-15.049237718297,12.9234094710806,132.105508422183)) ;
#120888 = CARTESIAN_POINT('Ctrl Pts',(-15.11234976022,12.7086523175308,132.256861037713)) ;
#120889 = CARTESIAN_POINT('Ctrl Pts',(-15.1918550986888,12.5444332801825,
132.456104683496)) ;
#120890 = CARTESIAN_POINT('Ctrl Pts',(-15.2838721870511,12.4422654275157,
132.691592196494)) ;
#120891 = CARTESIAN_POINT('Ctrl Pts',(-15.3809241567571,12.4113238215259,
132.942067261817)) ;
#120892 = CARTESIAN_POINT('Ctrl Pts',(-15.4776269938542,12.452199983914,133.191494717966)) ;
#120893 = CARTESIAN_POINT('Ctrl Pts',(-15.5682516153267,12.5635389999469,
133.422952701096)) ;
#120894 = CARTESIAN_POINT('Ctrl Pts',(-15.6457754650984,12.7354102811942,
133.616413756961)) ;
#120895 = CARTESIAN_POINT('Ctrl Pts',(-15.7063953713452,12.9568498442606,
133.76038439875)) ;
#120896 = CARTESIAN_POINT('Ctrl Pts',(-15.7461813643963,13.2117694969246,
133.843491058777)) ;
#120897 = CARTESIAN_POINT('Ctrl Pts',(-15.7630285422846,13.48252854114,133.859501479823)) ;
#120898 = CARTESIAN_POINT('Ctrl Pts',(-15.7563071367863,13.748482945783,133.806725663127)) ;
#120899 = CARTESIAN_POINT('Ctrl Pts',(-15.7275509102973,13.9900671624614,
133.689733432458)) ;
#120900 = CARTESIAN_POINT('Ctrl Pts',(-15.6792982108687,14.1922209506685,
133.515647821569)) ;
#120901 = CARTESIAN_POINT('Ctrl Pts',(-15.6155830086315,14.3393855753319,
133.296320311479)) ;
#120902 = CARTESIAN_POINT('Ctrl Pts',(-15.5422295688276,14.4204077482377,
133.04899534508)) ;
#120903 = CARTESIAN_POINT('Ctrl Pts',(-15.4646880996919,14.4304302068623,
132.789342072121)) ;
#120904 = CARTESIAN_POINT('Ctrl Pts',(-15.389253543915,14.3678711174913,132.53575988027)) ;
#120905 = CARTESIAN_POINT('Ctrl Pts',(-15.3224480781091,14.2376926994235,
132.307474173055)) ;
#120906 = CARTESIAN_POINT('Ctrl Pts',(-15.2695791733511,14.0489882455827,
132.119877916052)) ;
#120907 = CARTESIAN_POINT('Ctrl Pts',(-15.2352419555811,13.8164455432918,
131.986552716391)) ;
#120908 = CARTESIAN_POINT('Ctrl Pts',(-15.2224352712447,13.5541088077793,
131.915902354574)) ;
#120909 = CARTESIAN_POINT('Ctrl Pts',(-15.2328633064654,13.2846771651641,
131.913420948601)) ;
#120910 = CARTESIAN_POINT('Ctrl Pts',(-15.2666207126356,13.0230234432121,
131.978819239946)) ;
#120911 = CARTESIAN_POINT('Ctrl Pts',(-15.3219248693909,12.7908726515439,
132.107264949997)) ;
#120912 = CARTESIAN_POINT('Ctrl Pts',(-15.3955596009651,12.6038717726337,
132.289241148171)) ;
#120913 = CARTESIAN_POINT('Ctrl Pts',(-15.4829738673042,12.4755977885113,
132.511478747125)) ;
#120914 = CARTESIAN_POINT('Ctrl Pts',(-15.5787009690955,12.4151865367556,
132.757979288962)) ;
#120915 = CARTESIAN_POINT('Ctrl Pts',(-15.6763807869398,12.4270410724712,
133.010240147476)) ;
#120916 = CARTESIAN_POINT('Ctrl Pts',(-15.7698857979697,12.5098502892393,
133.250326255073)) ;
#120917 = CARTESIAN_POINT('Ctrl Pts',(-15.8537091275427,12.6589866450951,
133.46194433181)) ;
#120918 = CARTESIAN_POINT('Ctrl Pts',(-15.9215542492779,12.8615687451882,
133.627140073067)) ;
#120919 = CARTESIAN_POINT('Ctrl Pts',(-15.9702371826774,13.1050266769027,
133.736219667067)) ;
#120920 = CARTESIAN_POINT('Ctrl Pts',(-15.9965613702119,13.3718444110737,
133.779924979936)) ;
#120921 = CARTESIAN_POINT('Ctrl Pts',(-15.999444902403,13.6411904453346,133.755302949557)) ;
#120922 = CARTESIAN_POINT('Ctrl Pts',(-15.979202745745,13.8968635155474,133.662853690068)) ;
#120923 = CARTESIAN_POINT('Ctrl Pts',(-15.9385455558626,14.1159779799374,
133.511147245029)) ;
#120924 = CARTESIAN_POINT('Ctrl Pts',(-15.8804481741695,14.2873257027271,
133.308202911175)) ;
#120925 = CARTESIAN_POINT('Ctrl Pts',(-15.8103663899591,14.3958947377193,
133.070410963587)) ;
#120926 = CARTESIAN_POINT('Ctrl Pts',(-15.733745623836,14.4351265097039,132.813466935671)) ;
#120927 = CARTESIAN_POINT('Ctrl Pts',(-15.6568737721267,14.401957868835,132.555802882805)) ;
#120928 = CARTESIAN_POINT('Ctrl Pts',(-15.5857722650305,14.2982652122168,
132.314890619411)) ;
#120929 = CARTESIAN_POINT('Ctrl Pts',(-15.5267629965934,14.1324802087574,
132.109458823216)) ;
#120930 = CARTESIAN_POINT('Ctrl Pts',(-15.484312630846,13.9154628269439,131.9523001242)) ;
#120931 = CARTESIAN_POINT('Ctrl Pts',(-15.4624445929521,13.6633712406997,
131.855306338031)) ;
#120932 = CARTESIAN_POINT('Ctrl Pts',(-15.4633405140607,13.3940849340156,
131.824809337026)) ;
#120933 = CARTESIAN_POINT('Ctrl Pts',(-15.4877875794486,13.1263052582701,
131.863039831368)) ;
#120934 = CARTESIAN_POINT('Ctrl Pts',(-15.5346489194363,12.8804158513159,
131.96682400019)) ;
#120935 = CARTESIAN_POINT('Ctrl Pts',(-15.6012737282025,12.6733662735578,
132.128348254486)) ;
#120936 = CARTESIAN_POINT('Ctrl Pts',(-15.6838110767312,12.5197379021673,
132.336300360141)) ;
#120937 = CARTESIAN_POINT('Ctrl Pts',(-15.7769029536586,12.4310982059369,
132.575107599234)) ;
#120938 = CARTESIAN_POINT('Ctrl Pts',(-15.8743413642468,12.4134628316865,
132.82671087668)) ;
#120939 = CARTESIAN_POINT('Ctrl Pts',(-15.9705403191487,12.4679867596538,
133.074572192467)) ;
#120940 = CARTESIAN_POINT('Ctrl Pts',(-16.0590904745147,12.5916525961337,
133.300018721976)) ;
#120941 = CARTESIAN_POINT('Ctrl Pts',(-16.1336468131636,12.7734685194903,
133.484855342896)) ;
#120942 = CARTESIAN_POINT('Ctrl Pts',(-16.1906862831964,13.0028689239805,
133.61830847906)) ;
#120943 = CARTESIAN_POINT('Ctrl Pts',(-16.226261276871,13.261962548957,133.689131888325)) ;
#120944 = CARTESIAN_POINT('Ctrl Pts',(-16.2386405247801,13.5340193336117,
133.692012008431)) ;
#120945 = CARTESIAN_POINT('Ctrl Pts',(-16.227691036414,13.7955676266414,133.627073124232)) ;
#120946 = CARTESIAN_POINT('Ctrl Pts',(-16.1948762080394,14.0322614564451,
133.498024343725)) ;
#120947 = CARTESIAN_POINT('Ctrl Pts',(-16.1434360380022,14.2243899010379,
133.314703125322)) ;
#120948 = CARTESIAN_POINT('Ctrl Pts',(-16.0775677422439,14.3598901604785,
133.089143122656)) ;
#120949 = CARTESIAN_POINT('Ctrl Pts',(-16.0024062401398,14.4280176399282,
132.836283097058)) ;
#120950 = CARTESIAN_POINT('Ctrl Pts',(-15.9253625454778,14.4241023567618,
132.578322250813)) ;
#120951 = CARTESIAN_POINT('Ctrl Pts',(-15.8508506102757,14.3482279673457,
132.327343287973)) ;
#120952 = CARTESIAN_POINT('Ctrl Pts',(-15.786360116079,14.2060723674291,132.105843130321)) ;
#120953 = CARTESIAN_POINT('Ctrl Pts',(-15.7368242702798,14.0086807740354,
131.928116094623)) ;
#120954 = CARTESIAN_POINT('Ctrl Pts',(-15.7062275475401,13.7691470824975,
131.805652706501)) ;
#120955 = CARTESIAN_POINT('Ctrl Pts',(-15.6976947499871,13.5031160209837,
131.7474354851)) ;
#120956 = CARTESIAN_POINT('Ctrl Pts',(-15.7127216465963,13.2327333331826,
131.758218797029)) ;
#120957 = CARTESIAN_POINT('Ctrl Pts',(-15.7505752615138,12.976776614233,131.835791024487)) ;
#120958 = CARTESIAN_POINT('Ctrl Pts',(-15.8095780779271,12.7518156970481,
131.975032564164)) ;
#120959 = CARTESIAN_POINT('Ctrl Pts',(-15.8862411789886,12.5749030333723,
132.165838894875)) ;
#120960 = CARTESIAN_POINT('Ctrl Pts',(-15.9756600026082,12.4587258582811,
132.393929098427)) ;
#120961 = CARTESIAN_POINT('Ctrl Pts',(-16.0726294742164,12.4118884067616,
132.643935728496)) ;
#120962 = CARTESIAN_POINT('Ctrl Pts',(-16.1693474818951,12.4371448006442,
132.893616726414)) ;
#120963 = CARTESIAN_POINT('Ctrl Pts',(-16.2619924518505,12.5335140246063,
133.130965469335)) ;
#120964 = CARTESIAN_POINT('Ctrl Pts',(-16.3427349664474,12.6929505687292,
133.333809412538)) ;
#120965 = CARTESIAN_POINT('Ctrl Pts',(-16.4075929857113,12.9053983640665,
133.490085624717)) ;
#120966 = CARTESIAN_POINT('Ctrl Pts',(-16.4520337457546,13.1539498783259,
133.586871749901)) ;
#120967 = CARTESIAN_POINT('Ctrl Pts',(-16.4740125729542,13.422675078525,133.617911121948)) ;
#120968 = CARTESIAN_POINT('Ctrl Pts',(-16.4724822003861,13.691089143288,133.580327726125)) ;
#120969 = CARTESIAN_POINT('Ctrl Pts',(-16.4481242362547,13.9413684458137,
133.475899146845)) ;
#120970 = CARTESIAN_POINT('Ctrl Pts',(-16.4038361295165,14.1526799240858,
133.313515710715)) ;
#120971 = CARTESIAN_POINT('Ctrl Pts',(-16.3432199423983,14.3125333467772,
133.103328027861)) ;
#120972 = CARTESIAN_POINT('Ctrl Pts',(-16.2714680049075,14.408819463409,132.860643965138)) ;
#120973 = CARTESIAN_POINT('Ctrl Pts',(-16.1938245217602,14.4343198914763,
132.600502617637)) ;
#120974 = CARTESIAN_POINT('Ctrl Pts',(-16.1181031010312,14.3877722038871,
132.346416016408)) ;
#120975 = CARTESIAN_POINT('Ctrl Pts',(-16.0485304784478,14.2711470779282,
132.109837946035)) ;
#120976 = CARTESIAN_POINT('Ctrl Pts',(-15.9925306968979,14.0951742319451,
131.913300087355)) ;
#120977 = CARTESIAN_POINT('Ctrl Pts',(-15.953648770791,13.870335302896,131.766563806448)) ;
#120978 = CARTESIAN_POINT('Ctrl Pts',(-15.9359291073685,13.6128358613542,
131.681599922722)) ;
#120979 = CARTESIAN_POINT('Ctrl Pts',(-15.9412906023611,13.3431052342381,
131.664226615723)) ;
#120980 = CARTESIAN_POINT('Ctrl Pts',(-15.9699469241256,13.0784068980914,
131.71482665286)) ;
#120981 = CARTESIAN_POINT('Ctrl Pts',(-16.0211125920356,12.8371324748468,
131.830982955641)) ;
#120982 = CARTESIAN_POINT('Ctrl Pts',(-16.0908996434181,12.639991514166,132.001852443921)) ;
#120983 = CARTESIAN_POINT('Ctrl Pts',(-16.1757171914526,12.4979352238862,
132.21650801765)) ;
#120984 = CARTESIAN_POINT('Ctrl Pts',(-16.2703730971549,12.4220838446985,
132.459808435532)) ;
#120985 = CARTESIAN_POINT('Ctrl Pts',(-16.3683183392038,12.4184701426874,
132.712779770869)) ;
#120986 = CARTESIAN_POINT('Ctrl Pts',(-16.4628394543541,12.4860425111682,
132.955969482712)) ;
#120987 = CARTESIAN_POINT('Ctrl Pts',(-16.5492355946798,12.62129710121,133.175156001814)) ;
#120988 = CARTESIAN_POINT('Ctrl Pts',(-16.6209794354091,12.8133840710904,
133.351683229808)) ;
#120989 = CARTESIAN_POINT('Ctrl Pts',(-16.6742798344133,13.0503650213175,
133.474145212659)) ;
#120990 = CARTESIAN_POINT('Ctrl Pts',(-16.7054383248983,13.3123038567085,
133.532167225324)) ;
#120991 = CARTESIAN_POINT('Ctrl Pts',(-16.7134737697217,13.5832779933084,
133.522492394927)) ;
#120992 = CARTESIAN_POINT('Ctrl Pts',(-16.6982303620489,13.8428844537896,
133.444800801758)) ;
#120993 = CARTESIAN_POINT('Ctrl Pts',(-16.6616516930359,14.0720013816764,
133.304834740476)) ;
#120994 = CARTESIAN_POINT('Ctrl Pts',(-16.6071169159106,14.2546155978529,
133.11243298478)) ;
#120995 = CARTESIAN_POINT('Ctrl Pts',(-16.5391209400141,14.3779471702252,
132.880660794707)) ;
#120996 = CARTESIAN_POINT('Ctrl Pts',(-16.4632550759513,14.4327785527786,
132.625869651701)) ;
#120997 = CARTESIAN_POINT('Ctrl Pts',(-16.3859214509523,14.4152048360803,
132.366858853552)) ;
#120998 = CARTESIAN_POINT('Ctrl Pts',(-16.3131469320527,14.3266409428597,
132.121134580323)) ;
#120999 = CARTESIAN_POINT('Ctrl Pts',(-16.2508735851622,14.1729214671605,
131.906029507347)) ;
#121000 = CARTESIAN_POINT('Ctrl Pts',(-16.2046102027505,13.9662155184911,
131.737830097701)) ;
#121001 = CARTESIAN_POINT('Ctrl Pts',(-16.1779888101469,13.7208186547473,
131.627002572066)) ;
#121002 = CARTESIAN_POINT('Ctrl Pts',(-16.1738448501189,13.4521886594885,
131.581602362447)) ;
#121003 = CARTESIAN_POINT('Ctrl Pts',(-16.1931355127838,13.1838897369756,
131.604966282919)) ;
#121004 = CARTESIAN_POINT('Ctrl Pts',(-16.2352668534616,12.9313138648893,
131.694879378208)) ;
#121005 = CARTESIAN_POINT('Ctrl Pts',(-16.2979953414801,12.7142071163423,
131.844978217263)) ;
#121006 = CARTESIAN_POINT('Ctrl Pts',(-16.3773062651453,12.5481822878489,
132.043585307447)) ;
#121007 = CARTESIAN_POINT('Ctrl Pts',(-16.4685437718777,12.4445945503844,
132.27697928454)) ;
#121008 = CARTESIAN_POINT('Ctrl Pts',(-16.5655957618824,12.4110615289685,
132.527422237429)) ;
#121009 = CARTESIAN_POINT('Ctrl Pts',(-16.6628557772642,12.4502003413461,
132.778318054091)) ;
#121010 = CARTESIAN_POINT('Ctrl Pts',(-16.7531335309511,12.5587981618695,
133.008994097715)) ;
#121011 = CARTESIAN_POINT('Ctrl Pts',(-16.8314074438916,12.7290993092181,
133.20455574507)) ;
#121012 = CARTESIAN_POINT('Ctrl Pts',(-16.8928577533825,12.950564316011,133.350782950407)) ;
#121013 = CARTESIAN_POINT('Ctrl Pts',(-16.9330790264365,13.2039534170359,
133.435275758517)) ;
#121014 = CARTESIAN_POINT('Ctrl Pts',(-16.9506380553928,13.4737768777198,
133.45345380249)) ;
#121015 = CARTESIAN_POINT('Ctrl Pts',(-16.9446670676314,13.7408243981145,
133.402794669402)) ;
#121016 = CARTESIAN_POINT('Ctrl Pts',(-16.9163090827626,13.9843829005592,
133.286806456363)) ;
#121017 = CARTESIAN_POINT('Ctrl Pts',(-16.8687835725521,14.1867700874977,
133.115020926219)) ;
#121018 = CARTESIAN_POINT('Ctrl Pts',(-16.8054030141767,14.3360223630702,
132.896629962351)) ;
#121019 = CARTESIAN_POINT('Ctrl Pts',(-16.7322445813577,14.4190305114461,
132.649874649277)) ;
#121020 = CARTESIAN_POINT('Ctrl Pts',(-16.6547444226988,14.4311357302908,
132.390344056005)) ;
#121021 = CARTESIAN_POINT('Ctrl Pts',(-16.5792695493848,14.3708887604269,
132.136703574011)) ;
#121022 = CARTESIAN_POINT('Ctrl Pts',(-16.5120163560413,14.2422926303469,
131.907041000821)) ;
#121023 = CARTESIAN_POINT('Ctrl Pts',(-16.4588725477531,14.0562618591324,
131.718813468793)) ;
#121024 = CARTESIAN_POINT('Ctrl Pts',(-16.4236593544539,13.8231736000303,
131.582683084744)) ;
#121025 = CARTESIAN_POINT('Ctrl Pts',(-16.4102829007904,13.5622215659962,
131.510485072681)) ;
#121026 = CARTESIAN_POINT('Ctrl Pts',(-16.4200291090512,13.2923509313982,
131.505951545336)) ;
#121027 = CARTESIAN_POINT('Ctrl Pts',(-16.4530192792313,13.0307855165856,
131.569197474403)) ;
#121028 = CARTESIAN_POINT('Ctrl Pts',(-16.5079078696725,12.796715819409,131.696311601221)) ;
#121029 = CARTESIAN_POINT('Ctrl Pts',(-16.5810548280508,12.6083942037896,
131.876886012649)) ;
#121030 = CARTESIAN_POINT('Ctrl Pts',(-16.6682374248203,12.4782666718545,
132.098415600761)) ;
#121031 = CARTESIAN_POINT('Ctrl Pts',(-16.7634938948967,12.4160107552107,
132.343651107937)) ;
#121032 = CARTESIAN_POINT('Ctrl Pts',(-16.8614539449369,12.4255889321841,
132.596647127972)) ;
#121033 = CARTESIAN_POINT('Ctrl Pts',(-16.9555012968993,12.5070743683389,
132.838185834921)) ;
#121034 = CARTESIAN_POINT('Ctrl Pts',(-17.0392450020579,12.6538728233386,
133.049737407758)) ;
#121035 = CARTESIAN_POINT('Ctrl Pts',(-17.107726307674,12.8553500132408,133.216734480995)) ;
#121036 = CARTESIAN_POINT('Ctrl Pts',(-17.1570082574672,13.0981034422233,
133.327545614228)) ;
#121037 = CARTESIAN_POINT('Ctrl Pts',(-17.183965292424,13.3649638787798,133.373050395986)) ;
#121038 = CARTESIAN_POINT('Ctrl Pts',(-17.1874265803459,13.633409473525,133.350241103702)) ;
#121039 = CARTESIAN_POINT('Ctrl Pts',(-17.1680409732944,13.8886868708514,
133.260455975359)) ;
#121040 = CARTESIAN_POINT('Ctrl Pts',(-17.12776078413,14.1104518503625,133.109655864797)) ;
#121041 = CARTESIAN_POINT('Ctrl Pts',(-17.0700684671704,14.2832226352683,
132.90790533618)) ;
#121042 = CARTESIAN_POINT('Ctrl Pts',(-17.0003049596219,14.3937886252325,
132.671056763834)) ;
#121043 = CARTESIAN_POINT('Ctrl Pts',(-16.9234305592928,14.4350213811874,
132.413222353031)) ;
#121044 = CARTESIAN_POINT('Ctrl Pts',(-16.8468492367316,14.4038716557598,
132.156565176017)) ;
#121045 = CARTESIAN_POINT('Ctrl Pts',(-16.7753697290314,14.3020574418522,
131.914495582995)) ;
#121046 = CARTESIAN_POINT('Ctrl Pts',(-16.7159734074721,14.1377082714835,
131.707924566398)) ;
#121047 = CARTESIAN_POINT('Ctrl Pts',(-16.6730770027358,13.9225120842828,
131.549544677542)) ;
#121048 = CARTESIAN_POINT('Ctrl Pts',(-16.6505166862748,13.6705375094453,
131.45044216059)) ;
#121049 = CARTESIAN_POINT('Ctrl Pts',(-16.6508051559261,13.4018845199762,
131.418221579722)) ;
#121050 = CARTESIAN_POINT('Ctrl Pts',(-16.6744356225866,13.1344381552283,
131.454156161431)) ;
#121051 = CARTESIAN_POINT('Ctrl Pts',(-16.7209299074623,12.8864832879891,
131.556700740614)) ;
#121052 = CARTESIAN_POINT('Ctrl Pts',(-16.7867037912973,12.679196010264,131.715913956127)) ;
#121053 = CARTESIAN_POINT('Ctrl Pts',(-16.8689665205321,12.5233811225036,
131.922997628966)) ;
#121054 = CARTESIAN_POINT('Ctrl Pts',(-16.9617056853245,12.4327816487888,
132.160820091053)) ;
#121055 = CARTESIAN_POINT('Ctrl Pts',(-17.0594012996445,12.4129159597619,
132.41307010867)) ;
#121056 = CARTESIAN_POINT('Ctrl Pts',(-17.1556153739254,12.4655032985934,
132.66101261288)) ;
#121057 = CARTESIAN_POINT('Ctrl Pts',(-17.2441896100086,12.5866529745153,
132.886646653344)) ;
#121058 = CARTESIAN_POINT('Ctrl Pts',(-17.3195526790658,12.767439628638,133.073711296189)) ;
#121059 = CARTESIAN_POINT('Ctrl Pts',(-17.377292110819,12.9966808158701,133.209093801097)) ;
#121060 = CARTESIAN_POINT('Ctrl Pts',(-17.4132761779649,13.2541242728622,
133.281251443548)) ;
#121061 = CARTESIAN_POINT('Ctrl Pts',(-17.4264022871086,13.524842234863,133.286467705085)) ;
#121062 = CARTESIAN_POINT('Ctrl Pts',(-17.4161430564136,13.7882272307475,
133.223383906437)) ;
#121063 = CARTESIAN_POINT('Ctrl Pts',(-17.383874755988,14.0260984495824,133.095908384181)) ;
#121064 = CARTESIAN_POINT('Ctrl Pts',(-17.3327899753643,14.2200232579374,
132.913557519948)) ;
#121065 = CARTESIAN_POINT('Ctrl Pts',(-17.2673674124666,14.3567722758536,
132.6893718229)) ;
#121066 = CARTESIAN_POINT('Ctrl Pts',(-17.1928382513417,14.4269174595849,
132.438549893294)) ;
#121067 = CARTESIAN_POINT('Ctrl Pts',(-17.1151930703958,14.4252572802329,
132.178577294835)) ;
#121068 = CARTESIAN_POINT('Ctrl Pts',(-17.0407081937327,14.3512844314495,
131.927763325467)) ;
#121069 = CARTESIAN_POINT('Ctrl Pts',(-16.9760740580518,14.2117349601844,
131.705971266209)) ;
#121070 = CARTESIAN_POINT('Ctrl Pts',(-16.9257713272981,14.0152547415916,
131.52588164766)) ;
#121071 = CARTESIAN_POINT('Ctrl Pts',(-16.8945605226789,13.7756398670369,
131.401498225142)) ;
#121072 = CARTESIAN_POINT('Ctrl Pts',(-16.88541891899,13.5122934272068,131.341781181152)) ;
#121073 = CARTESIAN_POINT('Ctrl Pts',(-16.8996517098331,13.2411299536141,
131.350160139664)) ;
#121074 = CARTESIAN_POINT('Ctrl Pts',(-16.9369013734199,12.9839532693091,
131.425907297011)) ;
#121075 = CARTESIAN_POINT('Ctrl Pts',(-16.9955710856029,12.7572239501203,
131.564068015513)) ;
#121076 = CARTESIAN_POINT('Ctrl Pts',(-17.071467998947,12.5794741125724,131.752779615537)) ;
#121077 = CARTESIAN_POINT('Ctrl Pts',(-17.1608121883335,12.4611210628414,
131.980564154477)) ;
#121078 = CARTESIAN_POINT('Ctrl Pts',(-17.2571503761721,12.4122668253808,
132.228903249691)) ;
#121079 = CARTESIAN_POINT('Ctrl Pts',(-17.3546376058722,12.4354395157324,
132.480589572177)) ;
#121080 = CARTESIAN_POINT('Ctrl Pts',(-17.4474577248439,12.5301694906382,
132.718462736226)) ;
#121081 = CARTESIAN_POINT('Ctrl Pts',(-17.528398067295,12.6876686677728,132.921950991047)) ;
#121082 = CARTESIAN_POINT('Ctrl Pts',(-17.5936909444915,12.898212465334,133.079574187598)) ;
#121083 = CARTESIAN_POINT('Ctrl Pts',(-17.6389773689883,13.1472879217631,
133.178651901856)) ;
#121084 = CARTESIAN_POINT('Ctrl Pts',(-17.6614873036012,13.4151706305656,
133.211320240868)) ;
#121085 = CARTESIAN_POINT('Ctrl Pts',(-17.6606115793353,13.6833052701105,
133.175708233052)) ;
#121086 = CARTESIAN_POINT('Ctrl Pts',(-17.6370969311646,13.9335262167577,
133.073884888561)) ;
#121087 = CARTESIAN_POINT('Ctrl Pts',(-17.5929860893633,14.1479664881483,
132.911736516363)) ;
#121088 = CARTESIAN_POINT('Ctrl Pts',(-17.5328890109081,14.3087959188899,
132.703169232262)) ;
#121089 = CARTESIAN_POINT('Ctrl Pts',(-17.4613931385352,14.4069520257531,
132.461231766129)) ;
#121090 = CARTESIAN_POINT('Ctrl Pts',(-17.3841812797812,14.434703937208,132.202512060337)) ;
#121091 = CARTESIAN_POINT('Ctrl Pts',(-17.3078205401366,14.3899170706969,
131.946323472494)) ;
#121092 = CARTESIAN_POINT('Ctrl Pts',(-17.2383885165578,14.275848167113,131.710364627399)) ;
#121093 = CARTESIAN_POINT('Ctrl Pts',(-17.1816816715689,14.1010294116989,
131.511633889459)) ;
#121094 = CARTESIAN_POINT('Ctrl Pts',(-17.1422631986116,13.8772033892953,
131.363323086006)) ;
#121095 = CARTESIAN_POINT('Ctrl Pts',(-17.1239156778148,13.6206146695245,
131.276552146189)) ;
#121096 = CARTESIAN_POINT('Ctrl Pts',(-17.128571603957,13.3509220809883,131.257110126722)) ;
#121097 = CARTESIAN_POINT('Ctrl Pts',(-17.1566772042895,13.0853828321562,
131.306041738499)) ;
#121098 = CARTESIAN_POINT('Ctrl Pts',(-17.2068859584364,12.8445475509271,
131.419607688918)) ;
#121099 = CARTESIAN_POINT('Ctrl Pts',(-17.2763923833637,12.6449528168769,
131.589517903078)) ;
#121100 = CARTESIAN_POINT('Ctrl Pts',(-17.3608585228123,12.5012606134937,
131.803156341898)) ;
#121101 = CARTESIAN_POINT('Ctrl Pts',(-17.4549824595557,12.4235056415569,
132.045012563526)) ;
#121102 = CARTESIAN_POINT('Ctrl Pts',(-17.5529484609703,12.4173186288012,
132.298035942043)) ;
#121103 = CARTESIAN_POINT('Ctrl Pts',(-17.6482211097473,12.4833715210388,
132.543213532662)) ;
#121104 = CARTESIAN_POINT('Ctrl Pts',(-17.7345330550901,12.6162286422635,
132.762314386659)) ;
#121105 = CARTESIAN_POINT('Ctrl Pts',(-17.8070216390377,12.8073411346184,
132.940908095724)) ;
#121106 = CARTESIAN_POINT('Ctrl Pts',(-17.8608373477978,13.0432166498449,
133.064898766188)) ;
#121107 = CARTESIAN_POINT('Ctrl Pts',(-17.8926735534002,13.3046950611415,
133.124891631411)) ;
#121108 = CARTESIAN_POINT('Ctrl Pts',(-17.9013624719413,13.5764464662961,
133.117037886171)) ;
#121109 = CARTESIAN_POINT('Ctrl Pts',(-17.8866709778763,13.8363551234792,
133.040981956794)) ;
#121110 = CARTESIAN_POINT('Ctrl Pts',(-17.8508343744671,14.0655922643217,
132.903327377715)) ;
#121111 = CARTESIAN_POINT('Ctrl Pts',(-17.7966375360881,14.2503954850495,
132.711817289313)) ;
#121112 = CARTESIAN_POINT('Ctrl Pts',(-17.7287032482948,14.3757154300573,
132.480127244775)) ;
#121113 = CARTESIAN_POINT('Ctrl Pts',(-17.6531018723206,14.4321659963664,
132.226171168029)) ;
#121114 = CARTESIAN_POINT('Ctrl Pts',(-17.5759806284613,14.416734287709,131.967888324685)) ;
#121115 = CARTESIAN_POINT('Ctrl Pts',(-17.503004842333,14.330289953115,131.721586227307)) ;
#121116 = CARTESIAN_POINT('Ctrl Pts',(-17.4402855682396,14.1784243130749,
131.505170261232)) ;
#121117 = CARTESIAN_POINT('Ctrl Pts',(-17.3932928277742,13.9717507261075,
131.33465019109)) ;
#121118 = CARTESIAN_POINT('Ctrl Pts',(-17.3662979484006,13.7284356402105,
131.222910396826)) ;
#121119 = CARTESIAN_POINT('Ctrl Pts',(-17.3613675605102,13.4606301532886,
131.175263996789)) ;
#121120 = CARTESIAN_POINT('Ctrl Pts',(-17.3801479950331,13.1906191848992,
131.196949420637)) ;
#121121 = CARTESIAN_POINT('Ctrl Pts',(-17.4214109843812,12.9388679746563,
131.28453157571)) ;
#121122 = CARTESIAN_POINT('Ctrl Pts',(-17.4837628187899,12.7195132138376,
131.43340170599)) ;
#121123 = CARTESIAN_POINT('Ctrl Pts',(-17.5628590770987,12.5518557372857,
131.631327287361)) ;
#121124 = CARTESIAN_POINT('Ctrl Pts',(-17.6534051668585,12.4467157582098,
131.862855290462)) ;
#121125 = CARTESIAN_POINT('Ctrl Pts',(-17.750922989384,12.4110145773966,132.114468726418)) ;
#121126 = CARTESIAN_POINT('Ctrl Pts',(-17.8476115268141,12.4479828338558,
132.363921471666)) ;
#121127 = CARTESIAN_POINT('Ctrl Pts',(-17.9383943809633,12.5544308131199,
132.596009504229)) ;
#121128 = CARTESIAN_POINT('Ctrl Pts',(-18.0175559739188,12.7245572228014,
132.793937494374)) ;
#121129 = CARTESIAN_POINT('Ctrl Pts',(-18.0790907579623,12.9435040036317,
132.940630250791)) ;
#121130 = CARTESIAN_POINT('Ctrl Pts',(-18.1200567127323,13.1965754591591,
133.027234652194)) ;
#121131 = CARTESIAN_POINT('Ctrl Pts',(-18.1382282000561,13.4658054703846,
133.047256744435)) ;
#121132 = CARTESIAN_POINT('Ctrl Pts',(-18.1329659863274,13.732871013944,132.998710444717)) ;
#121133 = CARTESIAN_POINT('Ctrl Pts',(-18.10532591625,13.9772573341515,132.884851141224)) ;
#121134 = CARTESIAN_POINT('Ctrl Pts',(-18.0580724361184,14.1820529613216,
132.713691198042)) ;
#121135 = CARTESIAN_POINT('Ctrl Pts',(-17.9950516196932,14.3328844022839,
132.496365183043)) ;
#121136 = CARTESIAN_POINT('Ctrl Pts',(-17.9218660059439,14.4178011232664,
132.249431768721)) ;
#121137 = CARTESIAN_POINT('Ctrl Pts',(-17.8447787579686,14.4318123856393,
131.991276847606)) ;
#121138 = CARTESIAN_POINT('Ctrl Pts',(-17.7688468684742,14.3732302589804,
131.736154808824)) ;
#121139 = CARTESIAN_POINT('Ctrl Pts',(-17.7016395323525,14.2469702615313,
131.506798120837)) ;
#121140 = CARTESIAN_POINT('Ctrl Pts',(-17.6479009174849,14.062146427081,131.316760898445)) ;
#121141 = CARTESIAN_POINT('Ctrl Pts',(-17.6122040870272,13.8305006230351,
131.179278949391)) ;
#121142 = CARTESIAN_POINT('Ctrl Pts',(-17.59812106964,13.5704780261443,131.105053850186)) ;
#121143 = CARTESIAN_POINT('Ctrl Pts',(-17.6072307928306,13.2994605324582,
131.098521057394)) ;
#121144 = CARTESIAN_POINT('Ctrl Pts',(-17.6396331892695,13.037734227312,131.160085006349)) ;
#121145 = CARTESIAN_POINT('Ctrl Pts',(-17.6936156259918,12.803624496366,131.284711823525)) ;
#121146 = CARTESIAN_POINT('Ctrl Pts',(-17.7665279927222,12.6130122644718,
131.464475667698)) ;
#121147 = CARTESIAN_POINT('Ctrl Pts',(-17.8531437758454,12.4813447222013,
131.684440690985)) ;
#121148 = CARTESIAN_POINT('Ctrl Pts',(-17.9485680511644,12.4167223738628,
131.930048045931)) ;
#121149 = CARTESIAN_POINT('Ctrl Pts',(-18.0464149044187,12.4243656160183,
132.182759693883)) ;
#121150 = CARTESIAN_POINT('Ctrl Pts',(-18.1404091781105,12.5034383279314,
132.424237107159)) ;
#121151 = CARTESIAN_POINT('Ctrl Pts',(-18.2246786699213,12.6484426938847,
132.637280318487)) ;
#121152 = CARTESIAN_POINT('Ctrl Pts',(-18.2938530712968,12.8490572514717,
132.806215101685)) ;
#121153 = CARTESIAN_POINT('Ctrl Pts',(-18.3436429560685,13.0907450284177,
132.91853526463)) ;
#121154 = CARTESIAN_POINT('Ctrl Pts',(-18.371252264237,13.3559778959346,132.966092269471)) ;
#121155 = CARTESIAN_POINT('Ctrl Pts',(-18.3754407699862,13.6264773514175,
132.945172138598)) ;
#121156 = CARTESIAN_POINT('Ctrl Pts',(-18.3566809485503,13.8815734058857,
132.857323251945)) ;
#121157 = CARTESIAN_POINT('Ctrl Pts',(-18.3170081818755,14.1045282831523,
132.708304429531)) ;
#121158 = CARTESIAN_POINT('Ctrl Pts',(-18.2597751403882,14.2789670592856,
132.507903597064)) ;
#121159 = CARTESIAN_POINT('Ctrl Pts',(-18.1902019565029,14.391495176626,132.271568247248)) ;
#121160 = CARTESIAN_POINT('Ctrl Pts',(-18.1137540914775,14.4348607601378,
132.015118816648)) ;
#121161 = CARTESIAN_POINT('Ctrl Pts',(-18.0366821366047,14.4056890506022,
131.756845266094)) ;
#121162 = CARTESIAN_POINT('Ctrl Pts',(-17.9652797618649,14.3062653151645,
131.515158727385)) ;
#121163 = CARTESIAN_POINT('Ctrl Pts',(-17.9053122185148,14.143440527592,131.306846917921)) ;
#121164 = CARTESIAN_POINT('Ctrl Pts',(-17.8618616267719,13.9296996140236,
131.14687021965)) ;
#121165 = CARTESIAN_POINT('Ctrl Pts',(-17.8385996039929,13.6772902096435,
131.04555802276)) ;
#121166 = CARTESIAN_POINT('Ctrl Pts',(-17.8382591024878,13.409949714787,131.011638149779)) ;
#121167 = CARTESIAN_POINT('Ctrl Pts',(-17.8612351070141,13.1418739498075,
131.04561730523)) ;
#121168 = CARTESIAN_POINT('Ctrl Pts',(-17.9068955452945,12.8939990758876,
131.145858633822)) ;
#121169 = CARTESIAN_POINT('Ctrl Pts',(-17.9722749811336,12.6844790937915,
131.303812613166)) ;
#121170 = CARTESIAN_POINT('Ctrl Pts',(-18.0545827898634,12.5265062627849,
131.510876033157)) ;
#121171 = CARTESIAN_POINT('Ctrl Pts',(-18.1466282278198,12.4345049835541,
131.746844398259)) ;
#121172 = CARTESIAN_POINT('Ctrl Pts',(-18.2445839573682,12.4124896125378,
131.999744598179)) ;
#121173 = CARTESIAN_POINT('Ctrl Pts',(-18.3405183739417,12.4629155090419,
132.247009375301)) ;
#121174 = CARTESIAN_POINT('Ctrl Pts',(-18.4295849017639,12.5820912846789,
132.474029520711)) ;
#121175 = CARTESIAN_POINT('Ctrl Pts',(-18.5056519422923,12.762437228793,132.662998391459)) ;
#121176 = CARTESIAN_POINT('Ctrl Pts',(-18.5633863090852,12.9881392996051,
132.798710522865)) ;
#121177 = CARTESIAN_POINT('Ctrl Pts',(-18.6003855090257,13.2462583810271,
132.873643296643)) ;
#121178 = CARTESIAN_POINT('Ctrl Pts',(-18.6141306103123,13.5176872670076,
132.880577098406)) ;
#121179 = CARTESIAN_POINT('Ctrl Pts',(-18.6045499019302,13.7805945427873,
132.819592418361)) ;
#121180 = CARTESIAN_POINT('Ctrl Pts',(-18.5729239333371,14.0195270315699,
132.693993288043)) ;
#121181 = CARTESIAN_POINT('Ctrl Pts',(-18.522340896185,14.215038587717,132.513103225343)) ;
#121182 = CARTESIAN_POINT('Ctrl Pts',(-18.4571155071067,14.3538333245836,
132.289419709278)) ;
#121183 = CARTESIAN_POINT('Ctrl Pts',(-18.3828481440028,14.4259647082628,
132.039405260107)) ;
#121184 = CARTESIAN_POINT('Ctrl Pts',(-18.3049142988197,14.4260802645705,
131.778458304169)) ;
#121185 = CARTESIAN_POINT('Ctrl Pts',(-18.2309221252842,14.3549350188174,
131.529395653821)) ;
#121186 = CARTESIAN_POINT('Ctrl Pts',(-18.1653474115413,14.2162528409401,
131.304574043089)) ;
#121187 = CARTESIAN_POINT('Ctrl Pts',(-18.1147647836669,14.0213155988979,
131.123737866304)) ;
#121188 = CARTESIAN_POINT('Ctrl Pts',(-18.0829568038137,13.7835941603823,
130.997714182427)) ;
#121189 = CARTESIAN_POINT('Ctrl Pts',(-18.0731617219499,13.5186607714519,
130.935832378915)) ;
#121190 = CARTESIAN_POINT('Ctrl Pts',(-18.08665514099,13.2494161503812,130.942305026168)) ;
#121191 = CARTESIAN_POINT('Ctrl Pts',(-18.1234398333306,12.990369061565,131.01652371198)) ;
#121192 = CARTESIAN_POINT('Ctrl Pts',(-18.1811896004733,12.763690008938,131.1521929047)) ;
#121193 = CARTESIAN_POINT('Ctrl Pts',(-18.2573582331817,12.5829313612557,
131.341393014982)) ;
#121194 = CARTESIAN_POINT('Ctrl Pts',(-18.3454804211725,12.4640788232719,
131.565967626037)) ;
#121195 = CARTESIAN_POINT('Ctrl Pts',(-18.4422170243134,12.4125693563369,
131.815275161053)) ;
#121196 = CARTESIAN_POINT('Ctrl Pts',(-18.5394443787495,12.4337094288139,
132.066314652827)) ;
#121197 = CARTESIAN_POINT('Ctrl Pts',(-18.6326075786638,12.5263145417804,
132.305156553116)) ;
#121198 = CARTESIAN_POINT('Ctrl Pts',(-18.7140301788209,12.6822587586298,
132.51002276371)) ;
#121199 = CARTESIAN_POINT('Ctrl Pts',(-18.7798505478773,12.891562566965,132.669176374346)) ;
#121200 = CARTESIAN_POINT('Ctrl Pts',(-18.8257122760329,13.1392603161048,
132.770001449946)) ;
#121201 = CARTESIAN_POINT('Ctrl Pts',(-18.8489611088603,13.4076118666746,
132.804727708531)) ;
#121202 = CARTESIAN_POINT('Ctrl Pts',(-18.8487873523375,13.6757335651874,
132.77121043275)) ;
#121203 = CARTESIAN_POINT('Ctrl Pts',(-18.8256132329382,13.9281677218218,
132.670161224817)) ;
#121204 = CARTESIAN_POINT('Ctrl Pts',(-18.7826335465806,14.1410411473799,
132.511768994752)) ;
#121205 = CARTESIAN_POINT('Ctrl Pts',(-18.7225925718125,14.3051859898324,
132.303106999407)) ;
#121206 = CARTESIAN_POINT('Ctrl Pts',(-18.6513452461886,14.4050577743806,
132.061917791597)) ;
#121207 = CARTESIAN_POINT('Ctrl Pts',(-18.5741291719038,14.4349188602028,
131.80314713111)) ;
#121208 = CARTESIAN_POINT('Ctrl Pts',(-18.4977975157086,14.3922309332557,
131.547105617257)) ;
#121209 = CARTESIAN_POINT('Ctrl Pts',(-18.4280943233288,14.280180814084,131.310361629809)) ;
#121210 = CARTESIAN_POINT('Ctrl Pts',(-18.3708931056203,14.1070359905501,
131.110179808883)) ;
#121211 = CARTESIAN_POINT('Ctrl Pts',(-18.3308086150891,13.8833119230109,
130.959777523606)) ;
#121212 = CARTESIAN_POINT('Ctrl Pts',(-18.3119377968156,13.6288341860585,
130.871668553615)) ;
#121213 = CARTESIAN_POINT('Ctrl Pts',(-18.3159111846383,13.3582465565096,
130.850099973561)) ;
#121214 = CARTESIAN_POINT('Ctrl Pts',(-18.3433003468858,13.0930921360638,
130.897041192962)) ;
#121215 = CARTESIAN_POINT('Ctrl Pts',(-18.3929361586387,12.8509540623848,
131.008888330338)) ;
#121216 = CARTESIAN_POINT('Ctrl Pts',(-18.4619089664474,12.6500624789761,
131.177258567627)) ;
#121217 = CARTESIAN_POINT('Ctrl Pts',(-18.5461379773402,12.5043219731701,
131.390152397971)) ;
#121218 = CARTESIAN_POINT('Ctrl Pts',(-18.6402475797295,12.4246931364435,
131.631910775786)) ;
#121219 = CARTESIAN_POINT('Ctrl Pts',(-18.7376942627791,12.4164962070895,
131.883586283708)) ;
#121220 = CARTESIAN_POINT('Ctrl Pts',(-18.8331990949263,12.480251448006,132.129424653254)) ;
#121221 = CARTESIAN_POINT('Ctrl Pts',(-18.9200789894093,12.6116453538561,
132.350096934906)) ;
#121222 = CARTESIAN_POINT('Ctrl Pts',(-18.9929314642051,12.8011773158268,
132.529786089759)) ;
#121223 = CARTESIAN_POINT('Ctrl Pts',(-19.0472165928124,13.0350451037076,
132.655266689086)) ;
#121224 = CARTESIAN_POINT('Ctrl Pts',(-19.0798709801947,13.296978163916,132.717519763971)) ;
#121225 = CARTESIAN_POINT('Ctrl Pts',(-19.0892082104324,13.567734807944,132.711685741346)) ;
#121226 = CARTESIAN_POINT('Ctrl Pts',(-19.0753069867193,13.8283852939848,
132.637933494416)) ;
#121227 = CARTESIAN_POINT('Ctrl Pts',(-19.0398727138031,14.0598715137087,
132.501291676026)) ;
#121228 = CARTESIAN_POINT('Ctrl Pts',(-18.9862483048037,14.2455588284616,
132.311544093607)) ;
#121229 = CARTESIAN_POINT('Ctrl Pts',(-18.9189473375773,14.372564186769,132.081831246997)) ;
#121230 = CARTESIAN_POINT('Ctrl Pts',(-18.8432518289211,14.4315964784329,
131.82748588724)) ;
#121231 = CARTESIAN_POINT('Ctrl Pts',(-18.765913403393,14.4181824034525,131.568494223874)) ;
#121232 = CARTESIAN_POINT('Ctrl Pts',(-18.692751570031,14.3336377789342,131.321654785139)) ;
#121233 = CARTESIAN_POINT('Ctrl Pts',(-18.6298278945258,14.1840090727439,
131.10473755244)) ;
#121234 = CARTESIAN_POINT('Ctrl Pts',(-18.5822566163956,13.9789557865459,
130.932534794822)) ;
#121235 = CARTESIAN_POINT('Ctrl Pts',(-18.5545117957318,13.7355807215654,
130.818473396782)) ;
#121236 = CARTESIAN_POINT('Ctrl Pts',(-18.5490157747953,13.4678621828446,
130.769143890178)) ;
#121237 = CARTESIAN_POINT('Ctrl Pts',(-18.56696059197,13.1991327913341,130.788574867325)) ;
#121238 = CARTESIAN_POINT('Ctrl Pts',(-18.6078081529041,12.945225699974,130.874755629269)) ;
#121239 = CARTESIAN_POINT('Ctrl Pts',(-18.6692767013979,12.7259341324381,
131.021237394438)) ;
#121240 = CARTESIAN_POINT('Ctrl Pts',(-18.7480152928831,12.5559411157644,
131.218051157817)) ;
#121241 = CARTESIAN_POINT('Ctrl Pts',(-18.8388160211192,12.448546099201,131.450147238315)) ;
#121242 = CARTESIAN_POINT('Ctrl Pts',(-18.9356607715897,12.4111599417381,
131.699992854173)) ;
#121243 = CARTESIAN_POINT('Ctrl Pts',(-19.0325585145463,12.4456278236405,
131.95002607637)) ;
#121244 = CARTESIAN_POINT('Ctrl Pts',(-19.1242640700438,12.5514145638213,
132.184545497414)) ;
#121245 = CARTESIAN_POINT('Ctrl Pts',(-19.2029461856585,12.7181519506854,
132.381442208303)) ;
#121246 = CARTESIAN_POINT('Ctrl Pts',(-19.265372014259,12.9364297169796,132.530607306383)) ;
#121247 = CARTESIAN_POINT('Ctrl Pts',(-19.3069432913256,13.18875320047,132.618989652973)) ;
#121248 = CARTESIAN_POINT('Ctrl Pts',(-19.3258346486548,13.4580633582235,
132.641077480806)) ;
#121249 = CARTESIAN_POINT('Ctrl Pts',(-19.3212023059647,13.7256378176803,
132.594351189216)) ;
#121250 = CARTESIAN_POINT('Ctrl Pts',(-19.2942346936325,13.9704139793173,
132.482524019834)) ;
#121251 = CARTESIAN_POINT('Ctrl Pts',(-19.2474975955159,14.1767864699774,
132.312853122444)) ;
#121252 = CARTESIAN_POINT('Ctrl Pts',(-19.1848424036697,14.3292888824905,
132.096591593124)) ;
#121253 = CARTESIAN_POINT('Ctrl Pts',(-19.1121219052823,14.4162419172546,
131.851121689147)) ;
#121254 = CARTESIAN_POINT('Ctrl Pts',(-19.0345819635708,14.4323070544899,
131.59142753805)) ;
#121255 = CARTESIAN_POINT('Ctrl Pts',(-18.9591954174312,14.3764282188079,
131.338211778277)) ;
#121256 = CARTESIAN_POINT('Ctrl Pts',(-18.8911670048974,14.2515624978579,
131.106230242992)) ;
#121257 = CARTESIAN_POINT('Ctrl Pts',(-18.8370010450514,14.0682227623741,
130.914960556141)) ;
#121258 = CARTESIAN_POINT('Ctrl Pts',(-18.800665716264,13.8370232958438,130.775522481171)) ;
#121259 = CARTESIAN_POINT('Ctrl Pts',(-18.7860202678278,13.5786248872284,
130.699792853421)) ;
#121260 = CARTESIAN_POINT('Ctrl Pts',(-18.7943923368573,13.3076276344917,
130.69109892016)) ;
#121261 = CARTESIAN_POINT('Ctrl Pts',(-18.8260990797752,13.0452572131087,
130.75062398468)) ;
#121262 = CARTESIAN_POINT('Ctrl Pts',(-18.8797421459153,12.8091511761324,
130.874119491717)) ;
#121263 = CARTESIAN_POINT('Ctrl Pts',(-18.9521348210093,12.6175515473568,
131.052415653752)) ;
#121264 = CARTESIAN_POINT('Ctrl Pts',(-19.0381707151645,12.4843717623364,
131.27077668053)) ;
#121265 = CARTESIAN_POINT('Ctrl Pts',(-19.1335146928641,12.4175958607342,
131.516116935228)) ;
#121266 = CARTESIAN_POINT('Ctrl Pts',(-19.2312708874078,12.423055511444,131.768602952943)) ;
#121267 = CARTESIAN_POINT('Ctrl Pts',(-19.3256060412756,12.5002516966647,
132.011021092683)) ;
#121268 = CARTESIAN_POINT('Ctrl Pts',(-19.4100225537391,12.6429372151447,
132.22459247483)) ;
#121269 = CARTESIAN_POINT('Ctrl Pts',(-19.4800185412338,12.8430360326097,
132.395771984144)) ;
#121270 = CARTESIAN_POINT('Ctrl Pts',(-19.5302192048766,13.0829431740334,
132.509414453532)) ;
#121271 = CARTESIAN_POINT('Ctrl Pts',(-19.5585654550094,13.3482626607442,
132.55905272483)) ;
#121272 = CARTESIAN_POINT('Ctrl Pts',(-19.563461465539,13.6179806011048,132.540316904992)) ;
#121273 = CARTESIAN_POINT('Ctrl Pts',(-19.5452614806164,13.875457841107,132.453889291214)) ;
#121274 = CARTESIAN_POINT('Ctrl Pts',(-19.5059749293386,14.0994368558722,
132.305976912958)) ;
#121275 = CARTESIAN_POINT('Ctrl Pts',(-19.4495643240987,14.2743408494019,
132.108197550613)) ;
#121276 = CARTESIAN_POINT('Ctrl Pts',(-19.3801028719207,14.3892596808428,
131.872091124806)) ;
#121277 = CARTESIAN_POINT('Ctrl Pts',(-19.3038120358737,14.4346258040279,
131.616124870343)) ;
#121278 = CARTESIAN_POINT('Ctrl Pts',(-19.2264650722539,14.4074612293383,
131.356960779271)) ;
#121279 = CARTESIAN_POINT('Ctrl Pts',(-19.1548734293025,14.309698779788,131.114726202209)) ;
#121280 = CARTESIAN_POINT('Ctrl Pts',(-19.0947134293815,14.149377401071,130.905995069427)) ;
#121281 = CARTESIAN_POINT('Ctrl Pts',(-19.0505245415155,13.9355628699076,
130.743660881634)) ;
#121282 = CARTESIAN_POINT('Ctrl Pts',(-19.0268048363665,13.6861606150325,
130.641306302118)) ;
#121283 = CARTESIAN_POINT('Ctrl Pts',(-19.0257295347008,13.4167352196909,
130.604941607389)) ;
#121284 = CARTESIAN_POINT('Ctrl Pts',(-19.04808383544,13.1492793409581,130.637217629532)) ;
#121285 = CARTESIAN_POINT('Ctrl Pts',(-19.0930886530328,12.9005268752137,
130.73554146477)) ;
#121286 = CARTESIAN_POINT('Ctrl Pts',(-19.1580129920185,12.6897474195092,
130.892153881767)) ;
#121287 = CARTESIAN_POINT('Ctrl Pts',(-19.2395204495496,12.5306016213155,
131.0970291101)) ;
#121288 = CARTESIAN_POINT('Ctrl Pts',(-19.3317952144819,12.4360458788129,
131.333494889956)) ;
#121289 = CARTESIAN_POINT('Ctrl Pts',(-19.4295434756039,12.412131815675,131.585843687012)) ;
#121290 = CARTESIAN_POINT('Ctrl Pts',(-19.5258027055626,12.4605358152628,
131.833991352613)) ;
#121291 = CARTESIAN_POINT('Ctrl Pts',(-19.6152333793376,12.5784164712972,
132.062021657327)) ;
#121292 = CARTESIAN_POINT('Ctrl Pts',(-19.6911374309485,12.7554817105356,
132.250804667793)) ;
#121293 = CARTESIAN_POINT('Ctrl Pts',(-19.7499458974431,12.9817624941524,
132.389383273802)) ;
#121294 = CARTESIAN_POINT('Ctrl Pts',(-19.7873669405952,13.238159912852,132.465701955096)) ;
#121295 = CARTESIAN_POINT('Ctrl Pts',(-19.8018658367857,13.5101993099721,
132.474743662736)) ;
#121296 = CARTESIAN_POINT('Ctrl Pts',(-19.7929397566941,13.7733132280516,
132.415709326912)) ;
#121297 = CARTESIAN_POINT('Ctrl Pts',(-19.7617376794374,14.014064219241,132.291217067636)) ;
#121298 = CARTESIAN_POINT('Ctrl Pts',(-19.7118501129715,14.209874547802,132.112528195874)) ;
#121299 = CARTESIAN_POINT('Ctrl Pts',(-19.6470638524804,14.3505802758006,
131.890148790837)) ;
#121300 = CARTESIAN_POINT('Ctrl Pts',(-19.5728971610653,14.4248316803085,
131.640390131458)) ;
#121301 = CARTESIAN_POINT('Ctrl Pts',(-19.4950524479168,14.4272047931218,
131.379744281131)) ;
#121302 = CARTESIAN_POINT('Ctrl Pts',(-19.4206848800324,14.3577939123121,
131.129487152645)) ;
#121303 = CARTESIAN_POINT('Ctrl Pts',(-19.3550396477323,14.2217456845042,
130.904621923371)) ;
#121304 = CARTESIAN_POINT('Ctrl Pts',(-19.3035711789367,14.0267540354523,
130.720935325739)) ;
#121305 = CARTESIAN_POINT('Ctrl Pts',(-19.2714378715331,13.7911379046606,
130.594140611943)) ;
#121306 = CARTESIAN_POINT('Ctrl Pts',(-19.2608853613429,13.5273989700341,
130.530120327277)) ;
#121307 = CARTESIAN_POINT('Ctrl Pts',(-19.2737049786075,13.2571615768974,
130.534513540007)) ;
#121308 = CARTESIAN_POINT('Ctrl Pts',(-19.3098561857145,12.9974107950377,
130.606874926784)) ;
#121309 = CARTESIAN_POINT('Ctrl Pts',(-19.3671173273149,12.7695379002692,
130.741090474397)) ;
#121310 = CARTESIAN_POINT('Ctrl Pts',(-19.4423816889131,12.5879936402029,
130.927827001247)) ;
#121311 = CARTESIAN_POINT('Ctrl Pts',(-19.5307334454651,12.4663339482719,
131.152861116724)) ;
#121312 = CARTESIAN_POINT('Ctrl Pts',(-19.6273404115409,12.4130530274037,
131.401799903801)) ;
#121313 = CARTESIAN_POINT('Ctrl Pts',(-19.7244405424946,12.4321501261291,
131.652523062607)) ;
#121314 = CARTESIAN_POINT('Ctrl Pts',(-19.8176642020463,12.5224108266138,
131.891610555698)) ;
#121315 = CARTESIAN_POINT('Ctrl Pts',(-19.8998542340623,12.677312247728,132.098569709702)) ;
#121316 = CARTESIAN_POINT('Ctrl Pts',(-19.9660793378694,12.8853932149283,
132.258922203789)) ;
#121317 = CARTESIAN_POINT('Ctrl Pts',(-20.0123986186212,13.1311434716641,
132.361222124421)) ;
#121318 = CARTESIAN_POINT('Ctrl Pts',(-20.0364461583432,13.400088705093,132.398168019541)) ;
#121319 = CARTESIAN_POINT('Ctrl Pts',(-20.0368470691668,13.6679854897532,
132.366376497439)) ;
#121320 = CARTESIAN_POINT('Ctrl Pts',(-20.0146247443677,13.9198929111463,
132.268318118694)) ;
#121321 = CARTESIAN_POINT('Ctrl Pts',(-19.9716011530985,14.1367331628791,
132.109363562631)) ;
#121322 = CARTESIAN_POINT('Ctrl Pts',(-19.9125458930421,14.300676127775,131.903935240049)) ;
#121323 = CARTESIAN_POINT('Ctrl Pts',(-19.8411105246955,14.4034182514066,
131.661964468887)) ;
#121324 = CARTESIAN_POINT('Ctrl Pts',(-19.764157971726,14.4350219446425,131.404058044713)) ;
#121325 = CARTESIAN_POINT('Ctrl Pts',(-19.687633022118,14.3943912068368,131.147406929743)) ;
#121326 = CARTESIAN_POINT('Ctrl Pts',(-19.6176743104395,14.2842181110636,
130.909930061093)) ;
#121327 = CARTESIAN_POINT('Ctrl Pts',(-19.5600372344949,14.1123337735145,
130.708436969519)) ;
#121328 = CARTESIAN_POINT('Ctrl Pts',(-19.5196200459579,13.8914432947139,
130.557293195234)) ;
#121329 = CARTESIAN_POINT('Ctrl Pts',(-19.4999297703099,13.6364805468731,
130.466619696567)) ;
#121330 = CARTESIAN_POINT('Ctrl Pts',(-19.5032408659291,13.3663281054811,
130.443156629942)) ;
#121331 = CARTESIAN_POINT('Ctrl Pts',(-19.5299958970005,13.1002904156236,
130.488184032619)) ;
#121332 = CARTESIAN_POINT('Ctrl Pts',(-19.5790361835478,12.8573186036191,
130.598302560895)) ;
#121333 = CARTESIAN_POINT('Ctrl Pts',(-19.6475151340922,12.655055825907,130.765227996969)) ;
#121334 = CARTESIAN_POINT('Ctrl Pts',(-19.7312879255764,12.5076994513089,
130.976825411261)) ;
#121335 = CARTESIAN_POINT('Ctrl Pts',(-19.8251745452015,12.4260781925878,
131.217935682851)) ;
#121336 = CARTESIAN_POINT('Ctrl Pts',(-19.9225599733253,12.4155414447684,
131.469450266245)) ;
#121337 = CARTESIAN_POINT('Ctrl Pts',(-20.0189134984637,12.478090322654,131.71751385141)) ;
#121338 = CARTESIAN_POINT('Ctrl Pts',(-20.1052892315539,12.6066344478164,
131.937021849716)) ;
#121339 = CARTESIAN_POINT('Ctrl Pts',(-20.1789585189106,12.7952137023379,
132.118961495482)) ;
#121340 = CARTESIAN_POINT('Ctrl Pts',(-20.2337494135648,13.0279819979312,
132.245943194612)) ;
#121341 = CARTESIAN_POINT('Ctrl Pts',(-20.2670855507984,13.2896875880003,
132.310146572719)) ;
#121342 = CARTESIAN_POINT('Ctrl Pts',(-20.2770381998546,13.5603129292438,
132.306128411386)) ;
#121343 = CARTESIAN_POINT('Ctrl Pts',(-20.2638119493052,13.8211028677067,
132.234401447179)) ;
#121344 = CARTESIAN_POINT('Ctrl Pts',(-20.2289487599049,14.053803313072,132.099410060731)) ;
#121345 = CARTESIAN_POINT('Ctrl Pts',(-20.1757739845993,14.2410908350298,
131.910965000059)) ;
#121346 = CARTESIAN_POINT('Ctrl Pts',(-20.1085725822687,14.3701941601828,
131.681445986199)) ;
#121347 = CARTESIAN_POINT('Ctrl Pts',(-20.0330781315566,14.4308809616827,
131.427719983322)) ;
#121348 = CARTESIAN_POINT('Ctrl Pts',(-19.9559494024703,14.4196138695008,
131.169443863645)) ;
#121349 = CARTESIAN_POINT('Ctrl Pts',(-19.8824068556425,14.3368368148889,
130.921412444081)) ;
#121350 = CARTESIAN_POINT('Ctrl Pts',(-19.8192971637931,14.1892310626699,
130.704037107648)) ;
#121351 = CARTESIAN_POINT('Ctrl Pts',(-19.7712007701594,13.9859052749166,
130.53033092249)) ;
#121352 = CARTESIAN_POINT('Ctrl Pts',(-19.7427697939353,13.7426111503383,
130.414154891542)) ;
#121353 = CARTESIAN_POINT('Ctrl Pts',(-19.7366417092746,13.4761437933061,
130.363088987223)) ;
#121354 = CARTESIAN_POINT('Ctrl Pts',(-19.7538516960635,13.207093106288,130.38035702043)) ;
#121355 = CARTESIAN_POINT('Ctrl Pts',(-19.7941146155968,12.9521503447167,
130.464788413262)) ;
#121356 = CARTESIAN_POINT('Ctrl Pts',(-19.8550256367924,12.7315094010331,
130.609635495912)) ;
#121357 = CARTESIAN_POINT('Ctrl Pts',(-19.9336999560045,12.5595225483876,
130.806132413325)) ;
#121358 = CARTESIAN_POINT('Ctrl Pts',(-20.0235052591104,12.4509681320899,
131.035586591273)) ;
#121359 = CARTESIAN_POINT('Ctrl Pts',(-20.1210367820071,12.4111337662686,
131.287163832228)) ;
#121360 = CARTESIAN_POINT('Ctrl Pts',(-20.2175551658632,12.4436883981266,
131.536249097719)) ;
#121361 = CARTESIAN_POINT('Ctrl Pts',(-20.3095832198193,12.5474867377232,
131.771686083341)) ;
#121362 = CARTESIAN_POINT('Ctrl Pts',(-20.3885938102402,12.7123018064528,
131.969591631901)) ;
#121363 = CARTESIAN_POINT('Ctrl Pts',(-20.4517259907487,12.9300708063277,
132.120711783805)) ;
#121364 = CARTESIAN_POINT('Ctrl Pts',(-20.4937380782586,13.1802337565337,
132.21056605483)) ;
#121365 = CARTESIAN_POINT('Ctrl Pts',(-20.5134506438464,13.4510759335073,
132.234831539263)) ;
#121366 = CARTESIAN_POINT('Ctrl Pts',(-20.5094352277015,13.7180593172982,
132.190025271022)) ;
#121367 = CARTESIAN_POINT('Ctrl Pts',(-20.4830290210652,13.9642786305136,
132.079760168839)) ;
#121368 = CARTESIAN_POINT('Ctrl Pts',(-20.43689278128,14.1712561910319,131.911939492134)) ;
#121369 = CARTESIAN_POINT('Ctrl Pts',(-20.3749029793823,14.3253725381315,
131.697731780804)) ;
#121370 = CARTESIAN_POINT('Ctrl Pts',(-20.3018341343474,14.4148742721194,
131.450984618379)) ;
#121371 = CARTESIAN_POINT('Ctrl Pts',(-20.2249302855789,14.4329087862449,
131.193411182104)) ;
#121372 = CARTESIAN_POINT('Ctrl Pts',(-20.1488881094776,14.3788838227845,
130.938050037987)) ;
#121373 = CARTESIAN_POINT('Ctrl Pts',(-20.080797339942,14.2561019527568,130.706001182306)) ;
#121374 = CARTESIAN_POINT('Ctrl Pts',(-20.0261332992237,14.0742377640131,
130.513250821122)) ;
#121375 = CARTESIAN_POINT('Ctrl Pts',(-19.9893332364788,13.8451949445008,
130.372595598783)) ;
#121376 = CARTESIAN_POINT('Ctrl Pts',(-19.973868386846,13.58674350493,130.294374437478)) ;
#121377 = CARTESIAN_POINT('Ctrl Pts',(-19.9816774413976,13.3144404098801,
130.283872434014)) ;
#121378 = CARTESIAN_POINT('Ctrl Pts',(-20.0126413058548,13.0528695222705,
130.341385113357)) ;
#121379 = CARTESIAN_POINT('Ctrl Pts',(-20.065511341227,12.8160517966369,130.4626835875)) ;
#121380 = CARTESIAN_POINT('Ctrl Pts',(-20.1374567371324,12.6226065253332,
130.639635517755)) ;
#121381 = CARTESIAN_POINT('Ctrl Pts',(-20.2233273344394,12.4871996902566,
130.857443179732)) ;
#121382 = CARTESIAN_POINT('Ctrl Pts',(-20.318859154293,12.4184347650075,131.103214513939)) ;
#121383 = CARTESIAN_POINT('Ctrl Pts',(-20.4160586900493,12.4219001268695,
131.354266248446)) ;
#121384 = CARTESIAN_POINT('Ctrl Pts',(-20.5107057575997,12.4968774725135,
131.597561711737)) ;
#121385 = CARTESIAN_POINT('Ctrl Pts',(-20.5956132149196,12.6381726387492,
131.812503913232)) ;
#121386 = CARTESIAN_POINT('Ctrl Pts',(-20.6659104312661,12.8360677562161,
131.984677720499)) ;
#121387 = CARTESIAN_POINT('Ctrl Pts',(-20.7169616994697,13.0762566249802,
132.100631255503)) ;
#121388 = CARTESIAN_POINT('Ctrl Pts',(-20.7458024931045,13.3398740968699,
132.151878255805)) ;
#121389 = CARTESIAN_POINT('Ctrl Pts',(-20.7514496276872,13.6103044053491,
132.135261699282)) ;
#121390 = CARTESIAN_POINT('Ctrl Pts',(-20.7338894981992,13.86812497933,132.050741922307)) ;
#121391 = CARTESIAN_POINT('Ctrl Pts',(-20.6952759855552,14.0932871473164,
131.904822536434)) ;
#121392 = CARTESIAN_POINT('Ctrl Pts',(-20.6388857078219,14.2707836651958,
131.706880360139)) ;
#121393 = CARTESIAN_POINT('Ctrl Pts',(-20.5701123801385,14.3866738498425,
131.472993198284)) ;
#121394 = CARTESIAN_POINT('Ctrl Pts',(-20.4938977661901,14.4343395644747,
131.21722235527)) ;
#121395 = CARTESIAN_POINT('Ctrl Pts',(-20.4166445517324,14.4093417118186,
130.958399478142)) ;
#121396 = CARTESIAN_POINT('Ctrl Pts',(-20.344750708675,14.3139583253282,130.715285151649)) ;
#121397 = CARTESIAN_POINT('Ctrl Pts',(-20.283791621845,14.1538396084722,130.503960542603)) ;
#121398 = CARTESIAN_POINT('Ctrl Pts',(-20.2394788321261,13.9434082094923,
130.341592089435)) ;
#121399 = CARTESIAN_POINT('Ctrl Pts',(-20.2148885604201,13.6926166180059,
130.236385900469)) ;
#121400 = CARTESIAN_POINT('Ctrl Pts',(-20.2132281702384,13.4252309557657,
130.198542928982)) ;
#121401 = CARTESIAN_POINT('Ctrl Pts',(-20.2348670323948,13.15699249017,130.228662293908)) ;
#121402 = CARTESIAN_POINT('Ctrl Pts',(-20.2792098941449,12.9074157483193,
130.325066626541)) ;
#121403 = CARTESIAN_POINT('Ctrl Pts',(-20.3439168468294,12.6946405590363,
130.480906726514)) ;
#121404 = CARTESIAN_POINT('Ctrl Pts',(-20.4244393498658,12.5348309265639,
130.683142054182)) ;
#121405 = CARTESIAN_POINT('Ctrl Pts',(-20.5170520572993,12.4376124646164,
130.920376912197)) ;
#121406 = CARTESIAN_POINT('Ctrl Pts',(-20.614232235177,12.411847051691,131.17124526899)) ;
#121407 = CARTESIAN_POINT('Ctrl Pts',(-20.7107805897904,12.4580456629596,
131.420177217248)) ;
#121408 = CARTESIAN_POINT('Ctrl Pts',(-20.8003281359883,12.5736491425348,
131.648625222613)) ;
#121409 = CARTESIAN_POINT('Ctrl Pts',(-20.8769776512577,12.7495592043743,
131.839473480739)) ;
#121410 = CARTESIAN_POINT('Ctrl Pts',(-20.9364697192037,12.9753684252062,
131.979963656201)) ;
#121411 = CARTESIAN_POINT('Ctrl Pts',(-20.9744395485556,13.2312290478431,
132.057879143097)) ;
#121412 = CARTESIAN_POINT('Ctrl Pts',(-20.9895716582003,13.5022492390578,
132.068885248279)) ;
#121413 = CARTESIAN_POINT('Ctrl Pts',(-20.9812409962063,13.766376795235,132.011509443639)) ;
#121414 = CARTESIAN_POINT('Ctrl Pts',(-20.9509284133775,14.0063277413084,
131.889875566884)) ;
#121415 = CARTESIAN_POINT('Ctrl Pts',(-20.901397437773,14.2048736878869,131.712059721878)) ;
#121416 = CARTESIAN_POINT('Ctrl Pts',(-20.8367333930258,14.3476912358554,
131.489937969168)) ;
#121417 = CARTESIAN_POINT('Ctrl Pts',(-20.7626675459821,14.4237776456092,
131.240443597558)) ;
#121418 = CARTESIAN_POINT('Ctrl Pts',(-20.6850444981711,14.4280807671714,
130.980533757575)) ;
#121419 = CARTESIAN_POINT('Ctrl Pts',(-20.6104629916729,14.3608278404858,
130.729644462962)) ;
#121420 = CARTESIAN_POINT('Ctrl Pts',(-20.5442923362831,14.2256360028295,
130.503103888384)) ;
#121421 = CARTESIAN_POINT('Ctrl Pts',(-20.4928914107022,14.0344799528452,
130.320003827834)) ;
#121422 = CARTESIAN_POINT('Ctrl Pts',(-20.4597855514147,13.7980435581084,
130.190076931057)) ;
#121423 = CARTESIAN_POINT('Ctrl Pts',(-20.4486586873055,13.5353241773225,
130.124460154582)) ;
#121424 = CARTESIAN_POINT('Ctrl Pts',(-20.4608336123062,13.2644873700543,
130.126896090482)) ;
#121425 = CARTESIAN_POINT('Ctrl Pts',(-20.4962021630104,13.0050528435928,
130.197094463303)) ;
#121426 = CARTESIAN_POINT('Ctrl Pts',(-20.5529963678547,12.7754380039954,
130.329861771733)) ;
#121427 = CARTESIAN_POINT('Ctrl Pts',(-20.6277229494288,12.592596001974,130.515070189189)) ;
#121428 = CARTESIAN_POINT('Ctrl Pts',(-20.7157538716564,12.4690081971512,
130.7391650434)) ;
#121429 = CARTESIAN_POINT('Ctrl Pts',(-20.81215529802,12.4135709103977,130.987527049635)) ;
#121430 = CARTESIAN_POINT('Ctrl Pts',(-20.9094861728303,12.4306395059357,
131.238858431699)) ;
#121431 = CARTESIAN_POINT('Ctrl Pts',(-21.0026514401505,12.5185475341995,
131.477882625203)) ;
#121432 = CARTESIAN_POINT('Ctrl Pts',(-21.0853714580596,12.671844049154,131.686334990309)) ;
#121433 = CARTESIAN_POINT('Ctrl Pts',(-21.1520901264361,12.8780302029366,
131.848192197388)) ;
#121434 = CARTESIAN_POINT('Ctrl Pts',(-21.1993556490934,13.1252486430467,
131.952950580138)) ;
#121435 = CARTESIAN_POINT('Ctrl Pts',(-21.2237824667136,13.3909665765868,
131.991371817502)) ;
#121436 = CARTESIAN_POINT('Ctrl Pts',(-21.2249631077916,13.6612161076759,
131.961593524817)) ;
#121437 = CARTESIAN_POINT('Ctrl Pts',(-21.2032821738675,13.9131568870817,
131.865195643412)) ;
#121438 = CARTESIAN_POINT('Ctrl Pts',(-21.1610721766892,14.130438408173,131.708765378038)) ;
#121439 = CARTESIAN_POINT('Ctrl Pts',(-21.1021911877447,14.2969775109189,
131.503691498968)) ;
#121440 = CARTESIAN_POINT('Ctrl Pts',(-21.0308822540389,14.4015522166871,
131.262045908857)) ;
#121441 = CARTESIAN_POINT('Ctrl Pts',(-20.9542773305936,14.4350500551864,
131.005268144371)) ;
#121442 = CARTESIAN_POINT('Ctrl Pts',(-20.8777360660368,14.3967519658026,
130.748608972346)) ;
#121443 = CARTESIAN_POINT('Ctrl Pts',(-20.8074043524251,14.2884849185217,
130.510002599054)) ;
#121444 = CARTESIAN_POINT('Ctrl Pts',(-20.749265929619,14.1181740873397,130.307021314052)) ;
#121445 = CARTESIAN_POINT('Ctrl Pts',(-20.7082309862435,13.8977533327247,
130.153974766705)) ;
#121446 = CARTESIAN_POINT('Ctrl Pts',(-20.6879881266858,13.6446684520944,
130.061839853042)) ;
#121447 = CARTESIAN_POINT('Ctrl Pts',(-20.6906077186671,13.3734340111263,
130.036200343841)) ;
#121448 = CARTESIAN_POINT('Ctrl Pts',(-20.7167921465083,13.1072276556743,
130.079582037118)) ;
#121449 = CARTESIAN_POINT('Ctrl Pts',(-20.7650399369603,12.8641925362022,
130.187502545825)) ;
#121450 = CARTESIAN_POINT('Ctrl Pts',(-20.832963238355,12.6605227447286,130.352811316655)) ;
#121451 = CARTESIAN_POINT('Ctrl Pts',(-20.9161790737425,12.511411732543,130.562837268873)) ;
#121452 = CARTESIAN_POINT('Ctrl Pts',(-21.0104101058601,12.4272142071662,
130.804757170397)) ;
#121453 = CARTESIAN_POINT('Ctrl Pts',(-21.1076357922236,12.415034803424,131.055849599217)) ;
#121454 = CARTESIAN_POINT('Ctrl Pts',(-21.2035132942098,12.474749132082,131.302750086604)) ;
#121455 = CARTESIAN_POINT('Ctrl Pts',(-21.2909871122389,12.6023246098268,
131.525185960272)) ;
#121456 = CARTESIAN_POINT('Ctrl Pts',(-21.3650611723006,12.7898414639342,
131.708292226991)) ;
#121457 = CARTESIAN_POINT('Ctrl Pts',(-21.4202075769088,13.0206707820948,
131.836437001356)) ;
#121458 = CARTESIAN_POINT('Ctrl Pts',(-21.4542272676677,13.2818518807112,
131.902629387126)) ;
#121459 = CARTESIAN_POINT('Ctrl Pts',(-21.4648599024733,13.552127865025,131.900639172206)) ;
#121460 = CARTESIAN_POINT('Ctrl Pts',(-21.4523288216463,13.8139569141608,
131.830891201632)) ;
#121461 = CARTESIAN_POINT('Ctrl Pts',(-21.4178069877882,14.0485699408796,
131.696750338238)) ;
#121462 = CARTESIAN_POINT('Ctrl Pts',(-21.3654129791233,14.2361101899088,
131.510797708734)) ;
#121463 = CARTESIAN_POINT('Ctrl Pts',(-21.2983585521537,14.3675384217247,
131.281604089224)) ;
#121464 = CARTESIAN_POINT('Ctrl Pts',(-21.2231826385857,14.4300942313948,
131.028889010739)) ;
#121465 = CARTESIAN_POINT('Ctrl Pts',(-21.1459130475057,14.420886512356,130.770144409633)) ;
#121466 = CARTESIAN_POINT('Ctrl Pts',(-21.0723793346089,14.3405660853883,
130.522250778554)) ;
#121467 = CARTESIAN_POINT('Ctrl Pts',(-21.0083875990447,14.1934622330658,
130.302023410579)) ;
#121468 = CARTESIAN_POINT('Ctrl Pts',(-20.9600343878473,13.9917021731483,
130.127656755271)) ;
#121469 = CARTESIAN_POINT('Ctrl Pts',(-20.9311102303853,13.7502056369867,
130.010153543516)) ;
#121470 = CARTESIAN_POINT('Ctrl Pts',(-20.9242456069076,13.4844947151479,
129.956978964617)) ;
#121471 = CARTESIAN_POINT('Ctrl Pts',(-20.9408737681755,13.2141840714607,
129.972407443897)) ;
#121472 = CARTESIAN_POINT('Ctrl Pts',(-20.9804309573197,12.958922795002,130.054838696586)) ;
#121473 = CARTESIAN_POINT('Ctrl Pts',(-21.0412242853496,12.7362702687102,
130.199165296148)) ;
#121474 = CARTESIAN_POINT('Ctrl Pts',(-21.1183210212108,12.5648474915298,
130.391527393433)) ;
#121475 = CARTESIAN_POINT('Ctrl Pts',(-21.2088711021638,12.452872631945,130.622756430255)) ;
#121476 = CARTESIAN_POINT('Ctrl Pts',(-21.305434804131,12.41129419742,130.87181816482)) ;
#121477 = CARTESIAN_POINT('Ctrl Pts',(-21.4029320135723,12.4419882083232,
131.123442256635)) ;
#121478 = CARTESIAN_POINT('Ctrl Pts',(-21.494257982038,12.5427027848013,131.357191590523)) ;
#121479 = CARTESIAN_POINT('Ctrl Pts',(-21.57433818966,12.7067963976432,131.557963432826)) ;
#121480 = CARTESIAN_POINT('Ctrl Pts',(-21.637741419676,12.9221001541686,131.710056772353)) ;
#121481 = CARTESIAN_POINT('Ctrl Pts',(-21.6808145966047,13.1741319902504,
131.802654834912)) ;
#121482 = CARTESIAN_POINT('Ctrl Pts',(-21.7009520245888,13.4427023362762,
131.828426315282)) ;
#121483 = CARTESIAN_POINT('Ctrl Pts',(-21.6976514844297,13.7107857212086,
131.78560637095)) ;
#121484 = CARTESIAN_POINT('Ctrl Pts',(-21.6719724150692,13.956888330194,131.677603451996)) ;
#121485 = CARTESIAN_POINT('Ctrl Pts',(-21.6262697094113,14.1661036929037,
131.51093449669)) ;
#121486 = CARTESIAN_POINT('Ctrl Pts',(-21.5645026106687,14.3219385193613,
131.297320065824)) ;
#121487 = CARTESIAN_POINT('Ctrl Pts',(-21.4921557412151,14.4130180852625,
131.052898813796)) ;
#121488 = CARTESIAN_POINT('Ctrl Pts',(-21.4147863917618,14.4335349336769,
130.793743869836)) ;
#121489 = CARTESIAN_POINT('Ctrl Pts',(-21.3385730740908,14.3810414218173,
130.537852192733)) ;
#121490 = CARTESIAN_POINT('Ctrl Pts',(-21.2705346380607,14.2609490828525,
130.306144265951)) ;
#121491 = CARTESIAN_POINT('Ctrl Pts',(-21.2151219074894,14.079534400134,130.111008834385)) ;
#121492 = CARTESIAN_POINT('Ctrl Pts',(-21.177937738515,13.8529283959852,129.96942799476)) ;
#121493 = CARTESIAN_POINT('Ctrl Pts',(-21.1617508066486,13.5926907244754,
129.888787697885)) ;
#121494 = CARTESIAN_POINT('Ctrl Pts',(-21.1688878360298,13.3230678017147,
129.87665122898)) ;
#121495 = CARTESIAN_POINT('Ctrl Pts',(-21.1992585105796,13.0595444653147,
129.9322501518)) ;
#121496 = CARTESIAN_POINT('Ctrl Pts',(-21.251765609534,12.8214089114898,130.052423624605)) ;
#121497 = CARTESIAN_POINT('Ctrl Pts',(-21.3231412688293,12.6270967453298,
130.227778003325)) ;
#121498 = CARTESIAN_POINT('Ctrl Pts',(-21.4083872685259,12.4904301737517,
130.443872721006)) ;
#121499 = CARTESIAN_POINT('Ctrl Pts',(-21.5034218070146,12.41952640959,130.688294257978)) ;
#121500 = CARTESIAN_POINT('Ctrl Pts',(-21.6011087851476,12.4206998048116,
130.940608218909)) ;
#121501 = CARTESIAN_POINT('Ctrl Pts',(-21.696063140712,12.4940151693159,131.18475236496)) ;
#121502 = CARTESIAN_POINT('Ctrl Pts',(-21.7810646279155,12.6331734793058,
131.400063934903)) ;
#121503 = CARTESIAN_POINT('Ctrl Pts',(-21.8518067818107,12.8293256852298,
131.573571896818)) ;
#121504 = CARTESIAN_POINT('Ctrl Pts',(-21.9034926777369,13.0683012939604,
131.691398405443)) ;
#121505 = CARTESIAN_POINT('Ctrl Pts',(-21.9331090686563,13.3322967725392,
131.74480552703)) ;
#121506 = CARTESIAN_POINT('Ctrl Pts',(-21.9393783070901,13.6026350043085,
131.730028295471)) ;
#121507 = CARTESIAN_POINT('Ctrl Pts',(-21.9225550826518,13.8605088968992,
131.647745173543)) ;
#121508 = CARTESIAN_POINT('Ctrl Pts',(-21.8844777064328,14.0871784640944,
131.503344143957)) ;
#121509 = CARTESIAN_POINT('Ctrl Pts',(-21.8287676502295,14.265834440122,131.307501478219)) ;
#121510 = CARTESIAN_POINT('Ctrl Pts',(-21.760017708765,14.3843789684771,131.073534055057)) ;
#121511 = CARTESIAN_POINT('Ctrl Pts',(-21.6837666999361,14.4339734265458,
130.817596552073)) ;
#121512 = CARTESIAN_POINT('Ctrl Pts',(-21.6066788030557,14.4110559210102,
130.559350636955)) ;
#121513 = CARTESIAN_POINT('Ctrl Pts',(-21.5346094087633,14.3178924901581,
130.315757506672)) ;
#121514 = CARTESIAN_POINT('Ctrl Pts',(-21.4731242757902,14.1593686470185,
130.102848783246)) ;
#121515 = CARTESIAN_POINT('Ctrl Pts',(-21.4282515814187,13.9496805218115,
129.938774151377)) ;
#121516 = CARTESIAN_POINT('Ctrl Pts',(-21.4031364018714,13.7013469938743,
129.832244367826)) ;
#121517 = CARTESIAN_POINT('Ctrl Pts',(-21.4007180388891,13.4330164717232,
129.792025041528)) ;
#121518 = CARTESIAN_POINT('Ctrl Pts',(-21.4216646330142,13.1647607715786,
129.820160982068)) ;
#121519 = CARTESIAN_POINT('Ctrl Pts',(-21.4655479362394,12.9137312008662,
129.915122311114)) ;
#121520 = CARTESIAN_POINT('Ctrl Pts',(-21.529321250798,12.7007529783777,130.068427667511)) ;
#121521 = CARTESIAN_POINT('Ctrl Pts',(-21.6099312650928,12.5383275920807,
130.270711053567)) ;
#121522 = CARTESIAN_POINT('Ctrl Pts',(-21.7015227704485,12.4398166111486,
130.505243913684)) ;
#121523 = CARTESIAN_POINT('Ctrl Pts',(-21.7994399744814,12.4114725010168,
130.757982304775)) ;
#121524 = CARTESIAN_POINT('Ctrl Pts',(-21.8958871845684,12.4557968950616,
131.006694284982)) ;
#121525 = CARTESIAN_POINT('Ctrl Pts',(-21.9858132022225,12.569629101587,131.236208930516)) ;
